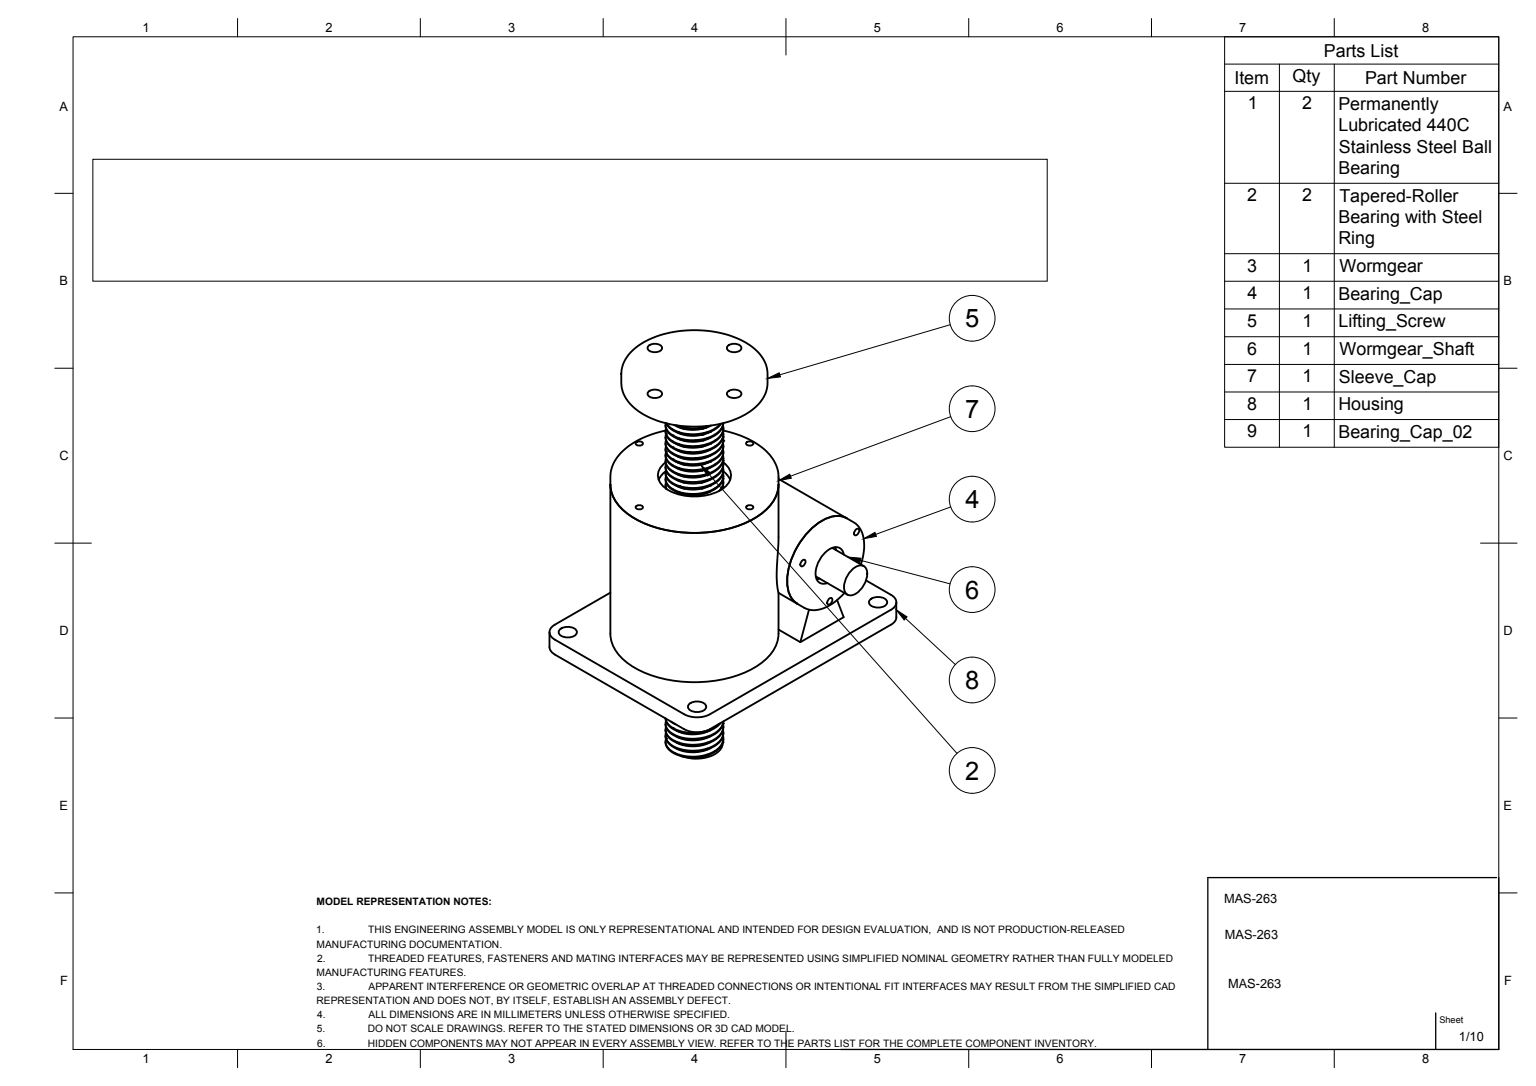
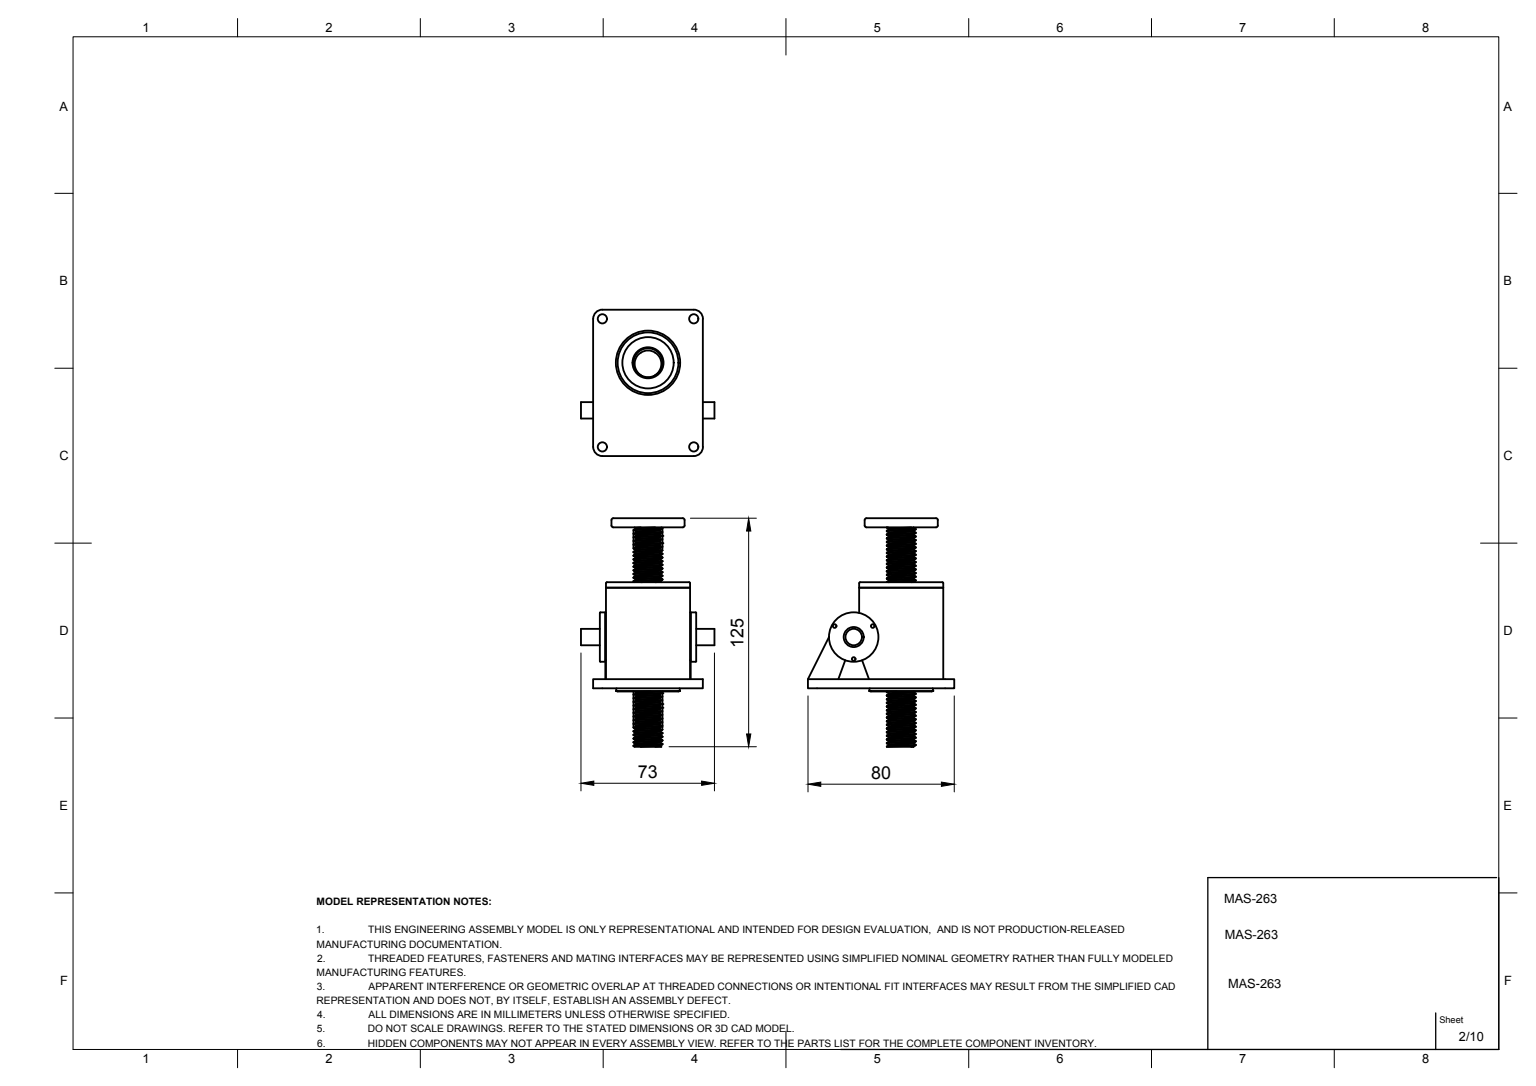
ISO-10303-21;
HEADER;
/* Generated by software containing ST-Developer
 * from STEP Tools, Inc. (www.steptools.com) 
 */

FILE_DESCRIPTION(
/* description */ (''),
/* implementation_level */ '2;1');

FILE_NAME(
/* name */ 'MAS-263',
/* time_stamp */ '2026-10-12T15:47:30-07:00',
/* author */ (''),
/* organization */ (''),
/* preprocessor_version */ 'ST-DEVELOPER v20.2',
/* originating_system */ 'Autodesk Translation Framework v15.15.0.0',
/* authorisation */ '');

FILE_SCHEMA (('AUTOMOTIVE_DESIGN { 1 0 10303 214 3 1 1 }'));
ENDSEC;

DATA;
#10=MECHANICAL_DESIGN_GEOMETRIC_PRESENTATION_REPRESENTATION('',(#82,#83,
#84,#85,#86,#87,#88,#89,#90,#91,#92,#93,#94,#95,#96,#97,#98,#99,#100,#101,
#102,#103,#104,#105,#106,#107,#108,#109,#110,#111,#112,#113,#114,#115,#116),
#88483);
#11=ITEM_DEFINED_TRANSFORMATION($,$,#13993,#14368);
#12=ITEM_DEFINED_TRANSFORMATION($,$,#14115,#14369);
#13=ITEM_DEFINED_TRANSFORMATION($,$,#13128,#14370);
#14=ITEM_DEFINED_TRANSFORMATION($,$,#13713,#14371);
#15=ITEM_DEFINED_TRANSFORMATION($,$,#13735,#14372);
#16=ITEM_DEFINED_TRANSFORMATION($,$,#13828,#14373);
#17=ITEM_DEFINED_TRANSFORMATION($,$,#13851,#14374);
#18=ITEM_DEFINED_TRANSFORMATION($,$,#13876,#14375);
#19=ITEM_DEFINED_TRANSFORMATION($,$,#13971,#14376);
#20=ITEM_DEFINED_TRANSFORMATION($,$,#13993,#14377);
#21=ITEM_DEFINED_TRANSFORMATION($,$,#14115,#14378);
#22=(
REPRESENTATION_RELATIONSHIP($,$,#88527,#88519)
REPRESENTATION_RELATIONSHIP_WITH_TRANSFORMATION(#11)
SHAPE_REPRESENTATION_RELATIONSHIP()
);
#23=(
REPRESENTATION_RELATIONSHIP($,$,#88528,#88519)
REPRESENTATION_RELATIONSHIP_WITH_TRANSFORMATION(#12)
SHAPE_REPRESENTATION_RELATIONSHIP()
);
#24=(
REPRESENTATION_RELATIONSHIP($,$,#88520,#88519)
REPRESENTATION_RELATIONSHIP_WITH_TRANSFORMATION(#13)
SHAPE_REPRESENTATION_RELATIONSHIP()
);
#25=(
REPRESENTATION_RELATIONSHIP($,$,#88521,#88519)
REPRESENTATION_RELATIONSHIP_WITH_TRANSFORMATION(#14)
SHAPE_REPRESENTATION_RELATIONSHIP()
);
#26=(
REPRESENTATION_RELATIONSHIP($,$,#88522,#88519)
REPRESENTATION_RELATIONSHIP_WITH_TRANSFORMATION(#15)
SHAPE_REPRESENTATION_RELATIONSHIP()
);
#27=(
REPRESENTATION_RELATIONSHIP($,$,#88523,#88519)
REPRESENTATION_RELATIONSHIP_WITH_TRANSFORMATION(#16)
SHAPE_REPRESENTATION_RELATIONSHIP()
);
#28=(
REPRESENTATION_RELATIONSHIP($,$,#88524,#88519)
REPRESENTATION_RELATIONSHIP_WITH_TRANSFORMATION(#17)
SHAPE_REPRESENTATION_RELATIONSHIP()
);
#29=(
REPRESENTATION_RELATIONSHIP($,$,#88525,#88519)
REPRESENTATION_RELATIONSHIP_WITH_TRANSFORMATION(#18)
SHAPE_REPRESENTATION_RELATIONSHIP()
);
#30=(
REPRESENTATION_RELATIONSHIP($,$,#88526,#88519)
REPRESENTATION_RELATIONSHIP_WITH_TRANSFORMATION(#19)
SHAPE_REPRESENTATION_RELATIONSHIP()
);
#31=(
REPRESENTATION_RELATIONSHIP($,$,#88527,#88519)
REPRESENTATION_RELATIONSHIP_WITH_TRANSFORMATION(#20)
SHAPE_REPRESENTATION_RELATIONSHIP()
);
#32=(
REPRESENTATION_RELATIONSHIP($,$,#88528,#88519)
REPRESENTATION_RELATIONSHIP_WITH_TRANSFORMATION(#21)
SHAPE_REPRESENTATION_RELATIONSHIP()
);
#33=CONTEXT_DEPENDENT_SHAPE_REPRESENTATION(#22,#88508);
#34=CONTEXT_DEPENDENT_SHAPE_REPRESENTATION(#23,#88509);
#35=CONTEXT_DEPENDENT_SHAPE_REPRESENTATION(#24,#88510);
#36=CONTEXT_DEPENDENT_SHAPE_REPRESENTATION(#25,#88511);
#37=CONTEXT_DEPENDENT_SHAPE_REPRESENTATION(#26,#88512);
#38=CONTEXT_DEPENDENT_SHAPE_REPRESENTATION(#27,#88513);
#39=CONTEXT_DEPENDENT_SHAPE_REPRESENTATION(#28,#88514);
#40=CONTEXT_DEPENDENT_SHAPE_REPRESENTATION(#29,#88515);
#41=CONTEXT_DEPENDENT_SHAPE_REPRESENTATION(#30,#88516);
#42=CONTEXT_DEPENDENT_SHAPE_REPRESENTATION(#31,#88517);
#43=CONTEXT_DEPENDENT_SHAPE_REPRESENTATION(#32,#88518);
#44=NEXT_ASSEMBLY_USAGE_OCCURRENCE(
'Permanently Lubricated 440C Stainless Steel Ball Bearing:1',
'Permanently Lubricated 440C Stainless Steel Ball Bearing:1',
'Permanently Lubricated 440C Stainless Steel Ball Bearing:1',#88530,#88538,
'Permanently Lubricated 440C Stainless Steel Ball Bearing:1');
#45=NEXT_ASSEMBLY_USAGE_OCCURRENCE(
'Tapered-Roller Bearing with Steel Ring:1',
'Tapered-Roller Bearing with Steel Ring:1',
'Tapered-Roller Bearing with Steel Ring:1',#88530,#88539,
'Tapered-Roller Bearing with Steel Ring:1');
#46=NEXT_ASSEMBLY_USAGE_OCCURRENCE('Wormgear:1','Wormgear:1',
'Wormgear:1',#88530,#88531,'Wormgear:1');
#47=NEXT_ASSEMBLY_USAGE_OCCURRENCE('Bearing_Cap:1','Bearing_Cap:1',
'Bearing_Cap:1',#88530,#88532,'Bearing_Cap:1');
#48=NEXT_ASSEMBLY_USAGE_OCCURRENCE('Lifting_Screw:1','Lifting_Screw:1',
'Lifting_Screw:1',#88530,#88533,'Lifting_Screw:1');
#49=NEXT_ASSEMBLY_USAGE_OCCURRENCE('Wormgear_Shaft:1',
'Wormgear_Shaft:1','Wormgear_Shaft:1',#88530,#88534,'Wormgear_Shaft:1');
#50=NEXT_ASSEMBLY_USAGE_OCCURRENCE('Sleeve_Cap:1','Sleeve_Cap:1',
'Sleeve_Cap:1',#88530,#88535,'Sleeve_Cap:1');
#51=NEXT_ASSEMBLY_USAGE_OCCURRENCE('Housing:1','Housing:1','Housing:1',
#88530,#88536,'Housing:1');
#52=NEXT_ASSEMBLY_USAGE_OCCURRENCE('Bearing_Cap_02:1',
'Bearing_Cap_02:1','Bearing_Cap_02:1',#88530,#88537,'Bearing_Cap_02:1');
#53=NEXT_ASSEMBLY_USAGE_OCCURRENCE(
'Permanently Lubricated 440C Stainless Steel Ball Bearing:2',
'Permanently Lubricated 440C Stainless Steel Ball Bearing:2',
'Permanently Lubricated 440C Stainless Steel Ball Bearing:2',#88530,#88538,
'Permanently Lubricated 440C Stainless Steel Ball Bearing:2');
#54=NEXT_ASSEMBLY_USAGE_OCCURRENCE(
'Tapered-Roller Bearing with Steel Ring:2',
'Tapered-Roller Bearing with Steel Ring:2',
'Tapered-Roller Bearing with Steel Ring:2',#88530,#88539,
'Tapered-Roller Bearing with Steel Ring:2');
#55=SPHERICAL_SURFACE('',#14025,2.0625);
#56=SPHERICAL_SURFACE('',#14081,2.0625);
#57=SPHERICAL_SURFACE('',#14083,2.0625);
#58=SPHERICAL_SURFACE('',#14085,2.0625);
#59=SPHERICAL_SURFACE('',#14087,2.0625);
#60=SPHERICAL_SURFACE('',#14089,2.0625);
#61=SPHERICAL_SURFACE('',#14091,2.0625);
#62=SPHERICAL_SURFACE('',#14093,2.0625);
#63=SPHERICAL_SURFACE('',#14095,2.0625);
#64=SHAPE_REPRESENTATION_RELATIONSHIP('SRR','None',#88520,#73);
#65=SHAPE_REPRESENTATION_RELATIONSHIP('SRR','None',#88521,#74);
#66=SHAPE_REPRESENTATION_RELATIONSHIP('SRR','None',#88522,#75);
#67=SHAPE_REPRESENTATION_RELATIONSHIP('SRR','None',#88523,#76);
#68=SHAPE_REPRESENTATION_RELATIONSHIP('SRR','None',#88524,#77);
#69=SHAPE_REPRESENTATION_RELATIONSHIP('SRR','None',#88525,#78);
#70=SHAPE_REPRESENTATION_RELATIONSHIP('SRR','None',#88526,#79);
#71=SHAPE_REPRESENTATION_RELATIONSHIP('SRR','None',#88527,#80);
#72=SHAPE_REPRESENTATION_RELATIONSHIP('SRR','None',#88528,#81);
#73=ADVANCED_BREP_SHAPE_REPRESENTATION('',(#117),#88474);
#74=ADVANCED_BREP_SHAPE_REPRESENTATION('',(#118),#88475);
#75=ADVANCED_BREP_SHAPE_REPRESENTATION('',(#119),#88476);
#76=ADVANCED_BREP_SHAPE_REPRESENTATION('',(#120),#88477);
#77=ADVANCED_BREP_SHAPE_REPRESENTATION('',(#121),#88478);
#78=ADVANCED_BREP_SHAPE_REPRESENTATION('',(#122),#88479);
#79=ADVANCED_BREP_SHAPE_REPRESENTATION('',(#123),#88480);
#80=ADVANCED_BREP_SHAPE_REPRESENTATION('',(#124,#125,#126,#127,#128,#129,
#130,#131,#132,#133,#134,#135,#136,#137),#88481);
#81=ADVANCED_BREP_SHAPE_REPRESENTATION('',(#138,#139,#140,#141,#142,#143,
#144,#145,#146,#147,#148,#149,#150,#151),#88482);
#82=STYLED_ITEM('',(#88574),#117);
#83=STYLED_ITEM('',(#88574),#118);
#84=STYLED_ITEM('',(#88574),#119);
#85=STYLED_ITEM('',(#88574),#120);
#86=STYLED_ITEM('',(#88574),#121);
#87=STYLED_ITEM('',(#88574),#122);
#88=STYLED_ITEM('',(#88574),#123);
#89=STYLED_ITEM('',(#88574),#124);
#90=STYLED_ITEM('',(#88574),#125);
#91=STYLED_ITEM('',(#88574),#126);
#92=STYLED_ITEM('',(#88574),#127);
#93=STYLED_ITEM('',(#88574),#128);
#94=STYLED_ITEM('',(#88574),#129);
#95=STYLED_ITEM('',(#88574),#130);
#96=STYLED_ITEM('',(#88574),#131);
#97=STYLED_ITEM('',(#88574),#132);
#98=STYLED_ITEM('',(#88574),#133);
#99=STYLED_ITEM('',(#88574),#134);
#100=STYLED_ITEM('',(#88574),#135);
#101=STYLED_ITEM('',(#88574),#136);
#102=STYLED_ITEM('',(#88574),#137);
#103=STYLED_ITEM('',(#88574),#138);
#104=STYLED_ITEM('',(#88574),#139);
#105=STYLED_ITEM('',(#88574),#140);
#106=STYLED_ITEM('',(#88574),#141);
#107=STYLED_ITEM('',(#88574),#142);
#108=STYLED_ITEM('',(#88574),#143);
#109=STYLED_ITEM('',(#88574),#144);
#110=STYLED_ITEM('',(#88574),#145);
#111=STYLED_ITEM('',(#88574),#146);
#112=STYLED_ITEM('',(#88574),#147);
#113=STYLED_ITEM('',(#88574),#148);
#114=STYLED_ITEM('',(#88574),#149);
#115=STYLED_ITEM('',(#88574),#150);
#116=STYLED_ITEM('',(#88574),#151);
#117=MANIFOLD_SOLID_BREP('Body1',#12992);
#118=MANIFOLD_SOLID_BREP('Body1',#12993);
#119=MANIFOLD_SOLID_BREP('Body1',#12994);
#120=MANIFOLD_SOLID_BREP('Body1',#12995);
#121=MANIFOLD_SOLID_BREP('Body1',#12996);
#122=MANIFOLD_SOLID_BREP('Body1',#12997);
#123=MANIFOLD_SOLID_BREP('Body1',#12998);
#124=MANIFOLD_SOLID_BREP('Body1',#12999);
#125=MANIFOLD_SOLID_BREP('Body2',#13000);
#126=MANIFOLD_SOLID_BREP('Body3',#13001);
#127=MANIFOLD_SOLID_BREP('Body4',#13002);
#128=MANIFOLD_SOLID_BREP('Body5',#13003);
#129=MANIFOLD_SOLID_BREP('Body6',#13004);
#130=MANIFOLD_SOLID_BREP('Body7',#13005);
#131=MANIFOLD_SOLID_BREP('Body8',#13006);
#132=MANIFOLD_SOLID_BREP('Body9',#13007);
#133=MANIFOLD_SOLID_BREP('Body10',#13008);
#134=MANIFOLD_SOLID_BREP('Body11',#13009);
#135=MANIFOLD_SOLID_BREP('Body12',#13010);
#136=MANIFOLD_SOLID_BREP('Body13',#13011);
#137=MANIFOLD_SOLID_BREP('Body14',#13012);
#138=MANIFOLD_SOLID_BREP('Body1',#13013);
#139=MANIFOLD_SOLID_BREP('Body2',#13014);
#140=MANIFOLD_SOLID_BREP('Body3',#13015);
#141=MANIFOLD_SOLID_BREP('Body4',#13016);
#142=MANIFOLD_SOLID_BREP('Body5',#13017);
#143=MANIFOLD_SOLID_BREP('Body6',#13018);
#144=MANIFOLD_SOLID_BREP('Body7',#13019);
#145=MANIFOLD_SOLID_BREP('Body8',#13020);
#146=MANIFOLD_SOLID_BREP('Body9',#13021);
#147=MANIFOLD_SOLID_BREP('Body10',#13022);
#148=MANIFOLD_SOLID_BREP('Body11',#13023);
#149=MANIFOLD_SOLID_BREP('Body12',#13024);
#150=MANIFOLD_SOLID_BREP('Body13',#13025);
#151=MANIFOLD_SOLID_BREP('Body14',#13026);
#152=TOROIDAL_SURFACE('',#13586,31.2524414898979,12.0232331490224);
#153=TOROIDAL_SURFACE('',#13587,31.2524414898979,12.0232331490224);
#154=TOROIDAL_SURFACE('',#13588,31.2524414898979,12.0232331490224);
#155=TOROIDAL_SURFACE('',#13589,31.2524414898979,12.0232331490224);
#156=TOROIDAL_SURFACE('',#13590,31.2524414898979,12.0232331490224);
#157=TOROIDAL_SURFACE('',#13591,31.2524414898979,12.0232331490224);
#158=TOROIDAL_SURFACE('',#13592,31.2524414898979,12.0232331490224);
#159=TOROIDAL_SURFACE('',#13593,31.2524414898979,12.0232331490224);
#160=TOROIDAL_SURFACE('',#13594,31.2524414898979,12.0232331490224);
#161=TOROIDAL_SURFACE('',#13595,31.2524414898979,12.0232331490224);
#162=TOROIDAL_SURFACE('',#13596,31.2524414898979,12.0232331490224);
#163=TOROIDAL_SURFACE('',#13597,31.2524414898979,12.0232331490224);
#164=TOROIDAL_SURFACE('',#13598,31.2524414898979,12.0232331490224);
#165=TOROIDAL_SURFACE('',#13599,31.2524414898979,12.0232331490224);
#166=TOROIDAL_SURFACE('',#13600,31.2524414898979,12.0232331490224);
#167=TOROIDAL_SURFACE('',#13601,31.2524414898979,12.0232331490224);
#168=TOROIDAL_SURFACE('',#13602,31.2524414898979,12.0232331490224);
#169=TOROIDAL_SURFACE('',#13603,31.2524414898979,12.0232331490224);
#170=TOROIDAL_SURFACE('',#13723,13.2,0.3);
#171=TOROIDAL_SURFACE('',#13814,19.,1.);
#172=TOROIDAL_SURFACE('',#13823,19.,1.);
#173=TOROIDAL_SURFACE('',#13852,22.5,0.5);
#174=TOROIDAL_SURFACE('',#13981,13.2,0.3);
#175=TOROIDAL_SURFACE('',#13994,7.57083333333333,2.0625);
#176=TOROIDAL_SURFACE('',#14007,5.00416666666667,0.260975870478375);
#177=TOROIDAL_SURFACE('',#14010,5.98069079618829,0.260975870478375);
#178=TOROIDAL_SURFACE('',#14017,5.98069079618829,0.260975870478375);
#179=TOROIDAL_SURFACE('',#14020,5.00416666666667,0.260975870478376);
#180=TOROIDAL_SURFACE('',#14030,6.50566666666666,0.0439999999999998);
#181=TOROIDAL_SURFACE('',#14047,6.50566666666666,0.0439999999999998);
#182=TOROIDAL_SURFACE('',#14075,7.57083333333333,2.0625);
#183=TOROIDAL_SURFACE('',#14100,6.32416666666667,0.0824999999999997);
#184=TOROIDAL_SURFACE('',#14105,6.42956528249449,0.0228986158278278);
#185=TOROIDAL_SURFACE('',#14116,19.725,0.275);
#186=TOROIDAL_SURFACE('',#14121,19.725,0.275);
#187=TOROIDAL_SURFACE('',#14141,13.4297712445485,0.500000000000001);
#188=TOROIDAL_SURFACE('',#14288,8.775,0.275);
#189=TOROIDAL_SURFACE('',#14293,8.775,0.275);
#190=ELLIPSE('',#13431,4.95617711892471,2.63133228090511);
#191=ELLIPSE('',#13435,4.75668688712327,2.27225375309584);
#192=ELLIPSE('',#13437,4.75863627530638,2.27415348140964);
#193=ELLIPSE('',#13440,4.95728877126817,2.63371397588203);
#194=ELLIPSE('',#13442,4.75866828260205,2.27425851275333);
#195=ELLIPSE('',#13445,4.75676106745748,2.27242229825786);
#196=ELLIPSE('',#13449,4.95667352087062,2.63240829794641);
#197=ELLIPSE('',#13451,4.7584190628443,2.27363285019894);
#198=ELLIPSE('',#13454,4.95667835669603,2.63239579497757);
#199=ELLIPSE('',#13456,4.75854812753772,2.27394108049538);
#200=ELLIPSE('',#13459,4.75677100793017,2.27242870543475);
#201=ELLIPSE('',#13461,4.75867193464204,2.27425380136302);
#202=ELLIPSE('',#13464,4.95726759568865,2.6336926662635);
#203=ELLIPSE('',#13468,4.95701438814411,2.63313504607068);
#204=ELLIPSE('',#13470,4.75854681981732,2.2739502765965);
#205=ELLIPSE('',#13473,4.95618501228156,2.63134042899261);
#206=ELLIPSE('',#13475,4.7584142614767,2.27361309014758);
#207=ELLIPSE('',#13478,4.75669159480521,2.2722579746974);
#208=ELLIPSE('',#13480,4.75864115660623,2.27415786894356);
#209=ELLIPSE('',#13483,4.95728232466036,2.63370732110983);
#210=ELLIPSE('',#13487,4.75677068526519,2.27243087287144);
#211=ELLIPSE('',#13489,4.7586448406126,2.27416728394003);
#212=ELLIPSE('',#13492,4.95668328813391,2.63241837237374);
#213=ELLIPSE('',#13494,4.75842436294074,2.27363759998898);
#214=ELLIPSE('',#13497,4.95667013101771,2.63238731158809);
#215=ELLIPSE('',#13499,4.75854743391675,2.27394045782711);
#216=ELLIPSE('',#13502,4.75676675579442,2.2724249104892);
#217=ELLIPSE('',#13504,4.75867738441917,2.27425870334034);
#218=ELLIPSE('',#13507,4.95726880833492,2.63369391317148);
#219=ELLIPSE('',#13511,4.75669596930896,2.27226683434943);
#220=ELLIPSE('',#13516,4.95643307274524,2.6318762393004);
#221=ELLIPSE('',#13520,4.75673549365485,2.27235394216187);
#222=ELLIPSE('',#13524,4.75679029012967,2.27247967692196);
#223=ELLIPSE('',#13528,4.7567393782921,2.272363575723);
#224=ELLIPSE('',#13532,4.75651933654551,2.27183321728508);
#225=ELLIPSE('',#13536,4.75664142700045,2.27213579341419);
#226=ELLIPSE('',#13540,4.75678866048944,2.27247015627199);
#227=ELLIPSE('',#13544,4.75677929568429,2.27246401653084);
#228=ELLIPSE('',#13548,4.7566467644084,2.27215101059843);
#229=ELLIPSE('',#13552,4.75649416981517,2.27179513573923);
#230=ELLIPSE('',#13556,4.75673834040189,2.27235649175302);
#231=ELLIPSE('',#13560,4.7567849310581,2.27247488275134);
#232=ELLIPSE('',#13564,4.75674169310957,2.27236560062855);
#233=ELLIPSE('',#13568,4.75650474573201,2.27182012088408);
#234=ELLIPSE('',#13572,4.75664401077444,2.27213811276921);
#235=ELLIPSE('',#13576,4.75677759115208,2.27246023178278);
#236=ELLIPSE('',#13580,4.95724426884637,2.63364727447111);
#237=ELLIPSE('',#13584,4.95686686267409,2.63282116312156);
#238=ELLIPSE('',#13840,8.40043383461932,7.09899410493904);
#239=ELLIPSE('',#13843,8.34870203930529,7.04180185640227);
#240=ELLIPSE('',#13948,67.247501203751,23.);
#241=ELLIPSE('',#13950,67.247501203751,23.);
#242=ELLIPSE('',#14151,15.0801280312954,14.5834816640173);
#243=ELLIPSE('',#14152,17.3517853554452,16.7803246128912);
#244=ELLIPSE('',#14153,17.3517853554452,16.7803246128912);
#245=ELLIPSE('',#14154,15.0801280312954,14.5834816640173);
#246=ELLIPSE('',#14155,15.0801280312954,14.5834816640173);
#247=ELLIPSE('',#14156,17.3517853554452,16.7803246128912);
#248=ELLIPSE('',#14157,17.3517853554886,16.7803246129121);
#249=ELLIPSE('',#14158,15.0801280313552,14.5834816640461);
#250=ELLIPSE('',#14159,17.351785355493,16.7803246129139);
#251=ELLIPSE('',#14160,15.0801280313139,14.5834816640261);
#252=ELLIPSE('',#14161,17.3517853552649,16.7803246128045);
#253=ELLIPSE('',#14162,15.0801280313118,14.583481664025);
#254=ELLIPSE('',#14163,17.3517853554016,16.7803246128701);
#255=ELLIPSE('',#14164,15.0801280313076,14.583481664023);
#256=ELLIPSE('',#14165,17.3517853554702,16.780324612903);
#257=ELLIPSE('',#14166,15.0801280313709,14.5834816640533);
#258=ELLIPSE('',#14167,17.3517853554861,16.7803246129107);
#259=ELLIPSE('',#14168,15.08012803127,14.583481664005);
#260=ELLIPSE('',#14169,17.3517853554707,16.7803246129033);
#261=ELLIPSE('',#14170,15.0801280312716,14.5834816640059);
#262=ELLIPSE('',#14171,17.3517853553197,16.7803246128311);
#263=ELLIPSE('',#14172,15.0801280311918,14.5834816639677);
#264=ELLIPSE('',#14173,17.3517853552856,16.7803246128146);
#265=ELLIPSE('',#14174,15.0801280313508,14.5834816640437);
#266=ELLIPSE('',#14176,18.421055935048,17.8143800174044);
#267=ELLIPSE('',#14177,16.1493986108983,15.6175370685304);
#268=ELLIPSE('',#14178,16.1493986108983,15.6175370685304);
#269=ELLIPSE('',#14179,18.421055935048,17.8143800174044);
#270=ELLIPSE('',#14180,16.1493986108983,15.6175370685304);
#271=ELLIPSE('',#14181,18.421055935048,17.8143800174044);
#272=ELLIPSE('',#14182,18.4210559352732,17.8143800175124);
#273=ELLIPSE('',#14183,16.1493986107542,15.6175370684613);
#274=ELLIPSE('',#14184,18.4210559346699,17.8143800172222);
#275=ELLIPSE('',#14185,16.1493986106406,15.6175370684066);
#276=ELLIPSE('',#14186,18.421055934899,17.8143800173331);
#277=ELLIPSE('',#14187,16.1493986106858,15.6175370684285);
#278=ELLIPSE('',#14188,18.4210559350675,17.8143800174135);
#279=ELLIPSE('',#14189,16.1493986109801,15.6175370685696);
#280=ELLIPSE('',#14190,18.4210559350065,17.8143800173844);
#281=ELLIPSE('',#14191,16.1493986108565,15.6175370685105);
#282=ELLIPSE('',#14192,18.4210559345343,17.8143800171572);
#283=ELLIPSE('',#14193,16.1493986108155,15.6175370684905);
#284=ELLIPSE('',#14194,18.4210559346994,17.8143800172367);
#285=ELLIPSE('',#14195,16.1493986107405,15.6175370684544);
#286=ELLIPSE('',#14196,18.4210559344304,17.814380017107);
#287=ELLIPSE('',#14197,16.1493986109695,15.6175370685645);
#288=ELLIPSE('',#14198,18.4210559346512,17.8143800172135);
#289=ELLIPSE('',#14199,16.1493986107542,15.6175370684612);
#290=CONICAL_SURFACE('',#13250,17.9979895488606,0.785398163397448);
#291=CONICAL_SURFACE('',#13253,17.9979895488606,0.785398163397448);
#292=CONICAL_SURFACE('',#13256,17.9979895488606,0.785398163397448);
#293=CONICAL_SURFACE('',#13259,17.9979895488606,0.785398163397448);
#294=CONICAL_SURFACE('',#13262,17.9979895488606,0.785398163397448);
#295=CONICAL_SURFACE('',#13265,17.9979895488606,0.785398163397448);
#296=CONICAL_SURFACE('',#13268,17.9979895488606,0.785398163397448);
#297=CONICAL_SURFACE('',#13271,17.9979895488606,0.785398163397448);
#298=CONICAL_SURFACE('',#13274,17.9979895488606,0.785398163397448);
#299=CONICAL_SURFACE('',#13277,17.9979895488606,0.785398163397448);
#300=CONICAL_SURFACE('',#13280,17.9979895488606,0.785398163397448);
#301=CONICAL_SURFACE('',#13283,17.9979895488606,0.785398163397448);
#302=CONICAL_SURFACE('',#13286,17.9979895488606,0.785398163397448);
#303=CONICAL_SURFACE('',#13289,17.9979895488606,0.785398163397448);
#304=CONICAL_SURFACE('',#13292,17.9979895488606,0.785398163397448);
#305=CONICAL_SURFACE('',#13295,17.9979895488606,0.785398163397448);
#306=CONICAL_SURFACE('',#13298,17.9979895488606,0.785398163397448);
#307=CONICAL_SURFACE('',#13301,17.9979895488606,0.785398163397448);
#308=CONICAL_SURFACE('',#13304,17.9979895488606,0.785398163397448);
#309=CONICAL_SURFACE('',#13309,17.9979895488606,0.785398163397448);
#310=CONICAL_SURFACE('',#13314,17.9979895488606,0.785398163397448);
#311=CONICAL_SURFACE('',#13319,17.9979895488606,0.785398163397448);
#312=CONICAL_SURFACE('',#13324,17.9979895488606,0.785398163397448);
#313=CONICAL_SURFACE('',#13329,17.9979895488606,0.785398163397448);
#314=CONICAL_SURFACE('',#13334,17.9979895488606,0.785398163397448);
#315=CONICAL_SURFACE('',#13339,17.9979895488606,0.785398163397448);
#316=CONICAL_SURFACE('',#13344,17.9979895488606,0.785398163397448);
#317=CONICAL_SURFACE('',#13349,17.9979895488606,0.785398163397448);
#318=CONICAL_SURFACE('',#13354,17.9979895488606,0.785398163397448);
#319=CONICAL_SURFACE('',#13359,17.9979895488606,0.785398163397448);
#320=CONICAL_SURFACE('',#13364,17.9979895488606,0.785398163397448);
#321=CONICAL_SURFACE('',#13369,17.9979895488606,0.785398163397448);
#322=CONICAL_SURFACE('',#13374,17.9979895488606,0.785398163397448);
#323=CONICAL_SURFACE('',#13379,17.9979895488606,0.785398163397448);
#324=CONICAL_SURFACE('',#13384,17.9979895488606,0.785398163397448);
#325=CONICAL_SURFACE('',#13389,17.9979895488606,0.785398163397448);
#326=CONICAL_SURFACE('',#13998,4.5,0.26179938779915);
#327=CONICAL_SURFACE('',#14005,4.75208333333333,0.261799387799149);
#328=CONICAL_SURFACE('',#14033,8.9,0.523598775598299);
#329=CONICAL_SURFACE('',#14050,8.79,0.523598775598297);
#330=CONICAL_SURFACE('',#14054,9.01847925309041,0.349065850398861);
#331=CONICAL_SURFACE('',#14057,9.16847925309041,0.78539816339744);
#332=CONICAL_SURFACE('',#14059,10.,0.523598775598291);
#333=CONICAL_SURFACE('',#14065,9.82679491924311,0.52359877559829);
#334=CONICAL_SURFACE('',#14067,9.0184792530904,0.78539816339744);
#335=CONICAL_SURFACE('',#14070,8.9,0.349065850398861);
#336=CONICAL_SURFACE('',#14109,6.46166666666667,0.17453292519942);
#337=CONICAL_SURFACE('',#14125,15.4,0.249233017184783);
#338=CONICAL_SURFACE('',#14131,12.7058184384753,1.32156330961012);
#339=CONICAL_SURFACE('',#14136,16.6071946160828,1.32156330961011);
#340=CONICAL_SURFACE('',#14146,13.3064408708579,1.32156330961011);
#341=CONICAL_SURFACE('',#14149,12.4591576910941,0.249233017184783);
#342=CONICAL_SURFACE('',#14150,13.0685506725942,0.249233017184784);
#343=CONICAL_SURFACE('',#14175,17.5762965073726,0.249233017184784);
#344=CONICAL_SURFACE('',#14297,10.6410293263727,1.32156330961011);
#345=CONICAL_SURFACE('',#14301,12.6998790237181,0.249233017184785);
#346=CONICAL_SURFACE('',#14304,14.0317131491268,1.32156330961011);
#347=FACE_BOUND('',#1491,.T.);
#348=FACE_BOUND('',#1720,.T.);
#349=FACE_BOUND('',#1788,.T.);
#350=FACE_BOUND('',#1789,.T.);
#351=FACE_BOUND('',#1790,.T.);
#352=FACE_BOUND('',#1791,.T.);
#353=FACE_BOUND('',#1794,.T.);
#354=FACE_BOUND('',#1795,.T.);
#355=FACE_BOUND('',#1796,.T.);
#356=FACE_BOUND('',#1797,.T.);
#357=FACE_BOUND('',#1869,.T.);
#358=FACE_BOUND('',#1870,.T.);
#359=FACE_BOUND('',#1871,.T.);
#360=FACE_BOUND('',#1872,.T.);
#361=FACE_BOUND('',#1873,.T.);
#362=FACE_BOUND('',#1876,.T.);
#363=FACE_BOUND('',#1877,.T.);
#364=FACE_BOUND('',#1878,.T.);
#365=FACE_BOUND('',#1879,.T.);
#366=FACE_BOUND('',#1889,.T.);
#367=FACE_BOUND('',#1894,.T.);
#368=FACE_BOUND('',#1937,.T.);
#369=FACE_BOUND('',#1938,.T.);
#370=FACE_BOUND('',#1939,.T.);
#371=FACE_BOUND('',#1940,.T.);
#372=FACE_BOUND('',#1941,.T.);
#373=FACE_BOUND('',#1948,.T.);
#374=FACE_BOUND('',#1949,.T.);
#375=FACE_BOUND('',#1950,.T.);
#376=FACE_BOUND('',#1951,.T.);
#377=FACE_BOUND('',#1952,.T.);
#378=FACE_BOUND('',#1974,.T.);
#379=FACE_BOUND('',#1975,.T.);
#380=FACE_BOUND('',#1976,.T.);
#381=FACE_BOUND('',#1977,.T.);
#382=FACE_BOUND('',#1995,.T.);
#383=FACE_BOUND('',#1999,.T.);
#384=FACE_BOUND('',#2001,.T.);
#385=FACE_BOUND('',#2003,.T.);
#386=FACE_BOUND('',#2004,.T.);
#387=FACE_BOUND('',#2005,.T.);
#388=FACE_BOUND('',#2006,.T.);
#389=FACE_BOUND('',#2007,.T.);
#390=FACE_BOUND('',#2010,.T.);
#391=FACE_BOUND('',#2011,.T.);
#392=FACE_BOUND('',#2012,.T.);
#393=FACE_BOUND('',#2013,.T.);
#394=FACE_BOUND('',#2015,.T.);
#395=FACE_BOUND('',#2016,.T.);
#396=FACE_BOUND('',#2017,.T.);
#397=FACE_BOUND('',#2018,.T.);
#398=FACE_BOUND('',#2019,.T.);
#399=FACE_BOUND('',#2026,.T.);
#400=FACE_BOUND('',#2027,.T.);
#401=FACE_BOUND('',#2028,.T.);
#402=FACE_BOUND('',#2029,.T.);
#403=FACE_BOUND('',#2032,.T.);
#404=FACE_BOUND('',#2033,.T.);
#405=FACE_BOUND('',#2034,.T.);
#406=FACE_BOUND('',#2035,.T.);
#407=FACE_BOUND('',#2047,.T.);
#408=FACE_BOUND('',#2049,.T.);
#409=FACE_BOUND('',#2056,.T.);
#410=FACE_BOUND('',#2058,.T.);
#411=FACE_BOUND('',#2064,.T.);
#412=FACE_BOUND('',#2066,.T.);
#413=FACE_BOUND('',#2078,.T.);
#414=FACE_BOUND('',#2080,.T.);
#415=FACE_BOUND('',#2096,.T.);
#416=FACE_BOUND('',#2102,.T.);
#417=FACE_BOUND('',#2104,.T.);
#418=FACE_BOUND('',#2111,.T.);
#419=FACE_BOUND('',#2112,.T.);
#420=FACE_BOUND('',#2113,.T.);
#421=FACE_BOUND('',#2114,.T.);
#422=FACE_BOUND('',#2115,.T.);
#423=FACE_BOUND('',#2116,.T.);
#424=FACE_BOUND('',#2117,.T.);
#425=FACE_BOUND('',#2118,.T.);
#426=FACE_BOUND('',#2119,.T.);
#427=FACE_BOUND('',#2120,.T.);
#428=FACE_BOUND('',#2122,.T.);
#429=FACE_BOUND('',#2123,.T.);
#430=FACE_BOUND('',#2124,.T.);
#431=FACE_BOUND('',#2125,.T.);
#432=FACE_BOUND('',#2126,.T.);
#433=FACE_BOUND('',#2127,.T.);
#434=FACE_BOUND('',#2128,.T.);
#435=FACE_BOUND('',#2129,.T.);
#436=FACE_BOUND('',#2130,.T.);
#437=FACE_BOUND('',#2131,.T.);
#438=FACE_BOUND('',#2185,.T.);
#439=FACE_BOUND('',#2187,.T.);
#440=PLANE('',#13159);
#441=PLANE('',#13196);
#442=PLANE('',#13199);
#443=PLANE('',#13202);
#444=PLANE('',#13205);
#445=PLANE('',#13208);
#446=PLANE('',#13211);
#447=PLANE('',#13214);
#448=PLANE('',#13217);
#449=PLANE('',#13220);
#450=PLANE('',#13223);
#451=PLANE('',#13226);
#452=PLANE('',#13229);
#453=PLANE('',#13232);
#454=PLANE('',#13235);
#455=PLANE('',#13238);
#456=PLANE('',#13241);
#457=PLANE('',#13244);
#458=PLANE('',#13247);
#459=PLANE('',#13394);
#460=PLANE('',#13396);
#461=PLANE('',#13398);
#462=PLANE('',#13400);
#463=PLANE('',#13402);
#464=PLANE('',#13404);
#465=PLANE('',#13406);
#466=PLANE('',#13408);
#467=PLANE('',#13410);
#468=PLANE('',#13412);
#469=PLANE('',#13414);
#470=PLANE('',#13416);
#471=PLANE('',#13418);
#472=PLANE('',#13420);
#473=PLANE('',#13422);
#474=PLANE('',#13424);
#475=PLANE('',#13426);
#476=PLANE('',#13428);
#477=PLANE('',#13430);
#478=PLANE('',#13434);
#479=PLANE('',#13439);
#480=PLANE('',#13444);
#481=PLANE('',#13448);
#482=PLANE('',#13453);
#483=PLANE('',#13458);
#484=PLANE('',#13463);
#485=PLANE('',#13467);
#486=PLANE('',#13472);
#487=PLANE('',#13477);
#488=PLANE('',#13482);
#489=PLANE('',#13486);
#490=PLANE('',#13491);
#491=PLANE('',#13496);
#492=PLANE('',#13501);
#493=PLANE('',#13506);
#494=PLANE('',#13510);
#495=PLANE('',#13514);
#496=PLANE('',#13518);
#497=PLANE('',#13522);
#498=PLANE('',#13526);
#499=PLANE('',#13530);
#500=PLANE('',#13534);
#501=PLANE('',#13538);
#502=PLANE('',#13542);
#503=PLANE('',#13546);
#504=PLANE('',#13550);
#505=PLANE('',#13554);
#506=PLANE('',#13558);
#507=PLANE('',#13562);
#508=PLANE('',#13566);
#509=PLANE('',#13570);
#510=PLANE('',#13574);
#511=PLANE('',#13578);
#512=PLANE('',#13582);
#513=PLANE('',#13680);
#514=PLANE('',#13730);
#515=PLANE('',#13734);
#516=PLANE('',#13822);
#517=PLANE('',#13826);
#518=PLANE('',#13827);
#519=PLANE('',#13839);
#520=PLANE('',#13842);
#521=PLANE('',#13849);
#522=PLANE('',#13850);
#523=PLANE('',#13859);
#524=PLANE('',#13875);
#525=PLANE('',#13880);
#526=PLANE('',#13884);
#527=PLANE('',#13888);
#528=PLANE('',#13892);
#529=PLANE('',#13899);
#530=PLANE('',#13903);
#531=PLANE('',#13907);
#532=PLANE('',#13923);
#533=PLANE('',#13929);
#534=PLANE('',#13934);
#535=PLANE('',#13937);
#536=PLANE('',#13938);
#537=PLANE('',#13940);
#538=PLANE('',#13941);
#539=PLANE('',#13946);
#540=PLANE('',#13947);
#541=PLANE('',#13949);
#542=PLANE('',#13951);
#543=PLANE('',#13954);
#544=PLANE('',#13955);
#545=PLANE('',#13957);
#546=PLANE('',#13959);
#547=PLANE('',#13962);
#548=PLANE('',#13966);
#549=PLANE('',#13969);
#550=PLANE('',#13970);
#551=PLANE('',#13988);
#552=PLANE('',#13992);
#553=PLANE('',#14023);
#554=PLANE('',#14024);
#555=PLANE('',#14039);
#556=PLANE('',#14040);
#557=PLANE('',#14052);
#558=PLANE('',#14053);
#559=PLANE('',#14079);
#560=PLANE('',#14080);
#561=PLANE('',#14114);
#562=PLANE('',#14129);
#563=PLANE('',#14130);
#564=PLANE('',#14206);
#565=PLANE('',#14207);
#566=PLANE('',#14214);
#567=PLANE('',#14215);
#568=PLANE('',#14222);
#569=PLANE('',#14223);
#570=PLANE('',#14230);
#571=PLANE('',#14231);
#572=PLANE('',#14238);
#573=PLANE('',#14239);
#574=PLANE('',#14246);
#575=PLANE('',#14247);
#576=PLANE('',#14254);
#577=PLANE('',#14255);
#578=PLANE('',#14262);
#579=PLANE('',#14263);
#580=PLANE('',#14270);
#581=PLANE('',#14271);
#582=PLANE('',#14278);
#583=PLANE('',#14279);
#584=PLANE('',#14286);
#585=PLANE('',#14287);
#586=PLANE('',#14311);
#587=PLANE('',#14312);
#588=PLANE('',#14316);
#589=PLANE('',#14317);
#590=PLANE('',#14321);
#591=PLANE('',#14322);
#592=PLANE('',#14326);
#593=PLANE('',#14327);
#594=PLANE('',#14331);
#595=PLANE('',#14332);
#596=PLANE('',#14336);
#597=PLANE('',#14337);
#598=PLANE('',#14341);
#599=PLANE('',#14342);
#600=PLANE('',#14346);
#601=PLANE('',#14347);
#602=PLANE('',#14351);
#603=PLANE('',#14352);
#604=PLANE('',#14356);
#605=PLANE('',#14357);
#606=PLANE('',#14361);
#607=PLANE('',#14362);
#608=PLANE('',#14366);
#609=PLANE('',#14367);
#610=B_SPLINE_SURFACE_WITH_KNOTS('',3,3,((#25169,#25170,#25171,#25172,#25173,
#25174,#25175,#25176,#25177,#25178,#25179,#25180,#25181,#25182,#25183,#25184,
#25185,#25186,#25187,#25188,#25189,#25190,#25191,#25192,#25193,#25194,#25195,
#25196,#25197,#25198,#25199,#25200,#25201,#25202,#25203,#25204,#25205,#25206,
#25207,#25208,#25209,#25210,#25211,#25212,#25213,#25214,#25215,#25216,#25217,
#25218,#25219,#25220,#25221,#25222,#25223,#25224,#25225,#25226,#25227,#25228,
#25229,#25230,#25231,#25232,#25233,#25234,#25235,#25236,#25237,#25238,#25239,
#25240,#25241,#25242,#25243,#25244,#25245,#25246,#25247,#25248,#25249,#25250,
#25251,#25252,#25253,#25254,#25255,#25256,#25257,#25258,#25259,#25260,#25261,
#25262,#25263,#25264,#25265,#25266,#25267,#25268,#25269,#25270,#25271,#25272,
#25273,#25274,#25275,#25276,#25277,#25278,#25279,#25280,#25281,#25282,#25283,
#25284,#25285,#25286,#25287,#25288,#25289,#25290,#25291,#25292,#25293,#25294,
#25295,#25296,#25297,#25298,#25299,#25300,#25301,#25302,#25303,#25304,#25305,
#25306,#25307,#25308,#25309,#25310,#25311,#25312,#25313,#25314,#25315,#25316,
#25317,#25318,#25319,#25320,#25321,#25322,#25323,#25324,#25325,#25326,#25327),
(#25328,#25329,#25330,#25331,#25332,#25333,#25334,#25335,#25336,#25337,
#25338,#25339,#25340,#25341,#25342,#25343,#25344,#25345,#25346,#25347,#25348,
#25349,#25350,#25351,#25352,#25353,#25354,#25355,#25356,#25357,#25358,#25359,
#25360,#25361,#25362,#25363,#25364,#25365,#25366,#25367,#25368,#25369,#25370,
#25371,#25372,#25373,#25374,#25375,#25376,#25377,#25378,#25379,#25380,#25381,
#25382,#25383,#25384,#25385,#25386,#25387,#25388,#25389,#25390,#25391,#25392,
#25393,#25394,#25395,#25396,#25397,#25398,#25399,#25400,#25401,#25402,#25403,
#25404,#25405,#25406,#25407,#25408,#25409,#25410,#25411,#25412,#25413,#25414,
#25415,#25416,#25417,#25418,#25419,#25420,#25421,#25422,#25423,#25424,#25425,
#25426,#25427,#25428,#25429,#25430,#25431,#25432,#25433,#25434,#25435,#25436,
#25437,#25438,#25439,#25440,#25441,#25442,#25443,#25444,#25445,#25446,#25447,
#25448,#25449,#25450,#25451,#25452,#25453,#25454,#25455,#25456,#25457,#25458,
#25459,#25460,#25461,#25462,#25463,#25464,#25465,#25466,#25467,#25468,#25469,
#25470,#25471,#25472,#25473,#25474,#25475,#25476,#25477,#25478,#25479,#25480,
#25481,#25482,#25483,#25484,#25485,#25486),(#25487,#25488,#25489,#25490,
#25491,#25492,#25493,#25494,#25495,#25496,#25497,#25498,#25499,#25500,#25501,
#25502,#25503,#25504,#25505,#25506,#25507,#25508,#25509,#25510,#25511,#25512,
#25513,#25514,#25515,#25516,#25517,#25518,#25519,#25520,#25521,#25522,#25523,
#25524,#25525,#25526,#25527,#25528,#25529,#25530,#25531,#25532,#25533,#25534,
#25535,#25536,#25537,#25538,#25539,#25540,#25541,#25542,#25543,#25544,#25545,
#25546,#25547,#25548,#25549,#25550,#25551,#25552,#25553,#25554,#25555,#25556,
#25557,#25558,#25559,#25560,#25561,#25562,#25563,#25564,#25565,#25566,#25567,
#25568,#25569,#25570,#25571,#25572,#25573,#25574,#25575,#25576,#25577,#25578,
#25579,#25580,#25581,#25582,#25583,#25584,#25585,#25586,#25587,#25588,#25589,
#25590,#25591,#25592,#25593,#25594,#25595,#25596,#25597,#25598,#25599,#25600,
#25601,#25602,#25603,#25604,#25605,#25606,#25607,#25608,#25609,#25610,#25611,
#25612,#25613,#25614,#25615,#25616,#25617,#25618,#25619,#25620,#25621,#25622,
#25623,#25624,#25625,#25626,#25627,#25628,#25629,#25630,#25631,#25632,#25633,
#25634,#25635,#25636,#25637,#25638,#25639,#25640,#25641,#25642,#25643,#25644,
#25645),(#25646,#25647,#25648,#25649,#25650,#25651,#25652,#25653,#25654,
#25655,#25656,#25657,#25658,#25659,#25660,#25661,#25662,#25663,#25664,#25665,
#25666,#25667,#25668,#25669,#25670,#25671,#25672,#25673,#25674,#25675,#25676,
#25677,#25678,#25679,#25680,#25681,#25682,#25683,#25684,#25685,#25686,#25687,
#25688,#25689,#25690,#25691,#25692,#25693,#25694,#25695,#25696,#25697,#25698,
#25699,#25700,#25701,#25702,#25703,#25704,#25705,#25706,#25707,#25708,#25709,
#25710,#25711,#25712,#25713,#25714,#25715,#25716,#25717,#25718,#25719,#25720,
#25721,#25722,#25723,#25724,#25725,#25726,#25727,#25728,#25729,#25730,#25731,
#25732,#25733,#25734,#25735,#25736,#25737,#25738,#25739,#25740,#25741,#25742,
#25743,#25744,#25745,#25746,#25747,#25748,#25749,#25750,#25751,#25752,#25753,
#25754,#25755,#25756,#25757,#25758,#25759,#25760,#25761,#25762,#25763,#25764,
#25765,#25766,#25767,#25768,#25769,#25770,#25771,#25772,#25773,#25774,#25775,
#25776,#25777,#25778,#25779,#25780,#25781,#25782,#25783,#25784,#25785,#25786,
#25787,#25788,#25789,#25790,#25791,#25792,#25793,#25794,#25795,#25796,#25797,
#25798,#25799,#25800,#25801,#25802,#25803,#25804)),.UNSPECIFIED.,.F.,.F.,
 .F.,(4,4),(4,1,1,1,1,1,1,1,1,1,1,1,1,1,1,1,1,1,1,1,1,1,1,1,1,1,1,1,1,1,
1,1,1,1,1,1,1,1,1,1,1,1,1,1,1,1,1,1,1,1,1,1,1,1,1,1,1,1,1,1,1,1,1,1,1,1,
1,1,1,1,1,1,1,1,1,1,1,1,1,1,1,1,1,1,1,1,1,1,1,1,1,1,1,1,1,1,1,1,1,1,1,1,
1,1,1,1,1,1,1,1,1,1,1,1,1,1,1,1,1,1,1,1,1,1,1,1,1,1,1,1,1,1,1,1,1,1,1,1,
1,1,1,1,1,1,1,1,1,1,1,1,1,1,1,1,1,1,4),(-8.30696747198589E-5,0.128693006748574),
(11.8548247440635,12.351182148212,12.8474564826858,13.3437308171596,13.8400051516334,
14.3362794861072,14.832553820581,15.3288281550548,15.8251024895286,16.3213768240024,
16.8176511584762,17.31392549295,17.8101998274238,18.3064741618976,18.8027484963714,
19.2990228308452,19.7952971653189,20.2915714997927,20.7878458342665,21.2841201687403,
21.7803945032141,22.2766688376879,22.7729431721617,23.2692175066355,23.7654918411093,
24.2617661755831,24.7580405100569,25.2543148445307,25.7505891790045,26.2468635134783,
26.7431378479521,27.2394121824259,27.7356865168997,28.2319608513735,28.7282351858473,
29.224509520321,29.7207838547948,30.2170581892686,30.7133325237424,31.2096068582162,
31.70588119269,32.2021555271638,32.6984298616376,33.1947041961114,33.6909785305852,
34.187252865059,34.6835271995328,35.1798015340066,35.6760758684804,36.1723502029542,
36.668624537428,37.1648988719018,37.6611732063756,38.1574475408493,38.6537218753231,
39.1499962097969,39.6462705442707,40.1425448787445,40.6388192132183,41.1350935476921,
41.6313678821659,42.1276422166397,42.6239165511135,43.1201908855873,43.6164652200611,
44.1127395545349,44.6090138890087,45.1052882234825,45.6015625579563,46.0978368924301,
46.5941112269039,47.0903855613777,47.5866598958514,48.0829342303252,48.579208564799,
49.0754828992728,49.5717572337466,50.0680315682204,50.5643059026942,51.060580237168,
51.5568545716418,52.0531289061156,52.5494032405894,53.0456775750632,53.541951909537,
54.0382262440108,54.5345005784846,55.0307749129584,55.5270492474322,56.023323581906,
56.5195979163798,57.0158722508535,57.5121465853273,58.0084209198011,58.5046952542749,
59.0009695887487,59.4972439232225,59.9935182576963,60.4897925921701,60.9860669266439,
61.4823412611177,61.9786155955915,62.4748899300653,62.9711642645391,63.4674385990129,
63.9637129334867,64.4599872679605,64.9562616024343,65.452535936908,65.9488102713818,
66.4450846058556,66.9413589403294,67.4376332748032,67.933907609277,68.4301819437508,
68.9264562782246,69.4227306126984,69.9190049471722,70.415279281646,70.9115536161198,
71.4078279505936,71.9041022850674,72.4003766195412,72.896650954015,73.3929252884888,
73.8891996229626,74.3854739574363,74.8817482919101,75.3780226263839,75.8742969608577,
76.3705712953315,76.8668456298053,77.3631199642791,77.8593942987529,78.3556686332267,
78.8519429677005,79.3482173021743,79.8444916366481,80.3407659711219,80.8370403055957,
81.3333146400695,81.8295889745433,82.3258633090171,82.8221376434909,83.3184119779647,
83.8146863124385,84.3109606469122,84.807234981386,85.3035093158598,85.7997836503336,
86.2960579848074,86.7923323192812,87.288606653755,87.7848809882288,88.2811553227026,
88.7774296571764,89.2737039916502),.UNSPECIFIED.);
#611=B_SPLINE_SURFACE_WITH_KNOTS('',3,3,((#26032,#26033,#26034,#26035,#26036,
#26037,#26038,#26039,#26040,#26041,#26042,#26043,#26044,#26045,#26046,#26047,
#26048,#26049,#26050,#26051,#26052,#26053,#26054,#26055,#26056,#26057,#26058,
#26059,#26060,#26061,#26062,#26063,#26064,#26065,#26066,#26067,#26068,#26069,
#26070,#26071,#26072,#26073,#26074,#26075,#26076,#26077,#26078,#26079,#26080,
#26081,#26082,#26083,#26084,#26085,#26086,#26087,#26088,#26089,#26090,#26091,
#26092,#26093,#26094,#26095,#26096,#26097,#26098,#26099,#26100,#26101,#26102,
#26103,#26104,#26105,#26106,#26107,#26108,#26109,#26110,#26111,#26112,#26113,
#26114,#26115,#26116,#26117,#26118,#26119,#26120,#26121,#26122,#26123,#26124,
#26125,#26126,#26127,#26128,#26129,#26130,#26131,#26132,#26133,#26134,#26135,
#26136,#26137,#26138,#26139,#26140,#26141,#26142,#26143,#26144,#26145,#26146,
#26147,#26148,#26149,#26150,#26151,#26152,#26153,#26154,#26155,#26156,#26157,
#26158,#26159,#26160,#26161,#26162,#26163,#26164,#26165,#26166,#26167,#26168,
#26169,#26170,#26171,#26172,#26173,#26174,#26175,#26176,#26177,#26178,#26179,
#26180,#26181,#26182,#26183,#26184,#26185,#26186,#26187,#26188,#26189,#26190),
(#26191,#26192,#26193,#26194,#26195,#26196,#26197,#26198,#26199,#26200,
#26201,#26202,#26203,#26204,#26205,#26206,#26207,#26208,#26209,#26210,#26211,
#26212,#26213,#26214,#26215,#26216,#26217,#26218,#26219,#26220,#26221,#26222,
#26223,#26224,#26225,#26226,#26227,#26228,#26229,#26230,#26231,#26232,#26233,
#26234,#26235,#26236,#26237,#26238,#26239,#26240,#26241,#26242,#26243,#26244,
#26245,#26246,#26247,#26248,#26249,#26250,#26251,#26252,#26253,#26254,#26255,
#26256,#26257,#26258,#26259,#26260,#26261,#26262,#26263,#26264,#26265,#26266,
#26267,#26268,#26269,#26270,#26271,#26272,#26273,#26274,#26275,#26276,#26277,
#26278,#26279,#26280,#26281,#26282,#26283,#26284,#26285,#26286,#26287,#26288,
#26289,#26290,#26291,#26292,#26293,#26294,#26295,#26296,#26297,#26298,#26299,
#26300,#26301,#26302,#26303,#26304,#26305,#26306,#26307,#26308,#26309,#26310,
#26311,#26312,#26313,#26314,#26315,#26316,#26317,#26318,#26319,#26320,#26321,
#26322,#26323,#26324,#26325,#26326,#26327,#26328,#26329,#26330,#26331,#26332,
#26333,#26334,#26335,#26336,#26337,#26338,#26339,#26340,#26341,#26342,#26343,
#26344,#26345,#26346,#26347,#26348,#26349),(#26350,#26351,#26352,#26353,
#26354,#26355,#26356,#26357,#26358,#26359,#26360,#26361,#26362,#26363,#26364,
#26365,#26366,#26367,#26368,#26369,#26370,#26371,#26372,#26373,#26374,#26375,
#26376,#26377,#26378,#26379,#26380,#26381,#26382,#26383,#26384,#26385,#26386,
#26387,#26388,#26389,#26390,#26391,#26392,#26393,#26394,#26395,#26396,#26397,
#26398,#26399,#26400,#26401,#26402,#26403,#26404,#26405,#26406,#26407,#26408,
#26409,#26410,#26411,#26412,#26413,#26414,#26415,#26416,#26417,#26418,#26419,
#26420,#26421,#26422,#26423,#26424,#26425,#26426,#26427,#26428,#26429,#26430,
#26431,#26432,#26433,#26434,#26435,#26436,#26437,#26438,#26439,#26440,#26441,
#26442,#26443,#26444,#26445,#26446,#26447,#26448,#26449,#26450,#26451,#26452,
#26453,#26454,#26455,#26456,#26457,#26458,#26459,#26460,#26461,#26462,#26463,
#26464,#26465,#26466,#26467,#26468,#26469,#26470,#26471,#26472,#26473,#26474,
#26475,#26476,#26477,#26478,#26479,#26480,#26481,#26482,#26483,#26484,#26485,
#26486,#26487,#26488,#26489,#26490,#26491,#26492,#26493,#26494,#26495,#26496,
#26497,#26498,#26499,#26500,#26501,#26502,#26503,#26504,#26505,#26506,#26507,
#26508),(#26509,#26510,#26511,#26512,#26513,#26514,#26515,#26516,#26517,
#26518,#26519,#26520,#26521,#26522,#26523,#26524,#26525,#26526,#26527,#26528,
#26529,#26530,#26531,#26532,#26533,#26534,#26535,#26536,#26537,#26538,#26539,
#26540,#26541,#26542,#26543,#26544,#26545,#26546,#26547,#26548,#26549,#26550,
#26551,#26552,#26553,#26554,#26555,#26556,#26557,#26558,#26559,#26560,#26561,
#26562,#26563,#26564,#26565,#26566,#26567,#26568,#26569,#26570,#26571,#26572,
#26573,#26574,#26575,#26576,#26577,#26578,#26579,#26580,#26581,#26582,#26583,
#26584,#26585,#26586,#26587,#26588,#26589,#26590,#26591,#26592,#26593,#26594,
#26595,#26596,#26597,#26598,#26599,#26600,#26601,#26602,#26603,#26604,#26605,
#26606,#26607,#26608,#26609,#26610,#26611,#26612,#26613,#26614,#26615,#26616,
#26617,#26618,#26619,#26620,#26621,#26622,#26623,#26624,#26625,#26626,#26627,
#26628,#26629,#26630,#26631,#26632,#26633,#26634,#26635,#26636,#26637,#26638,
#26639,#26640,#26641,#26642,#26643,#26644,#26645,#26646,#26647,#26648,#26649,
#26650,#26651,#26652,#26653,#26654,#26655,#26656,#26657,#26658,#26659,#26660,
#26661,#26662,#26663,#26664,#26665,#26666,#26667)),.UNSPECIFIED.,.F.,.F.,
 .F.,(4,4),(4,1,1,1,1,1,1,1,1,1,1,1,1,1,1,1,1,1,1,1,1,1,1,1,1,1,1,1,1,1,
1,1,1,1,1,1,1,1,1,1,1,1,1,1,1,1,1,1,1,1,1,1,1,1,1,1,1,1,1,1,1,1,1,1,1,1,
1,1,1,1,1,1,1,1,1,1,1,1,1,1,1,1,1,1,1,1,1,1,1,1,1,1,1,1,1,1,1,1,1,1,1,1,
1,1,1,1,1,1,1,1,1,1,1,1,1,1,1,1,1,1,1,1,1,1,1,1,1,1,1,1,1,1,1,1,1,1,1,1,
1,1,1,1,1,1,1,1,1,1,1,1,1,1,1,1,1,1,4),(-5.91850316919151E-5,0.128716709650167),
(14.3988535768129,14.8951279112866,15.3914022457604,15.8876765802342,16.383950914708,
16.8802252491818,17.3764995836556,17.8727739181294,18.3690482526032,18.865322587077,
19.3615969215508,19.8578712560246,20.3541455904984,20.8504199249722,21.346694259446,
21.8429685939198,22.3392429283936,22.8355172628674,23.3317915973412,23.828065931815,
24.3243402662887,24.8206146007625,25.3168889352363,25.8131632697101,26.3094376041839,
26.8057119386577,27.3019862731315,27.7982606076053,28.2945349420791,28.7908092765529,
29.2870836110267,29.7833579455005,30.2796322799743,30.7759066144481,31.2721809489219,
31.7684552833957,32.2647296178695,32.7610039523433,33.2572782868171,33.7535526212909,
34.2498269557646,34.7461012902384,35.2423756247122,35.738649959186,36.2349242936598,
36.7311986281336,37.2274729626074,37.7237472970812,38.220021631555,38.7162959660288,
39.2125703005026,39.7088446349764,40.2051189694502,40.701393303924,41.1976676383978,
41.6939419728716,42.1902163073454,42.6864906418191,43.1827649762929,43.6790393107667,
44.1753136452405,44.6715879797143,45.1678623141881,45.6641366486619,46.1604109831357,
46.6566853176095,47.1529596520833,47.6492339865571,48.1455083210309,48.6417826555047,
49.1380569899785,49.6343313244523,50.1306056589261,50.6268799933999,51.1231543278737,
51.6194286623475,52.1157029968213,52.6119773312951,53.1082516657688,53.6045260002426,
54.1008003347164,54.5970746691902,55.093349003664,55.5896233381378,56.0858976726116,
56.5821720070854,57.0784463415592,57.574720676033,58.0709950105068,58.5672693449806,
59.0635436794544,59.5598180139282,60.056092348402,60.5523666828758,61.0486410173496,
61.5449153518233,62.0411896862971,62.5374640207709,63.0337383552447,63.5300126897185,
64.0262870241923,64.5225613586661,65.0188356931399,65.5151100276137,66.0113843620875,
66.5076586965613,67.0039330310351,67.5002073655089,67.9964816999827,68.4927560344565,
68.9890303689303,69.4853047034041,69.9815790378779,70.4778533723517,70.9741277068254,
71.4704020412992,71.966676375773,72.4629507102468,72.9592250447206,73.4554993791944,
73.9517737136682,74.448048048142,74.9443223826158,75.4405967170896,75.9368710515634,
76.4331453860372,76.929419720511,77.4256940549848,77.9219683894586,78.4182427239324,
78.9145170584062,79.41079139288,79.9070657273538,80.4033400618275,80.8996143963013,
81.3958887307751,81.8921630652489,82.3884373997227,82.8847117341965,83.3809860686703,
83.8772604031441,84.3735347376179,84.8698090720917,85.3660834065655,85.8623577410393,
86.3586320755131,86.8549064099869,87.3511807444607,87.8474550789345,88.3437294134083,
88.8400037478821,89.3362780823559,89.8325524168297,90.3288267513034,90.8251010857772,
91.321375420251,91.8177328243995),.UNSPECIFIED.);
#612=B_SPLINE_SURFACE_WITH_KNOTS('',3,3,((#29359,#29360,#29361,#29362),
(#29363,#29364,#29365,#29366),(#29367,#29368,#29369,#29370),(#29371,#29372,
#29373,#29374)),.UNSPECIFIED.,.F.,.F.,.F.,(4,4),(4,4),(-1.00000000738492,
6.33181493099193E-12),(-0.228566601102733,0.828566601102733),
 .UNSPECIFIED.);
#613=B_SPLINE_SURFACE_WITH_KNOTS('',3,3,((#29383,#29384,#29385,#29386),
(#29387,#29388,#29389,#29390),(#29391,#29392,#29393,#29394),(#29395,#29396,
#29397,#29398)),.UNSPECIFIED.,.F.,.F.,.F.,(4,4),(4,4),(-1.00000000738848,
7.85174896767267E-12),(-0.228566601102733,0.828566601102734),
 .UNSPECIFIED.);
#614=B_SPLINE_SURFACE_WITH_KNOTS('',3,3,((#29407,#29408,#29409,#29410),
(#29411,#29412,#29413,#29414),(#29415,#29416,#29417,#29418),(#29419,#29420,
#29421,#29422)),.UNSPECIFIED.,.F.,.F.,.F.,(4,4),(4,4),(-1.00000000739146,
1.55845144401953E-11),(-0.228566601102734,0.828566601102734),
 .UNSPECIFIED.);
#615=B_SPLINE_SURFACE_WITH_KNOTS('',3,3,((#29431,#29432,#29433,#29434),
(#29435,#29436,#29437,#29438),(#29439,#29440,#29441,#29442),(#29443,#29444,
#29445,#29446)),.UNSPECIFIED.,.F.,.F.,.F.,(4,4),(4,4),(-1.00000000737499,
1.10248632487242E-11),(-0.228566601102733,0.828566601102734),
 .UNSPECIFIED.);
#616=B_SPLINE_SURFACE_WITH_KNOTS('',3,3,((#29455,#29456,#29457,#29458),
(#29459,#29460,#29461,#29462),(#29463,#29464,#29465,#29466),(#29467,#29468,
#29469,#29470)),.UNSPECIFIED.,.F.,.F.,.F.,(4,4),(4,4),(-1.00000000737555,
8.62684039186831E-12),(-0.228566601102733,0.828566601102733),
 .UNSPECIFIED.);
#617=B_SPLINE_SURFACE_WITH_KNOTS('',3,3,((#29479,#29480,#29481,#29482),
(#29483,#29484,#29485,#29486),(#29487,#29488,#29489,#29490),(#29491,#29492,
#29493,#29494)),.UNSPECIFIED.,.F.,.F.,.F.,(4,4),(4,4),(-1.00000000738693,
5.72012097454778E-12),(-0.228566601102733,0.828566601102734),
 .UNSPECIFIED.);
#618=B_SPLINE_SURFACE_WITH_KNOTS('',3,3,((#29503,#29504,#29505,#29506),
(#29507,#29508,#29509,#29510),(#29511,#29512,#29513,#29514),(#29515,#29516,
#29517,#29518)),.UNSPECIFIED.,.F.,.F.,.F.,(4,4),(4,4),(-1.00000000738919,
5.62379169111571E-12),(-0.228566601102733,0.828566601102734),
 .UNSPECIFIED.);
#619=B_SPLINE_SURFACE_WITH_KNOTS('',3,3,((#29527,#29528,#29529,#29530),
(#29531,#29532,#29533,#29534),(#29535,#29536,#29537,#29538),(#29539,#29540,
#29541,#29542)),.UNSPECIFIED.,.F.,.F.,.F.,(4,4),(4,4),(-1.00000000739289,
6.50467340161261E-12),(-0.228566601102733,0.828566601102733),
 .UNSPECIFIED.);
#620=B_SPLINE_SURFACE_WITH_KNOTS('',3,3,((#29551,#29552,#29553,#29554),
(#29555,#29556,#29557,#29558),(#29559,#29560,#29561,#29562),(#29563,#29564,
#29565,#29566)),.UNSPECIFIED.,.F.,.F.,.F.,(4,4),(4,4),(-1.00000000739148,
1.40793838710229E-11),(-0.228566601102733,0.828566601102734),
 .UNSPECIFIED.);
#621=B_SPLINE_SURFACE_WITH_KNOTS('',3,3,((#29575,#29576,#29577,#29578),
(#29579,#29580,#29581,#29582),(#29583,#29584,#29585,#29586),(#29587,#29588,
#29589,#29590)),.UNSPECIFIED.,.F.,.F.,.F.,(4,4),(4,4),(-1.00000000738262,
1.82838412051694E-11),(-0.228566601102733,0.828566601102734),
 .UNSPECIFIED.);
#622=B_SPLINE_SURFACE_WITH_KNOTS('',3,3,((#29599,#29600,#29601,#29602),
(#29603,#29604,#29605,#29606),(#29607,#29608,#29609,#29610),(#29611,#29612,
#29613,#29614)),.UNSPECIFIED.,.F.,.F.,.F.,(4,4),(4,4),(-1.00000000737784,
1.02973089179534E-11),(-0.228566601102733,0.828566601102734),
 .UNSPECIFIED.);
#623=B_SPLINE_SURFACE_WITH_KNOTS('',3,3,((#29623,#29624,#29625,#29626),
(#29627,#29628,#29629,#29630),(#29631,#29632,#29633,#29634),(#29635,#29636,
#29637,#29638)),.UNSPECIFIED.,.F.,.F.,.F.,(4,4),(4,4),(-1.00000000738658,
8.03237988227756E-12),(-0.228566601102733,0.828566601102733),
 .UNSPECIFIED.);
#624=B_SPLINE_SURFACE_WITH_KNOTS('',3,3,((#29647,#29648,#29649,#29650),
(#29651,#29652,#29653,#29654),(#29655,#29656,#29657,#29658),(#29659,#29660,
#29661,#29662)),.UNSPECIFIED.,.F.,.F.,.F.,(4,4),(4,4),(-1.00000000738646,
1.53840942326398E-11),(-0.228566601102734,0.828566601102734),
 .UNSPECIFIED.);
#625=B_SPLINE_SURFACE_WITH_KNOTS('',3,3,((#29671,#29672,#29673,#29674),
(#29675,#29676,#29677,#29678),(#29679,#29680,#29681,#29682),(#29683,#29684,
#29685,#29686)),.UNSPECIFIED.,.F.,.F.,.F.,(4,4),(4,4),(-1.00000000737555,
1.43664760969259E-11),(-0.228566601102733,0.828566601102734),
 .UNSPECIFIED.);
#626=B_SPLINE_SURFACE_WITH_KNOTS('',3,3,((#29695,#29696,#29697,#29698),
(#29699,#29700,#29701,#29702),(#29703,#29704,#29705,#29706),(#29707,#29708,
#29709,#29710)),.UNSPECIFIED.,.F.,.F.,.F.,(4,4),(4,4),(-1.00000000738601,
1.73046711715086E-14),(-0.228566601102733,0.828566601102733),
 .UNSPECIFIED.);
#627=B_SPLINE_SURFACE_WITH_KNOTS('',3,3,((#29719,#29720,#29721,#29722),
(#29723,#29724,#29725,#29726),(#29727,#29728,#29729,#29730),(#29731,#29732,
#29733,#29734)),.UNSPECIFIED.,.F.,.F.,.F.,(4,4),(4,4),(-1.00000000738919,
1.07500378715111E-11),(-0.228566601102733,0.828566601102734),
 .UNSPECIFIED.);
#628=B_SPLINE_SURFACE_WITH_KNOTS('',3,3,((#29743,#29744,#29745,#29746),
(#29747,#29748,#29749,#29750),(#29751,#29752,#29753,#29754),(#29755,#29756,
#29757,#29758)),.UNSPECIFIED.,.F.,.F.,.F.,(4,4),(4,4),(-1.00000000739238,
1.18069447204771E-11),(-0.228566601102733,0.828566601102734),
 .UNSPECIFIED.);
#629=B_SPLINE_SURFACE_WITH_KNOTS('',3,3,((#29767,#29768,#29769,#29770),
(#29771,#29772,#29773,#29774),(#29775,#29776,#29777,#29778),(#29779,#29780,
#29781,#29782)),.UNSPECIFIED.,.F.,.F.,.F.,(4,4),(4,4),(-1.00000000739217,
1.4414592214071E-11),(-0.228566601102733,0.828566601102734),
 .UNSPECIFIED.);
#630=B_SPLINE_SURFACE_WITH_KNOTS('',3,3,((#29791,#29792,#29793,#29794),
(#29795,#29796,#29797,#29798),(#29799,#29800,#29801,#29802),(#29803,#29804,
#29805,#29806),(#29807,#29808,#29809,#29810),(#29811,#29812,#29813,#29814),
(#29815,#29816,#29817,#29818)),.UNSPECIFIED.,.F.,.F.,.F.,(4,1,1,1,4),(4,
4),(-5.05014469441185E-14,0.1428571428571,0.28571428571425,0.571428571428551,
1.00000036560903),(-0.228509057368286,0.828509057368286),.UNSPECIFIED.);
#631=B_SPLINE_SURFACE_WITH_KNOTS('',3,3,((#29825,#29826,#29827,#29828),
(#29829,#29830,#29831,#29832),(#29833,#29834,#29835,#29836),(#29837,#29838,
#29839,#29840),(#29841,#29842,#29843,#29844),(#29845,#29846,#29847,#29848)),
 .UNSPECIFIED.,.F.,.F.,.F.,(4,1,1,4),(4,4),(-1.00000000000001,-0.42857142857138,
-0.214285714285645,9.03251141877686E-14),(-0.228509057368286,0.828509057368286),
 .UNSPECIFIED.);
#632=B_SPLINE_SURFACE_WITH_KNOTS('',3,3,((#29851,#29852,#29853,#29854),
(#29855,#29856,#29857,#29858),(#29859,#29860,#29861,#29862),(#29863,#29864,
#29865,#29866)),.UNSPECIFIED.,.F.,.F.,.F.,(4,4),(4,4),(-1.25904053593043E-16,
0.0850880881510745),(-0.100000001340248,0.1),.UNSPECIFIED.);
#633=B_SPLINE_SURFACE_WITH_KNOTS('',3,3,((#29867,#29868,#29869,#29870),
(#29871,#29872,#29873,#29874),(#29875,#29876,#29877,#29878),(#29879,#29880,
#29881,#29882)),.UNSPECIFIED.,.F.,.F.,.F.,(4,4),(4,4),(-1.25904053593043E-16,
0.0850880881510745),(0.5,0.700000001340097),.UNSPECIFIED.);
#634=B_SPLINE_SURFACE_WITH_KNOTS('',3,3,((#29883,#29884,#29885,#29886),
(#29887,#29888,#29889,#29890),(#29891,#29892,#29893,#29894),(#29895,#29896,
#29897,#29898),(#29899,#29900,#29901,#29902),(#29903,#29904,#29905,#29906)),
 .UNSPECIFIED.,.F.,.F.,.F.,(4,1,1,4),(4,4),(-5.14134515353765E-14,0.214285714285675,
0.4285714285714,1.),(-0.228509057368286,0.828509057368286),
 .UNSPECIFIED.);
#635=B_SPLINE_SURFACE_WITH_KNOTS('',3,3,((#29913,#29914,#29915,#29916),
(#29917,#29918,#29919,#29920),(#29921,#29922,#29923,#29924),(#29925,#29926,
#29927,#29928),(#29929,#29930,#29931,#29932),(#29933,#29934,#29935,#29936)),
 .UNSPECIFIED.,.F.,.F.,.F.,(4,1,1,4),(4,4),(-1.00000000000001,-0.428571428571412,
-0.214285714285689,3.45222547669068E-14),(-0.228509057368286,0.828509057368286),
 .UNSPECIFIED.);
#636=B_SPLINE_SURFACE_WITH_KNOTS('',3,3,((#29939,#29940,#29941,#29942),
(#29943,#29944,#29945,#29946),(#29947,#29948,#29949,#29950),(#29951,#29952,
#29953,#29954)),.UNSPECIFIED.,.F.,.F.,.F.,(4,4),(4,4),(-6.55275566865934E-17,
0.0850880881510748),(-0.100000001340248,0.1),.UNSPECIFIED.);
#637=B_SPLINE_SURFACE_WITH_KNOTS('',3,3,((#29955,#29956,#29957,#29958),
(#29959,#29960,#29961,#29962),(#29963,#29964,#29965,#29966),(#29967,#29968,
#29969,#29970)),.UNSPECIFIED.,.F.,.F.,.F.,(4,4),(4,4),(-6.55275566865934E-17,
0.0850880881510748),(0.5,0.700000001340096),.UNSPECIFIED.);
#638=B_SPLINE_SURFACE_WITH_KNOTS('',3,3,((#29971,#29972,#29973,#29974),
(#29975,#29976,#29977,#29978),(#29979,#29980,#29981,#29982),(#29983,#29984,
#29985,#29986),(#29987,#29988,#29989,#29990),(#29991,#29992,#29993,#29994),
(#29995,#29996,#29997,#29998)),.UNSPECIFIED.,.F.,.F.,.F.,(4,1,1,1,4),(4,
4),(-1.49004572061584E-13,0.142857142857015,0.28571428571418,0.571428571428509,
1.),(-0.228509057368286,0.828509057368286),.UNSPECIFIED.);
#639=B_SPLINE_SURFACE_WITH_KNOTS('',3,3,((#30005,#30006,#30007,#30008),
(#30009,#30010,#30011,#30012),(#30013,#30014,#30015,#30016),(#30017,#30018,
#30019,#30020),(#30021,#30022,#30023,#30024),(#30025,#30026,#30027,#30028),
(#30029,#30030,#30031,#30032)),.UNSPECIFIED.,.F.,.F.,.F.,(4,1,1,1,4),(4,
4),(-1.00000000194169,-0.571428572538049,-0.285714286268955,-0.142857143134408,
1.38482423202144E-13),(-0.228509057368286,0.828509057368287),
 .UNSPECIFIED.);
#640=B_SPLINE_SURFACE_WITH_KNOTS('',3,3,((#30035,#30036,#30037,#30038),
(#30039,#30040,#30041,#30042),(#30043,#30044,#30045,#30046),(#30047,#30048,
#30049,#30050)),.UNSPECIFIED.,.F.,.F.,.F.,(4,4),(4,4),(-8.47096787732307E-17,
0.0850880881510746),(-0.100000001340248,0.1),.UNSPECIFIED.);
#641=B_SPLINE_SURFACE_WITH_KNOTS('',3,3,((#30051,#30052,#30053,#30054),
(#30055,#30056,#30057,#30058),(#30059,#30060,#30061,#30062),(#30063,#30064,
#30065,#30066)),.UNSPECIFIED.,.F.,.F.,.F.,(4,4),(4,4),(-8.47096787732307E-17,
0.0850880881510746),(0.5,0.700000001340097),.UNSPECIFIED.);
#642=B_SPLINE_SURFACE_WITH_KNOTS('',3,3,((#30067,#30068,#30069,#30070),
(#30071,#30072,#30073,#30074),(#30075,#30076,#30077,#30078),(#30079,#30080,
#30081,#30082),(#30083,#30084,#30085,#30086),(#30087,#30088,#30089,#30090)),
 .UNSPECIFIED.,.F.,.F.,.F.,(4,1,1,4),(4,4),(-5.51374837743005E-14,0.214285714285672,
0.428571428571398,1.),(-0.228509057368286,0.828509057368286),
 .UNSPECIFIED.);
#643=B_SPLINE_SURFACE_WITH_KNOTS('',3,3,((#30097,#30098,#30099,#30100),
(#30101,#30102,#30103,#30104),(#30105,#30106,#30107,#30108),(#30109,#30110,
#30111,#30112),(#30113,#30114,#30115,#30116),(#30117,#30118,#30119,#30120),
(#30121,#30122,#30123,#30124)),.UNSPECIFIED.,.F.,.F.,.F.,(4,1,1,1,4),(4,
4),(-1.00000000194169,-0.571428572538072,-0.285714286268993,-0.142857143134453,
8.6647533219349E-14),(-0.228509057368286,0.828509057368286),
 .UNSPECIFIED.);
#644=B_SPLINE_SURFACE_WITH_KNOTS('',3,3,((#30127,#30128,#30129,#30130),
(#30131,#30132,#30133,#30134),(#30135,#30136,#30137,#30138),(#30139,#30140,
#30141,#30142)),.UNSPECIFIED.,.F.,.F.,.F.,(4,4),(4,4),(-7.29201002821673E-17,
0.0850880881510746),(-0.100000001340248,0.1),.UNSPECIFIED.);
#645=B_SPLINE_SURFACE_WITH_KNOTS('',3,3,((#30143,#30144,#30145,#30146),
(#30147,#30148,#30149,#30150),(#30151,#30152,#30153,#30154),(#30155,#30156,
#30157,#30158)),.UNSPECIFIED.,.F.,.F.,.F.,(4,4),(4,4),(-7.29201002821673E-17,
0.0850880881510746),(0.5,0.700000001340097),.UNSPECIFIED.);
#646=B_SPLINE_SURFACE_WITH_KNOTS('',3,3,((#30159,#30160,#30161,#30162),
(#30163,#30164,#30165,#30166),(#30167,#30168,#30169,#30170),(#30171,#30172,
#30173,#30174),(#30175,#30176,#30177,#30178),(#30179,#30180,#30181,#30182)),
 .UNSPECIFIED.,.F.,.F.,.F.,(4,1,1,4),(4,4),(-8.88579894424611E-14,0.214285714285645,
0.428571428571379,1.00000036560548),(-0.228509057368286,0.828509057368286),
 .UNSPECIFIED.);
#647=B_SPLINE_SURFACE_WITH_KNOTS('',3,3,((#30189,#30190,#30191,#30192),
(#30193,#30194,#30195,#30196),(#30197,#30198,#30199,#30200),(#30201,#30202,
#30203,#30204),(#30205,#30206,#30207,#30208),(#30209,#30210,#30211,#30212),
(#30213,#30214,#30215,#30216)),.UNSPECIFIED.,.F.,.F.,.F.,(4,1,1,1,4),(4,
4),(-1.00000000194169,-0.571428572538067,-0.285714286268987,-0.142857143134447,
9.29481593602791E-14),(-0.228509057368286,0.828509057368287),
 .UNSPECIFIED.);
#648=B_SPLINE_SURFACE_WITH_KNOTS('',3,3,((#30219,#30220,#30221,#30222),
(#30223,#30224,#30225,#30226),(#30227,#30228,#30229,#30230),(#30231,#30232,
#30233,#30234)),.UNSPECIFIED.,.F.,.F.,.F.,(4,4),(4,4),(-4.15613902556478E-17,
0.0850880881510746),(-0.100000001340247,0.1),.UNSPECIFIED.);
#649=B_SPLINE_SURFACE_WITH_KNOTS('',3,3,((#30235,#30236,#30237,#30238),
(#30239,#30240,#30241,#30242),(#30243,#30244,#30245,#30246),(#30247,#30248,
#30249,#30250)),.UNSPECIFIED.,.F.,.F.,.F.,(4,4),(4,4),(-4.15613902556478E-17,
0.0850880881510746),(0.5,0.700000001340097),.UNSPECIFIED.);
#650=B_SPLINE_SURFACE_WITH_KNOTS('',3,3,((#30251,#30252,#30253,#30254),
(#30255,#30256,#30257,#30258),(#30259,#30260,#30261,#30262),(#30263,#30264,
#30265,#30266),(#30267,#30268,#30269,#30270),(#30271,#30272,#30273,#30274),
(#30275,#30276,#30277,#30278)),.UNSPECIFIED.,.F.,.F.,.F.,(4,1,1,1,4),(4,
4),(-1.61169275568063E-13,0.142857142857005,0.285714285714171,0.571428571428504,
1.00000036560902),(-0.228509057368287,0.828509057368287),.UNSPECIFIED.);
#651=B_SPLINE_SURFACE_WITH_KNOTS('',3,3,((#30285,#30286,#30287,#30288),
(#30289,#30290,#30291,#30292),(#30293,#30294,#30295,#30296),(#30297,#30298,
#30299,#30300),(#30301,#30302,#30303,#30304),(#30305,#30306,#30307,#30308),
(#30309,#30310,#30311,#30312)),.UNSPECIFIED.,.F.,.F.,.F.,(4,1,1,1,4),(4,
4),(-1.00000000194169,-0.571428572538077,-0.285714286269001,-0.142857143134464,
7.42392258779034E-14),(-0.228509057368286,0.828509057368287),
 .UNSPECIFIED.);
#652=B_SPLINE_SURFACE_WITH_KNOTS('',3,3,((#30315,#30316,#30317,#30318),
(#30319,#30320,#30321,#30322),(#30323,#30324,#30325,#30326),(#30327,#30328,
#30329,#30330)),.UNSPECIFIED.,.F.,.F.,.F.,(4,4),(4,4),(-2.07473905953491E-17,
0.0850880881510745),(-0.100000001340248,0.1),.UNSPECIFIED.);
#653=B_SPLINE_SURFACE_WITH_KNOTS('',3,3,((#30331,#30332,#30333,#30334),
(#30335,#30336,#30337,#30338),(#30339,#30340,#30341,#30342),(#30343,#30344,
#30345,#30346)),.UNSPECIFIED.,.F.,.F.,.F.,(4,4),(4,4),(-2.07473905953491E-17,
0.0850880881510745),(0.5,0.700000001340097),.UNSPECIFIED.);
#654=B_SPLINE_SURFACE_WITH_KNOTS('',3,3,((#30347,#30348,#30349,#30350),
(#30351,#30352,#30353,#30354),(#30355,#30356,#30357,#30358),(#30359,#30360,
#30361,#30362),(#30363,#30364,#30365,#30366),(#30367,#30368,#30369,#30370)),
 .UNSPECIFIED.,.F.,.F.,.F.,(4,1,1,4),(4,4),(-5.7507029460608E-14,0.214285714285669,
0.428571428571396,1.),(-0.228509057368286,0.828509057368286),
 .UNSPECIFIED.);
#655=B_SPLINE_SURFACE_WITH_KNOTS('',3,3,((#30377,#30378,#30379,#30380),
(#30381,#30382,#30383,#30384),(#30385,#30386,#30387,#30388),(#30389,#30390,
#30391,#30392),(#30393,#30394,#30395,#30396),(#30397,#30398,#30399,#30400),
(#30401,#30402,#30403,#30404)),.UNSPECIFIED.,.F.,.F.,.F.,(4,1,1,1,4),(4,
4),(-1.00000036560901,-0.571428571428521,-0.285714285714198,-0.142857142857037,
1.24679780388881E-13),(-0.228509057368286,0.828509057368287),
 .UNSPECIFIED.);
#656=B_SPLINE_SURFACE_WITH_KNOTS('',3,3,((#30407,#30408,#30409,#30410),
(#30411,#30412,#30413,#30414),(#30415,#30416,#30417,#30418),(#30419,#30420,
#30421,#30422)),.UNSPECIFIED.,.F.,.F.,.F.,(4,4),(4,4),(-1.07135358020602E-16,
0.0850880881510746),(-0.100000001340247,0.1),.UNSPECIFIED.);
#657=B_SPLINE_SURFACE_WITH_KNOTS('',3,3,((#30423,#30424,#30425,#30426),
(#30427,#30428,#30429,#30430),(#30431,#30432,#30433,#30434),(#30435,#30436,
#30437,#30438)),.UNSPECIFIED.,.F.,.F.,.F.,(4,4),(4,4),(-1.07135358020602E-16,
0.0850880881510746),(0.5,0.700000001340097),.UNSPECIFIED.);
#658=B_SPLINE_SURFACE_WITH_KNOTS('',3,3,((#30439,#30440,#30441,#30442),
(#30443,#30444,#30445,#30446),(#30447,#30448,#30449,#30450),(#30451,#30452,
#30453,#30454),(#30455,#30456,#30457,#30458),(#30459,#30460,#30461,#30462),
(#30463,#30464,#30465,#30466)),.UNSPECIFIED.,.F.,.F.,.F.,(4,1,1,1,4),(4,
4),(-1.32140165738655E-13,0.14285714285703,0.285714285714192,0.571428571428516,
1.),(-0.228509057368287,0.828509057368286),.UNSPECIFIED.);
#659=B_SPLINE_SURFACE_WITH_KNOTS('',3,3,((#30473,#30474,#30475,#30476),
(#30477,#30478,#30479,#30480),(#30481,#30482,#30483,#30484),(#30485,#30486,
#30487,#30488),(#30489,#30490,#30491,#30492),(#30493,#30494,#30495,#30496),
(#30497,#30498,#30499,#30500)),.UNSPECIFIED.,.F.,.F.,.F.,(4,1,1,1,4),(4,
4),(-1.00000000194169,-0.571428572538052,-0.285714286268958,-0.142857143134411,
1.35967626047062E-13),(-0.228509057368286,0.828509057368287),
 .UNSPECIFIED.);
#660=B_SPLINE_SURFACE_WITH_KNOTS('',3,3,((#30503,#30504,#30505,#30506),
(#30507,#30508,#30509,#30510),(#30511,#30512,#30513,#30514),(#30515,#30516,
#30517,#30518)),.UNSPECIFIED.,.F.,.F.,.F.,(4,4),(4,4),(-8.26060906882159E-17,
0.0850880881510746),(-0.100000001340248,0.1),.UNSPECIFIED.);
#661=B_SPLINE_SURFACE_WITH_KNOTS('',3,3,((#30519,#30520,#30521,#30522),
(#30523,#30524,#30525,#30526),(#30527,#30528,#30529,#30530),(#30531,#30532,
#30533,#30534)),.UNSPECIFIED.,.F.,.F.,.F.,(4,4),(4,4),(-8.26060906882159E-17,
0.0850880881510746),(0.5,0.700000001340097),.UNSPECIFIED.);
#662=B_SPLINE_SURFACE_WITH_KNOTS('',3,3,((#30535,#30536,#30537,#30538),
(#30539,#30540,#30541,#30542),(#30543,#30544,#30545,#30546),(#30547,#30548,
#30549,#30550),(#30551,#30552,#30553,#30554),(#30555,#30556,#30557,#30558)),
 .UNSPECIFIED.,.F.,.F.,.F.,(4,1,1,4),(4,4),(-4.84798868997719E-14,0.214285714285676,
0.428571428571401,1.),(-0.228509057368286,0.828509057368286),
 .UNSPECIFIED.);
#663=B_SPLINE_SURFACE_WITH_KNOTS('',3,3,((#30565,#30566,#30567,#30568),
(#30569,#30570,#30571,#30572),(#30573,#30574,#30575,#30576),(#30577,#30578,
#30579,#30580),(#30581,#30582,#30583,#30584),(#30585,#30586,#30587,#30588),
(#30589,#30590,#30591,#30592)),.UNSPECIFIED.,.F.,.F.,.F.,(4,1,1,1,4),(4,
4),(-1.00000000194169,-0.571428572538047,-0.285714286268952,-0.142857143134404,
1.43590337818802E-13),(-0.228509057368286,0.828509057368287),
 .UNSPECIFIED.);
#664=B_SPLINE_SURFACE_WITH_KNOTS('',3,3,((#30595,#30596,#30597,#30598),
(#30599,#30600,#30601,#30602),(#30603,#30604,#30605,#30606),(#30607,#30608,
#30609,#30610)),.UNSPECIFIED.,.F.,.F.,.F.,(4,4),(4,4),(-2.90655708167386E-17,
0.0850880881510745),(-0.100000001340248,0.1),.UNSPECIFIED.);
#665=B_SPLINE_SURFACE_WITH_KNOTS('',3,3,((#30611,#30612,#30613,#30614),
(#30615,#30616,#30617,#30618),(#30619,#30620,#30621,#30622),(#30623,#30624,
#30625,#30626)),.UNSPECIFIED.,.F.,.F.,.F.,(4,4),(4,4),(-2.90655708167386E-17,
0.0850880881510745),(0.5,0.700000001340097),.UNSPECIFIED.);
#666=B_SPLINE_SURFACE_WITH_KNOTS('',3,3,((#30627,#30628,#30629,#30630),
(#30631,#30632,#30633,#30634),(#30635,#30636,#30637,#30638),(#30639,#30640,
#30641,#30642),(#30643,#30644,#30645,#30646),(#30647,#30648,#30649,#30650)),
 .UNSPECIFIED.,.F.,.F.,.F.,(4,1,1,4),(4,4),(-1.28256780196345E-13,0.214285714285614,
0.428571428571356,1.00000036560545),(-0.228509057368286,0.828509057368287),
 .UNSPECIFIED.);
#667=B_SPLINE_SURFACE_WITH_KNOTS('',3,3,((#30657,#30658,#30659,#30660),
(#30661,#30662,#30663,#30664),(#30665,#30666,#30667,#30668),(#30669,#30670,
#30671,#30672),(#30673,#30674,#30675,#30676),(#30677,#30678,#30679,#30680),
(#30681,#30682,#30683,#30684)),.UNSPECIFIED.,.F.,.F.,.F.,(4,1,1,1,4),(4,
4),(-1.00000000194169,-0.571428572538048,-0.285714286268956,-0.142857143134409,
1.3670329409697E-13),(-0.228509057368286,0.828509057368286),
 .UNSPECIFIED.);
#668=B_SPLINE_SURFACE_WITH_KNOTS('',3,3,((#30687,#30688,#30689,#30690),
(#30691,#30692,#30693,#30694),(#30695,#30696,#30697,#30698),(#30699,#30700,
#30701,#30702)),.UNSPECIFIED.,.F.,.F.,.F.,(4,4),(4,4),(-8.38546438727493E-17,
0.0850880881510746),(-0.100000001340248,0.1),.UNSPECIFIED.);
#669=B_SPLINE_SURFACE_WITH_KNOTS('',3,3,((#30703,#30704,#30705,#30706),
(#30707,#30708,#30709,#30710),(#30711,#30712,#30713,#30714),(#30715,#30716,
#30717,#30718)),.UNSPECIFIED.,.F.,.F.,.F.,(4,4),(4,4),(-8.38546438727493E-17,
0.0850880881510746),(0.5,0.700000001340096),.UNSPECIFIED.);
#670=B_SPLINE_SURFACE_WITH_KNOTS('',3,3,((#30719,#30720,#30721,#30722),
(#30723,#30724,#30725,#30726),(#30727,#30728,#30729,#30730),(#30731,#30732,
#30733,#30734),(#30735,#30736,#30737,#30738),(#30739,#30740,#30741,#30742)),
 .UNSPECIFIED.,.F.,.F.,.F.,(4,1,1,4),(4,4),(-8.42716484967992E-14,0.214285714285649,
0.428571428571382,1.),(-0.228509057368286,0.828509057368286),
 .UNSPECIFIED.);
#671=B_SPLINE_SURFACE_WITH_KNOTS('',3,3,((#30749,#30750,#30751,#30752),
(#30753,#30754,#30755,#30756),(#30757,#30758,#30759,#30760),(#30761,#30762,
#30763,#30764),(#30765,#30766,#30767,#30768),(#30769,#30770,#30771,#30772),
(#30773,#30774,#30775,#30776)),.UNSPECIFIED.,.F.,.F.,.F.,(4,1,1,1,4),(4,
4),(-1.00000000000001,-0.571428571428515,-0.285714285714187,-0.142857142857022,
1.42032265556368E-13),(-0.228509057368286,0.828509057368287),
 .UNSPECIFIED.);
#672=B_SPLINE_SURFACE_WITH_KNOTS('',3,3,((#30779,#30780,#30781,#30782),
(#30783,#30784,#30785,#30786),(#30787,#30788,#30789,#30790),(#30791,#30792,
#30793,#30794)),.UNSPECIFIED.,.F.,.F.,.F.,(4,4),(4,4),(-2.97741345382747E-17,
0.0850880881510747),(-0.100000001340248,0.1),.UNSPECIFIED.);
#673=B_SPLINE_SURFACE_WITH_KNOTS('',3,3,((#30795,#30796,#30797,#30798),
(#30799,#30800,#30801,#30802),(#30803,#30804,#30805,#30806),(#30807,#30808,
#30809,#30810)),.UNSPECIFIED.,.F.,.F.,.F.,(4,4),(4,4),(-2.97741345382747E-17,
0.0850880881510747),(0.5,0.700000001340097),.UNSPECIFIED.);
#674=B_SPLINE_SURFACE_WITH_KNOTS('',3,3,((#30811,#30812,#30813,#30814),
(#30815,#30816,#30817,#30818),(#30819,#30820,#30821,#30822),(#30823,#30824,
#30825,#30826),(#30827,#30828,#30829,#30830),(#30831,#30832,#30833,#30834),
(#30835,#30836,#30837,#30838)),.UNSPECIFIED.,.F.,.F.,.F.,(4,1,1,1,4),(4,
4),(-2.83059630199531E-14,0.142857142857119,0.285714285714266,0.57142857142856,
1.),(-0.228509057368285,0.828509057368286),.UNSPECIFIED.);
#675=B_SPLINE_SURFACE_WITH_KNOTS('',3,3,((#30845,#30846,#30847,#30848),
(#30849,#30850,#30851,#30852),(#30853,#30854,#30855,#30856),(#30857,#30858,
#30859,#30860),(#30861,#30862,#30863,#30864),(#30865,#30866,#30867,#30868),
(#30869,#30870,#30871,#30872)),.UNSPECIFIED.,.F.,.F.,.F.,(4,1,1,1,4),(4,
4),(-1.00000000194169,-0.571428572538095,-0.285714286269031,-0.1428571431345,
3.20438120482436E-14),(-0.228509057368286,0.828509057368286),
 .UNSPECIFIED.);
#676=B_SPLINE_SURFACE_WITH_KNOTS('',3,3,((#30875,#30876,#30877,#30878),
(#30879,#30880,#30881,#30882),(#30883,#30884,#30885,#30886),(#30887,#30888,
#30889,#30890)),.UNSPECIFIED.,.F.,.F.,.F.,(4,4),(4,4),(-5.63046512512485E-17,
0.0850880881510746),(-0.100000001340247,0.1),.UNSPECIFIED.);
#677=B_SPLINE_SURFACE_WITH_KNOTS('',3,3,((#30891,#30892,#30893,#30894),
(#30895,#30896,#30897,#30898),(#30899,#30900,#30901,#30902),(#30903,#30904,
#30905,#30906)),.UNSPECIFIED.,.F.,.F.,.F.,(4,4),(4,4),(-5.63046512512485E-17,
0.0850880881510746),(0.5,0.700000001340097),.UNSPECIFIED.);
#678=B_SPLINE_SURFACE_WITH_KNOTS('',3,3,((#30907,#30908,#30909,#30910),
(#30911,#30912,#30913,#30914),(#30915,#30916,#30917,#30918),(#30919,#30920,
#30921,#30922),(#30923,#30924,#30925,#30926),(#30927,#30928,#30929,#30930)),
 .UNSPECIFIED.,.F.,.F.,.F.,(4,1,1,4),(4,4),(-7.28930804605454E-14,0.214285714285657,
0.428571428571387,1.),(-0.228509057368286,0.828509057368286),
 .UNSPECIFIED.);
#679=B_SPLINE_SURFACE_WITH_KNOTS('',3,3,((#30937,#30938,#30939,#30940),
(#30941,#30942,#30943,#30944),(#30945,#30946,#30947,#30948),(#30949,#30950,
#30951,#30952),(#30953,#30954,#30955,#30956),(#30957,#30958,#30959,#30960),
(#30961,#30962,#30963,#30964)),.UNSPECIFIED.,.F.,.F.,.F.,(4,1,1,1,4),(4,
4),(-1.00000000194169,-0.571428572538071,-0.285714286268993,-0.142857143134454,
8.48557335508815E-14),(-0.228509057368286,0.828509057368286),
 .UNSPECIFIED.);
#680=B_SPLINE_SURFACE_WITH_KNOTS('',3,3,((#30967,#30968,#30969,#30970),
(#30971,#30972,#30973,#30974),(#30975,#30976,#30977,#30978),(#30979,#30980,
#30981,#30982)),.UNSPECIFIED.,.F.,.F.,.F.,(4,4),(4,4),(-2.55704448513501E-18,
0.0850880881510746),(-0.100000001340247,0.1),.UNSPECIFIED.);
#681=B_SPLINE_SURFACE_WITH_KNOTS('',3,3,((#30983,#30984,#30985,#30986),
(#30987,#30988,#30989,#30990),(#30991,#30992,#30993,#30994),(#30995,#30996,
#30997,#30998)),.UNSPECIFIED.,.F.,.F.,.F.,(4,4),(4,4),(-2.55704448513501E-18,
0.0850880881510746),(0.5,0.700000001340097),.UNSPECIFIED.);
#682=B_SPLINE_SURFACE_WITH_KNOTS('',3,3,((#30999,#31000,#31001,#31002),
(#31003,#31004,#31005,#31006),(#31007,#31008,#31009,#31010),(#31011,#31012,
#31013,#31014),(#31015,#31016,#31017,#31018),(#31019,#31020,#31021,#31022)),
 .UNSPECIFIED.,.F.,.F.,.F.,(4,1,1,4),(4,4),(-7.99234215486585E-14,0.214285714285652,
0.428571428571384,1.00000036560556),(-0.228509057368286,0.828509057368286),
 .UNSPECIFIED.);
#683=B_SPLINE_SURFACE_WITH_KNOTS('',3,3,((#31029,#31030,#31031,#31032),
(#31033,#31034,#31035,#31036),(#31037,#31038,#31039,#31040),(#31041,#31042,
#31043,#31044),(#31045,#31046,#31047,#31048),(#31049,#31050,#31051,#31052),
(#31053,#31054,#31055,#31056)),.UNSPECIFIED.,.F.,.F.,.F.,(4,1,1,1,4),(4,
4),(-1.00000000194169,-0.571428572538088,-0.28571428626902,-0.142857143134486,
4.79429694563687E-14),(-0.228509057368286,0.828509057368286),
 .UNSPECIFIED.);
#684=B_SPLINE_SURFACE_WITH_KNOTS('',3,3,((#31059,#31060,#31061,#31062),
(#31063,#31064,#31065,#31066),(#31067,#31068,#31069,#31070),(#31071,#31072,
#31073,#31074)),.UNSPECIFIED.,.F.,.F.,.F.,(4,4),(4,4),(-3.9786331981339E-17,
0.0850880881510746),(-0.100000001340247,0.1),.UNSPECIFIED.);
#685=B_SPLINE_SURFACE_WITH_KNOTS('',3,3,((#31075,#31076,#31077,#31078),
(#31079,#31080,#31081,#31082),(#31083,#31084,#31085,#31086),(#31087,#31088,
#31089,#31090)),.UNSPECIFIED.,.F.,.F.,.F.,(4,4),(4,4),(-3.9786331981339E-17,
0.0850880881510746),(0.5,0.700000001340097),.UNSPECIFIED.);
#686=B_SPLINE_SURFACE_WITH_KNOTS('',3,3,((#31091,#31092,#31093,#31094),
(#31095,#31096,#31097,#31098),(#31099,#31100,#31101,#31102),(#31103,#31104,
#31105,#31106),(#31107,#31108,#31109,#31110),(#31111,#31112,#31113,#31114),
(#31115,#31116,#31117,#31118)),.UNSPECIFIED.,.F.,.F.,.F.,(4,1,1,1,4),(4,
4),(-4.11753964257855E-14,0.142857142857108,0.285714285714257,0.571428571428555,
1.00000036560902),(-0.228509057368286,0.828509057368286),.UNSPECIFIED.);
#687=B_SPLINE_SURFACE_WITH_KNOTS('',3,3,((#31125,#31126,#31127,#31128),
(#31129,#31130,#31131,#31132),(#31133,#31134,#31135,#31136),(#31137,#31138,
#31139,#31140),(#31141,#31142,#31143,#31144),(#31145,#31146,#31147,#31148),
(#31149,#31150,#31151,#31152)),.UNSPECIFIED.,.F.,.F.,.F.,(4,1,1,1,4),(4,
4),(-1.00000000000001,-0.571428571428513,-0.285714285714184,-0.14285714285702,
1.44717038445973E-13),(-0.228509057368286,0.828509057368287),
 .UNSPECIFIED.);
#688=B_SPLINE_SURFACE_WITH_KNOTS('',3,3,((#31155,#31156,#31157,#31158),
(#31159,#31160,#31161,#31162),(#31163,#31164,#31165,#31166),(#31167,#31168,
#31169,#31170)),.UNSPECIFIED.,.F.,.F.,.F.,(4,4),(4,4),(-5.86293617278695E-17,
0.0850880881510746),(-0.100000001340248,0.1),.UNSPECIFIED.);
#689=B_SPLINE_SURFACE_WITH_KNOTS('',3,3,((#31171,#31172,#31173,#31174),
(#31175,#31176,#31177,#31178),(#31179,#31180,#31181,#31182),(#31183,#31184,
#31185,#31186)),.UNSPECIFIED.,.F.,.F.,.F.,(4,4),(4,4),(-5.86293617278695E-17,
0.0850880881510746),(0.5,0.700000001340097),.UNSPECIFIED.);
#690=B_SPLINE_SURFACE_WITH_KNOTS('',3,3,((#31187,#31188,#31189,#31190),
(#31191,#31192,#31193,#31194),(#31195,#31196,#31197,#31198),(#31199,#31200,
#31201,#31202),(#31203,#31204,#31205,#31206),(#31207,#31208,#31209,#31210)),
 .UNSPECIFIED.,.F.,.F.,.F.,(4,1,1,4),(4,4),(-9.25699570363353E-14,0.214285714285642,
0.428571428571376,1.),(-0.228509057368286,0.828509057368287),
 .UNSPECIFIED.);
#691=B_SPLINE_SURFACE_WITH_KNOTS('',3,3,((#31217,#31218,#31219,#31220),
(#31221,#31222,#31223,#31224),(#31225,#31226,#31227,#31228),(#31229,#31230,
#31231,#31232),(#31233,#31234,#31235,#31236),(#31237,#31238,#31239,#31240),
(#31241,#31242,#31243,#31244)),.UNSPECIFIED.,.F.,.F.,.F.,(4,1,1,1,4),(4,
4),(-1.00000000194169,-0.571428572538053,-0.285714286268962,-0.142857143134417,
1.28531982146453E-13),(-0.228509057368285,0.828509057368287),
 .UNSPECIFIED.);
#692=B_SPLINE_SURFACE_WITH_KNOTS('',3,3,((#31247,#31248,#31249,#31250),
(#31251,#31252,#31253,#31254),(#31255,#31256,#31257,#31258),(#31259,#31260,
#31261,#31262)),.UNSPECIFIED.,.F.,.F.,.F.,(4,4),(4,4),(-1.09019546950253E-16,
0.0850880881510746),(-0.100000001340248,0.1),.UNSPECIFIED.);
#693=B_SPLINE_SURFACE_WITH_KNOTS('',3,3,((#31263,#31264,#31265,#31266),
(#31267,#31268,#31269,#31270),(#31271,#31272,#31273,#31274),(#31275,#31276,
#31277,#31278)),.UNSPECIFIED.,.F.,.F.,.F.,(4,4),(4,4),(-1.09019546950253E-16,
0.0850880881510746),(0.5,0.700000001340097),.UNSPECIFIED.);
#694=B_SPLINE_SURFACE_WITH_KNOTS('',3,3,((#31279,#31280,#31281,#31282),
(#31283,#31284,#31285,#31286),(#31287,#31288,#31289,#31290),(#31291,#31292,
#31293,#31294),(#31295,#31296,#31297,#31298),(#31299,#31300,#31301,#31302),
(#31303,#31304,#31305,#31306)),.UNSPECIFIED.,.F.,.F.,.F.,(4,1,1,1,4),(4,
4),(-8.76619728054132E-14,0.142857142857068,0.285714285714223,0.571428571428534,
1.),(-0.228509057368286,0.828509057368286),.UNSPECIFIED.);
#695=B_SPLINE_SURFACE_WITH_KNOTS('',3,3,((#31313,#31314,#31315,#31316),
(#31317,#31318,#31319,#31320),(#31321,#31322,#31323,#31324),(#31325,#31326,
#31327,#31328),(#31329,#31330,#31331,#31332),(#31333,#31334,#31335,#31336),
(#31337,#31338,#31339,#31340)),.UNSPECIFIED.,.F.,.F.,.F.,(4,1,1,1,4),(4,
4),(-1.00000000194169,-0.571428572538084,-0.285714286269015,-0.14285714313448,
5.42037452861625E-14),(-0.228509057368285,0.828509057368286),
 .UNSPECIFIED.);
#696=B_SPLINE_SURFACE_WITH_KNOTS('',3,3,((#31343,#31344,#31345,#31346),
(#31347,#31348,#31349,#31350),(#31351,#31352,#31353,#31354),(#31355,#31356,
#31357,#31358)),.UNSPECIFIED.,.F.,.F.,.F.,(4,4),(4,4),(-7.28779245561565E-17,
0.0850880881510746),(-0.100000001340248,0.1),.UNSPECIFIED.);
#697=B_SPLINE_SURFACE_WITH_KNOTS('',3,3,((#31359,#31360,#31361,#31362),
(#31363,#31364,#31365,#31366),(#31367,#31368,#31369,#31370),(#31371,#31372,
#31373,#31374)),.UNSPECIFIED.,.F.,.F.,.F.,(4,4),(4,4),(-7.28779245561565E-17,
0.0850880881510746),(0.5,0.700000001340097),.UNSPECIFIED.);
#698=B_SPLINE_SURFACE_WITH_KNOTS('',3,3,((#31375,#31376,#31377,#31378),
(#31379,#31380,#31381,#31382),(#31383,#31384,#31385,#31386),(#31387,#31388,
#31389,#31390),(#31391,#31392,#31393,#31394),(#31395,#31396,#31397,#31398)),
 .UNSPECIFIED.,.F.,.F.,.F.,(4,1,1,4),(4,4),(-4.97324904964964E-14,0.214285714285675,
0.4285714285714,1.),(-0.228509057368285,0.828509057368286),
 .UNSPECIFIED.);
#699=B_SPLINE_SURFACE_WITH_KNOTS('',3,3,((#31405,#31406,#31407,#31408),
(#31409,#31410,#31411,#31412),(#31413,#31414,#31415,#31416),(#31417,#31418,
#31419,#31420),(#31421,#31422,#31423,#31424),(#31425,#31426,#31427,#31428)),
 .UNSPECIFIED.,.F.,.F.,.F.,(4,1,1,4),(4,4),(-1.0000003656055,-0.428571428571403,
-0.214285714285677,4.91672674796106E-14),(-0.228509057368286,0.828509057368286),
 .UNSPECIFIED.);
#700=B_SPLINE_SURFACE_WITH_KNOTS('',3,3,((#31431,#31432,#31433,#31434),
(#31435,#31436,#31437,#31438),(#31439,#31440,#31441,#31442),(#31443,#31444,
#31445,#31446)),.UNSPECIFIED.,.F.,.F.,.F.,(4,4),(4,4),(-2.90655708167386E-17,
0.0850880881510745),(-0.100000001340247,0.1),.UNSPECIFIED.);
#701=B_SPLINE_SURFACE_WITH_KNOTS('',3,3,((#31447,#31448,#31449,#31450),
(#31451,#31452,#31453,#31454),(#31455,#31456,#31457,#31458),(#31459,#31460,
#31461,#31462)),.UNSPECIFIED.,.F.,.F.,.F.,(4,4),(4,4),(-2.90655708167386E-17,
0.0850880881510745),(0.5,0.700000001340097),.UNSPECIFIED.);
#702=B_SPLINE_SURFACE_WITH_KNOTS('',3,3,((#31463,#31464,#31465,#31466),
(#31467,#31468,#31469,#31470),(#31471,#31472,#31473,#31474),(#31475,#31476,
#31477,#31478)),.UNSPECIFIED.,.F.,.F.,.F.,(4,4),(4,4),(-0.871332876340297,
-0.774999998579001),(-0.3,0.9),.UNSPECIFIED.);
#703=B_SPLINE_SURFACE_WITH_KNOTS('',3,3,((#31494,#31495,#31496,#31497),
(#31498,#31499,#31500,#31501),(#31502,#31503,#31504,#31505),(#31506,#31507,
#31508,#31509)),.UNSPECIFIED.,.F.,.F.,.F.,(4,4),(4,4),(-5.14197626699797E-6,
1.00000003476692),(-0.228566601398621,0.828566601398622),.UNSPECIFIED.);
#704=B_SPLINE_SURFACE_WITH_KNOTS('',3,3,((#31514,#31515,#31516,#31517),
(#31518,#31519,#31520,#31521),(#31522,#31523,#31524,#31525),(#31526,#31527,
#31528,#31529)),.UNSPECIFIED.,.F.,.F.,.F.,(4,4),(4,4),(0.774999998579001,
0.871332876340297),(-0.3,0.9),.UNSPECIFIED.);
#705=B_SPLINE_SURFACE_WITH_KNOTS('',3,3,((#31577,#31578,#31579,#31580),
(#31581,#31582,#31583,#31584),(#31585,#31586,#31587,#31588),(#31589,#31590,
#31591,#31592)),.UNSPECIFIED.,.F.,.F.,.F.,(4,4),(4,4),(0.774999998579001,
0.871332876340298),(-0.3,0.9),.UNSPECIFIED.);
#706=B_SPLINE_SURFACE_WITH_KNOTS('',3,3,((#31612,#31613,#31614,#31615),
(#31616,#31617,#31618,#31619),(#31620,#31621,#31622,#31623),(#31624,#31625,
#31626,#31627)),.UNSPECIFIED.,.F.,.F.,.F.,(4,4),(4,4),(-0.871332876340297,
-0.774999998579),(-0.3,0.9),.UNSPECIFIED.);
#707=B_SPLINE_SURFACE_WITH_KNOTS('',3,3,((#31629,#31630,#31631,#31632),
(#31633,#31634,#31635,#31636),(#31637,#31638,#31639,#31640),(#31641,#31642,
#31643,#31644)),.UNSPECIFIED.,.F.,.F.,.F.,(4,4),(4,4),(-5.14198768541974E-6,
1.00000001443829),(-0.228566601398622,0.828566601398622),.UNSPECIFIED.);
#708=B_SPLINE_SURFACE_WITH_KNOTS('',3,3,((#31645,#31646,#31647,#31648),
(#31649,#31650,#31651,#31652),(#31653,#31654,#31655,#31656),(#31657,#31658,
#31659,#31660)),.UNSPECIFIED.,.F.,.F.,.F.,(4,4),(4,4),(-0.871332876340297,
-0.774999998579),(-0.3,0.9),.UNSPECIFIED.);
#709=B_SPLINE_SURFACE_WITH_KNOTS('',3,3,((#31676,#31677,#31678,#31679),
(#31680,#31681,#31682,#31683),(#31684,#31685,#31686,#31687),(#31688,#31689,
#31690,#31691)),.UNSPECIFIED.,.F.,.F.,.F.,(4,4),(4,4),(0.774999998579,0.871332876340298),
(-0.3,0.9),.UNSPECIFIED.);
#710=B_SPLINE_SURFACE_WITH_KNOTS('',3,3,((#31711,#31712,#31713,#31714),
(#31715,#31716,#31717,#31718),(#31719,#31720,#31721,#31722),(#31723,#31724,
#31725,#31726)),.UNSPECIFIED.,.F.,.F.,.F.,(4,4),(4,4),(-5.14198403323007E-6,
1.00000003476684),(-0.228566601398622,0.828566601398622),.UNSPECIFIED.);
#711=B_SPLINE_SURFACE_WITH_KNOTS('',3,3,((#31817,#31818,#31819,#31820),
(#31821,#31822,#31823,#31824),(#31825,#31826,#31827,#31828),(#31829,#31830,
#31831,#31832)),.UNSPECIFIED.,.F.,.F.,.F.,(4,4),(4,4),(-0.871332876340297,
-0.774999998579),(-0.3,0.9),.UNSPECIFIED.);
#712=B_SPLINE_SURFACE_WITH_KNOTS('',3,3,((#31833,#31834,#31835,#31836),
(#31837,#31838,#31839,#31840),(#31841,#31842,#31843,#31844),(#31845,#31846,
#31847,#31848)),.UNSPECIFIED.,.F.,.F.,.F.,(4,4),(4,4),(-5.14197252954318E-6,
1.00000003476695),(-0.228566601398621,0.828566601398621),.UNSPECIFIED.);
#713=B_SPLINE_SURFACE_WITH_KNOTS('',3,3,((#31853,#31854,#31855,#31856),
(#31857,#31858,#31859,#31860),(#31861,#31862,#31863,#31864),(#31865,#31866,
#31867,#31868)),.UNSPECIFIED.,.F.,.F.,.F.,(4,4),(4,4),(0.774999998579001,
0.871332876340297),(-0.3,0.9),.UNSPECIFIED.);
#714=B_SPLINE_SURFACE_WITH_KNOTS('',3,3,((#31897,#31898,#31899,#31900),
(#31901,#31902,#31903,#31904),(#31905,#31906,#31907,#31908),(#31909,#31910,
#31911,#31912)),.UNSPECIFIED.,.F.,.F.,.F.,(4,4),(4,4),(0.774999998579,0.871332876340298),
(-0.3,0.9),.UNSPECIFIED.);
#715=B_SPLINE_SURFACE_WITH_KNOTS('',3,3,((#31930,#31931,#31932,#31933),
(#31934,#31935,#31936,#31937),(#31938,#31939,#31940,#31941),(#31942,#31943,
#31944,#31945)),.UNSPECIFIED.,.F.,.F.,.F.,(4,4),(4,4),(-0.871332876340297,
-0.774999998579),(-0.3,0.9),.UNSPECIFIED.);
#716=B_SPLINE_SURFACE_WITH_KNOTS('',3,3,((#31946,#31947,#31948,#31949),
(#31950,#31951,#31952,#31953),(#31954,#31955,#31956,#31957),(#31958,#31959,
#31960,#31961)),.UNSPECIFIED.,.F.,.F.,.F.,(4,4),(4,4),(-5.14197203926869E-6,
1.00000003476844),(-0.228566601398621,0.828566601398622),.UNSPECIFIED.);
#717=B_SPLINE_SURFACE_WITH_KNOTS('',3,3,((#31962,#31963,#31964,#31965),
(#31966,#31967,#31968,#31969),(#31970,#31971,#31972,#31973),(#31974,#31975,
#31976,#31977)),.UNSPECIFIED.,.F.,.F.,.F.,(4,4),(4,4),(-0.871332876340297,
-0.774999998579),(-0.3,0.9),.UNSPECIFIED.);
#718=B_SPLINE_SURFACE_WITH_KNOTS('',3,3,((#31991,#31992,#31993,#31994),
(#31995,#31996,#31997,#31998),(#31999,#32000,#32001,#32002),(#32003,#32004,
#32005,#32006)),.UNSPECIFIED.,.F.,.F.,.F.,(4,4),(4,4),(0.774999998579,0.871332876340298),
(-0.3,0.9),.UNSPECIFIED.);
#719=B_SPLINE_SURFACE_WITH_KNOTS('',3,3,((#32024,#32025,#32026,#32027),
(#32028,#32029,#32030,#32031),(#32032,#32033,#32034,#32035),(#32036,#32037,
#32038,#32039)),.UNSPECIFIED.,.F.,.F.,.F.,(4,4),(4,4),(-5.14197986944964E-6,
1.00000003476884),(-0.228566601398622,0.828566601398622),.UNSPECIFIED.);
#720=B_SPLINE_SURFACE_WITH_KNOTS('',3,3,((#32054,#32055,#32056,#32057),
(#32058,#32059,#32060,#32061),(#32062,#32063,#32064,#32065),(#32066,#32067,
#32068,#32069)),.UNSPECIFIED.,.F.,.F.,.F.,(4,4),(4,4),(-0.871332876340297,
-0.774999998579),(-0.3,0.9),.UNSPECIFIED.);
#721=B_SPLINE_SURFACE_WITH_KNOTS('',3,3,((#32070,#32071,#32072,#32073),
(#32074,#32075,#32076,#32077),(#32078,#32079,#32080,#32081),(#32082,#32083,
#32084,#32085)),.UNSPECIFIED.,.F.,.F.,.F.,(4,4),(4,4),(-5.14196888445895E-6,
1.0000000144377),(-0.228566601398621,0.828566601398621),.UNSPECIFIED.);
#722=B_SPLINE_SURFACE_WITH_KNOTS('',3,3,((#32090,#32091,#32092,#32093),
(#32094,#32095,#32096,#32097),(#32098,#32099,#32100,#32101),(#32102,#32103,
#32104,#32105)),.UNSPECIFIED.,.F.,.F.,.F.,(4,4),(4,4),(0.774999998579,0.871332876340297),
(-0.3,0.9),.UNSPECIFIED.);
#723=B_SPLINE_SURFACE_WITH_KNOTS('',3,3,((#32134,#32135,#32136,#32137),
(#32138,#32139,#32140,#32141),(#32142,#32143,#32144,#32145),(#32146,#32147,
#32148,#32149)),.UNSPECIFIED.,.F.,.F.,.F.,(4,4),(4,4),(0.774999998579,0.871332876340298),
(-0.3,0.9),.UNSPECIFIED.);
#724=B_SPLINE_SURFACE_WITH_KNOTS('',3,3,((#32167,#32168,#32169,#32170),
(#32171,#32172,#32173,#32174),(#32175,#32176,#32177,#32178),(#32179,#32180,
#32181,#32182)),.UNSPECIFIED.,.F.,.F.,.F.,(4,4),(4,4),(-0.871332876340297,
-0.774999998579),(-0.3,0.9),.UNSPECIFIED.);
#725=B_SPLINE_SURFACE_WITH_KNOTS('',3,3,((#32183,#32184,#32185,#32186),
(#32187,#32188,#32189,#32190),(#32191,#32192,#32193,#32194),(#32195,#32196,
#32197,#32198)),.UNSPECIFIED.,.F.,.F.,.F.,(4,4),(4,4),(-5.14198304557567E-6,
1.00000001443821),(-0.228566601398622,0.828566601398623),.UNSPECIFIED.);
#726=B_SPLINE_SURFACE_WITH_KNOTS('',3,3,((#32199,#32200,#32201,#32202),
(#32203,#32204,#32205,#32206),(#32207,#32208,#32209,#32210),(#32211,#32212,
#32213,#32214)),.UNSPECIFIED.,.F.,.F.,.F.,(4,4),(4,4),(-0.871332876340297,
-0.774999998579),(-0.3,0.9),.UNSPECIFIED.);
#727=B_SPLINE_SURFACE_WITH_KNOTS('',3,3,((#32228,#32229,#32230,#32231),
(#32232,#32233,#32234,#32235),(#32236,#32237,#32238,#32239),(#32240,#32241,
#32242,#32243)),.UNSPECIFIED.,.F.,.F.,.F.,(4,4),(4,4),(0.774999998579,0.871332876340297),
(-0.3,0.9),.UNSPECIFIED.);
#728=B_SPLINE_SURFACE_WITH_KNOTS('',3,3,((#32261,#32262,#32263,#32264),
(#32265,#32266,#32267,#32268),(#32269,#32270,#32271,#32272),(#32273,#32274,
#32275,#32276)),.UNSPECIFIED.,.F.,.F.,.F.,(4,4),(4,4),(-5.14198393375409E-6,
1.0000000347646),(-0.228566601398622,0.828566601398623),.UNSPECIFIED.);
#729=B_SPLINE_SURFACE_WITH_KNOTS('',3,3,((#32291,#32292,#32293,#32294),
(#32295,#32296,#32297,#32298),(#32299,#32300,#32301,#32302),(#32303,#32304,
#32305,#32306)),.UNSPECIFIED.,.F.,.F.,.F.,(4,4),(4,4),(-0.871332876340297,
-0.774999998579),(-0.3,0.9),.UNSPECIFIED.);
#730=B_SPLINE_SURFACE_WITH_KNOTS('',3,3,((#32307,#32308,#32309,#32310),
(#32311,#32312,#32313,#32314),(#32315,#32316,#32317,#32318),(#32319,#32320,
#32321,#32322)),.UNSPECIFIED.,.F.,.F.,.F.,(4,4),(4,4),(-5.14198745804606E-6,
1.00000001443741),(-0.228566601398622,0.828566601398622),.UNSPECIFIED.);
#731=B_SPLINE_SURFACE_WITH_KNOTS('',3,3,((#32327,#32328,#32329,#32330),
(#32331,#32332,#32333,#32334),(#32335,#32336,#32337,#32338),(#32339,#32340,
#32341,#32342)),.UNSPECIFIED.,.F.,.F.,.F.,(4,4),(4,4),(0.774999998579001,
0.871332876340298),(-0.3,0.900000000000001),.UNSPECIFIED.);
#732=B_SPLINE_SURFACE_WITH_KNOTS('',3,3,((#32371,#32372,#32373,#32374),
(#32375,#32376,#32377,#32378),(#32379,#32380,#32381,#32382),(#32383,#32384,
#32385,#32386)),.UNSPECIFIED.,.F.,.F.,.F.,(4,4),(4,4),(0.774999998579001,
0.871332876340297),(-0.3,0.9),.UNSPECIFIED.);
#733=B_SPLINE_SURFACE_WITH_KNOTS('',3,3,((#32404,#32405,#32406,#32407),
(#32408,#32409,#32410,#32411),(#32412,#32413,#32414,#32415),(#32416,#32417,
#32418,#32419)),.UNSPECIFIED.,.F.,.F.,.F.,(4,4),(4,4),(-0.871332876340297,
-0.774999998579),(-0.3,0.9),.UNSPECIFIED.);
#734=B_SPLINE_SURFACE_WITH_KNOTS('',3,3,((#32420,#32421,#32422,#32423),
(#32424,#32425,#32426,#32427),(#32428,#32429,#32430,#32431),(#32432,#32433,
#32434,#32435)),.UNSPECIFIED.,.F.,.F.,.F.,(4,4),(4,4),(-5.14199177104047E-6,
1.0000000347666),(-0.228566601398622,0.828566601398623),.UNSPECIFIED.);
#735=B_SPLINE_SURFACE_WITH_KNOTS('',3,3,((#32436,#32437,#32438,#32439),
(#32440,#32441,#32442,#32443),(#32444,#32445,#32446,#32447),(#32448,#32449,
#32450,#32451)),.UNSPECIFIED.,.F.,.F.,.F.,(4,4),(4,4),(-0.871332876340297,
-0.774999998579),(-0.3,0.9),.UNSPECIFIED.);
#736=B_SPLINE_SURFACE_WITH_KNOTS('',3,3,((#32465,#32466,#32467,#32468),
(#32469,#32470,#32471,#32472),(#32473,#32474,#32475,#32476),(#32477,#32478,
#32479,#32480)),.UNSPECIFIED.,.F.,.F.,.F.,(4,4),(4,4),(0.774999998579,0.871332876340298),
(-0.3,0.9),.UNSPECIFIED.);
#737=B_SPLINE_SURFACE_WITH_KNOTS('',3,3,((#32498,#32499,#32500,#32501),
(#32502,#32503,#32504,#32505),(#32506,#32507,#32508,#32509),(#32510,#32511,
#32512,#32513)),.UNSPECIFIED.,.F.,.F.,.F.,(4,4),(4,4),(-5.14197888179524E-6,
1.00000003476801),(-0.228566601398622,0.828566601398622),.UNSPECIFIED.);
#738=B_SPLINE_SURFACE_WITH_KNOTS('',3,3,((#32528,#32529,#32530,#32531),
(#32532,#32533,#32534,#32535),(#32536,#32537,#32538,#32539),(#32540,#32541,
#32542,#32543)),.UNSPECIFIED.,.F.,.F.,.F.,(4,4),(4,4),(-0.871332876340297,
-0.774999998579),(-0.3,0.9),.UNSPECIFIED.);
#739=B_SPLINE_SURFACE_WITH_KNOTS('',3,3,((#32544,#32545,#32546,#32547),
(#32548,#32549,#32550,#32551),(#32552,#32553,#32554,#32555),(#32556,#32557,
#32558,#32559)),.UNSPECIFIED.,.F.,.F.,.F.,(4,4),(4,4),(-5.1419737019387E-6,
1.00000001443723),(-0.228566601398621,0.828566601398621),.UNSPECIFIED.);
#740=B_SPLINE_SURFACE_WITH_KNOTS('',3,3,((#32564,#32565,#32566,#32567),
(#32568,#32569,#32570,#32571),(#32572,#32573,#32574,#32575),(#32576,#32577,
#32578,#32579)),.UNSPECIFIED.,.F.,.F.,.F.,(4,4),(4,4),(0.774999998579,0.871332876340297),
(-0.3,0.9),.UNSPECIFIED.);
#741=B_SPLINE_SURFACE_WITH_KNOTS('',3,3,((#32608,#32609,#32610,#32611),
(#32612,#32613,#32614,#32615),(#32616,#32617,#32618,#32619),(#32620,#32621,
#32622,#32623)),.UNSPECIFIED.,.F.,.F.,.F.,(4,4),(4,4),(0.774999998579,0.871332876340297),
(-0.3,0.9),.UNSPECIFIED.);
#742=B_SPLINE_SURFACE_WITH_KNOTS('',3,3,((#32641,#32642,#32643,#32644),
(#32645,#32646,#32647,#32648),(#32649,#32650,#32651,#32652),(#32653,#32654,
#32655,#32656)),.UNSPECIFIED.,.F.,.F.,.F.,(4,4),(4,4),(-0.871332876340297,
-0.774999998579),(-0.3,0.9),.UNSPECIFIED.);
#743=B_SPLINE_SURFACE_WITH_KNOTS('',3,3,((#32657,#32658,#32659,#32660),
(#32661,#32662,#32663,#32664),(#32665,#32666,#32667,#32668),(#32669,#32670,
#32671,#32672)),.UNSPECIFIED.,.F.,.F.,.F.,(4,4),(4,4),(-5.1419868967173E-6,
1.00000003476766),(-0.228566601398622,0.828566601398622),.UNSPECIFIED.);
#744=B_SPLINE_SURFACE_WITH_KNOTS('',3,3,((#32673,#32674,#32675,#32676),
(#32677,#32678,#32679,#32680),(#32681,#32682,#32683,#32684),(#32685,#32686,
#32687,#32688)),.UNSPECIFIED.,.F.,.F.,.F.,(4,4),(4,4),(-0.871332876340297,
-0.774999998579),(-0.3,0.9),.UNSPECIFIED.);
#745=B_SPLINE_SURFACE_WITH_KNOTS('',3,3,((#32702,#32703,#32704,#32705),
(#32706,#32707,#32708,#32709),(#32710,#32711,#32712,#32713),(#32714,#32715,
#32716,#32717)),.UNSPECIFIED.,.F.,.F.,.F.,(4,4),(4,4),(0.774999998579001,
0.871332876340297),(-0.3,0.9),.UNSPECIFIED.);
#746=B_SPLINE_SURFACE_WITH_KNOTS('',3,3,((#32735,#32736,#32737,#32738),
(#32739,#32740,#32741,#32742),(#32743,#32744,#32745,#32746),(#32747,#32748,
#32749,#32750)),.UNSPECIFIED.,.F.,.F.,.F.,(4,4),(4,4),(-5.14197624568169E-6,
1.00000001444045),(-0.228566601398621,0.828566601398622),.UNSPECIFIED.);
#747=B_SPLINE_SURFACE_WITH_KNOTS('',3,3,((#32765,#32766,#32767,#32768),
(#32769,#32770,#32771,#32772),(#32773,#32774,#32775,#32776),(#32777,#32778,
#32779,#32780)),.UNSPECIFIED.,.F.,.F.,.F.,(4,4),(4,4),(-0.871332876340297,
-0.774999998579),(-0.3,0.9),.UNSPECIFIED.);
#748=B_SPLINE_SURFACE_WITH_KNOTS('',3,3,((#32781,#32782,#32783,#32784),
(#32785,#32786,#32787,#32788),(#32789,#32790,#32791,#32792),(#32793,#32794,
#32795,#32796)),.UNSPECIFIED.,.F.,.F.,.F.,(4,4),(4,4),(-5.14197358114643E-6,
1.00000003476771),(-0.228566601398621,0.828566601398622),.UNSPECIFIED.);
#749=B_SPLINE_SURFACE_WITH_KNOTS('',3,3,((#32801,#32802,#32803,#32804),
(#32805,#32806,#32807,#32808),(#32809,#32810,#32811,#32812),(#32813,#32814,
#32815,#32816)),.UNSPECIFIED.,.F.,.F.,.F.,(4,4),(4,4),(0.774999998579,0.871332876340297),
(-0.3,0.9),.UNSPECIFIED.);
#750=B_SPLINE_SURFACE_WITH_KNOTS('',3,3,((#32845,#32846,#32847,#32848),
(#32849,#32850,#32851,#32852),(#32853,#32854,#32855,#32856),(#32857,#32858,
#32859,#32860)),.UNSPECIFIED.,.F.,.F.,.F.,(4,4),(4,4),(0.774999998579,0.871332876340298),
(-0.3,0.9),.UNSPECIFIED.);
#751=B_SPLINE_SURFACE_WITH_KNOTS('',3,3,((#32878,#32879,#32880,#32881),
(#32882,#32883,#32884,#32885),(#32886,#32887,#32888,#32889),(#32890,#32891,
#32892,#32893)),.UNSPECIFIED.,.F.,.F.,.F.,(4,4),(4,4),(-0.871332876340297,
-0.774999998579001),(-0.3,0.9),.UNSPECIFIED.);
#752=B_SPLINE_SURFACE_WITH_KNOTS('',3,3,((#32894,#32895,#32896,#32897),
(#32898,#32899,#32900,#32901),(#32902,#32903,#32904,#32905),(#32906,#32907,
#32908,#32909)),.UNSPECIFIED.,.F.,.F.,.F.,(4,4),(4,4),(-5.14197949286199E-6,
1.00000003476611),(-0.228566601398621,0.828566601398622),.UNSPECIFIED.);
#753=B_SPLINE_SURFACE_WITH_KNOTS('',3,3,((#32910,#32911,#32912,#32913),
(#32914,#32915,#32916,#32917),(#32918,#32919,#32920,#32921),(#32922,#32923,
#32924,#32925)),.UNSPECIFIED.,.F.,.F.,.F.,(4,4),(4,4),(-0.871332876340297,
-0.774999998579),(-0.3,0.9),.UNSPECIFIED.);
#754=B_SPLINE_SURFACE_WITH_KNOTS('',3,3,((#32939,#32940,#32941,#32942),
(#32943,#32944,#32945,#32946),(#32947,#32948,#32949,#32950),(#32951,#32952,
#32953,#32954)),.UNSPECIFIED.,.F.,.F.,.F.,(4,4),(4,4),(0.774999998579,0.871332876340297),
(-0.3,0.9),.UNSPECIFIED.);
#755=B_SPLINE_SURFACE_WITH_KNOTS('',3,3,((#32959,#32960,#32961,#32962),
(#32963,#32964,#32965,#32966),(#32967,#32968,#32969,#32970),(#32971,#32972,
#32973,#32974)),.UNSPECIFIED.,.F.,.F.,.F.,(4,4),(4,4),(-5.14197984813336E-6,
1.00000003476548),(-0.228566601398621,0.828566601398622),.UNSPECIFIED.);
#756=B_SPLINE_SURFACE_WITH_KNOTS('',3,3,((#77101,#77102,#77103,#77104,#77105,
#77106,#77107,#77108,#77109,#77110,#77111,#77112,#77113,#77114,#77115,#77116,
#77117,#77118,#77119,#77120,#77121,#77122,#77123,#77124,#77125,#77126,#77127,
#77128,#77129,#77130,#77131,#77132,#77133,#77134,#77135,#77136,#77137,#77138,
#77139,#77140,#77141,#77142,#77143,#77144,#77145,#77146,#77147,#77148,#77149,
#77150,#77151,#77152,#77153,#77154,#77155,#77156,#77157,#77158,#77159,#77160,
#77161,#77162,#77163,#77164,#77165,#77166,#77167,#77168,#77169,#77170,#77171,
#77172,#77173,#77174,#77175,#77176,#77177,#77178,#77179,#77180,#77181,#77182,
#77183,#77184,#77185,#77186,#77187,#77188,#77189,#77190,#77191,#77192,#77193,
#77194,#77195,#77196,#77197,#77198,#77199,#77200,#77201,#77202,#77203,#77204,
#77205,#77206,#77207,#77208,#77209,#77210,#77211,#77212,#77213,#77214,#77215,
#77216,#77217,#77218,#77219,#77220,#77221,#77222,#77223,#77224,#77225,#77226,
#77227,#77228,#77229,#77230,#77231,#77232,#77233,#77234,#77235,#77236,#77237,
#77238,#77239,#77240,#77241,#77242,#77243,#77244,#77245,#77246,#77247,#77248,
#77249,#77250,#77251,#77252,#77253,#77254,#77255,#77256,#77257,#77258,#77259,
#77260,#77261,#77262,#77263,#77264,#77265,#77266,#77267,#77268,#77269,#77270,
#77271,#77272,#77273,#77274,#77275,#77276,#77277,#77278,#77279,#77280,#77281,
#77282,#77283,#77284,#77285,#77286,#77287,#77288,#77289,#77290,#77291,#77292,
#77293,#77294,#77295,#77296,#77297,#77298,#77299,#77300,#77301,#77302,#77303,
#77304,#77305,#77306,#77307,#77308,#77309,#77310,#77311,#77312,#77313,#77314,
#77315,#77316,#77317,#77318,#77319,#77320,#77321,#77322,#77323,#77324,#77325,
#77326,#77327,#77328,#77329,#77330,#77331,#77332,#77333,#77334,#77335,#77336,
#77337,#77338,#77339,#77340,#77341,#77342,#77343,#77344,#77345,#77346,#77347,
#77348,#77349,#77350,#77351,#77352,#77353,#77354,#77355,#77356,#77357,#77358,
#77359,#77360,#77361,#77362,#77363,#77364,#77365,#77366,#77367,#77368,#77369,
#77370,#77371,#77372,#77373,#77374,#77375,#77376,#77377,#77378,#77379,#77380,
#77381,#77382,#77383,#77384,#77385,#77386,#77387,#77388,#77389,#77390,#77391,
#77392,#77393,#77394,#77395,#77396,#77397,#77398,#77399,#77400,#77401,#77402,
#77403,#77404,#77405,#77406,#77407,#77408,#77409,#77410,#77411,#77412,#77413,
#77414,#77415,#77416,#77417,#77418,#77419,#77420,#77421,#77422,#77423,#77424,
#77425,#77426,#77427,#77428,#77429,#77430,#77431,#77432,#77433,#77434,#77435,
#77436,#77437,#77438,#77439,#77440,#77441,#77442,#77443,#77444,#77445,#77446,
#77447,#77448,#77449,#77450,#77451,#77452,#77453,#77454,#77455,#77456,#77457,
#77458,#77459,#77460,#77461,#77462,#77463,#77464,#77465,#77466,#77467,#77468,
#77469,#77470,#77471,#77472,#77473,#77474,#77475,#77476,#77477,#77478,#77479,
#77480,#77481,#77482,#77483,#77484,#77485,#77486,#77487,#77488,#77489,#77490,
#77491,#77492,#77493,#77494,#77495,#77496,#77497,#77498,#77499,#77500,#77501,
#77502,#77503,#77504,#77505,#77506,#77507,#77508,#77509,#77510,#77511,#77512,
#77513,#77514,#77515,#77516,#77517,#77518,#77519,#77520,#77521,#77522,#77523,
#77524,#77525,#77526,#77527,#77528,#77529,#77530,#77531,#77532,#77533,#77534,
#77535,#77536,#77537,#77538,#77539,#77540,#77541,#77542,#77543,#77544,#77545,
#77546,#77547,#77548,#77549,#77550,#77551,#77552,#77553,#77554,#77555,#77556,
#77557,#77558,#77559,#77560,#77561,#77562,#77563,#77564,#77565,#77566,#77567,
#77568,#77569,#77570,#77571,#77572,#77573,#77574,#77575,#77576,#77577,#77578,
#77579,#77580,#77581,#77582,#77583,#77584,#77585,#77586,#77587,#77588,#77589,
#77590,#77591,#77592,#77593,#77594,#77595,#77596,#77597,#77598,#77599,#77600,
#77601,#77602,#77603,#77604,#77605,#77606,#77607,#77608,#77609,#77610,#77611,
#77612,#77613,#77614,#77615,#77616,#77617,#77618,#77619,#77620,#77621,#77622,
#77623,#77624,#77625,#77626,#77627,#77628,#77629,#77630,#77631,#77632,#77633,
#77634,#77635,#77636,#77637,#77638,#77639,#77640,#77641,#77642,#77643,#77644,
#77645,#77646),(#77647,#77648,#77649,#77650,#77651,#77652,#77653,#77654,
#77655,#77656,#77657,#77658,#77659,#77660,#77661,#77662,#77663,#77664,#77665,
#77666,#77667,#77668,#77669,#77670,#77671,#77672,#77673,#77674,#77675,#77676,
#77677,#77678,#77679,#77680,#77681,#77682,#77683,#77684,#77685,#77686,#77687,
#77688,#77689,#77690,#77691,#77692,#77693,#77694,#77695,#77696,#77697,#77698,
#77699,#77700,#77701,#77702,#77703,#77704,#77705,#77706,#77707,#77708,#77709,
#77710,#77711,#77712,#77713,#77714,#77715,#77716,#77717,#77718,#77719,#77720,
#77721,#77722,#77723,#77724,#77725,#77726,#77727,#77728,#77729,#77730,#77731,
#77732,#77733,#77734,#77735,#77736,#77737,#77738,#77739,#77740,#77741,#77742,
#77743,#77744,#77745,#77746,#77747,#77748,#77749,#77750,#77751,#77752,#77753,
#77754,#77755,#77756,#77757,#77758,#77759,#77760,#77761,#77762,#77763,#77764,
#77765,#77766,#77767,#77768,#77769,#77770,#77771,#77772,#77773,#77774,#77775,
#77776,#77777,#77778,#77779,#77780,#77781,#77782,#77783,#77784,#77785,#77786,
#77787,#77788,#77789,#77790,#77791,#77792,#77793,#77794,#77795,#77796,#77797,
#77798,#77799,#77800,#77801,#77802,#77803,#77804,#77805,#77806,#77807,#77808,
#77809,#77810,#77811,#77812,#77813,#77814,#77815,#77816,#77817,#77818,#77819,
#77820,#77821,#77822,#77823,#77824,#77825,#77826,#77827,#77828,#77829,#77830,
#77831,#77832,#77833,#77834,#77835,#77836,#77837,#77838,#77839,#77840,#77841,
#77842,#77843,#77844,#77845,#77846,#77847,#77848,#77849,#77850,#77851,#77852,
#77853,#77854,#77855,#77856,#77857,#77858,#77859,#77860,#77861,#77862,#77863,
#77864,#77865,#77866,#77867,#77868,#77869,#77870,#77871,#77872,#77873,#77874,
#77875,#77876,#77877,#77878,#77879,#77880,#77881,#77882,#77883,#77884,#77885,
#77886,#77887,#77888,#77889,#77890,#77891,#77892,#77893,#77894,#77895,#77896,
#77897,#77898,#77899,#77900,#77901,#77902,#77903,#77904,#77905,#77906,#77907,
#77908,#77909,#77910,#77911,#77912,#77913,#77914,#77915,#77916,#77917,#77918,
#77919,#77920,#77921,#77922,#77923,#77924,#77925,#77926,#77927,#77928,#77929,
#77930,#77931,#77932,#77933,#77934,#77935,#77936,#77937,#77938,#77939,#77940,
#77941,#77942,#77943,#77944,#77945,#77946,#77947,#77948,#77949,#77950,#77951,
#77952,#77953,#77954,#77955,#77956,#77957,#77958,#77959,#77960,#77961,#77962,
#77963,#77964,#77965,#77966,#77967,#77968,#77969,#77970,#77971,#77972,#77973,
#77974,#77975,#77976,#77977,#77978,#77979,#77980,#77981,#77982,#77983,#77984,
#77985,#77986,#77987,#77988,#77989,#77990,#77991,#77992,#77993,#77994,#77995,
#77996,#77997,#77998,#77999,#78000,#78001,#78002,#78003,#78004,#78005,#78006,
#78007,#78008,#78009,#78010,#78011,#78012,#78013,#78014,#78015,#78016,#78017,
#78018,#78019,#78020,#78021,#78022,#78023,#78024,#78025,#78026,#78027,#78028,
#78029,#78030,#78031,#78032,#78033,#78034,#78035,#78036,#78037,#78038,#78039,
#78040,#78041,#78042,#78043,#78044,#78045,#78046,#78047,#78048,#78049,#78050,
#78051,#78052,#78053,#78054,#78055,#78056,#78057,#78058,#78059,#78060,#78061,
#78062,#78063,#78064,#78065,#78066,#78067,#78068,#78069,#78070,#78071,#78072,
#78073,#78074,#78075,#78076,#78077,#78078,#78079,#78080,#78081,#78082,#78083,
#78084,#78085,#78086,#78087,#78088,#78089,#78090,#78091,#78092,#78093,#78094,
#78095,#78096,#78097,#78098,#78099,#78100,#78101,#78102,#78103,#78104,#78105,
#78106,#78107,#78108,#78109,#78110,#78111,#78112,#78113,#78114,#78115,#78116,
#78117,#78118,#78119,#78120,#78121,#78122,#78123,#78124,#78125,#78126,#78127,
#78128,#78129,#78130,#78131,#78132,#78133,#78134,#78135,#78136,#78137,#78138,
#78139,#78140,#78141,#78142,#78143,#78144,#78145,#78146,#78147,#78148,#78149,
#78150,#78151,#78152,#78153,#78154,#78155,#78156,#78157,#78158,#78159,#78160,
#78161,#78162,#78163,#78164,#78165,#78166,#78167,#78168,#78169,#78170,#78171,
#78172,#78173,#78174,#78175,#78176,#78177,#78178,#78179,#78180,#78181,#78182,
#78183,#78184,#78185,#78186,#78187,#78188,#78189,#78190,#78191,#78192),
(#78193,#78194,#78195,#78196,#78197,#78198,#78199,#78200,#78201,#78202,
#78203,#78204,#78205,#78206,#78207,#78208,#78209,#78210,#78211,#78212,#78213,
#78214,#78215,#78216,#78217,#78218,#78219,#78220,#78221,#78222,#78223,#78224,
#78225,#78226,#78227,#78228,#78229,#78230,#78231,#78232,#78233,#78234,#78235,
#78236,#78237,#78238,#78239,#78240,#78241,#78242,#78243,#78244,#78245,#78246,
#78247,#78248,#78249,#78250,#78251,#78252,#78253,#78254,#78255,#78256,#78257,
#78258,#78259,#78260,#78261,#78262,#78263,#78264,#78265,#78266,#78267,#78268,
#78269,#78270,#78271,#78272,#78273,#78274,#78275,#78276,#78277,#78278,#78279,
#78280,#78281,#78282,#78283,#78284,#78285,#78286,#78287,#78288,#78289,#78290,
#78291,#78292,#78293,#78294,#78295,#78296,#78297,#78298,#78299,#78300,#78301,
#78302,#78303,#78304,#78305,#78306,#78307,#78308,#78309,#78310,#78311,#78312,
#78313,#78314,#78315,#78316,#78317,#78318,#78319,#78320,#78321,#78322,#78323,
#78324,#78325,#78326,#78327,#78328,#78329,#78330,#78331,#78332,#78333,#78334,
#78335,#78336,#78337,#78338,#78339,#78340,#78341,#78342,#78343,#78344,#78345,
#78346,#78347,#78348,#78349,#78350,#78351,#78352,#78353,#78354,#78355,#78356,
#78357,#78358,#78359,#78360,#78361,#78362,#78363,#78364,#78365,#78366,#78367,
#78368,#78369,#78370,#78371,#78372,#78373,#78374,#78375,#78376,#78377,#78378,
#78379,#78380,#78381,#78382,#78383,#78384,#78385,#78386,#78387,#78388,#78389,
#78390,#78391,#78392,#78393,#78394,#78395,#78396,#78397,#78398,#78399,#78400,
#78401,#78402,#78403,#78404,#78405,#78406,#78407,#78408,#78409,#78410,#78411,
#78412,#78413,#78414,#78415,#78416,#78417,#78418,#78419,#78420,#78421,#78422,
#78423,#78424,#78425,#78426,#78427,#78428,#78429,#78430,#78431,#78432,#78433,
#78434,#78435,#78436,#78437,#78438,#78439,#78440,#78441,#78442,#78443,#78444,
#78445,#78446,#78447,#78448,#78449,#78450,#78451,#78452,#78453,#78454,#78455,
#78456,#78457,#78458,#78459,#78460,#78461,#78462,#78463,#78464,#78465,#78466,
#78467,#78468,#78469,#78470,#78471,#78472,#78473,#78474,#78475,#78476,#78477,
#78478,#78479,#78480,#78481,#78482,#78483,#78484,#78485,#78486,#78487,#78488,
#78489,#78490,#78491,#78492,#78493,#78494,#78495,#78496,#78497,#78498,#78499,
#78500,#78501,#78502,#78503,#78504,#78505,#78506,#78507,#78508,#78509,#78510,
#78511,#78512,#78513,#78514,#78515,#78516,#78517,#78518,#78519,#78520,#78521,
#78522,#78523,#78524,#78525,#78526,#78527,#78528,#78529,#78530,#78531,#78532,
#78533,#78534,#78535,#78536,#78537,#78538,#78539,#78540,#78541,#78542,#78543,
#78544,#78545,#78546,#78547,#78548,#78549,#78550,#78551,#78552,#78553,#78554,
#78555,#78556,#78557,#78558,#78559,#78560,#78561,#78562,#78563,#78564,#78565,
#78566,#78567,#78568,#78569,#78570,#78571,#78572,#78573,#78574,#78575,#78576,
#78577,#78578,#78579,#78580,#78581,#78582,#78583,#78584,#78585,#78586,#78587,
#78588,#78589,#78590,#78591,#78592,#78593,#78594,#78595,#78596,#78597,#78598,
#78599,#78600,#78601,#78602,#78603,#78604,#78605,#78606,#78607,#78608,#78609,
#78610,#78611,#78612,#78613,#78614,#78615,#78616,#78617,#78618,#78619,#78620,
#78621,#78622,#78623,#78624,#78625,#78626,#78627,#78628,#78629,#78630,#78631,
#78632,#78633,#78634,#78635,#78636,#78637,#78638,#78639,#78640,#78641,#78642,
#78643,#78644,#78645,#78646,#78647,#78648,#78649,#78650,#78651,#78652,#78653,
#78654,#78655,#78656,#78657,#78658,#78659,#78660,#78661,#78662,#78663,#78664,
#78665,#78666,#78667,#78668,#78669,#78670,#78671,#78672,#78673,#78674,#78675,
#78676,#78677,#78678,#78679,#78680,#78681,#78682,#78683,#78684,#78685,#78686,
#78687,#78688,#78689,#78690,#78691,#78692,#78693,#78694,#78695,#78696,#78697,
#78698,#78699,#78700,#78701,#78702,#78703,#78704,#78705,#78706,#78707,#78708,
#78709,#78710,#78711,#78712,#78713,#78714,#78715,#78716,#78717,#78718,#78719,
#78720,#78721,#78722,#78723,#78724,#78725,#78726,#78727,#78728,#78729,#78730,
#78731,#78732,#78733,#78734,#78735,#78736,#78737,#78738),(#78739,#78740,
#78741,#78742,#78743,#78744,#78745,#78746,#78747,#78748,#78749,#78750,#78751,
#78752,#78753,#78754,#78755,#78756,#78757,#78758,#78759,#78760,#78761,#78762,
#78763,#78764,#78765,#78766,#78767,#78768,#78769,#78770,#78771,#78772,#78773,
#78774,#78775,#78776,#78777,#78778,#78779,#78780,#78781,#78782,#78783,#78784,
#78785,#78786,#78787,#78788,#78789,#78790,#78791,#78792,#78793,#78794,#78795,
#78796,#78797,#78798,#78799,#78800,#78801,#78802,#78803,#78804,#78805,#78806,
#78807,#78808,#78809,#78810,#78811,#78812,#78813,#78814,#78815,#78816,#78817,
#78818,#78819,#78820,#78821,#78822,#78823,#78824,#78825,#78826,#78827,#78828,
#78829,#78830,#78831,#78832,#78833,#78834,#78835,#78836,#78837,#78838,#78839,
#78840,#78841,#78842,#78843,#78844,#78845,#78846,#78847,#78848,#78849,#78850,
#78851,#78852,#78853,#78854,#78855,#78856,#78857,#78858,#78859,#78860,#78861,
#78862,#78863,#78864,#78865,#78866,#78867,#78868,#78869,#78870,#78871,#78872,
#78873,#78874,#78875,#78876,#78877,#78878,#78879,#78880,#78881,#78882,#78883,
#78884,#78885,#78886,#78887,#78888,#78889,#78890,#78891,#78892,#78893,#78894,
#78895,#78896,#78897,#78898,#78899,#78900,#78901,#78902,#78903,#78904,#78905,
#78906,#78907,#78908,#78909,#78910,#78911,#78912,#78913,#78914,#78915,#78916,
#78917,#78918,#78919,#78920,#78921,#78922,#78923,#78924,#78925,#78926,#78927,
#78928,#78929,#78930,#78931,#78932,#78933,#78934,#78935,#78936,#78937,#78938,
#78939,#78940,#78941,#78942,#78943,#78944,#78945,#78946,#78947,#78948,#78949,
#78950,#78951,#78952,#78953,#78954,#78955,#78956,#78957,#78958,#78959,#78960,
#78961,#78962,#78963,#78964,#78965,#78966,#78967,#78968,#78969,#78970,#78971,
#78972,#78973,#78974,#78975,#78976,#78977,#78978,#78979,#78980,#78981,#78982,
#78983,#78984,#78985,#78986,#78987,#78988,#78989,#78990,#78991,#78992,#78993,
#78994,#78995,#78996,#78997,#78998,#78999,#79000,#79001,#79002,#79003,#79004,
#79005,#79006,#79007,#79008,#79009,#79010,#79011,#79012,#79013,#79014,#79015,
#79016,#79017,#79018,#79019,#79020,#79021,#79022,#79023,#79024,#79025,#79026,
#79027,#79028,#79029,#79030,#79031,#79032,#79033,#79034,#79035,#79036,#79037,
#79038,#79039,#79040,#79041,#79042,#79043,#79044,#79045,#79046,#79047,#79048,
#79049,#79050,#79051,#79052,#79053,#79054,#79055,#79056,#79057,#79058,#79059,
#79060,#79061,#79062,#79063,#79064,#79065,#79066,#79067,#79068,#79069,#79070,
#79071,#79072,#79073,#79074,#79075,#79076,#79077,#79078,#79079,#79080,#79081,
#79082,#79083,#79084,#79085,#79086,#79087,#79088,#79089,#79090,#79091,#79092,
#79093,#79094,#79095,#79096,#79097,#79098,#79099,#79100,#79101,#79102,#79103,
#79104,#79105,#79106,#79107,#79108,#79109,#79110,#79111,#79112,#79113,#79114,
#79115,#79116,#79117,#79118,#79119,#79120,#79121,#79122,#79123,#79124,#79125,
#79126,#79127,#79128,#79129,#79130,#79131,#79132,#79133,#79134,#79135,#79136,
#79137,#79138,#79139,#79140,#79141,#79142,#79143,#79144,#79145,#79146,#79147,
#79148,#79149,#79150,#79151,#79152,#79153,#79154,#79155,#79156,#79157,#79158,
#79159,#79160,#79161,#79162,#79163,#79164,#79165,#79166,#79167,#79168,#79169,
#79170,#79171,#79172,#79173,#79174,#79175,#79176,#79177,#79178,#79179,#79180,
#79181,#79182,#79183,#79184,#79185,#79186,#79187,#79188,#79189,#79190,#79191,
#79192,#79193,#79194,#79195,#79196,#79197,#79198,#79199,#79200,#79201,#79202,
#79203,#79204,#79205,#79206,#79207,#79208,#79209,#79210,#79211,#79212,#79213,
#79214,#79215,#79216,#79217,#79218,#79219,#79220,#79221,#79222,#79223,#79224,
#79225,#79226,#79227,#79228,#79229,#79230,#79231,#79232,#79233,#79234,#79235,
#79236,#79237,#79238,#79239,#79240,#79241,#79242,#79243,#79244,#79245,#79246,
#79247,#79248,#79249,#79250,#79251,#79252,#79253,#79254,#79255,#79256,#79257,
#79258,#79259,#79260,#79261,#79262,#79263,#79264,#79265,#79266,#79267,#79268,
#79269,#79270,#79271,#79272,#79273,#79274,#79275,#79276,#79277,#79278,#79279,
#79280,#79281,#79282,#79283,#79284)),.UNSPECIFIED.,.F.,.F.,.F.,(4,4),(4,
1,1,1,1,1,1,1,1,1,1,1,1,1,1,1,1,1,1,1,1,1,1,1,1,1,1,1,1,1,1,1,1,1,1,1,1,
1,1,1,1,1,1,1,1,1,1,1,1,1,1,1,1,1,1,1,1,1,1,1,1,1,1,1,1,1,1,1,1,1,1,1,1,
1,1,1,1,1,1,1,1,1,1,1,1,1,1,1,1,1,1,1,1,1,1,1,1,1,1,1,1,1,1,1,1,1,1,1,1,
1,1,1,1,1,1,1,1,1,1,1,1,1,1,1,1,1,1,1,1,1,1,1,1,1,1,1,1,1,1,1,1,1,1,1,1,
1,1,1,1,1,1,1,1,1,1,1,1,1,1,1,1,1,1,1,1,1,1,1,1,1,1,1,1,1,1,1,1,1,1,1,1,
1,1,1,1,1,1,1,1,1,1,1,1,1,1,1,1,1,1,1,1,1,1,1,1,1,1,1,1,1,1,1,1,1,1,1,1,
1,1,1,1,1,1,1,1,1,1,1,1,1,1,1,1,1,1,1,1,1,1,1,1,1,1,1,1,1,1,1,1,1,1,1,1,
1,1,1,1,1,1,1,1,1,1,1,1,1,1,1,1,1,1,1,1,1,1,1,1,1,1,1,1,1,1,1,1,1,1,1,1,
1,1,1,1,1,1,1,1,1,1,1,1,1,1,1,1,1,1,1,1,1,1,1,1,1,1,1,1,1,1,1,1,1,1,1,1,
1,1,1,1,1,1,1,1,1,1,1,1,1,1,1,1,1,1,1,1,1,1,1,1,1,1,1,1,1,1,1,1,1,1,1,1,
1,1,1,1,1,1,1,1,1,1,1,1,1,1,1,1,1,1,1,1,1,1,1,1,1,1,1,1,1,1,1,1,1,1,1,1,
1,1,1,1,1,1,1,1,1,1,1,1,1,1,1,1,1,1,1,1,1,1,1,1,1,1,1,1,1,1,1,1,1,1,1,1,
1,1,1,1,1,1,1,1,1,1,1,1,1,1,1,1,1,1,1,1,1,1,1,1,1,1,1,1,1,1,1,1,1,1,1,1,
1,1,1,1,1,1,1,1,1,1,1,1,1,1,1,1,1,1,1,1,1,1,1,1,1,1,1,1,1,1,1,1,1,1,1,1,
1,1,1,1,1,1,1,1,1,1,1,1,1,1,1,1,1,1,1,1,1,1,1,1,1,1,1,1,1,1,1,1,1,1,1,1,
1,1,4),(-0.000633646794057276,0.135400040464203),(8.30104353460145,8.79990044528941,
9.29867163595186,9.7974428266143,10.2962140172767,11.2937563986016,12.2912987799265,
13.2888411612514,13.7876123519139,14.2863835425763,14.7851547332388,15.2839259239012,
16.2814683052261,16.7802394958886,17.279010686551,18.2765530678759,19.2740954492008,
20.2716378305257,20.7704090211881,21.2691802118506,21.767951402513,22.2667225931755,
23.2642649745004,23.7630361651628,24.2618073558252,25.2593497371501,26.256892118475,
27.2544344997999,27.7532056904624,28.2519768811248,28.7507480717873,29.2495192624497,
30.2470616437746,30.745832834437,31.2446040250995,32.2421464064244,33.2396887877493,
34.2372311690742,34.7360023597366,35.2347735503991,35.7335447410615,36.232315931724,
37.2298583130489,37.7286295037113,38.2274006943737,39.2249430756986,40.2224854570235,
41.2200278383484,41.7187990290109,42.2175702196733,42.7163414103358,43.2151126009982,
44.2126549823231,44.7114261729855,45.210197363648,46.2077397449729,47.2052821262978,
48.2028245076227,48.7015956982851,49.2003668889476,49.69913807961,50.1979092702725,
51.1954516515974,51.6942228422598,52.1929940329222,53.1905364142471,54.188078795572,
55.1856211768969,55.6843923675594,56.1831635582218,56.6819347488843,57.1807059395467,
58.1782483208716,58.677019511534,59.1757907021965,60.1733330835214,61.1708754648463,
62.1684178461712,62.6671890368336,63.1659602274961,63.6647314181585,64.1635026088209,
65.1610449901458,65.6598161808083,66.1585873714707,67.1561297527956,68.1536721341205,
69.1512145154454,69.6499857061079,70.1487568967703,70.6475280874328,71.1462992780952,
72.1438416594201,72.6426128500825,73.141384040745,74.1389264220699,75.1364688033948,
76.1340111847197,76.6327823753821,77.1315535660446,77.630324756707,78.1290959473694,
79.1266383286943,79.6254095193568,80.1241807100192,81.1217230913441,82.119265472669,
83.1168078539939,83.6155790446564,84.1143502353188,84.6131214259813,85.1118926166437,
86.1094349979686,86.608206188631,87.1069773792935,88.1045197606184,89.1020621419433,
90.0996045232682,90.5983757139306,91.097146904593,91.5959180952555,92.0946892859179,
93.0922316672428,93.5910028579053,94.0897740485677,95.0873164298926,96.0848588112175,
97.0824011925424,97.5811723832049,98.0799435738673,98.5787147645297,99.0774859551922,
100.075028336517,100.57379952718,101.072570717842,102.070113099167,103.067655480492,
104.065197861817,104.563969052479,105.062740243142,105.561511433804,106.060282624466,
107.057825005791,107.556596196454,108.055367387116,109.052909768441,110.050452149766,
111.047994531091,111.546765721753,112.045536912416,112.544308103078,113.043079293741,
114.040621675066,114.539392865728,115.03816405639,116.035706437715,117.03324881904,
118.030791200365,118.529562391028,119.02833358169,119.527104772352,120.025875963015,
121.02341834434,121.522189535002,122.020960725665,123.01850310699,124.016045488315,
125.013587869639,125.512359060302,126.011130250964,126.509901441627,127.008672632289,
128.006215013614,128.504986204277,129.003757394939,130.001299776264,130.998842157589,
131.996384538914,132.495155729576,132.993926920239,133.492698110901,133.991469301563,
134.989011682888,135.487782873551,135.986554064213,136.984096445538,137.981638826863,
138.979181208188,139.47795239885,139.976723589513,140.475494780175,140.974265970838,
141.971808352163,142.470579542825,142.969350733487,143.966893114812,144.964435496137,
145.961977877462,146.460749068125,146.959520258787,147.45829144945,147.957062640112,
148.954605021437,149.453376212099,149.952147402762,150.949689784087,151.947232165412,
152.944774546736,153.443545737399,153.942316928061,154.441088118724,154.939859309386,
155.937401690711,156.436172881374,156.934944072036,157.932486453361,158.930028834686,
159.927571216011,160.426342406673,160.925113597336,161.423884787998,161.92265597866,
162.920198359985,163.418969550648,163.91774074131,164.915283122635,165.91282550396,
166.910367885285,167.409139075947,167.90791026661,168.406681457272,168.905452647935,
169.90299502926,170.401766219922,170.900537410584,171.898079791909,172.895622173234,
173.893164554559,174.391935745222,174.890706935884,175.389478126546,175.888249317209,
176.885791698534,177.384562889196,177.883334079859,178.880876461184,179.878418842509,
180.875961223833,181.374732414496,181.873503605158,182.372274795821,182.871045986483,
183.868588367808,184.367359558471,184.866130749133,185.863673130458,186.861215511783,
187.858757893108,188.35752908377,188.856300274433,189.355071465095,189.853842655757,
190.851385037082,191.350156227745,191.848927418407,192.846469799732,193.844012181057,
194.841554562382,195.340325753044,195.839096943707,196.337868134369,196.836639325032,
197.834181706357,198.332952897019,198.831724087681,199.829266469006,200.826808850331,
201.824351231656,202.821893612981,203.819435994306,204.318207184968,204.816978375631,
205.814520756956,206.313291947618,206.812063138281,207.310834328943,207.809605519605,
208.80714790093,209.804690282255,210.80223266358,211.301003854243,211.799775044905,
212.79731742623,213.296088616892,213.794859807555,214.293630998217,214.79240218888,
215.789944570205,216.78748695153,217.785029332854,218.283800523517,218.782571714179,
219.780114095504,220.278885286167,220.777656476829,221.276427667492,221.775198858154,
222.772741239479,223.770283620804,224.767826002129,225.266597192791,225.765368383454,
226.762910764778,227.261681955441,227.760453146103,228.259224336766,228.757995527428,
229.755537908753,230.753080290078,231.750622671403,232.249393862065,232.748165052728,
233.745707434053,234.244478624715,234.743249815378,235.24202100604,235.740792196703,
236.738334578027,237.735876959352,238.733419340677,239.23219053134,239.730961722002,
240.728504103327,241.227275293989,241.726046484652,242.224817675314,242.723588865977,
243.721131247302,244.718673628627,245.716216009951,246.214987200614,246.713758391276,
247.711300772601,248.210071963264,248.708843153926,249.207614344589,249.706385535251,
250.703927916576,251.701470297901,252.699012679226,253.197783869888,253.696555060551,
254.694097441875,255.192868632538,255.6916398232,256.190411013863,256.689182204525,
257.68672458585,258.684266967175,259.6818093485,260.180580539162,260.679351729825,
261.67689411115,262.175665301812,262.674436492475,263.173207683137,263.6719788738,
264.669521255124,265.667063636449,266.664606017774,267.163377208437,267.662148399099,
268.659690780424,269.158461971086,269.657233161749,270.156004352411,270.654775543074,
271.652317924399,272.649860305724,273.647402687048,274.146173877711,274.644945068373,
275.642487449698,276.141258640361,276.640029831023,277.138801021686,277.637572212348,
278.635114593673,279.632656974998,280.630199356323,281.128970546985,281.627741737648,
282.625284118972,283.124055309635,283.622826500297,284.12159769096,284.620368881622,
285.617911262947,286.615453644272,287.612996025597,288.111767216259,288.610538406922,
289.608080788247,290.106851978909,290.605623169572,291.104394360234,291.603165550897,
292.600707932221,293.598250313546,294.595792694871,295.094563885534,295.593335076196,
296.590877457521,297.089648648183,297.588419838846,298.087191029508,298.585962220171,
299.583504601496,300.581046982821,301.578589364145,302.077360554808,302.57613174547,
303.573674126795,304.072445317458,304.57121650812,305.069987698783,305.568758889445,
306.56630127077,307.563843652095,308.56138603342,309.060157224082,309.558928414745,
310.556470796069,311.055241986732,311.554013177394,312.052784368057,312.551555558719,
313.549097940044,314.546640321369,315.544182702694,316.042953893356,316.541725084019,
317.539267465344,318.038038656006,318.536809846669,319.035581037331,319.534352227994,
320.531894609318,321.529436990643,322.526979371968,323.025750562631,323.524521753293,
324.522064134618,325.02083532528,325.519606515943,326.018377706605,326.517148897268,
327.514691278593,328.512233659918,329.509776041242,330.008547231905,330.507318422567,
331.504860803892,332.003631994555,332.502403185217,333.00117437588,333.499945566542,
334.497487947867,335.495030329192,336.492572710517,336.991343901179,337.490115091842,
338.487657473166,338.986428663829,339.485199854491,339.983971045154,340.482742235816,
341.480284617141,342.477826998466,343.475369379791,343.974140570453,344.472911761116,
345.470454142441,345.969225333103,346.467996523766,346.966767714428,347.465538905091,
348.463081286415,349.46062366774,350.458166049065,350.956937239728,351.45570843039,
352.453250811715,352.952022002377,353.45079319304,353.949564383702,354.448335574365,
355.44587795569,356.443420337015,357.440962718339,357.939733909002,358.438505099664,
359.436047480989,359.934818671652,360.433589862314,360.932361052977,361.431132243639,
362.428674624964,363.426217006289,364.423759387614,364.922530578276,365.421301768939,
366.418844150263,366.917615340926,367.416386531588,367.915157722251,368.413928912913,
369.411471294238,370.409013675563,371.406556056888,371.90532724755,372.404098438213,
373.401640819538,373.9004120102,374.399183200863,374.897954391525,375.396725582188,
376.394267963512,377.391810344837,378.389352726162,378.888123916825,379.386895107487,
380.384437488812,380.883208679474,381.381979870137,381.880751060799,382.379522251462,
383.377064632787,384.374607014112,385.372149395436,385.870920586099,386.369691776761,
386.868462967424,387.367297249874),.UNSPECIFIED.);
#757=B_SPLINE_SURFACE_WITH_KNOTS('',3,3,((#79509,#79510,#79511,#79512,#79513,
#79514,#79515,#79516,#79517,#79518,#79519,#79520,#79521,#79522,#79523,#79524,
#79525,#79526,#79527,#79528,#79529,#79530,#79531,#79532,#79533,#79534,#79535,
#79536,#79537,#79538,#79539,#79540,#79541,#79542,#79543,#79544,#79545,#79546,
#79547,#79548,#79549,#79550,#79551,#79552,#79553,#79554,#79555,#79556,#79557,
#79558,#79559,#79560,#79561,#79562,#79563,#79564,#79565,#79566,#79567,#79568,
#79569,#79570,#79571,#79572,#79573,#79574,#79575,#79576,#79577,#79578,#79579,
#79580,#79581,#79582,#79583,#79584,#79585,#79586,#79587,#79588,#79589,#79590,
#79591,#79592,#79593,#79594,#79595,#79596,#79597,#79598,#79599,#79600,#79601,
#79602,#79603,#79604,#79605,#79606,#79607,#79608,#79609,#79610,#79611,#79612,
#79613,#79614,#79615,#79616,#79617,#79618,#79619,#79620,#79621,#79622,#79623,
#79624,#79625,#79626,#79627,#79628,#79629,#79630,#79631,#79632,#79633,#79634,
#79635,#79636,#79637,#79638,#79639,#79640,#79641,#79642,#79643,#79644,#79645,
#79646,#79647,#79648,#79649,#79650,#79651,#79652,#79653,#79654,#79655,#79656,
#79657,#79658,#79659,#79660,#79661,#79662,#79663,#79664,#79665,#79666,#79667,
#79668,#79669,#79670,#79671,#79672,#79673,#79674,#79675,#79676,#79677,#79678,
#79679,#79680,#79681,#79682,#79683,#79684,#79685,#79686,#79687,#79688,#79689,
#79690,#79691,#79692,#79693,#79694,#79695,#79696,#79697,#79698,#79699,#79700,
#79701,#79702,#79703,#79704,#79705,#79706,#79707,#79708,#79709,#79710,#79711,
#79712,#79713,#79714,#79715,#79716,#79717,#79718,#79719,#79720,#79721,#79722,
#79723,#79724,#79725,#79726,#79727,#79728,#79729,#79730,#79731,#79732,#79733,
#79734,#79735,#79736,#79737,#79738,#79739,#79740,#79741,#79742,#79743,#79744,
#79745,#79746,#79747,#79748,#79749,#79750,#79751,#79752,#79753,#79754,#79755,
#79756,#79757,#79758,#79759,#79760,#79761,#79762,#79763,#79764,#79765,#79766,
#79767,#79768,#79769,#79770,#79771,#79772,#79773,#79774,#79775,#79776,#79777,
#79778,#79779,#79780,#79781,#79782,#79783,#79784,#79785,#79786,#79787,#79788,
#79789,#79790,#79791,#79792,#79793,#79794,#79795,#79796,#79797,#79798,#79799,
#79800,#79801,#79802,#79803,#79804,#79805,#79806,#79807,#79808,#79809,#79810,
#79811,#79812,#79813,#79814,#79815,#79816,#79817,#79818,#79819,#79820,#79821,
#79822,#79823,#79824,#79825,#79826,#79827,#79828,#79829,#79830,#79831,#79832,
#79833,#79834,#79835,#79836,#79837,#79838,#79839,#79840,#79841,#79842,#79843,
#79844,#79845,#79846,#79847,#79848,#79849,#79850,#79851,#79852,#79853,#79854,
#79855,#79856,#79857,#79858,#79859,#79860,#79861,#79862,#79863,#79864,#79865,
#79866,#79867,#79868,#79869,#79870,#79871,#79872,#79873,#79874,#79875,#79876,
#79877,#79878,#79879,#79880,#79881,#79882,#79883,#79884,#79885,#79886,#79887,
#79888,#79889,#79890,#79891,#79892,#79893,#79894,#79895,#79896,#79897,#79898,
#79899,#79900,#79901,#79902,#79903,#79904,#79905,#79906,#79907,#79908,#79909,
#79910,#79911,#79912,#79913,#79914,#79915,#79916,#79917,#79918,#79919,#79920,
#79921,#79922,#79923,#79924,#79925,#79926,#79927,#79928,#79929,#79930,#79931,
#79932,#79933,#79934,#79935,#79936,#79937,#79938,#79939,#79940,#79941,#79942,
#79943,#79944,#79945,#79946,#79947,#79948,#79949,#79950,#79951,#79952,#79953,
#79954,#79955,#79956,#79957,#79958,#79959,#79960,#79961,#79962,#79963,#79964,
#79965,#79966,#79967,#79968,#79969,#79970,#79971,#79972,#79973,#79974,#79975,
#79976,#79977,#79978,#79979,#79980,#79981,#79982,#79983,#79984,#79985,#79986,
#79987,#79988,#79989,#79990,#79991,#79992,#79993,#79994,#79995,#79996,#79997,
#79998,#79999,#80000,#80001,#80002,#80003,#80004,#80005,#80006,#80007,#80008,
#80009,#80010,#80011,#80012,#80013,#80014,#80015,#80016,#80017,#80018,#80019,
#80020,#80021,#80022,#80023,#80024,#80025,#80026,#80027,#80028,#80029,#80030,
#80031,#80032,#80033,#80034,#80035,#80036,#80037,#80038,#80039,#80040,#80041,
#80042,#80043,#80044,#80045,#80046,#80047,#80048,#80049,#80050,#80051,#80052,
#80053,#80054),(#80055,#80056,#80057,#80058,#80059,#80060,#80061,#80062,
#80063,#80064,#80065,#80066,#80067,#80068,#80069,#80070,#80071,#80072,#80073,
#80074,#80075,#80076,#80077,#80078,#80079,#80080,#80081,#80082,#80083,#80084,
#80085,#80086,#80087,#80088,#80089,#80090,#80091,#80092,#80093,#80094,#80095,
#80096,#80097,#80098,#80099,#80100,#80101,#80102,#80103,#80104,#80105,#80106,
#80107,#80108,#80109,#80110,#80111,#80112,#80113,#80114,#80115,#80116,#80117,
#80118,#80119,#80120,#80121,#80122,#80123,#80124,#80125,#80126,#80127,#80128,
#80129,#80130,#80131,#80132,#80133,#80134,#80135,#80136,#80137,#80138,#80139,
#80140,#80141,#80142,#80143,#80144,#80145,#80146,#80147,#80148,#80149,#80150,
#80151,#80152,#80153,#80154,#80155,#80156,#80157,#80158,#80159,#80160,#80161,
#80162,#80163,#80164,#80165,#80166,#80167,#80168,#80169,#80170,#80171,#80172,
#80173,#80174,#80175,#80176,#80177,#80178,#80179,#80180,#80181,#80182,#80183,
#80184,#80185,#80186,#80187,#80188,#80189,#80190,#80191,#80192,#80193,#80194,
#80195,#80196,#80197,#80198,#80199,#80200,#80201,#80202,#80203,#80204,#80205,
#80206,#80207,#80208,#80209,#80210,#80211,#80212,#80213,#80214,#80215,#80216,
#80217,#80218,#80219,#80220,#80221,#80222,#80223,#80224,#80225,#80226,#80227,
#80228,#80229,#80230,#80231,#80232,#80233,#80234,#80235,#80236,#80237,#80238,
#80239,#80240,#80241,#80242,#80243,#80244,#80245,#80246,#80247,#80248,#80249,
#80250,#80251,#80252,#80253,#80254,#80255,#80256,#80257,#80258,#80259,#80260,
#80261,#80262,#80263,#80264,#80265,#80266,#80267,#80268,#80269,#80270,#80271,
#80272,#80273,#80274,#80275,#80276,#80277,#80278,#80279,#80280,#80281,#80282,
#80283,#80284,#80285,#80286,#80287,#80288,#80289,#80290,#80291,#80292,#80293,
#80294,#80295,#80296,#80297,#80298,#80299,#80300,#80301,#80302,#80303,#80304,
#80305,#80306,#80307,#80308,#80309,#80310,#80311,#80312,#80313,#80314,#80315,
#80316,#80317,#80318,#80319,#80320,#80321,#80322,#80323,#80324,#80325,#80326,
#80327,#80328,#80329,#80330,#80331,#80332,#80333,#80334,#80335,#80336,#80337,
#80338,#80339,#80340,#80341,#80342,#80343,#80344,#80345,#80346,#80347,#80348,
#80349,#80350,#80351,#80352,#80353,#80354,#80355,#80356,#80357,#80358,#80359,
#80360,#80361,#80362,#80363,#80364,#80365,#80366,#80367,#80368,#80369,#80370,
#80371,#80372,#80373,#80374,#80375,#80376,#80377,#80378,#80379,#80380,#80381,
#80382,#80383,#80384,#80385,#80386,#80387,#80388,#80389,#80390,#80391,#80392,
#80393,#80394,#80395,#80396,#80397,#80398,#80399,#80400,#80401,#80402,#80403,
#80404,#80405,#80406,#80407,#80408,#80409,#80410,#80411,#80412,#80413,#80414,
#80415,#80416,#80417,#80418,#80419,#80420,#80421,#80422,#80423,#80424,#80425,
#80426,#80427,#80428,#80429,#80430,#80431,#80432,#80433,#80434,#80435,#80436,
#80437,#80438,#80439,#80440,#80441,#80442,#80443,#80444,#80445,#80446,#80447,
#80448,#80449,#80450,#80451,#80452,#80453,#80454,#80455,#80456,#80457,#80458,
#80459,#80460,#80461,#80462,#80463,#80464,#80465,#80466,#80467,#80468,#80469,
#80470,#80471,#80472,#80473,#80474,#80475,#80476,#80477,#80478,#80479,#80480,
#80481,#80482,#80483,#80484,#80485,#80486,#80487,#80488,#80489,#80490,#80491,
#80492,#80493,#80494,#80495,#80496,#80497,#80498,#80499,#80500,#80501,#80502,
#80503,#80504,#80505,#80506,#80507,#80508,#80509,#80510,#80511,#80512,#80513,
#80514,#80515,#80516,#80517,#80518,#80519,#80520,#80521,#80522,#80523,#80524,
#80525,#80526,#80527,#80528,#80529,#80530,#80531,#80532,#80533,#80534,#80535,
#80536,#80537,#80538,#80539,#80540,#80541,#80542,#80543,#80544,#80545,#80546,
#80547,#80548,#80549,#80550,#80551,#80552,#80553,#80554,#80555,#80556,#80557,
#80558,#80559,#80560,#80561,#80562,#80563,#80564,#80565,#80566,#80567,#80568,
#80569,#80570,#80571,#80572,#80573,#80574,#80575,#80576,#80577,#80578,#80579,
#80580,#80581,#80582,#80583,#80584,#80585,#80586,#80587,#80588,#80589,#80590,
#80591,#80592,#80593,#80594,#80595,#80596,#80597,#80598,#80599,#80600),
(#80601,#80602,#80603,#80604,#80605,#80606,#80607,#80608,#80609,#80610,
#80611,#80612,#80613,#80614,#80615,#80616,#80617,#80618,#80619,#80620,#80621,
#80622,#80623,#80624,#80625,#80626,#80627,#80628,#80629,#80630,#80631,#80632,
#80633,#80634,#80635,#80636,#80637,#80638,#80639,#80640,#80641,#80642,#80643,
#80644,#80645,#80646,#80647,#80648,#80649,#80650,#80651,#80652,#80653,#80654,
#80655,#80656,#80657,#80658,#80659,#80660,#80661,#80662,#80663,#80664,#80665,
#80666,#80667,#80668,#80669,#80670,#80671,#80672,#80673,#80674,#80675,#80676,
#80677,#80678,#80679,#80680,#80681,#80682,#80683,#80684,#80685,#80686,#80687,
#80688,#80689,#80690,#80691,#80692,#80693,#80694,#80695,#80696,#80697,#80698,
#80699,#80700,#80701,#80702,#80703,#80704,#80705,#80706,#80707,#80708,#80709,
#80710,#80711,#80712,#80713,#80714,#80715,#80716,#80717,#80718,#80719,#80720,
#80721,#80722,#80723,#80724,#80725,#80726,#80727,#80728,#80729,#80730,#80731,
#80732,#80733,#80734,#80735,#80736,#80737,#80738,#80739,#80740,#80741,#80742,
#80743,#80744,#80745,#80746,#80747,#80748,#80749,#80750,#80751,#80752,#80753,
#80754,#80755,#80756,#80757,#80758,#80759,#80760,#80761,#80762,#80763,#80764,
#80765,#80766,#80767,#80768,#80769,#80770,#80771,#80772,#80773,#80774,#80775,
#80776,#80777,#80778,#80779,#80780,#80781,#80782,#80783,#80784,#80785,#80786,
#80787,#80788,#80789,#80790,#80791,#80792,#80793,#80794,#80795,#80796,#80797,
#80798,#80799,#80800,#80801,#80802,#80803,#80804,#80805,#80806,#80807,#80808,
#80809,#80810,#80811,#80812,#80813,#80814,#80815,#80816,#80817,#80818,#80819,
#80820,#80821,#80822,#80823,#80824,#80825,#80826,#80827,#80828,#80829,#80830,
#80831,#80832,#80833,#80834,#80835,#80836,#80837,#80838,#80839,#80840,#80841,
#80842,#80843,#80844,#80845,#80846,#80847,#80848,#80849,#80850,#80851,#80852,
#80853,#80854,#80855,#80856,#80857,#80858,#80859,#80860,#80861,#80862,#80863,
#80864,#80865,#80866,#80867,#80868,#80869,#80870,#80871,#80872,#80873,#80874,
#80875,#80876,#80877,#80878,#80879,#80880,#80881,#80882,#80883,#80884,#80885,
#80886,#80887,#80888,#80889,#80890,#80891,#80892,#80893,#80894,#80895,#80896,
#80897,#80898,#80899,#80900,#80901,#80902,#80903,#80904,#80905,#80906,#80907,
#80908,#80909,#80910,#80911,#80912,#80913,#80914,#80915,#80916,#80917,#80918,
#80919,#80920,#80921,#80922,#80923,#80924,#80925,#80926,#80927,#80928,#80929,
#80930,#80931,#80932,#80933,#80934,#80935,#80936,#80937,#80938,#80939,#80940,
#80941,#80942,#80943,#80944,#80945,#80946,#80947,#80948,#80949,#80950,#80951,
#80952,#80953,#80954,#80955,#80956,#80957,#80958,#80959,#80960,#80961,#80962,
#80963,#80964,#80965,#80966,#80967,#80968,#80969,#80970,#80971,#80972,#80973,
#80974,#80975,#80976,#80977,#80978,#80979,#80980,#80981,#80982,#80983,#80984,
#80985,#80986,#80987,#80988,#80989,#80990,#80991,#80992,#80993,#80994,#80995,
#80996,#80997,#80998,#80999,#81000,#81001,#81002,#81003,#81004,#81005,#81006,
#81007,#81008,#81009,#81010,#81011,#81012,#81013,#81014,#81015,#81016,#81017,
#81018,#81019,#81020,#81021,#81022,#81023,#81024,#81025,#81026,#81027,#81028,
#81029,#81030,#81031,#81032,#81033,#81034,#81035,#81036,#81037,#81038,#81039,
#81040,#81041,#81042,#81043,#81044,#81045,#81046,#81047,#81048,#81049,#81050,
#81051,#81052,#81053,#81054,#81055,#81056,#81057,#81058,#81059,#81060,#81061,
#81062,#81063,#81064,#81065,#81066,#81067,#81068,#81069,#81070,#81071,#81072,
#81073,#81074,#81075,#81076,#81077,#81078,#81079,#81080,#81081,#81082,#81083,
#81084,#81085,#81086,#81087,#81088,#81089,#81090,#81091,#81092,#81093,#81094,
#81095,#81096,#81097,#81098,#81099,#81100,#81101,#81102,#81103,#81104,#81105,
#81106,#81107,#81108,#81109,#81110,#81111,#81112,#81113,#81114,#81115,#81116,
#81117,#81118,#81119,#81120,#81121,#81122,#81123,#81124,#81125,#81126,#81127,
#81128,#81129,#81130,#81131,#81132,#81133,#81134,#81135,#81136,#81137,#81138,
#81139,#81140,#81141,#81142,#81143,#81144,#81145,#81146),(#81147,#81148,
#81149,#81150,#81151,#81152,#81153,#81154,#81155,#81156,#81157,#81158,#81159,
#81160,#81161,#81162,#81163,#81164,#81165,#81166,#81167,#81168,#81169,#81170,
#81171,#81172,#81173,#81174,#81175,#81176,#81177,#81178,#81179,#81180,#81181,
#81182,#81183,#81184,#81185,#81186,#81187,#81188,#81189,#81190,#81191,#81192,
#81193,#81194,#81195,#81196,#81197,#81198,#81199,#81200,#81201,#81202,#81203,
#81204,#81205,#81206,#81207,#81208,#81209,#81210,#81211,#81212,#81213,#81214,
#81215,#81216,#81217,#81218,#81219,#81220,#81221,#81222,#81223,#81224,#81225,
#81226,#81227,#81228,#81229,#81230,#81231,#81232,#81233,#81234,#81235,#81236,
#81237,#81238,#81239,#81240,#81241,#81242,#81243,#81244,#81245,#81246,#81247,
#81248,#81249,#81250,#81251,#81252,#81253,#81254,#81255,#81256,#81257,#81258,
#81259,#81260,#81261,#81262,#81263,#81264,#81265,#81266,#81267,#81268,#81269,
#81270,#81271,#81272,#81273,#81274,#81275,#81276,#81277,#81278,#81279,#81280,
#81281,#81282,#81283,#81284,#81285,#81286,#81287,#81288,#81289,#81290,#81291,
#81292,#81293,#81294,#81295,#81296,#81297,#81298,#81299,#81300,#81301,#81302,
#81303,#81304,#81305,#81306,#81307,#81308,#81309,#81310,#81311,#81312,#81313,
#81314,#81315,#81316,#81317,#81318,#81319,#81320,#81321,#81322,#81323,#81324,
#81325,#81326,#81327,#81328,#81329,#81330,#81331,#81332,#81333,#81334,#81335,
#81336,#81337,#81338,#81339,#81340,#81341,#81342,#81343,#81344,#81345,#81346,
#81347,#81348,#81349,#81350,#81351,#81352,#81353,#81354,#81355,#81356,#81357,
#81358,#81359,#81360,#81361,#81362,#81363,#81364,#81365,#81366,#81367,#81368,
#81369,#81370,#81371,#81372,#81373,#81374,#81375,#81376,#81377,#81378,#81379,
#81380,#81381,#81382,#81383,#81384,#81385,#81386,#81387,#81388,#81389,#81390,
#81391,#81392,#81393,#81394,#81395,#81396,#81397,#81398,#81399,#81400,#81401,
#81402,#81403,#81404,#81405,#81406,#81407,#81408,#81409,#81410,#81411,#81412,
#81413,#81414,#81415,#81416,#81417,#81418,#81419,#81420,#81421,#81422,#81423,
#81424,#81425,#81426,#81427,#81428,#81429,#81430,#81431,#81432,#81433,#81434,
#81435,#81436,#81437,#81438,#81439,#81440,#81441,#81442,#81443,#81444,#81445,
#81446,#81447,#81448,#81449,#81450,#81451,#81452,#81453,#81454,#81455,#81456,
#81457,#81458,#81459,#81460,#81461,#81462,#81463,#81464,#81465,#81466,#81467,
#81468,#81469,#81470,#81471,#81472,#81473,#81474,#81475,#81476,#81477,#81478,
#81479,#81480,#81481,#81482,#81483,#81484,#81485,#81486,#81487,#81488,#81489,
#81490,#81491,#81492,#81493,#81494,#81495,#81496,#81497,#81498,#81499,#81500,
#81501,#81502,#81503,#81504,#81505,#81506,#81507,#81508,#81509,#81510,#81511,
#81512,#81513,#81514,#81515,#81516,#81517,#81518,#81519,#81520,#81521,#81522,
#81523,#81524,#81525,#81526,#81527,#81528,#81529,#81530,#81531,#81532,#81533,
#81534,#81535,#81536,#81537,#81538,#81539,#81540,#81541,#81542,#81543,#81544,
#81545,#81546,#81547,#81548,#81549,#81550,#81551,#81552,#81553,#81554,#81555,
#81556,#81557,#81558,#81559,#81560,#81561,#81562,#81563,#81564,#81565,#81566,
#81567,#81568,#81569,#81570,#81571,#81572,#81573,#81574,#81575,#81576,#81577,
#81578,#81579,#81580,#81581,#81582,#81583,#81584,#81585,#81586,#81587,#81588,
#81589,#81590,#81591,#81592,#81593,#81594,#81595,#81596,#81597,#81598,#81599,
#81600,#81601,#81602,#81603,#81604,#81605,#81606,#81607,#81608,#81609,#81610,
#81611,#81612,#81613,#81614,#81615,#81616,#81617,#81618,#81619,#81620,#81621,
#81622,#81623,#81624,#81625,#81626,#81627,#81628,#81629,#81630,#81631,#81632,
#81633,#81634,#81635,#81636,#81637,#81638,#81639,#81640,#81641,#81642,#81643,
#81644,#81645,#81646,#81647,#81648,#81649,#81650,#81651,#81652,#81653,#81654,
#81655,#81656,#81657,#81658,#81659,#81660,#81661,#81662,#81663,#81664,#81665,
#81666,#81667,#81668,#81669,#81670,#81671,#81672,#81673,#81674,#81675,#81676,
#81677,#81678,#81679,#81680,#81681,#81682,#81683,#81684,#81685,#81686,#81687,
#81688,#81689,#81690,#81691,#81692)),.UNSPECIFIED.,.F.,.F.,.F.,(4,4),(4,
1,1,1,1,1,1,1,1,1,1,1,1,1,1,1,1,1,1,1,1,1,1,1,1,1,1,1,1,1,1,1,1,1,1,1,1,
1,1,1,1,1,1,1,1,1,1,1,1,1,1,1,1,1,1,1,1,1,1,1,1,1,1,1,1,1,1,1,1,1,1,1,1,
1,1,1,1,1,1,1,1,1,1,1,1,1,1,1,1,1,1,1,1,1,1,1,1,1,1,1,1,1,1,1,1,1,1,1,1,
1,1,1,1,1,1,1,1,1,1,1,1,1,1,1,1,1,1,1,1,1,1,1,1,1,1,1,1,1,1,1,1,1,1,1,1,
1,1,1,1,1,1,1,1,1,1,1,1,1,1,1,1,1,1,1,1,1,1,1,1,1,1,1,1,1,1,1,1,1,1,1,1,
1,1,1,1,1,1,1,1,1,1,1,1,1,1,1,1,1,1,1,1,1,1,1,1,1,1,1,1,1,1,1,1,1,1,1,1,
1,1,1,1,1,1,1,1,1,1,1,1,1,1,1,1,1,1,1,1,1,1,1,1,1,1,1,1,1,1,1,1,1,1,1,1,
1,1,1,1,1,1,1,1,1,1,1,1,1,1,1,1,1,1,1,1,1,1,1,1,1,1,1,1,1,1,1,1,1,1,1,1,
1,1,1,1,1,1,1,1,1,1,1,1,1,1,1,1,1,1,1,1,1,1,1,1,1,1,1,1,1,1,1,1,1,1,1,1,
1,1,1,1,1,1,1,1,1,1,1,1,1,1,1,1,1,1,1,1,1,1,1,1,1,1,1,1,1,1,1,1,1,1,1,1,
1,1,1,1,1,1,1,1,1,1,1,1,1,1,1,1,1,1,1,1,1,1,1,1,1,1,1,1,1,1,1,1,1,1,1,1,
1,1,1,1,1,1,1,1,1,1,1,1,1,1,1,1,1,1,1,1,1,1,1,1,1,1,1,1,1,1,1,1,1,1,1,1,
1,1,1,1,1,1,1,1,1,1,1,1,1,1,1,1,1,1,1,1,1,1,1,1,1,1,1,1,1,1,1,1,1,1,1,1,
1,1,1,1,1,1,1,1,1,1,1,1,1,1,1,1,1,1,1,1,1,1,1,1,1,1,1,1,1,1,1,1,1,1,1,1,
1,1,1,1,1,1,1,1,1,1,1,1,1,1,1,1,1,1,1,1,1,1,1,1,1,1,1,1,1,1,1,1,1,1,1,1,
1,1,4),(-0.000757559510207718,0.132914936587996),(11.614729191302,12.1138040384816,
12.612575229144,13.1113464198064,13.6101176104689,14.6076599917938,15.6052023731187,
16.6027447544436,17.101515945106,17.6002871357685,18.0990583264309,18.5978295170934,
19.5953718984182,20.0941430890807,20.5929142797431,21.590456661068,22.5879990423929,
23.5855414237178,24.0843126143803,24.5830838050427,25.0818549957052,25.5806261863676,
26.5781685676925,27.0769397583549,27.5757109490174,28.5732533303423,29.5707957116672,
30.5683380929921,31.0671092836545,31.565880474317,32.0646516649794,32.5634228556418,
33.5609652369667,34.0597364276292,34.5585076182916,35.5560499996165,36.5535923809414,
37.5511347622663,38.0499059529288,38.5486771435912,39.0474483342537,39.5462195249161,
40.543761906241,41.0425330969034,41.5413042875659,42.5388466688908,43.5363890502157,
44.5339314315406,45.032702622203,45.5314738128654,46.0302450035279,46.5290161941903,
47.5265585755152,48.0253297661777,48.5241009568401,49.521643338165,50.5191857194899,
51.5167281008148,52.0154992914772,52.5142704821397,53.0130416728021,53.5118128634646,
54.5093552447895,55.0081264354519,55.5068976261144,56.5044400074393,57.5019823887642,
58.4995247700891,58.9982959607515,59.4970671514139,59.9958383420764,60.4946095327388,
61.4921519140637,61.9909231047262,62.4896942953886,63.4872366767135,64.4847790580384,
65.4823214393633,65.9810926300257,66.4798638206882,66.9786350113506,67.4774062020131,
68.474948583338,68.9737197740004,69.4724909646629,70.4700333459878,71.4675757273126,
72.4651181086375,72.9638892993,73.4626604899624,73.9614316806249,74.4602028712873,
75.4577452526122,75.9565164432747,76.4552876339371,77.452830015262,78.4503723965869,
79.4479147779118,79.9466859685742,80.4454571592367,80.9442283498991,81.4429995405616,
82.4405419218865,82.9393131125489,83.4380843032114,84.4356266845362,85.4331690658612,
86.430711447186,86.9294826378485,87.4282538285109,87.9270250191734,88.4257962098358,
89.4233385911607,89.9221097818232,90.4208809724856,91.4184233538105,92.4159657351354,
93.4135081164603,93.9122793071227,94.4110504977852,94.9098216884476,95.4085928791101,
96.406135260435,96.9049064510974,97.4036776417599,98.4012200230847,99.3987624044096,
100.396304785735,100.895075976397,101.393847167059,101.892618357722,102.391389548384,
103.388931929709,103.887703120372,104.386474311034,105.384016692359,106.381559073684,
107.379101455009,107.877872645671,108.376643836334,108.875415026996,109.374186217659,
110.371728598983,110.870499789646,111.369270980308,112.366813361633,113.364355742958,
114.361898124283,114.860669314945,115.359440505608,115.85821169627,116.356982886933,
117.354525268258,117.85329645892,118.352067649583,119.349610030907,120.347152412232,
121.344694793557,121.84346598422,122.342237174882,122.841008365545,123.339779556207,
124.337321937532,124.836093128194,125.334864318857,126.332406700182,127.329949081507,
128.327491462832,128.826262653494,129.325033844156,129.823805034819,130.322576225481,
131.320118606806,131.818889797469,132.317660988131,133.315203369456,134.312745750781,
135.310288132106,135.809059322768,136.307830513431,136.806601704093,137.305372894756,
138.30291527608,138.801686466743,139.300457657405,140.29800003873,141.295542420055,
142.29308480138,142.791855992042,143.290627182705,143.789398373367,144.28816956403,
145.285711945355,145.784483136017,146.28325432668,147.280796708004,148.278339089329,
149.275881470654,149.774652661317,150.273423851979,150.772195042642,151.270966233304,
152.268508614629,152.767279805291,153.266050995954,154.263593377279,155.261135758604,
156.258678139929,156.757449330591,157.256220521253,157.754991711916,158.253762902578,
159.251305283903,159.750076474566,160.248847665228,161.246390046553,162.243932427878,
163.241474809203,163.740245999865,164.239017190528,164.73778838119,165.236559571853,
166.234101953177,166.73287314384,167.231644334502,168.229186715827,169.226729097152,
170.224271478477,170.723042669139,171.221813859802,171.720585050464,172.219356241127,
173.216898622452,173.715669813114,174.214441003777,175.211983385101,176.209525766426,
177.207068147751,177.705839338414,178.204610529076,178.703381719739,179.202152910401,
180.199695291726,180.698466482388,181.197237673051,182.194780054376,183.192322435701,
184.189864817025,184.688636007688,185.18740719835,185.686178389013,186.184949579675,
187.182491961,187.681263151663,188.180034342325,189.17757672365,190.175119104975,
191.1726614863,191.671432676962,192.170203867625,192.668975058287,193.16774624895,
194.165288630274,194.664059820937,195.162831011599,196.160373392924,197.157915774249,
198.155458155574,198.654229346236,199.153000536899,199.651771727561,200.150542918224,
201.148085299549,201.646856490211,202.145627680874,203.143170062198,204.140712443523,
205.138254824848,206.135797206173,207.133339587498,207.63211077816,208.130881968823,
209.128424350148,209.62719554081,210.125966731473,210.624737922135,211.123509112798,
212.121051494122,213.118593875447,214.116136256772,214.614907447435,215.113678638097,
216.111221019422,216.609992210084,217.108763400747,217.607534591409,218.106305782072,
219.103848163397,220.101390544722,221.098932926047,221.597704116709,222.096475307371,
223.094017688696,223.592788879359,224.091560070021,224.590331260684,225.089102451346,
226.086644832671,227.084187213996,228.081729595321,228.580500785983,229.079271976646,
230.076814357971,230.575585548633,231.074356739295,231.573127929958,232.07189912062,
233.069441501945,234.06698388327,235.064526264595,235.563297455257,236.06206864592,
237.059611027245,237.558382217907,238.05715340857,238.555924599232,239.054695789895,
240.052238171219,241.049780552544,242.047322933869,242.546094124532,243.044865315194,
244.042407696519,244.541178887181,245.039950077844,245.538721268506,246.037492459169,
247.035034840494,248.032577221819,249.030119603143,249.528890793806,250.027661984468,
251.025204365793,251.523975556456,252.022746747118,252.521517937781,253.020289128443,
254.017831509768,255.015373891093,256.012916272418,256.51168746308,257.010458653743,
258.008001035068,258.50677222573,259.005543416392,259.504314607055,260.003085797717,
261.000628179042,261.998170560367,262.995712941692,263.494484132354,263.993255323017,
264.990797704342,265.489568895004,265.988340085667,266.487111276329,266.985882466992,
267.983424848316,268.980967229641,269.978509610966,270.477280801629,270.976051992291,
271.973594373616,272.472365564278,272.971136754941,273.469907945603,273.968679136266,
274.966221517591,275.963763898916,276.96130628024,277.460077470903,277.958848661565,
278.95639104289,279.455162233553,279.953933424215,280.452704614878,280.95147580554,
281.949018186865,282.94656056819,283.944102949515,284.442874140177,284.94164533084,
285.939187712165,286.437958902827,286.936730093489,287.435501284152,287.934272474814,
288.931814856139,289.929357237464,290.926899618789,291.425670809451,291.924442000114,
292.921984381439,293.420755572101,293.919526762764,294.418297953426,294.917069144089,
295.914611525413,296.912153906738,297.909696288063,298.408467478726,298.907238669388,
299.904781050713,300.403552241375,300.902323432038,301.4010946227,301.899865813363,
302.897408194688,303.894950576013,304.892492957337,305.391264148,305.890035338662,
306.887577719987,307.38634891065,307.885120101312,308.383891291975,308.882662482637,
309.880204863962,310.877747245287,311.875289626612,312.374060817274,312.872832007937,
313.870374389261,314.369145579924,314.867916770586,315.366687961249,315.865459151911,
316.863001533236,317.860543914561,318.858086295886,319.356857486548,319.855628677211,
320.853171058536,321.351942249198,321.850713439861,322.349484630523,322.848255821186,
323.84579820251,324.843340583835,325.84088296516,326.339654155823,326.838425346485,
327.83596772781,328.334738918472,328.833510109135,329.332281299797,329.83105249046,
330.828594871785,331.82613725311,332.823679634434,333.322450825097,333.821222015759,
334.818764397084,335.317535587747,335.816306778409,336.315077969072,336.813849159734,
337.811391541059,338.808933922384,339.806476303709,340.305247494371,340.804018685034,
341.801561066358,342.300332257021,342.799103447683,343.297874638346,343.796645829008,
344.794188210333,345.791730591658,346.789272972983,347.288044163645,347.786815354308,
348.784357735633,349.283128926295,349.781900116958,350.28067130762,350.779442498283,
351.776984879607,352.774527260932,353.772069642257,354.27084083292,354.769612023582,
355.767154404907,356.265925595569,356.764696786232,357.263467976894,357.762239167557,
358.759781548882,359.757323930207,360.754866311531,361.253637502194,361.752408692856,
362.749951074181,363.248722264844,363.747493455506,364.246264646169,364.745035836831,
365.742578218156,366.740120599481,367.737662980806,368.236434171468,368.735205362131,
369.732747743455,370.231518934118,370.73029012478,371.229061315443,371.727832506105,
372.72537488743,373.722917268755,374.72045965008,375.219230840742,375.718002031405,
376.71554441273,377.214315603392,377.713086794055,378.211857984717,378.710629175379,
379.708171556704,380.705713938029,381.703256319354,382.202027510017,382.700798700679,
383.698341082004,384.197112272666,384.695883463329,385.194654653991,385.693425844654,
386.690968225979,387.688510607304,388.686052988628,389.184824179291,389.683595369953,
390.182366560616,390.681747047565),.UNSPECIFIED.);
#758=B_SPLINE_SURFACE_WITH_KNOTS('',3,3,((#85029,#85030,#85031,#85032),
(#85033,#85034,#85035,#85036),(#85037,#85038,#85039,#85040),(#85041,#85042,
#85043,#85044)),.UNSPECIFIED.,.F.,.F.,.F.,(4,4),(4,4),(0.0217391304347818,
0.617536119336012),(0.774386899537597,1.),.UNSPECIFIED.);
#759=B_SPLINE_SURFACE_WITH_KNOTS('',3,3,((#85046,#85047,#85048,#85049,#85050,
#85051,#85052,#85053,#85054,#85055),(#85056,#85057,#85058,#85059,#85060,
#85061,#85062,#85063,#85064,#85065),(#85066,#85067,#85068,#85069,#85070,
#85071,#85072,#85073,#85074,#85075),(#85076,#85077,#85078,#85079,#85080,
#85081,#85082,#85083,#85084,#85085)),.UNSPECIFIED.,.F.,.F.,.F.,(4,4),(4,
1,1,1,1,1,1,4),(0.0216104565420008,1.00130145442866),(-0.000128673892780755,
0.142857142857143,0.285714285714286,0.428571428571429,0.571428571428571,
0.714285714285714,0.857142857142857,1.00130145442866),.UNSPECIFIED.);
#760=B_SPLINE_SURFACE_WITH_KNOTS('',3,3,((#85096,#85097,#85098,#85099,#85100,
#85101,#85102,#85103),(#85104,#85105,#85106,#85107,#85108,#85109,#85110,
#85111),(#85112,#85113,#85114,#85115,#85116,#85117,#85118,#85119),(#85120,
#85121,#85122,#85123,#85124,#85125,#85126,#85127)),.UNSPECIFIED.,.F.,.F.,
 .F.,(4,4),(4,1,1,1,1,4),(0.,1.00001448148635),(0.144829272278474,0.266996519095835,
0.389163765913196,0.633498259547918,0.877832753182639,1.00001448148635),
 .UNSPECIFIED.);
#761=B_SPLINE_SURFACE_WITH_KNOTS('',3,3,((#85395,#85396,#85397,#85398,#85399,
#85400,#85401,#85402,#85403),(#85404,#85405,#85406,#85407,#85408,#85409,
#85410,#85411,#85412),(#85413,#85414,#85415,#85416,#85417,#85418,#85419,
#85420,#85421),(#85422,#85423,#85424,#85425,#85426,#85427,#85428,#85429,
#85430)),.UNSPECIFIED.,.F.,.F.,.F.,(4,4),(4,1,1,1,1,1,4),(-1.22172294938054E-5,
1.),(-1.22172294938054E-5,0.12216720883009,0.24433441766018,0.488668835320359,
0.610836044150449,0.733003252980539,0.855170461810629),.UNSPECIFIED.);
#762=B_SPLINE_SURFACE_WITH_KNOTS('',3,3,((#85465,#85466,#85467,#85468),
(#85469,#85470,#85471,#85472),(#85473,#85474,#85475,#85476),(#85477,#85478,
#85479,#85480)),.UNSPECIFIED.,.F.,.F.,.F.,(4,4),(4,4),(0.512899287463832,
1.),(0.,0.18445259717643),.UNSPECIFIED.);
#763=B_SPLINE_SURFACE_WITH_KNOTS('',3,3,((#85482,#85483,#85484,#85485,#85486,
#85487,#85488,#85489,#85490,#85491),(#85492,#85493,#85494,#85495,#85496,
#85497,#85498,#85499,#85500,#85501),(#85502,#85503,#85504,#85505,#85506,
#85507,#85508,#85509,#85510,#85511),(#85512,#85513,#85514,#85515,#85516,
#85517,#85518,#85519,#85520,#85521)),.UNSPECIFIED.,.F.,.F.,.F.,(4,4),(4,
1,1,1,1,1,1,4),(0.0216104646765061,1.),(-0.000128665758275638,0.142857142857143,
0.285714285714286,0.428571428571429,0.571428571428571,0.714285714285714,
0.857142857142857,1.),.UNSPECIFIED.);
#764=B_SPLINE_SURFACE_WITH_KNOTS('',3,3,((#85543,#85544,#85545,#85546),
(#85547,#85548,#85549,#85550),(#85551,#85552,#85553,#85554),(#85555,#85556,
#85557,#85558)),.UNSPECIFIED.,.F.,.F.,.F.,(4,4),(4,4),(0.382464506767468,
0.978260874456547),(0.,0.225612834551505),.UNSPECIFIED.);
#765=B_SPLINE_SURFACE_WITH_KNOTS('',3,3,((#85560,#85561,#85562,#85563,#85564,
#85565,#85566,#85567,#85568,#85569),(#85570,#85571,#85572,#85573,#85574,
#85575,#85576,#85577,#85578,#85579),(#85580,#85581,#85582,#85583,#85584,
#85585,#85586,#85587,#85588,#85589),(#85590,#85591,#85592,#85593,#85594,
#85595,#85596,#85597,#85598,#85599)),.UNSPECIFIED.,.F.,.F.,.F.,(4,4),(4,
1,1,1,1,1,1,4),(0.,0.97838954356546),(-0.00012866910891396,0.142857142857143,
0.285714285714286,0.428571428571429,0.571428571428571,0.714285714285714,
0.857142857142857,1.00010925279131),.UNSPECIFIED.);
#766=B_SPLINE_SURFACE_WITH_KNOTS('',3,3,((#85613,#85614,#85615,#85616,#85617,
#85618,#85619,#85620,#85621,#85622),(#85623,#85624,#85625,#85626,#85627,
#85628,#85629,#85630,#85631,#85632),(#85633,#85634,#85635,#85636,#85637,
#85638,#85639,#85640,#85641,#85642),(#85643,#85644,#85645,#85646,#85647,
#85648,#85649,#85650,#85651,#85652)),.UNSPECIFIED.,.F.,.F.,.F.,(4,4),(4,
1,1,1,1,1,1,4),(0.,1.),(0.,0.142857142857143,0.285714285714286,0.428571428571429,
0.571428571428571,0.714285714285714,0.857142857142857,1.),.UNSPECIFIED.);
#767=B_SPLINE_SURFACE_WITH_KNOTS('',3,3,((#85654,#85655,#85656,#85657,#85658,
#85659,#85660,#85661,#85662,#85663),(#85664,#85665,#85666,#85667,#85668,
#85669,#85670,#85671,#85672,#85673),(#85674,#85675,#85676,#85677,#85678,
#85679,#85680,#85681,#85682,#85683),(#85684,#85685,#85686,#85687,#85688,
#85689,#85690,#85691,#85692,#85693)),.UNSPECIFIED.,.F.,.F.,.F.,(4,4),(4,
1,1,1,1,1,1,4),(0.0216103522188689,1.),(-0.00012877821591213,0.142857142857143,
0.285714285714286,0.428571428571429,0.571428571428571,0.714285714285714,
0.857142857142857,1.00010930858083),.UNSPECIFIED.);
#768=B_SPLINE_SURFACE_WITH_KNOTS('',3,3,((#85708,#85709,#85710,#85711,#85712,
#85713,#85714,#85715,#85716,#85717),(#85718,#85719,#85720,#85721,#85722,
#85723,#85724,#85725,#85726,#85727),(#85728,#85729,#85730,#85731,#85732,
#85733,#85734,#85735,#85736,#85737),(#85738,#85739,#85740,#85741,#85742,
#85743,#85744,#85745,#85746,#85747)),.UNSPECIFIED.,.F.,.F.,.F.,(4,4),(4,
1,1,1,1,1,1,4),(0.,0.97838966897386),(-0.00012879451731267,0.142857142857143,
0.285714285714286,0.428571428571429,0.571428571428571,0.714285714285714,
0.857142857142857,1.00010890844888),.UNSPECIFIED.);
#769=B_SPLINE_SURFACE_WITH_KNOTS('',3,3,((#85762,#85763,#85764,#85765,#85766,
#85767,#85768,#85769,#85770,#85771),(#85772,#85773,#85774,#85775,#85776,
#85777,#85778,#85779,#85780,#85781),(#85782,#85783,#85784,#85785,#85786,
#85787,#85788,#85789,#85790,#85791),(#85792,#85793,#85794,#85795,#85796,
#85797,#85798,#85799,#85800,#85801)),.UNSPECIFIED.,.F.,.F.,.F.,(4,4),(4,
1,1,1,1,1,1,4),(0.,1.),(0.,0.142857142857143,0.285714285714286,0.428571428571429,
0.571428571428571,0.714285714285714,0.857142857142857,1.),.UNSPECIFIED.);
#770=B_SPLINE_SURFACE_WITH_KNOTS('',3,3,((#85804,#85805,#85806,#85807,#85808,
#85809,#85810,#85811,#85812,#85813),(#85814,#85815,#85816,#85817,#85818,
#85819,#85820,#85821,#85822,#85823),(#85824,#85825,#85826,#85827,#85828,
#85829,#85830,#85831,#85832,#85833),(#85834,#85835,#85836,#85837,#85838,
#85839,#85840,#85841,#85842,#85843)),.UNSPECIFIED.,.F.,.F.,.F.,(4,4),(4,
1,1,1,1,1,1,4),(0.0216102027499123,1.),(-0.000128927684868709,0.142857142857143,
0.285714285714286,0.428571428571429,0.571428571428571,0.714285714285714,
0.857142857142857,1.00010894090728),.UNSPECIFIED.);
#771=B_SPLINE_SURFACE_WITH_KNOTS('',3,3,((#85858,#85859,#85860,#85861,#85862,
#85863,#85864,#85865,#85866,#85867),(#85868,#85869,#85870,#85871,#85872,
#85873,#85874,#85875,#85876,#85877),(#85878,#85879,#85880,#85881,#85882,
#85883,#85884,#85885,#85886,#85887),(#85888,#85889,#85890,#85891,#85892,
#85893,#85894,#85895,#85896,#85897)),.UNSPECIFIED.,.F.,.F.,.F.,(4,4),(4,
1,1,1,1,1,1,4),(-3.49469805785124E-7,0.978389836394998),(-0.000128961938451469,
0.142857142857143,0.285714285714286,0.428571428571429,0.571428571428571,
0.714285714285714,0.857142857142857,1.00010852689685),.UNSPECIFIED.);
#772=B_SPLINE_SURFACE_WITH_KNOTS('',3,3,((#85920,#85921,#85922,#85923,#85924,
#85925,#85926,#85927,#85928,#85929),(#85930,#85931,#85932,#85933,#85934,
#85935,#85936,#85937,#85938,#85939),(#85940,#85941,#85942,#85943,#85944,
#85945,#85946,#85947,#85948,#85949),(#85950,#85951,#85952,#85953,#85954,
#85955,#85956,#85957,#85958,#85959)),.UNSPECIFIED.,.F.,.F.,.F.,(4,4),(4,
1,1,1,1,1,1,4),(0.,1.00000113587033),(0.,0.142857142857143,0.285714285714286,
0.428571428571429,0.571428571428571,0.714285714285714,0.857142857142857,
1.),.UNSPECIFIED.);
#773=B_SPLINE_SURFACE_WITH_KNOTS('',3,3,((#85962,#85963,#85964,#85965,#85966,
#85967,#85968,#85969,#85970,#85971),(#85972,#85973,#85974,#85975,#85976,
#85977,#85978,#85979,#85980,#85981),(#85982,#85983,#85984,#85985,#85986,
#85987,#85988,#85989,#85990,#85991),(#85992,#85993,#85994,#85995,#85996,
#85997,#85998,#85999,#86000,#86001)),.UNSPECIFIED.,.F.,.F.,.F.,(4,4),(4,
1,1,1,1,1,1,4),(0.0216101883594699,1.),(-0.000128942075311584,0.142857142857143,
0.285714285714286,0.428571428571429,0.571428571428571,0.714285714285714,
0.857142857142857,1.00010890887743),.UNSPECIFIED.);
#774=B_SPLINE_SURFACE_WITH_KNOTS('',3,3,((#86028,#86029,#86030,#86031,#86032,
#86033,#86034,#86035,#86036,#86037),(#86038,#86039,#86040,#86041,#86042,
#86043,#86044,#86045,#86046,#86047),(#86048,#86049,#86050,#86051,#86052,
#86053,#86054,#86055,#86056,#86057),(#86058,#86059,#86060,#86061,#86062,
#86063,#86064,#86065,#86066,#86067)),.UNSPECIFIED.,.F.,.F.,.F.,(4,4),(4,
1,1,1,1,1,1,4),(0.,0.978389731943835),(-0.00012885748728817,0.142857142857143,
0.285714285714286,0.428571428571429,0.571428571428571,0.714285714285714,
0.857142857142857,1.00010875621283),.UNSPECIFIED.);
#775=B_SPLINE_SURFACE_WITH_KNOTS('',3,3,((#86082,#86083,#86084,#86085,#86086,
#86087,#86088,#86089,#86090,#86091),(#86092,#86093,#86094,#86095,#86096,
#86097,#86098,#86099,#86100,#86101),(#86102,#86103,#86104,#86105,#86106,
#86107,#86108,#86109,#86110,#86111),(#86112,#86113,#86114,#86115,#86116,
#86117,#86118,#86119,#86120,#86121)),.UNSPECIFIED.,.F.,.F.,.F.,(4,4),(4,
1,1,1,1,1,1,4),(0.,1.),(0.,0.142857142857143,0.285714285714286,0.428571428571429,
0.571428571428571,0.714285714285714,0.857142857142857,1.),.UNSPECIFIED.);
#776=B_SPLINE_SURFACE_WITH_KNOTS('',3,3,((#86124,#86125,#86126,#86127,#86128,
#86129,#86130,#86131,#86132,#86133),(#86134,#86135,#86136,#86137,#86138,
#86139,#86140,#86141,#86142,#86143),(#86144,#86145,#86146,#86147,#86148,
#86149,#86150,#86151,#86152,#86153),(#86154,#86155,#86156,#86157,#86158,
#86159,#86160,#86161,#86162,#86163)),.UNSPECIFIED.,.F.,.F.,.F.,(4,4),(4,
1,1,1,1,1,1,4),(0.0216103414761888,1.),(-0.000128788958592299,0.142857142857143,
0.285714285714286,0.428571428571429,0.571428571428571,0.714285714285714,
0.857142857142857,1.00010927970758),.UNSPECIFIED.);
#777=B_SPLINE_SURFACE_WITH_KNOTS('',3,3,((#86190,#86191,#86192,#86193,#86194,
#86195,#86196,#86197,#86198,#86199),(#86200,#86201,#86202,#86203,#86204,
#86205,#86206,#86207,#86208,#86209),(#86210,#86211,#86212,#86213,#86214,
#86215,#86216,#86217,#86218,#86219),(#86220,#86221,#86222,#86223,#86224,
#86225,#86226,#86227,#86228,#86229)),.UNSPECIFIED.,.F.,.F.,.F.,(4,4),(4,
1,1,1,1,1,1,4),(0.,0.978389590969423),(-0.000128716512876252,0.142857142857143,
0.285714285714286,0.428571428571429,0.571428571428571,0.714285714285714,
0.857142857142857,1.00010911520136),.UNSPECIFIED.);
#778=B_SPLINE_SURFACE_WITH_KNOTS('',3,3,((#86244,#86245,#86246,#86247,#86248,
#86249,#86250,#86251,#86252,#86253),(#86254,#86255,#86256,#86257,#86258,
#86259,#86260,#86261,#86262,#86263),(#86264,#86265,#86266,#86267,#86268,
#86269,#86270,#86271,#86272,#86273),(#86274,#86275,#86276,#86277,#86278,
#86279,#86280,#86281,#86282,#86283)),.UNSPECIFIED.,.F.,.F.,.F.,(4,4),(4,
1,1,1,1,1,1,4),(0.,1.),(0.,0.142857142857143,0.285714285714286,0.428571428571429,
0.571428571428571,0.714285714285714,0.857142857142857,1.),.UNSPECIFIED.);
#779=B_SPLINE_SURFACE_WITH_KNOTS('',3,3,((#86286,#86287,#86288,#86289),
(#86290,#86291,#86292,#86293),(#86294,#86295,#86296,#86297),(#86298,#86299,
#86300,#86301)),.UNSPECIFIED.,.F.,.F.,.F.,(4,4),(4,4),(0.,0.487101414751205),
(0.815547136912673,1.),.UNSPECIFIED.);
#780=B_SPLINE_SURFACE_WITH_KNOTS('',3,3,((#86303,#86304,#86305,#86306,#86307,
#86308,#86309,#86310,#86311,#86312),(#86313,#86314,#86315,#86316,#86317,
#86318,#86319,#86320,#86321,#86322),(#86323,#86324,#86325,#86326,#86327,
#86328,#86329,#86330,#86331,#86332),(#86333,#86334,#86335,#86336,#86337,
#86338,#86339,#86340,#86341,#86342)),.UNSPECIFIED.,.F.,.F.,.F.,(4,4),(4,
1,1,1,1,1,1,4),(-0.00139422224055136,0.978389538674135),(-0.00139422224055136,
0.142857142857143,0.285714285714286,0.428571428571429,0.571428571428571,
0.714285714285714,0.857142857142857,1.00012866910892),.UNSPECIFIED.);
#781=B_SPLINE_SURFACE_WITH_KNOTS('',3,3,((#86343,#86344,#86345,#86346,#86347,
#86348,#86349,#86350,#86351,#86352),(#86353,#86354,#86355,#86356,#86357,
#86358,#86359,#86360,#86361,#86362),(#86363,#86364,#86365,#86366,#86367,
#86368,#86369,#86370,#86371,#86372),(#86373,#86374,#86375,#86376,#86377,
#86378,#86379,#86380,#86381,#86382)),.UNSPECIFIED.,.F.,.F.,.F.,(4,4),(4,
1,1,1,1,1,1,4),(0.0216103522188697,1.),(-0.000128778215911952,0.142857142857143,
0.285714285714286,0.428571428571429,0.571428571428571,0.714285714285714,
0.857142857142857,1.00012877821591),.UNSPECIFIED.);
#782=B_SPLINE_SURFACE_WITH_KNOTS('',3,3,((#86393,#86394,#86395,#86396,#86397,
#86398,#86399,#86400,#86401,#86402),(#86403,#86404,#86405,#86406,#86407,
#86408,#86409,#86410,#86411,#86412),(#86413,#86414,#86415,#86416,#86417,
#86418,#86419,#86420,#86421,#86422),(#86423,#86424,#86425,#86426,#86427,
#86428,#86429,#86430,#86431,#86432)),.UNSPECIFIED.,.F.,.F.,.F.,(4,4),(4,
1,1,1,1,1,1,4),(0.,0.978389664082536),(-0.000128794517316134,0.142857142857143,
0.285714285714286,0.428571428571429,0.571428571428571,0.714285714285714,
0.857142857142857,1.00012879451732),.UNSPECIFIED.);
#783=B_SPLINE_SURFACE_WITH_KNOTS('',3,3,((#86443,#86444,#86445,#86446,#86447,
#86448,#86449,#86450,#86451,#86452),(#86453,#86454,#86455,#86456,#86457,
#86458,#86459,#86460,#86461,#86462),(#86463,#86464,#86465,#86466,#86467,
#86468,#86469,#86470,#86471,#86472),(#86473,#86474,#86475,#86476,#86477,
#86478,#86479,#86480,#86481,#86482)),.UNSPECIFIED.,.F.,.F.,.F.,(4,4),(4,
1,1,1,1,1,1,4),(0.,1.),(0.,0.142857142857143,0.285714285714286,0.428571428571429,
0.571428571428571,0.714285714285714,0.857142857142857,1.),.UNSPECIFIED.);
#784=B_SPLINE_SURFACE_WITH_KNOTS('',3,3,((#86483,#86484,#86485,#86486,#86487,
#86488,#86489,#86490,#86491,#86492),(#86493,#86494,#86495,#86496,#86497,
#86498,#86499,#86500,#86501,#86502),(#86503,#86504,#86505,#86506,#86507,
#86508,#86509,#86510,#86511,#86512),(#86513,#86514,#86515,#86516,#86517,
#86518,#86519,#86520,#86521,#86522)),.UNSPECIFIED.,.F.,.F.,.F.,(4,4),(4,
1,1,1,1,1,1,4),(0.0216102027499124,1.),(-0.000128927684869032,0.142857142857143,
0.285714285714286,0.428571428571429,0.571428571428571,0.714285714285714,
0.857142857142857,1.00012892768487),.UNSPECIFIED.);
#785=B_SPLINE_SURFACE_WITH_KNOTS('',3,3,((#86533,#86534,#86535,#86536,#86537,
#86538,#86539,#86540,#86541,#86542),(#86543,#86544,#86545,#86546,#86547,
#86548,#86549,#86550,#86551,#86552),(#86553,#86554,#86555,#86556,#86557,
#86558,#86559,#86560,#86561,#86562),(#86563,#86564,#86565,#86566,#86567,
#86568,#86569,#86570,#86571,#86572)),.UNSPECIFIED.,.F.,.F.,.F.,(4,4),(4,
1,1,1,1,1,1,4),(-3.49469809180723E-7,0.978389831503672),(-0.000128961938453871,
0.142857142857143,0.285714285714286,0.428571428571429,0.571428571428571,
0.714285714285714,0.857142857142857,1.00012896193845),.UNSPECIFIED.);
#786=B_SPLINE_SURFACE_WITH_KNOTS('',3,3,((#86591,#86592,#86593,#86594,#86595,
#86596,#86597,#86598,#86599,#86600),(#86601,#86602,#86603,#86604,#86605,
#86606,#86607,#86608,#86609,#86610),(#86611,#86612,#86613,#86614,#86615,
#86616,#86617,#86618,#86619,#86620),(#86621,#86622,#86623,#86624,#86625,
#86626,#86627,#86628,#86629,#86630)),.UNSPECIFIED.,.F.,.F.,.F.,(4,4),(4,
1,1,1,1,1,1,4),(0.,1.00000113587032),(0.,0.142857142857143,0.285714285714286,
0.428571428571429,0.571428571428571,0.714285714285714,0.857142857142857,
1.),.UNSPECIFIED.);
#787=B_SPLINE_SURFACE_WITH_KNOTS('',3,3,((#86631,#86632,#86633,#86634,#86635,
#86636,#86637,#86638,#86639,#86640),(#86641,#86642,#86643,#86644,#86645,
#86646,#86647,#86648,#86649,#86650),(#86651,#86652,#86653,#86654,#86655,
#86656,#86657,#86658,#86659,#86660),(#86661,#86662,#86663,#86664,#86665,
#86666,#86667,#86668,#86669,#86670)),.UNSPECIFIED.,.F.,.F.,.F.,(4,4),(4,
1,1,1,1,1,1,4),(0.0216101418372936,1.00000073923771),(-0.000128988597488103,
0.142857142857143,0.285714285714286,0.428571428571429,0.571428571428571,
0.714285714285714,0.857142857142857,1.00012898859749),.UNSPECIFIED.);
#788=B_SPLINE_SURFACE_WITH_KNOTS('',3,3,((#86689,#86690,#86691,#86692,#86693,
#86694,#86695,#86696,#86697,#86698),(#86699,#86700,#86701,#86702,#86703,
#86704,#86705,#86706,#86707,#86708),(#86709,#86710,#86711,#86712,#86713,
#86714,#86715,#86716,#86717,#86718),(#86719,#86720,#86721,#86722,#86723,
#86724,#86725,#86726,#86727,#86728)),.UNSPECIFIED.,.F.,.F.,.F.,(4,4),(4,
1,1,1,1,1,1,4),(0.,0.978389769713518),(-0.000128900148299539,0.142857142857143,
0.285714285714286,0.428571428571429,0.571428571428571,0.714285714285714,
0.857142857142857,1.0001289001483),.UNSPECIFIED.);
#789=B_SPLINE_SURFACE_WITH_KNOTS('',3,3,((#86739,#86740,#86741,#86742,#86743,
#86744,#86745,#86746,#86747,#86748),(#86749,#86750,#86751,#86752,#86753,
#86754,#86755,#86756,#86757,#86758),(#86759,#86760,#86761,#86762,#86763,
#86764,#86765,#86766,#86767,#86768),(#86769,#86770,#86771,#86772,#86773,
#86774,#86775,#86776,#86777,#86778)),.UNSPECIFIED.,.F.,.F.,.F.,(4,4),(4,
1,1,1,1,1,1,4),(-6.04327751791771E-7,1.),(0.,0.142857142857143,0.285714285714286,
0.428571428571429,0.571428571428571,0.714285714285714,0.857142857142857,
1.),.UNSPECIFIED.);
#790=B_SPLINE_SURFACE_WITH_KNOTS('',3,3,((#86779,#86780,#86781,#86782,#86783,
#86784,#86785,#86786,#86787,#86788),(#86789,#86790,#86791,#86792,#86793,
#86794,#86795,#86796,#86797,#86798),(#86799,#86800,#86801,#86802,#86803,
#86804,#86805,#86806,#86807,#86808),(#86809,#86810,#86811,#86812,#86813,
#86814,#86815,#86816,#86817,#86818)),.UNSPECIFIED.,.F.,.F.,.F.,(4,4),(4,
1,1,1,1,1,1,4),(0.0216103068508826,1.),(-0.000128823583898755,0.142857142857143,
0.285714285714286,0.428571428571429,0.571428571428571,0.714285714285714,
0.857142857142857,1.0001288235839),.UNSPECIFIED.);
#791=B_SPLINE_SURFACE_WITH_KNOTS('',3,3,((#86841,#86842,#86843,#86844,#86845,
#86846,#86847,#86848,#86849,#86850),(#86851,#86852,#86853,#86854,#86855,
#86856,#86857,#86858,#86859,#86860),(#86861,#86862,#86863,#86864,#86865,
#86866,#86867,#86868,#86869,#86870),(#86871,#86872,#86873,#86874,#86875,
#86876,#86877,#86878,#86879,#86880)),.UNSPECIFIED.,.F.,.F.,.F.,(4,4),(4,
1,1,1,1,1,1,4),(0.,0.978389618033113),(-0.000128748467894749,0.142857142857143,
0.285714285714286,0.428571428571429,0.571428571428571,0.714285714285714,
0.857142857142857,1.0001287484679),.UNSPECIFIED.);
#792=B_SPLINE_SURFACE_WITH_KNOTS('',3,3,((#86891,#86892,#86893,#86894,#86895,
#86896,#86897,#86898,#86899,#86900),(#86901,#86902,#86903,#86904,#86905,
#86906,#86907,#86908,#86909,#86910),(#86911,#86912,#86913,#86914,#86915,
#86916,#86917,#86918,#86919,#86920),(#86921,#86922,#86923,#86924,#86925,
#86926,#86927,#86928,#86929,#86930)),.UNSPECIFIED.,.F.,.F.,.F.,(4,4),(4,
1,1,1,1,1,1,4),(0.,1.),(0.,0.142857142857143,0.285714285714286,0.428571428571429,
0.571428571428571,0.714285714285714,0.857142857142857,1.),.UNSPECIFIED.);
#793=B_SPLINE_SURFACE_WITH_KNOTS('',3,3,((#86931,#86932,#86933,#86934,#86935,
#86936,#86937,#86938,#86939,#86940),(#86941,#86942,#86943,#86944,#86945,
#86946,#86947,#86948,#86949,#86950),(#86951,#86952,#86953,#86954,#86955,
#86956,#86957,#86958,#86959,#86960),(#86961,#86962,#86963,#86964,#86965,
#86966,#86967,#86968,#86969,#86970)),.UNSPECIFIED.,.F.,.F.,.F.,(4,4),(4,
1,1,1,1,1,1,4),(0.0216104303767174,1.),(-0.000128700058064298,0.142857142857143,
0.285714285714286,0.428571428571429,0.571428571428571,0.714285714285714,
0.857142857142857,1.00012870005806),.UNSPECIFIED.);
#794=B_SPLINE_SURFACE_WITH_KNOTS('',3,3,((#86993,#86994,#86995,#86996,#86997,
#86998,#86999,#87000,#87001,#87002),(#87003,#87004,#87005,#87006,#87007,
#87008,#87009,#87010,#87011,#87012),(#87013,#87014,#87015,#87016,#87017,
#87018,#87019,#87020,#87021,#87022),(#87023,#87024,#87025,#87026,#87027,
#87028,#87029,#87030,#87031,#87032)),.UNSPECIFIED.,.F.,.F.,.F.,(4,4),(4,
1,1,1,1,1,1,4),(0.,0.978370229937023),(0.,0.142857142857143,0.285714285714286,
0.428571428571429,0.571428571428571,0.714285714285714,0.857142857142857,
1.0001093603718),.UNSPECIFIED.);
#795=B_SPLINE_SURFACE_WITH_KNOTS('',3,3,((#87043,#87044,#87045,#87046,#87047,
#87048,#87049,#87050,#87051,#87052),(#87053,#87054,#87055,#87056,#87057,
#87058,#87059,#87060,#87061,#87062),(#87063,#87064,#87065,#87066,#87067,
#87068,#87069,#87070,#87071,#87072),(#87073,#87074,#87075,#87076,#87077,
#87078,#87079,#87080,#87081,#87082)),.UNSPECIFIED.,.F.,.F.,.F.,(4,4),(4,
1,1,1,1,1,1,4),(0.,1.),(0.,0.142857142857143,0.285714285714286,0.428571428571429,
0.571428571428571,0.714285714285714,0.857142857142857,1.),.UNSPECIFIED.);
#796=FACE_OUTER_BOUND('',#1462,.T.);
#797=FACE_OUTER_BOUND('',#1463,.T.);
#798=FACE_OUTER_BOUND('',#1464,.T.);
#799=FACE_OUTER_BOUND('',#1465,.T.);
#800=FACE_OUTER_BOUND('',#1466,.T.);
#801=FACE_OUTER_BOUND('',#1467,.T.);
#802=FACE_OUTER_BOUND('',#1468,.T.);
#803=FACE_OUTER_BOUND('',#1469,.T.);
#804=FACE_OUTER_BOUND('',#1470,.T.);
#805=FACE_OUTER_BOUND('',#1471,.T.);
#806=FACE_OUTER_BOUND('',#1472,.T.);
#807=FACE_OUTER_BOUND('',#1473,.T.);
#808=FACE_OUTER_BOUND('',#1474,.T.);
#809=FACE_OUTER_BOUND('',#1475,.T.);
#810=FACE_OUTER_BOUND('',#1476,.T.);
#811=FACE_OUTER_BOUND('',#1477,.T.);
#812=FACE_OUTER_BOUND('',#1478,.T.);
#813=FACE_OUTER_BOUND('',#1479,.T.);
#814=FACE_OUTER_BOUND('',#1480,.T.);
#815=FACE_OUTER_BOUND('',#1481,.T.);
#816=FACE_OUTER_BOUND('',#1482,.T.);
#817=FACE_OUTER_BOUND('',#1483,.T.);
#818=FACE_OUTER_BOUND('',#1484,.T.);
#819=FACE_OUTER_BOUND('',#1485,.T.);
#820=FACE_OUTER_BOUND('',#1486,.T.);
#821=FACE_OUTER_BOUND('',#1487,.T.);
#822=FACE_OUTER_BOUND('',#1488,.T.);
#823=FACE_OUTER_BOUND('',#1489,.T.);
#824=FACE_OUTER_BOUND('',#1490,.T.);
#825=FACE_OUTER_BOUND('',#1492,.T.);
#826=FACE_OUTER_BOUND('',#1493,.T.);
#827=FACE_OUTER_BOUND('',#1494,.T.);
#828=FACE_OUTER_BOUND('',#1495,.T.);
#829=FACE_OUTER_BOUND('',#1496,.T.);
#830=FACE_OUTER_BOUND('',#1497,.T.);
#831=FACE_OUTER_BOUND('',#1498,.T.);
#832=FACE_OUTER_BOUND('',#1499,.T.);
#833=FACE_OUTER_BOUND('',#1500,.T.);
#834=FACE_OUTER_BOUND('',#1501,.T.);
#835=FACE_OUTER_BOUND('',#1502,.T.);
#836=FACE_OUTER_BOUND('',#1503,.T.);
#837=FACE_OUTER_BOUND('',#1504,.T.);
#838=FACE_OUTER_BOUND('',#1505,.T.);
#839=FACE_OUTER_BOUND('',#1506,.T.);
#840=FACE_OUTER_BOUND('',#1507,.T.);
#841=FACE_OUTER_BOUND('',#1508,.T.);
#842=FACE_OUTER_BOUND('',#1509,.T.);
#843=FACE_OUTER_BOUND('',#1510,.T.);
#844=FACE_OUTER_BOUND('',#1511,.T.);
#845=FACE_OUTER_BOUND('',#1512,.T.);
#846=FACE_OUTER_BOUND('',#1513,.T.);
#847=FACE_OUTER_BOUND('',#1514,.T.);
#848=FACE_OUTER_BOUND('',#1515,.T.);
#849=FACE_OUTER_BOUND('',#1516,.T.);
#850=FACE_OUTER_BOUND('',#1517,.T.);
#851=FACE_OUTER_BOUND('',#1518,.T.);
#852=FACE_OUTER_BOUND('',#1519,.T.);
#853=FACE_OUTER_BOUND('',#1520,.T.);
#854=FACE_OUTER_BOUND('',#1521,.T.);
#855=FACE_OUTER_BOUND('',#1522,.T.);
#856=FACE_OUTER_BOUND('',#1523,.T.);
#857=FACE_OUTER_BOUND('',#1524,.T.);
#858=FACE_OUTER_BOUND('',#1525,.T.);
#859=FACE_OUTER_BOUND('',#1526,.T.);
#860=FACE_OUTER_BOUND('',#1527,.T.);
#861=FACE_OUTER_BOUND('',#1528,.T.);
#862=FACE_OUTER_BOUND('',#1529,.T.);
#863=FACE_OUTER_BOUND('',#1530,.T.);
#864=FACE_OUTER_BOUND('',#1531,.T.);
#865=FACE_OUTER_BOUND('',#1532,.T.);
#866=FACE_OUTER_BOUND('',#1533,.T.);
#867=FACE_OUTER_BOUND('',#1534,.T.);
#868=FACE_OUTER_BOUND('',#1535,.T.);
#869=FACE_OUTER_BOUND('',#1536,.T.);
#870=FACE_OUTER_BOUND('',#1537,.T.);
#871=FACE_OUTER_BOUND('',#1538,.T.);
#872=FACE_OUTER_BOUND('',#1539,.T.);
#873=FACE_OUTER_BOUND('',#1540,.T.);
#874=FACE_OUTER_BOUND('',#1541,.T.);
#875=FACE_OUTER_BOUND('',#1542,.T.);
#876=FACE_OUTER_BOUND('',#1543,.T.);
#877=FACE_OUTER_BOUND('',#1544,.T.);
#878=FACE_OUTER_BOUND('',#1545,.T.);
#879=FACE_OUTER_BOUND('',#1546,.T.);
#880=FACE_OUTER_BOUND('',#1547,.T.);
#881=FACE_OUTER_BOUND('',#1548,.T.);
#882=FACE_OUTER_BOUND('',#1549,.T.);
#883=FACE_OUTER_BOUND('',#1550,.T.);
#884=FACE_OUTER_BOUND('',#1551,.T.);
#885=FACE_OUTER_BOUND('',#1552,.T.);
#886=FACE_OUTER_BOUND('',#1553,.T.);
#887=FACE_OUTER_BOUND('',#1554,.T.);
#888=FACE_OUTER_BOUND('',#1555,.T.);
#889=FACE_OUTER_BOUND('',#1556,.T.);
#890=FACE_OUTER_BOUND('',#1557,.T.);
#891=FACE_OUTER_BOUND('',#1558,.T.);
#892=FACE_OUTER_BOUND('',#1559,.T.);
#893=FACE_OUTER_BOUND('',#1560,.T.);
#894=FACE_OUTER_BOUND('',#1561,.T.);
#895=FACE_OUTER_BOUND('',#1562,.T.);
#896=FACE_OUTER_BOUND('',#1563,.T.);
#897=FACE_OUTER_BOUND('',#1564,.T.);
#898=FACE_OUTER_BOUND('',#1565,.T.);
#899=FACE_OUTER_BOUND('',#1566,.T.);
#900=FACE_OUTER_BOUND('',#1567,.T.);
#901=FACE_OUTER_BOUND('',#1568,.T.);
#902=FACE_OUTER_BOUND('',#1569,.T.);
#903=FACE_OUTER_BOUND('',#1570,.T.);
#904=FACE_OUTER_BOUND('',#1571,.T.);
#905=FACE_OUTER_BOUND('',#1572,.T.);
#906=FACE_OUTER_BOUND('',#1573,.T.);
#907=FACE_OUTER_BOUND('',#1574,.T.);
#908=FACE_OUTER_BOUND('',#1575,.T.);
#909=FACE_OUTER_BOUND('',#1576,.T.);
#910=FACE_OUTER_BOUND('',#1577,.T.);
#911=FACE_OUTER_BOUND('',#1578,.T.);
#912=FACE_OUTER_BOUND('',#1579,.T.);
#913=FACE_OUTER_BOUND('',#1580,.T.);
#914=FACE_OUTER_BOUND('',#1581,.T.);
#915=FACE_OUTER_BOUND('',#1582,.T.);
#916=FACE_OUTER_BOUND('',#1583,.T.);
#917=FACE_OUTER_BOUND('',#1584,.T.);
#918=FACE_OUTER_BOUND('',#1585,.T.);
#919=FACE_OUTER_BOUND('',#1586,.T.);
#920=FACE_OUTER_BOUND('',#1587,.T.);
#921=FACE_OUTER_BOUND('',#1588,.T.);
#922=FACE_OUTER_BOUND('',#1589,.T.);
#923=FACE_OUTER_BOUND('',#1590,.T.);
#924=FACE_OUTER_BOUND('',#1591,.T.);
#925=FACE_OUTER_BOUND('',#1592,.T.);
#926=FACE_OUTER_BOUND('',#1593,.T.);
#927=FACE_OUTER_BOUND('',#1594,.T.);
#928=FACE_OUTER_BOUND('',#1595,.T.);
#929=FACE_OUTER_BOUND('',#1596,.T.);
#930=FACE_OUTER_BOUND('',#1597,.T.);
#931=FACE_OUTER_BOUND('',#1598,.T.);
#932=FACE_OUTER_BOUND('',#1599,.T.);
#933=FACE_OUTER_BOUND('',#1600,.T.);
#934=FACE_OUTER_BOUND('',#1601,.T.);
#935=FACE_OUTER_BOUND('',#1602,.T.);
#936=FACE_OUTER_BOUND('',#1603,.T.);
#937=FACE_OUTER_BOUND('',#1604,.T.);
#938=FACE_OUTER_BOUND('',#1605,.T.);
#939=FACE_OUTER_BOUND('',#1606,.T.);
#940=FACE_OUTER_BOUND('',#1607,.T.);
#941=FACE_OUTER_BOUND('',#1608,.T.);
#942=FACE_OUTER_BOUND('',#1609,.T.);
#943=FACE_OUTER_BOUND('',#1610,.T.);
#944=FACE_OUTER_BOUND('',#1611,.T.);
#945=FACE_OUTER_BOUND('',#1612,.T.);
#946=FACE_OUTER_BOUND('',#1613,.T.);
#947=FACE_OUTER_BOUND('',#1614,.T.);
#948=FACE_OUTER_BOUND('',#1615,.T.);
#949=FACE_OUTER_BOUND('',#1616,.T.);
#950=FACE_OUTER_BOUND('',#1617,.T.);
#951=FACE_OUTER_BOUND('',#1618,.T.);
#952=FACE_OUTER_BOUND('',#1619,.T.);
#953=FACE_OUTER_BOUND('',#1620,.T.);
#954=FACE_OUTER_BOUND('',#1621,.T.);
#955=FACE_OUTER_BOUND('',#1622,.T.);
#956=FACE_OUTER_BOUND('',#1623,.T.);
#957=FACE_OUTER_BOUND('',#1624,.T.);
#958=FACE_OUTER_BOUND('',#1625,.T.);
#959=FACE_OUTER_BOUND('',#1626,.T.);
#960=FACE_OUTER_BOUND('',#1627,.T.);
#961=FACE_OUTER_BOUND('',#1628,.T.);
#962=FACE_OUTER_BOUND('',#1629,.T.);
#963=FACE_OUTER_BOUND('',#1630,.T.);
#964=FACE_OUTER_BOUND('',#1631,.T.);
#965=FACE_OUTER_BOUND('',#1632,.T.);
#966=FACE_OUTER_BOUND('',#1633,.T.);
#967=FACE_OUTER_BOUND('',#1634,.T.);
#968=FACE_OUTER_BOUND('',#1635,.T.);
#969=FACE_OUTER_BOUND('',#1636,.T.);
#970=FACE_OUTER_BOUND('',#1637,.T.);
#971=FACE_OUTER_BOUND('',#1638,.T.);
#972=FACE_OUTER_BOUND('',#1639,.T.);
#973=FACE_OUTER_BOUND('',#1640,.T.);
#974=FACE_OUTER_BOUND('',#1641,.T.);
#975=FACE_OUTER_BOUND('',#1642,.T.);
#976=FACE_OUTER_BOUND('',#1643,.T.);
#977=FACE_OUTER_BOUND('',#1644,.T.);
#978=FACE_OUTER_BOUND('',#1645,.T.);
#979=FACE_OUTER_BOUND('',#1646,.T.);
#980=FACE_OUTER_BOUND('',#1647,.T.);
#981=FACE_OUTER_BOUND('',#1648,.T.);
#982=FACE_OUTER_BOUND('',#1649,.T.);
#983=FACE_OUTER_BOUND('',#1650,.T.);
#984=FACE_OUTER_BOUND('',#1651,.T.);
#985=FACE_OUTER_BOUND('',#1652,.T.);
#986=FACE_OUTER_BOUND('',#1653,.T.);
#987=FACE_OUTER_BOUND('',#1654,.T.);
#988=FACE_OUTER_BOUND('',#1655,.T.);
#989=FACE_OUTER_BOUND('',#1656,.T.);
#990=FACE_OUTER_BOUND('',#1657,.T.);
#991=FACE_OUTER_BOUND('',#1658,.T.);
#992=FACE_OUTER_BOUND('',#1659,.T.);
#993=FACE_OUTER_BOUND('',#1660,.T.);
#994=FACE_OUTER_BOUND('',#1661,.T.);
#995=FACE_OUTER_BOUND('',#1662,.T.);
#996=FACE_OUTER_BOUND('',#1663,.T.);
#997=FACE_OUTER_BOUND('',#1664,.T.);
#998=FACE_OUTER_BOUND('',#1665,.T.);
#999=FACE_OUTER_BOUND('',#1666,.T.);
#1000=FACE_OUTER_BOUND('',#1667,.T.);
#1001=FACE_OUTER_BOUND('',#1668,.T.);
#1002=FACE_OUTER_BOUND('',#1669,.T.);
#1003=FACE_OUTER_BOUND('',#1670,.T.);
#1004=FACE_OUTER_BOUND('',#1671,.T.);
#1005=FACE_OUTER_BOUND('',#1672,.T.);
#1006=FACE_OUTER_BOUND('',#1673,.T.);
#1007=FACE_OUTER_BOUND('',#1674,.T.);
#1008=FACE_OUTER_BOUND('',#1675,.T.);
#1009=FACE_OUTER_BOUND('',#1676,.T.);
#1010=FACE_OUTER_BOUND('',#1677,.T.);
#1011=FACE_OUTER_BOUND('',#1678,.T.);
#1012=FACE_OUTER_BOUND('',#1679,.T.);
#1013=FACE_OUTER_BOUND('',#1680,.T.);
#1014=FACE_OUTER_BOUND('',#1681,.T.);
#1015=FACE_OUTER_BOUND('',#1682,.T.);
#1016=FACE_OUTER_BOUND('',#1683,.T.);
#1017=FACE_OUTER_BOUND('',#1684,.T.);
#1018=FACE_OUTER_BOUND('',#1685,.T.);
#1019=FACE_OUTER_BOUND('',#1686,.T.);
#1020=FACE_OUTER_BOUND('',#1687,.T.);
#1021=FACE_OUTER_BOUND('',#1688,.T.);
#1022=FACE_OUTER_BOUND('',#1689,.T.);
#1023=FACE_OUTER_BOUND('',#1690,.T.);
#1024=FACE_OUTER_BOUND('',#1691,.T.);
#1025=FACE_OUTER_BOUND('',#1692,.T.);
#1026=FACE_OUTER_BOUND('',#1693,.T.);
#1027=FACE_OUTER_BOUND('',#1694,.T.);
#1028=FACE_OUTER_BOUND('',#1695,.T.);
#1029=FACE_OUTER_BOUND('',#1696,.T.);
#1030=FACE_OUTER_BOUND('',#1697,.T.);
#1031=FACE_OUTER_BOUND('',#1698,.T.);
#1032=FACE_OUTER_BOUND('',#1699,.T.);
#1033=FACE_OUTER_BOUND('',#1700,.T.);
#1034=FACE_OUTER_BOUND('',#1701,.T.);
#1035=FACE_OUTER_BOUND('',#1702,.T.);
#1036=FACE_OUTER_BOUND('',#1703,.T.);
#1037=FACE_OUTER_BOUND('',#1704,.T.);
#1038=FACE_OUTER_BOUND('',#1705,.T.);
#1039=FACE_OUTER_BOUND('',#1706,.T.);
#1040=FACE_OUTER_BOUND('',#1707,.T.);
#1041=FACE_OUTER_BOUND('',#1708,.T.);
#1042=FACE_OUTER_BOUND('',#1709,.T.);
#1043=FACE_OUTER_BOUND('',#1710,.T.);
#1044=FACE_OUTER_BOUND('',#1711,.T.);
#1045=FACE_OUTER_BOUND('',#1712,.T.);
#1046=FACE_OUTER_BOUND('',#1713,.T.);
#1047=FACE_OUTER_BOUND('',#1714,.T.);
#1048=FACE_OUTER_BOUND('',#1715,.T.);
#1049=FACE_OUTER_BOUND('',#1716,.T.);
#1050=FACE_OUTER_BOUND('',#1717,.T.);
#1051=FACE_OUTER_BOUND('',#1718,.T.);
#1052=FACE_OUTER_BOUND('',#1719,.T.);
#1053=FACE_OUTER_BOUND('',#1721,.T.);
#1054=FACE_OUTER_BOUND('',#1722,.T.);
#1055=FACE_OUTER_BOUND('',#1723,.T.);
#1056=FACE_OUTER_BOUND('',#1724,.T.);
#1057=FACE_OUTER_BOUND('',#1725,.T.);
#1058=FACE_OUTER_BOUND('',#1726,.T.);
#1059=FACE_OUTER_BOUND('',#1727,.T.);
#1060=FACE_OUTER_BOUND('',#1728,.T.);
#1061=FACE_OUTER_BOUND('',#1729,.T.);
#1062=FACE_OUTER_BOUND('',#1730,.T.);
#1063=FACE_OUTER_BOUND('',#1731,.T.);
#1064=FACE_OUTER_BOUND('',#1732,.T.);
#1065=FACE_OUTER_BOUND('',#1733,.T.);
#1066=FACE_OUTER_BOUND('',#1734,.T.);
#1067=FACE_OUTER_BOUND('',#1735,.T.);
#1068=FACE_OUTER_BOUND('',#1736,.T.);
#1069=FACE_OUTER_BOUND('',#1737,.T.);
#1070=FACE_OUTER_BOUND('',#1738,.T.);
#1071=FACE_OUTER_BOUND('',#1739,.T.);
#1072=FACE_OUTER_BOUND('',#1740,.T.);
#1073=FACE_OUTER_BOUND('',#1741,.T.);
#1074=FACE_OUTER_BOUND('',#1742,.T.);
#1075=FACE_OUTER_BOUND('',#1743,.T.);
#1076=FACE_OUTER_BOUND('',#1744,.T.);
#1077=FACE_OUTER_BOUND('',#1745,.T.);
#1078=FACE_OUTER_BOUND('',#1746,.T.);
#1079=FACE_OUTER_BOUND('',#1747,.T.);
#1080=FACE_OUTER_BOUND('',#1748,.T.);
#1081=FACE_OUTER_BOUND('',#1749,.T.);
#1082=FACE_OUTER_BOUND('',#1750,.T.);
#1083=FACE_OUTER_BOUND('',#1751,.T.);
#1084=FACE_OUTER_BOUND('',#1752,.T.);
#1085=FACE_OUTER_BOUND('',#1753,.T.);
#1086=FACE_OUTER_BOUND('',#1754,.T.);
#1087=FACE_OUTER_BOUND('',#1755,.T.);
#1088=FACE_OUTER_BOUND('',#1756,.T.);
#1089=FACE_OUTER_BOUND('',#1757,.T.);
#1090=FACE_OUTER_BOUND('',#1758,.T.);
#1091=FACE_OUTER_BOUND('',#1759,.T.);
#1092=FACE_OUTER_BOUND('',#1760,.T.);
#1093=FACE_OUTER_BOUND('',#1761,.T.);
#1094=FACE_OUTER_BOUND('',#1762,.T.);
#1095=FACE_OUTER_BOUND('',#1763,.T.);
#1096=FACE_OUTER_BOUND('',#1764,.T.);
#1097=FACE_OUTER_BOUND('',#1765,.T.);
#1098=FACE_OUTER_BOUND('',#1766,.T.);
#1099=FACE_OUTER_BOUND('',#1767,.T.);
#1100=FACE_OUTER_BOUND('',#1768,.T.);
#1101=FACE_OUTER_BOUND('',#1769,.T.);
#1102=FACE_OUTER_BOUND('',#1770,.T.);
#1103=FACE_OUTER_BOUND('',#1771,.T.);
#1104=FACE_OUTER_BOUND('',#1772,.T.);
#1105=FACE_OUTER_BOUND('',#1773,.T.);
#1106=FACE_OUTER_BOUND('',#1774,.T.);
#1107=FACE_OUTER_BOUND('',#1775,.T.);
#1108=FACE_OUTER_BOUND('',#1776,.T.);
#1109=FACE_OUTER_BOUND('',#1777,.T.);
#1110=FACE_OUTER_BOUND('',#1778,.T.);
#1111=FACE_OUTER_BOUND('',#1779,.T.);
#1112=FACE_OUTER_BOUND('',#1780,.T.);
#1113=FACE_OUTER_BOUND('',#1781,.T.);
#1114=FACE_OUTER_BOUND('',#1782,.T.);
#1115=FACE_OUTER_BOUND('',#1783,.T.);
#1116=FACE_OUTER_BOUND('',#1784,.T.);
#1117=FACE_OUTER_BOUND('',#1785,.T.);
#1118=FACE_OUTER_BOUND('',#1786,.T.);
#1119=FACE_OUTER_BOUND('',#1787,.T.);
#1120=FACE_OUTER_BOUND('',#1792,.T.);
#1121=FACE_OUTER_BOUND('',#1793,.T.);
#1122=FACE_OUTER_BOUND('',#1798,.T.);
#1123=FACE_OUTER_BOUND('',#1799,.T.);
#1124=FACE_OUTER_BOUND('',#1800,.T.);
#1125=FACE_OUTER_BOUND('',#1801,.T.);
#1126=FACE_OUTER_BOUND('',#1802,.T.);
#1127=FACE_OUTER_BOUND('',#1803,.T.);
#1128=FACE_OUTER_BOUND('',#1804,.T.);
#1129=FACE_OUTER_BOUND('',#1805,.T.);
#1130=FACE_OUTER_BOUND('',#1806,.T.);
#1131=FACE_OUTER_BOUND('',#1807,.T.);
#1132=FACE_OUTER_BOUND('',#1808,.T.);
#1133=FACE_OUTER_BOUND('',#1809,.T.);
#1134=FACE_OUTER_BOUND('',#1810,.T.);
#1135=FACE_OUTER_BOUND('',#1811,.T.);
#1136=FACE_OUTER_BOUND('',#1812,.T.);
#1137=FACE_OUTER_BOUND('',#1813,.T.);
#1138=FACE_OUTER_BOUND('',#1814,.T.);
#1139=FACE_OUTER_BOUND('',#1815,.T.);
#1140=FACE_OUTER_BOUND('',#1816,.T.);
#1141=FACE_OUTER_BOUND('',#1817,.T.);
#1142=FACE_OUTER_BOUND('',#1818,.T.);
#1143=FACE_OUTER_BOUND('',#1819,.T.);
#1144=FACE_OUTER_BOUND('',#1820,.T.);
#1145=FACE_OUTER_BOUND('',#1821,.T.);
#1146=FACE_OUTER_BOUND('',#1822,.T.);
#1147=FACE_OUTER_BOUND('',#1823,.T.);
#1148=FACE_OUTER_BOUND('',#1824,.T.);
#1149=FACE_OUTER_BOUND('',#1825,.T.);
#1150=FACE_OUTER_BOUND('',#1826,.T.);
#1151=FACE_OUTER_BOUND('',#1827,.T.);
#1152=FACE_OUTER_BOUND('',#1828,.T.);
#1153=FACE_OUTER_BOUND('',#1829,.T.);
#1154=FACE_OUTER_BOUND('',#1830,.T.);
#1155=FACE_OUTER_BOUND('',#1831,.T.);
#1156=FACE_OUTER_BOUND('',#1832,.T.);
#1157=FACE_OUTER_BOUND('',#1833,.T.);
#1158=FACE_OUTER_BOUND('',#1834,.T.);
#1159=FACE_OUTER_BOUND('',#1835,.T.);
#1160=FACE_OUTER_BOUND('',#1836,.T.);
#1161=FACE_OUTER_BOUND('',#1837,.T.);
#1162=FACE_OUTER_BOUND('',#1838,.T.);
#1163=FACE_OUTER_BOUND('',#1839,.T.);
#1164=FACE_OUTER_BOUND('',#1840,.T.);
#1165=FACE_OUTER_BOUND('',#1841,.T.);
#1166=FACE_OUTER_BOUND('',#1842,.T.);
#1167=FACE_OUTER_BOUND('',#1843,.T.);
#1168=FACE_OUTER_BOUND('',#1844,.T.);
#1169=FACE_OUTER_BOUND('',#1845,.T.);
#1170=FACE_OUTER_BOUND('',#1846,.T.);
#1171=FACE_OUTER_BOUND('',#1847,.T.);
#1172=FACE_OUTER_BOUND('',#1848,.T.);
#1173=FACE_OUTER_BOUND('',#1849,.T.);
#1174=FACE_OUTER_BOUND('',#1850,.T.);
#1175=FACE_OUTER_BOUND('',#1851,.T.);
#1176=FACE_OUTER_BOUND('',#1852,.T.);
#1177=FACE_OUTER_BOUND('',#1853,.T.);
#1178=FACE_OUTER_BOUND('',#1854,.T.);
#1179=FACE_OUTER_BOUND('',#1855,.T.);
#1180=FACE_OUTER_BOUND('',#1856,.T.);
#1181=FACE_OUTER_BOUND('',#1857,.T.);
#1182=FACE_OUTER_BOUND('',#1858,.T.);
#1183=FACE_OUTER_BOUND('',#1859,.T.);
#1184=FACE_OUTER_BOUND('',#1860,.T.);
#1185=FACE_OUTER_BOUND('',#1861,.T.);
#1186=FACE_OUTER_BOUND('',#1862,.T.);
#1187=FACE_OUTER_BOUND('',#1863,.T.);
#1188=FACE_OUTER_BOUND('',#1864,.T.);
#1189=FACE_OUTER_BOUND('',#1865,.T.);
#1190=FACE_OUTER_BOUND('',#1866,.T.);
#1191=FACE_OUTER_BOUND('',#1867,.T.);
#1192=FACE_OUTER_BOUND('',#1868,.T.);
#1193=FACE_OUTER_BOUND('',#1874,.T.);
#1194=FACE_OUTER_BOUND('',#1875,.T.);
#1195=FACE_OUTER_BOUND('',#1880,.T.);
#1196=FACE_OUTER_BOUND('',#1881,.T.);
#1197=FACE_OUTER_BOUND('',#1882,.T.);
#1198=FACE_OUTER_BOUND('',#1883,.T.);
#1199=FACE_OUTER_BOUND('',#1884,.T.);
#1200=FACE_OUTER_BOUND('',#1885,.T.);
#1201=FACE_OUTER_BOUND('',#1886,.T.);
#1202=FACE_OUTER_BOUND('',#1887,.T.);
#1203=FACE_OUTER_BOUND('',#1888,.T.);
#1204=FACE_OUTER_BOUND('',#1890,.T.);
#1205=FACE_OUTER_BOUND('',#1891,.T.);
#1206=FACE_OUTER_BOUND('',#1892,.T.);
#1207=FACE_OUTER_BOUND('',#1893,.T.);
#1208=FACE_OUTER_BOUND('',#1895,.T.);
#1209=FACE_OUTER_BOUND('',#1896,.T.);
#1210=FACE_OUTER_BOUND('',#1897,.T.);
#1211=FACE_OUTER_BOUND('',#1898,.T.);
#1212=FACE_OUTER_BOUND('',#1899,.T.);
#1213=FACE_OUTER_BOUND('',#1900,.T.);
#1214=FACE_OUTER_BOUND('',#1901,.T.);
#1215=FACE_OUTER_BOUND('',#1902,.T.);
#1216=FACE_OUTER_BOUND('',#1903,.T.);
#1217=FACE_OUTER_BOUND('',#1904,.T.);
#1218=FACE_OUTER_BOUND('',#1905,.T.);
#1219=FACE_OUTER_BOUND('',#1906,.T.);
#1220=FACE_OUTER_BOUND('',#1907,.T.);
#1221=FACE_OUTER_BOUND('',#1908,.T.);
#1222=FACE_OUTER_BOUND('',#1909,.T.);
#1223=FACE_OUTER_BOUND('',#1910,.T.);
#1224=FACE_OUTER_BOUND('',#1911,.T.);
#1225=FACE_OUTER_BOUND('',#1912,.T.);
#1226=FACE_OUTER_BOUND('',#1913,.T.);
#1227=FACE_OUTER_BOUND('',#1914,.T.);
#1228=FACE_OUTER_BOUND('',#1915,.T.);
#1229=FACE_OUTER_BOUND('',#1916,.T.);
#1230=FACE_OUTER_BOUND('',#1917,.T.);
#1231=FACE_OUTER_BOUND('',#1918,.T.);
#1232=FACE_OUTER_BOUND('',#1919,.T.);
#1233=FACE_OUTER_BOUND('',#1920,.T.);
#1234=FACE_OUTER_BOUND('',#1921,.T.);
#1235=FACE_OUTER_BOUND('',#1922,.T.);
#1236=FACE_OUTER_BOUND('',#1923,.T.);
#1237=FACE_OUTER_BOUND('',#1924,.T.);
#1238=FACE_OUTER_BOUND('',#1925,.T.);
#1239=FACE_OUTER_BOUND('',#1926,.T.);
#1240=FACE_OUTER_BOUND('',#1927,.T.);
#1241=FACE_OUTER_BOUND('',#1928,.T.);
#1242=FACE_OUTER_BOUND('',#1929,.T.);
#1243=FACE_OUTER_BOUND('',#1930,.T.);
#1244=FACE_OUTER_BOUND('',#1931,.T.);
#1245=FACE_OUTER_BOUND('',#1932,.T.);
#1246=FACE_OUTER_BOUND('',#1933,.T.);
#1247=FACE_OUTER_BOUND('',#1934,.T.);
#1248=FACE_OUTER_BOUND('',#1935,.T.);
#1249=FACE_OUTER_BOUND('',#1936,.T.);
#1250=FACE_OUTER_BOUND('',#1942,.T.);
#1251=FACE_OUTER_BOUND('',#1943,.T.);
#1252=FACE_OUTER_BOUND('',#1944,.T.);
#1253=FACE_OUTER_BOUND('',#1945,.T.);
#1254=FACE_OUTER_BOUND('',#1946,.T.);
#1255=FACE_OUTER_BOUND('',#1947,.T.);
#1256=FACE_OUTER_BOUND('',#1953,.T.);
#1257=FACE_OUTER_BOUND('',#1954,.T.);
#1258=FACE_OUTER_BOUND('',#1955,.T.);
#1259=FACE_OUTER_BOUND('',#1956,.T.);
#1260=FACE_OUTER_BOUND('',#1957,.T.);
#1261=FACE_OUTER_BOUND('',#1958,.T.);
#1262=FACE_OUTER_BOUND('',#1959,.T.);
#1263=FACE_OUTER_BOUND('',#1960,.T.);
#1264=FACE_OUTER_BOUND('',#1961,.T.);
#1265=FACE_OUTER_BOUND('',#1962,.T.);
#1266=FACE_OUTER_BOUND('',#1963,.T.);
#1267=FACE_OUTER_BOUND('',#1964,.T.);
#1268=FACE_OUTER_BOUND('',#1965,.T.);
#1269=FACE_OUTER_BOUND('',#1966,.T.);
#1270=FACE_OUTER_BOUND('',#1967,.T.);
#1271=FACE_OUTER_BOUND('',#1968,.T.);
#1272=FACE_OUTER_BOUND('',#1969,.T.);
#1273=FACE_OUTER_BOUND('',#1970,.T.);
#1274=FACE_OUTER_BOUND('',#1971,.T.);
#1275=FACE_OUTER_BOUND('',#1972,.T.);
#1276=FACE_OUTER_BOUND('',#1973,.T.);
#1277=FACE_OUTER_BOUND('',#1978,.T.);
#1278=FACE_OUTER_BOUND('',#1979,.T.);
#1279=FACE_OUTER_BOUND('',#1980,.T.);
#1280=FACE_OUTER_BOUND('',#1981,.T.);
#1281=FACE_OUTER_BOUND('',#1982,.T.);
#1282=FACE_OUTER_BOUND('',#1983,.T.);
#1283=FACE_OUTER_BOUND('',#1984,.T.);
#1284=FACE_OUTER_BOUND('',#1985,.T.);
#1285=FACE_OUTER_BOUND('',#1986,.T.);
#1286=FACE_OUTER_BOUND('',#1987,.T.);
#1287=FACE_OUTER_BOUND('',#1988,.T.);
#1288=FACE_OUTER_BOUND('',#1989,.T.);
#1289=FACE_OUTER_BOUND('',#1990,.T.);
#1290=FACE_OUTER_BOUND('',#1991,.T.);
#1291=FACE_OUTER_BOUND('',#1992,.T.);
#1292=FACE_OUTER_BOUND('',#1993,.T.);
#1293=FACE_OUTER_BOUND('',#1994,.T.);
#1294=FACE_OUTER_BOUND('',#1996,.T.);
#1295=FACE_OUTER_BOUND('',#1997,.T.);
#1296=FACE_OUTER_BOUND('',#1998,.T.);
#1297=FACE_OUTER_BOUND('',#2000,.T.);
#1298=FACE_OUTER_BOUND('',#2002,.T.);
#1299=FACE_OUTER_BOUND('',#2008,.T.);
#1300=FACE_OUTER_BOUND('',#2009,.T.);
#1301=FACE_OUTER_BOUND('',#2014,.T.);
#1302=FACE_OUTER_BOUND('',#2020,.T.);
#1303=FACE_OUTER_BOUND('',#2021,.T.);
#1304=FACE_OUTER_BOUND('',#2022,.T.);
#1305=FACE_OUTER_BOUND('',#2023,.T.);
#1306=FACE_OUTER_BOUND('',#2024,.T.);
#1307=FACE_OUTER_BOUND('',#2025,.T.);
#1308=FACE_OUTER_BOUND('',#2030,.T.);
#1309=FACE_OUTER_BOUND('',#2031,.T.);
#1310=FACE_OUTER_BOUND('',#2036,.T.);
#1311=FACE_OUTER_BOUND('',#2037,.T.);
#1312=FACE_OUTER_BOUND('',#2038,.T.);
#1313=FACE_OUTER_BOUND('',#2039,.T.);
#1314=FACE_OUTER_BOUND('',#2040,.T.);
#1315=FACE_OUTER_BOUND('',#2041,.T.);
#1316=FACE_OUTER_BOUND('',#2042,.T.);
#1317=FACE_OUTER_BOUND('',#2043,.T.);
#1318=FACE_OUTER_BOUND('',#2044,.T.);
#1319=FACE_OUTER_BOUND('',#2045,.T.);
#1320=FACE_OUTER_BOUND('',#2046,.T.);
#1321=FACE_OUTER_BOUND('',#2048,.T.);
#1322=FACE_OUTER_BOUND('',#2050,.T.);
#1323=FACE_OUTER_BOUND('',#2051,.T.);
#1324=FACE_OUTER_BOUND('',#2052,.T.);
#1325=FACE_OUTER_BOUND('',#2053,.T.);
#1326=FACE_OUTER_BOUND('',#2054,.T.);
#1327=FACE_OUTER_BOUND('',#2055,.T.);
#1328=FACE_OUTER_BOUND('',#2057,.T.);
#1329=FACE_OUTER_BOUND('',#2059,.T.);
#1330=FACE_OUTER_BOUND('',#2060,.T.);
#1331=FACE_OUTER_BOUND('',#2061,.T.);
#1332=FACE_OUTER_BOUND('',#2062,.T.);
#1333=FACE_OUTER_BOUND('',#2063,.T.);
#1334=FACE_OUTER_BOUND('',#2065,.T.);
#1335=FACE_OUTER_BOUND('',#2067,.T.);
#1336=FACE_OUTER_BOUND('',#2068,.T.);
#1337=FACE_OUTER_BOUND('',#2069,.T.);
#1338=FACE_OUTER_BOUND('',#2070,.T.);
#1339=FACE_OUTER_BOUND('',#2071,.T.);
#1340=FACE_OUTER_BOUND('',#2072,.T.);
#1341=FACE_OUTER_BOUND('',#2073,.T.);
#1342=FACE_OUTER_BOUND('',#2074,.T.);
#1343=FACE_OUTER_BOUND('',#2075,.T.);
#1344=FACE_OUTER_BOUND('',#2076,.T.);
#1345=FACE_OUTER_BOUND('',#2077,.T.);
#1346=FACE_OUTER_BOUND('',#2079,.T.);
#1347=FACE_OUTER_BOUND('',#2081,.T.);
#1348=FACE_OUTER_BOUND('',#2082,.T.);
#1349=FACE_OUTER_BOUND('',#2083,.T.);
#1350=FACE_OUTER_BOUND('',#2084,.T.);
#1351=FACE_OUTER_BOUND('',#2085,.T.);
#1352=FACE_OUTER_BOUND('',#2086,.T.);
#1353=FACE_OUTER_BOUND('',#2087,.T.);
#1354=FACE_OUTER_BOUND('',#2088,.T.);
#1355=FACE_OUTER_BOUND('',#2089,.T.);
#1356=FACE_OUTER_BOUND('',#2090,.T.);
#1357=FACE_OUTER_BOUND('',#2091,.T.);
#1358=FACE_OUTER_BOUND('',#2092,.T.);
#1359=FACE_OUTER_BOUND('',#2093,.T.);
#1360=FACE_OUTER_BOUND('',#2094,.T.);
#1361=FACE_OUTER_BOUND('',#2095,.T.);
#1362=FACE_OUTER_BOUND('',#2097,.T.);
#1363=FACE_OUTER_BOUND('',#2098,.T.);
#1364=FACE_OUTER_BOUND('',#2099,.T.);
#1365=FACE_OUTER_BOUND('',#2100,.T.);
#1366=FACE_OUTER_BOUND('',#2101,.T.);
#1367=FACE_OUTER_BOUND('',#2103,.T.);
#1368=FACE_OUTER_BOUND('',#2105,.T.);
#1369=FACE_OUTER_BOUND('',#2106,.T.);
#1370=FACE_OUTER_BOUND('',#2107,.T.);
#1371=FACE_OUTER_BOUND('',#2108,.T.);
#1372=FACE_OUTER_BOUND('',#2109,.T.);
#1373=FACE_OUTER_BOUND('',#2110,.T.);
#1374=FACE_OUTER_BOUND('',#2121,.T.);
#1375=FACE_OUTER_BOUND('',#2132,.T.);
#1376=FACE_OUTER_BOUND('',#2133,.T.);
#1377=FACE_OUTER_BOUND('',#2134,.T.);
#1378=FACE_OUTER_BOUND('',#2135,.T.);
#1379=FACE_OUTER_BOUND('',#2136,.T.);
#1380=FACE_OUTER_BOUND('',#2137,.T.);
#1381=FACE_OUTER_BOUND('',#2138,.T.);
#1382=FACE_OUTER_BOUND('',#2139,.T.);
#1383=FACE_OUTER_BOUND('',#2140,.T.);
#1384=FACE_OUTER_BOUND('',#2141,.T.);
#1385=FACE_OUTER_BOUND('',#2142,.T.);
#1386=FACE_OUTER_BOUND('',#2143,.T.);
#1387=FACE_OUTER_BOUND('',#2144,.T.);
#1388=FACE_OUTER_BOUND('',#2145,.T.);
#1389=FACE_OUTER_BOUND('',#2146,.T.);
#1390=FACE_OUTER_BOUND('',#2147,.T.);
#1391=FACE_OUTER_BOUND('',#2148,.T.);
#1392=FACE_OUTER_BOUND('',#2149,.T.);
#1393=FACE_OUTER_BOUND('',#2150,.T.);
#1394=FACE_OUTER_BOUND('',#2151,.T.);
#1395=FACE_OUTER_BOUND('',#2152,.T.);
#1396=FACE_OUTER_BOUND('',#2153,.T.);
#1397=FACE_OUTER_BOUND('',#2154,.T.);
#1398=FACE_OUTER_BOUND('',#2155,.T.);
#1399=FACE_OUTER_BOUND('',#2156,.T.);
#1400=FACE_OUTER_BOUND('',#2157,.T.);
#1401=FACE_OUTER_BOUND('',#2158,.T.);
#1402=FACE_OUTER_BOUND('',#2159,.T.);
#1403=FACE_OUTER_BOUND('',#2160,.T.);
#1404=FACE_OUTER_BOUND('',#2161,.T.);
#1405=FACE_OUTER_BOUND('',#2162,.T.);
#1406=FACE_OUTER_BOUND('',#2163,.T.);
#1407=FACE_OUTER_BOUND('',#2164,.T.);
#1408=FACE_OUTER_BOUND('',#2165,.T.);
#1409=FACE_OUTER_BOUND('',#2166,.T.);
#1410=FACE_OUTER_BOUND('',#2167,.T.);
#1411=FACE_OUTER_BOUND('',#2168,.T.);
#1412=FACE_OUTER_BOUND('',#2169,.T.);
#1413=FACE_OUTER_BOUND('',#2170,.T.);
#1414=FACE_OUTER_BOUND('',#2171,.T.);
#1415=FACE_OUTER_BOUND('',#2172,.T.);
#1416=FACE_OUTER_BOUND('',#2173,.T.);
#1417=FACE_OUTER_BOUND('',#2174,.T.);
#1418=FACE_OUTER_BOUND('',#2175,.T.);
#1419=FACE_OUTER_BOUND('',#2176,.T.);
#1420=FACE_OUTER_BOUND('',#2177,.T.);
#1421=FACE_OUTER_BOUND('',#2178,.T.);
#1422=FACE_OUTER_BOUND('',#2179,.T.);
#1423=FACE_OUTER_BOUND('',#2180,.T.);
#1424=FACE_OUTER_BOUND('',#2181,.T.);
#1425=FACE_OUTER_BOUND('',#2182,.T.);
#1426=FACE_OUTER_BOUND('',#2183,.T.);
#1427=FACE_OUTER_BOUND('',#2184,.T.);
#1428=FACE_OUTER_BOUND('',#2186,.T.);
#1429=FACE_OUTER_BOUND('',#2188,.T.);
#1430=FACE_OUTER_BOUND('',#2189,.T.);
#1431=FACE_OUTER_BOUND('',#2190,.T.);
#1432=FACE_OUTER_BOUND('',#2191,.T.);
#1433=FACE_OUTER_BOUND('',#2192,.T.);
#1434=FACE_OUTER_BOUND('',#2193,.T.);
#1435=FACE_OUTER_BOUND('',#2194,.T.);
#1436=FACE_OUTER_BOUND('',#2195,.T.);
#1437=FACE_OUTER_BOUND('',#2196,.T.);
#1438=FACE_OUTER_BOUND('',#2197,.T.);
#1439=FACE_OUTER_BOUND('',#2198,.T.);
#1440=FACE_OUTER_BOUND('',#2199,.T.);
#1441=FACE_OUTER_BOUND('',#2200,.T.);
#1442=FACE_OUTER_BOUND('',#2201,.T.);
#1443=FACE_OUTER_BOUND('',#2202,.T.);
#1444=FACE_OUTER_BOUND('',#2203,.T.);
#1445=FACE_OUTER_BOUND('',#2204,.T.);
#1446=FACE_OUTER_BOUND('',#2205,.T.);
#1447=FACE_OUTER_BOUND('',#2206,.T.);
#1448=FACE_OUTER_BOUND('',#2207,.T.);
#1449=FACE_OUTER_BOUND('',#2208,.T.);
#1450=FACE_OUTER_BOUND('',#2209,.T.);
#1451=FACE_OUTER_BOUND('',#2210,.T.);
#1452=FACE_OUTER_BOUND('',#2211,.T.);
#1453=FACE_OUTER_BOUND('',#2212,.T.);
#1454=FACE_OUTER_BOUND('',#2213,.T.);
#1455=FACE_OUTER_BOUND('',#2214,.T.);
#1456=FACE_OUTER_BOUND('',#2215,.T.);
#1457=FACE_OUTER_BOUND('',#2216,.T.);
#1458=FACE_OUTER_BOUND('',#2217,.T.);
#1459=FACE_OUTER_BOUND('',#2218,.T.);
#1460=FACE_OUTER_BOUND('',#2219,.T.);
#1461=FACE_OUTER_BOUND('',#2220,.T.);
#1462=EDGE_LOOP('',(#8072,#8073,#8074,#8075));
#1463=EDGE_LOOP('',(#8076,#8077,#8078,#8079,#8080,#8081));
#1464=EDGE_LOOP('',(#8082,#8083,#8084,#8085,#8086,#8087));
#1465=EDGE_LOOP('',(#8088,#8089,#8090,#8091,#8092,#8093));
#1466=EDGE_LOOP('',(#8094,#8095,#8096,#8097,#8098,#8099));
#1467=EDGE_LOOP('',(#8100,#8101,#8102,#8103,#8104,#8105));
#1468=EDGE_LOOP('',(#8106,#8107,#8108,#8109,#8110,#8111));
#1469=EDGE_LOOP('',(#8112,#8113,#8114,#8115,#8116,#8117));
#1470=EDGE_LOOP('',(#8118,#8119,#8120,#8121,#8122,#8123));
#1471=EDGE_LOOP('',(#8124,#8125,#8126,#8127,#8128,#8129));
#1472=EDGE_LOOP('',(#8130,#8131,#8132,#8133,#8134,#8135));
#1473=EDGE_LOOP('',(#8136,#8137,#8138,#8139,#8140,#8141));
#1474=EDGE_LOOP('',(#8142,#8143,#8144,#8145));
#1475=EDGE_LOOP('',(#8146,#8147,#8148,#8149,#8150));
#1476=EDGE_LOOP('',(#8151,#8152,#8153,#8154,#8155,#8156));
#1477=EDGE_LOOP('',(#8157,#8158,#8159,#8160,#8161,#8162));
#1478=EDGE_LOOP('',(#8163,#8164,#8165,#8166,#8167,#8168));
#1479=EDGE_LOOP('',(#8169,#8170,#8171,#8172,#8173,#8174));
#1480=EDGE_LOOP('',(#8175,#8176,#8177,#8178,#8179,#8180));
#1481=EDGE_LOOP('',(#8181,#8182,#8183,#8184,#8185));
#1482=EDGE_LOOP('',(#8186,#8187,#8188,#8189,#8190,#8191));
#1483=EDGE_LOOP('',(#8192,#8193,#8194,#8195,#8196));
#1484=EDGE_LOOP('',(#8197,#8198,#8199,#8200,#8201));
#1485=EDGE_LOOP('',(#8202,#8203,#8204,#8205,#8206));
#1486=EDGE_LOOP('',(#8207,#8208,#8209,#8210,#8211,#8212));
#1487=EDGE_LOOP('',(#8213,#8214,#8215,#8216,#8217,#8218));
#1488=EDGE_LOOP('',(#8219,#8220,#8221,#8222,#8223,#8224,#8225,#8226,#8227,
#8228,#8229,#8230,#8231,#8232,#8233,#8234,#8235,#8236,#8237,#8238,#8239,
#8240,#8241,#8242,#8243,#8244,#8245,#8246,#8247,#8248,#8249,#8250,#8251,
#8252,#8253,#8254,#8255,#8256,#8257,#8258,#8259,#8260,#8261,#8262,#8263,
#8264,#8265,#8266,#8267,#8268,#8269));
#1489=EDGE_LOOP('',(#8270,#8271,#8272,#8273,#8274,#8275,#8276,#8277,#8278,
#8279,#8280,#8281,#8282,#8283,#8284,#8285,#8286,#8287,#8288,#8289,#8290,
#8291,#8292,#8293,#8294,#8295,#8296,#8297,#8298,#8299,#8300,#8301,#8302,
#8303,#8304,#8305,#8306,#8307,#8308,#8309,#8310,#8311,#8312,#8313,#8314,
#8315,#8316,#8317,#8318));
#1490=EDGE_LOOP('',(#8319,#8320,#8321,#8322,#8323,#8324,#8325,#8326,#8327,
#8328,#8329,#8330,#8331,#8332,#8333,#8334,#8335,#8336,#8337,#8338,#8339,
#8340,#8341,#8342,#8343,#8344,#8345,#8346,#8347,#8348,#8349,#8350,#8351,
#8352,#8353,#8354,#8355,#8356,#8357,#8358,#8359,#8360,#8361,#8362,#8363,
#8364,#8365,#8366,#8367,#8368,#8369,#8370,#8371,#8372,#8373,#8374,#8375,
#8376,#8377,#8378,#8379,#8380,#8381,#8382,#8383,#8384,#8385,#8386,#8387,
#8388,#8389,#8390));
#1491=EDGE_LOOP('',(#8391,#8392,#8393,#8394));
#1492=EDGE_LOOP('',(#8395,#8396,#8397,#8398));
#1493=EDGE_LOOP('',(#8399,#8400,#8401,#8402));
#1494=EDGE_LOOP('',(#8403,#8404,#8405,#8406));
#1495=EDGE_LOOP('',(#8407,#8408,#8409,#8410));
#1496=EDGE_LOOP('',(#8411,#8412,#8413,#8414));
#1497=EDGE_LOOP('',(#8415,#8416,#8417,#8418));
#1498=EDGE_LOOP('',(#8419,#8420,#8421,#8422));
#1499=EDGE_LOOP('',(#8423,#8424,#8425,#8426));
#1500=EDGE_LOOP('',(#8427,#8428,#8429,#8430));
#1501=EDGE_LOOP('',(#8431,#8432,#8433,#8434));
#1502=EDGE_LOOP('',(#8435,#8436,#8437,#8438));
#1503=EDGE_LOOP('',(#8439,#8440,#8441,#8442));
#1504=EDGE_LOOP('',(#8443,#8444,#8445,#8446));
#1505=EDGE_LOOP('',(#8447,#8448,#8449,#8450));
#1506=EDGE_LOOP('',(#8451,#8452,#8453,#8454));
#1507=EDGE_LOOP('',(#8455,#8456,#8457,#8458));
#1508=EDGE_LOOP('',(#8459,#8460,#8461,#8462));
#1509=EDGE_LOOP('',(#8463,#8464,#8465,#8466));
#1510=EDGE_LOOP('',(#8467,#8468,#8469,#8470,#8471,#8472,#8473,#8474));
#1511=EDGE_LOOP('',(#8475,#8476,#8477,#8478,#8479,#8480,#8481,#8482));
#1512=EDGE_LOOP('',(#8483,#8484,#8485,#8486,#8487,#8488,#8489,#8490));
#1513=EDGE_LOOP('',(#8491,#8492,#8493,#8494,#8495,#8496,#8497,#8498));
#1514=EDGE_LOOP('',(#8499,#8500,#8501,#8502,#8503,#8504,#8505,#8506));
#1515=EDGE_LOOP('',(#8507,#8508,#8509,#8510,#8511,#8512,#8513,#8514));
#1516=EDGE_LOOP('',(#8515,#8516,#8517,#8518,#8519,#8520,#8521,#8522));
#1517=EDGE_LOOP('',(#8523,#8524,#8525,#8526,#8527,#8528,#8529,#8530));
#1518=EDGE_LOOP('',(#8531,#8532,#8533,#8534,#8535,#8536,#8537,#8538));
#1519=EDGE_LOOP('',(#8539,#8540,#8541,#8542,#8543,#8544,#8545,#8546));
#1520=EDGE_LOOP('',(#8547,#8548,#8549,#8550,#8551,#8552,#8553,#8554));
#1521=EDGE_LOOP('',(#8555,#8556,#8557,#8558,#8559,#8560,#8561,#8562));
#1522=EDGE_LOOP('',(#8563,#8564,#8565,#8566,#8567,#8568,#8569,#8570));
#1523=EDGE_LOOP('',(#8571,#8572,#8573,#8574,#8575,#8576,#8577,#8578));
#1524=EDGE_LOOP('',(#8579,#8580,#8581,#8582,#8583,#8584,#8585,#8586));
#1525=EDGE_LOOP('',(#8587,#8588,#8589,#8590,#8591,#8592,#8593,#8594));
#1526=EDGE_LOOP('',(#8595,#8596,#8597,#8598,#8599,#8600,#8601,#8602));
#1527=EDGE_LOOP('',(#8603,#8604,#8605,#8606,#8607,#8608,#8609,#8610));
#1528=EDGE_LOOP('',(#8611,#8612,#8613,#8614,#8615,#8616,#8617,#8618));
#1529=EDGE_LOOP('',(#8619,#8620,#8621,#8622,#8623,#8624,#8625,#8626));
#1530=EDGE_LOOP('',(#8627,#8628,#8629,#8630,#8631,#8632,#8633,#8634));
#1531=EDGE_LOOP('',(#8635,#8636,#8637,#8638,#8639,#8640,#8641,#8642));
#1532=EDGE_LOOP('',(#8643,#8644,#8645,#8646,#8647,#8648,#8649,#8650));
#1533=EDGE_LOOP('',(#8651,#8652,#8653,#8654,#8655,#8656,#8657,#8658));
#1534=EDGE_LOOP('',(#8659,#8660,#8661,#8662,#8663,#8664,#8665,#8666));
#1535=EDGE_LOOP('',(#8667,#8668,#8669,#8670,#8671,#8672,#8673,#8674));
#1536=EDGE_LOOP('',(#8675,#8676,#8677,#8678,#8679,#8680,#8681,#8682));
#1537=EDGE_LOOP('',(#8683,#8684,#8685,#8686,#8687,#8688,#8689,#8690));
#1538=EDGE_LOOP('',(#8691,#8692,#8693,#8694,#8695,#8696,#8697,#8698));
#1539=EDGE_LOOP('',(#8699,#8700,#8701,#8702,#8703,#8704,#8705,#8706));
#1540=EDGE_LOOP('',(#8707,#8708,#8709,#8710,#8711,#8712,#8713,#8714));
#1541=EDGE_LOOP('',(#8715,#8716,#8717,#8718,#8719,#8720,#8721,#8722));
#1542=EDGE_LOOP('',(#8723,#8724,#8725,#8726,#8727,#8728,#8729,#8730));
#1543=EDGE_LOOP('',(#8731,#8732,#8733,#8734,#8735,#8736,#8737,#8738));
#1544=EDGE_LOOP('',(#8739,#8740,#8741,#8742,#8743,#8744,#8745,#8746));
#1545=EDGE_LOOP('',(#8747,#8748,#8749,#8750,#8751,#8752,#8753,#8754));
#1546=EDGE_LOOP('',(#8755,#8756,#8757,#8758));
#1547=EDGE_LOOP('',(#8759,#8760,#8761,#8762));
#1548=EDGE_LOOP('',(#8763,#8764,#8765,#8766));
#1549=EDGE_LOOP('',(#8767,#8768,#8769,#8770));
#1550=EDGE_LOOP('',(#8771,#8772,#8773,#8774));
#1551=EDGE_LOOP('',(#8775,#8776,#8777,#8778));
#1552=EDGE_LOOP('',(#8779,#8780,#8781,#8782));
#1553=EDGE_LOOP('',(#8783,#8784,#8785,#8786));
#1554=EDGE_LOOP('',(#8787,#8788,#8789,#8790));
#1555=EDGE_LOOP('',(#8791,#8792,#8793,#8794));
#1556=EDGE_LOOP('',(#8795,#8796,#8797,#8798));
#1557=EDGE_LOOP('',(#8799,#8800,#8801,#8802));
#1558=EDGE_LOOP('',(#8803,#8804,#8805,#8806));
#1559=EDGE_LOOP('',(#8807,#8808,#8809,#8810));
#1560=EDGE_LOOP('',(#8811,#8812,#8813,#8814));
#1561=EDGE_LOOP('',(#8815,#8816,#8817,#8818));
#1562=EDGE_LOOP('',(#8819,#8820,#8821,#8822));
#1563=EDGE_LOOP('',(#8823,#8824,#8825,#8826));
#1564=EDGE_LOOP('',(#8827,#8828,#8829,#8830));
#1565=EDGE_LOOP('',(#8831,#8832,#8833,#8834));
#1566=EDGE_LOOP('',(#8835,#8836,#8837,#8838));
#1567=EDGE_LOOP('',(#8839,#8840,#8841,#8842));
#1568=EDGE_LOOP('',(#8843,#8844,#8845,#8846));
#1569=EDGE_LOOP('',(#8847,#8848,#8849,#8850));
#1570=EDGE_LOOP('',(#8851,#8852,#8853,#8854));
#1571=EDGE_LOOP('',(#8855,#8856,#8857,#8858));
#1572=EDGE_LOOP('',(#8859,#8860,#8861,#8862));
#1573=EDGE_LOOP('',(#8863,#8864,#8865,#8866));
#1574=EDGE_LOOP('',(#8867,#8868,#8869,#8870));
#1575=EDGE_LOOP('',(#8871,#8872,#8873,#8874));
#1576=EDGE_LOOP('',(#8875,#8876,#8877,#8878));
#1577=EDGE_LOOP('',(#8879,#8880,#8881,#8882));
#1578=EDGE_LOOP('',(#8883,#8884,#8885,#8886));
#1579=EDGE_LOOP('',(#8887,#8888,#8889,#8890));
#1580=EDGE_LOOP('',(#8891,#8892,#8893,#8894));
#1581=EDGE_LOOP('',(#8895,#8896,#8897,#8898));
#1582=EDGE_LOOP('',(#8899,#8900,#8901,#8902));
#1583=EDGE_LOOP('',(#8903,#8904,#8905,#8906));
#1584=EDGE_LOOP('',(#8907,#8908,#8909,#8910));
#1585=EDGE_LOOP('',(#8911,#8912,#8913,#8914));
#1586=EDGE_LOOP('',(#8915,#8916,#8917,#8918));
#1587=EDGE_LOOP('',(#8919,#8920,#8921,#8922));
#1588=EDGE_LOOP('',(#8923,#8924,#8925,#8926));
#1589=EDGE_LOOP('',(#8927,#8928,#8929,#8930));
#1590=EDGE_LOOP('',(#8931,#8932,#8933,#8934));
#1591=EDGE_LOOP('',(#8935,#8936,#8937,#8938));
#1592=EDGE_LOOP('',(#8939,#8940,#8941,#8942));
#1593=EDGE_LOOP('',(#8943,#8944,#8945,#8946));
#1594=EDGE_LOOP('',(#8947,#8948,#8949,#8950));
#1595=EDGE_LOOP('',(#8951,#8952,#8953,#8954));
#1596=EDGE_LOOP('',(#8955,#8956,#8957,#8958));
#1597=EDGE_LOOP('',(#8959,#8960,#8961,#8962));
#1598=EDGE_LOOP('',(#8963,#8964,#8965,#8966));
#1599=EDGE_LOOP('',(#8967,#8968,#8969,#8970));
#1600=EDGE_LOOP('',(#8971,#8972,#8973,#8974));
#1601=EDGE_LOOP('',(#8975,#8976,#8977,#8978));
#1602=EDGE_LOOP('',(#8979,#8980,#8981,#8982));
#1603=EDGE_LOOP('',(#8983,#8984,#8985,#8986));
#1604=EDGE_LOOP('',(#8987,#8988,#8989,#8990));
#1605=EDGE_LOOP('',(#8991,#8992,#8993,#8994));
#1606=EDGE_LOOP('',(#8995,#8996,#8997,#8998));
#1607=EDGE_LOOP('',(#8999,#9000,#9001,#9002));
#1608=EDGE_LOOP('',(#9003,#9004,#9005,#9006));
#1609=EDGE_LOOP('',(#9007,#9008,#9009,#9010));
#1610=EDGE_LOOP('',(#9011,#9012,#9013,#9014));
#1611=EDGE_LOOP('',(#9015,#9016,#9017,#9018));
#1612=EDGE_LOOP('',(#9019,#9020,#9021,#9022));
#1613=EDGE_LOOP('',(#9023,#9024,#9025,#9026));
#1614=EDGE_LOOP('',(#9027,#9028,#9029,#9030));
#1615=EDGE_LOOP('',(#9031,#9032,#9033,#9034));
#1616=EDGE_LOOP('',(#9035,#9036,#9037,#9038));
#1617=EDGE_LOOP('',(#9039,#9040,#9041,#9042));
#1618=EDGE_LOOP('',(#9043,#9044,#9045,#9046));
#1619=EDGE_LOOP('',(#9047,#9048,#9049,#9050));
#1620=EDGE_LOOP('',(#9051,#9052,#9053,#9054));
#1621=EDGE_LOOP('',(#9055,#9056,#9057,#9058));
#1622=EDGE_LOOP('',(#9059,#9060,#9061,#9062));
#1623=EDGE_LOOP('',(#9063,#9064,#9065,#9066));
#1624=EDGE_LOOP('',(#9067,#9068,#9069,#9070));
#1625=EDGE_LOOP('',(#9071,#9072,#9073,#9074));
#1626=EDGE_LOOP('',(#9075,#9076,#9077,#9078));
#1627=EDGE_LOOP('',(#9079,#9080,#9081,#9082));
#1628=EDGE_LOOP('',(#9083,#9084,#9085,#9086));
#1629=EDGE_LOOP('',(#9087,#9088,#9089,#9090));
#1630=EDGE_LOOP('',(#9091,#9092,#9093,#9094));
#1631=EDGE_LOOP('',(#9095,#9096,#9097,#9098));
#1632=EDGE_LOOP('',(#9099,#9100,#9101,#9102));
#1633=EDGE_LOOP('',(#9103,#9104,#9105,#9106));
#1634=EDGE_LOOP('',(#9107,#9108,#9109,#9110));
#1635=EDGE_LOOP('',(#9111,#9112,#9113,#9114));
#1636=EDGE_LOOP('',(#9115,#9116,#9117,#9118,#9119,#9120,#9121,#9122,#9123,
#9124));
#1637=EDGE_LOOP('',(#9125,#9126,#9127,#9128,#9129,#9130,#9131,#9132,#9133,
#9134));
#1638=EDGE_LOOP('',(#9135,#9136,#9137,#9138));
#1639=EDGE_LOOP('',(#9139,#9140,#9141,#9142));
#1640=EDGE_LOOP('',(#9143,#9144,#9145,#9146,#9147,#9148,#9149,#9150,#9151,
#9152));
#1641=EDGE_LOOP('',(#9153,#9154,#9155,#9156,#9157,#9158,#9159,#9160,#9161,
#9162));
#1642=EDGE_LOOP('',(#9163,#9164,#9165,#9166));
#1643=EDGE_LOOP('',(#9167,#9168,#9169,#9170));
#1644=EDGE_LOOP('',(#9171,#9172,#9173,#9174,#9175,#9176,#9177,#9178,#9179,
#9180));
#1645=EDGE_LOOP('',(#9181,#9182,#9183,#9184,#9185,#9186,#9187,#9188,#9189,
#9190));
#1646=EDGE_LOOP('',(#9191,#9192,#9193,#9194));
#1647=EDGE_LOOP('',(#9195,#9196,#9197,#9198));
#1648=EDGE_LOOP('',(#9199,#9200,#9201,#9202,#9203,#9204,#9205,#9206,#9207,
#9208));
#1649=EDGE_LOOP('',(#9209,#9210,#9211,#9212,#9213,#9214,#9215,#9216,#9217,
#9218));
#1650=EDGE_LOOP('',(#9219,#9220,#9221,#9222));
#1651=EDGE_LOOP('',(#9223,#9224,#9225,#9226));
#1652=EDGE_LOOP('',(#9227,#9228,#9229,#9230,#9231,#9232,#9233,#9234,#9235,
#9236));
#1653=EDGE_LOOP('',(#9237,#9238,#9239,#9240,#9241,#9242,#9243,#9244,#9245,
#9246));
#1654=EDGE_LOOP('',(#9247,#9248,#9249,#9250));
#1655=EDGE_LOOP('',(#9251,#9252,#9253,#9254));
#1656=EDGE_LOOP('',(#9255,#9256,#9257,#9258,#9259,#9260,#9261,#9262,#9263,
#9264));
#1657=EDGE_LOOP('',(#9265,#9266,#9267,#9268,#9269,#9270,#9271,#9272,#9273,
#9274));
#1658=EDGE_LOOP('',(#9275,#9276,#9277,#9278));
#1659=EDGE_LOOP('',(#9279,#9280,#9281,#9282));
#1660=EDGE_LOOP('',(#9283,#9284,#9285,#9286,#9287,#9288,#9289,#9290,#9291,
#9292));
#1661=EDGE_LOOP('',(#9293,#9294,#9295,#9296,#9297,#9298,#9299,#9300,#9301,
#9302));
#1662=EDGE_LOOP('',(#9303,#9304,#9305,#9306));
#1663=EDGE_LOOP('',(#9307,#9308,#9309,#9310));
#1664=EDGE_LOOP('',(#9311,#9312,#9313,#9314,#9315,#9316,#9317,#9318,#9319,
#9320));
#1665=EDGE_LOOP('',(#9321,#9322,#9323,#9324,#9325,#9326,#9327,#9328,#9329,
#9330));
#1666=EDGE_LOOP('',(#9331,#9332,#9333,#9334));
#1667=EDGE_LOOP('',(#9335,#9336,#9337,#9338));
#1668=EDGE_LOOP('',(#9339,#9340,#9341,#9342,#9343,#9344,#9345,#9346,#9347,
#9348));
#1669=EDGE_LOOP('',(#9349,#9350,#9351,#9352,#9353,#9354,#9355,#9356,#9357,
#9358));
#1670=EDGE_LOOP('',(#9359,#9360,#9361,#9362));
#1671=EDGE_LOOP('',(#9363,#9364,#9365,#9366));
#1672=EDGE_LOOP('',(#9367,#9368,#9369,#9370,#9371,#9372,#9373,#9374,#9375,
#9376));
#1673=EDGE_LOOP('',(#9377,#9378,#9379,#9380,#9381,#9382,#9383,#9384,#9385,
#9386));
#1674=EDGE_LOOP('',(#9387,#9388,#9389,#9390));
#1675=EDGE_LOOP('',(#9391,#9392,#9393,#9394));
#1676=EDGE_LOOP('',(#9395,#9396,#9397,#9398,#9399,#9400,#9401,#9402,#9403,
#9404));
#1677=EDGE_LOOP('',(#9405,#9406,#9407,#9408,#9409,#9410,#9411,#9412,#9413,
#9414));
#1678=EDGE_LOOP('',(#9415,#9416,#9417,#9418));
#1679=EDGE_LOOP('',(#9419,#9420,#9421,#9422));
#1680=EDGE_LOOP('',(#9423,#9424,#9425,#9426,#9427,#9428,#9429,#9430,#9431,
#9432));
#1681=EDGE_LOOP('',(#9433,#9434,#9435,#9436,#9437,#9438,#9439,#9440,#9441,
#9442));
#1682=EDGE_LOOP('',(#9443,#9444,#9445,#9446));
#1683=EDGE_LOOP('',(#9447,#9448,#9449,#9450));
#1684=EDGE_LOOP('',(#9451,#9452,#9453,#9454,#9455,#9456,#9457,#9458,#9459,
#9460));
#1685=EDGE_LOOP('',(#9461,#9462,#9463,#9464,#9465,#9466,#9467,#9468,#9469,
#9470));
#1686=EDGE_LOOP('',(#9471,#9472,#9473,#9474));
#1687=EDGE_LOOP('',(#9475,#9476,#9477,#9478));
#1688=EDGE_LOOP('',(#9479,#9480,#9481,#9482,#9483,#9484,#9485,#9486,#9487,
#9488));
#1689=EDGE_LOOP('',(#9489,#9490,#9491,#9492,#9493,#9494,#9495,#9496,#9497,
#9498));
#1690=EDGE_LOOP('',(#9499,#9500,#9501,#9502));
#1691=EDGE_LOOP('',(#9503,#9504,#9505,#9506));
#1692=EDGE_LOOP('',(#9507,#9508,#9509,#9510,#9511,#9512,#9513,#9514,#9515,
#9516));
#1693=EDGE_LOOP('',(#9517,#9518,#9519,#9520,#9521,#9522,#9523,#9524,#9525,
#9526));
#1694=EDGE_LOOP('',(#9527,#9528,#9529,#9530));
#1695=EDGE_LOOP('',(#9531,#9532,#9533,#9534));
#1696=EDGE_LOOP('',(#9535,#9536,#9537,#9538,#9539,#9540,#9541,#9542,#9543,
#9544));
#1697=EDGE_LOOP('',(#9545,#9546,#9547,#9548,#9549,#9550,#9551,#9552,#9553,
#9554));
#1698=EDGE_LOOP('',(#9555,#9556,#9557,#9558));
#1699=EDGE_LOOP('',(#9559,#9560,#9561,#9562));
#1700=EDGE_LOOP('',(#9563,#9564,#9565,#9566,#9567,#9568,#9569,#9570,#9571,
#9572));
#1701=EDGE_LOOP('',(#9573,#9574,#9575,#9576,#9577,#9578,#9579,#9580,#9581,
#9582));
#1702=EDGE_LOOP('',(#9583,#9584,#9585,#9586));
#1703=EDGE_LOOP('',(#9587,#9588,#9589,#9590));
#1704=EDGE_LOOP('',(#9591,#9592,#9593,#9594,#9595,#9596,#9597,#9598,#9599,
#9600));
#1705=EDGE_LOOP('',(#9601,#9602,#9603,#9604,#9605,#9606,#9607,#9608,#9609,
#9610));
#1706=EDGE_LOOP('',(#9611,#9612,#9613,#9614));
#1707=EDGE_LOOP('',(#9615,#9616,#9617,#9618));
#1708=EDGE_LOOP('',(#9619,#9620,#9621,#9622,#9623,#9624));
#1709=EDGE_LOOP('',(#9625,#9626,#9627,#9628));
#1710=EDGE_LOOP('',(#9629,#9630,#9631,#9632,#9633,#9634));
#1711=EDGE_LOOP('',(#9635,#9636,#9637,#9638));
#1712=EDGE_LOOP('',(#9639,#9640,#9641,#9642));
#1713=EDGE_LOOP('',(#9643,#9644,#9645,#9646,#9647,#9648));
#1714=EDGE_LOOP('',(#9649,#9650,#9651,#9652,#9653,#9654));
#1715=EDGE_LOOP('',(#9655,#9656,#9657,#9658));
#1716=EDGE_LOOP('',(#9659,#9660,#9661,#9662,#9663,#9664));
#1717=EDGE_LOOP('',(#9665,#9666,#9667,#9668,#9669,#9670));
#1718=EDGE_LOOP('',(#9671,#9672,#9673,#9674));
#1719=EDGE_LOOP('',(#9675,#9676,#9677,#9678,#9679,#9680,#9681,#9682,#9683,
#9684,#9685,#9686,#9687,#9688,#9689,#9690,#9691,#9692,#9693,#9694,#9695,
#9696,#9697,#9698,#9699,#9700,#9701,#9702,#9703,#9704,#9705,#9706,#9707,
#9708,#9709,#9710,#9711,#9712,#9713,#9714,#9715,#9716,#9717,#9718,#9719,
#9720,#9721,#9722,#9723,#9724,#9725,#9726,#9727,#9728,#9729,#9730,#9731,
#9732,#9733,#9734,#9735,#9736,#9737,#9738,#9739,#9740,#9741,#9742,#9743,
#9744,#9745,#9746));
#1720=EDGE_LOOP('',(#9747,#9748,#9749,#9750,#9751));
#1721=EDGE_LOOP('',(#9752,#9753,#9754,#9755));
#1722=EDGE_LOOP('',(#9756,#9757,#9758,#9759,#9760,#9761));
#1723=EDGE_LOOP('',(#9762,#9763,#9764,#9765));
#1724=EDGE_LOOP('',(#9766,#9767,#9768,#9769,#9770,#9771));
#1725=EDGE_LOOP('',(#9772,#9773,#9774,#9775));
#1726=EDGE_LOOP('',(#9776,#9777,#9778,#9779));
#1727=EDGE_LOOP('',(#9780,#9781,#9782,#9783,#9784,#9785));
#1728=EDGE_LOOP('',(#9786,#9787,#9788,#9789,#9790,#9791));
#1729=EDGE_LOOP('',(#9792,#9793,#9794,#9795));
#1730=EDGE_LOOP('',(#9796,#9797,#9798,#9799,#9800,#9801));
#1731=EDGE_LOOP('',(#9802,#9803,#9804,#9805,#9806,#9807));
#1732=EDGE_LOOP('',(#9808,#9809,#9810,#9811));
#1733=EDGE_LOOP('',(#9812,#9813,#9814,#9815));
#1734=EDGE_LOOP('',(#9816,#9817,#9818,#9819,#9820,#9821));
#1735=EDGE_LOOP('',(#9822,#9823,#9824,#9825));
#1736=EDGE_LOOP('',(#9826,#9827,#9828,#9829,#9830,#9831));
#1737=EDGE_LOOP('',(#9832,#9833,#9834,#9835));
#1738=EDGE_LOOP('',(#9836,#9837,#9838,#9839));
#1739=EDGE_LOOP('',(#9840,#9841,#9842,#9843,#9844,#9845));
#1740=EDGE_LOOP('',(#9846,#9847,#9848,#9849,#9850,#9851));
#1741=EDGE_LOOP('',(#9852,#9853,#9854,#9855));
#1742=EDGE_LOOP('',(#9856,#9857,#9858,#9859,#9860,#9861));
#1743=EDGE_LOOP('',(#9862,#9863,#9864,#9865,#9866,#9867));
#1744=EDGE_LOOP('',(#9868,#9869,#9870,#9871));
#1745=EDGE_LOOP('',(#9872,#9873,#9874,#9875));
#1746=EDGE_LOOP('',(#9876,#9877,#9878,#9879,#9880,#9881));
#1747=EDGE_LOOP('',(#9882,#9883,#9884,#9885));
#1748=EDGE_LOOP('',(#9886,#9887,#9888,#9889,#9890,#9891));
#1749=EDGE_LOOP('',(#9892,#9893,#9894,#9895));
#1750=EDGE_LOOP('',(#9896,#9897,#9898,#9899));
#1751=EDGE_LOOP('',(#9900,#9901,#9902,#9903,#9904,#9905));
#1752=EDGE_LOOP('',(#9906,#9907,#9908,#9909,#9910,#9911));
#1753=EDGE_LOOP('',(#9912,#9913,#9914,#9915));
#1754=EDGE_LOOP('',(#9916,#9917,#9918,#9919,#9920,#9921));
#1755=EDGE_LOOP('',(#9922,#9923,#9924,#9925,#9926,#9927));
#1756=EDGE_LOOP('',(#9928,#9929,#9930,#9931));
#1757=EDGE_LOOP('',(#9932,#9933,#9934,#9935));
#1758=EDGE_LOOP('',(#9936,#9937,#9938,#9939,#9940,#9941));
#1759=EDGE_LOOP('',(#9942,#9943,#9944,#9945));
#1760=EDGE_LOOP('',(#9946,#9947,#9948,#9949,#9950,#9951));
#1761=EDGE_LOOP('',(#9952,#9953,#9954,#9955));
#1762=EDGE_LOOP('',(#9956,#9957,#9958,#9959));
#1763=EDGE_LOOP('',(#9960,#9961,#9962,#9963,#9964,#9965));
#1764=EDGE_LOOP('',(#9966,#9967,#9968,#9969,#9970,#9971));
#1765=EDGE_LOOP('',(#9972,#9973,#9974,#9975));
#1766=EDGE_LOOP('',(#9976,#9977,#9978,#9979,#9980,#9981));
#1767=EDGE_LOOP('',(#9982,#9983,#9984,#9985,#9986,#9987));
#1768=EDGE_LOOP('',(#9988,#9989,#9990,#9991));
#1769=EDGE_LOOP('',(#9992,#9993,#9994,#9995));
#1770=EDGE_LOOP('',(#9996,#9997,#9998,#9999,#10000,#10001));
#1771=EDGE_LOOP('',(#10002,#10003,#10004,#10005));
#1772=EDGE_LOOP('',(#10006,#10007,#10008,#10009,#10010,#10011));
#1773=EDGE_LOOP('',(#10012,#10013,#10014,#10015));
#1774=EDGE_LOOP('',(#10016,#10017,#10018,#10019));
#1775=EDGE_LOOP('',(#10020,#10021,#10022,#10023,#10024,#10025));
#1776=EDGE_LOOP('',(#10026,#10027,#10028,#10029,#10030,#10031));
#1777=EDGE_LOOP('',(#10032,#10033,#10034,#10035));
#1778=EDGE_LOOP('',(#10036,#10037,#10038,#10039,#10040,#10041));
#1779=EDGE_LOOP('',(#10042,#10043,#10044,#10045,#10046,#10047));
#1780=EDGE_LOOP('',(#10048,#10049,#10050,#10051));
#1781=EDGE_LOOP('',(#10052,#10053,#10054,#10055));
#1782=EDGE_LOOP('',(#10056,#10057,#10058,#10059));
#1783=EDGE_LOOP('',(#10060,#10061,#10062,#10063));
#1784=EDGE_LOOP('',(#10064,#10065,#10066,#10067));
#1785=EDGE_LOOP('',(#10068,#10069,#10070,#10071,#10072));
#1786=EDGE_LOOP('',(#10073,#10074,#10075,#10076,#10077));
#1787=EDGE_LOOP('',(#10078));
#1788=EDGE_LOOP('',(#10079));
#1789=EDGE_LOOP('',(#10080));
#1790=EDGE_LOOP('',(#10081));
#1791=EDGE_LOOP('',(#10082));
#1792=EDGE_LOOP('',(#10083,#10084,#10085,#10086));
#1793=EDGE_LOOP('',(#10087));
#1794=EDGE_LOOP('',(#10088));
#1795=EDGE_LOOP('',(#10089));
#1796=EDGE_LOOP('',(#10090));
#1797=EDGE_LOOP('',(#10091));
#1798=EDGE_LOOP('',(#10092,#10093,#10094,#10095));
#1799=EDGE_LOOP('',(#10096,#10097,#10098,#10099,#10100,#10101));
#1800=EDGE_LOOP('',(#10102,#10103,#10104,#10105,#10106,#10107));
#1801=EDGE_LOOP('',(#10108,#10109,#10110,#10111,#10112,#10113));
#1802=EDGE_LOOP('',(#10114,#10115,#10116,#10117,#10118,#10119));
#1803=EDGE_LOOP('',(#10120,#10121,#10122,#10123,#10124,#10125));
#1804=EDGE_LOOP('',(#10126,#10127,#10128,#10129,#10130,#10131));
#1805=EDGE_LOOP('',(#10132,#10133,#10134,#10135,#10136,#10137));
#1806=EDGE_LOOP('',(#10138,#10139,#10140,#10141,#10142,#10143));
#1807=EDGE_LOOP('',(#10144,#10145,#10146,#10147,#10148,#10149));
#1808=EDGE_LOOP('',(#10150,#10151,#10152,#10153,#10154,#10155));
#1809=EDGE_LOOP('',(#10156,#10157,#10158,#10159,#10160,#10161));
#1810=EDGE_LOOP('',(#10162,#10163,#10164,#10165,#10166,#10167));
#1811=EDGE_LOOP('',(#10168,#10169,#10170,#10171,#10172,#10173));
#1812=EDGE_LOOP('',(#10174,#10175,#10176,#10177,#10178,#10179));
#1813=EDGE_LOOP('',(#10180,#10181,#10182,#10183,#10184,#10185));
#1814=EDGE_LOOP('',(#10186,#10187,#10188,#10189,#10190,#10191));
#1815=EDGE_LOOP('',(#10192,#10193,#10194,#10195,#10196,#10197));
#1816=EDGE_LOOP('',(#10198,#10199,#10200,#10201,#10202,#10203));
#1817=EDGE_LOOP('',(#10204,#10205,#10206,#10207,#10208,#10209));
#1818=EDGE_LOOP('',(#10210,#10211,#10212,#10213,#10214,#10215));
#1819=EDGE_LOOP('',(#10216,#10217,#10218,#10219,#10220,#10221));
#1820=EDGE_LOOP('',(#10222,#10223,#10224,#10225,#10226,#10227));
#1821=EDGE_LOOP('',(#10228,#10229,#10230,#10231,#10232,#10233));
#1822=EDGE_LOOP('',(#10234,#10235,#10236,#10237,#10238,#10239));
#1823=EDGE_LOOP('',(#10240,#10241,#10242,#10243,#10244,#10245));
#1824=EDGE_LOOP('',(#10246,#10247,#10248,#10249,#10250,#10251));
#1825=EDGE_LOOP('',(#10252,#10253,#10254,#10255,#10256,#10257));
#1826=EDGE_LOOP('',(#10258,#10259,#10260,#10261,#10262,#10263));
#1827=EDGE_LOOP('',(#10264,#10265,#10266,#10267,#10268,#10269));
#1828=EDGE_LOOP('',(#10270,#10271,#10272,#10273,#10274,#10275));
#1829=EDGE_LOOP('',(#10276,#10277,#10278,#10279,#10280,#10281));
#1830=EDGE_LOOP('',(#10282,#10283,#10284,#10285,#10286,#10287));
#1831=EDGE_LOOP('',(#10288,#10289,#10290,#10291,#10292,#10293));
#1832=EDGE_LOOP('',(#10294,#10295,#10296,#10297,#10298,#10299));
#1833=EDGE_LOOP('',(#10300,#10301,#10302,#10303,#10304,#10305));
#1834=EDGE_LOOP('',(#10306,#10307,#10308,#10309,#10310,#10311));
#1835=EDGE_LOOP('',(#10312,#10313,#10314,#10315,#10316,#10317));
#1836=EDGE_LOOP('',(#10318,#10319,#10320,#10321,#10322,#10323));
#1837=EDGE_LOOP('',(#10324,#10325,#10326,#10327,#10328,#10329));
#1838=EDGE_LOOP('',(#10330,#10331,#10332,#10333,#10334,#10335));
#1839=EDGE_LOOP('',(#10336,#10337,#10338,#10339,#10340,#10341));
#1840=EDGE_LOOP('',(#10342,#10343,#10344,#10345,#10346,#10347));
#1841=EDGE_LOOP('',(#10348,#10349,#10350,#10351,#10352,#10353));
#1842=EDGE_LOOP('',(#10354,#10355,#10356,#10357,#10358,#10359));
#1843=EDGE_LOOP('',(#10360,#10361,#10362,#10363,#10364,#10365));
#1844=EDGE_LOOP('',(#10366,#10367,#10368,#10369,#10370,#10371));
#1845=EDGE_LOOP('',(#10372,#10373,#10374,#10375,#10376,#10377));
#1846=EDGE_LOOP('',(#10378,#10379,#10380,#10381,#10382,#10383));
#1847=EDGE_LOOP('',(#10384,#10385,#10386,#10387,#10388,#10389));
#1848=EDGE_LOOP('',(#10390,#10391,#10392,#10393,#10394,#10395));
#1849=EDGE_LOOP('',(#10396,#10397,#10398,#10399,#10400,#10401));
#1850=EDGE_LOOP('',(#10402,#10403,#10404,#10405,#10406,#10407));
#1851=EDGE_LOOP('',(#10408,#10409,#10410,#10411,#10412,#10413));
#1852=EDGE_LOOP('',(#10414,#10415,#10416,#10417,#10418,#10419));
#1853=EDGE_LOOP('',(#10420,#10421,#10422,#10423,#10424,#10425));
#1854=EDGE_LOOP('',(#10426,#10427,#10428,#10429,#10430,#10431));
#1855=EDGE_LOOP('',(#10432,#10433,#10434,#10435,#10436,#10437));
#1856=EDGE_LOOP('',(#10438,#10439,#10440,#10441,#10442,#10443));
#1857=EDGE_LOOP('',(#10444,#10445,#10446,#10447,#10448,#10449));
#1858=EDGE_LOOP('',(#10450,#10451,#10452,#10453,#10454,#10455,#10456,#10457,
#10458,#10459,#10460,#10461,#10462,#10463,#10464,#10465,#10466,#10467,#10468,
#10469,#10470,#10471,#10472,#10473,#10474,#10475,#10476,#10477,#10478,#10479,
#10480,#10481,#10482,#10483,#10484,#10485,#10486,#10487,#10488,#10489,#10490,
#10491,#10492,#10493,#10494,#10495,#10496,#10497,#10498,#10499,#10500,#10501,
#10502,#10503,#10504,#10505,#10506,#10507,#10508,#10509,#10510,#10511,#10512,
#10513,#10514,#10515,#10516,#10517,#10518,#10519,#10520,#10521,#10522,#10523,
#10524,#10525,#10526,#10527,#10528,#10529,#10530,#10531,#10532,#10533,#10534,
#10535,#10536,#10537,#10538,#10539,#10540,#10541,#10542,#10543,#10544,#10545,
#10546,#10547,#10548,#10549,#10550,#10551,#10552,#10553));
#1859=EDGE_LOOP('',(#10554,#10555,#10556,#10557,#10558,#10559));
#1860=EDGE_LOOP('',(#10560,#10561,#10562,#10563,#10564,#10565,#10566,#10567,
#10568,#10569,#10570,#10571,#10572,#10573,#10574,#10575,#10576,#10577,#10578,
#10579,#10580,#10581,#10582,#10583,#10584,#10585,#10586,#10587,#10588,#10589,
#10590,#10591,#10592,#10593,#10594,#10595,#10596,#10597,#10598,#10599,#10600,
#10601,#10602,#10603,#10604,#10605,#10606,#10607,#10608,#10609,#10610,#10611,
#10612,#10613,#10614,#10615,#10616,#10617,#10618,#10619,#10620,#10621,#10622,
#10623,#10624,#10625,#10626,#10627,#10628,#10629,#10630,#10631,#10632,#10633,
#10634,#10635,#10636,#10637,#10638,#10639,#10640,#10641,#10642,#10643,#10644,
#10645,#10646,#10647,#10648,#10649,#10650,#10651,#10652,#10653,#10654,#10655,
#10656,#10657,#10658,#10659,#10660,#10661,#10662,#10663,#10664,#10665,#10666,
#10667,#10668,#10669,#10670,#10671,#10672,#10673,#10674,#10675,#10676,#10677,
#10678,#10679,#10680,#10681,#10682,#10683,#10684,#10685,#10686,#10687,#10688,
#10689,#10690,#10691,#10692,#10693,#10694,#10695,#10696,#10697,#10698,#10699,
#10700,#10701,#10702,#10703,#10704,#10705,#10706,#10707,#10708,#10709,#10710,
#10711,#10712,#10713,#10714,#10715,#10716,#10717,#10718,#10719,#10720,#10721,
#10722,#10723));
#1861=EDGE_LOOP('',(#10724,#10725,#10726,#10727,#10728,#10729,#10730,#10731,
#10732,#10733,#10734,#10735,#10736,#10737,#10738,#10739,#10740,#10741,#10742,
#10743,#10744,#10745,#10746,#10747,#10748,#10749,#10750,#10751,#10752,#10753,
#10754,#10755,#10756,#10757,#10758,#10759,#10760,#10761,#10762,#10763,#10764,
#10765,#10766,#10767,#10768,#10769,#10770,#10771,#10772,#10773,#10774,#10775,
#10776,#10777,#10778,#10779,#10780,#10781,#10782,#10783,#10784,#10785,#10786,
#10787,#10788,#10789,#10790,#10791,#10792,#10793,#10794,#10795,#10796,#10797,
#10798,#10799,#10800,#10801,#10802,#10803,#10804,#10805,#10806,#10807,#10808,
#10809,#10810,#10811,#10812,#10813,#10814,#10815,#10816,#10817,#10818,#10819,
#10820,#10821,#10822,#10823,#10824,#10825,#10826,#10827,#10828,#10829,#10830,
#10831,#10832,#10833,#10834,#10835,#10836,#10837,#10838,#10839,#10840,#10841,
#10842,#10843,#10844,#10845,#10846,#10847,#10848,#10849,#10850,#10851,#10852,
#10853,#10854,#10855,#10856,#10857,#10858,#10859,#10860,#10861,#10862,#10863,
#10864,#10865,#10866,#10867,#10868,#10869,#10870,#10871,#10872,#10873,#10874,
#10875,#10876,#10877,#10878,#10879,#10880,#10881,#10882,#10883,#10884,#10885,
#10886,#10887,#10888,#10889,#10890,#10891,#10892,#10893,#10894,#10895,#10896,
#10897,#10898,#10899,#10900,#10901,#10902,#10903,#10904,#10905,#10906,#10907));
#1862=EDGE_LOOP('',(#10908,#10909,#10910,#10911));
#1863=EDGE_LOOP('',(#10912,#10913,#10914,#10915));
#1864=EDGE_LOOP('',(#10916,#10917,#10918,#10919));
#1865=EDGE_LOOP('',(#10920,#10921,#10922,#10923));
#1866=EDGE_LOOP('',(#10924,#10925,#10926,#10927,#10928));
#1867=EDGE_LOOP('',(#10929,#10930,#10931,#10932,#10933,#10934));
#1868=EDGE_LOOP('',(#10935));
#1869=EDGE_LOOP('',(#10936,#10937,#10938,#10939));
#1870=EDGE_LOOP('',(#10940));
#1871=EDGE_LOOP('',(#10941));
#1872=EDGE_LOOP('',(#10942));
#1873=EDGE_LOOP('',(#10943));
#1874=EDGE_LOOP('',(#10944,#10945,#10946,#10947,#10948));
#1875=EDGE_LOOP('',(#10949));
#1876=EDGE_LOOP('',(#10950));
#1877=EDGE_LOOP('',(#10951));
#1878=EDGE_LOOP('',(#10952));
#1879=EDGE_LOOP('',(#10953));
#1880=EDGE_LOOP('',(#10954,#10955,#10956,#10957));
#1881=EDGE_LOOP('',(#10958,#10959,#10960,#10961,#10962,#10963));
#1882=EDGE_LOOP('',(#10964,#10965,#10966,#10967,#10968,#10969,#10970,#10971));
#1883=EDGE_LOOP('',(#10972,#10973,#10974,#10975,#10976,#10977,#10978,#10979));
#1884=EDGE_LOOP('',(#10980,#10981,#10982,#10983,#10984,#10985,#10986,#10987));
#1885=EDGE_LOOP('',(#10988,#10989,#10990,#10991,#10992,#10993,#10994,#10995));
#1886=EDGE_LOOP('',(#10996,#10997,#10998,#10999,#11000,#11001,#11002,#11003,
#11004));
#1887=EDGE_LOOP('',(#11005,#11006,#11007));
#1888=EDGE_LOOP('',(#11008,#11009,#11010,#11011,#11012,#11013));
#1889=EDGE_LOOP('',(#11014));
#1890=EDGE_LOOP('',(#11015,#11016,#11017));
#1891=EDGE_LOOP('',(#11018,#11019,#11020,#11021,#11022,#11023));
#1892=EDGE_LOOP('',(#11024,#11025,#11026,#11027));
#1893=EDGE_LOOP('',(#11028,#11029,#11030,#11031,#11032,#11033,#11034));
#1894=EDGE_LOOP('',(#11035));
#1895=EDGE_LOOP('',(#11036,#11037,#11038,#11039));
#1896=EDGE_LOOP('',(#11040,#11041,#11042));
#1897=EDGE_LOOP('',(#11043,#11044,#11045,#11046,#11047,#11048));
#1898=EDGE_LOOP('',(#11049,#11050,#11051,#11052));
#1899=EDGE_LOOP('',(#11053,#11054,#11055,#11056));
#1900=EDGE_LOOP('',(#11057));
#1901=EDGE_LOOP('',(#11058,#11059,#11060));
#1902=EDGE_LOOP('',(#11061,#11062,#11063,#11064,#11065));
#1903=EDGE_LOOP('',(#11066,#11067,#11068,#11069));
#1904=EDGE_LOOP('',(#11070,#11071,#11072,#11073,#11074));
#1905=EDGE_LOOP('',(#11075,#11076,#11077,#11078,#11079));
#1906=EDGE_LOOP('',(#11080,#11081,#11082,#11083));
#1907=EDGE_LOOP('',(#11084,#11085,#11086,#11087,#11088));
#1908=EDGE_LOOP('',(#11089,#11090,#11091,#11092,#11093));
#1909=EDGE_LOOP('',(#11094,#11095,#11096,#11097));
#1910=EDGE_LOOP('',(#11098,#11099,#11100,#11101,#11102));
#1911=EDGE_LOOP('',(#11103,#11104,#11105,#11106,#11107));
#1912=EDGE_LOOP('',(#11108,#11109,#11110,#11111));
#1913=EDGE_LOOP('',(#11112,#11113,#11114,#11115,#11116));
#1914=EDGE_LOOP('',(#11117,#11118,#11119,#11120,#11121));
#1915=EDGE_LOOP('',(#11122,#11123,#11124,#11125));
#1916=EDGE_LOOP('',(#11126,#11127,#11128));
#1917=EDGE_LOOP('',(#11129,#11130,#11131,#11132,#11133));
#1918=EDGE_LOOP('',(#11134,#11135,#11136,#11137));
#1919=EDGE_LOOP('',(#11138,#11139,#11140,#11141));
#1920=EDGE_LOOP('',(#11142,#11143,#11144,#11145));
#1921=EDGE_LOOP('',(#11146,#11147,#11148,#11149));
#1922=EDGE_LOOP('',(#11150,#11151,#11152,#11153));
#1923=EDGE_LOOP('',(#11154,#11155,#11156,#11157));
#1924=EDGE_LOOP('',(#11158,#11159,#11160,#11161));
#1925=EDGE_LOOP('',(#11162,#11163,#11164,#11165));
#1926=EDGE_LOOP('',(#11166,#11167,#11168,#11169));
#1927=EDGE_LOOP('',(#11170,#11171,#11172,#11173));
#1928=EDGE_LOOP('',(#11174,#11175,#11176,#11177));
#1929=EDGE_LOOP('',(#11178,#11179,#11180,#11181));
#1930=EDGE_LOOP('',(#11182,#11183,#11184,#11185));
#1931=EDGE_LOOP('',(#11186,#11187,#11188,#11189,#11190));
#1932=EDGE_LOOP('',(#11191,#11192,#11193,#11194));
#1933=EDGE_LOOP('',(#11195));
#1934=EDGE_LOOP('',(#11196,#11197,#11198,#11199,#11200));
#1935=EDGE_LOOP('',(#11201,#11202,#11203,#11204,#11205));
#1936=EDGE_LOOP('',(#11206));
#1937=EDGE_LOOP('',(#11207));
#1938=EDGE_LOOP('',(#11208));
#1939=EDGE_LOOP('',(#11209));
#1940=EDGE_LOOP('',(#11210));
#1941=EDGE_LOOP('',(#11211));
#1942=EDGE_LOOP('',(#11212,#11213,#11214,#11215));
#1943=EDGE_LOOP('',(#11216,#11217,#11218,#11219));
#1944=EDGE_LOOP('',(#11220,#11221,#11222,#11223));
#1945=EDGE_LOOP('',(#11224,#11225,#11226,#11227));
#1946=EDGE_LOOP('',(#11228,#11229,#11230,#11231));
#1947=EDGE_LOOP('',(#11232));
#1948=EDGE_LOOP('',(#11233));
#1949=EDGE_LOOP('',(#11234));
#1950=EDGE_LOOP('',(#11235));
#1951=EDGE_LOOP('',(#11236));
#1952=EDGE_LOOP('',(#11237));
#1953=EDGE_LOOP('',(#11238,#11239,#11240,#11241));
#1954=EDGE_LOOP('',(#11242));
#1955=EDGE_LOOP('',(#11243,#11244,#11245,#11246));
#1956=EDGE_LOOP('',(#11247));
#1957=EDGE_LOOP('',(#11248,#11249,#11250,#11251));
#1958=EDGE_LOOP('',(#11252));
#1959=EDGE_LOOP('',(#11253,#11254,#11255,#11256));
#1960=EDGE_LOOP('',(#11257));
#1961=EDGE_LOOP('',(#11258,#11259,#11260,#11261));
#1962=EDGE_LOOP('',(#11262,#11263,#11264,#11265));
#1963=EDGE_LOOP('',(#11266));
#1964=EDGE_LOOP('',(#11267,#11268,#11269,#11270));
#1965=EDGE_LOOP('',(#11271));
#1966=EDGE_LOOP('',(#11272,#11273,#11274,#11275));
#1967=EDGE_LOOP('',(#11276));
#1968=EDGE_LOOP('',(#11277,#11278,#11279,#11280));
#1969=EDGE_LOOP('',(#11281,#11282,#11283,#11284));
#1970=EDGE_LOOP('',(#11285,#11286,#11287,#11288));
#1971=EDGE_LOOP('',(#11289,#11290,#11291,#11292));
#1972=EDGE_LOOP('',(#11293,#11294,#11295,#11296));
#1973=EDGE_LOOP('',(#11297,#11298,#11299,#11300,#11301,#11302,#11303,#11304,
#11305,#11306,#11307,#11308,#11309,#11310,#11311,#11312,#11313,#11314,#11315));
#1974=EDGE_LOOP('',(#11316));
#1975=EDGE_LOOP('',(#11317));
#1976=EDGE_LOOP('',(#11318));
#1977=EDGE_LOOP('',(#11319));
#1978=EDGE_LOOP('',(#11320,#11321,#11322,#11323));
#1979=EDGE_LOOP('',(#11324,#11325,#11326,#11327));
#1980=EDGE_LOOP('',(#11328,#11329,#11330,#11331));
#1981=EDGE_LOOP('',(#11332,#11333,#11334,#11335,#11336,#11337));
#1982=EDGE_LOOP('',(#11338,#11339,#11340,#11341));
#1983=EDGE_LOOP('',(#11342,#11343,#11344,#11345));
#1984=EDGE_LOOP('',(#11346,#11347,#11348,#11349));
#1985=EDGE_LOOP('',(#11350,#11351,#11352,#11353));
#1986=EDGE_LOOP('',(#11354,#11355,#11356,#11357));
#1987=EDGE_LOOP('',(#11358,#11359,#11360,#11361,#11362,#11363,#11364,#11365,
#11366,#11367));
#1988=EDGE_LOOP('',(#11368,#11369,#11370,#11371));
#1989=EDGE_LOOP('',(#11372,#11373,#11374,#11375));
#1990=EDGE_LOOP('',(#11376,#11377,#11378,#11379));
#1991=EDGE_LOOP('',(#11380,#11381,#11382,#11383,#11384));
#1992=EDGE_LOOP('',(#11385,#11386,#11387,#11388));
#1993=EDGE_LOOP('',(#11389,#11390,#11391,#11392));
#1994=EDGE_LOOP('',(#11393,#11394,#11395));
#1995=EDGE_LOOP('',(#11396));
#1996=EDGE_LOOP('',(#11397,#11398,#11399,#11400));
#1997=EDGE_LOOP('',(#11401,#11402,#11403,#11404,#11405,#11406,#11407,#11408,
#11409));
#1998=EDGE_LOOP('',(#11410));
#1999=EDGE_LOOP('',(#11411));
#2000=EDGE_LOOP('',(#11412,#11413,#11414,#11415));
#2001=EDGE_LOOP('',(#11416,#11417,#11418));
#2002=EDGE_LOOP('',(#11419));
#2003=EDGE_LOOP('',(#11420));
#2004=EDGE_LOOP('',(#11421));
#2005=EDGE_LOOP('',(#11422));
#2006=EDGE_LOOP('',(#11423));
#2007=EDGE_LOOP('',(#11424));
#2008=EDGE_LOOP('',(#11425,#11426,#11427,#11428,#11429,#11430,#11431,#11432));
#2009=EDGE_LOOP('',(#11433,#11434));
#2010=EDGE_LOOP('',(#11435));
#2011=EDGE_LOOP('',(#11436));
#2012=EDGE_LOOP('',(#11437));
#2013=EDGE_LOOP('',(#11438));
#2014=EDGE_LOOP('',(#11439,#11440,#11441,#11442,#11443,#11444,#11445,#11446));
#2015=EDGE_LOOP('',(#11447));
#2016=EDGE_LOOP('',(#11448));
#2017=EDGE_LOOP('',(#11449));
#2018=EDGE_LOOP('',(#11450));
#2019=EDGE_LOOP('',(#11451));
#2020=EDGE_LOOP('',(#11452,#11453,#11454,#11455));
#2021=EDGE_LOOP('',(#11456,#11457,#11458,#11459));
#2022=EDGE_LOOP('',(#11460,#11461,#11462,#11463));
#2023=EDGE_LOOP('',(#11464,#11465,#11466,#11467,#11468));
#2024=EDGE_LOOP('',(#11469,#11470,#11471,#11472,#11473));
#2025=EDGE_LOOP('',(#11474));
#2026=EDGE_LOOP('',(#11475));
#2027=EDGE_LOOP('',(#11476));
#2028=EDGE_LOOP('',(#11477));
#2029=EDGE_LOOP('',(#11478));
#2030=EDGE_LOOP('',(#11479,#11480,#11481,#11482));
#2031=EDGE_LOOP('',(#11483));
#2032=EDGE_LOOP('',(#11484));
#2033=EDGE_LOOP('',(#11485));
#2034=EDGE_LOOP('',(#11486));
#2035=EDGE_LOOP('',(#11487));
#2036=EDGE_LOOP('',(#11488,#11489,#11490,#11491));
#2037=EDGE_LOOP('',(#11492,#11493,#11494,#11495,#11496,#11497));
#2038=EDGE_LOOP('',(#11498,#11499,#11500,#11501,#11502));
#2039=EDGE_LOOP('',(#11503,#11504,#11505,#11506));
#2040=EDGE_LOOP('',(#11507,#11508,#11509,#11510));
#2041=EDGE_LOOP('',(#11511,#11512,#11513,#11514));
#2042=EDGE_LOOP('',(#11515,#11516,#11517,#11518));
#2043=EDGE_LOOP('',(#11519,#11520,#11521,#11522));
#2044=EDGE_LOOP('',(#11523,#11524,#11525,#11526));
#2045=EDGE_LOOP('',(#11527,#11528,#11529,#11530,#11531));
#2046=EDGE_LOOP('',(#11532));
#2047=EDGE_LOOP('',(#11533));
#2048=EDGE_LOOP('',(#11534));
#2049=EDGE_LOOP('',(#11535));
#2050=EDGE_LOOP('',(#11536,#11537));
#2051=EDGE_LOOP('',(#11538,#11539,#11540,#11541));
#2052=EDGE_LOOP('',(#11542,#11543,#11544,#11545));
#2053=EDGE_LOOP('',(#11546,#11547,#11548,#11549,#11550));
#2054=EDGE_LOOP('',(#11551,#11552,#11553,#11554,#11555));
#2055=EDGE_LOOP('',(#11556));
#2056=EDGE_LOOP('',(#11557));
#2057=EDGE_LOOP('',(#11558));
#2058=EDGE_LOOP('',(#11559));
#2059=EDGE_LOOP('',(#11560,#11561,#11562,#11563));
#2060=EDGE_LOOP('',(#11564,#11565,#11566,#11567));
#2061=EDGE_LOOP('',(#11568,#11569,#11570,#11571));
#2062=EDGE_LOOP('',(#11572,#11573,#11574,#11575));
#2063=EDGE_LOOP('',(#11576));
#2064=EDGE_LOOP('',(#11577));
#2065=EDGE_LOOP('',(#11578));
#2066=EDGE_LOOP('',(#11579));
#2067=EDGE_LOOP('',(#11580,#11581,#11582,#11583));
#2068=EDGE_LOOP('',(#11584,#11585,#11586,#11587));
#2069=EDGE_LOOP('',(#11588,#11589,#11590,#11591,#11592));
#2070=EDGE_LOOP('',(#11593,#11594,#11595,#11596,#11597));
#2071=EDGE_LOOP('',(#11598,#11599,#11600,#11601));
#2072=EDGE_LOOP('',(#11602,#11603,#11604,#11605));
#2073=EDGE_LOOP('',(#11606,#11607,#11608,#11609,#11610));
#2074=EDGE_LOOP('',(#11611,#11612,#11613,#11614,#11615));
#2075=EDGE_LOOP('',(#11616,#11617,#11618,#11619));
#2076=EDGE_LOOP('',(#11620,#11621,#11622,#11623));
#2077=EDGE_LOOP('',(#11624));
#2078=EDGE_LOOP('',(#11625));
#2079=EDGE_LOOP('',(#11626));
#2080=EDGE_LOOP('',(#11627));
#2081=EDGE_LOOP('',(#11628,#11629));
#2082=EDGE_LOOP('',(#11630,#11631));
#2083=EDGE_LOOP('',(#11632,#11633));
#2084=EDGE_LOOP('',(#11634,#11635));
#2085=EDGE_LOOP('',(#11636,#11637));
#2086=EDGE_LOOP('',(#11638,#11639));
#2087=EDGE_LOOP('',(#11640,#11641));
#2088=EDGE_LOOP('',(#11642,#11643));
#2089=EDGE_LOOP('',(#11644,#11645,#11646,#11647));
#2090=EDGE_LOOP('',(#11648,#11649,#11650,#11651));
#2091=EDGE_LOOP('',(#11652,#11653,#11654,#11655));
#2092=EDGE_LOOP('',(#11656,#11657,#11658,#11659,#11660));
#2093=EDGE_LOOP('',(#11661,#11662,#11663,#11664,#11665,#11666));
#2094=EDGE_LOOP('',(#11667,#11668,#11669,#11670,#11671));
#2095=EDGE_LOOP('',(#11672));
#2096=EDGE_LOOP('',(#11673));
#2097=EDGE_LOOP('',(#11674,#11675,#11676,#11677,#11678));
#2098=EDGE_LOOP('',(#11679,#11680,#11681,#11682));
#2099=EDGE_LOOP('',(#11683,#11684,#11685,#11686));
#2100=EDGE_LOOP('',(#11687,#11688,#11689,#11690,#11691));
#2101=EDGE_LOOP('',(#11692));
#2102=EDGE_LOOP('',(#11693));
#2103=EDGE_LOOP('',(#11694));
#2104=EDGE_LOOP('',(#11695));
#2105=EDGE_LOOP('',(#11696,#11697,#11698,#11699,#11700,#11701));
#2106=EDGE_LOOP('',(#11702,#11703,#11704,#11705,#11706,#11707));
#2107=EDGE_LOOP('',(#11708,#11709,#11710,#11711,#11712));
#2108=EDGE_LOOP('',(#11713,#11714,#11715,#11716,#11717));
#2109=EDGE_LOOP('',(#11718,#11719,#11720,#11721,#11722,#11723));
#2110=EDGE_LOOP('',(#11724,#11725,#11726,#11727,#11728,#11729,#11730,#11731,
#11732,#11733,#11734,#11735,#11736,#11737));
#2111=EDGE_LOOP('',(#11738,#11739,#11740,#11741));
#2112=EDGE_LOOP('',(#11742,#11743,#11744,#11745));
#2113=EDGE_LOOP('',(#11746,#11747,#11748,#11749));
#2114=EDGE_LOOP('',(#11750,#11751,#11752,#11753));
#2115=EDGE_LOOP('',(#11754,#11755,#11756,#11757));
#2116=EDGE_LOOP('',(#11758,#11759,#11760,#11761));
#2117=EDGE_LOOP('',(#11762,#11763,#11764,#11765));
#2118=EDGE_LOOP('',(#11766,#11767,#11768,#11769));
#2119=EDGE_LOOP('',(#11770,#11771,#11772,#11773));
#2120=EDGE_LOOP('',(#11774,#11775,#11776,#11777));
#2121=EDGE_LOOP('',(#11778,#11779,#11780,#11781,#11782,#11783,#11784,#11785,
#11786,#11787,#11788,#11789,#11790,#11791));
#2122=EDGE_LOOP('',(#11792,#11793,#11794,#11795));
#2123=EDGE_LOOP('',(#11796,#11797,#11798,#11799));
#2124=EDGE_LOOP('',(#11800,#11801,#11802,#11803));
#2125=EDGE_LOOP('',(#11804,#11805,#11806,#11807));
#2126=EDGE_LOOP('',(#11808,#11809,#11810,#11811));
#2127=EDGE_LOOP('',(#11812,#11813,#11814,#11815));
#2128=EDGE_LOOP('',(#11816,#11817,#11818,#11819));
#2129=EDGE_LOOP('',(#11820,#11821,#11822,#11823));
#2130=EDGE_LOOP('',(#11824,#11825,#11826,#11827));
#2131=EDGE_LOOP('',(#11828,#11829,#11830,#11831));
#2132=EDGE_LOOP('',(#11832,#11833,#11834,#11835));
#2133=EDGE_LOOP('',(#11836,#11837,#11838,#11839));
#2134=EDGE_LOOP('',(#11840,#11841,#11842,#11843));
#2135=EDGE_LOOP('',(#11844,#11845,#11846,#11847));
#2136=EDGE_LOOP('',(#11848,#11849,#11850,#11851));
#2137=EDGE_LOOP('',(#11852,#11853,#11854,#11855));
#2138=EDGE_LOOP('',(#11856,#11857,#11858,#11859));
#2139=EDGE_LOOP('',(#11860,#11861,#11862,#11863));
#2140=EDGE_LOOP('',(#11864,#11865,#11866,#11867));
#2141=EDGE_LOOP('',(#11868,#11869,#11870,#11871));
#2142=EDGE_LOOP('',(#11872,#11873,#11874,#11875));
#2143=EDGE_LOOP('',(#11876,#11877,#11878,#11879));
#2144=EDGE_LOOP('',(#11880,#11881,#11882,#11883));
#2145=EDGE_LOOP('',(#11884,#11885,#11886,#11887));
#2146=EDGE_LOOP('',(#11888,#11889,#11890,#11891));
#2147=EDGE_LOOP('',(#11892,#11893,#11894,#11895));
#2148=EDGE_LOOP('',(#11896,#11897,#11898,#11899));
#2149=EDGE_LOOP('',(#11900,#11901,#11902,#11903));
#2150=EDGE_LOOP('',(#11904,#11905,#11906,#11907));
#2151=EDGE_LOOP('',(#11908,#11909,#11910,#11911));
#2152=EDGE_LOOP('',(#11912,#11913,#11914,#11915));
#2153=EDGE_LOOP('',(#11916,#11917,#11918,#11919));
#2154=EDGE_LOOP('',(#11920,#11921,#11922,#11923));
#2155=EDGE_LOOP('',(#11924,#11925,#11926,#11927));
#2156=EDGE_LOOP('',(#11928,#11929,#11930,#11931));
#2157=EDGE_LOOP('',(#11932,#11933,#11934,#11935));
#2158=EDGE_LOOP('',(#11936,#11937,#11938,#11939));
#2159=EDGE_LOOP('',(#11940,#11941,#11942,#11943));
#2160=EDGE_LOOP('',(#11944,#11945,#11946,#11947));
#2161=EDGE_LOOP('',(#11948,#11949,#11950,#11951));
#2162=EDGE_LOOP('',(#11952,#11953,#11954,#11955));
#2163=EDGE_LOOP('',(#11956,#11957,#11958,#11959));
#2164=EDGE_LOOP('',(#11960,#11961,#11962,#11963));
#2165=EDGE_LOOP('',(#11964,#11965,#11966,#11967));
#2166=EDGE_LOOP('',(#11968,#11969,#11970,#11971));
#2167=EDGE_LOOP('',(#11972,#11973,#11974,#11975));
#2168=EDGE_LOOP('',(#11976,#11977,#11978,#11979));
#2169=EDGE_LOOP('',(#11980,#11981,#11982,#11983));
#2170=EDGE_LOOP('',(#11984,#11985,#11986,#11987,#11988,#11989));
#2171=EDGE_LOOP('',(#11990,#11991,#11992,#11993,#11994,#11995));
#2172=EDGE_LOOP('',(#11996,#11997,#11998,#11999));
#2173=EDGE_LOOP('',(#12000,#12001,#12002,#12003));
#2174=EDGE_LOOP('',(#12004,#12005,#12006,#12007));
#2175=EDGE_LOOP('',(#12008,#12009,#12010,#12011));
#2176=EDGE_LOOP('',(#12012,#12013,#12014,#12015,#12016));
#2177=EDGE_LOOP('',(#12017,#12018,#12019,#12020));
#2178=EDGE_LOOP('',(#12021,#12022,#12023,#12024,#12025));
#2179=EDGE_LOOP('',(#12026,#12027,#12028,#12029,#12030,#12031));
#2180=EDGE_LOOP('',(#12032,#12033,#12034,#12035,#12036));
#2181=EDGE_LOOP('',(#12037,#12038,#12039,#12040));
#2182=EDGE_LOOP('',(#12041,#12042,#12043,#12044,#12045));
#2183=EDGE_LOOP('',(#12046,#12047,#12048,#12049));
#2184=EDGE_LOOP('',(#12050));
#2185=EDGE_LOOP('',(#12051));
#2186=EDGE_LOOP('',(#12052));
#2187=EDGE_LOOP('',(#12053));
#2188=EDGE_LOOP('',(#12054,#12055,#12056,#12057));
#2189=EDGE_LOOP('',(#12058));
#2190=EDGE_LOOP('',(#12059));
#2191=EDGE_LOOP('',(#12060,#12061,#12062,#12063));
#2192=EDGE_LOOP('',(#12064));
#2193=EDGE_LOOP('',(#12065));
#2194=EDGE_LOOP('',(#12066,#12067,#12068,#12069));
#2195=EDGE_LOOP('',(#12070));
#2196=EDGE_LOOP('',(#12071));
#2197=EDGE_LOOP('',(#12072,#12073,#12074,#12075));
#2198=EDGE_LOOP('',(#12076));
#2199=EDGE_LOOP('',(#12077));
#2200=EDGE_LOOP('',(#12078,#12079,#12080,#12081));
#2201=EDGE_LOOP('',(#12082));
#2202=EDGE_LOOP('',(#12083));
#2203=EDGE_LOOP('',(#12084,#12085,#12086,#12087));
#2204=EDGE_LOOP('',(#12088));
#2205=EDGE_LOOP('',(#12089));
#2206=EDGE_LOOP('',(#12090,#12091,#12092,#12093));
#2207=EDGE_LOOP('',(#12094));
#2208=EDGE_LOOP('',(#12095));
#2209=EDGE_LOOP('',(#12096,#12097,#12098,#12099));
#2210=EDGE_LOOP('',(#12100));
#2211=EDGE_LOOP('',(#12101));
#2212=EDGE_LOOP('',(#12102,#12103,#12104,#12105));
#2213=EDGE_LOOP('',(#12106));
#2214=EDGE_LOOP('',(#12107));
#2215=EDGE_LOOP('',(#12108,#12109,#12110,#12111));
#2216=EDGE_LOOP('',(#12112));
#2217=EDGE_LOOP('',(#12113));
#2218=EDGE_LOOP('',(#12114,#12115,#12116,#12117));
#2219=EDGE_LOOP('',(#12118));
#2220=EDGE_LOOP('',(#12119));
#2221=CIRCLE('',#13130,8.12525);
#2222=CIRCLE('',#13142,8.12525);
#2223=CIRCLE('',#13144,7.01125);
#2224=CIRCLE('',#13156,7.01125);
#2225=CIRCLE('',#13160,15.9979895488606);
#2226=CIRCLE('',#13161,15.5);
#2227=CIRCLE('',#13162,15.9979895488606);
#2228=CIRCLE('',#13163,15.5);
#2229=CIRCLE('',#13164,15.9979895488606);
#2230=CIRCLE('',#13165,15.5);
#2231=CIRCLE('',#13166,15.9979895488606);
#2232=CIRCLE('',#13167,15.5);
#2233=CIRCLE('',#13168,15.9979895488606);
#2234=CIRCLE('',#13169,15.5);
#2235=CIRCLE('',#13170,15.9979895488606);
#2236=CIRCLE('',#13171,15.5);
#2237=CIRCLE('',#13172,15.9979895488606);
#2238=CIRCLE('',#13173,15.5);
#2239=CIRCLE('',#13174,15.9979895488606);
#2240=CIRCLE('',#13175,15.5);
#2241=CIRCLE('',#13176,15.9979895488606);
#2242=CIRCLE('',#13177,15.5);
#2243=CIRCLE('',#13178,15.9979895488606);
#2244=CIRCLE('',#13179,15.5);
#2245=CIRCLE('',#13180,15.9979895488606);
#2246=CIRCLE('',#13181,15.5);
#2247=CIRCLE('',#13182,15.9979895488606);
#2248=CIRCLE('',#13183,15.5);
#2249=CIRCLE('',#13184,15.9979895488606);
#2250=CIRCLE('',#13185,15.5);
#2251=CIRCLE('',#13186,15.9979895488606);
#2252=CIRCLE('',#13187,15.5);
#2253=CIRCLE('',#13188,15.9979895488606);
#2254=CIRCLE('',#13189,15.5);
#2255=CIRCLE('',#13190,15.9979895488606);
#2256=CIRCLE('',#13191,15.5);
#2257=CIRCLE('',#13192,15.9979895488606);
#2258=CIRCLE('',#13193,15.5);
#2259=CIRCLE('',#13194,15.9979895488606);
#2260=CIRCLE('',#13195,15.5);
#2261=CIRCLE('',#13197,19.9979895488606);
#2262=CIRCLE('',#13198,20.0030144756463);
#2263=CIRCLE('',#13200,19.9979895488606);
#2264=CIRCLE('',#13201,20.0030144756504);
#2265=CIRCLE('',#13203,19.9979895488606);
#2266=CIRCLE('',#13204,20.0030144756628);
#2267=CIRCLE('',#13206,19.9979895488606);
#2268=CIRCLE('',#13207,20.0030144756547);
#2269=CIRCLE('',#13209,19.9979895488606);
#2270=CIRCLE('',#13210,20.0030144756757);
#2271=CIRCLE('',#13212,19.9979895488606);
#2272=CIRCLE('',#13213,20.003014475647);
#2273=CIRCLE('',#13215,19.9979895488606);
#2274=CIRCLE('',#13216,20.0030144756693);
#2275=CIRCLE('',#13218,19.9979895488606);
#2276=CIRCLE('',#13219,20.0030144756498);
#2277=CIRCLE('',#13221,19.9979895488606);
#2278=CIRCLE('',#13222,20.0030144756644);
#2279=CIRCLE('',#13224,19.9979895488606);
#2280=CIRCLE('',#13225,20.0030144756482);
#2281=CIRCLE('',#13227,19.9979895488606);
#2282=CIRCLE('',#13228,20.0030144756504);
#2283=CIRCLE('',#13230,19.9979895488606);
#2284=CIRCLE('',#13231,20.0030144756643);
#2285=CIRCLE('',#13233,19.9979895488606);
#2286=CIRCLE('',#13234,20.0030144756551);
#2287=CIRCLE('',#13236,19.9979895488606);
#2288=CIRCLE('',#13237,20.003014475638);
#2289=CIRCLE('',#13239,19.9979895488606);
#2290=CIRCLE('',#13240,20.0030144756176);
#2291=CIRCLE('',#13242,19.9979895488606);
#2292=CIRCLE('',#13243,20.0030144756693);
#2293=CIRCLE('',#13245,19.9979895488606);
#2294=CIRCLE('',#13246,20.0030144756499);
#2295=CIRCLE('',#13248,19.9979895488606);
#2296=CIRCLE('',#13249,20.0030144756645);
#2297=CIRCLE('',#13251,153.58770900085);
#2298=CIRCLE('',#13252,153.587709001305);
#2299=CIRCLE('',#13254,153.587709000006);
#2300=CIRCLE('',#13255,153.587709000986);
#2301=CIRCLE('',#13257,153.587709000895);
#2302=CIRCLE('',#13258,153.587709000364);
#2303=CIRCLE('',#13260,153.587709000872);
#2304=CIRCLE('',#13261,153.587709001053);
#2305=CIRCLE('',#13263,153.587709000643);
#2306=CIRCLE('',#13264,153.587709000849);
#2307=CIRCLE('',#13266,153.587709004083);
#2308=CIRCLE('',#13267,153.587709001836);
#2309=CIRCLE('',#13269,153.5877090017);
#2310=CIRCLE('',#13270,153.587709001977);
#2311=CIRCLE('',#13272,153.587709000674);
#2312=CIRCLE('',#13273,153.587709000286);
#2313=CIRCLE('',#13275,153.58770900064);
#2314=CIRCLE('',#13276,153.587709001091);
#2315=CIRCLE('',#13278,153.587709000099);
#2316=CIRCLE('',#13279,153.587709001243);
#2317=CIRCLE('',#13281,153.587709001448);
#2318=CIRCLE('',#13282,153.587709000446);
#2319=CIRCLE('',#13284,153.587709000445);
#2320=CIRCLE('',#13285,153.587709000972);
#2321=CIRCLE('',#13287,153.587709000937);
#2322=CIRCLE('',#13288,153.587709001348);
#2323=CIRCLE('',#13290,153.587709001259);
#2324=CIRCLE('',#13291,153.587709000715);
#2325=CIRCLE('',#13293,153.587709001696);
#2326=CIRCLE('',#13294,153.587709001411);
#2327=CIRCLE('',#13296,153.587709001257);
#2328=CIRCLE('',#13297,153.587709000945);
#2329=CIRCLE('',#13299,153.587709001131);
#2330=CIRCLE('',#13300,153.58770900096);
#2331=CIRCLE('',#13302,153.587709000845);
#2332=CIRCLE('',#13303,153.587709000983);
#2333=CIRCLE('',#13305,153.587709001349);
#2334=CIRCLE('',#13306,15.9979895488606);
#2335=CIRCLE('',#13307,153.587709000931);
#2336=CIRCLE('',#13308,19.9979895488606);
#2337=CIRCLE('',#13310,153.587709001089);
#2338=CIRCLE('',#13311,15.9979895488606);
#2339=CIRCLE('',#13312,153.587709001593);
#2340=CIRCLE('',#13313,19.9979895488606);
#2341=CIRCLE('',#13315,153.587709000602);
#2342=CIRCLE('',#13316,15.9979895488606);
#2343=CIRCLE('',#13317,153.587709000574);
#2344=CIRCLE('',#13318,19.9979895488606);
#2345=CIRCLE('',#13320,153.587709001501);
#2346=CIRCLE('',#13321,15.9979895488606);
#2347=CIRCLE('',#13322,153.587709000733);
#2348=CIRCLE('',#13323,19.9979895488606);
#2349=CIRCLE('',#13325,153.587709001334);
#2350=CIRCLE('',#13326,15.9979895488606);
#2351=CIRCLE('',#13327,153.587709000931);
#2352=CIRCLE('',#13328,19.9979895488606);
#2353=CIRCLE('',#13330,153.587709000819);
#2354=CIRCLE('',#13331,15.9979895488606);
#2355=CIRCLE('',#13332,153.587709001092);
#2356=CIRCLE('',#13333,19.9979895488606);
#2357=CIRCLE('',#13335,153.587709000441);
#2358=CIRCLE('',#13336,15.9979895488606);
#2359=CIRCLE('',#13337,153.587709000835);
#2360=CIRCLE('',#13338,19.9979895488606);
#2361=CIRCLE('',#13340,153.587708999976);
#2362=CIRCLE('',#13341,15.9979895488606);
#2363=CIRCLE('',#13342,153.587709002011);
#2364=CIRCLE('',#13343,19.9979895488606);
#2365=CIRCLE('',#13345,153.587709000862);
#2366=CIRCLE('',#13346,15.9979895488606);
#2367=CIRCLE('',#13347,153.587709000429);
#2368=CIRCLE('',#13348,19.9979895488606);
#2369=CIRCLE('',#13350,153.587709000768);
#2370=CIRCLE('',#13351,15.9979895488606);
#2371=CIRCLE('',#13352,153.587709000924);
#2372=CIRCLE('',#13353,19.9979895488606);
#2373=CIRCLE('',#13355,153.587709001594);
#2374=CIRCLE('',#13356,15.9979895488606);
#2375=CIRCLE('',#13357,153.587709001193);
#2376=CIRCLE('',#13358,19.9979895488606);
#2377=CIRCLE('',#13360,153.587708999931);
#2378=CIRCLE('',#13361,15.9979895488606);
#2379=CIRCLE('',#13362,153.587709001467);
#2380=CIRCLE('',#13363,19.9979895488606);
#2381=CIRCLE('',#13365,153.587709001247);
#2382=CIRCLE('',#13366,15.9979895488606);
#2383=CIRCLE('',#13367,153.587709000706);
#2384=CIRCLE('',#13368,19.9979895488606);
#2385=CIRCLE('',#13370,153.587709001118);
#2386=CIRCLE('',#13371,15.9979895488606);
#2387=CIRCLE('',#13372,153.587709000915);
#2388=CIRCLE('',#13373,19.9979895488606);
#2389=CIRCLE('',#13375,153.587709000848);
#2390=CIRCLE('',#13376,15.9979895488606);
#2391=CIRCLE('',#13377,153.587709000911);
#2392=CIRCLE('',#13378,19.9979895488606);
#2393=CIRCLE('',#13380,153.587709000116);
#2394=CIRCLE('',#13381,15.9979895488606);
#2395=CIRCLE('',#13382,153.587709000787);
#2396=CIRCLE('',#13383,19.9979895488606);
#2397=CIRCLE('',#13385,153.587709000229);
#2398=CIRCLE('',#13386,15.9979895488606);
#2399=CIRCLE('',#13387,153.587709001888);
#2400=CIRCLE('',#13388,19.9979895488606);
#2401=CIRCLE('',#13390,153.587709000873);
#2402=CIRCLE('',#13391,15.9979895488606);
#2403=CIRCLE('',#13392,153.587709000422);
#2404=CIRCLE('',#13393,19.9979895488606);
#2405=CIRCLE('',#13395,20.0030144756182);
#2406=CIRCLE('',#13397,20.0030144756451);
#2407=CIRCLE('',#13399,20.0030144756147);
#2408=CIRCLE('',#13401,20.0030144756611);
#2409=CIRCLE('',#13403,20.0030144756232);
#2410=CIRCLE('',#13405,20.0030144756284);
#2411=CIRCLE('',#13407,20.0030144756652);
#2412=CIRCLE('',#13409,20.0030144756486);
#2413=CIRCLE('',#13411,20.0030144756281);
#2414=CIRCLE('',#13413,20.0030144756182);
#2415=CIRCLE('',#13415,20.0030144756466);
#2416=CIRCLE('',#13417,20.003014475679);
#2417=CIRCLE('',#13419,20.0030144756625);
#2418=CIRCLE('',#13421,20.0030144756237);
#2419=CIRCLE('',#13423,20.003014475629);
#2420=CIRCLE('',#13425,20.0030144756642);
#2421=CIRCLE('',#13427,20.0030144756486);
#2422=CIRCLE('',#13429,20.0030144756277);
#2423=CIRCLE('',#13432,20.0030144756662);
#2424=CIRCLE('',#13433,19.9140934904867);
#2425=CIRCLE('',#13436,20.0030144756255);
#2426=CIRCLE('',#13438,19.9140934904867);
#2427=CIRCLE('',#13441,20.0030144756289);
#2428=CIRCLE('',#13443,19.9140934904867);
#2429=CIRCLE('',#13446,20.0030144756142);
#2430=CIRCLE('',#13447,19.9140934904867);
#2431=CIRCLE('',#13450,20.0030144756439);
#2432=CIRCLE('',#13452,19.9140934904867);
#2433=CIRCLE('',#13455,20.0030144756117);
#2434=CIRCLE('',#13457,19.9140934904867);
#2435=CIRCLE('',#13460,20.0030144756195);
#2436=CIRCLE('',#13462,19.9140934904867);
#2437=CIRCLE('',#13465,20.003014475617);
#2438=CIRCLE('',#13466,19.9140934904867);
#2439=CIRCLE('',#13469,20.0030144756512);
#2440=CIRCLE('',#13471,19.9140934904867);
#2441=CIRCLE('',#13474,20.0030144756233);
#2442=CIRCLE('',#13476,19.9140934904867);
#2443=CIRCLE('',#13479,20.0030144756255);
#2444=CIRCLE('',#13481,19.9140934904867);
#2445=CIRCLE('',#13484,20.0030144756289);
#2446=CIRCLE('',#13485,19.9140934904867);
#2447=CIRCLE('',#13488,20.0030144756141);
#2448=CIRCLE('',#13490,19.9140934904867);
#2449=CIRCLE('',#13493,20.0030144756447);
#2450=CIRCLE('',#13495,19.9140934904867);
#2451=CIRCLE('',#13498,20.003014475657);
#2452=CIRCLE('',#13500,19.9140934904867);
#2453=CIRCLE('',#13503,20.0030144756171);
#2454=CIRCLE('',#13505,19.9140934904867);
#2455=CIRCLE('',#13508,20.0030144756463);
#2456=CIRCLE('',#13509,19.9140934904867);
#2457=CIRCLE('',#13512,20.003014475691);
#2458=CIRCLE('',#13513,19.9140934904867);
#2459=CIRCLE('',#13515,19.9140934904867);
#2460=CIRCLE('',#13517,20.0030144756501);
#2461=CIRCLE('',#13519,19.9140934904867);
#2462=CIRCLE('',#13521,20.0030144756426);
#2463=CIRCLE('',#13523,19.9140934904867);
#2464=CIRCLE('',#13525,20.0030144756575);
#2465=CIRCLE('',#13527,19.9140934904867);
#2466=CIRCLE('',#13529,20.0030144756947);
#2467=CIRCLE('',#13531,19.9140934904867);
#2468=CIRCLE('',#13533,20.0030144756567);
#2469=CIRCLE('',#13535,19.9140934904867);
#2470=CIRCLE('',#13537,20.0030144756689);
#2471=CIRCLE('',#13539,19.9140934904867);
#2472=CIRCLE('',#13541,20.0030144756252);
#2473=CIRCLE('',#13543,19.9140934904867);
#2474=CIRCLE('',#13545,20.0030144756634);
#2475=CIRCLE('',#13547,19.9140934904867);
#2476=CIRCLE('',#13549,20.0030144756389);
#2477=CIRCLE('',#13551,19.9140934904867);
#2478=CIRCLE('',#13553,20.0030144756501);
#2479=CIRCLE('',#13555,19.9140934904867);
#2480=CIRCLE('',#13557,20.003014475641);
#2481=CIRCLE('',#13559,19.9140934904867);
#2482=CIRCLE('',#13561,20.0030144756575);
#2483=CIRCLE('',#13563,19.9140934904867);
#2484=CIRCLE('',#13565,20.0030144756939);
#2485=CIRCLE('',#13567,19.9140934904867);
#2486=CIRCLE('',#13569,20.0030144756567);
#2487=CIRCLE('',#13571,19.9140934904867);
#2488=CIRCLE('',#13573,20.00301447567);
#2489=CIRCLE('',#13575,19.9140934904867);
#2490=CIRCLE('',#13577,20.0030144756496);
#2491=CIRCLE('',#13579,19.9140934904867);
#2492=CIRCLE('',#13581,20.0030144756634);
#2493=CIRCLE('',#13583,19.9140934904867);
#2494=CIRCLE('',#13585,20.0030144756377);
#2495=CIRCLE('',#13604,1187.25159941003);
#2496=CIRCLE('',#13605,1187.25159940698);
#2497=CIRCLE('',#13606,1187.25159941794);
#2498=CIRCLE('',#13607,1187.25159940193);
#2499=CIRCLE('',#13608,1187.25159944622);
#2500=CIRCLE('',#13609,1187.2515994077);
#2501=CIRCLE('',#13610,1187.25159945662);
#2502=CIRCLE('',#13611,1187.2515994434);
#2503=CIRCLE('',#13612,1187.25159941087);
#2504=CIRCLE('',#13613,1187.2515994045);
#2505=CIRCLE('',#13614,1187.25365514628);
#2506=CIRCLE('',#13615,1187.25431298417);
#2507=CIRCLE('',#13616,1187.25159941029);
#2508=CIRCLE('',#13617,1187.2515994038);
#2509=CIRCLE('',#13618,1187.25365511458);
#2510=CIRCLE('',#13619,1187.25431295325);
#2511=CIRCLE('',#13620,1187.25159942133);
#2512=CIRCLE('',#13621,1187.25159939926);
#2513=CIRCLE('',#13622,1187.25365512903);
#2514=CIRCLE('',#13623,1187.2543129837);
#2515=CIRCLE('',#13624,1187.2515994291);
#2516=CIRCLE('',#13625,1187.25159943443);
#2517=CIRCLE('',#13626,1187.25365512723);
#2518=CIRCLE('',#13627,1187.25431299336);
#2519=CIRCLE('',#13628,1187.25159941435);
#2520=CIRCLE('',#13629,1187.25159942688);
#2521=CIRCLE('',#13630,1187.25159941979);
#2522=CIRCLE('',#13631,1187.25159941986);
#2523=CIRCLE('',#13632,1187.25159943305);
#2524=CIRCLE('',#13633,1187.2515994192);
#2525=CIRCLE('',#13634,1187.25365512172);
#2526=CIRCLE('',#13635,1187.25431297033);
#2527=CIRCLE('',#13636,1187.2515994132);
#2528=CIRCLE('',#13637,1187.25159939511);
#2529=CIRCLE('',#13638,1187.25365511663);
#2530=CIRCLE('',#13639,1187.25431293833);
#2531=CIRCLE('',#13640,1187.25159941033);
#2532=CIRCLE('',#13641,1187.25159940711);
#2533=CIRCLE('',#13642,1187.25365511087);
#2534=CIRCLE('',#13643,1187.25431299739);
#2535=CIRCLE('',#13644,1187.25159944517);
#2536=CIRCLE('',#13645,1187.25159940862);
#2537=CIRCLE('',#13646,1187.25159943111);
#2538=CIRCLE('',#13647,1187.25159944031);
#2539=CIRCLE('',#13648,1187.25159941049);
#2540=CIRCLE('',#13649,1187.25159940449);
#2541=CIRCLE('',#13650,1187.25365511182);
#2542=CIRCLE('',#13651,1187.25431298523);
#2543=CIRCLE('',#13652,1187.25159941186);
#2544=CIRCLE('',#13653,1187.2515994023);
#2545=CIRCLE('',#13654,1187.2536551145);
#2546=CIRCLE('',#13655,1187.25431297681);
#2547=CIRCLE('',#13656,1187.25159942333);
#2548=CIRCLE('',#13657,1187.25159939856);
#2549=CIRCLE('',#13658,1187.25365512919);
#2550=CIRCLE('',#13659,1187.25431298215);
#2551=CIRCLE('',#13660,1187.2515994291);
#2552=CIRCLE('',#13661,1187.25159943443);
#2553=CIRCLE('',#13662,1187.25159944835);
#2554=CIRCLE('',#13663,1187.25159943896);
#2555=CIRCLE('',#13664,1187.25159941435);
#2556=CIRCLE('',#13665,1187.25159942352);
#2557=CIRCLE('',#13666,1187.25365510695);
#2558=CIRCLE('',#13667,1187.25431298853);
#2559=CIRCLE('',#13668,1187.25159940573);
#2560=CIRCLE('',#13669,1187.25159941578);
#2561=CIRCLE('',#13670,1187.25365512172);
#2562=CIRCLE('',#13671,1187.25431296975);
#2563=CIRCLE('',#13672,1187.25159941323);
#2564=CIRCLE('',#13673,1187.25159939663);
#2565=CIRCLE('',#13674,1187.25159940667);
#2566=CIRCLE('',#13675,1187.25159943706);
#2567=CIRCLE('',#13677,15.5);
#2568=CIRCLE('',#13679,15.5);
#2569=CIRCLE('',#13681,15.5);
#2570=CIRCLE('',#13682,15.5);
#2571=CIRCLE('',#13683,15.5);
#2572=CIRCLE('',#13684,15.5);
#2573=CIRCLE('',#13685,15.5);
#2574=CIRCLE('',#13686,15.5);
#2575=CIRCLE('',#13687,15.5);
#2576=CIRCLE('',#13688,15.5);
#2577=CIRCLE('',#13689,15.5);
#2578=CIRCLE('',#13690,15.5);
#2579=CIRCLE('',#13691,15.5);
#2580=CIRCLE('',#13692,15.5);
#2581=CIRCLE('',#13693,15.5);
#2582=CIRCLE('',#13694,15.5);
#2583=CIRCLE('',#13695,15.5);
#2584=CIRCLE('',#13696,15.5);
#2585=CIRCLE('',#13715,1.);
#2586=CIRCLE('',#13716,1.);
#2587=CIRCLE('',#13718,1.);
#2588=CIRCLE('',#13719,1.);
#2589=CIRCLE('',#13721,1.);
#2590=CIRCLE('',#13722,1.);
#2591=CIRCLE('',#13724,13.2);
#2592=CIRCLE('',#13725,0.3);
#2593=CIRCLE('',#13726,13.5);
#2594=CIRCLE('',#13727,13.5);
#2595=CIRCLE('',#13729,13.5);
#2596=CIRCLE('',#13731,5.5);
#2597=CIRCLE('',#13733,5.5);
#2598=CIRCLE('',#13737,6.767);
#2599=CIRCLE('',#13798,7.911);
#2600=CIRCLE('',#13799,7.911);
#2601=CIRCLE('',#13801,6.767);
#2602=CIRCLE('',#13803,2.);
#2603=CIRCLE('',#13804,2.);
#2604=CIRCLE('',#13806,2.);
#2605=CIRCLE('',#13807,2.);
#2606=CIRCLE('',#13809,2.);
#2607=CIRCLE('',#13810,2.);
#2608=CIRCLE('',#13812,2.);
#2609=CIRCLE('',#13813,2.);
#2610=CIRCLE('',#13815,20.);
#2611=CIRCLE('',#13816,1.);
#2612=CIRCLE('',#13817,19.);
#2613=CIRCLE('',#13818,20.);
#2614=CIRCLE('',#13820,20.);
#2615=CIRCLE('',#13821,20.);
#2616=CIRCLE('',#13824,19.);
#2617=CIRCLE('',#13825,1.);
#2618=CIRCLE('',#13830,6.);
#2619=CIRCLE('',#13836,6.);
#2620=CIRCLE('',#13838,6.);
#2621=CIRCLE('',#13841,4.5);
#2622=CIRCLE('',#13844,4.5);
#2623=CIRCLE('',#13846,4.5);
#2624=CIRCLE('',#13848,4.5);
#2625=CIRCLE('',#13853,22.5);
#2626=CIRCLE('',#13854,0.5);
#2627=CIRCLE('',#13855,23.);
#2628=CIRCLE('',#13856,23.);
#2629=CIRCLE('',#13858,23.);
#2630=CIRCLE('',#13860,1.);
#2631=CIRCLE('',#13861,1.);
#2632=CIRCLE('',#13862,1.);
#2633=CIRCLE('',#13863,1.);
#2634=CIRCLE('',#13864,10.);
#2635=CIRCLE('',#13866,1.);
#2636=CIRCLE('',#13868,1.);
#2637=CIRCLE('',#13870,1.);
#2638=CIRCLE('',#13872,1.);
#2639=CIRCLE('',#13874,10.);
#2640=CIRCLE('',#13878,1.);
#2641=CIRCLE('',#13879,1.);
#2642=CIRCLE('',#13882,1.);
#2643=CIRCLE('',#13883,1.);
#2644=CIRCLE('',#13886,1.);
#2645=CIRCLE('',#13887,1.);
#2646=CIRCLE('',#13890,1.);
#2647=CIRCLE('',#13891,1.);
#2648=CIRCLE('',#13894,8.5);
#2649=CIRCLE('',#13895,8.5);
#2650=CIRCLE('',#13897,1.);
#2651=CIRCLE('',#13898,1.);
#2652=CIRCLE('',#13901,1.);
#2653=CIRCLE('',#13902,1.);
#2654=CIRCLE('',#13905,1.);
#2655=CIRCLE('',#13906,1.);
#2656=CIRCLE('',#13909,2.5);
#2657=CIRCLE('',#13910,2.5);
#2658=CIRCLE('',#13912,2.5);
#2659=CIRCLE('',#13913,2.5);
#2660=CIRCLE('',#13915,2.5);
#2661=CIRCLE('',#13916,2.5);
#2662=CIRCLE('',#13918,2.5);
#2663=CIRCLE('',#13919,2.5);
#2664=CIRCLE('',#13921,5.);
#2665=CIRCLE('',#13922,5.);
#2666=CIRCLE('',#13924,5.);
#2667=CIRCLE('',#13925,5.);
#2668=CIRCLE('',#13926,23.);
#2669=CIRCLE('',#13927,23.);
#2670=CIRCLE('',#13928,5.);
#2671=CIRCLE('',#13931,5.);
#2672=CIRCLE('',#13933,5.);
#2673=CIRCLE('',#13936,5.);
#2674=CIRCLE('',#13939,13.5);
#2675=CIRCLE('',#13942,13.5);
#2676=CIRCLE('',#13944,13.5);
#2677=CIRCLE('',#13945,13.5);
#2678=CIRCLE('',#13952,13.5);
#2679=CIRCLE('',#13953,13.5);
#2680=CIRCLE('',#13956,13.5);
#2681=CIRCLE('',#13958,10.5);
#2682=CIRCLE('',#13961,10.5);
#2683=CIRCLE('',#13963,20.);
#2684=CIRCLE('',#13965,20.);
#2685=CIRCLE('',#13967,23.);
#2686=CIRCLE('',#13973,1.);
#2687=CIRCLE('',#13974,1.);
#2688=CIRCLE('',#13976,1.);
#2689=CIRCLE('',#13977,1.);
#2690=CIRCLE('',#13979,1.);
#2691=CIRCLE('',#13980,1.);
#2692=CIRCLE('',#13982,13.2);
#2693=CIRCLE('',#13983,0.3);
#2694=CIRCLE('',#13984,13.5);
#2695=CIRCLE('',#13985,13.5);
#2696=CIRCLE('',#13987,13.5);
#2697=CIRCLE('',#13989,5.5);
#2698=CIRCLE('',#13991,5.5);
#2699=CIRCLE('',#13995,6.24166666666667);
#2700=CIRCLE('',#13996,2.0625);
#2701=CIRCLE('',#13997,6.24166666666667);
#2702=CIRCLE('',#13999,4.5);
#2703=CIRCLE('',#14000,4.75208333333333);
#2704=CIRCLE('',#14001,4.75208333333333);
#2705=CIRCLE('',#14002,4.5);
#2706=CIRCLE('',#14004,4.5);
#2707=CIRCLE('',#14006,4.75208333333333);
#2708=CIRCLE('',#14008,0.260975870478375);
#2709=CIRCLE('',#14009,5.00416666666667);
#2710=CIRCLE('',#14011,5.98069079618829);
#2711=CIRCLE('',#14012,0.260975870478375);
#2712=CIRCLE('',#14013,6.24166666666667);
#2713=CIRCLE('',#14016,6.24166666666667);
#2714=CIRCLE('',#14018,0.260975870478375);
#2715=CIRCLE('',#14019,5.98069079618829);
#2716=CIRCLE('',#14021,5.00416666666667);
#2717=CIRCLE('',#14022,0.260975870478376);
#2718=CIRCLE('',#14026,2.0625);
#2719=CIRCLE('',#14028,6.46166666666667);
#2720=CIRCLE('',#14029,6.46166666666667);
#2721=CIRCLE('',#14031,0.0439999999999998);
#2722=CIRCLE('',#14032,6.50566666666666);
#2723=CIRCLE('',#14034,8.9);
#2724=CIRCLE('',#14035,8.79);
#2725=CIRCLE('',#14036,8.9);
#2726=CIRCLE('',#14038,8.9);
#2727=CIRCLE('',#14042,8.9);
#2728=CIRCLE('',#14043,8.9);
#2729=CIRCLE('',#14045,6.46166666666667);
#2730=CIRCLE('',#14046,6.46166666666667);
#2731=CIRCLE('',#14048,6.50566666666666);
#2732=CIRCLE('',#14049,0.0439999999999998);
#2733=CIRCLE('',#14051,8.79);
#2734=CIRCLE('',#14055,8.9);
#2735=CIRCLE('',#14056,9.01847925309041);
#2736=CIRCLE('',#14058,9.16847925309041);
#2737=CIRCLE('',#14060,10.);
#2738=CIRCLE('',#14061,9.82679491924311);
#2739=CIRCLE('',#14062,10.);
#2740=CIRCLE('',#14064,10.);
#2741=CIRCLE('',#14066,9.82679491924311);
#2742=CIRCLE('',#14068,9.0184792530904);
#2743=CIRCLE('',#14069,9.1684792530904);
#2744=CIRCLE('',#14071,8.9);
#2745=CIRCLE('',#14072,8.9);
#2746=CIRCLE('',#14074,8.9);
#2747=CIRCLE('',#14076,2.0625);
#2748=CIRCLE('',#14077,8.9);
#2749=CIRCLE('',#14082,2.0625);
#2750=CIRCLE('',#14084,2.0625);
#2751=CIRCLE('',#14086,2.0625);
#2752=CIRCLE('',#14088,2.0625);
#2753=CIRCLE('',#14090,2.0625);
#2754=CIRCLE('',#14092,2.0625);
#2755=CIRCLE('',#14094,2.0625);
#2756=CIRCLE('',#14096,2.0625);
#2757=CIRCLE('',#14098,6.24166666666667);
#2758=CIRCLE('',#14099,6.24166666666667);
#2759=CIRCLE('',#14101,0.0824999999999997);
#2760=CIRCLE('',#14102,6.40666666666666);
#2761=CIRCLE('',#14104,6.40666666666667);
#2762=CIRCLE('',#14106,0.0228986158278278);
#2763=CIRCLE('',#14107,6.45211601689499);
#2764=CIRCLE('',#14108,6.45211601689499);
#2765=CIRCLE('',#14110,6.46166666666667);
#2766=CIRCLE('',#14111,6.46166666666667);
#2767=CIRCLE('',#14113,6.46166666666667);
#2768=CIRCLE('',#14117,20.);
#2769=CIRCLE('',#14118,20.);
#2770=CIRCLE('',#14119,0.275);
#2771=CIRCLE('',#14120,19.725);
#2772=CIRCLE('',#14122,20.);
#2773=CIRCLE('',#14123,0.275);
#2774=CIRCLE('',#14124,19.725);
#2775=CIRCLE('',#14126,15.4);
#2776=CIRCLE('',#14127,18.1997760045464);
#2777=CIRCLE('',#14132,13.0685506725942);
#2778=CIRCLE('',#14133,13.0685506725942);
#2779=CIRCLE('',#14134,12.7058184384753);
#2780=CIRCLE('',#14135,12.7058184384753);
#2781=CIRCLE('',#14137,17.5762965073726);
#2782=CIRCLE('',#14138,17.5762965073726);
#2783=CIRCLE('',#14139,16.6071946160828);
#2784=CIRCLE('',#14140,16.6071946160828);
#2785=CIRCLE('',#14142,13.3064408708579);
#2786=CIRCLE('',#14143,0.500000000000001);
#2787=CIRCLE('',#14144,13.9143221901933);
#2788=CIRCLE('',#14145,13.9143221901933);
#2789=CIRCLE('',#14147,12.4591576910941);
#2790=CIRCLE('',#14148,12.4591576910941);
#2791=CIRCLE('',#14201,2.74859462638384);
#2792=CIRCLE('',#14202,2.74859462638384);
#2793=CIRCLE('',#14204,2.74859462638384);
#2794=CIRCLE('',#14205,2.74859462638384);
#2795=CIRCLE('',#14209,2.74859462638384);
#2796=CIRCLE('',#14210,2.74859462638384);
#2797=CIRCLE('',#14212,2.74859462638384);
#2798=CIRCLE('',#14213,2.74859462638384);
#2799=CIRCLE('',#14217,2.74859462638385);
#2800=CIRCLE('',#14218,2.74859462638384);
#2801=CIRCLE('',#14220,2.74859462638384);
#2802=CIRCLE('',#14221,2.74859462638385);
#2803=CIRCLE('',#14225,2.74859462638384);
#2804=CIRCLE('',#14226,2.74859462638384);
#2805=CIRCLE('',#14228,2.74859462638384);
#2806=CIRCLE('',#14229,2.74859462638384);
#2807=CIRCLE('',#14233,2.74859462638384);
#2808=CIRCLE('',#14234,2.74859462638384);
#2809=CIRCLE('',#14236,2.74859462638384);
#2810=CIRCLE('',#14237,2.74859462638384);
#2811=CIRCLE('',#14241,2.74859462638384);
#2812=CIRCLE('',#14242,2.74859462638384);
#2813=CIRCLE('',#14244,2.74859462638384);
#2814=CIRCLE('',#14245,2.74859462638384);
#2815=CIRCLE('',#14249,2.74859462638384);
#2816=CIRCLE('',#14250,2.74859462638384);
#2817=CIRCLE('',#14252,2.74859462638384);
#2818=CIRCLE('',#14253,2.74859462638384);
#2819=CIRCLE('',#14257,2.74859462638384);
#2820=CIRCLE('',#14258,2.74859462638384);
#2821=CIRCLE('',#14260,2.74859462638384);
#2822=CIRCLE('',#14261,2.74859462638384);
#2823=CIRCLE('',#14265,2.74859462638384);
#2824=CIRCLE('',#14266,2.74859462638384);
#2825=CIRCLE('',#14268,2.74859462638384);
#2826=CIRCLE('',#14269,2.74859462638384);
#2827=CIRCLE('',#14273,2.74859462638384);
#2828=CIRCLE('',#14274,2.74859462638384);
#2829=CIRCLE('',#14276,2.74859462638384);
#2830=CIRCLE('',#14277,2.74859462638384);
#2831=CIRCLE('',#14281,2.74859462638384);
#2832=CIRCLE('',#14282,2.74859462638384);
#2833=CIRCLE('',#14284,2.74859462638384);
#2834=CIRCLE('',#14285,2.74859462638384);
#2835=CIRCLE('',#14289,8.775);
#2836=CIRCLE('',#14290,0.275);
#2837=CIRCLE('',#14291,8.5);
#2838=CIRCLE('',#14292,8.5);
#2839=CIRCLE('',#14294,8.775);
#2840=CIRCLE('',#14295,0.275);
#2841=CIRCLE('',#14296,8.5);
#2842=CIRCLE('',#14298,11.9728634517814);
#2843=CIRCLE('',#14299,10.6410293263727);
#2844=CIRCLE('',#14300,10.6410293263727);
#2845=CIRCLE('',#14302,12.6998790237181);
#2846=CIRCLE('',#14303,12.6998790237181);
#2847=CIRCLE('',#14305,14.0317131491268);
#2848=CIRCLE('',#14307,14.0317131491268);
#2849=CIRCLE('',#14310,11.9728634517814);
#2850=CIRCLE('',#14314,2.62159462638384);
#2851=CIRCLE('',#14315,2.62159462638384);
#2852=CIRCLE('',#14319,2.62159462638384);
#2853=CIRCLE('',#14320,2.62159462638384);
#2854=CIRCLE('',#14324,2.62159462638384);
#2855=CIRCLE('',#14325,2.62159462638384);
#2856=CIRCLE('',#14329,2.62159462638384);
#2857=CIRCLE('',#14330,2.62159462638384);
#2858=CIRCLE('',#14334,2.62159462638384);
#2859=CIRCLE('',#14335,2.62159462638384);
#2860=CIRCLE('',#14339,2.62159462638384);
#2861=CIRCLE('',#14340,2.62159462638384);
#2862=CIRCLE('',#14344,2.62159462638384);
#2863=CIRCLE('',#14345,2.62159462638384);
#2864=CIRCLE('',#14349,2.62159462638384);
#2865=CIRCLE('',#14350,2.62159462638384);
#2866=CIRCLE('',#14354,2.62159462638384);
#2867=CIRCLE('',#14355,2.62159462638384);
#2868=CIRCLE('',#14359,2.62159462638384);
#2869=CIRCLE('',#14360,2.62159462638384);
#2870=CIRCLE('',#14364,2.62159462638384);
#2871=CIRCLE('',#14365,2.62159462638384);
#2872=B_SPLINE_CURVE_WITH_KNOTS('',3,(#17360,#17361,#17362,#17363,#17364,
#17365,#17366,#17367),.UNSPECIFIED.,.F.,.F.,(4,1,1,1,1,4),(87.0483584551456,
87.288606653755,87.7848809882288,88.2811553227026,88.7774296571764,89.2737039916502),
 .UNSPECIFIED.);
#2873=B_SPLINE_CURVE_WITH_KNOTS('',3,(#17370,#17371,#17372,#17373,#17374,
#17375,#17376,#17377,#17378),.UNSPECIFIED.,.F.,.F.,(4,1,1,1,1,1,4),(87.0483757384693,
87.3511807444607,87.8474550789345,88.3437294134083,88.8400037478821,89.3362780823559,
89.7970772629679),.UNSPECIFIED.);
#2874=B_SPLINE_CURVE_WITH_KNOTS('',3,(#17384,#17385,#17386,#17387,#17388,
#17389,#17390,#17391,#17392,#17393,#17394,#17395,#17396,#17397,#17398,#17399,
#17400,#17401,#17402,#17403,#17404,#17405,#17406,#17407,#17408,#17409,#17410,
#17411,#17412,#17413,#17414,#17415,#17416,#17417,#17418,#17419,#17420,#17421,
#17422,#17423,#17424,#17425,#17426,#17427,#17428,#17429,#17430,#17431,#17432,
#17433,#17434,#17435,#17436,#17437,#17438,#17439,#17440,#17441,#17442,#17443,
#17444,#17445,#17446,#17447,#17448,#17449,#17450,#17451,#17452,#17453,#17454,
#17455,#17456,#17457,#17458,#17459,#17460,#17461,#17462,#17463,#17464,#17465,
#17466,#17467,#17468,#17469,#17470,#17471,#17472,#17473,#17474,#17475,#17476,
#17477,#17478,#17479,#17480,#17481,#17482,#17483,#17484,#17485,#17486,#17487,
#17488,#17489,#17490,#17491,#17492,#17493,#17494,#17495,#17496,#17497,#17498,
#17499,#17500,#17501,#17502,#17503,#17504,#17505,#17506,#17507,#17508,#17509,
#17510,#17511,#17512,#17513,#17514,#17515,#17516,#17517,#17518,#17519,#17520,
#17521,#17522,#17523,#17524,#17525,#17526,#17527,#17528,#17529,#17530,#17531,
#17532,#17533,#17534,#17535,#17536,#17537,#17538,#17539,#17540,#17541,#17542,
#17543,#17544,#17545,#17546,#17547,#17548,#17549,#17550,#17551,#17552,#17553,
#17554,#17555,#17556,#17557,#17558),.UNSPECIFIED.,.F.,.F.,(4,3,3,3,3,3,
3,3,3,3,3,3,3,3,3,3,3,3,3,3,3,3,3,3,3,3,3,3,3,3,3,3,3,3,3,3,3,3,3,3,3,3,
3,3,3,3,3,3,3,3,3,3,3,3,3,3,3,3,4),(80.7651597880717,80.8370403055957,80.914545344832,
80.9920362923502,81.0695186842698,81.1470072216587,81.2244955439902,81.3020000212182,
81.3333146400695,81.4108196470028,81.4883105620921,81.5657929215612,81.6432814267086,
81.7207697169786,81.7982741626174,81.8295889745433,81.9070940470507,81.9845850279213,
82.0620674531671,82.1395560235961,82.2170443787414,82.2945488882385,82.3258633090171,
82.4033682793892,82.4808591578936,82.5583414808702,82.6358299499321,82.7133182044183,
82.790822614948,82.8221376434909,82.8996427153748,82.9771336953985,83.0546161195796,
83.1321046886325,83.2095930422246,83.2870975499181,83.3184119779647,83.3959170883937,
83.4734081078065,83.5508905720845,83.6283791819793,83.7058675767654,83.7833721259062,
83.8146863124385,83.8921909082518,83.9696814101362,84.0471633556579,84.1246514488292,
84.2021393290257,84.2796433700398,84.3109606469122,84.3884668552791,84.4659589764845,
84.5434425428528,84.6209322471122,84.6984217297766,84.7759273502229,84.807234981386,
84.8230016469244),.UNSPECIFIED.);
#2875=B_SPLINE_CURVE_WITH_KNOTS('',3,(#17559,#17560,#17561,#17562,#17563,
#17564,#17565,#17566),.UNSPECIFIED.,.F.,.F.,(4,1,1,1,1,4),(84.8230016659403,
85.3035093158598,85.7997836503336,86.2960579848074,86.7923323192812,87.0483584551456),
 .UNSPECIFIED.);
#2876=B_SPLINE_CURVE_WITH_KNOTS('',3,(#17568,#17569,#17570,#17571,#17572,
#17573,#17574,#17575,#17576),.UNSPECIFIED.,.F.,.F.,(4,1,1,1,1,1,4),(84.8230016469244,
84.8698090720917,85.3660834065655,85.8623577410393,86.3586320755131,86.8549064099869,
87.0483757384693),.UNSPECIFIED.);
#2877=B_SPLINE_CURVE_WITH_KNOTS('',3,(#17577,#17578,#17579,#17580,#17581,
#17582,#17583,#17584,#17585,#17586,#17587,#17588,#17589,#17590,#17591,#17592,
#17593,#17594,#17595,#17596,#17597,#17598,#17599,#17600,#17601,#17602,#17603,
#17604,#17605,#17606,#17607,#17608,#17609,#17610,#17611,#17612,#17613,#17614,
#17615,#17616,#17617,#17618,#17619,#17620,#17621,#17622,#17623,#17624,#17625,
#17626,#17627,#17628,#17629,#17630,#17631,#17632,#17633,#17634,#17635,#17636,
#17637,#17638,#17639,#17640,#17641,#17642,#17643,#17644,#17645,#17646,#17647,
#17648,#17649,#17650,#17651,#17652,#17653,#17654,#17655,#17656,#17657,#17658,
#17659,#17660,#17661,#17662,#17663,#17664,#17665,#17666,#17667,#17668,#17669,
#17670,#17671,#17672,#17673,#17674,#17675,#17676,#17677,#17678,#17679,#17680,
#17681,#17682,#17683,#17684,#17685,#17686,#17687,#17688,#17689,#17690,#17691,
#17692,#17693,#17694,#17695,#17696,#17697,#17698,#17699,#17700,#17701,#17702,
#17703,#17704,#17705,#17706,#17707,#17708,#17709,#17710,#17711,#17712,#17713,
#17714,#17715,#17716,#17717,#17718,#17719,#17720,#17721,#17722,#17723,#17724,
#17725,#17726,#17727,#17728,#17729,#17730,#17731,#17732,#17733,#17734,#17735,
#17736,#17737,#17738,#17739,#17740,#17741,#17742,#17743,#17744,#17745,#17746,
#17747,#17748),.UNSPECIFIED.,.F.,.F.,(4,3,3,3,3,3,3,3,3,3,3,3,3,3,3,3,3,
3,3,3,3,3,3,3,3,3,3,3,3,3,3,3,3,3,3,3,3,3,3,3,3,3,3,3,3,3,3,3,3,3,3,3,3,
3,3,3,3,4),(80.7651593553048,80.8426649664577,80.8996143963013,80.9771194265575,
81.0546103650544,81.1320927479402,81.2095812763449,81.2870695897373,81.3645740581496,
81.3958887307751,81.4733937598586,81.5508846971797,81.6283670788907,81.7058556061292,
81.7833439183629,81.860848385635,81.8921630652489,81.9696680959697,82.0471590349305,
82.1246414182788,82.2021299471396,82.2796182609839,82.3571227298382,82.3884373997227,
82.4659424292746,82.5434333670696,82.6209157492587,82.6984042769776,82.7758925896912,
82.8533970574419,82.8847117341965,82.962216761565,83.0397076971565,83.1171900771288,
83.1946786026281,83.2721669131255,83.3496713786775,83.3809860686703,83.4584911079066,
83.5359820554258,83.6134644473447,83.6909529847341,83.7684413070656,83.8459457842936,
83.8772604031441,83.9547654100771,84.0322563251666,84.1097386846358,84.1872271897834,
84.2647154800541,84.3422199256925,84.3735347376179,84.4507891948756,84.5280287669538,
84.6052689644067,84.6825047195202,84.7597573289946,84.8230016469244),
 .UNSPECIFIED.);
#2878=B_SPLINE_CURVE_WITH_KNOTS('',3,(#17754,#17755,#17756,#17757,#17758,
#17759,#17760,#17761,#17762,#17763,#17764,#17765),.UNSPECIFIED.,.F.,.F.,
(4,1,1,1,1,1,1,1,1,4),(74.4820139112556,74.8817482919101,75.3780226263839,
75.8742969608577,76.3705712953315,76.8668456298053,77.3631199642791,77.8593942987529,
78.3556686332267,78.5398163045171),.UNSPECIFIED.);
#2879=B_SPLINE_CURVE_WITH_KNOTS('',3,(#17766,#17767,#17768,#17769,#17770,
#17771,#17772,#17773,#17774,#17775,#17776,#17777,#17778,#17779,#17780,#17781,
#17782,#17783,#17784,#17785,#17786,#17787,#17788,#17789,#17790,#17791,#17792,
#17793,#17794,#17795,#17796,#17797,#17798,#17799,#17800,#17801,#17802,#17803,
#17804,#17805,#17806,#17807,#17808,#17809,#17810,#17811,#17812,#17813,#17814,
#17815,#17816,#17817,#17818,#17819,#17820,#17821,#17822,#17823,#17824,#17825,
#17826,#17827,#17828,#17829,#17830,#17831,#17832,#17833,#17834,#17835,#17836,
#17837,#17838,#17839,#17840,#17841,#17842,#17843,#17844,#17845,#17846,#17847,
#17848,#17849,#17850,#17851,#17852,#17853,#17854,#17855,#17856,#17857,#17858,
#17859),.UNSPECIFIED.,.F.,.F.,(4,3,3,3,3,3,3,3,3,3,3,3,3,3,3,3,3,3,3,3,
3,3,3,3,3,3,3,3,3,3,3,4),(78.5398163397448,78.6178479967337,78.6954897638523,
78.7737163657764,78.8519429677005,78.9294479967842,79.0069389341053,79.084421315816,
79.1619098430544,79.2393981552877,79.3169026225599,79.3482173021743,79.4257223328949,
79.5032132718561,79.5806956552048,79.6581841840654,79.735672497909,79.8131769667635,
79.8444916366481,79.9219966662,79.9994876039955,80.0769699861842,80.1544585139031,
80.2319468266171,80.3094512943681,80.3407659711219,80.4182703729319,80.495760433696,
80.5732483850591,80.6507311082695,80.7282234409962,80.7651597880717),
 .UNSPECIFIED.);
#2880=B_SPLINE_CURVE_WITH_KNOTS('',3,(#17861,#17862,#17863,#17864,#17865,
#17866,#17867,#17868,#17869,#17870,#17871,#17872,#17873,#17874,#17875,#17876,
#17877,#17878,#17879,#17880,#17881,#17882,#17883,#17884,#17885,#17886,#17887,
#17888,#17889,#17890,#17891,#17892,#17893,#17894,#17895,#17896,#17897,#17898,
#17899,#17900,#17901,#17902,#17903,#17904,#17905,#17906,#17907,#17908,#17909,
#17910,#17911,#17912,#17913,#17914,#17915,#17916,#17917,#17918,#17919,#17920,
#17921,#17922,#17923,#17924,#17925,#17926,#17927,#17928,#17929,#17930,#17931,
#17932,#17933,#17934,#17935,#17936,#17937,#17938,#17939,#17940,#17941,#17942,
#17943,#17944,#17945,#17946,#17947,#17948,#17949,#17950,#17951,#17952,#17953,
#17954),.UNSPECIFIED.,.F.,.F.,(4,3,3,3,3,3,3,3,3,3,3,3,3,3,3,3,3,3,3,3,
3,3,3,3,3,3,3,3,3,3,3,4),(78.5398163397448,78.6170621768428,78.6943109079355,
78.7715563124194,78.8488208011277,78.9145170584062,78.9920220882176,79.0695130262683,
79.1469954087081,79.2244839366697,79.3019722496216,79.3794767176006,79.41079139288,
79.4882964226991,79.5657873607574,79.6432697432046,79.7207582711736,79.7982465841325,
79.8757510521183,79.9070657273538,79.9845707572399,80.0620616953655,80.139544077881,
80.2170326059175,80.2945209189436,80.3720253869959,80.4033400618275,80.4808443139909,
80.5583386268419,80.6358226274582,80.713310678145,80.7651593553048),
 .UNSPECIFIED.);
#2881=B_SPLINE_CURVE_WITH_KNOTS('',3,(#17955,#17956,#17957,#17958,#17959,
#17960,#17961,#17962,#17963,#17964,#17965,#17966,#17967,#17968,#17969,#17970,
#17971,#17972,#17973,#17974,#17975,#17976,#17977,#17978,#17979,#17980,#17981,
#17982,#17983,#17984,#17985,#17986,#17987,#17988,#17989,#17990,#17991,#17992,
#17993,#17994,#17995,#17996,#17997,#17998,#17999,#18000,#18001,#18002,#18003,
#18004,#18005,#18006,#18007,#18008,#18009,#18010,#18011,#18012,#18013,#18014,
#18015,#18016,#18017,#18018,#18019,#18020,#18021,#18022,#18023,#18024,#18025,
#18026,#18027,#18028,#18029,#18030,#18031,#18032,#18033,#18034,#18035,#18036,
#18037,#18038,#18039,#18040,#18041,#18042,#18043,#18044,#18045,#18046,#18047,
#18048,#18049,#18050,#18051,#18052,#18053,#18054,#18055,#18056,#18057,#18058,
#18059,#18060,#18061,#18062,#18063,#18064,#18065,#18066,#18067,#18068,#18069,
#18070,#18071,#18072,#18073,#18074,#18075,#18076,#18077,#18078,#18079,#18080,
#18081,#18082,#18083,#18084,#18085,#18086,#18087,#18088,#18089,#18090,#18091,
#18092,#18093,#18094,#18095,#18096,#18097,#18098,#18099,#18100,#18101,#18102,
#18103,#18104,#18105,#18106,#18107,#18108,#18109,#18110,#18111,#18112,#18113,
#18114,#18115,#18116,#18117,#18118,#18119,#18120,#18121,#18122,#18123,#18124,
#18125,#18126),.UNSPECIFIED.,.F.,.F.,(4,3,3,3,3,3,3,3,3,3,3,3,3,3,3,3,3,
3,3,3,3,3,3,3,3,3,3,3,3,3,3,3,3,3,3,3,3,3,3,3,3,3,3,3,3,3,3,3,3,3,3,3,3,
3,3,3,3,4),(74.4819991062224,74.5594972817628,74.6369837912023,74.7144748782765,
74.7919626281567,74.8694696203011,74.9443223826158,75.0218274124397,75.0993183505029,
75.1768007329554,75.2542892609294,75.3317775738933,75.4092820418842,75.4405967170896,
75.5181017469132,75.5955926849761,75.6730750674282,75.7505635954018,75.8280519083655,
75.9055563763561,75.9368710515634,76.0143760813873,76.0918670194505,76.1693494019029,
76.2468379298769,76.3243262428409,76.4018307108318,76.4331453860372,76.5106504158612,
76.5881413539246,76.6656237363772,76.7431122643514,76.8206005773155,76.8981050453065,
76.929419720511,77.0069247503333,77.0844156883949,77.1618980708456,77.239386598818,
77.3168749117803,77.3943793797696,77.4256940549848,77.5031990848125,77.5806900228796,
77.658172405336,77.7356609333137,77.8131492462817,77.8906537142763,77.9219683894586,
77.9994734192743,78.0769643573295,78.1544467397738,78.2319352677398,78.3094235806959,
78.3869280486788,78.4182427239324,78.4997461276738,78.5398163396564),
 .UNSPECIFIED.);
#2882=B_SPLINE_CURVE_WITH_KNOTS('',3,(#18132,#18133,#18134,#18135,#18136,
#18137,#18138,#18139,#18140,#18141,#18142,#18143,#18144,#18145,#18146,#18147,
#18148,#18149,#18150,#18151,#18152,#18153,#18154,#18155,#18156,#18157,#18158,
#18159,#18160,#18161,#18162,#18163,#18164,#18165,#18166,#18167,#18168,#18169,
#18170,#18171,#18172,#18173,#18174,#18175,#18176,#18177,#18178,#18179,#18180,
#18181,#18182,#18183,#18184,#18185,#18186,#18187,#18188,#18189,#18190,#18191,
#18192,#18193,#18194,#18195,#18196,#18197,#18198,#18199,#18200,#18201,#18202,
#18203,#18204,#18205,#18206,#18207,#18208,#18209,#18210,#18211,#18212,#18213,
#18214,#18215,#18216,#18217,#18218,#18219,#18220,#18221,#18222,#18223,#18224,
#18225,#18226,#18227,#18228,#18229,#18230,#18231,#18232,#18233,#18234,#18235,
#18236,#18237,#18238,#18239,#18240,#18241,#18242,#18243,#18244,#18245,#18246,
#18247,#18248,#18249,#18250,#18251,#18252,#18253,#18254,#18255,#18256,#18257,
#18258,#18259,#18260,#18261,#18262,#18263,#18264,#18265,#18266,#18267,#18268,
#18269,#18270,#18271,#18272,#18273,#18274,#18275,#18276,#18277,#18278,#18279,
#18280,#18281,#18282,#18283,#18284,#18285,#18286,#18287,#18288,#18289,#18290,
#18291,#18292,#18293,#18294,#18295,#18296,#18297,#18298,#18299,#18300,#18301,
#18302,#18303),.UNSPECIFIED.,.F.,.F.,(4,3,3,3,3,3,3,3,3,3,3,3,3,3,3,3,3,
3,3,3,3,3,3,3,3,3,3,3,3,3,3,3,3,3,3,3,3,3,3,3,3,3,3,3,3,3,3,3,3,3,3,3,3,
3,3,3,3,4),(68.198801431243,68.2762891932681,68.3537963258945,68.4301819437508,
68.5076869735746,68.5851779116379,68.6626602940891,68.740148822063,68.8176371350266,
68.8951416030175,68.9264562782246,69.0039613080483,69.0814522461114,69.1589346285636,
69.2364231565373,69.3139114695007,69.3914159374917,69.4227306126984,69.500235642522,
69.5777265805855,69.6552089630386,69.7326974910125,69.8101858039759,69.8876902719668,
69.9190049471722,69.9965099769959,70.0740009150587,70.1514832975117,70.2289718254855,
70.306460138449,70.38396460644,70.415279281646,70.4927843114698,70.5702752495332,
70.6477576319852,70.7252461599591,70.8027344729236,70.8802389409149,70.9115536161198,
70.9890586459435,71.0665495840061,71.1440319664588,71.2215204944324,71.2990088073963,
71.3765132753868,71.4078279505936,71.4853329804172,71.5628239184807,71.6403063009341,
71.7177948289081,71.7952831418719,71.872787609863,71.9041022850674,71.9814641664295,
72.0588148259056,72.1361550941926,72.213498904701,72.2566310325652),
 .UNSPECIFIED.);
#2883=B_SPLINE_CURVE_WITH_KNOTS('',3,(#18304,#18305,#18306,#18307,#18308,
#18309,#18310,#18311,#18312),.UNSPECIFIED.,.F.,.F.,(4,1,1,1,1,1,4),(72.2566310562343,
72.4003766195412,72.896650954015,73.3929252884888,73.8891996229626,74.3854739574363,
74.4820139112556),.UNSPECIFIED.);
#2884=B_SPLINE_CURVE_WITH_KNOTS('',3,(#18314,#18315,#18316,#18317,#18318,
#18319,#18320,#18321,#18322,#18323,#18324,#18325,#18326,#18327,#18328,#18329,
#18330,#18331,#18332,#18333,#18334,#18335,#18336,#18337,#18338,#18339,#18340,
#18341,#18342,#18343,#18344,#18345,#18346,#18347,#18348,#18349,#18350,#18351,
#18352,#18353,#18354,#18355,#18356,#18357,#18358,#18359,#18360,#18361,#18362,
#18363,#18364,#18365,#18366,#18367,#18368,#18369,#18370,#18371,#18372,#18373,
#18374,#18375,#18376,#18377,#18378,#18379,#18380,#18381,#18382,#18383,#18384,
#18385,#18386,#18387,#18388,#18389,#18390,#18391,#18392,#18393,#18394,#18395,
#18396,#18397,#18398,#18399,#18400,#18401,#18402,#18403,#18404,#18405,#18406,
#18407,#18408,#18409,#18410),.UNSPECIFIED.,.F.,.F.,(4,3,3,3,3,3,3,3,3,3,
3,3,3,3,3,3,3,3,3,3,3,3,3,3,3,3,3,3,3,3,3,3,4),(72.2566310326268,72.3358367452908,
72.4150680313353,72.4629507102468,72.5404557400706,72.6179466781338,72.695429060586,
72.7729175885598,72.8504059015235,72.927910369514,72.9592250447206,73.0367300745445,
73.1142210126076,73.1917033950602,73.269191923034,73.3466802359978,73.4241847039887,
73.4554993791944,73.5330044090182,73.6104953470813,73.6879777295337,73.7654662575075,
73.8429545704714,73.9204590384622,73.9517737136682,74.029278743492,74.1067696815552,
74.1842520640075,74.2617405919814,74.3392289049453,74.4167333729361,74.448048048142,
74.4819991062224),.UNSPECIFIED.);
#2885=B_SPLINE_CURVE_WITH_KNOTS('',3,(#18411,#18412,#18413,#18414,#18415,
#18416,#18417,#18418,#18419,#18420,#18421,#18422,#18423,#18424,#18425,#18426,
#18427,#18428,#18429,#18430,#18431,#18432,#18433,#18434,#18435,#18436,#18437,
#18438,#18439,#18440,#18441,#18442,#18443,#18444,#18445,#18446,#18447,#18448,
#18449,#18450,#18451,#18452,#18453,#18454,#18455,#18456,#18457,#18458,#18459,
#18460,#18461,#18462,#18463,#18464,#18465,#18466,#18467,#18468,#18469,#18470,
#18471,#18472,#18473,#18474,#18475,#18476,#18477,#18478,#18479,#18480,#18481,
#18482,#18483,#18484,#18485,#18486,#18487,#18488,#18489,#18490,#18491,#18492,
#18493,#18494,#18495,#18496,#18497,#18498,#18499,#18500,#18501,#18502,#18503,
#18504,#18505,#18506,#18507,#18508,#18509,#18510,#18511,#18512,#18513,#18514,
#18515,#18516,#18517,#18518,#18519,#18520,#18521,#18522,#18523,#18524,#18525,
#18526,#18527,#18528,#18529,#18530,#18531,#18532,#18533,#18534,#18535,#18536,
#18537,#18538,#18539,#18540,#18541,#18542,#18543,#18544,#18545,#18546,#18547,
#18548,#18549,#18550,#18551,#18552,#18553,#18554,#18555,#18556,#18557,#18558,
#18559,#18560,#18561,#18562,#18563,#18564,#18565,#18566,#18567,#18568,#18569,
#18570,#18571,#18572,#18573,#18574,#18575,#18576,#18577,#18578,#18579,#18580,
#18581,#18582),.UNSPECIFIED.,.F.,.F.,(4,3,3,3,3,3,3,3,3,3,3,3,3,3,3,3,3,
3,3,3,3,3,3,3,3,3,3,3,3,3,3,3,3,3,3,3,3,3,3,3,3,3,3,3,3,3,3,3,3,3,3,3,3,
3,3,3,3,4),(68.198812002236,68.2763021152483,68.3537898515224,68.4312957656329,
68.4927560344565,68.5702610642803,68.6477520023434,68.7252343847957,68.8027229127696,
68.8802112257334,68.9577156937242,68.9890303689303,69.0665353987541,69.1440263368171,
69.2215087192695,69.2989972472433,69.3764855602071,69.4539900281979,69.4853047034041,
69.5628097332279,69.640300671291,69.7177830537434,69.7952715817172,69.8727598946811,
69.9502643626719,69.9815790378779,70.0590840677017,70.1365750057647,70.214057388217,
70.2915459161909,70.3690342291547,70.4465386971454,70.4778533723517,70.5553584021755,
70.6328493402385,70.7103317226907,70.7878202506645,70.8653085636282,70.942813031619,
70.9741277068254,71.0516327366491,71.1291236747122,71.2066060571644,71.2840945851382,
71.361582898102,71.4390873660927,71.4704020412992,71.547907071123,71.6253980091863,
71.7028803916382,71.780368919612,71.8578572325758,71.9353617005666,71.966676375773,
72.0445687492081,72.122444909863,72.2003138435325,72.2566310325652),
 .UNSPECIFIED.);
#2886=B_SPLINE_CURVE_WITH_KNOTS('',3,(#18588,#18589,#18590,#18591,#18592,
#18593,#18594,#18595,#18596,#18597,#18598,#18599,#18600,#18601,#18602,#18603,
#18604,#18605,#18606,#18607,#18608,#18609,#18610,#18611,#18612,#18613,#18614,
#18615,#18616,#18617,#18618,#18619,#18620,#18621,#18622,#18623,#18624,#18625,
#18626,#18627,#18628,#18629,#18630,#18631,#18632,#18633,#18634,#18635,#18636,
#18637,#18638,#18639,#18640,#18641,#18642,#18643,#18644,#18645,#18646,#18647,
#18648,#18649,#18650,#18651,#18652,#18653,#18654,#18655,#18656,#18657,#18658,
#18659,#18660,#18661,#18662,#18663,#18664,#18665,#18666,#18667,#18668,#18669,
#18670,#18671,#18672,#18673,#18674,#18675,#18676,#18677,#18678,#18679,#18680,
#18681,#18682,#18683,#18684,#18685,#18686,#18687,#18688,#18689,#18690,#18691,
#18692,#18693,#18694,#18695,#18696,#18697,#18698,#18699,#18700,#18701,#18702,
#18703,#18704,#18705,#18706,#18707,#18708,#18709,#18710,#18711,#18712,#18713,
#18714,#18715,#18716,#18717,#18718,#18719,#18720,#18721,#18722,#18723,#18724,
#18725,#18726,#18727,#18728,#18729,#18730,#18731,#18732,#18733,#18734,#18735,
#18736,#18737,#18738,#18739,#18740,#18741,#18742,#18743,#18744,#18745,#18746,
#18747,#18748,#18749,#18750,#18751,#18752,#18753,#18754,#18755,#18756,#18757,
#18758,#18759,#18760,#18761,#18762),.UNSPECIFIED.,.F.,.F.,(4,3,3,3,3,3,
3,3,3,3,3,3,3,3,3,3,3,3,3,3,3,3,3,3,3,3,3,3,3,3,3,3,3,3,3,3,3,3,3,3,3,3,
3,3,3,3,3,3,3,3,3,3,3,3,3,3,3,3,4),(61.9156047763896,61.9786155955915,62.0561206254154,
62.1336115634786,62.2110939459307,62.2885824739047,62.3660707868687,62.4435752548594,
62.4748899300653,62.552394959889,62.6298858979524,62.7073682804045,62.7848568083784,
62.862345121342,62.9398495893327,62.9711642645391,63.0486692943629,63.126160232426,
63.2036426148776,63.2811311428513,63.3586194558156,63.4361239238064,63.4674385990129,
63.5449436288367,63.6224345668995,63.6999169493516,63.7774054773254,63.8548937902894,
63.9323982582801,63.9637129334867,64.0412179633103,64.1187089013731,64.1961912838254,
64.2736798117994,64.3511681247633,64.4286725927539,64.4599872679605,64.5374922977843,
64.614983235847,64.6924656183003,64.7699541462741,64.8474424592383,64.924946927229,
64.9562616024343,65.0337666322583,65.1112575703216,65.188739952774,65.266228480748,
65.3437167937126,65.4212212617037,65.452535936908,65.5300409667316,65.6075319047948,
65.6850142872465,65.7625028152201,65.8399911281846,65.9174955961746,65.9488102713818,
65.9734457253856),.UNSPECIFIED.);
#2887=B_SPLINE_CURVE_WITH_KNOTS('',3,(#18763,#18764,#18765,#18766,#18767,
#18768,#18769,#18770,#18771,#18772,#18773,#18774,#18775,#18776,#18777,#18778,
#18779,#18780,#18781,#18782,#18783,#18784,#18785,#18786,#18787,#18788,#18789,
#18790,#18791,#18792,#18793,#18794,#18795,#18796,#18797,#18798,#18799,#18800,
#18801,#18802,#18803,#18804,#18805,#18806,#18807,#18808,#18809,#18810,#18811,
#18812,#18813,#18814,#18815,#18816,#18817,#18818,#18819,#18820,#18821,#18822,
#18823,#18824,#18825,#18826,#18827,#18828,#18829,#18830,#18831,#18832,#18833,
#18834,#18835,#18836,#18837,#18838,#18839,#18840,#18841,#18842,#18843,#18844,
#18845,#18846,#18847,#18848,#18849,#18850,#18851,#18852,#18853,#18854,#18855,
#18856),.UNSPECIFIED.,.F.,.F.,(4,3,3,3,3,3,3,3,3,3,3,3,3,3,3,3,3,3,3,3,
3,3,3,3,3,3,3,3,3,3,3,4),(65.9734457254986,66.0507928770444,66.1281258638911,
66.2073655493822,66.2846965630064,66.364890584431,66.4450846058556,66.5225896356792,
66.6000805737422,66.6775629561948,66.7550514841686,66.8325397971324,66.910044265123,
66.9413589403294,67.0188639701531,67.0963549082163,67.173837290669,67.2513258186429,
67.3288141316065,67.4063185995973,67.4376332748032,67.5151383046269,67.5926292426899,
67.6701116251421,67.7476001531158,67.8250884660794,67.9025929340702,67.933907609277,
68.0114130956238,68.0889034409014,68.1663881412969,68.198801431243),
 .UNSPECIFIED.);
#2888=B_SPLINE_CURVE_WITH_KNOTS('',3,(#18858,#18859,#18860,#18861,#18862,
#18863,#18864,#18865,#18866,#18867,#18868,#18869,#18870,#18871,#18872,#18873,
#18874,#18875,#18876,#18877,#18878,#18879,#18880,#18881,#18882,#18883,#18884,
#18885,#18886,#18887,#18888,#18889,#18890,#18891,#18892,#18893,#18894,#18895,
#18896,#18897,#18898,#18899,#18900,#18901,#18902,#18903,#18904,#18905,#18906,
#18907,#18908,#18909,#18910,#18911,#18912,#18913,#18914,#18915,#18916,#18917,
#18918,#18919,#18920,#18921,#18922,#18923,#18924,#18925,#18926,#18927,#18928,
#18929,#18930,#18931,#18932,#18933,#18934,#18935,#18936,#18937,#18938,#18939,
#18940,#18941,#18942,#18943,#18944,#18945,#18946,#18947,#18948,#18949,#18950,
#18951,#18952,#18953,#18954),.UNSPECIFIED.,.F.,.F.,(4,3,3,3,3,3,3,3,3,3,
3,3,3,3,3,3,3,3,3,3,3,3,3,3,3,3,3,3,3,3,3,3,4),(65.9734457253856,66.0113843620875,
66.0888893919113,66.1663803299744,66.2438627124269,66.3213512404007,66.3988395533646,
66.4763440213554,66.5076586965613,66.5851637263852,66.6626546644483,66.7401370469007,
66.8176255748745,66.8951138878385,66.9726183558293,67.0039330310351,67.0814380608589,
67.1589289989221,67.2364113813744,67.3138999093482,67.3913882223121,67.4688926903028,
67.5002073655089,67.5777123953327,67.6552033333958,67.7326857158482,67.810174243822,
67.8876625567858,67.9651670247766,67.9964816999827,68.0739860168883,68.1514785081145,
68.198812002236),.UNSPECIFIED.);
#2889=B_SPLINE_CURVE_WITH_KNOTS('',3,(#18955,#18956,#18957,#18958,#18959,
#18960,#18961,#18962,#18963,#18964,#18965,#18966),.UNSPECIFIED.,.F.,.F.,
(4,1,1,1,1,1,1,1,1,4),(61.915593798429,62.0411896862971,62.5374640207709,
63.0337383552447,63.5300126897185,64.0262870241923,64.5225613586661,65.0188356931399,
65.5151100276137,65.973445690953),.UNSPECIFIED.);
#2890=B_SPLINE_CURVE_WITH_KNOTS('',3,(#18972,#18973,#18974,#18975,#18976,
#18977,#18978,#18979,#18980,#18981,#18982,#18983,#18984,#18985,#18986,#18987,
#18988,#18989,#18990,#18991,#18992,#18993,#18994,#18995,#18996,#18997,#18998,
#18999,#19000,#19001,#19002,#19003,#19004,#19005,#19006,#19007,#19008,#19009,
#19010,#19011,#19012,#19013,#19014,#19015,#19016,#19017,#19018,#19019,#19020,
#19021,#19022,#19023,#19024,#19025,#19026,#19027,#19028,#19029,#19030,#19031,
#19032,#19033,#19034,#19035,#19036,#19037,#19038,#19039,#19040,#19041,#19042,
#19043,#19044,#19045,#19046,#19047,#19048,#19049,#19050,#19051,#19052,#19053,
#19054,#19055,#19056,#19057,#19058,#19059,#19060,#19061,#19062,#19063,#19064,
#19065,#19066,#19067,#19068,#19069,#19070,#19071,#19072,#19073,#19074,#19075,
#19076,#19077,#19078,#19079,#19080,#19081,#19082,#19083,#19084,#19085,#19086,
#19087,#19088,#19089,#19090,#19091,#19092,#19093,#19094,#19095,#19096,#19097,
#19098,#19099,#19100,#19101,#19102,#19103,#19104,#19105,#19106,#19107,#19108,
#19109,#19110,#19111,#19112,#19113,#19114,#19115,#19116,#19117,#19118,#19119,
#19120,#19121,#19122,#19123,#19124,#19125,#19126,#19127,#19128,#19129,#19130,
#19131,#19132,#19133,#19134,#19135,#19136,#19137,#19138,#19139,#19140,#19141,
#19142,#19143),.UNSPECIFIED.,.F.,.F.,(4,3,3,3,3,3,3,3,3,3,3,3,3,3,3,3,3,
3,3,3,3,3,3,3,3,3,3,3,3,3,3,3,3,3,3,3,3,3,3,3,3,3,3,3,3,3,3,3,3,3,3,3,3,
3,3,3,3,4),(55.6324502817996,55.7099375026088,55.7882840224331,55.8657718222351,
55.9445477020706,56.023323581906,56.1008286117298,56.1783195497928,56.2558019322451,
56.3332904602189,56.4107787731827,56.4882832411734,56.5195979163798,56.5971029462036,
56.6745938842667,56.752076266719,56.8295647946928,56.9070531076567,56.9845575756474,
57.0158722508535,57.0933772806773,57.1708682187403,57.2483506011926,57.3258391291664,
57.4033274421302,57.4808319101209,57.5121465853273,57.5896516151511,57.6671425532142,
57.7446249356666,57.8221134636404,57.8996017766043,57.9771062445951,58.0084209198011,
58.0859259496249,58.1634168876881,58.2408992701405,58.3183877981143,58.3958761110781,
58.4733805790688,58.5046952542749,58.5822002840987,58.6596912221618,58.7371736046139,
58.8146621325877,58.8921504455517,58.9696549135425,59.0009695887487,59.0784746185724,
59.1559655566355,59.2334479390883,59.3109364670621,59.3884247800259,59.4659292480167,
59.4972439232225,59.5767649286567,59.6562642201875,59.6902604181339),
 .UNSPECIFIED.);
#2891=B_SPLINE_CURVE_WITH_KNOTS('',3,(#19144,#19145,#19146,#19147,#19148,
#19149,#19150,#19151,#19152,#19153,#19154,#19155,#19156,#19157,#19158,#19159,
#19160,#19161,#19162,#19163,#19164,#19165,#19166,#19167,#19168,#19169,#19170,
#19171,#19172,#19173,#19174,#19175,#19176,#19177,#19178,#19179,#19180,#19181,
#19182,#19183,#19184,#19185,#19186,#19187,#19188,#19189,#19190,#19191,#19192,
#19193,#19194,#19195,#19196,#19197,#19198,#19199,#19200,#19201,#19202,#19203,
#19204,#19205,#19206,#19207,#19208,#19209,#19210,#19211,#19212,#19213,#19214,
#19215,#19216,#19217,#19218,#19219,#19220,#19221,#19222,#19223,#19224,#19225,
#19226,#19227,#19228,#19229,#19230,#19231,#19232,#19233,#19234,#19235,#19236,
#19237),.UNSPECIFIED.,.F.,.F.,(4,3,3,3,3,3,3,3,3,3,3,3,3,3,3,3,3,3,3,3,
3,3,3,3,3,3,3,3,3,3,3,4),(59.690260418206,59.7679892440258,59.8457171883824,
59.9234656380215,59.9935182576963,60.0710232875201,60.1485142255832,60.2259966080357,
60.3034851360095,60.3809734489736,60.4584779169643,60.4897925921701,60.5672976219939,
60.6447885600572,60.7222709425095,60.7997594704833,60.8772477834472,60.954752251438,
60.9860669266439,61.0635719564677,61.1410628945307,61.2185452769831,61.296033804957,
61.3735221179207,61.4510265859116,61.4823412611177,61.5598457164873,61.6373358615963,
61.714824493991,61.7923078312911,61.8698020429645,61.9156047763896),
 .UNSPECIFIED.);
#2892=B_SPLINE_CURVE_WITH_KNOTS('',3,(#19239,#19240,#19241,#19242,#19243,
#19244,#19245,#19246),.UNSPECIFIED.,.F.,.F.,(4,1,1,1,1,4),(59.690260418206,
60.056092348402,60.5523666828758,61.0486410173496,61.5449153518233,61.915593798429),
 .UNSPECIFIED.);
#2893=B_SPLINE_CURVE_WITH_KNOTS('',3,(#19247,#19248,#19249,#19250,#19251,
#19252,#19253,#19254,#19255,#19256,#19257,#19258,#19259,#19260,#19261,#19262,
#19263,#19264,#19265,#19266,#19267,#19268,#19269,#19270,#19271,#19272,#19273,
#19274,#19275,#19276,#19277,#19278,#19279,#19280,#19281,#19282,#19283,#19284,
#19285,#19286,#19287,#19288,#19289,#19290,#19291,#19292,#19293,#19294,#19295,
#19296,#19297,#19298,#19299,#19300,#19301,#19302,#19303,#19304,#19305,#19306,
#19307,#19308,#19309,#19310,#19311,#19312,#19313,#19314,#19315,#19316,#19317,
#19318,#19319,#19320,#19321,#19322,#19323,#19324,#19325,#19326,#19327,#19328,
#19329,#19330,#19331,#19332,#19333,#19334,#19335,#19336,#19337,#19338,#19339,
#19340,#19341,#19342,#19343,#19344,#19345,#19346,#19347,#19348,#19349,#19350,
#19351,#19352,#19353,#19354,#19355,#19356,#19357,#19358,#19359,#19360,#19361,
#19362,#19363,#19364,#19365,#19366,#19367,#19368,#19369,#19370,#19371,#19372,
#19373,#19374,#19375,#19376,#19377,#19378,#19379,#19380,#19381,#19382,#19383,
#19384,#19385,#19386,#19387,#19388,#19389,#19390,#19391,#19392,#19393,#19394,
#19395,#19396,#19397,#19398,#19399,#19400,#19401,#19402,#19403,#19404,#19405,
#19406,#19407,#19408,#19409,#19410,#19411,#19412,#19413,#19414,#19415,#19416,
#19417,#19418),.UNSPECIFIED.,.F.,.F.,(4,3,3,3,3,3,3,3,3,3,3,3,3,3,3,3,3,
3,3,3,3,3,3,3,3,3,3,3,3,3,3,3,3,3,3,3,3,3,3,3,3,3,3,3,3,3,3,3,3,3,3,3,3,
3,3,3,3,4),(55.6324449452842,55.7099415050222,55.7874270322703,55.8649174558887,
55.9424051781908,56.0199114266392,56.0858976726116,56.1634027024354,56.2408936404985,
56.3183760229507,56.3958645509246,56.4733528638884,56.5508573318792,56.5821720070854,
56.6596770369092,56.7371679749723,56.8146503574246,56.8921388853984,56.9696271983623,
57.0471316663531,57.0784463415592,57.155951371383,57.2334423094461,57.3109246918983,
57.3884132198722,57.465901532836,57.5434060008268,57.574720676033,57.6522257058568,
57.7297166439199,57.8071990263723,57.8846875543461,57.96217586731,58.0396803353008,
58.0709950105068,58.1485000403306,58.2259909783937,58.3034733608458,58.3809618888196,
58.4584502017835,58.5359546697743,58.5672693449806,58.6447743748043,58.7222653128674,
58.7997476953199,58.8772362232938,58.9547245362576,59.0322290042483,59.0635436794544,
59.1410487092782,59.2185396473415,59.2960220297936,59.3735105577675,59.4509988707312,
59.528503338722,59.5598180139282,59.6410306749168,59.6902604165018),
 .UNSPECIFIED.);
#2894=B_SPLINE_CURVE_WITH_KNOTS('',3,(#19424,#19425,#19426,#19427,#19428,
#19429,#19430,#19431,#19432,#19433,#19434,#19435),.UNSPECIFIED.,.F.,.F.,
(4,1,1,1,1,1,1,1,1,4),(49.3492407452519,49.5717572337466,50.0680315682204,
50.5643059026942,51.060580237168,51.5568545716418,52.0531289061156,52.5494032405894,
53.0456775750632,53.4070751110264),.UNSPECIFIED.);
#2895=B_SPLINE_CURVE_WITH_KNOTS('',3,(#19436,#19437,#19438,#19439,#19440,
#19441,#19442,#19443,#19444,#19445,#19446,#19447,#19448,#19449,#19450,#19451,
#19452,#19453,#19454,#19455,#19456,#19457,#19458,#19459,#19460,#19461,#19462,
#19463,#19464,#19465,#19466,#19467,#19468,#19469,#19470,#19471,#19472,#19473,
#19474,#19475,#19476,#19477,#19478,#19479,#19480,#19481,#19482,#19483,#19484,
#19485,#19486,#19487,#19488,#19489,#19490,#19491,#19492,#19493,#19494,#19495,
#19496,#19497,#19498,#19499,#19500,#19501,#19502,#19503,#19504,#19505,#19506,
#19507,#19508,#19509,#19510,#19511,#19512,#19513,#19514,#19515,#19516,#19517,
#19518,#19519,#19520,#19521,#19522,#19523,#19524,#19525,#19526,#19527,#19528,
#19529,#19530,#19531,#19532),.UNSPECIFIED.,.F.,.F.,(4,3,3,3,3,3,3,3,3,3,
3,3,3,3,3,3,3,3,3,3,3,3,3,3,3,3,3,3,3,3,3,3,4),(53.40707511313,53.488147551321,
53.541951909537,53.6194569393608,53.6969478774239,53.7744302598764,53.8519187878503,
53.929407100814,54.0069115688048,54.0382262440108,54.1157312738346,54.1932222118976,
54.2707045943503,54.348193122324,54.425681435288,54.5031859032787,54.5345005784846,
54.6120056083084,54.6894965463715,54.7669789288238,54.8444674567977,54.9219557697616,
54.9994602377522,55.0307749129584,55.1082799427822,55.1857708808453,55.2632532632976,
55.3407417912714,55.4182301042351,55.4957345722259,55.5270492474322,55.6045536371399,
55.6324502817996),.UNSPECIFIED.);
#2896=B_SPLINE_CURVE_WITH_KNOTS('',3,(#19534,#19535,#19536,#19537,#19538,
#19539,#19540,#19541,#19542,#19543,#19544,#19545,#19546,#19547,#19548,#19549,
#19550,#19551,#19552,#19553,#19554,#19555,#19556,#19557,#19558,#19559,#19560,
#19561,#19562,#19563,#19564,#19565,#19566,#19567,#19568,#19569,#19570,#19571,
#19572,#19573,#19574,#19575,#19576,#19577,#19578,#19579,#19580,#19581,#19582,
#19583,#19584,#19585,#19586,#19587,#19588,#19589,#19590,#19591,#19592,#19593,
#19594,#19595,#19596,#19597,#19598,#19599,#19600,#19601,#19602,#19603,#19604,
#19605,#19606,#19607,#19608,#19609,#19610,#19611,#19612,#19613,#19614,#19615,
#19616,#19617,#19618,#19619,#19620,#19621,#19622,#19623,#19624,#19625,#19626,
#19627,#19628,#19629,#19630),.UNSPECIFIED.,.F.,.F.,(4,3,3,3,3,3,3,3,3,3,
3,3,3,3,3,3,3,3,3,3,3,3,3,3,3,3,3,3,3,3,3,3,4),(53.4070751110957,53.4864712424076,
53.5658927786533,53.6045260002426,53.6820310300664,53.7595219681295,53.8370043505816,
53.9144928785553,53.9919811915191,54.0694856595099,54.1008003347164,54.1783053645402,
54.2557963026032,54.3332786850558,54.4107672130297,54.4882555259938,54.5657599939845,
54.5970746691902,54.6745796990139,54.7520706370771,54.8295530195294,54.9070415475032,
54.9845298604671,55.0620343284579,55.093349003664,55.1708540334878,55.2483449715509,
55.3258273540031,55.403315881977,55.4808041949409,55.5583086629317,55.5896233381378,
55.6324449452842),.UNSPECIFIED.);
#2897=B_SPLINE_CURVE_WITH_KNOTS('',3,(#19631,#19632,#19633,#19634,#19635,
#19636,#19637,#19638,#19639,#19640,#19641,#19642,#19643,#19644,#19645,#19646,
#19647,#19648,#19649,#19650,#19651,#19652,#19653,#19654,#19655,#19656,#19657,
#19658,#19659,#19660,#19661,#19662,#19663,#19664,#19665,#19666,#19667,#19668,
#19669,#19670,#19671,#19672,#19673,#19674,#19675,#19676,#19677,#19678,#19679,
#19680,#19681,#19682,#19683,#19684,#19685,#19686,#19687,#19688,#19689,#19690,
#19691,#19692,#19693,#19694,#19695,#19696,#19697,#19698,#19699,#19700,#19701,
#19702,#19703,#19704,#19705,#19706,#19707,#19708,#19709,#19710,#19711,#19712,
#19713,#19714,#19715,#19716,#19717,#19718,#19719,#19720,#19721,#19722,#19723,
#19724,#19725,#19726,#19727,#19728,#19729,#19730,#19731,#19732,#19733,#19734,
#19735,#19736,#19737,#19738,#19739,#19740,#19741,#19742,#19743,#19744,#19745,
#19746,#19747,#19748,#19749,#19750,#19751,#19752,#19753,#19754,#19755,#19756,
#19757,#19758,#19759,#19760,#19761,#19762,#19763,#19764,#19765,#19766,#19767,
#19768,#19769,#19770,#19771,#19772,#19773,#19774,#19775,#19776,#19777,#19778,
#19779,#19780,#19781,#19782,#19783,#19784,#19785,#19786,#19787,#19788,#19789,
#19790,#19791,#19792,#19793,#19794,#19795,#19796,#19797,#19798,#19799,#19800,
#19801,#19802),.UNSPECIFIED.,.F.,.F.,(4,3,3,3,3,3,3,3,3,3,3,3,3,3,3,3,3,
3,3,3,3,3,3,3,3,3,3,3,3,3,3,3,3,3,3,3,3,3,3,3,3,3,3,3,3,3,3,3,3,3,3,3,3,
3,3,3,3,4),(49.3492546709687,49.4267442304708,49.5042320490615,49.581737396915,
49.6343313244523,49.7118363542761,49.7893272923391,49.8668096747915,49.9442982027653,
50.0217865157291,50.0992909837199,50.1306056589261,50.2081106887499,50.285601626813,
50.3630840092653,50.4405725372391,50.5180608502029,50.5955653181937,50.6268799933999,
50.7043850232237,50.7818759612868,50.8593583437391,50.9368468717129,51.0143351846768,
51.0918396526675,51.1231543278737,51.2006593576975,51.2781502957606,51.3556326782129,
51.4331212061867,51.5106095191505,51.5881139871414,51.6194286623475,51.6969336921713,
51.7744246302345,51.8519070126868,51.9293955406606,52.0068838536244,52.0843883216152,
52.1157029968213,52.1932080266451,52.2706989647081,52.3481813471605,52.4256698751343,
52.5031581880983,52.580662656089,52.6119773312951,52.6894823611189,52.7669732991819,
52.8444556816342,52.9219442096081,52.9994325225718,53.0769369905626,53.1082516657688,
53.1860463074653,53.2638247514645,53.3415977600619,53.4070751110264),
 .UNSPECIFIED.);
#2898=B_SPLINE_CURVE_WITH_KNOTS('',3,(#19808,#19809,#19810,#19811,#19812,
#19813,#19814,#19815,#19816,#19817,#19818,#19819,#19820,#19821,#19822,#19823,
#19824,#19825,#19826,#19827,#19828,#19829,#19830,#19831,#19832,#19833,#19834,
#19835,#19836,#19837,#19838,#19839,#19840,#19841,#19842,#19843,#19844,#19845,
#19846,#19847,#19848,#19849,#19850,#19851,#19852,#19853,#19854,#19855,#19856,
#19857,#19858,#19859,#19860,#19861,#19862,#19863,#19864,#19865,#19866,#19867,
#19868,#19869,#19870,#19871,#19872,#19873,#19874,#19875,#19876,#19877,#19878,
#19879,#19880,#19881,#19882,#19883,#19884,#19885,#19886,#19887,#19888,#19889,
#19890,#19891,#19892,#19893,#19894,#19895,#19896,#19897,#19898,#19899,#19900,
#19901,#19902,#19903,#19904,#19905,#19906,#19907,#19908,#19909,#19910,#19911,
#19912,#19913,#19914,#19915,#19916,#19917,#19918,#19919,#19920,#19921,#19922,
#19923,#19924,#19925,#19926,#19927,#19928,#19929,#19930,#19931,#19932,#19933,
#19934,#19935,#19936,#19937,#19938,#19939,#19940,#19941,#19942,#19943,#19944,
#19945,#19946,#19947,#19948,#19949,#19950,#19951,#19952,#19953,#19954,#19955,
#19956,#19957,#19958,#19959,#19960,#19961,#19962,#19963,#19964,#19965,#19966,
#19967,#19968,#19969,#19970,#19971,#19972,#19973,#19974,#19975,#19976,#19977,
#19978,#19979,#19980,#19981,#19982),.UNSPECIFIED.,.F.,.F.,(4,3,3,3,3,3,
3,3,3,3,3,3,3,3,3,3,3,3,3,3,3,3,3,3,3,3,3,3,3,3,3,3,3,3,3,3,3,3,3,3,3,3,
3,3,3,3,3,3,3,3,3,3,3,3,3,3,3,3,4),(43.0660500108131,43.1201908855873,43.1976959154111,
43.2751868534745,43.3526692359268,43.4301577639007,43.5076460768648,43.5851505448554,
43.6164652200611,43.6939702498849,43.7714611879481,43.8489435704003,43.9264320983741,
44.0039204113377,44.0814248793284,44.1127395545349,44.1902445843586,44.2677355224217,
44.3452179048738,44.4227064328476,44.5001947458119,44.5776992138026,44.6090138890087,
44.6865189188325,44.7640098568957,44.841492239348,44.9189807673218,44.9964690802853,
45.0739735482761,45.1052882234825,45.1827932533063,45.2602841913696,45.337766573823,
45.4152551017967,45.4927434147604,45.5702478827512,45.6015625579563,45.6790675877801,
45.7565585258428,45.8340409082948,45.9115294362686,45.9890177492321,46.0665222172227,
46.0978368924301,46.175341922254,46.252832860317,46.3303152427694,46.4078037707431,
46.4852920837064,46.5627965516972,46.5941112269039,46.6716162567278,46.7491071947912,
46.8265895772435,46.9040781052176,46.9815664181814,47.0590708861724,47.0903855613777,
47.1238898038468),.UNSPECIFIED.);
#2899=B_SPLINE_CURVE_WITH_KNOTS('',3,(#19983,#19984,#19985,#19986,#19987,
#19988,#19989,#19990),.UNSPECIFIED.,.F.,.F.,(4,1,1,1,1,4),(47.1238898363668,
47.5866598958514,48.0829342303252,48.579208564799,49.0754828992728,49.3492407452519),
 .UNSPECIFIED.);
#2900=B_SPLINE_CURVE_WITH_KNOTS('',3,(#19992,#19993,#19994,#19995,#19996,
#19997,#19998,#19999,#20000,#20001,#20002,#20003,#20004,#20005,#20006,#20007,
#20008,#20009,#20010,#20011,#20012,#20013,#20014,#20015,#20016,#20017,#20018,
#20019,#20020,#20021,#20022,#20023,#20024,#20025,#20026,#20027,#20028,#20029,
#20030,#20031,#20032,#20033,#20034,#20035,#20036,#20037,#20038,#20039,#20040,
#20041,#20042,#20043,#20044,#20045,#20046,#20047,#20048,#20049,#20050,#20051,
#20052,#20053,#20054,#20055,#20056,#20057,#20058,#20059,#20060,#20061,#20062,
#20063,#20064,#20065,#20066,#20067,#20068,#20069,#20070,#20071,#20072,#20073,
#20074,#20075,#20076,#20077,#20078,#20079,#20080,#20081,#20082,#20083,#20084,
#20085,#20086,#20087,#20088),.UNSPECIFIED.,.F.,.F.,(4,3,3,3,3,3,3,3,3,3,
3,3,3,3,3,3,3,3,3,3,3,3,3,3,3,3,3,3,3,3,3,3,4),(47.1238898038468,47.1529596520833,
47.2304646819071,47.3079556199699,47.3854380024221,47.462926530396,47.5404148433597,
47.6179193113505,47.6492339865571,47.7267390163809,47.8042299544441,47.8817123368962,
47.95920086487,48.0366891778341,48.1141936458248,48.1455083210309,48.2230133508547,
48.3005042889178,48.3779866713703,48.4554751993441,48.5329635123081,48.6104679802988,
48.6417826555047,48.7192876853285,48.7967786233916,48.8742610058439,48.9517495338177,
49.0292378467816,49.1067423147723,49.1380569899785,49.2155613837407,49.2930547509972,
49.3492546709687),.UNSPECIFIED.);
#2901=B_SPLINE_CURVE_WITH_KNOTS('',3,(#20089,#20090,#20091,#20092,#20093,
#20094,#20095,#20096,#20097,#20098,#20099,#20100),.UNSPECIFIED.,.F.,.F.,
(4,1,1,1,1,1,1,1,1,4),(43.0660378051096,43.1827649762929,43.6790393107667,
44.1753136452405,44.6715879797143,45.1678623141881,45.6641366486619,46.1604109831357,
46.6566853176095,47.1238897738335),.UNSPECIFIED.);
#2902=B_SPLINE_CURVE_WITH_KNOTS('',3,(#20106,#20107,#20108,#20109,#20110,
#20111,#20112,#20113,#20114,#20115,#20116,#20117),.UNSPECIFIED.,.F.,.F.,
(4,1,1,1,1,1,1,1,1,4),(36.7829030456445,37.1648988719018,37.6611732063756,
38.1574475408493,38.6537218753231,39.1499962097969,39.6462705442707,40.1425448787445,
40.6388192132183,40.8407044662609),.UNSPECIFIED.);
#2903=B_SPLINE_CURVE_WITH_KNOTS('',3,(#20118,#20119,#20120,#20121,#20122,
#20123,#20124,#20125,#20126,#20127,#20128,#20129,#20130,#20131,#20132,#20133,
#20134,#20135,#20136,#20137,#20138,#20139,#20140,#20141,#20142,#20143,#20144,
#20145,#20146,#20147,#20148,#20149,#20150,#20151,#20152,#20153,#20154,#20155,
#20156,#20157,#20158,#20159,#20160,#20161,#20162,#20163,#20164,#20165,#20166,
#20167,#20168,#20169,#20170,#20171,#20172,#20173,#20174,#20175,#20176,#20177,
#20178,#20179,#20180,#20181,#20182,#20183,#20184,#20185,#20186,#20187,#20188,
#20189,#20190,#20191,#20192,#20193,#20194,#20195,#20196,#20197,#20198,#20199,
#20200,#20201,#20202,#20203,#20204,#20205,#20206,#20207,#20208,#20209,#20210,
#20211),.UNSPECIFIED.,.F.,.F.,(4,3,3,3,3,3,3,3,3,3,3,3,3,3,3,3,3,3,3,3,
3,3,3,3,3,3,3,3,3,3,3,4),(40.8407044966673,40.9185261972124,40.9963482049705,
41.0741901903445,41.1350935476921,41.212598577516,41.2900895155792,41.3675718980314,
41.4450604260052,41.5225487389693,41.6000532069602,41.6313678821659,41.7088729119896,
41.7863638500527,41.8638462325043,41.9413347604782,42.0188230734419,42.0963275414328,
42.1276422166397,42.2051472464636,42.2826381845264,42.3601205669791,42.4376090949529,
42.5150974079168,42.5926018759076,42.6239165511135,42.701421064934,42.7789112992601,
42.8564006396014,42.9338846178947,43.0113808235583,43.0660500108131),
 .UNSPECIFIED.);
#2904=B_SPLINE_CURVE_WITH_KNOTS('',3,(#20213,#20214,#20215,#20216,#20217,
#20218,#20219,#20220),.UNSPECIFIED.,.F.,.F.,(4,1,1,1,1,4),(40.8407044966673,
41.1976676383978,41.6939419728716,42.1902163073454,42.6864906418191,43.0660378051096),
 .UNSPECIFIED.);
#2905=B_SPLINE_CURVE_WITH_KNOTS('',3,(#20221,#20222,#20223,#20224,#20225,
#20226,#20227,#20228,#20229,#20230,#20231,#20232,#20233,#20234,#20235,#20236,
#20237,#20238,#20239,#20240,#20241,#20242,#20243,#20244,#20245,#20246,#20247,
#20248,#20249,#20250,#20251,#20252,#20253,#20254,#20255,#20256,#20257,#20258,
#20259,#20260,#20261,#20262,#20263,#20264,#20265,#20266,#20267,#20268,#20269,
#20270,#20271,#20272,#20273,#20274,#20275,#20276,#20277,#20278,#20279,#20280,
#20281,#20282,#20283,#20284,#20285,#20286,#20287,#20288,#20289,#20290,#20291,
#20292,#20293,#20294,#20295,#20296,#20297,#20298,#20299,#20300,#20301,#20302,
#20303,#20304,#20305,#20306,#20307,#20308,#20309,#20310,#20311,#20312,#20313,
#20314,#20315,#20316,#20317,#20318,#20319,#20320,#20321,#20322,#20323,#20324,
#20325,#20326,#20327,#20328,#20329,#20330,#20331,#20332,#20333,#20334,#20335,
#20336,#20337,#20338,#20339,#20340,#20341,#20342,#20343,#20344,#20345,#20346,
#20347,#20348,#20349,#20350,#20351,#20352,#20353,#20354,#20355,#20356,#20357,
#20358,#20359,#20360,#20361,#20362,#20363,#20364,#20365,#20366,#20367,#20368,
#20369,#20370,#20371,#20372,#20373,#20374,#20375,#20376,#20377,#20378,#20379,
#20380,#20381,#20382,#20383,#20384,#20385,#20386,#20387,#20388,#20389,#20390,
#20391,#20392),.UNSPECIFIED.,.F.,.F.,(4,3,3,3,3,3,3,3,3,3,3,3,3,3,3,3,3,
3,3,3,3,3,3,3,3,3,3,3,3,3,3,3,3,3,3,3,3,3,3,3,3,3,3,3,3,3,3,3,3,3,3,3,3,
3,3,3,3,4),(36.7828905111531,36.8603855276508,36.9378701451936,37.0153599781323,
37.0928477456159,37.1703533678302,37.2274729626074,37.3049779924312,37.3824689304943,
37.4599513129466,37.5374398409205,37.6149281538843,37.6924326218751,37.7237472970812,
37.801252326905,37.8787432649681,37.9562256474204,38.0337141753942,38.111202488358,
38.1887069563488,38.220021631555,38.2975266613788,38.3750175994419,38.4524999818942,
38.529988509868,38.6074768228319,38.6849812908227,38.7162959660288,38.7938009958526,
38.8712919339157,38.9487743163681,39.0262628443419,39.1037511573058,39.1812556252966,
39.2125703005026,39.2900753303264,39.3675662683894,39.4450486508418,39.5225371788156,
39.6000254917794,39.6775299597702,39.7088446349764,39.7863496648002,39.8638406028632,
39.9413229853155,40.0188115132893,40.0962998262532,40.173804294244,40.2051189694502,
40.282623999274,40.3601149373372,40.4375973197892,40.5150858477629,40.592574160727,
40.6700786287177,40.701393303924,40.7823288599563,40.8407044942733),
 .UNSPECIFIED.);
#2906=B_SPLINE_CURVE_WITH_KNOTS('',3,(#20398,#20399,#20400,#20401,#20402,
#20403,#20404,#20405,#20406,#20407,#20408,#20409,#20410,#20411,#20412,#20413,
#20414,#20415,#20416,#20417,#20418,#20419,#20420,#20421,#20422,#20423,#20424,
#20425,#20426,#20427,#20428,#20429,#20430,#20431,#20432,#20433,#20434,#20435,
#20436,#20437,#20438,#20439,#20440,#20441,#20442,#20443,#20444,#20445,#20446,
#20447,#20448,#20449,#20450,#20451,#20452,#20453,#20454,#20455,#20456,#20457,
#20458,#20459,#20460,#20461,#20462,#20463,#20464,#20465,#20466,#20467,#20468,
#20469,#20470,#20471,#20472,#20473,#20474,#20475,#20476,#20477,#20478,#20479,
#20480,#20481,#20482,#20483,#20484,#20485,#20486,#20487,#20488,#20489,#20490,
#20491,#20492,#20493,#20494,#20495,#20496,#20497,#20498,#20499,#20500,#20501,
#20502,#20503,#20504,#20505,#20506,#20507,#20508,#20509,#20510,#20511,#20512,
#20513,#20514,#20515,#20516,#20517,#20518,#20519,#20520,#20521,#20522,#20523,
#20524,#20525,#20526,#20527,#20528,#20529,#20530,#20531,#20532,#20533,#20534,
#20535,#20536,#20537,#20538,#20539,#20540,#20541,#20542,#20543,#20544,#20545,
#20546,#20547,#20548,#20549,#20550,#20551,#20552,#20553,#20554,#20555,#20556,
#20557,#20558,#20559,#20560,#20561,#20562,#20563,#20564,#20565,#20566,#20567,
#20568,#20569),.UNSPECIFIED.,.F.,.F.,(4,3,3,3,3,3,3,3,3,3,3,3,3,3,3,3,3,
3,3,3,3,3,3,3,3,3,3,3,3,3,3,3,3,3,3,3,3,3,3,3,3,3,3,3,3,3,3,3,3,3,3,3,3,
3,3,3,3,4),(30.4996866134875,30.5771743679583,30.6546800900358,30.7133325237424,
30.7908375535663,30.8683284916292,30.9458108740808,31.0232994020546,31.1007877150188,
31.1782921830093,31.2096068582162,31.2871118880399,31.364602826103,31.4420852085554,
31.5195737365294,31.5970620494926,31.6745665174833,31.70588119269,31.7833862225136,
31.8608771605768,31.9383595430285,32.0158480710025,32.0933363839657,32.1708408519566,
32.2021555271638,32.2796605569876,32.3571514950511,32.4346338775035,32.5121224054774,
32.589610718441,32.6671151864316,32.6984298616376,32.7759348914614,32.8534258295247,
32.9309082119769,33.0083967399509,33.0858850529152,33.1633895209059,33.1947041961114,
33.2722092259351,33.3497001639985,33.4271825464495,33.5046710744235,33.5821593873876,
33.6596638553783,33.6909785305852,33.7684835604093,33.8459744984727,33.9234568809248,
34.0009454088985,34.078433721862,34.155938189853,34.187252865059,34.2645317736749,
34.341800711369,34.4190593754722,34.4963250242707,34.5575191894877),
 .UNSPECIFIED.);
#2907=B_SPLINE_CURVE_WITH_KNOTS('',3,(#20570,#20571,#20572,#20573,#20574,
#20575,#20576,#20577,#20578),.UNSPECIFIED.,.F.,.F.,(4,1,1,1,1,1,4),(34.5575191995802,
34.6835271995328,35.1798015340066,35.6760758684804,36.1723502029542,36.668624537428,
36.7829030456445),.UNSPECIFIED.);
#2908=B_SPLINE_CURVE_WITH_KNOTS('',3,(#20580,#20581,#20582,#20583,#20584,
#20585,#20586,#20587,#20588,#20589,#20590,#20591,#20592,#20593,#20594,#20595,
#20596,#20597,#20598,#20599,#20600,#20601,#20602,#20603,#20604,#20605,#20606,
#20607,#20608,#20609,#20610,#20611,#20612,#20613,#20614,#20615,#20616,#20617,
#20618,#20619,#20620,#20621,#20622,#20623,#20624,#20625,#20626,#20627,#20628,
#20629,#20630,#20631,#20632,#20633,#20634,#20635,#20636,#20637,#20638,#20639,
#20640,#20641,#20642,#20643,#20644,#20645,#20646,#20647,#20648,#20649,#20650,
#20651,#20652,#20653,#20654,#20655,#20656,#20657,#20658,#20659,#20660,#20661,
#20662,#20663,#20664,#20665,#20666,#20667,#20668,#20669,#20670,#20671,#20672,
#20673,#20674,#20675,#20676),.UNSPECIFIED.,.F.,.F.,(4,3,3,3,3,3,3,3,3,3,
3,3,3,3,3,3,3,3,3,3,3,3,3,3,3,3,3,3,3,3,3,3,4),(34.5575191941331,34.6371161377194,
34.7167383160435,34.7461012902384,34.8236063200621,34.9010972581253,34.9785796405779,
35.0560681685518,35.1335564815155,35.2110609495063,35.2423756247122,35.319880654536,
35.3973715925991,35.4748539750512,35.5523425030251,35.6298308159892,35.7073352839799,
35.738649959186,35.8161549890098,35.8936459270729,35.9711283095253,36.0486168374991,
36.1261051504629,36.2036096184536,36.2349242936598,36.3124293234836,36.3899202615467,
36.4674026439991,36.5448911719729,36.6223794849368,36.6998839529276,36.7311986281336,
36.7828905111531),.UNSPECIFIED.);
#2909=B_SPLINE_CURVE_WITH_KNOTS('',3,(#20677,#20678,#20679,#20680,#20681,
#20682,#20683,#20684,#20685,#20686,#20687,#20688),.UNSPECIFIED.,.F.,.F.,
(4,1,1,1,1,1,1,1,1,4),(30.4997008468882,30.7759066144481,31.2721809489219,
31.7684552833957,32.2647296178695,32.7610039523433,33.2572782868171,33.7535526212909,
34.2498269557646,34.5575191894877),.UNSPECIFIED.);
#2910=B_SPLINE_CURVE_WITH_KNOTS('',3,(#20694,#20695,#20696,#20697,#20698,
#20699,#20700,#20701,#20702,#20703,#20704,#20705,#20706),.UNSPECIFIED.,
 .F.,.F.,(4,1,1,1,1,1,1,1,1,1,4),(24.2164925491897,24.2617661755831,24.7580405100569,
25.2543148445307,25.7505891790045,26.2468635134783,26.7431378479521,27.2394121824259,
27.7356865168997,28.2319608513735,28.2743338823081),.UNSPECIFIED.);
#2911=B_SPLINE_CURVE_WITH_KNOTS('',3,(#20707,#20708,#20709,#20710,#20711,
#20712,#20713,#20714,#20715,#20716,#20717,#20718,#20719,#20720,#20721,#20722,
#20723,#20724,#20725,#20726,#20727,#20728,#20729,#20730,#20731,#20732,#20733,
#20734,#20735,#20736,#20737,#20738,#20739,#20740,#20741,#20742,#20743,#20744,
#20745,#20746,#20747,#20748,#20749,#20750,#20751,#20752,#20753,#20754,#20755,
#20756,#20757,#20758,#20759,#20760,#20761,#20762,#20763,#20764,#20765,#20766,
#20767,#20768,#20769,#20770,#20771,#20772,#20773,#20774,#20775,#20776,#20777,
#20778,#20779,#20780,#20781,#20782,#20783,#20784,#20785,#20786,#20787,#20788,
#20789,#20790,#20791,#20792,#20793,#20794,#20795,#20796,#20797,#20798,#20799,
#20800),.UNSPECIFIED.,.F.,.F.,(4,3,3,3,3,3,3,3,3,3,3,3,3,3,3,3,3,3,3,3,
3,3,3,3,3,3,3,3,3,3,3,4),(28.2743338823081,28.3516005304913,28.4288535310633,
28.5061092838686,28.5833615214816,28.6606328802227,28.7282351858473,28.805740215671,
28.8832311537342,28.9607135361864,29.0382020641603,29.1156903771241,29.1931948451148,
29.224509520321,29.3020145501449,29.379505488208,29.4569878706601,29.5344763986339,
29.6119647115976,29.6894691795883,29.7207838547948,29.7982888846186,29.8757798226816,
29.9532622051341,30.0307507331081,30.1082390460719,30.1857435140626,30.2170581892686,
30.2945642729969,30.3720550819576,30.4495420149547,30.4996866134875),
 .UNSPECIFIED.);
#2912=B_SPLINE_CURVE_WITH_KNOTS('',3,(#20802,#20803,#20804,#20805,#20806,
#20807,#20808,#20809,#20810),.UNSPECIFIED.,.F.,.F.,(4,1,1,1,1,1,4),(28.2743338823081,
28.2945349420791,28.7908092765529,29.2870836110267,29.7833579455005,30.2796322799743,
30.4997008468882),.UNSPECIFIED.);
#2913=B_SPLINE_CURVE_WITH_KNOTS('',3,(#20811,#20812,#20813,#20814,#20815,
#20816,#20817,#20818,#20819,#20820,#20821,#20822,#20823,#20824,#20825,#20826,
#20827,#20828,#20829,#20830,#20831,#20832,#20833,#20834,#20835,#20836,#20837,
#20838,#20839,#20840,#20841,#20842,#20843,#20844,#20845,#20846,#20847,#20848,
#20849,#20850,#20851,#20852,#20853,#20854,#20855,#20856,#20857,#20858,#20859,
#20860,#20861,#20862,#20863,#20864,#20865,#20866,#20867,#20868,#20869,#20870,
#20871,#20872,#20873,#20874,#20875,#20876,#20877,#20878,#20879,#20880,#20881,
#20882,#20883,#20884,#20885,#20886,#20887,#20888,#20889,#20890,#20891,#20892,
#20893,#20894,#20895,#20896,#20897,#20898,#20899,#20900,#20901,#20902,#20903,
#20904,#20905,#20906,#20907,#20908,#20909,#20910,#20911,#20912,#20913,#20914,
#20915,#20916,#20917,#20918,#20919,#20920,#20921,#20922,#20923,#20924,#20925,
#20926,#20927,#20928,#20929,#20930,#20931,#20932,#20933,#20934,#20935,#20936,
#20937,#20938,#20939,#20940,#20941,#20942,#20943,#20944,#20945,#20946,#20947,
#20948,#20949,#20950,#20951,#20952,#20953,#20954,#20955,#20956,#20957,#20958,
#20959,#20960,#20961,#20962,#20963,#20964,#20965,#20966,#20967,#20968,#20969,
#20970,#20971,#20972,#20973,#20974,#20975,#20976,#20977,#20978,#20979,#20980,
#20981,#20982,#20983,#20984,#20985),.UNSPECIFIED.,.F.,.F.,(4,3,3,3,3,3,
3,3,3,3,3,3,3,3,3,3,3,3,3,3,3,3,3,3,3,3,3,3,3,3,3,3,3,3,3,3,3,3,3,3,3,3,
3,3,3,3,3,3,3,3,3,3,3,3,3,3,3,3,4),(24.2164906146016,24.293995059513,24.3243402662887,
24.4018452953929,24.4793362327265,24.5568186144429,24.6343071416759,24.7117954538968,
24.7892999211475,24.8206146007625,24.8981196310086,24.9756105694992,25.0530929523823,
25.1305814807896,25.2080697941879,25.285574262611,25.3168889352363,25.3943939648685,
25.4718849027378,25.5493672849951,25.6268558127727,25.7043441255404,25.7818485933357,
25.8131632697101,25.8906682995953,25.9681592377207,26.0456416202358,26.1231301482722,
26.2006184612982,26.2781229293511,26.3094376041839,26.3869426340027,26.4644335720607,
26.5419159545076,26.6194044824769,26.6968927954367,26.7743972634227,26.8057119386577,
26.8832169684698,26.9607079065205,27.0381902889601,27.1156788169219,27.1931671298729,
27.2706715978511,27.3019862731315,27.3794913029673,27.4569822410422,27.5344646235078,
27.6119531514941,27.6894414644704,27.7669459324735,27.7982606076053,27.8756329726693,
27.952990826376,28.033326590359,28.1106815343842,28.1880375066588,28.2654085791595,
28.2743338823081),.UNSPECIFIED.);
#2914=B_SPLINE_CURVE_WITH_KNOTS('',3,(#20991,#20992,#20993,#20994,#20995,
#20996,#20997,#20998,#20999),.UNSPECIFIED.,.F.,.F.,(4,1,1,1,1,1,4),(15.7079632679489,
15.8876765802342,16.383950914708,16.8802252491818,17.3764995836556,17.8727739181294,
17.9333400728794),.UNSPECIFIED.);
#2915=B_SPLINE_CURVE_WITH_KNOTS('',3,(#21001,#21002,#21003,#21004,#21005,
#21006),.UNSPECIFIED.,.F.,.F.,(4,1,1,4),(14.3988535768129,14.8951279112866,
15.3914022457604,15.7079632679489),.UNSPECIFIED.);
#2916=B_SPLINE_CURVE_WITH_KNOTS('',3,(#21010,#21011,#21012,#21013,#21014,
#21015,#21016,#21017,#21018,#21019,#21020,#21021,#21022,#21023,#21024,#21025,
#21026,#21027,#21028,#21029,#21030,#21031,#21032,#21033,#21034,#21035,#21036,
#21037,#21038,#21039,#21040,#21041,#21042,#21043,#21044,#21045,#21046,#21047,
#21048,#21049,#21050,#21051,#21052,#21053,#21054,#21055,#21056,#21057,#21058,
#21059,#21060,#21061,#21062,#21063,#21064,#21065,#21066,#21067,#21068,#21069,
#21070,#21071,#21072,#21073,#21074,#21075,#21076,#21077,#21078,#21079,#21080,
#21081,#21082,#21083,#21084,#21085),.UNSPECIFIED.,.F.,.F.,(4,3,3,3,3,3,
3,3,3,3,3,3,3,3,3,3,3,3,3,3,3,3,3,3,3,4),(13.8754803054952,13.9527915991825,
14.0300891179163,14.1073893679387,14.1846856665792,14.2620014441097,14.3362794861072,
14.4137829478898,14.4912723246912,14.5687531577414,14.6462401656036,14.7237269782611,
14.801229985091,14.832553820581,14.9100553301433,14.987542692496,15.0650214555568,
15.142506326132,15.2199909664686,15.2974917626711,15.3288281550548,15.4060793552377,
15.4833212986073,15.5605530255635,15.6377935536614,15.7079632679489),
 .UNSPECIFIED.);
#2917=B_SPLINE_CURVE_WITH_KNOTS('',3,(#21086,#21087,#21088,#21089,#21090,
#21091,#21092,#21093,#21094,#21095,#21096,#21097,#21098,#21099,#21100,#21101,
#21102,#21103,#21104,#21105,#21106,#21107,#21108,#21109,#21110,#21111,#21112,
#21113,#21114,#21115,#21116,#21117,#21118,#21119,#21120,#21121,#21122,#21123,
#21124,#21125,#21126,#21127,#21128,#21129,#21130,#21131,#21132,#21133,#21134,
#21135,#21136,#21137,#21138,#21139,#21140,#21141,#21142,#21143,#21144,#21145,
#21146,#21147,#21148,#21149,#21150,#21151,#21152,#21153,#21154,#21155,#21156,
#21157,#21158,#21159,#21160,#21161,#21162,#21163,#21164,#21165,#21166,#21167,
#21168,#21169,#21170,#21171,#21172,#21173,#21174,#21175,#21176,#21177,#21178,
#21179,#21180,#21181,#21182),.UNSPECIFIED.,.F.,.F.,(4,3,3,3,3,3,3,3,3,3,
3,3,3,3,3,3,3,3,3,3,3,3,3,3,3,3,3,3,3,3,3,3,4),(15.7079632680288,15.7896238438224,
15.8251024895286,15.9026051904092,15.9800937703955,16.0575737733851,16.1350599078411,
16.2125458235925,16.2900479042311,16.3213768240024,16.3988830078092,16.4763751134108,
16.5538586731209,16.6313483840178,16.7088378809863,16.7863435270014,16.8176511584762,
16.895155760811,16.9726462668389,17.0501282141283,17.1276163055372,17.2051041819359,
17.2826082161604,17.31392549295,17.3914306039829,17.4689216237793,17.5464040882215,
17.6238926979533,17.7013810923885,17.7788856409009,17.8101998274238,17.8877048528018,
17.9333380487234),.UNSPECIFIED.);
#2918=B_SPLINE_CURVE_WITH_KNOTS('',3,(#21188,#21189,#21190,#21191,#21192,
#21193,#21194,#21195),.UNSPECIFIED.,.F.,.F.,(4,2,2,4),(-0.24984933934325,
-0.173343887030935,-0.120986450366014,-5.83022767437317E-5),
 .UNSPECIFIED.);
#2919=B_SPLINE_CURVE_WITH_KNOTS('',3,(#21198,#21199,#21200,#21201,#21202,
#21203,#21204,#21205,#21206,#21207,#21208,#21209,#21210,#21211,#21212,#21213,
#21214,#21215,#21216,#21217,#21218,#21219,#21220,#21221,#21222,#21223,#21224,
#21225,#21226,#21227,#21228,#21229,#21230,#21231,#21232,#21233,#21234,#21235,
#21236,#21237,#21238,#21239,#21240,#21241,#21242,#21243,#21244,#21245,#21246,
#21247,#21248,#21249,#21250,#21251,#21252,#21253,#21254,#21255,#21256,#21257,
#21258,#21259,#21260,#21261,#21262,#21263,#21264,#21265,#21266,#21267,#21268,
#21269,#21270,#21271,#21272,#21273,#21274,#21275,#21276,#21277,#21278,#21279,
#21280,#21281,#21282,#21283,#21284,#21285),.UNSPECIFIED.,.F.,.F.,(4,3,3,
3,3,3,3,3,3,3,3,3,3,3,3,3,3,3,3,3,3,3,3,3,3,3,3,3,3,4),(-75.398223608073,
-75.318009037967,-75.2378091726219,-75.1576065863558,-75.0774076436808,
-74.9971894012001,-74.937424505543,-74.8570105508218,-74.7766116468169,
-74.69274627788,-74.6123498096441,-74.5319524963766,-74.4515392340459,-74.4411501710692,
-74.3607382418802,-74.2803414302624,-74.1964750318456,-74.1160807873363,
-74.0356857342678,-73.9552747701957,-73.9448758365954,-73.8644565163834,
-73.7840522023662,-73.700189527305,-73.6197876282239,-73.539384899434,-73.4589662739223,
-73.4486015021216,-73.3682988747528,-73.3238177496334),.UNSPECIFIED.);
#2920=B_SPLINE_CURVE_WITH_KNOTS('',3,(#21290,#21291,#21292,#21293,#21294,
#21295,#21296,#21297,#21298,#21299,#21300,#21301,#21302,#21303,#21304,#21305,
#21306,#21307,#21308,#21309,#21310,#21311,#21312,#21313,#21314,#21315,#21316,
#21317,#21318,#21319,#21320,#21321,#21322,#21323,#21324,#21325,#21326,#21327,
#21328,#21329,#21330,#21331,#21332,#21333,#21334,#21335,#21336,#21337,#21338,
#21339,#21340,#21341,#21342,#21343,#21344,#21345,#21346,#21347,#21348,#21349,
#21350,#21351,#21352,#21353,#21354,#21355,#21356,#21357,#21358,#21359,#21360,
#21361,#21362,#21363,#21364,#21365,#21366,#21367,#21368,#21369,#21370,#21371,
#21372,#21373,#21374,#21375,#21376,#21377,#21378,#21379,#21380,#21381,#21382,
#21383,#21384,#21385,#21386,#21387,#21388,#21389,#21390,#21391,#21392,#21393,
#21394,#21395,#21396,#21397,#21398,#21399,#21400,#21401,#21402,#21403,#21404,
#21405,#21406,#21407,#21408,#21409,#21410,#21411,#21412,#21413,#21414,#21415,
#21416,#21417,#21418,#21419,#21420,#21421,#21422,#21423,#21424,#21425,#21426,
#21427,#21428,#21429,#21430,#21431,#21432,#21433,#21434,#21435,#21436,#21437,
#21438,#21439,#21440,#21441,#21442,#21443),.UNSPECIFIED.,.F.,.F.,(4,2,2,
2,2,2,2,2,2,2,2,2,2,2,2,2,2,2,2,2,2,2,2,2,2,2,2,2,2,2,2,2,2,2,2,2,2,2,2,
2,2,2,2,2,2,2,2,2,2,2,2,2,2,2,2,2,2,2,2,2,2,2,2,2,2,2,2,2,2,2,2,2,2,2,2,
2,4),(-4.6604807148913,-4.61334475694576,-4.55984181574834,-4.53242377612221,
-4.5107875949951,-4.42356313296582,-4.35683282385191,-4.29437188688845,
-4.20601588083401,-4.17280892017205,-4.11426280773656,-4.04896992918726,
-3.99267617112123,-3.91273796752958,-3.86163756290624,-3.82680962834829,
-3.77698350095406,-3.70606384614301,-3.64832213371534,-3.53312480790826,
-3.50975322979048,-3.4763685978861,-3.41697863169213,-3.351940989318,-3.29570890247222,
-3.21866506262813,-3.16591823667992,-3.13061402538623,-3.06420103444955,
-3.02019411022275,-2.95843573977559,-2.83467487239128,-2.78861356788968,
-2.7491478137684,-2.668206714305,-2.60791226229094,-2.49096078734472,-2.45512420992431,
-2.42379811483375,-2.40623558811782,-2.34983856552957,-2.27766018523853,
-2.22111731642953,-2.15489946542858,-2.09929972861543,-2.06675245307284,
-1.98003559810137,-1.91589221954151,-1.85163962848125,-1.76974127329886,
-1.73549093138055,-1.67210578483828,-1.57986492237622,-1.52261465929151,
-1.45413293650151,-1.39911962377229,-1.36454975712187,-1.31406964444337,
-1.23315151866149,-1.17747412332377,-1.11354560615875,-1.05123048084556,
-1.01671421042371,-0.966982982709164,-0.883978144907126,-0.826699521657825,
-0.758975125168801,-0.704205029792625,-0.670313095416478,-0.646154031014603,
-0.534877130256036,-0.483215096994178,-0.419123134283916,-0.357410058846901,
-0.328069350014561,-0.290289649212232,-0.24984933934325),.UNSPECIFIED.);
#2921=B_SPLINE_CURVE_WITH_KNOTS('',3,(#21445,#21446,#21447,#21448,#21449,
#21450,#21451,#21452,#21453,#21454,#21455,#21456,#21457,#21458,#21459,#21460),
 .UNSPECIFIED.,.F.,.F.,(4,3,3,3,3,4),(-73.3238177496334,-73.2435365115161,
-73.1632507410983,-73.0829664079746,-73.0026647607017,-72.9680938357794),
 .UNSPECIFIED.);
#2922=B_SPLINE_CURVE_WITH_KNOTS('',3,(#21461,#21462,#21463,#21464,#21465,
#21466,#21467,#21468,#21469,#21470,#21471,#21472,#21473,#21474,#21475,#21476,
#21477),.UNSPECIFIED.,.F.,.F.,(4,2,1,1,1,1,1,1,1,1,1,1,1,4),(-72.9680938331862,
-72.9523271676478,-72.456052833174,-71.9597784987002,-71.4635041642264,
-70.9672298297526,-70.4709554952788,-69.974681160805,-69.4784068263312,
-68.9821324918575,-68.4858581573837,-67.9895838229099,-67.4933094884361,
-67.0406615200402),.UNSPECIFIED.);
#2923=B_SPLINE_CURVE_WITH_KNOTS('',3,(#21483,#21484,#21485,#21486,#21487,
#21488,#21489,#21490,#21491,#21492,#21493,#21494,#21495,#21496,#21497,#21498),
 .UNSPECIFIED.,.F.,.F.,(4,1,1,1,1,1,1,1,1,1,1,1,1,4),(64.4966950710674,
64.5156634815933,65.0119378160671,65.5082121505409,66.0044864850147,66.5007608194885,
66.9970351539623,67.4933094884361,67.9895838229099,68.4858581573837,68.9821324918575,
69.4784068263313,69.9746811608051,70.4241480285323),.UNSPECIFIED.);
#2924=B_SPLINE_CURVE_WITH_KNOTS('',3,(#21499,#21500,#21501,#21502,#21503,
#21504,#21505,#21506,#21507,#21508,#21509,#21510),.UNSPECIFIED.,.F.,.F.,
(4,2,2,2,2,4),(-4.91020706723789,-4.88001929369499,-4.84959643912597,-4.74176696137822,
-4.68911415734267,-4.6604807148913),.UNSPECIFIED.);
#2925=B_SPLINE_CURVE_WITH_KNOTS('',3,(#21512,#21513,#21514,#21515,#21516),
 .UNSPECIFIED.,.F.,.F.,(4,1,4),(-67.0406615200402,-66.9970351539623,-66.6849085260066),
 .UNSPECIFIED.);
#2926=B_SPLINE_CURVE_WITH_KNOTS('',3,(#21517,#21518,#21519,#21520,#21521,
#21522,#21523,#21524,#21525,#21526,#21527,#21528,#21529,#21530,#21531,#21532,
#21533,#21534,#21535,#21536,#21537,#21538,#21539,#21540,#21541,#21542,#21543,
#21544,#21545,#21546,#21547,#21548,#21549,#21550,#21551,#21552,#21553,#21554,
#21555,#21556,#21557,#21558,#21559,#21560,#21561,#21562,#21563,#21564,#21565,
#21566,#21567,#21568,#21569,#21570,#21571,#21572,#21573,#21574,#21575,#21576,
#21577,#21578,#21579,#21580,#21581,#21582,#21583,#21584,#21585,#21586,#21587,
#21588,#21589,#21590,#21591,#21592,#21593,#21594,#21595,#21596,#21597,#21598,
#21599,#21600,#21601,#21602,#21603,#21604,#21605,#21606,#21607,#21608,#21609,
#21610,#21611,#21612,#21613,#21614,#21615,#21616,#21617,#21618,#21619,#21620,
#21621,#21622,#21623,#21624,#21625,#21626,#21627,#21628,#21629,#21630,#21631,
#21632,#21633,#21634,#21635,#21636,#21637,#21638,#21639,#21640,#21641,#21642,
#21643,#21644,#21645,#21646,#21647,#21648,#21649,#21650,#21651,#21652,#21653,
#21654,#21655,#21656,#21657,#21658,#21659,#21660,#21661,#21662,#21663,#21664,
#21665,#21666,#21667,#21668,#21669,#21670,#21671,#21672,#21673,#21674,#21675,
#21676,#21677,#21678,#21679,#21680,#21681,#21682,#21683,#21684,#21685,#21686,
#21687,#21688,#21689,#21690,#21691,#21692,#21693,#21694,#21695,#21696,#21697,
#21698,#21699,#21700,#21701,#21702,#21703,#21704,#21705,#21706,#21707,#21708,
#21709,#21710,#21711,#21712,#21713,#21714,#21715,#21716,#21717,#21718,#21719,
#21720,#21721,#21722,#21723,#21724,#21725,#21726,#21727,#21728,#21729,#21730,
#21731,#21732,#21733,#21734,#21735,#21736,#21737,#21738,#21739,#21740,#21741,
#21742,#21743,#21744,#21745,#21746,#21747,#21748,#21749,#21750,#21751,#21752,
#21753,#21754,#21755,#21756,#21757,#21758,#21759,#21760,#21761,#21762,#21763,
#21764,#21765,#21766,#21767,#21768,#21769),.UNSPECIFIED.,.F.,.F.,(4,3,3,
3,3,3,3,3,3,3,3,3,3,3,3,3,3,3,3,3,3,3,3,3,3,3,3,3,3,3,3,3,3,3,3,3,3,3,3,
3,3,3,3,3,3,3,3,3,3,3,3,3,3,3,3,3,3,3,3,3,3,3,3,3,3,3,3,3,3,3,3,3,3,3,3,
3,3,3,3,3,3,3,3,3,4),(-66.6849085260066,-66.6022141450956,-66.5194935653768,
-66.5007608194885,-66.4203452380402,-66.3399447147115,-66.2560801572873,
-66.175682114948,-66.0952832498526,-66.0148684756778,-66.0044864850147,
-65.9240709033037,-65.8436703797093,-65.7598058224172,-65.6794077798094,
-65.599008914445,-65.5185941400035,-65.5082121505409,-65.4277965688989,
-65.3473960453742,-65.2635314880474,-65.1831334455096,-65.1027345802153,
-65.0223198058429,-65.0119378160671,-64.9315222344323,-64.8511217109148,
-64.7672571535845,-64.6868591110544,-64.6064602457679,-64.5260454714036,
-64.5156634815933,-64.4352478999337,-64.3548473763912,-64.2709828190733,
-64.1905847765176,-64.1101859112055,-64.0297711368156,-64.0193891471195,
-63.9389735654804,-63.8585730419587,-63.7747084846305,-63.6943104420959,
-63.6139115768051,-63.5334968024362,-63.5231148126457,-63.4426992309946,
-63.3622987074607,-63.2784341501385,-63.1980361075916,-63.1176372422883,
-63.0372224679071,-63.0268404781719,-62.9464248965263,-62.8660243729978,
-62.7821598156729,-62.7017617731316,-62.6213629078341,-62.5409481334585,
-62.5305661436981,-62.4501505620507,-62.3697500385205,-62.2858854811964,
-62.2054874386533,-62.125088573354,-62.0446737989765,-62.0342918092243,
-61.953876227577,-61.873475704047,-61.7896111467229,-61.7092131041798,-61.6288142388805,
-61.5483994645032,-61.5380174747505,-61.4576018931038,-61.3772013695742,
-61.2933368122498,-61.2129387697073,-61.1325399044087,-61.0521251300321,
-61.0417431402768,-60.9613264014195,-60.8809260071003,-60.8005299808948,
-60.7574681838464),.UNSPECIFIED.);
#2927=B_SPLINE_CURVE_WITH_KNOTS('',3,(#21775,#21776,#21777,#21778,#21779,
#21780,#21781,#21782,#21783,#21784,#21785,#21786,#21787,#21788,#21789,#21790,
#21791,#21792,#21793,#21794,#21795,#21796,#21797,#21798,#21799,#21800,#21801,
#21802,#21803,#21804,#21805,#21806,#21807,#21808,#21809,#21810,#21811,#21812,
#21813,#21814,#21815,#21816,#21817,#21818,#21819,#21820,#21821,#21822,#21823,
#21824,#21825,#21826,#21827,#21828,#21829,#21830,#21831,#21832,#21833,#21834,
#21835,#21836,#21837,#21838,#21839,#21840,#21841,#21842,#21843,#21844,#21845,
#21846,#21847,#21848,#21849,#21850,#21851,#21852,#21853,#21854,#21855,#21856,
#21857,#21858,#21859,#21860,#21861,#21862,#21863,#21864,#21865,#21866,#21867,
#21868,#21869,#21870,#21871,#21872,#21873,#21874,#21875,#21876,#21877,#21878,
#21879,#21880,#21881,#21882,#21883,#21884,#21885,#21886,#21887,#21888,#21889,
#21890,#21891,#21892,#21893,#21894,#21895,#21896,#21897,#21898,#21899,#21900,
#21901,#21902,#21903,#21904,#21905,#21906,#21907,#21908,#21909,#21910,#21911,
#21912,#21913,#21914,#21915,#21916,#21917,#21918,#21919,#21920,#21921,#21922,
#21923,#21924,#21925,#21926,#21927,#21928,#21929,#21930,#21931,#21932,#21933,
#21934,#21935,#21936,#21937,#21938,#21939,#21940,#21941,#21942,#21943,#21944,
#21945,#21946,#21947,#21948,#21949,#21950,#21951,#21952,#21953,#21954,#21955,
#21956,#21957,#21958,#21959,#21960,#21961,#21962,#21963,#21964,#21965,#21966,
#21967,#21968,#21969,#21970,#21971,#21972,#21973,#21974,#21975,#21976,#21977,
#21978,#21979,#21980,#21981,#21982,#21983,#21984,#21985,#21986,#21987,#21988,
#21989,#21990,#21991,#21992,#21993,#21994,#21995,#21996,#21997,#21998,#21999,
#22000,#22001,#22002,#22003,#22004,#22005,#22006,#22007,#22008,#22009,#22010,
#22011,#22012,#22013,#22014,#22015,#22016,#22017,#22018,#22019,#22020,#22021,
#22022,#22023,#22024,#22025,#22026,#22027),.UNSPECIFIED.,.F.,.F.,(4,3,3,
3,3,3,3,3,3,3,3,3,3,3,3,3,3,3,3,3,3,3,3,3,3,3,3,3,3,3,3,3,3,3,3,3,3,3,3,
3,3,3,3,3,3,3,3,3,3,3,3,3,3,3,3,3,3,3,3,3,3,3,3,3,3,3,3,3,3,3,3,3,3,3,3,
3,3,3,3,3,3,3,3,3,4),(58.2135306995125,58.2939232292864,58.3743217990603,
58.4547200449574,58.5351349677853,58.5603714679078,58.6407870495549,58.7211875730847,
58.8050521304089,58.8854501729518,58.9658490382507,59.0462638126277,59.0566458023816,
59.1370613840286,59.2174619075586,59.3013264648828,59.3817245074256,59.4621233727246,
59.5425381471016,59.5529201368554,59.6333357185025,59.7137362420324,59.7976007993566,
59.8779988418995,59.9583977071986,60.0388124815757,60.0491944713292,60.1296100529762,
60.210010576506,60.2938751338303,60.374273176373,60.4546720416721,60.5350868160491,
60.545468805803,60.6258843874502,60.7062849109802,60.7901494683044,60.8705475108473,
60.9509463761467,61.0313611505239,61.0417431402768,61.1221587219237,61.2025592454535,
61.2864238027778,61.3668218453204,61.4472207106195,61.5276354849965,61.5380174747506,
61.6184330563977,61.6988335799276,61.7826981372518,61.8630961797946,61.9434950450938,
62.023909819471,62.0342918092243,62.1147073908717,62.195107914402,62.278972471726,
62.3593705142691,62.4397693795688,62.5201841539462,62.5305661436981,62.6109817253437,
62.6913822488721,62.7752468061971,62.8556448487385,62.9360437140362,63.0164584884119,
63.0268404781719,63.107256059823,63.187656583357,63.2715211406792,63.351919183226,
63.4323180485291,63.5127328229102,63.5231148126457,63.6035303942844,63.683930917806,
63.7677954751344,63.8481935176689,63.9285923829598,64.0090071573289,64.0193891471195,
64.1039532538953,64.1409627629319),.UNSPECIFIED.);
#2928=B_SPLINE_CURVE_WITH_KNOTS('',3,(#22028,#22029,#22030,#22031),
 .UNSPECIFIED.,.F.,.F.,(4,4),(64.1409627629319,64.4966950710674),
 .UNSPECIFIED.);
#2929=B_SPLINE_CURVE_WITH_KNOTS('',3,(#22033,#22034,#22035,#22036,#22037,
#22038,#22039,#22040,#22041,#22042,#22043,#22044,#22045,#22046,#22047,#22048),
 .UNSPECIFIED.,.F.,.F.,(4,3,3,3,3,4),(-60.7574681838464,-60.6770705117027,
-60.5966545091061,-60.545468805803,-60.4616324956271,-60.401723218827),
 .UNSPECIFIED.);
#2930=B_SPLINE_CURVE_WITH_KNOTS('',3,(#22049,#22050,#22051,#22052,#22053,
#22054,#22055,#22056,#22057,#22058,#22059,#22060,#22061,#22062,#22063,#22064),
 .UNSPECIFIED.,.F.,.F.,(4,1,1,1,1,1,1,1,1,1,1,1,1,4),(-60.401723218827,
-60.0491944713291,-59.5529201368554,-59.0566458023816,-58.5603714679078,
-58.064097133434,-57.5678227989602,-57.0715484644864,-56.5752741300126,
-56.0789997955388,-55.582725461065,-55.0864511265912,-54.5901767921174,
-54.4742514652626),.UNSPECIFIED.);
#2931=B_SPLINE_CURVE_WITH_KNOTS('',3,(#22070,#22071,#22072,#22073,#22074,
#22075,#22076,#22077,#22078,#22079,#22080,#22081,#22082,#22083,#22084,#22085),
 .UNSPECIFIED.,.F.,.F.,(4,1,1,1,1,1,1,1,1,1,1,1,1,4),(51.9303121562591,
52.1088051197484,52.6050794542222,53.101353788696,53.5976281231698,54.0939024576436,
54.5901767921174,55.0864511265912,55.582725461065,56.0789997955388,56.5752741300126,
57.0715484644864,57.5678227989602,57.8577774557523),.UNSPECIFIED.);
#2932=B_SPLINE_CURVE_WITH_KNOTS('',3,(#22086,#22087,#22088,#22089,#22090,
#22091,#22092,#22093,#22094,#22095,#22096,#22097,#22098,#22099,#22100,#22101),
 .UNSPECIFIED.,.F.,.F.,(4,3,3,3,3,4),(57.8577774557523,57.9399575861014,
58.0221642585411,58.064097133434,58.1445144829838,58.2135306995125),
 .UNSPECIFIED.);
#2933=B_SPLINE_CURVE_WITH_KNOTS('',3,(#22103,#22104,#22105,#22106),
 .UNSPECIFIED.,.F.,.F.,(4,4),(-54.4742514652626,-54.118537942137),
 .UNSPECIFIED.);
#2934=B_SPLINE_CURVE_WITH_KNOTS('',3,(#22107,#22108,#22109,#22110,#22111,
#22112,#22113,#22114,#22115,#22116,#22117,#22118,#22119,#22120,#22121,#22122,
#22123,#22124,#22125,#22126,#22127,#22128,#22129,#22130,#22131,#22132,#22133,
#22134,#22135,#22136,#22137,#22138,#22139,#22140,#22141,#22142,#22143,#22144,
#22145,#22146,#22147,#22148,#22149,#22150,#22151,#22152,#22153,#22154,#22155,
#22156,#22157,#22158,#22159,#22160,#22161,#22162,#22163,#22164,#22165,#22166,
#22167,#22168,#22169,#22170,#22171,#22172,#22173,#22174,#22175,#22176,#22177,
#22178,#22179,#22180,#22181,#22182,#22183,#22184,#22185,#22186,#22187,#22188,
#22189,#22190,#22191,#22192,#22193,#22194,#22195,#22196,#22197,#22198,#22199,
#22200,#22201,#22202,#22203,#22204,#22205,#22206,#22207,#22208,#22209,#22210,
#22211,#22212,#22213,#22214,#22215,#22216,#22217,#22218,#22219,#22220,#22221,
#22222,#22223,#22224,#22225,#22226,#22227,#22228,#22229,#22230,#22231,#22232,
#22233,#22234,#22235,#22236,#22237,#22238,#22239,#22240,#22241,#22242,#22243,
#22244,#22245,#22246,#22247,#22248,#22249,#22250,#22251,#22252,#22253,#22254,
#22255,#22256,#22257,#22258,#22259,#22260,#22261,#22262,#22263,#22264,#22265,
#22266,#22267,#22268,#22269,#22270,#22271,#22272,#22273,#22274,#22275,#22276,
#22277,#22278,#22279,#22280,#22281,#22282,#22283,#22284,#22285,#22286,#22287,
#22288,#22289,#22290,#22291,#22292,#22293,#22294,#22295,#22296,#22297,#22298,
#22299,#22300,#22301,#22302,#22303,#22304,#22305,#22306,#22307,#22308,#22309,
#22310,#22311,#22312,#22313,#22314,#22315,#22316,#22317,#22318,#22319,#22320,
#22321,#22322,#22323,#22324,#22325,#22326,#22327,#22328,#22329,#22330,#22331,
#22332,#22333,#22334,#22335,#22336,#22337,#22338,#22339,#22340,#22341,#22342,
#22343,#22344,#22345,#22346,#22347,#22348,#22349,#22350,#22351,#22352,#22353,
#22354,#22355,#22356,#22357,#22358,#22359),.UNSPECIFIED.,.F.,.F.,(4,3,3,
3,3,3,3,3,3,3,3,3,3,3,3,3,3,3,3,3,3,3,3,3,3,3,3,3,3,3,3,3,3,3,3,3,3,3,3,
3,3,3,3,3,3,3,3,3,3,3,3,3,3,3,3,3,3,3,3,3,3,3,3,3,3,3,3,3,3,3,3,3,3,3,3,
3,3,3,3,3,3,3,3,3,4),(-54.1185379116474,-54.0939024576436,-54.0134868759983,
-53.9330863524702,-53.8492217951451,-53.768823752604,-53.6884248873065,
-53.6080101129313,-53.5976281231698,-53.517212541522,-53.4368120179915,
-53.3529474606676,-53.2725494181242,-53.1921505528245,-53.1117357784469,
-53.101353788696,-53.0209382070492,-52.9405376835194,-52.8566731261951,
-52.7762750836525,-52.6958762183537,-52.6154614439767,-52.6050794542222,
-52.5246638725751,-52.4442633490453,-52.3603987917211,-52.2800007491782,
-52.199601883879,-52.1191871095019,-52.1088051197484,-52.0283895381012,
-51.9479890145712,-51.864124457247,-51.7837264147041,-51.7033275494047,
-51.6229127750274,-51.6125307852746,-51.5321152036277,-51.451714680098,
-51.3678501227737,-51.2874520802311,-51.2070532149321,-51.1266384405552,
-51.1162564508009,-51.0358408691537,-50.9554403456238,-50.8715757882996,
-50.7911777457567,-50.7107788804575,-50.6303641060803,-50.6199821163271,
-50.53956653468,-50.45916601115,-50.3753014538258,-50.294903411283,-50.2145045459838,
-50.1340897716066,-50.1237077818533,-50.0432922002063,-49.9628916766764,
-49.8790271193522,-49.7986290768094,-49.7182302115103,-49.6378154371333,
-49.6274334473795,-49.5470178657324,-49.4666173422025,-49.3827527848783,
-49.3023547423355,-49.2219558770364,-49.1415411026592,-49.1311591129057,
-49.0507435312586,-48.9703430077288,-48.8864784504046,-48.8060804078618,
-48.7256815425627,-48.6452667681856,-48.6348847784319,-48.5544697200655,
-48.4740699157614,-48.3936710920797,-48.3132774925887,-48.232871672302,
-48.1911042754973),.UNSPECIFIED.);
#2935=B_SPLINE_CURVE_WITH_KNOTS('',3,(#22365,#22366,#22367,#22368,#22369,
#22370,#22371,#22372,#22373,#22374,#22375,#22376,#22377,#22378,#22379,#22380,
#22381,#22382,#22383,#22384,#22385,#22386,#22387,#22388,#22389,#22390,#22391,
#22392,#22393,#22394,#22395,#22396,#22397,#22398,#22399,#22400,#22401,#22402,
#22403,#22404,#22405,#22406,#22407,#22408,#22409,#22410,#22411,#22412,#22413,
#22414,#22415,#22416,#22417,#22418,#22419,#22420,#22421,#22422,#22423,#22424,
#22425,#22426,#22427,#22428,#22429,#22430,#22431,#22432,#22433,#22434,#22435,
#22436,#22437,#22438,#22439,#22440,#22441,#22442,#22443,#22444,#22445,#22446,
#22447,#22448,#22449,#22450,#22451,#22452,#22453,#22454,#22455,#22456,#22457,
#22458,#22459,#22460,#22461,#22462,#22463,#22464,#22465,#22466,#22467,#22468,
#22469,#22470,#22471,#22472,#22473,#22474,#22475,#22476,#22477,#22478,#22479,
#22480,#22481,#22482,#22483,#22484,#22485,#22486,#22487,#22488,#22489,#22490,
#22491,#22492,#22493,#22494,#22495,#22496,#22497,#22498,#22499,#22500,#22501,
#22502,#22503,#22504,#22505,#22506,#22507,#22508,#22509,#22510,#22511,#22512,
#22513,#22514,#22515,#22516,#22517,#22518,#22519,#22520,#22521,#22522,#22523,
#22524,#22525,#22526,#22527,#22528,#22529,#22530,#22531,#22532,#22533,#22534,
#22535,#22536,#22537,#22538,#22539,#22540,#22541,#22542,#22543,#22544,#22545,
#22546,#22547,#22548,#22549,#22550,#22551,#22552,#22553,#22554,#22555,#22556,
#22557,#22558,#22559,#22560,#22561,#22562,#22563,#22564,#22565,#22566,#22567,
#22568,#22569,#22570,#22571,#22572,#22573,#22574,#22575,#22576,#22577,#22578,
#22579,#22580,#22581,#22582,#22583,#22584,#22585,#22586,#22587,#22588,#22589,
#22590,#22591,#22592,#22593,#22594,#22595,#22596,#22597,#22598,#22599,#22600,
#22601,#22602,#22603,#22604,#22605,#22606,#22607,#22608,#22609,#22610,#22611,
#22612,#22613,#22614,#22615,#22616,#22617),.UNSPECIFIED.,.F.,.F.,(4,3,3,
3,3,3,3,3,3,3,3,3,3,3,3,3,3,3,3,3,3,3,3,3,3,3,3,3,3,3,3,3,3,3,3,3,3,3,3,
3,3,3,3,3,3,3,3,3,3,3,3,3,3,3,3,3,3,3,3,3,3,3,3,3,3,3,3,3,3,3,3,3,3,3,3,
3,3,3,3,3,3,3,3,3,4),(45.647142400955,45.6572387715891,45.7376543532363,
45.8180548767661,45.9019194340903,45.9823174766332,46.0627163419325,46.1431311163099,
46.1535131060629,46.2339286877099,46.3143292112395,46.3981937685638,46.4785918111067,
46.5589906764063,46.6394054507831,46.6497874405367,46.7302030221839,46.8106035457137,
46.8944681030379,46.9748661455806,47.0552650108795,47.135679785257,47.1460617750105,
47.2264773566577,47.3068778801874,47.3907424375117,47.4711404800545,47.5515393453538,
47.6319541197311,47.6423361094843,47.7227516911314,47.8031522146613,47.8870167719855,
47.9674148145283,48.0478136798277,48.1282284542052,48.1386104439581,48.2190260256053,
48.2994265491352,48.3832911064594,48.4636891490023,48.5440880143019,48.6245027886792,
48.6348847784319,48.7153003600789,48.7957008836091,48.8795654409332,48.959963483476,
49.0403623487745,49.1207771231514,49.1311591129057,49.2115746945528,49.2919752180826,
49.3758397754068,49.4562378179496,49.5366366832484,49.6170514576258,49.6274334473795,
49.7078490290264,49.7882495525564,49.8721141098806,49.9525121524234,50.0329110177216,
50.113325792099,50.1237077818533,50.2041233635004,50.2845238870303,50.3683884443545,
50.4487864868975,50.5291853521968,50.6096001265737,50.6199821163271,50.7003976979744,
50.7807982215041,50.8646627788283,50.9450608213712,51.0254596866705,51.1058744610481,
51.1162564508009,51.1964454262238,51.2766186167369,51.3567929105404,51.4369628388392,
51.5171506432341,51.5745921433062),.UNSPECIFIED.);
#2936=B_SPLINE_CURVE_WITH_KNOTS('',3,(#22618,#22619,#22620,#22621,#22622),
 .UNSPECIFIED.,.F.,.F.,(4,1,4),(51.5745921485727,51.6125307852747,51.9303121562591),
 .UNSPECIFIED.);
#2937=B_SPLINE_CURVE_WITH_KNOTS('',3,(#22624,#22625,#22626,#22627,#22628,
#22629,#22630,#22631,#22632,#22633,#22634,#22635,#22636,#22637,#22638,#22639),
 .UNSPECIFIED.,.F.,.F.,(4,3,3,3,3,4),(-48.1911042754973,-48.1386104439581,
-48.0579420042558,-47.9772908992282,-47.8966451486634,-47.8353526044678),
 .UNSPECIFIED.);
#2938=B_SPLINE_CURVE_WITH_KNOTS('',3,(#22640,#22641,#22642,#22643,#22644,
#22645,#22646,#22647,#22648,#22649,#22650,#22651,#22652,#22653,#22654,#22655),
 .UNSPECIFIED.,.F.,.F.,(4,1,1,1,1,1,1,1,1,1,1,1,1,4),(-47.8353525749775,
-47.6423361094843,-47.1460617750105,-46.6497874405367,-46.1535131060629,
-45.6572387715891,-45.1609644371153,-44.6646901026415,-44.1684157681677,
-43.6721414336939,-43.1758670992201,-42.6795927647463,-42.1833184302725,
-41.9079142575377),.UNSPECIFIED.);
#2939=B_SPLINE_CURVE_WITH_KNOTS('',3,(#22661,#22662,#22663,#22664,#22665,
#22666,#22667,#22668,#22669,#22670,#22671,#22672,#22673,#22674,#22675,#22676,
#22677,#22678,#22679,#22680,#22681,#22682,#22683,#22684,#22685,#22686,#22687,
#22688,#22689,#22690,#22691,#22692,#22693,#22694,#22695,#22696,#22697,#22698,
#22699,#22700,#22701,#22702,#22703,#22704,#22705,#22706,#22707,#22708,#22709,
#22710,#22711,#22712,#22713,#22714,#22715,#22716,#22717,#22718,#22719,#22720,
#22721,#22722,#22723,#22724,#22725,#22726,#22727,#22728,#22729,#22730,#22731,
#22732,#22733,#22734,#22735,#22736,#22737,#22738,#22739,#22740,#22741,#22742,
#22743,#22744,#22745,#22746,#22747,#22748,#22749,#22750,#22751,#22752,#22753,
#22754,#22755,#22756,#22757,#22758,#22759,#22760,#22761,#22762,#22763,#22764,
#22765,#22766,#22767,#22768,#22769,#22770,#22771,#22772,#22773,#22774,#22775,
#22776,#22777,#22778,#22779,#22780,#22781,#22782,#22783,#22784,#22785,#22786,
#22787,#22788,#22789,#22790,#22791,#22792,#22793,#22794,#22795,#22796),
 .UNSPECIFIED.,.F.,.F.,(4,2,2,2,2,2,2,2,2,2,2,2,2,2,2,2,2,2,2,2,2,2,2,2,
2,2,2,2,2,2,2,2,2,2,2,2,2,2,2,2,2,2,2,2,2,2,2,2,2,2,2,2,2,2,2,2,2,2,2,2,
2,2,2,2,2,2,2,4),(-4.16125843062839,-4.1108086605335,-4.05416447052261,
-3.98749224892683,-3.93335266536444,-3.90089760007793,-3.81396261840104,
-3.75034504100606,-3.68650609084296,-3.60473171151153,-3.57003366441495,
-3.50441512059131,-3.41364754281864,-3.35686392893218,-3.28964848409738,
-3.23537623700149,-3.20235008820308,-3.17963213204777,-3.05593950076319,
-2.99418126756799,-2.95018762802497,-2.88372166014699,-2.84839584138017,
-2.79557554860951,-2.71865311166099,-2.66243250284885,-2.59742866299811,
-2.53793459965514,-2.50453156308288,-2.48112530574869,-2.36122344306523,
-2.30092403435905,-2.21995596297141,-2.18052956626483,-2.13434766972314,
-2.01080383157267,-1.94908345957558,-1.83812709929393,-1.80245275651468,
-1.74842312898728,-1.67350706895093,-1.6173100370115,-1.55240221556747,
-1.49258544298174,-1.45911175717965,-1.43557908690942,-1.31490300923238,
-1.25386188550675,-1.16989048405493,-1.13360923308017,-1.08140683606103,
-0.96871936538971,-0.909129093310782,-0.831008023402229,-0.791565263964351,
-0.75438182047145,-0.695006080529864,-0.621258347948833,-0.56218228778284,
-0.486096455137806,-0.442681649268167,-0.404944314135633,-0.343370842314088,
-0.277218096883528,-0.225297486579145,-0.119533728146101,-0.0878835127706171,
-0.000106117481471679),.UNSPECIFIED.);
#2940=B_SPLINE_CURVE_WITH_KNOTS('',3,(#22797,#22798,#22799,#22800,#22801,
#22802,#22803,#22804,#22805,#22806,#22807,#22808,#22809,#22810,#22811,#22812),
 .UNSPECIFIED.,.F.,.F.,(4,3,3,3,3,4),(45.2914068413931,45.3715871243321,
45.4517702421806,45.5319511477599,45.6121488851322,45.647142400955),
 .UNSPECIFIED.);
#2941=B_SPLINE_CURVE_WITH_KNOTS('',3,(#22814,#22815,#22816,#22817,#22818),
 .UNSPECIFIED.,.F.,.F.,(4,1,4),(-41.9079142575377,-41.6870440957988,-41.5521673127012),
 .UNSPECIFIED.);
#2942=B_SPLINE_CURVE_WITH_KNOTS('',3,(#22819,#22820,#22821,#22822,#22823,
#22824,#22825,#22826,#22827,#22828,#22829,#22830,#22831,#22832,#22833,#22834,
#22835,#22836,#22837,#22838,#22839,#22840,#22841,#22842,#22843,#22844,#22845,
#22846,#22847,#22848,#22849,#22850,#22851,#22852,#22853,#22854,#22855,#22856,
#22857,#22858,#22859,#22860,#22861,#22862,#22863,#22864,#22865,#22866,#22867,
#22868,#22869,#22870,#22871,#22872,#22873,#22874,#22875,#22876,#22877,#22878,
#22879,#22880,#22881,#22882,#22883,#22884,#22885,#22886,#22887,#22888,#22889,
#22890,#22891,#22892,#22893,#22894,#22895,#22896,#22897,#22898,#22899,#22900,
#22901,#22902,#22903,#22904,#22905,#22906,#22907,#22908,#22909,#22910,#22911,
#22912,#22913,#22914,#22915,#22916,#22917,#22918,#22919,#22920,#22921,#22922,
#22923,#22924,#22925,#22926,#22927,#22928,#22929,#22930,#22931,#22932,#22933,
#22934,#22935,#22936,#22937,#22938,#22939,#22940,#22941,#22942,#22943,#22944,
#22945,#22946,#22947,#22948,#22949,#22950,#22951,#22952,#22953,#22954,#22955,
#22956,#22957,#22958,#22959,#22960,#22961,#22962,#22963,#22964,#22965,#22966,
#22967,#22968,#22969,#22970,#22971,#22972,#22973,#22974,#22975,#22976,#22977,
#22978,#22979,#22980,#22981,#22982,#22983,#22984,#22985,#22986,#22987,#22988,
#22989,#22990,#22991,#22992,#22993,#22994,#22995,#22996,#22997,#22998,#22999,
#23000,#23001,#23002,#23003,#23004,#23005,#23006,#23007,#23008,#23009,#23010,
#23011,#23012,#23013,#23014,#23015,#23016,#23017,#23018,#23019,#23020,#23021,
#23022,#23023,#23024,#23025,#23026,#23027,#23028,#23029,#23030,#23031,#23032,
#23033,#23034,#23035,#23036,#23037,#23038,#23039,#23040,#23041,#23042,#23043,
#23044,#23045,#23046,#23047,#23048,#23049,#23050,#23051,#23052,#23053,#23054,
#23055,#23056,#23057,#23058,#23059,#23060,#23061,#23062,#23063,#23064,#23065,
#23066,#23067,#23068,#23069,#23070,#23071),.UNSPECIFIED.,.F.,.F.,(4,3,3,
3,3,3,3,3,3,3,3,3,3,3,3,3,3,3,3,3,3,3,3,3,3,3,3,3,3,3,3,3,3,3,3,3,3,3,3,
3,3,3,3,3,3,3,3,3,3,3,3,3,3,3,3,3,3,3,3,3,3,3,3,3,3,3,3,3,3,3,3,3,3,3,3,
3,3,3,3,3,3,3,3,3,4),(-41.5521672972882,-41.4719671688436,-41.3917628968607,
-41.3115604309128,-41.2313396225703,-41.190769761325,-41.1103541796779,
-41.0299536561481,-40.9460890988238,-40.865691056281,-40.7852921909818,
-40.7048774166049,-40.6944954268512,-40.6140798452041,-40.533679321674,
-40.4498147643498,-40.369416721807,-40.2890178565077,-40.2086030821303,
-40.1982210923774,-40.1178055107303,-40.0374049872004,-39.9535404298762,
-39.8731423873333,-39.7927435220346,-39.7123287476571,-39.7019467579036,
-39.6215311762567,-39.5411306527269,-39.4572660954026,-39.3768680528599,
-39.2964691875608,-39.2160544131837,-39.2056724234298,-39.1252568417827,
-39.0448563182525,-38.9609917609284,-38.8805937183855,-38.8001948530866,
-38.7197800787096,-38.709398088956,-38.6289825073088,-38.5485819837791,
-38.4647174264549,-38.3843193839121,-38.3039205186132,-38.2235057442359,
-38.2131237544822,-38.1327081728352,-38.0523076493057,-37.9684430919814,
-37.8880450494384,-37.8076461841394,-37.7272314097624,-37.7168494200084,
-37.6364338383614,-37.5560333148318,-37.4721687575075,-37.3917707149647,
-37.311371849666,-37.2309570752894,-37.2205750855346,-37.1401595038874,
-37.0597589803572,-36.9758944230331,-36.8954963804905,-36.815097515191,
-36.7346827408139,-36.7243007510608,-36.6438851694137,-36.5634846458835,
-36.4796200885594,-36.3992220460168,-36.3188231807168,-36.2384084063399,
-36.228026416587,-36.1476108349403,-36.0672103114103,-35.983345754086,-35.9029477115432,
-35.8225488462444,-35.7421340718673,-35.7317520821132,-35.6515438818655,
-35.6247062080056),.UNSPECIFIED.);
#2943=B_SPLINE_CURVE_WITH_KNOTS('',3,(#23076,#23077,#23078,#23079,#23080,
#23081,#23082,#23083,#23084,#23085,#23086,#23087,#23088,#23089,#23090,#23091,
#23092,#23093,#23094,#23095,#23096,#23097,#23098,#23099,#23100,#23101,#23102,
#23103,#23104,#23105,#23106,#23107,#23108,#23109,#23110,#23111,#23112,#23113,
#23114,#23115,#23116,#23117,#23118,#23119,#23120,#23121,#23122,#23123,#23124,
#23125,#23126,#23127,#23128,#23129,#23130,#23131,#23132,#23133,#23134,#23135,
#23136,#23137,#23138,#23139,#23140,#23141,#23142,#23143,#23144,#23145,#23146,
#23147,#23148,#23149,#23150,#23151,#23152,#23153,#23154,#23155,#23156,#23157,
#23158,#23159,#23160,#23161,#23162,#23163,#23164,#23165,#23166,#23167,#23168,
#23169,#23170,#23171,#23172,#23173,#23174,#23175,#23176,#23177,#23178,#23179,
#23180,#23181,#23182,#23183,#23184,#23185,#23186,#23187,#23188,#23189,#23190,
#23191,#23192,#23193,#23194,#23195,#23196,#23197,#23198,#23199,#23200,#23201,
#23202,#23203,#23204,#23205,#23206,#23207,#23208,#23209,#23210,#23211,#23212,
#23213,#23214,#23215,#23216,#23217,#23218,#23219,#23220,#23221,#23222,#23223,
#23224,#23225,#23226,#23227),.UNSPECIFIED.,.F.,.F.,(4,2,2,2,2,2,2,2,2,2,
2,2,2,2,2,2,2,2,2,2,2,2,2,2,2,2,2,2,2,2,2,2,2,2,2,2,2,2,2,2,2,2,2,2,2,2,
2,2,2,2,2,2,2,2,2,2,2,2,2,2,2,2,2,2,2,2,2,2,2,2,2,2,2,2,2,4),(-8.57214567350776,
-8.5266526945173,-8.47967990369863,-8.45352593416885,-8.41269080105662,
-8.32357750766793,-8.26675918760088,-8.17541753599182,-8.11128974902864,
-8.07734762921564,-7.99492171986943,-7.93051510561155,-7.867438884642,-7.78085350584145,
-7.74794241748207,-7.68271771847744,-7.62071885661382,-7.59482270420592,
-7.53820554178689,-7.41727315483455,-7.38527882315083,-7.30251478290774,
-7.23574075296484,-7.17329952166471,-7.08490414212474,-7.05168861272035,
-6.99309313453794,-6.92780991550629,-6.87151711115175,-6.79163488564728,
-6.74049863515228,-6.70565835006123,-6.65581906752867,-6.58489709551557,
-6.52715000382637,-6.41197745733838,-6.38859477706288,-6.35520388857515,
-6.29576392880009,-6.23073825351169,-6.17451102941036,-6.09734748834294,
-6.0446691883285,-6.00938343143802,-5.96661625394913,-5.89148028632875,
-5.8326462101903,-5.75898501190176,-5.69985734716562,-5.66274231957707,
-5.6232229887053,-5.54517646139644,-5.48560457797253,-5.37305407574671,
-5.32076994023303,-5.28450800708924,-5.20050925348284,-5.13946077987214,
-5.01875985988877,-4.99523565647675,-4.96176632701582,-4.90196426199717,
-4.83704884082245,-4.7808499002071,-4.70579620245074,-4.65185471080323,
-4.61620534622512,-4.56149675036933,-4.49267357885504,-4.46599248140042,
-4.41096987361156,-4.38049219746669,-4.29791625040967,-4.2646669972504,
-4.19899215883652,-4.16125843062839),.UNSPECIFIED.);
#2944=B_SPLINE_CURVE_WITH_KNOTS('',3,(#23229,#23230,#23231,#23232,#23233,
#23234,#23235,#23236,#23237,#23238,#23239,#23240,#23241,#23242,#23243,#23244),
 .UNSPECIFIED.,.F.,.F.,(4,3,3,3,3,4),(-35.6247062080056,-35.5445172087638,
-35.4643253594168,-35.3841357287812,-35.3039293308426,-35.2689819950581),
 .UNSPECIFIED.);
#2945=B_SPLINE_CURVE_WITH_KNOTS('',3,(#23245,#23246,#23247,#23248,#23249,
#23250,#23251,#23252,#23253,#23254,#23255,#23256,#23257,#23258,#23259,#23260),
 .UNSPECIFIED.,.F.,.F.,(4,1,1,1,1,1,1,1,1,1,1,1,1,4),(-35.2689819901086,
-35.2354777476394,-34.7392034131656,-34.2429290786918,-33.746654744218,
-33.2503804097442,-32.7541060752704,-32.2578317407966,-31.7615574063229,
-31.2652830718491,-30.7690087373753,-30.2727344029015,-29.7764600684277,
-29.3415541759224),.UNSPECIFIED.);
#2946=B_SPLINE_CURVE_WITH_KNOTS('',3,(#23266,#23267,#23268,#23269,#23270,
#23271,#23272,#23273,#23274,#23275,#23276,#23277,#23278,#23279,#23280,#23281,
#23282,#23283,#23284,#23285,#23286,#23287,#23288,#23289,#23290,#23291,#23292,
#23293,#23294,#23295,#23296,#23297,#23298,#23299,#23300,#23301,#23302,#23303,
#23304,#23305,#23306,#23307,#23308,#23309,#23310,#23311,#23312,#23313,#23314,
#23315,#23316,#23317,#23318,#23319,#23320,#23321,#23322,#23323,#23324,#23325,
#23326,#23327,#23328,#23329,#23330,#23331,#23332,#23333,#23334,#23335,#23336,
#23337,#23338,#23339,#23340,#23341,#23342,#23343,#23344,#23345,#23346,#23347,
#23348,#23349,#23350,#23351,#23352,#23353,#23354,#23355,#23356,#23357,#23358,
#23359,#23360,#23361,#23362,#23363,#23364,#23365,#23366,#23367,#23368,#23369,
#23370,#23371,#23372,#23373,#23374,#23375,#23376,#23377,#23378,#23379,#23380,
#23381,#23382,#23383,#23384,#23385,#23386,#23387,#23388,#23389,#23390,#23391,
#23392,#23393,#23394,#23395,#23396,#23397,#23398,#23399,#23400,#23401,#23402,
#23403,#23404,#23405,#23406,#23407,#23408,#23409,#23410,#23411,#23412,#23413,
#23414,#23415,#23416,#23417,#23418,#23419,#23420,#23421,#23422,#23423,#23424,
#23425,#23426,#23427,#23428,#23429,#23430,#23431,#23432,#23433,#23434,#23435,
#23436,#23437,#23438,#23439,#23440,#23441,#23442,#23443,#23444,#23445,#23446,
#23447,#23448,#23449,#23450,#23451,#23452,#23453,#23454,#23455,#23456,#23457,
#23458,#23459,#23460,#23461,#23462,#23463,#23464,#23465,#23466,#23467,#23468,
#23469,#23470,#23471,#23472,#23473,#23474,#23475,#23476,#23477,#23478,#23479,
#23480,#23481,#23482,#23483,#23484,#23485,#23486,#23487,#23488,#23489,#23490,
#23491,#23492,#23493,#23494,#23495,#23496,#23497,#23498,#23499,#23500,#23501,
#23502,#23503,#23504,#23505,#23506,#23507,#23508,#23509,#23510,#23511,#23512,
#23513,#23514,#23515,#23516,#23517,#23518),.UNSPECIFIED.,.F.,.F.,(4,3,3,
3,3,3,3,3,3,3,3,3,3,3,3,3,3,3,3,3,3,3,3,3,3,3,3,3,3,3,3,3,3,3,3,3,3,3,3,
3,3,3,3,3,3,3,3,3,3,3,3,3,3,3,3,3,3,3,3,3,3,3,3,3,3,3,3,3,3,3,3,3,3,3,3,
3,3,3,3,3,3,3,3,3,4),(26.7975893262247,26.7988140615849,26.8792296432319,
26.9596301667617,27.043494724086,27.1238927666289,27.2042916319276,27.2847064063046,
27.2950883960587,27.3755039777059,27.4559045012358,27.53976905856,27.6201671011028,
27.700565966402,27.7809807407789,27.7913627305325,27.8717783121796,27.9521788357092,
28.0360433930335,28.1164414355764,28.1968403008755,28.2772550752525,28.2876370650063,
28.3680526466533,28.448453170183,28.5323177275073,28.61271577005,28.6931146353489,
28.7735294097261,28.7839113994801,28.8643269811273,28.9447275046572,29.0285920619814,
29.1089901045244,29.1893889698233,29.2698037442009,29.2801857339539,29.360601315601,
29.4410018391309,29.5248663964551,29.6052644389978,29.6856633042968,29.7660780786739,
29.7764600684277,29.8568756500748,29.9372761736052,30.0211407309293,30.1015387734722,
30.1819376387715,30.262352413149,30.2727344029015,30.3531499845486,30.4335505080785,
30.5174150654027,30.5978131079454,30.6782119732445,30.7586267476212,30.7690087373753,
30.8494243190225,30.929824842553,31.013689399877,31.0940874424199,31.1744863077184,
31.2549010820954,31.2652830718491,31.3456986534964,31.4260991770262,31.5099637343504,
31.5903617768931,31.6707606421923,31.7511754165694,31.7615574063229,31.8419729879701,
31.9223735115007,32.0062380688247,32.0866361113677,32.1670349766674,32.2474497510447,
32.2578317407967,32.3380614960746,32.4182755973972,32.4984913520439,32.5787024990809,
32.6589326269847,32.72503622265),.UNSPECIFIED.);
#2947=B_SPLINE_CURVE_WITH_KNOTS('',3,(#23519,#23520,#23521,#23522,#23523,
#23524,#23525,#23526,#23527,#23528,#23529,#23530),.UNSPECIFIED.,.F.,.F.,
(4,2,2,2,2,4),(-8.82186319664549,-8.79141945747857,-8.74049362082466,-8.66687908944385,
-8.61461409729926,-8.57214567350776),.UNSPECIFIED.);
#2948=B_SPLINE_CURVE_WITH_KNOTS('',3,(#23532,#23533,#23534,#23535,#23536),
 .UNSPECIFIED.,.F.,.F.,(4,1,4),(-29.3415541759224,-29.2801857339539,-28.985796682929),
 .UNSPECIFIED.);
#2949=B_SPLINE_CURVE_WITH_KNOTS('',3,(#23537,#23538,#23539,#23540,#23541,
#23542,#23543,#23544,#23545,#23546,#23547,#23548,#23549,#23550,#23551,#23552,
#23553,#23554,#23555,#23556,#23557,#23558,#23559,#23560,#23561,#23562,#23563,
#23564,#23565,#23566,#23567,#23568,#23569,#23570,#23571,#23572,#23573,#23574,
#23575,#23576,#23577,#23578,#23579,#23580,#23581,#23582,#23583,#23584,#23585,
#23586,#23587,#23588,#23589,#23590,#23591,#23592,#23593,#23594,#23595,#23596,
#23597,#23598,#23599,#23600,#23601,#23602,#23603,#23604,#23605,#23606,#23607,
#23608,#23609,#23610,#23611,#23612,#23613,#23614,#23615,#23616,#23617,#23618,
#23619,#23620,#23621,#23622,#23623,#23624,#23625,#23626,#23627,#23628,#23629,
#23630,#23631,#23632,#23633,#23634,#23635,#23636,#23637,#23638,#23639,#23640,
#23641,#23642,#23643,#23644,#23645,#23646,#23647,#23648,#23649,#23650,#23651,
#23652,#23653,#23654,#23655,#23656,#23657,#23658,#23659,#23660,#23661,#23662,
#23663,#23664,#23665,#23666,#23667,#23668,#23669,#23670,#23671,#23672,#23673,
#23674),.UNSPECIFIED.,.F.,.F.,(4,2,2,2,2,2,2,2,2,2,2,2,2,2,2,2,2,2,2,2,
2,2,2,2,2,2,2,2,2,2,2,2,2,2,2,2,2,2,2,2,2,2,2,2,2,2,2,2,2,2,2,2,2,2,2,2,
2,2,2,2,2,2,2,2,2,2,2,2,4),(-8.82172059392306,-8.71505368676722,-8.68624371205641,
-8.65611514691957,-8.54557674370032,-8.49338883640374,-8.40158893096534,
-8.35665083111386,-8.32980663957806,-8.28691118496182,-8.21003328989268,
-8.15075738237388,-8.07570115263926,-8.01696196782507,-7.97995546412746,
-7.94025100202579,-7.86237138033921,-7.80284299793858,-7.73325471975515,
-7.6705356287488,-7.63244458781466,-7.58491672932839,-7.51108418160777,
-7.45258680549647,-7.37981951316885,-7.32053733326194,-7.28338074337444,
-7.2439083516446,-7.16581840375805,-7.10623786727216,-6.99361175932215,
-6.94138128277694,-6.90510911230878,-6.82112971419231,-6.76008840114547,
-6.63941157246137,-6.61588393384177,-6.58241383775098,-6.52780156363633,
-6.46035964173157,-6.40351868950041,-6.31168471996753,-6.24706609050832,
-6.2124428079742,-6.12588788695974,-6.06419368677298,-5.94075834738571,
-5.89452728609497,-5.85512965052663,-5.77413146740684,-5.71382525966102,
-5.59389389757059,-5.57049885079202,-5.53710218161794,-5.47763050823255,
-5.41261884996788,-5.35639726446858,-5.28316424821052,-5.22801481061597,
-5.19202016590582,-5.08111441265303,-5.01923283027586,-4.9515521806941,
-4.86795926594443,-4.85351588792323,-4.81890838662932,-4.7323315443045,
-4.6706319387406,-4.660704216232),.UNSPECIFIED.);
#2950=B_SPLINE_CURVE_WITH_KNOTS('',3,(#23680,#23681,#23682,#23683,#23684,
#23685,#23686,#23687,#23688,#23689,#23690,#23691,#23692,#23693,#23694,#23695,
#23696,#23697,#23698,#23699,#23700,#23701,#23702,#23703,#23704,#23705,#23706,
#23707,#23708,#23709,#23710,#23711,#23712,#23713,#23714,#23715,#23716,#23717,
#23718,#23719,#23720,#23721,#23722,#23723,#23724,#23725,#23726,#23727,#23728,
#23729,#23730,#23731,#23732,#23733,#23734,#23735,#23736,#23737,#23738,#23739,
#23740,#23741,#23742,#23743,#23744,#23745,#23746,#23747,#23748,#23749,#23750,
#23751,#23752,#23753,#23754,#23755,#23756,#23757,#23758,#23759,#23760,#23761,
#23762,#23763,#23764,#23765,#23766,#23767,#23768,#23769,#23770,#23771,#23772,
#23773,#23774,#23775,#23776,#23777,#23778,#23779,#23780,#23781,#23782,#23783,
#23784,#23785,#23786,#23787,#23788,#23789,#23790,#23791,#23792,#23793,#23794,
#23795,#23796,#23797,#23798,#23799,#23800,#23801,#23802,#23803,#23804,#23805,
#23806,#23807,#23808,#23809,#23810,#23811),.UNSPECIFIED.,.F.,.F.,(4,2,2,
2,2,2,2,2,2,2,2,2,2,2,2,2,2,2,2,2,2,2,2,2,2,2,2,2,2,2,2,2,2,2,2,2,2,2,2,
2,2,2,2,2,2,2,2,2,2,2,2,2,2,2,2,2,2,2,2,2,2,2,2,2,2,4),(-4.16138304547812,
-4.10880352144696,-4.04805008561075,-3.96523095703559,-3.92757479253391,
-3.87734452415319,-3.7613557865919,-3.70123826662044,-3.62100074986933,
-3.58082982128405,-3.53586596392477,-3.40982075028046,-3.34742356816844,
-3.23988682517842,-3.20580322670447,-3.15728421195415,-3.07244360287468,
-3.01596606526195,-2.94994473558394,-2.89376227702972,-2.8609918600829,
-2.83875677645363,-2.713177381296,-2.65091225920373,-2.54277365518383,-2.50846622597842,
-2.4591702484774,-2.37584352543414,-2.31943100330132,-2.25366876917332,
-2.1966509079333,-2.16373525390199,-2.07714140578139,-2.01407762942821,
-1.94966166227699,-1.86723904862984,-1.83330977350635,-1.76858209765694,
-1.67797231069848,-1.62119634461225,-1.55401342392953,-1.49980315704946,
-1.4668438961061,-1.44425152277379,-1.32007145222321,-1.25818624235187,
-1.14729443100237,-1.11131094387604,-1.05620309810477,-0.982935406714329,
-0.926724669947922,-0.861764380026687,-0.802118393454944,-0.768681882116029,
-0.745216402820036,-0.624295447520146,-0.563199493245989,-0.479013994167103,
-0.442911235281126,-0.415516240580332,-0.362141659965845,-0.286147608388949,
-0.233496139249837,-0.125746681025646,-0.0941040473628391,-0.000106119371468615),
 .UNSPECIFIED.);
#2951=B_SPLINE_CURVE_WITH_KNOTS('',3,(#23812,#23813,#23814,#23815,#23816,
#23817,#23818,#23819,#23820,#23821,#23822,#23823,#23824,#23825,#23826,#23827),
 .UNSPECIFIED.,.F.,.F.,(4,3,3,3,3,4),(26.4418509198543,26.522072587646,
26.6022987878389,26.6825236672068,26.7627664191034,26.7975893262247),
 .UNSPECIFIED.);
#2952=B_SPLINE_CURVE_WITH_KNOTS('',3,(#23828,#23829,#23830,#23831,#23832,
#23833,#23834,#23835,#23836,#23837,#23838,#23839,#23840,#23841,#23842,#23843,
#23844,#23845,#23846,#23847,#23848,#23849,#23850,#23851,#23852,#23853,#23854,
#23855,#23856,#23857,#23858,#23859,#23860,#23861,#23862,#23863,#23864,#23865,
#23866,#23867,#23868,#23869,#23870,#23871,#23872,#23873,#23874,#23875,#23876,
#23877,#23878,#23879,#23880,#23881,#23882,#23883,#23884,#23885,#23886,#23887,
#23888,#23889,#23890,#23891,#23892,#23893,#23894,#23895,#23896,#23897,#23898,
#23899,#23900,#23901,#23902,#23903,#23904,#23905,#23906,#23907,#23908,#23909,
#23910,#23911,#23912,#23913,#23914,#23915,#23916,#23917,#23918,#23919,#23920,
#23921,#23922,#23923,#23924,#23925,#23926,#23927,#23928,#23929,#23930,#23931,
#23932,#23933,#23934,#23935,#23936,#23937,#23938,#23939,#23940,#23941,#23942,
#23943,#23944,#23945,#23946,#23947,#23948,#23949,#23950,#23951,#23952,#23953,
#23954,#23955,#23956,#23957,#23958,#23959,#23960,#23961,#23962,#23963,#23964,
#23965,#23966,#23967,#23968,#23969,#23970,#23971,#23972,#23973,#23974,#23975),
 .UNSPECIFIED.,.F.,.F.,(4,2,2,2,2,2,2,2,2,2,2,2,2,2,2,2,2,2,2,2,2,2,2,2,
2,2,2,2,2,2,2,2,2,2,2,2,2,2,2,2,2,2,2,2,2,2,2,2,2,2,2,2,2,2,2,2,2,2,2,2,
2,2,2,2,2,2,2,2,2,2,2,2,2,4),(-4.660704216232,-4.54717480836569,-4.52439802262577,
-4.49134032769968,-4.41095770906608,-4.33846805041116,-4.28202925163412,
-4.21615621482939,-4.15950699887394,-4.12665741613199,-4.08257226621711,
-3.98859124966383,-3.931639734452,-3.8637717708191,-3.8088144078729,-3.77453866438938,
-3.72535087666706,-3.64181968159527,-3.58539993883686,-3.51960524249073,
-3.46269887573972,-3.42980362476136,-3.38554825092803,-3.29191886988205,
-3.23498348594814,-3.16718122252458,-3.11225612445079,-3.07810177585851,
-3.02933756822755,-2.94497659794237,-2.88851973318813,-2.82258247217076,
-2.76612709165884,-2.73330995681478,-2.66158730669186,-2.59494606351099,
-2.53791946566919,-2.46976809087832,-2.41473488817004,-2.37996583558301,
-2.32907305363151,-2.24874533318724,-2.1924410454408,-2.12710903943484,
-2.06868969505259,-2.0355088158653,-1.9472743563323,-1.88471530185778,-1.8181228971323,
-1.73537908631784,-1.70329384084289,-1.58051101535088,-1.52975767095848,
-1.44746322211503,-1.3730957337222,-1.34052211829442,-1.25387596864685,
-1.19030967730142,-1.12641693492717,-1.04155617290932,-1.00816851100997,
-0.875070668338063,-0.820273992003613,-0.793332950341518,-0.722356942616175,
-0.67273142763783,-0.637974179999183,-0.587120874394874,-0.506724252010099,
-0.453316858963204,-0.390466277726096,-0.328215731381091,-0.296710621679306,
-0.249923280266006),.UNSPECIFIED.);
#2953=B_SPLINE_CURVE_WITH_KNOTS('',3,(#23980,#23981,#23982,#23983,#23984,
#23985,#23986,#23987,#23988,#23989,#23990,#23991,#23992,#23993,#23994,#23995,
#23996,#23997,#23998,#23999,#24000,#24001,#24002,#24003,#24004,#24005,#24006,
#24007,#24008,#24009,#24010,#24011,#24012,#24013,#24014,#24015,#24016,#24017,
#24018,#24019,#24020,#24021,#24022,#24023,#24024,#24025,#24026,#24027,#24028,
#24029,#24030,#24031,#24032,#24033,#24034,#24035,#24036,#24037,#24038,#24039,
#24040,#24041,#24042,#24043,#24044,#24045,#24046,#24047,#24048,#24049,#24050,
#24051,#24052,#24053,#24054,#24055,#24056,#24057,#24058,#24059,#24060,#24061,
#24062,#24063,#24064,#24065,#24066,#24067,#24068,#24069,#24070,#24071,#24072,
#24073,#24074,#24075,#24076,#24077,#24078,#24079,#24080,#24081,#24082,#24083,
#24084,#24085,#24086,#24087,#24088,#24089,#24090,#24091,#24092,#24093,#24094,
#24095,#24096,#24097,#24098,#24099,#24100,#24101,#24102,#24103,#24104,#24105,
#24106,#24107,#24108,#24109,#24110,#24111,#24112,#24113,#24114,#24115,#24116,
#24117,#24118,#24119,#24120,#24121,#24122,#24123,#24124,#24125,#24126,#24127),
 .UNSPECIFIED.,.F.,.F.,(4,2,2,2,2,2,2,2,2,2,2,2,2,2,2,2,2,2,2,2,2,2,2,2,
2,2,2,2,2,2,2,2,2,2,2,2,2,2,2,2,2,2,2,2,2,2,2,2,2,2,2,2,2,2,2,2,2,2,2,2,
2,2,2,2,2,2,2,2,2,2,2,2,2,4),(-8.57207326543173,-8.52540157720413,-8.48258196231714,
-8.45354508349237,-8.40816043619921,-8.32814767430087,-8.27172870728119,
-8.18823972312311,-8.13903307648575,-8.104751464036,-7.99668303756801,-7.93440105020989,
-7.80876681606068,-7.78654819712475,-7.75378653899148,-7.69977967941424,
-7.63269438177325,-7.57594519780263,-7.48580263904452,-7.42151370133059,
-7.38811004137267,-7.30325416509756,-7.23938405597625,-7.17580111269242,
-7.08904419035894,-7.05652048815099,-7.00189634746641,-6.9353791069696,
-6.8787756658092,-6.79136222217601,-6.72539664972693,-6.69233904816397,
-6.60740205800124,-6.54309020535531,-6.47865734322217,-6.39324180946986,
-6.37786536766714,-6.34521886813112,-6.26251897439032,-6.19636468789063,
-6.13350594686396,-6.04579945998549,-6.01266771602776,-5.95830159661692,
-5.89103040409763,-5.83423267327737,-5.74321587174528,-5.68184083926186,
-5.64992581521011,-5.56715567188756,-5.50022934259423,-5.43789336089576,
-5.34936433787834,-5.31612168526708,-5.26166689922114,-5.19433972773177,
-5.13752754186971,-5.04624537886821,-4.98104132260954,-4.94632315303402,
-4.86456245237656,-4.80073608887504,-4.73710628141658,-4.65010069051738,
-4.61767551275871,-4.55556568905253,-4.49267278742941,-4.46668244678827,
-4.41110587693669,-4.34647792101919,-4.28573190276621,-4.25204675379642,
-4.22813653827197,-4.16138304547812),.UNSPECIFIED.);
#2954=B_SPLINE_CURVE_WITH_KNOTS('',3,(#24129,#24130,#24131,#24132,#24133,
#24134,#24135,#24136),.UNSPECIFIED.,.F.,.F.,(4,2,2,4),(-0.249923280266006,
-0.171457320855668,-0.119217469302637,-0.000106124780310168),
 .UNSPECIFIED.);
#2955=B_SPLINE_CURVE_WITH_KNOTS('',3,(#24137,#24138,#24139,#24140,#24141,
#24142,#24143,#24144,#24145,#24146,#24147,#24148,#24149,#24150,#24151,#24152,
#24153,#24154,#24155,#24156,#24157,#24158,#24159,#24160,#24161,#24162,#24163,
#24164,#24165,#24166,#24167,#24168,#24169,#24170,#24171,#24172,#24173,#24174,
#24175,#24176,#24177,#24178,#24179,#24180,#24181,#24182,#24183,#24184,#24185,
#24186,#24187,#24188,#24189,#24190,#24191,#24192,#24193,#24194,#24195,#24196,
#24197,#24198,#24199,#24200,#24201,#24202,#24203,#24204,#24205,#24206,#24207,
#24208,#24209,#24210,#24211,#24212,#24213,#24214,#24215,#24216,#24217,#24218,
#24219,#24220,#24221,#24222,#24223,#24224,#24225,#24226,#24227,#24228,#24229,
#24230,#24231,#24232,#24233,#24234,#24235,#24236,#24237,#24238,#24239,#24240,
#24241,#24242,#24243,#24244,#24245,#24246,#24247,#24248,#24249,#24250,#24251,
#24252,#24253,#24254,#24255,#24256,#24257,#24258,#24259,#24260,#24261,#24262,
#24263,#24264,#24265,#24266,#24267,#24268,#24269,#24270,#24271,#24272,#24273,
#24274,#24275,#24276,#24277,#24278,#24279,#24280,#24281,#24282,#24283,#24284,
#24285,#24286,#24287,#24288,#24289,#24290,#24291,#24292,#24293,#24294,#24295,
#24296,#24297,#24298,#24299,#24300,#24301,#24302,#24303,#24304,#24305,#24306,
#24307,#24308,#24309,#24310,#24311,#24312,#24313,#24314,#24315,#24316,#24317,
#24318,#24319,#24320,#24321,#24322,#24323,#24324,#24325,#24326,#24327,#24328,
#24329,#24330,#24331,#24332,#24333,#24334,#24335,#24336,#24337,#24338,#24339,
#24340,#24341,#24342,#24343,#24344,#24345,#24346,#24347,#24348,#24349,#24350,
#24351,#24352,#24353,#24354,#24355,#24356,#24357,#24358,#24359,#24360,#24361,
#24362,#24363,#24364,#24365,#24366,#24367,#24368,#24369,#24370,#24371,#24372,
#24373,#24374,#24375,#24376,#24377,#24378,#24379,#24380,#24381,#24382,#24383,
#24384,#24385,#24386,#24387,#24388,#24389),.UNSPECIFIED.,.F.,.F.,(4,3,3,
3,3,3,3,3,3,3,3,3,3,3,3,3,3,3,3,3,3,3,3,3,3,3,3,3,3,3,3,3,3,3,3,3,3,3,3,
3,3,3,3,3,3,3,3,3,3,3,3,3,3,3,3,3,3,3,3,3,3,3,3,3,3,3,3,3,3,3,3,3,3,3,3,
3,3,3,3,3,3,3,3,3,4),(-16.4194260685698,-16.3770530376352,-16.2966374559875,
-16.2162369324569,-16.132372375133,-16.0519743325897,-15.9715754672898,
-15.8911606929121,-15.8807787031614,-15.8003631215144,-15.7199625979849,
-15.6360980406606,-15.555699998118,-15.4753011328189,-15.394886358442,-15.3845043686876,
-15.3040887870402,-15.2236882635099,-15.1398237061858,-15.0594256636427,
-14.9790267983431,-14.8986120239656,-14.8882300342138,-14.8078144525681,
-14.7274139290397,-14.6435493717148,-14.5631513291734,-14.4827524638757,
-14.4023376895001,-14.39195569974,-14.311540118089,-14.2311395945552,-14.147275037233,
-14.0668769946863,-13.9864781293833,-13.9060633550023,-13.8956813652663,
-13.8152657836274,-13.7348652601058,-13.6510007027774,-13.5706026602428,
-13.4902037949517,-13.4097890205825,-13.3994070307925,-13.3189914491325,
-13.2385909255897,-13.154726368272,-13.0743283257164,-12.9939294604045,
-12.913514686015,-12.9031326963187,-12.8227171146844,-12.7423165911674,
-12.6584520338368,-12.5780539913066,-12.4976551260199,-12.417240351655,
-12.4068583618449,-12.3264427802026,-12.2460422566776,-12.162177699351,
-12.0817796568132,-12.0013807915192,-11.9209660171472,-11.9105840273711,
-11.8301684456594,-11.7497679220645,-11.6659033647727,-11.585505322165,
-11.5051064568015,-11.4246916823607,-11.4143096928973,-11.3338941114529,
-11.2534935881266,-11.1696290307009,-11.0892309883605,-11.0088321232625,
-10.9284173490835,-10.9180353584235,-10.8376204161101,-10.7572207940968,
-10.676823409421,-10.5964311048214,-10.5160291436,-10.4919945899008),
 .UNSPECIFIED.);
#2956=B_SPLINE_CURVE_WITH_KNOTS('',3,(#24395,#24396,#24397,#24398,#24399),
 .UNSPECIFIED.,.F.,.F.,(4,1,4),(-4.20879728873375,-3.97019467579036,-3.85305545639561),
 .UNSPECIFIED.);
#2957=B_SPLINE_CURVE_WITH_KNOTS('',3,(#24401,#24402,#24403,#24404,#24405,
#24406,#24407,#24408,#24409,#24410,#24411,#24412,#24413,#24414,#24415,#24416,
#24417,#24418,#24419,#24420,#24421,#24422,#24423,#24424,#24425,#24426,#24427,
#24428,#24429,#24430,#24431,#24432,#24433,#24434,#24435,#24436,#24437,#24438,
#24439,#24440,#24441,#24442,#24443,#24444,#24445,#24446,#24447,#24448,#24449,
#24450,#24451,#24452,#24453,#24454,#24455,#24456,#24457,#24458,#24459,#24460,
#24461,#24462,#24463,#24464,#24465,#24466,#24467,#24468,#24469,#24470,#24471,
#24472,#24473,#24474,#24475,#24476,#24477,#24478,#24479,#24480,#24481,#24482,
#24483,#24484,#24485,#24486,#24487,#24488,#24489,#24490,#24491,#24492,#24493,
#24494,#24495,#24496,#24497,#24498,#24499,#24500,#24501,#24502,#24503,#24504,
#24505,#24506,#24507,#24508,#24509,#24510,#24511,#24512,#24513,#24514,#24515,
#24516,#24517,#24518,#24519,#24520,#24521,#24522,#24523,#24524,#24525,#24526,
#24527,#24528,#24529,#24530,#24531,#24532,#24533,#24534,#24535,#24536,#24537,
#24538,#24539,#24540,#24541,#24542,#24543,#24544,#24545,#24546,#24547,#24548,
#24549,#24550,#24551,#24552,#24553,#24554,#24555,#24556,#24557,#24558,#24559,
#24560),.UNSPECIFIED.,.F.,.F.,(4,3,3,3,3,3,3,3,3,3,3,3,3,3,3,3,3,3,3,3,
3,3,3,3,3,3,3,3,3,3,3,3,3,3,3,3,3,3,3,3,3,3,3,3,3,3,3,3,3,3,3,3,3,4),(-3.85305545421067,
-3.77291964238566,-3.69278153984504,-3.61264712623592,-3.53249330145913,
-3.47392034131656,-3.39350856937354,-3.31311185551211,-3.22924539334477,
-3.14885109862192,-3.06845594440698,-2.98804480902414,-2.97764600684277,
-2.89723194483455,-2.81683297413262,-2.73296764869171,-2.65257121471742,
-2.5721739704636,-2.4917608250185,-2.48137167236897,-2.40093647695799,-2.32051622613262,
-2.23666150407326,-2.15624377821962,-2.07582532646403,-1.99539121234268,
-1.98509733789518,-1.90474324759607,-1.82440447274427,-1.74050910541355,
-1.66017244479229,-1.57983458393119,-1.4994799427304,-1.48882300342138,
-1.40826740291856,-1.32772640753817,-1.24393197289052,-1.16339467572715,
-1.08285756497712,-1.00230674301718,-0.99254866894759,-0.912388322686476,
-0.832243389392974,-0.748251125663179,-0.668105491870725,-0.587956937046544,
-0.507788147193865,-0.496274334473794,-0.415365456522927,-0.334472363569503,
-0.250854272677127,-0.169974037999006,-0.0849870189995029,0.),
 .UNSPECIFIED.);
#2958=B_SPLINE_CURVE_WITH_KNOTS('',3,(#24563,#24564,#24565,#24566,#24567,
#24568,#24569,#24570,#24571,#24572,#24573,#24574,#24575,#24576,#24577,#24578,
#24579,#24580,#24581,#24582,#24583,#24584,#24585,#24586,#24587,#24588,#24589,
#24590,#24591,#24592,#24593,#24594,#24595,#24596,#24597,#24598,#24599,#24600,
#24601,#24602,#24603,#24604,#24605,#24606,#24607,#24608,#24609,#24610,#24611,
#24612,#24613,#24614,#24615,#24616,#24617,#24618,#24619,#24620,#24621,#24622,
#24623,#24624,#24625,#24626,#24627,#24628,#24629,#24630,#24631,#24632,#24633,
#24634,#24635,#24636,#24637,#24638,#24639,#24640,#24641,#24642,#24643,#24644,
#24645,#24646,#24647,#24648,#24649,#24650,#24651,#24652,#24653,#24654,#24655,
#24656,#24657,#24658,#24659,#24660,#24661,#24662,#24663,#24664,#24665,#24666,
#24667,#24668,#24669,#24670,#24671,#24672,#24673,#24674,#24675,#24676,#24677,
#24678,#24679,#24680,#24681,#24682,#24683,#24684,#24685,#24686,#24687,#24688,
#24689,#24690,#24691,#24692,#24693,#24694,#24695,#24696,#24697,#24698,#24699,
#24700),.UNSPECIFIED.,.F.,.F.,(4,2,2,2,2,2,2,2,2,2,2,2,2,2,2,2,2,2,2,2,
2,2,2,2,2,2,2,2,2,2,2,2,2,2,2,2,2,2,2,2,2,2,2,2,2,2,2,2,2,2,2,2,2,2,2,2,
2,2,2,2,2,2,2,2,2,2,2,2,4),(-8.32193337931491,-8.19665781353201,-8.1427529639967,
-8.02220072731463,-7.99255198247967,-7.94385232850661,-7.87303717104052,
-7.82270695671389,-7.69679462639956,-7.67463489572474,-7.6419389575693,
-7.58786118762996,-7.52072419252838,-7.46394288169517,-7.37415689321913,
-7.30823185140564,-7.27385373582285,-7.19183114545146,-7.12772906426362,
-7.06306346937112,-6.97762663172909,-6.94495075490186,-6.88928089675609,
-6.8230946558089,-6.76657808334903,-6.69760602277879,-6.63903708717948,
-6.60207759364124,-6.56362835461421,-6.48500962592191,-6.42528878653741,
-6.35583897708348,-6.2928149402416,-6.25464003254163,-6.20734561495133,
-6.13334845796692,-6.07480848589869,-6.01432373401582,-5.9465127727114,
-5.90709862009578,-5.86436758857633,-5.77267610384581,-5.74681023095454,
-5.69007100024129,-5.56944863910889,-5.53738516985327,-5.45463390315573,
-5.38799611725067,-5.32546887649081,-5.23719453118219,-5.20400494179616,
-5.14958925729567,-5.08228560596609,-5.02547738868342,-4.9343210120028,
-4.87303275504826,-4.84110725070179,-4.7583339931184,-4.69142205281254,
-4.62907103673601,-4.54055340354179,-4.50731238809251,-4.44858947671009,
-4.38334647012783,-4.32706453012634,-4.24752462083681,-4.19620040999603,
-4.16130608063852,-4.16130056038158),.UNSPECIFIED.);
#2959=B_SPLINE_CURVE_WITH_KNOTS('',3,(#24703,#24704,#24705,#24706,#24707,
#24708,#24709,#24710,#24711,#24712,#24713,#24714,#24715,#24716,#24717,#24718,
#24719,#24720,#24721,#24722,#24723,#24724,#24725,#24726,#24727,#24728,#24729,
#24730,#24731,#24732,#24733,#24734,#24735,#24736,#24737,#24738,#24739,#24740,
#24741,#24742,#24743,#24744,#24745,#24746,#24747,#24748,#24749,#24750,#24751,
#24752,#24753,#24754,#24755,#24756,#24757,#24758,#24759,#24760,#24761,#24762,
#24763,#24764,#24765,#24766,#24767,#24768,#24769,#24770,#24771,#24772,#24773,
#24774,#24775,#24776,#24777,#24778,#24779,#24780,#24781,#24782,#24783,#24784,
#24785,#24786,#24787,#24788,#24789,#24790,#24791,#24792,#24793,#24794,#24795,
#24796,#24797,#24798,#24799,#24800,#24801,#24802,#24803,#24804,#24805,#24806,
#24807,#24808,#24809,#24810,#24811,#24812,#24813,#24814,#24815,#24816,#24817,
#24818,#24819,#24820,#24821,#24822,#24823,#24824,#24825,#24826,#24827,#24828,
#24829,#24830,#24831,#24832,#24833,#24834),.UNSPECIFIED.,.F.,.F.,(4,2,2,
2,2,2,2,2,2,2,2,2,2,2,2,2,2,2,2,2,2,2,2,2,2,2,2,2,2,2,2,2,2,2,2,2,2,2,2,
2,2,2,2,2,2,2,2,2,2,2,2,2,2,2,2,2,2,2,2,2,2,2,2,2,2,4),(-4.16130056038158,
-4.14695393791753,-4.06352973478219,-3.99548150715283,-3.93379535980784,
-3.84727841182617,-3.81262648858228,-3.74894939215065,-3.65595505377096,
-3.59905127916525,-3.53137331181627,-3.47652887803669,-3.44260623387991,
-3.41827850791444,-3.30037702990747,-3.23990795474275,-3.15825244353961,
-3.11950337566717,-3.07200793984769,-2.95226383378267,-2.89199586497062,
-2.81115409710204,-2.77160112118748,-2.72564150774563,-2.60165031294345,
-2.5398150447074,-2.44638631193077,-2.41429831063311,-2.35007478735879,
-2.26329695406303,-2.20672615451093,-2.14033861576261,-2.08531481131674,
-2.05272994009653,-1.96611697937537,-1.90191556761914,-1.83736857855361,
-1.75492110859993,-1.72110895505862,-1.70636375952528,-1.62121747498458,
-1.55519381364485,-1.49224145259603,-1.40074251949297,-1.36878041841618,
-1.30285834918699,-1.21855005778575,-1.162097566399,-1.0961716147161,-1.03968999970123,
-1.00686929024496,-0.962893811918559,-0.868682850224344,-0.811720046912751,
-0.743809316271993,-0.688833908848399,-0.654481905197044,-0.605029867622139,
-0.522007255792696,-0.469543740804877,-0.407196423362226,-0.343212260589455,
-0.312139103092669,-0.206243036740045,-0.149073400185228,-0.000110996093532989),
 .UNSPECIFIED.);
#2960=B_SPLINE_CURVE_WITH_KNOTS('',3,(#24835,#24836,#24837,#24838,#24839,
#24840,#24841,#24842,#24843,#24844,#24845,#24846),.UNSPECIFIED.,.F.,.F.,
(4,2,2,2,2,4),(-8.82178672303514,-8.79444566643878,-8.74517120012775,-8.67475029100605,
-8.62305989272208,-8.57207326543173),.UNSPECIFIED.);
#2961=B_SPLINE_CURVE_WITH_KNOTS('',3,(#24848,#24849,#24850,#24851,#24852,
#24853,#24854,#24855,#24856,#24857,#24858,#24859,#24860,#24861,#24862,#24863),
 .UNSPECIFIED.,.F.,.F.,(4,3,3,3,3,4),(-10.4919945899008,-10.4217610239497,
-10.3408897465942,-10.2600358481682,-10.1791909548845,-10.1362407613903),
 .UNSPECIFIED.);
#2962=B_SPLINE_CURVE_WITH_KNOTS('',3,(#24864,#24865,#24866,#24867,#24868,
#24869,#24870,#24871,#24872,#24873,#24874,#24875,#24876,#24877,#24878,#24879),
 .UNSPECIFIED.,.F.,.F.,(4,1,1,1,1,1,1,1,1,1,1,1,1,4),(-10.1362407381615,
-9.92548668947589,-9.4292123550021,-8.9329380205283,-8.43666368605451,-7.94038935158072,
-7.44411501710692,-6.94784068263312,-6.45156634815933,-5.95529201368554,
-5.45901767921174,-4.96274334473795,-4.46646901026415,-4.20879728873375),
 .UNSPECIFIED.);
#2963=B_SPLINE_CURVE_WITH_KNOTS('',3,(#24882,#24883,#24884,#24885,#24886,
#24887,#24888,#24889,#24890,#24891,#24892,#24893,#24894,#24895,#24896,#24897,
#24898,#24899,#24900,#24901,#24902,#24903,#24904,#24905,#24906,#24907,#24908,
#24909,#24910,#24911,#24912,#24913,#24914,#24915,#24916,#24917,#24918,#24919,
#24920,#24921,#24922,#24923,#24924,#24925,#24926,#24927,#24928,#24929,#24930,
#24931,#24932,#24933,#24934,#24935,#24936,#24937,#24938,#24939,#24940,#24941,
#24942,#24943,#24944,#24945,#24946,#24947,#24948,#24949,#24950,#24951,#24952,
#24953,#24954,#24955,#24956,#24957,#24958,#24959,#24960,#24961,#24962,#24963,
#24964,#24965,#24966,#24967,#24968,#24969,#24970,#24971,#24972,#24973,#24974,
#24975,#24976,#24977,#24978,#24979,#24980,#24981,#24982,#24983,#24984,#24985,
#24986,#24987,#24988,#24989,#24990,#24991,#24992,#24993,#24994,#24995,#24996,
#24997,#24998,#24999,#25000,#25001,#25002,#25003,#25004,#25005,#25006,#25007,
#25008,#25009,#25010,#25011,#25012,#25013,#25014,#25015,#25016,#25017,#25018,
#25019,#25020,#25021,#25022,#25023,#25024,#25025,#25026,#25027,#25028,#25029,
#25030,#25031,#25032,#25033,#25034,#25035,#25036,#25037,#25038,#25039,#25040,
#25041,#25042,#25043,#25044,#25045,#25046,#25047,#25048,#25049,#25050,#25051,
#25052,#25053),.UNSPECIFIED.,.F.,.F.,(4,3,3,3,3,3,3,3,3,3,3,3,3,3,3,3,3,
3,3,3,3,3,3,3,3,3,3,3,3,3,3,3,3,3,3,3,3,3,3,3,3,3,3,3,3,3,3,3,3,3,3,3,3,
3,3,3,3,4),(17.9333380487234,18.0108233197382,18.0883135892053,18.1658013598437,
18.2433074384587,18.3064741618976,18.3839791341702,18.4614700138817,18.538952337374,
18.6164408059227,18.6939290593022,18.7714334678537,18.8027484963714,18.8802535677613,
18.9577445479216,19.0352269728638,19.1127155435947,19.1902038993907,19.2677084100512,
19.2990228308452,19.3765278382868,19.454018753699,19.5315011133061,19.6089896183162,
19.6864779082904,19.7639823534002,19.7952971653189,19.8728022043913,19.9502931518055,
20.027775543681,20.1052640811144,20.1827524035413,20.2602568809398,20.2915714997927,
20.369076527175,20.4465674627749,20.5240498427505,20.6015383682459,20.6790266787349,
20.7565311442723,20.7878458342665,20.8653508638495,20.9428418016642,21.0203241838615,
21.097812711572,21.1753010242683,21.2528054919869,21.2841201687403,21.3616251994293,
21.4391161383701,21.51659852171,21.5940870505792,21.6715753644414,21.7490798333289,
21.7803945032141,21.8595346027181,21.9386551930325,21.9911485717322),
 .UNSPECIFIED.);
#2964=B_SPLINE_CURVE_WITH_KNOTS('',3,(#25054,#25055,#25056,#25057,#25058,
#25059,#25060,#25061),.UNSPECIFIED.,.F.,.F.,(4,1,1,1,1,4),(21.9911485751285,
22.2766688376879,22.7729431721617,23.2692175066355,23.7654918411093,24.2164925491897),
 .UNSPECIFIED.);
#2965=B_SPLINE_CURVE_WITH_KNOTS('',3,(#25063,#25064,#25065,#25066,#25067,
#25068,#25069,#25070,#25071,#25072,#25073,#25074,#25075,#25076,#25077,#25078,
#25079,#25080,#25081,#25082,#25083,#25084,#25085,#25086,#25087,#25088,#25089,
#25090,#25091,#25092,#25093,#25094,#25095,#25096,#25097,#25098,#25099,#25100,
#25101,#25102,#25103,#25104,#25105,#25106,#25107,#25108,#25109,#25110,#25111,
#25112,#25113,#25114,#25115,#25116,#25117,#25118,#25119,#25120,#25121,#25122,
#25123,#25124,#25125,#25126,#25127,#25128,#25129,#25130,#25131,#25132,#25133,
#25134,#25135,#25136,#25137,#25138,#25139,#25140,#25141,#25142,#25143,#25144,
#25145,#25146,#25147,#25148,#25149,#25150,#25151,#25152,#25153,#25154,#25155,
#25156),.UNSPECIFIED.,.F.,.F.,(4,3,3,3,3,3,3,3,3,3,3,3,3,3,3,3,3,3,3,3,
3,3,3,3,3,3,3,3,3,3,3,4),(21.9911485751285,22.0685137227498,22.14588444626,
22.2232545020621,22.3006419241412,22.3392429283936,22.416747967466,22.4942389148803,
22.571721306756,22.6492098441894,22.7266981666165,22.804202644015,22.8355172628674,
22.9130222902497,22.9905132258493,23.0679956058247,23.1454841313203,23.2229724418092,
23.3004769073466,23.3317915973412,23.4092966269243,23.486787564739,23.5642699469356,
23.641758474646,23.7192467873425,23.7967512550612,23.828065931815,23.9055702049626,
23.9833003073723,24.0607857874918,24.1386382010467,24.2164906146016),
 .UNSPECIFIED.);
#2966=B_SPLINE_CURVE_WITH_KNOTS('',3,(#25157,#25158,#25159,#25160,#25161,
#25162,#25163,#25164,#25165,#25166,#25167,#25168),.UNSPECIFIED.,.F.,.F.,
(4,1,1,1,1,1,1,1,1,4),(17.9333400728794,18.3690482526032,18.865322587077,
19.3615969215508,19.8578712560246,20.3541455904984,20.8504199249722,21.346694259446,
21.8429685939198,21.9911485487957),.UNSPECIFIED.);
#2967=B_SPLINE_CURVE_WITH_KNOTS('',3,(#25805,#25806,#25807,#25808,#25809,
#25810,#25811,#25812,#25813,#25814,#25815,#25816,#25817,#25818,#25819,#25820,
#25821,#25822,#25823,#25824,#25825,#25826,#25827,#25828,#25829,#25830,#25831,
#25832,#25833,#25834,#25835,#25836,#25837,#25838,#25839,#25840,#25841,#25842,
#25843,#25844,#25845,#25846,#25847,#25848,#25849,#25850,#25851,#25852,#25853,
#25854,#25855,#25856,#25857,#25858,#25859,#25860,#25861,#25862,#25863,#25864,
#25865,#25866,#25867,#25868,#25869,#25870,#25871,#25872,#25873,#25874,#25875,
#25876,#25877,#25878,#25879,#25880,#25881,#25882,#25883,#25884,#25885,#25886,
#25887,#25888,#25889,#25890,#25891,#25892,#25893,#25894,#25895,#25896,#25897,
#25898,#25899,#25900,#25901,#25902,#25903,#25904,#25905,#25906,#25907,#25908,
#25909,#25910,#25911,#25912,#25913),.UNSPECIFIED.,.F.,.F.,(4,3,3,3,3,3,
3,3,3,3,3,3,3,3,3,3,3,3,3,3,3,3,3,3,3,3,3,3,3,3,3,3,3,3,3,3,4),(0.,0.0625573555055976,
0.125878327368043,0.18909072172842,0.251393671417134,0.304922771869898,
0.312525381797511,0.319603549735867,0.381466347527152,0.398722998462767,
0.460761132960107,0.522788946210543,0.584119984043925,0.609251897050035,
0.616406215049582,0.623860834291625,0.684593333574402,0.744931857036463,
0.784341213415679,0.847163709339813,0.909986205263948,0.918319049054216,
0.97788433880908,1.03729699480677,1.09693860144022,1.15658020807367,1.18303706385244,
1.19757756249814,1.20796090274694,1.26646558172373,1.3247313868406,1.36823505430382,
1.37738657121944,1.43493464047012,1.49171401465407,1.51467421871742,1.53973642054055),
 .UNSPECIFIED.);
#2968=B_SPLINE_CURVE_WITH_KNOTS('',3,(#25914,#25915,#25916,#25917,#25918,
#25919,#25920,#25921,#25922,#25923,#25924,#25925,#25926,#25927,#25928,#25929,
#25930,#25931,#25932,#25933,#25934,#25935,#25936,#25937,#25938,#25939,#25940,
#25941,#25942,#25943,#25944,#25945,#25946,#25947,#25948,#25949,#25950,#25951,
#25952,#25953,#25954,#25955,#25956,#25957,#25958,#25959,#25960,#25961,#25962,
#25963,#25964,#25965,#25966,#25967,#25968,#25969,#25970,#25971,#25972,#25973,
#25974,#25975,#25976,#25977,#25978,#25979,#25980,#25981,#25982,#25983,#25984,
#25985,#25986,#25987,#25988,#25989,#25990,#25991,#25992,#25993,#25994,#25995,
#25996,#25997,#25998,#25999,#26000,#26001,#26002,#26003,#26004,#26005,#26006,
#26007,#26008,#26009,#26010,#26011,#26012,#26013,#26014,#26015,#26016,#26017,
#26018,#26019,#26020,#26021,#26022,#26023,#26024,#26025,#26026,#26027,#26028,
#26029,#26030,#26031),.UNSPECIFIED.,.F.,.F.,(4,3,3,3,3,3,3,3,3,3,3,3,3,
3,3,3,3,3,3,3,3,3,3,3,3,3,3,3,3,3,3,3,3,3,3,3,3,3,3,4),(0.,0.0558770828944057,
0.113141002024866,0.170836081600947,0.226512310746881,0.254350425319848,
0.268269482606332,0.277344944194597,0.282188539892815,0.341010793961021,
0.356700869327603,0.414900143477246,0.473727786287952,0.532755410441651,
0.550847767022388,0.561747769745167,0.570285683041986,0.630075869297723,
0.690421239086179,0.726872796438621,0.786792026171573,0.847034073674744,
0.85453090427754,0.863944001987961,0.925525636112025,0.986994127643801,
1.04863233306401,1.11027053848422,1.15749615432221,1.16513297885951,1.22688035244015,
1.28927963589503,1.32015168917181,1.33465273393439,1.34439171958657,1.35395106897205,
1.4172068923124,1.4805171829652,1.50616871736932,1.53495510956274),
 .UNSPECIFIED.);
#2969=B_SPLINE_CURVE_WITH_KNOTS('',3,(#26668,#26669,#26670,#26671,#26672,
#26673,#26674,#26675,#26676,#26677,#26678,#26679,#26680,#26681,#26682,#26683,
#26684,#26685,#26686,#26687,#26688,#26689,#26690,#26691,#26692,#26693,#26694,
#26695,#26696,#26697,#26698,#26699,#26700,#26701,#26702,#26703,#26704,#26705,
#26706,#26707,#26708,#26709,#26710,#26711,#26712,#26713,#26714,#26715,#26716,
#26717,#26718,#26719,#26720,#26721,#26722,#26723,#26724,#26725,#26726,#26727,
#26728,#26729,#26730,#26731,#26732,#26733,#26734,#26735,#26736,#26737,#26738,
#26739,#26740,#26741,#26742,#26743,#26744,#26745,#26746,#26747,#26748,#26749,
#26750,#26751,#26752,#26753,#26754,#26755,#26756,#26757,#26758,#26759,#26760,
#26761,#26762,#26763,#26764,#26765,#26766,#26767,#26768,#26769,#26770,#26771,
#26772,#26773),.UNSPECIFIED.,.F.,.F.,(4,3,3,3,3,3,3,3,3,3,3,3,3,3,3,3,3,
3,3,3,3,3,3,3,3,3,3,3,3,3,3,3,3,3,3,4),(0.,0.0558602583733117,0.113102874179053,
0.170787757446949,0.228459514024139,0.275917418730984,0.284810036819283,
0.343644920942749,0.35670086932759,0.414962508627316,0.47376239878265,0.532768485616126,
0.557903354456782,0.567232860585173,0.62699085349851,0.687333251691766,
0.726872796438614,0.78679202603564,0.847034072316043,0.85453090427055,0.861553469994431,
0.923732737116866,0.985191220366593,1.04773087942538,1.11027053848417,1.15749615445995,
1.16513297888962,1.22688035264506,1.2892796358153,1.32015168909275,1.34459345495989,
1.35352159663707,1.41677518013709,1.48008662244226,1.50616871736924,1.53495770636289),
 .UNSPECIFIED.);
#2970=B_SPLINE_CURVE_WITH_KNOTS('',3,(#26775,#26776,#26777,#26778),
 .UNSPECIFIED.,.F.,.F.,(4,4),(-0.000938309331961322,0.),.UNSPECIFIED.);
#2971=B_SPLINE_CURVE_WITH_KNOTS('',3,(#26779,#26780,#26781,#26782,#26783,
#26784,#26785,#26786,#26787,#26788,#26789,#26790,#26791,#26792,#26793,#26794,
#26795,#26796,#26797,#26798,#26799,#26800,#26801,#26802,#26803,#26804,#26805,
#26806,#26807,#26808,#26809,#26810,#26811,#26812,#26813,#26814,#26815,#26816,
#26817,#26818,#26819,#26820,#26821,#26822,#26823,#26824,#26825,#26826,#26827,
#26828,#26829,#26830,#26831,#26832,#26833,#26834,#26835,#26836,#26837,#26838,
#26839,#26840,#26841,#26842,#26843,#26844,#26845,#26846,#26847,#26848,#26849,
#26850,#26851,#26852,#26853,#26854,#26855,#26856,#26857,#26858,#26859,#26860,
#26861,#26862,#26863,#26864,#26865,#26866,#26867,#26868,#26869,#26870,#26871,
#26872,#26873,#26874,#26875,#26876,#26877,#26878,#26879,#26880,#26881,#26882,
#26883,#26884,#26885,#26886,#26887,#26888,#26889,#26890,#26891,#26892,#26893),
 .UNSPECIFIED.,.F.,.F.,(4,3,3,3,3,3,3,3,3,3,3,3,3,3,3,3,3,3,3,3,3,3,3,3,
3,3,3,3,3,3,3,3,3,3,3,3,3,3,4),(8.32765479367532E-15,0.0625573555448621,
0.125878327380841,0.189090721668103,0.251393670961933,0.304922771867042,
0.312525381935688,0.319603549767331,0.38146634752137,0.398722998462751,
0.460761132980128,0.522788946141237,0.584119984199227,0.609251897024497,
0.616406215120755,0.623860834300335,0.684593333606756,0.744931857050254,
0.784341213415659,0.845068255831707,0.884007249861946,0.901043059750176,
0.912236715472706,0.920839905576931,0.980342222581217,1.03974346201836,
1.09825254793676,1.15658020807362,1.18303706386245,1.1975775625098,1.20796090260796,
1.26646558135057,1.32473138703364,1.36823505438423,1.37738657107583,1.43493464029449,
1.49171401425249,1.51467421871737,1.53973642054051),.UNSPECIFIED.);
#2972=B_SPLINE_CURVE_WITH_KNOTS('',3,(#27208,#27209,#27210,#27211,#27212,
#27213,#27214,#27215),.UNSPECIFIED.,.F.,.F.,(4,2,2,4),(9.38674526974159E-7,
0.197912071307587,0.244750653263811,0.283675624189322),.UNSPECIFIED.);
#2973=B_SPLINE_CURVE_WITH_KNOTS('',3,(#27217,#27218,#27219,#27220,#27221,
#27222,#27223,#27224,#27225,#27226),.UNSPECIFIED.,.F.,.F.,(4,2,2,2,4),(0.,
0.00238154318238252,0.00529193749553023,0.0121953093380869,0.0169288782364552),
 .UNSPECIFIED.);
#2974=B_SPLINE_CURVE_WITH_KNOTS('',3,(#27235,#27236,#27237,#27238,#27239,
#27240,#27241,#27242),.UNSPECIFIED.,.F.,.F.,(4,2,2,4),(9.39134819485715E-7,
0.313007067364836,0.466067686181722,0.641395236280365),.UNSPECIFIED.);
#2975=B_SPLINE_CURVE_WITH_KNOTS('',3,(#27244,#27245,#27246,#27247,#27248,
#27249,#27250,#27251,#27252,#27253),.UNSPECIFIED.,.F.,.F.,(4,2,2,2,4),(0.,
0.00238340067887078,0.00529624616302871,0.0122051825225569,0.0169424867765656),
 .UNSPECIFIED.);
#2976=B_SPLINE_CURVE_WITH_KNOTS('',3,(#27262,#27263,#27264,#27265,#27266,
#27267,#27268,#27269),.UNSPECIFIED.,.F.,.F.,(4,2,2,4),(9.38674282470181E-7,
0.197987316009641,0.244851770135215,0.28379594641037),.UNSPECIFIED.);
#2977=B_SPLINE_CURVE_WITH_KNOTS('',3,(#27271,#27272,#27273,#27274,#27275,
#27276,#27277,#27278),.UNSPECIFIED.,.F.,.F.,(4,2,2,4),(0.,0.0047633736137187,
0.00902722460288498,0.0150831942940084),.UNSPECIFIED.);
#2978=B_SPLINE_CURVE_WITH_KNOTS('',3,(#27287,#27288,#27289,#27290,#27291,
#27292,#27293,#27294),.UNSPECIFIED.,.F.,.F.,(4,2,2,4),(9.39136670358377E-7,
0.313011184875832,0.466084249009382,0.641473613344403),.UNSPECIFIED.);
#2979=B_SPLINE_CURVE_WITH_KNOTS('',3,(#27296,#27297,#27298,#27299,#27300,
#27301,#27302,#27303,#27304,#27305),.UNSPECIFIED.,.F.,.F.,(4,2,2,2,4),(0.,
0.00237357460738177,0.0052734579858211,0.0121529658906331,0.0168705147066673),
 .UNSPECIFIED.);
#2980=B_SPLINE_CURVE_WITH_KNOTS('',3,(#27314,#27315,#27316,#27317,#27318,
#27319,#27320,#27321),.UNSPECIFIED.,.F.,.F.,(4,2,2,4),(9.39136720441153E-7,
0.313011292240562,0.466084402983163,0.641474389410526),.UNSPECIFIED.);
#2981=B_SPLINE_CURVE_WITH_KNOTS('',3,(#27323,#27324,#27325,#27326,#27327,
#27328,#27329,#27330,#27331,#27332),.UNSPECIFIED.,.F.,.F.,(4,2,2,2,4),(0.,
0.0023782900743644,0.00528439250760633,0.0121780205899161,0.0169050485394452),
 .UNSPECIFIED.);
#2982=B_SPLINE_CURVE_WITH_KNOTS('',3,(#27341,#27342,#27343,#27344,#27345,
#27346,#27347,#27348),.UNSPECIFIED.,.F.,.F.,(4,2,2,4),(9.38674284612347E-7,
0.197985480739605,0.244849302967186,0.283793010207111),.UNSPECIFIED.);
#2983=B_SPLINE_CURVE_WITH_KNOTS('',3,(#27350,#27351,#27352,#27353,#27354,
#27355,#27356,#27357,#27358,#27359),.UNSPECIFIED.,.F.,.F.,(4,2,2,2,4),(0.,
0.00238320602712813,0.00529579462832576,0.0122041478366525,0.016941060634997),
 .UNSPECIFIED.);
#2984=B_SPLINE_CURVE_WITH_KNOTS('',3,(#27368,#27369,#27370,#27371,#27372,
#27373,#27374,#27375),.UNSPECIFIED.,.F.,.F.,(4,2,2,4),(9.39134818369318E-7,
0.31300706365764,0.466067681436598,0.641395213194101),.UNSPECIFIED.);
#2985=B_SPLINE_CURVE_WITH_KNOTS('',3,(#27377,#27378,#27379,#27380,#27381,
#27382,#27383,#27384),.UNSPECIFIED.,.F.,.F.,(4,2,2,4),(0.,0.00476388970796606,
0.00902830722597645,0.0150851135700706),.UNSPECIFIED.);
#2986=B_SPLINE_CURVE_WITH_KNOTS('',3,(#27393,#27394,#27395,#27396,#27397,
#27398,#27399,#27400),.UNSPECIFIED.,.F.,.F.,(4,2,2,4),(9.39135631813739E-7,
0.313008884693273,0.466070291990264,0.641408534042971),.UNSPECIFIED.);
#2987=B_SPLINE_CURVE_WITH_KNOTS('',3,(#27402,#27403,#27404,#27405,#27406,
#27407,#27408,#27409,#27410,#27411),.UNSPECIFIED.,.F.,.F.,(4,2,2,2,4),(0.,
0.0023785439095033,0.00528498118810588,0.0121793694890388,0.0169069077752386),
 .UNSPECIFIED.);
#2988=B_SPLINE_CURVE_WITH_KNOTS('',3,(#27420,#27421,#27422,#27423,#27424,
#27425,#27426,#27427),.UNSPECIFIED.,.F.,.F.,(4,2,2,4),(9.39138223560896E-7,
0.313014634420147,0.466099866256976,0.641546846663167),.UNSPECIFIED.);
#2989=B_SPLINE_CURVE_WITH_KNOTS('',3,(#27429,#27430,#27431,#27432,#27433,
#27434,#27435,#27436,#27437,#27438),.UNSPECIFIED.,.F.,.F.,(4,2,2,2,4),(0.,
0.00237319534257096,0.0052725786320786,0.0121509510394241,0.0168677375635532),
 .UNSPECIFIED.);
#2990=B_SPLINE_CURVE_WITH_KNOTS('',3,(#27447,#27448,#27449,#27450,#27451,
#27452,#27453,#27454),.UNSPECIFIED.,.F.,.F.,(4,2,2,4),(9.38674527823462E-7,
0.197912070601848,0.244750652620493,0.283675623600454),.UNSPECIFIED.);
#2991=B_SPLINE_CURVE_WITH_KNOTS('',3,(#27456,#27457,#27458,#27459,#27460,
#27461,#27462,#27463,#27464,#27465),.UNSPECIFIED.,.F.,.F.,(4,2,2,2,4),(0.,
0.00238154317971207,0.00529193748943623,0.012195309323669,0.0169288782166237),
 .UNSPECIFIED.);
#2992=B_SPLINE_CURVE_WITH_KNOTS('',3,(#27474,#27475,#27476,#27477,#27478,
#27479,#27480,#27481),.UNSPECIFIED.,.F.,.F.,(4,2,2,4),(9.3913481761243E-7,
0.31300706664949,0.466067685923882,0.641395236588582),.UNSPECIFIED.);
#2993=B_SPLINE_CURVE_WITH_KNOTS('',3,(#27483,#27484,#27485,#27486,#27487,
#27488,#27489,#27490),.UNSPECIFIED.,.F.,.F.,(4,2,2,4),(0.,0.00476393585611593,
0.00902840402447764,0.0150852851575008),.UNSPECIFIED.);
#2994=B_SPLINE_CURVE_WITH_KNOTS('',3,(#27499,#27500,#27501,#27502,#27503,
#27504,#27505,#27506),.UNSPECIFIED.,.F.,.F.,(4,2,2,4),(9.38674282697379E-7,
0.197987318201236,0.24485177211621,0.283795948207931),.UNSPECIFIED.);
#2995=B_SPLINE_CURVE_WITH_KNOTS('',3,(#27508,#27509,#27510,#27511,#27512,
#27513,#27514,#27515,#27516,#27517),.UNSPECIFIED.,.F.,.F.,(4,2,2,2,4),(0.,
0.0023816918039995,0.00529228222519305,0.0121960992691896,0.0169299670267326),
 .UNSPECIFIED.);
#2996=B_SPLINE_CURVE_WITH_KNOTS('',3,(#27526,#27527,#27528,#27529,#27530,
#27531,#27532,#27533),.UNSPECIFIED.,.F.,.F.,(4,2,2,4),(9.39136669948809E-7,
0.313011185099831,0.466084249090031,0.641473613246853),.UNSPECIFIED.);
#2997=B_SPLINE_CURVE_WITH_KNOTS('',3,(#27535,#27536,#27537,#27538,#27539,
#27540,#27541,#27542,#27543,#27544),.UNSPECIFIED.,.F.,.F.,(4,2,2,2,4),(0.,
0.00237357460648197,0.00527345798380301,0.0121529658846397,0.016870514699817),
 .UNSPECIFIED.);
#2998=B_SPLINE_CURVE_WITH_KNOTS('',3,(#27553,#27554,#27555,#27556,#27557,
#27558,#27559,#27560),.UNSPECIFIED.,.F.,.F.,(4,2,2,4),(9.39136719522134E-7,
0.313011292197314,0.466084402967806,0.641474389430124),.UNSPECIFIED.);
#2999=B_SPLINE_CURVE_WITH_KNOTS('',3,(#27562,#27563,#27564,#27565,#27566,
#27567,#27568,#27569,#27570,#27571),.UNSPECIFIED.,.F.,.F.,(4,2,2,2,4),(0.,
0.00237829007741614,0.00528439251454885,0.0121780206098593,0.0169050485629513),
 .UNSPECIFIED.);
#3000=B_SPLINE_CURVE_WITH_KNOTS('',3,(#27580,#27581,#27582,#27583,#27584,
#27585,#27586,#27587),.UNSPECIFIED.,.F.,.F.,(4,2,2,4),(9.38674290583485E-7,
0.197985478708047,0.244849301132532,0.283793008543649),.UNSPECIFIED.);
#3001=B_SPLINE_CURVE_WITH_KNOTS('',3,(#27589,#27590,#27591,#27592,#27593,
#27594,#27595,#27596,#27597,#27598),.UNSPECIFIED.,.F.,.F.,(4,2,2,2,4),(0.,
0.00238320602681499,0.00529579462760504,0.0122041478355376,0.0169410606327885),
 .UNSPECIFIED.);
#3002=B_SPLINE_CURVE_WITH_KNOTS('',3,(#27607,#27608,#27609,#27610,#27611,
#27612,#27613,#27614),.UNSPECIFIED.,.F.,.F.,(4,2,2,4),(9.39134818485942E-7,
0.313007063639476,0.466067681430211,0.641395213202689),.UNSPECIFIED.);
#3003=B_SPLINE_CURVE_WITH_KNOTS('',3,(#27616,#27617,#27618,#27619,#27620,
#27621,#27622,#27623,#27624,#27625),.UNSPECIFIED.,.F.,.F.,(4,2,2,2,4),(0.,
0.00288584394666921,0.00676564596185734,0.0194599953243108,0.045988200349411),
 .UNSPECIFIED.);
#3004=B_SPLINE_CURVE_WITH_KNOTS('',3,(#27634,#27635,#27636,#27637,#27638,
#27639,#27640,#27641),.UNSPECIFIED.,.F.,.F.,(4,2,2,4),(9.39138223334931E-7,
0.31301463434841,0.466099866231014,0.641546846692122),.UNSPECIFIED.);
#3005=B_SPLINE_CURVE_WITH_KNOTS('',3,(#27643,#27644,#27645,#27646,#27647,
#27648,#27649,#27650,#27651,#27652),.UNSPECIFIED.,.F.,.F.,(4,2,2,2,4),(0.,
0.00288578889265372,0.00676552602658123,0.0194588364051688,0.0459849509963726),
 .UNSPECIFIED.);
#3006=B_SPLINE_CURVE_WITH_KNOTS('',3,(#27661,#27662,#27663,#27664,#27665,
#27666,#27667,#27668),.UNSPECIFIED.,.F.,.F.,(4,2,2,4),(9.38674512203643E-7,
0.197915707554863,0.244755539870822,0.283681439071384),.UNSPECIFIED.);
#3007=B_SPLINE_CURVE_WITH_KNOTS('',3,(#27670,#27671,#27672,#27673,#27674,
#27675,#27676,#27677,#27678,#27679),.UNSPECIFIED.,.F.,.F.,(4,2,2,2,4),(0.,
0.00288581812123732,0.00676558988611721,0.0194594510099433,0.0459866741536432),
 .UNSPECIFIED.);
#3008=B_SPLINE_CURVE_WITH_KNOTS('',3,(#27692,#27693,#27694,#27695,#27696,
#27697,#27698,#27699),.UNSPECIFIED.,.F.,.F.,(4,2,2,4),(9.3913745254888E-7,
0.313012920882138,0.466097404509773,0.641534556152897),.UNSPECIFIED.);
#3009=B_SPLINE_CURVE_WITH_KNOTS('',3,(#27703,#27704,#27705,#27706,#27707,
#27708,#27709,#27710,#27711,#27712),.UNSPECIFIED.,.F.,.F.,(4,2,2,2,4),(0.,
0.00288577255855134,0.00676549015491415,0.0194584932984043,0.0459839884509012),
 .UNSPECIFIED.);
#3010=B_SPLINE_CURVE_WITH_KNOTS('',3,(#27725,#27726,#27727,#27728,#27729,
#27730,#27731,#27732,#27733,#27734),.UNSPECIFIED.,.F.,.F.,(4,2,2,2,4),(9.38676322936076E-7,
0.190216558583583,0.359875507174653,0.441533870949612,0.507581347070439),
 .UNSPECIFIED.);
#3011=B_SPLINE_CURVE_WITH_KNOTS('',3,(#27738,#27739,#27740,#27741,#27742,
#27743,#27744,#27745),.UNSPECIFIED.,.F.,.F.,(4,2,2,4),(0.,0.00476287317060948,
0.0090261747394427,0.0150813329561307),.UNSPECIFIED.);
#3012=B_SPLINE_CURVE_WITH_KNOTS('',3,(#27758,#27759,#27760,#27761,#27762,
#27763,#27764,#27765,#27766,#27767),.UNSPECIFIED.,.F.,.F.,(4,2,2,2,4),(9.38676132424859E-7,
0.190216675552138,0.359875382199115,0.441534255569763,0.507580281805651),
 .UNSPECIFIED.);
#3013=B_SPLINE_CURVE_WITH_KNOTS('',3,(#27771,#27772,#27773,#27774,#27775,
#27776,#27777,#27778,#27779,#27780),.UNSPECIFIED.,.F.,.F.,(4,2,2,2,4),(0.,
0.00288584518508398,0.00676564864347784,0.0194600214082376,0.0459882734084581),
 .UNSPECIFIED.);
#3014=B_SPLINE_CURVE_WITH_KNOTS('',3,(#27793,#27794,#27795,#27796,#27797,
#27798,#27799,#27800),.UNSPECIFIED.,.F.,.F.,(4,2,2,4),(9.38674377615734E-7,
0.19795837352917,0.244812875199329,0.283749664140645),.UNSPECIFIED.);
#3015=B_SPLINE_CURVE_WITH_KNOTS('',3,(#27804,#27805,#27806,#27807,#27808,
#27809,#27810,#27811),.UNSPECIFIED.,.F.,.F.,(4,2,2,4),(0.,0.00476368678937328,
0.00902788155483768,0.0150843589237395),.UNSPECIFIED.);
#3016=B_SPLINE_CURVE_WITH_KNOTS('',3,(#27824,#27825,#27826,#27827,#27828,
#27829,#27830,#27831,#27832,#27833),.UNSPECIFIED.,.F.,.F.,(4,2,2,2,4),(9.38677117360782E-7,
0.190216058945539,0.359865342787696,0.44150491422111,0.507545138629862),
 .UNSPECIFIED.);
#3017=B_SPLINE_CURVE_WITH_KNOTS('',3,(#27837,#27838,#27839,#27840,#27841,
#27842,#27843,#27844,#27845,#27846),.UNSPECIFIED.,.F.,.F.,(4,2,2,2,4),(0.,
0.00288580557302315,0.00676556252532466,0.0194591867332428,0.0459859327527602),
 .UNSPECIFIED.);
#3018=B_SPLINE_CURVE_WITH_KNOTS('',3,(#27859,#27860,#27861,#27862,#27863,
#27864,#27865,#27866,#27867,#27868),.UNSPECIFIED.,.F.,.F.,(4,2,2,2,4),(9.38676644870429E-7,
0.190216354160521,0.359865058426445,0.441505964266297,0.507542572156931),
 .UNSPECIFIED.);
#3019=B_SPLINE_CURVE_WITH_KNOTS('',3,(#27872,#27873,#27874,#27875,#27876,
#27877,#27878,#27879,#27880,#27881),.UNSPECIFIED.,.F.,.F.,(4,2,2,2,4),(0.,
0.00288580454690941,0.00676556028459874,0.0194591651238233,0.0459858721133107),
 .UNSPECIFIED.);
#3020=B_SPLINE_CURVE_WITH_KNOTS('',3,(#27894,#27895,#27896,#27897,#27898,
#27899,#27900,#27901,#27902,#27903),.UNSPECIFIED.,.F.,.F.,(4,2,2,2,4),(9.38676160620083E-7,
0.19021666331625,0.359875396536414,0.441534218705211,0.507580398815235),
 .UNSPECIFIED.);
#3021=B_SPLINE_CURVE_WITH_KNOTS('',3,(#27907,#27908,#27909,#27910,#27911,
#27912,#27913,#27914),.UNSPECIFIED.,.F.,.F.,(4,2,2,4),(0.,0.00476366682174163,
0.00902783959238785,0.0150842843350958),.UNSPECIFIED.);
#3022=B_SPLINE_CURVE_WITH_KNOTS('',3,(#27927,#27928,#27929,#27930,#27931,
#27932,#27933,#27934),.UNSPECIFIED.,.F.,.F.,(4,2,2,4),(9.38674218968633E-7,
0.198006053174433,0.24487695114834,0.283825910095945),.UNSPECIFIED.);
#3023=B_SPLINE_CURVE_WITH_KNOTS('',3,(#27938,#27939,#27940,#27941,#27942,
#27943,#27944,#27945,#27946,#27947),.UNSPECIFIED.,.F.,.F.,(4,2,2,2,4),(0.,
0.00288584520885465,0.00676564869365475,0.0194600220037921,0.0459882752473628),
 .UNSPECIFIED.);
#3024=B_SPLINE_CURVE_WITH_KNOTS('',3,(#27960,#27961,#27962,#27963,#27964,
#27965,#27966,#27967,#27968,#27969),.UNSPECIFIED.,.F.,.F.,(4,2,2,2,4),(9.38676621047222E-7,
0.190216370014355,0.35986504387141,0.4415060225351,0.507542435940933),
 .UNSPECIFIED.);
#3025=B_SPLINE_CURVE_WITH_KNOTS('',3,(#27973,#27974,#27975,#27976,#27977,
#27978,#27979,#27980,#27981,#27982),.UNSPECIFIED.,.F.,.F.,(4,2,2,2,4),(0.,
0.00288582767659631,0.00676561067367699,0.0194596521031919,0.0459872376775252),
 .UNSPECIFIED.);
#3026=B_SPLINE_CURVE_WITH_KNOTS('',3,(#27995,#27996,#27997,#27998,#27999,
#28000,#28001,#28002,#28003,#28004),.UNSPECIFIED.,.F.,.F.,(4,2,2,2,4),(9.38677156228019E-7,
0.190216034794342,0.359865371222063,0.44150484321002,0.507545363962411),
 .UNSPECIFIED.);
#3027=B_SPLINE_CURVE_WITH_KNOTS('',3,(#28008,#28009,#28010,#28011,#28012,
#28013,#28014,#28015,#28016,#28017),.UNSPECIFIED.,.F.,.F.,(4,2,2,2,4),(0.,
0.00288577255842772,0.00676549015463377,0.0194584932973895,0.0459839884562596),
 .UNSPECIFIED.);
#3028=B_SPLINE_CURVE_WITH_KNOTS('',3,(#28030,#28031,#28032,#28033,#28034,
#28035,#28036,#28037,#28038,#28039),.UNSPECIFIED.,.F.,.F.,(4,2,2,2,4),(9.38676323177046E-7,
0.190216558327547,0.359875507149927,0.441533871021912,0.507581347237268),
 .UNSPECIFIED.);
#3029=B_SPLINE_CURVE_WITH_KNOTS('',3,(#28043,#28044,#28045,#28046,#28047,
#28048,#28049,#28050),.UNSPECIFIED.,.F.,.F.,(4,2,2,4),(0.,0.00476287319732046,
0.00902617482142203,0.0150813331688102),.UNSPECIFIED.);
#3030=B_SPLINE_CURVE_WITH_KNOTS('',3,(#28063,#28064,#28065,#28066,#28067,
#28068,#28069,#28070),.UNSPECIFIED.,.F.,.F.,(4,2,2,4),(9.38674206481295E-7,
0.198010313344894,0.244882676520894,0.28383272291311),.UNSPECIFIED.);
#3031=B_SPLINE_CURVE_WITH_KNOTS('',3,(#28074,#28075,#28076,#28077,#28078,
#28079,#28080,#28081,#28082,#28083),.UNSPECIFIED.,.F.,.F.,(4,2,2,2,4),(0.,
0.00288584517738443,0.00676564862539164,0.0194600213508031,0.0459882734381834),
 .UNSPECIFIED.);
#3032=B_SPLINE_CURVE_WITH_KNOTS('',3,(#28096,#28097,#28098,#28099,#28100,
#28101,#28102,#28103,#28104,#28105),.UNSPECIFIED.,.F.,.F.,(4,2,2,2,4),(9.38676310254617E-7,
0.190216568196222,0.359875496482002,0.441533899642992,0.507581258743622),
 .UNSPECIFIED.);
#3033=B_SPLINE_CURVE_WITH_KNOTS('',3,(#28109,#28110,#28111,#28112,#28113,
#28114,#28115,#28116),.UNSPECIFIED.,.F.,.F.,(4,2,2,4),(0.,0.00476368668604745,
0.0090278812393193,0.0150843581077754),.UNSPECIFIED.);
#3034=B_SPLINE_CURVE_WITH_KNOTS('',3,(#28129,#28130,#28131,#28132,#28133,
#28134,#28135,#28136,#28137,#28138),.UNSPECIFIED.,.F.,.F.,(4,2,2,2,4),(9.38677117179183E-7,
0.190216058846508,0.359865342778253,0.44150491424923,0.507545138694429),
 .UNSPECIFIED.);
#3035=B_SPLINE_CURVE_WITH_KNOTS('',3,(#28142,#28143,#28144,#28145,#28146,
#28147,#28148,#28149,#28150,#28151),.UNSPECIFIED.,.F.,.F.,(4,2,2,2,4),(0.,
0.0028858055760958,0.00676556253253746,0.0194591867562179,0.0459859327383561),
 .UNSPECIFIED.);
#3036=B_SPLINE_CURVE_WITH_KNOTS('',3,(#28164,#28165,#28166,#28167,#28168,
#28169,#28170,#28171,#28172,#28173),.UNSPECIFIED.,.F.,.F.,(4,2,2,2,4),(9.38676644713873E-7,
0.190216354185753,0.359865058428838,0.441505964259139,0.507542572138923),
 .UNSPECIFIED.);
#3037=B_SPLINE_CURVE_WITH_KNOTS('',3,(#28177,#28178,#28179,#28180,#28181,
#28182,#28183,#28184,#28185,#28186),.UNSPECIFIED.,.F.,.F.,(4,2,2,2,4),(0.,
0.00288580454917283,0.00676556028991565,0.0194591651405655,0.045985872109436),
 .UNSPECIFIED.);
#3038=B_SPLINE_CURVE_WITH_KNOTS('',3,(#28199,#28200,#28201,#28202,#28203,
#28204,#28205,#28206,#28207,#28208),.UNSPECIFIED.,.F.,.F.,(4,2,2,2,4),(9.38676160335773E-7,
0.190216663193983,0.35987539652473,0.441534218739778,0.507580398893346),
 .UNSPECIFIED.);
#3039=B_SPLINE_CURVE_WITH_KNOTS('',3,(#28212,#28213,#28214,#28215,#28216,
#28217,#28218,#28219),.UNSPECIFIED.,.F.,.F.,(4,2,2,4),(0.,0.00476366691827938,
0.00902783988845374,0.0150842851027805),.UNSPECIFIED.);
#3040=B_SPLINE_CURVE_WITH_KNOTS('',3,(#28232,#28233,#28234,#28235,#28236,
#28237,#28238,#28239),.UNSPECIFIED.,.F.,.F.,(4,2,2,4),(9.39134874106605E-7,
0.313007195011186,0.466067869529335,0.641396175473332),.UNSPECIFIED.);
#3041=B_SPLINE_CURVE_WITH_KNOTS('',3,(#28243,#28244,#28245,#28246,#28247,
#28248,#28249,#28250,#28251,#28252),.UNSPECIFIED.,.F.,.F.,(4,2,2,2,4),(0.,
0.00288584520947008,0.00676564869509268,0.019460022008105,0.0459882752517017),
 .UNSPECIFIED.);
#3042=B_SPLINE_CURVE_WITH_KNOTS('',3,(#28265,#28266,#28267,#28268,#28269,
#28270,#28271,#28272),.UNSPECIFIED.,.F.,.F.,(4,2,2,4),(9.39136080394831E-7,
0.313009874980368,0.466082370050846,0.641464116445783),.UNSPECIFIED.);
#3043=B_SPLINE_CURVE_WITH_KNOTS('',3,(#28276,#28277,#28278,#28279,#28280,
#28281,#28282,#28283),.UNSPECIFIED.,.F.,.F.,(4,2,2,4),(0.,0.0047629124728381,
0.00902625721222522,0.0150814792303183),.UNSPECIFIED.);
#3044=B_SPLINE_CURVE_WITH_KNOTS('',3,(#28400,#28401,#28402,#28403,#28404,
#28405),.UNSPECIFIED.,.F.,.F.,(4,2,4),(-0.00983438259802202,-0.00492102107344964,
0.),.UNSPECIFIED.);
#3045=B_SPLINE_CURVE_WITH_KNOTS('',3,(#28432,#28433,#28434,#28435,#28436,
#28437),.UNSPECIFIED.,.F.,.F.,(4,2,4),(-0.00983535924918913,-0.00492266478240658,
0.),.UNSPECIFIED.);
#3046=B_SPLINE_CURVE_WITH_KNOTS('',3,(#28473,#28474,#28475,#28476,#28477,
#28478),.UNSPECIFIED.,.F.,.F.,(4,2,4),(-0.00983535878889612,-0.00492266422265586,
0.),.UNSPECIFIED.);
#3047=B_SPLINE_CURVE_WITH_KNOTS('',3,(#28514,#28515,#28516,#28517,#28518,
#28519),.UNSPECIFIED.,.F.,.F.,(4,2,4),(-0.0098353587479088,-0.00492266417261958,
0.),.UNSPECIFIED.);
#3048=B_SPLINE_CURVE_WITH_KNOTS('',3,(#28564,#28565,#28566,#28567,#28568,
#28569),.UNSPECIFIED.,.F.,.F.,(4,2,4),(-0.00983437497489847,-0.00492101512779726,
0.),.UNSPECIFIED.);
#3049=B_SPLINE_CURVE_WITH_KNOTS('',3,(#28578,#28579,#28580,#28581,#28582,
#28583),.UNSPECIFIED.,.F.,.F.,(4,2,4),(-0.0098343785393361,-0.00492101790414255,
0.),.UNSPECIFIED.);
#3050=B_SPLINE_CURVE_WITH_KNOTS('',3,(#28588,#28589,#28590,#28591,#28592,
#28593),.UNSPECIFIED.,.F.,.F.,(4,2,4),(-0.00983438488091109,-0.00492102285998894,
0.),.UNSPECIFIED.);
#3051=B_SPLINE_CURVE_WITH_KNOTS('',3,(#28602,#28603,#28604,#28605,#28606,
#28607),.UNSPECIFIED.,.F.,.F.,(4,2,4),(-0.00983535969514932,-0.00492266532538871,
0.),.UNSPECIFIED.);
#3052=B_SPLINE_CURVE_WITH_KNOTS('',3,(#28616,#28617,#28618,#28619,#28620,
#28621),.UNSPECIFIED.,.F.,.F.,(4,2,4),(-0.00983437480440195,-0.00492101499529718,
0.),.UNSPECIFIED.);
#3053=B_SPLINE_CURVE_WITH_KNOTS('',3,(#28630,#28631,#28632,#28633,#28634,
#28635),.UNSPECIFIED.,.F.,.F.,(4,2,4),(-0.00983535897005503,-0.00492266444295711,
0.),.UNSPECIFIED.);
#3054=B_SPLINE_CURVE_WITH_KNOTS('',3,(#28644,#28645,#28646,#28647,#28648,
#28649),.UNSPECIFIED.,.F.,.F.,(4,2,4),(-0.00983438028091156,-0.00492101926303028,
0.),.UNSPECIFIED.);
#3055=B_SPLINE_CURVE_WITH_KNOTS('',3,(#28658,#28659,#28660,#28661,#28662,
#28663),.UNSPECIFIED.,.F.,.F.,(4,2,4),(-0.00983438042371488,-0.00492101937453644,
0.),.UNSPECIFIED.);
#3056=B_SPLINE_CURVE_WITH_KNOTS('',3,(#28672,#28673,#28674,#28675,#28676,
#28677),.UNSPECIFIED.,.F.,.F.,(4,2,4),(-0.00983535898766203,-0.00492266446437622,
0.),.UNSPECIFIED.);
#3057=B_SPLINE_CURVE_WITH_KNOTS('',3,(#28686,#28687,#28688,#28689,#28690,
#28691),.UNSPECIFIED.,.F.,.F.,(4,2,4),(-0.00983437480033418,-0.00492101499217869,
0.),.UNSPECIFIED.);
#3058=B_SPLINE_CURVE_WITH_KNOTS('',3,(#28700,#28701,#28702,#28703,#28704,
#28705),.UNSPECIFIED.,.F.,.F.,(4,2,4),(-0.00983437721979582,-0.00492101687559478,
0.),.UNSPECIFIED.);
#3059=B_SPLINE_CURVE_WITH_KNOTS('',3,(#28714,#28715,#28716,#28717,#28718,
#28719),.UNSPECIFIED.,.F.,.F.,(4,2,4),(-0.00983438488112925,-0.00492102286014865,
0.),.UNSPECIFIED.);
#3060=B_SPLINE_CURVE_WITH_KNOTS('',3,(#28728,#28729,#28730,#28731,#28732,
#28733),.UNSPECIFIED.,.F.,.F.,(4,2,4),(-0.00983535969514463,-0.0049226653253664,
0.),.UNSPECIFIED.);
#3061=B_SPLINE_CURVE_WITH_KNOTS('',3,(#28742,#28743,#28744,#28745,#28746,
#28747),.UNSPECIFIED.,.F.,.F.,(4,2,4),(-0.00983437480384014,-0.00492101499504691,
0.),.UNSPECIFIED.);
#3062=B_SPLINE_CURVE_WITH_KNOTS('',3,(#28756,#28757,#28758,#28759,#28760,
#28761),.UNSPECIFIED.,.F.,.F.,(4,2,4),(-0.00983535896995666,-0.00492266444279139,
0.),.UNSPECIFIED.);
#3063=B_SPLINE_CURVE_WITH_KNOTS('',3,(#28770,#28771,#28772,#28773,#28774,
#28775),.UNSPECIFIED.,.F.,.F.,(4,2,4),(-0.00983438028095572,-0.00492101926308378,
0.),.UNSPECIFIED.);
#3064=B_SPLINE_CURVE_WITH_KNOTS('',3,(#28784,#28785,#28786,#28787,#28788,
#28789),.UNSPECIFIED.,.F.,.F.,(4,2,4),(-0.00983438042362209,-0.00492101937455925,
0.),.UNSPECIFIED.);
#3065=B_SPLINE_CURVE_WITH_KNOTS('',3,(#28798,#28799,#28800,#28801,#28802,
#28803),.UNSPECIFIED.,.F.,.F.,(4,2,4),(-0.00983535898790276,-0.00492266446462651,
0.),.UNSPECIFIED.);
#3066=B_SPLINE_CURVE_WITH_KNOTS('',3,(#28812,#28813,#28814,#28815,#28816,
#28817),.UNSPECIFIED.,.F.,.F.,(4,2,4),(-0.00983437479993856,-0.00492101499183855,
0.),.UNSPECIFIED.);
#3067=B_SPLINE_CURVE_WITH_KNOTS('',3,(#28826,#28827,#28828,#28829,#28830,
#28831),.UNSPECIFIED.,.F.,.F.,(4,2,4),(-0.00983535966014206,-0.00492266528281923,
0.),.UNSPECIFIED.);
#3068=B_SPLINE_CURVE_WITH_KNOTS('',3,(#28838,#28839,#28840,#28841,#28842,
#28843,#28844,#28845,#28846,#28847,#28848,#28849,#28850,#28851),
 .UNSPECIFIED.,.F.,.F.,(4,2,2,2,2,2,4),(-0.82600395443711,-0.625773509086572,
-0.500319880314509,-0.4128988677948,-0.323416359045162,-0.187269988974532,
-3.37805815843223E-6),.UNSPECIFIED.);
#3069=B_SPLINE_CURVE_WITH_KNOTS('',3,(#28852,#28853,#28854,#28855,#28856,
#28857,#28858,#28859,#28860,#28861,#28862,#28863,#28864,#28865),
 .UNSPECIFIED.,.F.,.F.,(4,2,2,2,2,2,4),(-0.826003693746637,-0.62577441198849,
-0.500320233133826,-0.41289872345655,-0.323415723219816,-0.187268878424026,
-3.38098086435097E-6),.UNSPECIFIED.);
#3070=B_SPLINE_CURVE_WITH_KNOTS('',3,(#28867,#28868,#28869,#28870,#28871,
#28872,#28873,#28874,#28875,#28876,#28877,#28878,#28879,#28880),
 .UNSPECIFIED.,.F.,.F.,(4,2,2,2,2,2,4),(-0.826160973205696,-0.625505733497847,
-0.500256557879679,-0.412982835097184,-0.323646851595676,-0.187689432402941,
-2.22228171383796E-6),.UNSPECIFIED.);
#3071=B_SPLINE_CURVE_WITH_KNOTS('',3,(#28881,#28882,#28883,#28884,#28885,
#28886,#28887,#28888,#28889,#28890,#28891,#28892,#28893,#28894),
 .UNSPECIFIED.,.F.,.F.,(4,2,2,2,2,2,4),(-0.826160921263055,-0.625505869063133,
-0.500256603642305,-0.412982806908025,-0.323646750043836,-0.187689250732374,
-2.2228099030522E-6),.UNSPECIFIED.);
#3072=B_SPLINE_CURVE_WITH_KNOTS('',3,(#28896,#28897,#28898,#28899,#28900,
#28901,#28902,#28903,#28904,#28905,#28906,#28907,#28908,#28909),
 .UNSPECIFIED.,.F.,.F.,(4,2,2,2,2,2,4),(-0.826002804744842,-0.625777498404662,
-0.500321440270458,-0.412898231168244,-0.323413550926482,-0.187265084649461,
-3.39095613572205E-6),.UNSPECIFIED.);
#3073=B_SPLINE_CURVE_WITH_KNOTS('',3,(#28910,#28911,#28912,#28913,#28914,
#28915,#28916,#28917,#28918,#28919,#28920,#28921,#28922,#28923),
 .UNSPECIFIED.,.F.,.F.,(4,2,2,2,2,2,4),(-0.826160850959899,-0.625506052002871,
-0.50025666536275,-0.412982768750562,-0.323646612808788,-0.187689005398769,
-2.22350912481821E-6),.UNSPECIFIED.);
#3074=B_SPLINE_CURVE_WITH_KNOTS('',3,(#28925,#28926,#28927,#28928,#28929,
#28930,#28931,#28932,#28933,#28934,#28935,#28936,#28937,#28938),
 .UNSPECIFIED.,.F.,.F.,(4,2,2,2,2,2,4),(-0.826160879595006,-0.625505976987524,
-0.500256640008355,-0.412982784285415,-0.32364666890615,-0.18768910580297,
-2.22321262101263E-6),.UNSPECIFIED.);
#3075=B_SPLINE_CURVE_WITH_KNOTS('',3,(#28939,#28940,#28941,#28942,#28943,
#28944,#28945,#28946,#28947,#28948,#28949,#28950,#28951,#28952),
 .UNSPECIFIED.,.F.,.F.,(4,2,2,2,2,2,4),(-0.826160915626209,-0.625505883254,
-0.500256608389856,-0.412982803848779,-0.323646739244151,-0.187689231547272,
-2.22285427832525E-6),.UNSPECIFIED.);
#3076=B_SPLINE_CURVE_WITH_KNOTS('',3,(#28954,#28955,#28956,#28957,#28958,
#28959,#28960,#28961,#28962,#28963,#28964,#28965,#28966,#28967),
 .UNSPECIFIED.,.F.,.F.,(4,2,2,2,2,2,4),(-0.826003429306002,-0.625775328896998,
-0.500320591576485,-0.412898577035401,-0.32341507769936,-0.187267750996852,
-3.38394675953995E-6),.UNSPECIFIED.);
#3077=B_SPLINE_CURVE_WITH_KNOTS('',3,(#28968,#28969,#28970,#28971,#28972,
#28973,#28974,#28975,#28976,#28977,#28978,#28979,#28980,#28981),
 .UNSPECIFIED.,.F.,.F.,(4,2,2,2,2,2,4),(-0.826161221320018,-0.625505089589237,
-0.500256340926373,-0.412982969745037,-0.323647335030655,-0.187690296613032,
-2.21982746541616E-6),.UNSPECIFIED.);
#3078=B_SPLINE_CURVE_WITH_KNOTS('',3,(#28983,#28984,#28985,#28986,#28987,
#28988,#28989,#28990,#28991,#28992,#28993,#28994,#28995,#28996),
 .UNSPECIFIED.,.F.,.F.,(4,2,2,2,2,2,4),(-0.826003445592927,-0.625775272398046,
-0.500320569485795,-0.412898586055166,-0.323415117474739,-0.187267820464824,
-3.38376405458033E-6),.UNSPECIFIED.);
#3079=B_SPLINE_CURVE_WITH_KNOTS('',3,(#28997,#28998,#28999,#29000,#29001,
#29002,#29003,#29004,#29005,#29006,#29007,#29008,#29009,#29010),
 .UNSPECIFIED.,.F.,.F.,(4,2,2,2,2,2,4),(-0.826161044059661,-0.625505549780422,
-0.500256495972241,-0.412982873540227,-0.323646989578432,-0.187689678966569,
-2.22158898431419E-6),.UNSPECIFIED.);
#3080=B_SPLINE_CURVE_WITH_KNOTS('',3,(#29012,#29013,#29014,#29015,#29016,
#29017,#29018,#29019,#29020,#29021,#29022,#29023,#29024,#29025),
 .UNSPECIFIED.,.F.,.F.,(4,2,2,2,2,2,4),(-0.826160881882724,-0.62550597104126,
-0.500256638003748,-0.412982785530703,-0.323646673376656,-0.187689113795201,
-2.22318986310915E-6),.UNSPECIFIED.);
#3081=B_SPLINE_CURVE_WITH_KNOTS('',3,(#29026,#29027,#29028,#29029,#29030,
#29031,#29032,#29033,#29034,#29035,#29036,#29037,#29038,#29039),
 .UNSPECIFIED.,.F.,.F.,(4,2,2,2,2,2,4),(-0.826160858333095,-0.625506032805967,
-0.50025665888393,-0.412982772750447,-0.323646627202582,-0.187689031129653,
-2.22343578162597E-6),.UNSPECIFIED.);
#3082=B_SPLINE_CURVE_WITH_KNOTS('',3,(#29041,#29042,#29043,#29044,#29045,
#29046,#29047,#29048,#29049,#29050,#29051,#29052,#29053,#29054),
 .UNSPECIFIED.,.F.,.F.,(4,2,2,2,2,2,4),(-0.82600280426376,-0.625777500099417,
-0.500321440937581,-0.412898230912546,-0.323413549762581,-0.187265082618854,
-3.3909615432171E-6),.UNSPECIFIED.);
#3083=B_SPLINE_CURVE_WITH_KNOTS('',3,(#29055,#29056,#29057,#29058,#29059,
#29060,#29061,#29062,#29063,#29064,#29065,#29066,#29067,#29068),
 .UNSPECIFIED.,.F.,.F.,(4,2,2,2,2,2,4),(-0.826160856252331,-0.625506037746287,
-0.500256660510859,-0.412982771619331,-0.323646623338634,-0.187689024343634,
-2.22344480128072E-6),.UNSPECIFIED.);
#3084=B_SPLINE_CURVE_WITH_KNOTS('',3,(#29070,#29071,#29072,#29073,#29074,
#29075,#29076,#29077,#29078,#29079,#29080,#29081,#29082,#29083),
 .UNSPECIFIED.,.F.,.F.,(4,2,2,2,2,2,4),(-0.826003080122764,-0.625776541178574,
-0.500321065714738,-0.412898383680039,-0.323414224480335,-0.187266260903283,
-3.3878648413558E-6),.UNSPECIFIED.);
#3085=B_SPLINE_CURVE_WITH_KNOTS('',3,(#29084,#29085,#29086,#29087,#29088,
#29089,#29090,#29091,#29092,#29093,#29094,#29095,#29096,#29097),
 .UNSPECIFIED.,.F.,.F.,(4,2,2,2,2,2,4),(-0.826161034493358,-0.625505574643043,
-0.500256504354302,-0.412982868350074,-0.323646970925289,-0.187689645618028,
-2.2216840828131E-6),.UNSPECIFIED.);
#3086=B_SPLINE_CURVE_WITH_KNOTS('',3,(#29099,#29100,#29101,#29102,#29103,
#29104,#29105,#29106,#29107,#29108,#29109,#29110,#29111,#29112),
 .UNSPECIFIED.,.F.,.F.,(4,2,2,2,2,2,4),(-0.826003954437199,-0.62577350908337,
-0.500319880312736,-0.412898867793276,-0.32341635904328,-0.187269988970896,
-3.37805815897863E-6),.UNSPECIFIED.);
#3087=B_SPLINE_CURVE_WITH_KNOTS('',3,(#29113,#29114,#29115,#29116,#29117,
#29118,#29119,#29120,#29121,#29122,#29123,#29124,#29125,#29126),
 .UNSPECIFIED.,.F.,.F.,(4,2,2,2,2,2,4),(-0.826161235539218,-0.62550505270487,
-0.500256328505594,-0.412982977460568,-0.323647362721577,-0.187690346125095,
-2.21968621033823E-6),.UNSPECIFIED.);
#3088=B_SPLINE_CURVE_WITH_KNOTS('',3,(#29128,#29129,#29130,#29131,#29132,
#29133,#29134,#29135,#29136,#29137,#29138,#29139,#29140,#29141),
 .UNSPECIFIED.,.F.,.F.,(4,2,2,2,2,2,4),(-0.826160973205453,-0.625505733506315,
-0.500256557884447,-0.412982835101311,-0.323646851600755,-0.187689432412604,
-2.22228171405919E-6),.UNSPECIFIED.);
#3089=B_SPLINE_CURVE_WITH_KNOTS('',3,(#29142,#29143,#29144,#29145,#29146,
#29147,#29148,#29149,#29150,#29151,#29152,#29153,#29154,#29155),
 .UNSPECIFIED.,.F.,.F.,(4,2,2,2,2,2,4),(-0.826160921263198,-0.625505869052163,
-0.500256603636118,-0.412982806902687,-0.32364675003728,-0.187689250719983,
-2.222809903634E-6),.UNSPECIFIED.);
#3090=B_SPLINE_CURVE_WITH_KNOTS('',3,(#29157,#29158,#29159,#29160,#29161,
#29162,#29163,#29164,#29165,#29166,#29167,#29168,#29169,#29170),
 .UNSPECIFIED.,.F.,.F.,(4,2,2,2,2,2,4),(-0.826002804744918,-0.625777498402643,
-0.500321440269319,-0.412898231167257,-0.323413550925271,-0.187265084647106,
-3.39095613619537E-6),.UNSPECIFIED.);
#3091=B_SPLINE_CURVE_WITH_KNOTS('',3,(#29171,#29172,#29173,#29174,#29175,
#29176,#29177,#29178,#29179,#29180,#29181,#29182,#29183,#29184),
 .UNSPECIFIED.,.F.,.F.,(4,2,2,2,2,2,4),(-0.826160850943245,-0.625506051581447,
-0.500256665182958,-0.412982768745325,-0.32364661298202,-0.187689005830614,
-2.22349760923232E-6),.UNSPECIFIED.);
#3092=B_SPLINE_CURVE_WITH_KNOTS('',3,(#29186,#29187,#29188,#29189,#29190,
#29191,#29192,#29193,#29194,#29195,#29196,#29197,#29198,#29199),
 .UNSPECIFIED.,.F.,.F.,(4,2,2,2,2,2,4),(-0.826160879595277,-0.625505977003457,
-0.500256640017278,-0.412982784293015,-0.32364666891538,-0.187689105820326,
-2.22321261846373E-6),.UNSPECIFIED.);
#3093=B_SPLINE_CURVE_WITH_KNOTS('',3,(#29200,#29201,#29202,#29203,#29204,
#29205,#29206,#29207,#29208,#29209,#29210,#29211,#29212,#29213),
 .UNSPECIFIED.,.F.,.F.,(4,2,2,2,2,2,4),(-0.826160915642974,-0.625505883674515,
-0.500256608569079,-0.41298280385346,-0.323646739070228,-0.187689231114119,
-2.2228657925752E-6),.UNSPECIFIED.);
#3094=B_SPLINE_CURVE_WITH_KNOTS('',3,(#29215,#29216,#29217,#29218,#29219,
#29220,#29221,#29222,#29223,#29224,#29225,#29226,#29227,#29228),
 .UNSPECIFIED.,.F.,.F.,(4,2,2,2,2,2,4),(-0.826003429305969,-0.62577532888724,
-0.500320591570943,-0.412898577030623,-0.323415077693532,-0.187267750985861,
-3.38394675763227E-6),.UNSPECIFIED.);
#3095=B_SPLINE_CURVE_WITH_KNOTS('',3,(#29229,#29230,#29231,#29232,#29233,
#29234,#29235,#29236,#29237,#29238,#29239,#29240,#29241,#29242),
 .UNSPECIFIED.,.F.,.F.,(4,2,2,2,2,2,4),(-0.826161221319965,-0.62550508958843,
-0.500256340925903,-0.412982969744594,-0.323647335030077,-0.187690296611956,
-2.21982746525486E-6),.UNSPECIFIED.);
#3096=B_SPLINE_CURVE_WITH_KNOTS('',3,(#29244,#29245,#29246,#29247,#29248,
#29249,#29250,#29251,#29252,#29253,#29254,#29255,#29256,#29257),
 .UNSPECIFIED.,.F.,.F.,(4,2,2,2,2,2,4),(-0.826003445593229,-0.625775272394187,
-0.500320569483619,-0.41289858605328,-0.323415117472456,-0.187267820460476,
-3.38376405419045E-6),.UNSPECIFIED.);
#3097=B_SPLINE_CURVE_WITH_KNOTS('',3,(#29258,#29259,#29260,#29261,#29262,
#29263,#29264,#29265,#29266,#29267,#29268,#29269,#29270,#29271),
 .UNSPECIFIED.,.F.,.F.,(4,2,2,2,2,2,4),(-0.826161044059727,-0.625505549788039,
-0.500256495976546,-0.412982873543913,-0.32364698958292,-0.187689678975083,
-2.22158898273768E-6),.UNSPECIFIED.);
#3098=B_SPLINE_CURVE_WITH_KNOTS('',3,(#29273,#29274,#29275,#29276,#29277,
#29278,#29279,#29280,#29281,#29282,#29283,#29284,#29285,#29286),
 .UNSPECIFIED.,.F.,.F.,(4,2,2,2,2,2,4),(-0.826160881882804,-0.625505971051268,
-0.500256638009421,-0.412982785535515,-0.32364667338246,-0.187689113806309,
-2.2231898652661E-6),.UNSPECIFIED.);
#3099=B_SPLINE_CURVE_WITH_KNOTS('',3,(#29287,#29288,#29289,#29290,#29291,
#29292,#29293,#29294,#29295,#29296,#29297,#29298,#29299,#29300),
 .UNSPECIFIED.,.F.,.F.,(4,2,2,2,2,2,4),(-0.82616085833322,-0.625506032808248,
-0.500256658885217,-0.412982772751494,-0.323646627203788,-0.187689031131961,
-2.22343578221399E-6),.UNSPECIFIED.);
#3100=B_SPLINE_CURVE_WITH_KNOTS('',3,(#29302,#29303,#29304,#29305,#29306,
#29307,#29308,#29309,#29310,#29311,#29312,#29313,#29314,#29315),
 .UNSPECIFIED.,.F.,.F.,(4,2,2,2,2,2,4),(-0.826002804263561,-0.625777500092833,
-0.500321440933868,-0.412898230909481,-0.32341354975897,-0.187265082612001,
-3.39096154339912E-6),.UNSPECIFIED.);
#3101=B_SPLINE_CURVE_WITH_KNOTS('',3,(#29316,#29317,#29318,#29319,#29320,
#29321,#29322,#29323,#29324,#29325,#29326,#29327,#29328,#29329),
 .UNSPECIFIED.,.F.,.F.,(4,2,2,2,2,2,4),(-0.826002824122889,-0.625777431019925,
-0.500321413899708,-0.412898241904804,-0.323413598347589,-0.187265167461547,
-3.39073857045983E-6),.UNSPECIFIED.);
#3102=B_SPLINE_CURVE_WITH_KNOTS('',3,(#29331,#29332,#29333,#29334,#29335,
#29336,#29337,#29338,#29339,#29340,#29341,#29342,#29343,#29344),
 .UNSPECIFIED.,.F.,.F.,(4,2,2,2,2,2,4),(-0.826160968685895,-0.625505745254935,
-0.500256561845671,-0.412982832646704,-0.323646842781018,-0.187689416644658,
-2.22232665636257E-6),.UNSPECIFIED.);
#3103=B_SPLINE_CURVE_WITH_KNOTS('',3,(#29345,#29346,#29347,#29348,#29349,
#29350,#29351,#29352,#29353,#29354,#29355,#29356,#29357,#29358),
 .UNSPECIFIED.,.F.,.F.,(4,2,2,2,2,2,4),(-0.826003230622126,-0.625776018447498,
-0.500320861233349,-0.412898467008696,-0.323414592324213,-0.18726690330586,
-3.38617589407379E-6),.UNSPECIFIED.);
#3104=B_SPLINE_CURVE_WITH_KNOTS('',3,(#29375,#29376,#29377,#29378),
 .UNSPECIFIED.,.F.,.F.,(4,4),(-0.228509057368285,0.828509057368286),
 .UNSPECIFIED.);
#3105=B_SPLINE_CURVE_WITH_KNOTS('',3,(#29379,#29380,#29381,#29382),
 .UNSPECIFIED.,.F.,.F.,(4,4),(-0.228566601102733,0.828566601102733),
 .UNSPECIFIED.);
#3106=B_SPLINE_CURVE_WITH_KNOTS('',3,(#29399,#29400,#29401,#29402),
 .UNSPECIFIED.,.F.,.F.,(4,4),(-0.228509057368286,0.828509057368286),
 .UNSPECIFIED.);
#3107=B_SPLINE_CURVE_WITH_KNOTS('',3,(#29403,#29404,#29405,#29406),
 .UNSPECIFIED.,.F.,.F.,(4,4),(-0.228566601102733,0.828566601102733),
 .UNSPECIFIED.);
#3108=B_SPLINE_CURVE_WITH_KNOTS('',3,(#29423,#29424,#29425,#29426),
 .UNSPECIFIED.,.F.,.F.,(4,4),(-0.228509057368285,0.828509057368286),
 .UNSPECIFIED.);
#3109=B_SPLINE_CURVE_WITH_KNOTS('',3,(#29427,#29428,#29429,#29430),
 .UNSPECIFIED.,.F.,.F.,(4,4),(-0.228566601102733,0.828566601102733),
 .UNSPECIFIED.);
#3110=B_SPLINE_CURVE_WITH_KNOTS('',3,(#29447,#29448,#29449,#29450),
 .UNSPECIFIED.,.F.,.F.,(4,4),(-0.228509057368286,0.828509057368286),
 .UNSPECIFIED.);
#3111=B_SPLINE_CURVE_WITH_KNOTS('',3,(#29451,#29452,#29453,#29454),
 .UNSPECIFIED.,.F.,.F.,(4,4),(-0.228566601102733,0.828566601102733),
 .UNSPECIFIED.);
#3112=B_SPLINE_CURVE_WITH_KNOTS('',3,(#29471,#29472,#29473,#29474),
 .UNSPECIFIED.,.F.,.F.,(4,4),(-0.228509057368286,0.828509057368286),
 .UNSPECIFIED.);
#3113=B_SPLINE_CURVE_WITH_KNOTS('',3,(#29475,#29476,#29477,#29478),
 .UNSPECIFIED.,.F.,.F.,(4,4),(-0.228566601102733,0.828566601102733),
 .UNSPECIFIED.);
#3114=B_SPLINE_CURVE_WITH_KNOTS('',3,(#29495,#29496,#29497,#29498),
 .UNSPECIFIED.,.F.,.F.,(4,4),(-0.228509057368285,0.828509057368286),
 .UNSPECIFIED.);
#3115=B_SPLINE_CURVE_WITH_KNOTS('',3,(#29499,#29500,#29501,#29502),
 .UNSPECIFIED.,.F.,.F.,(4,4),(-0.228566601102733,0.828566601102733),
 .UNSPECIFIED.);
#3116=B_SPLINE_CURVE_WITH_KNOTS('',3,(#29519,#29520,#29521,#29522),
 .UNSPECIFIED.,.F.,.F.,(4,4),(-0.228509057368285,0.828509057368286),
 .UNSPECIFIED.);
#3117=B_SPLINE_CURVE_WITH_KNOTS('',3,(#29523,#29524,#29525,#29526),
 .UNSPECIFIED.,.F.,.F.,(4,4),(-0.228566601102733,0.828566601102733),
 .UNSPECIFIED.);
#3118=B_SPLINE_CURVE_WITH_KNOTS('',3,(#29543,#29544,#29545,#29546),
 .UNSPECIFIED.,.F.,.F.,(4,4),(-0.228509057368286,0.828509057368286),
 .UNSPECIFIED.);
#3119=B_SPLINE_CURVE_WITH_KNOTS('',3,(#29547,#29548,#29549,#29550),
 .UNSPECIFIED.,.F.,.F.,(4,4),(-0.228566601102733,0.828566601102733),
 .UNSPECIFIED.);
#3120=B_SPLINE_CURVE_WITH_KNOTS('',3,(#29567,#29568,#29569,#29570),
 .UNSPECIFIED.,.F.,.F.,(4,4),(-0.228509057368285,0.828509057368286),
 .UNSPECIFIED.);
#3121=B_SPLINE_CURVE_WITH_KNOTS('',3,(#29571,#29572,#29573,#29574),
 .UNSPECIFIED.,.F.,.F.,(4,4),(-0.228566601102733,0.828566601102733),
 .UNSPECIFIED.);
#3122=B_SPLINE_CURVE_WITH_KNOTS('',3,(#29591,#29592,#29593,#29594),
 .UNSPECIFIED.,.F.,.F.,(4,4),(-0.228509057368285,0.828509057368286),
 .UNSPECIFIED.);
#3123=B_SPLINE_CURVE_WITH_KNOTS('',3,(#29595,#29596,#29597,#29598),
 .UNSPECIFIED.,.F.,.F.,(4,4),(-0.228566601102733,0.828566601102733),
 .UNSPECIFIED.);
#3124=B_SPLINE_CURVE_WITH_KNOTS('',3,(#29615,#29616,#29617,#29618),
 .UNSPECIFIED.,.F.,.F.,(4,4),(-0.228509057368286,0.828509057368286),
 .UNSPECIFIED.);
#3125=B_SPLINE_CURVE_WITH_KNOTS('',3,(#29619,#29620,#29621,#29622),
 .UNSPECIFIED.,.F.,.F.,(4,4),(-0.228566601102733,0.828566601102733),
 .UNSPECIFIED.);
#3126=B_SPLINE_CURVE_WITH_KNOTS('',3,(#29639,#29640,#29641,#29642),
 .UNSPECIFIED.,.F.,.F.,(4,4),(-0.228509057368285,0.828509057368286),
 .UNSPECIFIED.);
#3127=B_SPLINE_CURVE_WITH_KNOTS('',3,(#29643,#29644,#29645,#29646),
 .UNSPECIFIED.,.F.,.F.,(4,4),(-0.228566601102733,0.828566601102733),
 .UNSPECIFIED.);
#3128=B_SPLINE_CURVE_WITH_KNOTS('',3,(#29663,#29664,#29665,#29666),
 .UNSPECIFIED.,.F.,.F.,(4,4),(-0.228509057368285,0.828509057368286),
 .UNSPECIFIED.);
#3129=B_SPLINE_CURVE_WITH_KNOTS('',3,(#29667,#29668,#29669,#29670),
 .UNSPECIFIED.,.F.,.F.,(4,4),(-0.228566601102734,0.828566601102734),
 .UNSPECIFIED.);
#3130=B_SPLINE_CURVE_WITH_KNOTS('',3,(#29687,#29688,#29689,#29690),
 .UNSPECIFIED.,.F.,.F.,(4,4),(-0.228509057368285,0.828509057368286),
 .UNSPECIFIED.);
#3131=B_SPLINE_CURVE_WITH_KNOTS('',3,(#29691,#29692,#29693,#29694),
 .UNSPECIFIED.,.F.,.F.,(4,4),(-0.228566601102733,0.828566601102733),
 .UNSPECIFIED.);
#3132=B_SPLINE_CURVE_WITH_KNOTS('',3,(#29711,#29712,#29713,#29714),
 .UNSPECIFIED.,.F.,.F.,(4,4),(-0.228509057368285,0.828509057368286),
 .UNSPECIFIED.);
#3133=B_SPLINE_CURVE_WITH_KNOTS('',3,(#29715,#29716,#29717,#29718),
 .UNSPECIFIED.,.F.,.F.,(4,4),(-0.228566601102733,0.828566601102733),
 .UNSPECIFIED.);
#3134=B_SPLINE_CURVE_WITH_KNOTS('',3,(#29735,#29736,#29737,#29738),
 .UNSPECIFIED.,.F.,.F.,(4,4),(-0.228509057368285,0.828509057368286),
 .UNSPECIFIED.);
#3135=B_SPLINE_CURVE_WITH_KNOTS('',3,(#29739,#29740,#29741,#29742),
 .UNSPECIFIED.,.F.,.F.,(4,4),(-0.228566601102733,0.828566601102733),
 .UNSPECIFIED.);
#3136=B_SPLINE_CURVE_WITH_KNOTS('',3,(#29759,#29760,#29761,#29762),
 .UNSPECIFIED.,.F.,.F.,(4,4),(-0.228509057368285,0.828509057368286),
 .UNSPECIFIED.);
#3137=B_SPLINE_CURVE_WITH_KNOTS('',3,(#29763,#29764,#29765,#29766),
 .UNSPECIFIED.,.F.,.F.,(4,4),(-0.228566601102733,0.828566601102733),
 .UNSPECIFIED.);
#3138=B_SPLINE_CURVE_WITH_KNOTS('',3,(#29783,#29784,#29785,#29786),
 .UNSPECIFIED.,.F.,.F.,(4,4),(-0.228509057368285,0.828509057368286),
 .UNSPECIFIED.);
#3139=B_SPLINE_CURVE_WITH_KNOTS('',3,(#29787,#29788,#29789,#29790),
 .UNSPECIFIED.,.F.,.F.,(4,4),(-0.228566601102733,0.828566601102733),
 .UNSPECIFIED.);
#3140=B_SPLINE_CURVE_WITH_KNOTS('',3,(#29819,#29820,#29821,#29822),
 .UNSPECIFIED.,.F.,.F.,(4,4),(-0.228509057368286,0.828509057368286),
 .UNSPECIFIED.);
#3141=B_SPLINE_CURVE_WITH_KNOTS('',3,(#29907,#29908,#29909,#29910),
 .UNSPECIFIED.,.F.,.F.,(4,4),(-0.228509057368286,0.828509057368286),
 .UNSPECIFIED.);
#3142=B_SPLINE_CURVE_WITH_KNOTS('',3,(#29999,#30000,#30001,#30002),
 .UNSPECIFIED.,.F.,.F.,(4,4),(-0.228509057368285,0.828509057368286),
 .UNSPECIFIED.);
#3143=B_SPLINE_CURVE_WITH_KNOTS('',3,(#30091,#30092,#30093,#30094),
 .UNSPECIFIED.,.F.,.F.,(4,4),(-0.228509057368286,0.828509057368286),
 .UNSPECIFIED.);
#3144=B_SPLINE_CURVE_WITH_KNOTS('',3,(#30183,#30184,#30185,#30186),
 .UNSPECIFIED.,.F.,.F.,(4,4),(-0.228509057368286,0.828509057368286),
 .UNSPECIFIED.);
#3145=B_SPLINE_CURVE_WITH_KNOTS('',3,(#30279,#30280,#30281,#30282),
 .UNSPECIFIED.,.F.,.F.,(4,4),(-0.228509057368287,0.828509057368287),
 .UNSPECIFIED.);
#3146=B_SPLINE_CURVE_WITH_KNOTS('',3,(#30371,#30372,#30373,#30374),
 .UNSPECIFIED.,.F.,.F.,(4,4),(-0.228509057368286,0.828509057368286),
 .UNSPECIFIED.);
#3147=B_SPLINE_CURVE_WITH_KNOTS('',3,(#30467,#30468,#30469,#30470),
 .UNSPECIFIED.,.F.,.F.,(4,4),(-0.228509057368286,0.828509057368286),
 .UNSPECIFIED.);
#3148=B_SPLINE_CURVE_WITH_KNOTS('',3,(#30559,#30560,#30561,#30562),
 .UNSPECIFIED.,.F.,.F.,(4,4),(-0.228509057368286,0.828509057368286),
 .UNSPECIFIED.);
#3149=B_SPLINE_CURVE_WITH_KNOTS('',3,(#30651,#30652,#30653,#30654),
 .UNSPECIFIED.,.F.,.F.,(4,4),(-0.228509057368286,0.828509057368287),
 .UNSPECIFIED.);
#3150=B_SPLINE_CURVE_WITH_KNOTS('',3,(#30743,#30744,#30745,#30746),
 .UNSPECIFIED.,.F.,.F.,(4,4),(-0.228509057368286,0.828509057368286),
 .UNSPECIFIED.);
#3151=B_SPLINE_CURVE_WITH_KNOTS('',3,(#30839,#30840,#30841,#30842),
 .UNSPECIFIED.,.F.,.F.,(4,4),(-0.228509057368285,0.828509057368286),
 .UNSPECIFIED.);
#3152=B_SPLINE_CURVE_WITH_KNOTS('',3,(#30931,#30932,#30933,#30934),
 .UNSPECIFIED.,.F.,.F.,(4,4),(-0.228509057368286,0.828509057368286),
 .UNSPECIFIED.);
#3153=B_SPLINE_CURVE_WITH_KNOTS('',3,(#31023,#31024,#31025,#31026),
 .UNSPECIFIED.,.F.,.F.,(4,4),(-0.228509057368286,0.828509057368286),
 .UNSPECIFIED.);
#3154=B_SPLINE_CURVE_WITH_KNOTS('',3,(#31119,#31120,#31121,#31122),
 .UNSPECIFIED.,.F.,.F.,(4,4),(-0.228509057368286,0.828509057368286),
 .UNSPECIFIED.);
#3155=B_SPLINE_CURVE_WITH_KNOTS('',3,(#31211,#31212,#31213,#31214),
 .UNSPECIFIED.,.F.,.F.,(4,4),(-0.228509057368286,0.828509057368287),
 .UNSPECIFIED.);
#3156=B_SPLINE_CURVE_WITH_KNOTS('',3,(#31307,#31308,#31309,#31310),
 .UNSPECIFIED.,.F.,.F.,(4,4),(-0.228509057368286,0.828509057368286),
 .UNSPECIFIED.);
#3157=B_SPLINE_CURVE_WITH_KNOTS('',3,(#31399,#31400,#31401,#31402),
 .UNSPECIFIED.,.F.,.F.,(4,4),(-0.228509057368285,0.828509057368286),
 .UNSPECIFIED.);
#3158=B_SPLINE_CURVE_WITH_KNOTS('',3,(#31481,#31482,#31483,#31484,#31485,
#31486,#31487,#31488,#31489,#31490,#31491,#31492,#31493),.UNSPECIFIED.,
 .F.,.F.,(4,3,3,3,4),(-0.301665508889116,0.,0.301549467956627,0.603098935913254,
0.904721008425295),.UNSPECIFIED.);
#3159=B_SPLINE_CURVE_WITH_KNOTS('',3,(#31510,#31511,#31512,#31513),
 .UNSPECIFIED.,.F.,.F.,(4,4),(-0.228566601102733,0.828566601102733),
 .UNSPECIFIED.);
#3160=B_SPLINE_CURVE_WITH_KNOTS('',3,(#31531,#31532,#31533,#31534,#31535,
#31536,#31537,#31538,#31539,#31540,#31541,#31542,#31543),.UNSPECIFIED.,
 .F.,.F.,(4,3,3,3,4),(-0.301622072512042,0.,0.301549467956626,0.603098935913254,
0.90476444480237),.UNSPECIFIED.);
#3161=B_SPLINE_CURVE_WITH_KNOTS('',3,(#31548,#31549,#31550,#31551,#31552,
#31553,#31554,#31555,#31556,#31557,#31558,#31559,#31560),.UNSPECIFIED.,
 .F.,.F.,(4,3,3,3,4),(-0.301622072512042,0.,0.301549467956627,0.603098935913254,
0.904764444802371),.UNSPECIFIED.);
#3162=B_SPLINE_CURVE_WITH_KNOTS('',3,(#31563,#31564,#31565,#31566,#31567,
#31568,#31569,#31570,#31571,#31572,#31573,#31574,#31575),.UNSPECIFIED.,
 .F.,.F.,(4,3,3,3,4),(-0.301665508889117,0.,0.301549467956628,0.603098935913255,
0.904721008425297),.UNSPECIFIED.);
#3163=B_SPLINE_CURVE_WITH_KNOTS('',3,(#31594,#31595,#31596,#31597,#31598,
#31599,#31600,#31601,#31602,#31603,#31604,#31605,#31606),.UNSPECIFIED.,
 .F.,.F.,(4,3,3,3,4),(-0.301622072512041,0.,0.301549467956627,0.603098935913255,
0.904764444802372),.UNSPECIFIED.);
#3164=B_SPLINE_CURVE_WITH_KNOTS('',3,(#31608,#31609,#31610,#31611),
 .UNSPECIFIED.,.F.,.F.,(4,4),(-0.228566601102733,0.828566601102733),
 .UNSPECIFIED.);
#3165=B_SPLINE_CURVE_WITH_KNOTS('',3,(#31663,#31664,#31665,#31666,#31667,
#31668,#31669,#31670,#31671,#31672,#31673,#31674,#31675),.UNSPECIFIED.,
 .F.,.F.,(4,3,3,3,4),(-0.301665508889116,0.,0.301549467956627,0.603098935913254,
0.904721008425296),.UNSPECIFIED.);
#3166=B_SPLINE_CURVE_WITH_KNOTS('',3,(#31693,#31694,#31695,#31696,#31697,
#31698,#31699,#31700,#31701,#31702,#31703,#31704,#31705),.UNSPECIFIED.,
 .F.,.F.,(4,3,3,3,4),(-0.301622072512042,0.,0.301549467956626,0.603098935913253,
0.90476444480237),.UNSPECIFIED.);
#3167=B_SPLINE_CURVE_WITH_KNOTS('',3,(#31707,#31708,#31709,#31710),
 .UNSPECIFIED.,.F.,.F.,(4,4),(-0.228566601102733,0.828566601102733),
 .UNSPECIFIED.);
#3168=B_SPLINE_CURVE_WITH_KNOTS('',3,(#31804,#31805,#31806,#31807,#31808,
#31809,#31810,#31811,#31812,#31813,#31814,#31815,#31816),.UNSPECIFIED.,
 .F.,.F.,(4,3,3,3,4),(-0.301665508889116,0.,0.301549467956627,0.603098935913254,
0.904721008425295),.UNSPECIFIED.);
#3169=B_SPLINE_CURVE_WITH_KNOTS('',3,(#31849,#31850,#31851,#31852),
 .UNSPECIFIED.,.F.,.F.,(4,4),(-0.228566601102733,0.828566601102733),
 .UNSPECIFIED.);
#3170=B_SPLINE_CURVE_WITH_KNOTS('',3,(#31869,#31870,#31871,#31872,#31873,
#31874,#31875,#31876,#31877,#31878,#31879,#31880,#31881),.UNSPECIFIED.,
 .F.,.F.,(4,3,3,3,4),(-0.301622072512042,0.,0.301549467956627,0.603098935913254,
0.90476444480237),.UNSPECIFIED.);
#3171=B_SPLINE_CURVE_WITH_KNOTS('',3,(#31884,#31885,#31886,#31887,#31888,
#31889,#31890,#31891,#31892,#31893,#31894,#31895,#31896),.UNSPECIFIED.,
 .F.,.F.,(4,3,3,3,4),(-0.301665508889116,0.,0.301549467956627,0.603098935913254,
0.904721008425296),.UNSPECIFIED.);
#3172=B_SPLINE_CURVE_WITH_KNOTS('',3,(#31913,#31914,#31915,#31916,#31917,
#31918,#31919,#31920,#31921,#31922,#31923,#31924,#31925),.UNSPECIFIED.,
 .F.,.F.,(4,3,3,3,4),(-0.301622072512042,0.,0.301549467956627,0.603098935913254,
0.90476444480237),.UNSPECIFIED.);
#3173=B_SPLINE_CURVE_WITH_KNOTS('',3,(#31926,#31927,#31928,#31929),
 .UNSPECIFIED.,.F.,.F.,(4,4),(-0.228566601102733,0.828566601102733),
 .UNSPECIFIED.);
#3174=B_SPLINE_CURVE_WITH_KNOTS('',3,(#31978,#31979,#31980,#31981,#31982,
#31983,#31984,#31985,#31986,#31987,#31988,#31989,#31990),.UNSPECIFIED.,
 .F.,.F.,(4,3,3,3,4),(-0.301665508889117,0.,0.301549467956627,0.603098935913253,
0.904721008425295),.UNSPECIFIED.);
#3175=B_SPLINE_CURVE_WITH_KNOTS('',3,(#32007,#32008,#32009,#32010,#32011,
#32012,#32013,#32014,#32015,#32016,#32017,#32018,#32019),.UNSPECIFIED.,
 .F.,.F.,(4,3,3,3,4),(-0.301622072512042,0.,0.301549467956627,0.603098935913255,
0.904764444802371),.UNSPECIFIED.);
#3176=B_SPLINE_CURVE_WITH_KNOTS('',3,(#32020,#32021,#32022,#32023),
 .UNSPECIFIED.,.F.,.F.,(4,4),(-0.228566601102733,0.828566601102733),
 .UNSPECIFIED.);
#3177=B_SPLINE_CURVE_WITH_KNOTS('',3,(#32041,#32042,#32043,#32044,#32045,
#32046,#32047,#32048,#32049,#32050,#32051,#32052,#32053),.UNSPECIFIED.,
 .F.,.F.,(4,3,3,3,4),(-0.301665508889116,0.,0.301549467956625,0.603098935913253,
0.904721008425295),.UNSPECIFIED.);
#3178=B_SPLINE_CURVE_WITH_KNOTS('',3,(#32086,#32087,#32088,#32089),
 .UNSPECIFIED.,.F.,.F.,(4,4),(-0.228566601102733,0.828566601102734),
 .UNSPECIFIED.);
#3179=B_SPLINE_CURVE_WITH_KNOTS('',3,(#32106,#32107,#32108,#32109,#32110,
#32111,#32112,#32113,#32114,#32115,#32116,#32117,#32118),.UNSPECIFIED.,
 .F.,.F.,(4,3,3,3,4),(-0.301622072512042,0.,0.301549467956624,0.603098935913253,
0.90476444480237),.UNSPECIFIED.);
#3180=B_SPLINE_CURVE_WITH_KNOTS('',3,(#32121,#32122,#32123,#32124,#32125,
#32126,#32127,#32128,#32129,#32130,#32131,#32132,#32133),.UNSPECIFIED.,
 .F.,.F.,(4,3,3,3,4),(-0.301665508889116,0.,0.301549467956627,0.603098935913255,
0.904721008425296),.UNSPECIFIED.);
#3181=B_SPLINE_CURVE_WITH_KNOTS('',3,(#32150,#32151,#32152,#32153,#32154,
#32155,#32156,#32157,#32158,#32159,#32160,#32161,#32162),.UNSPECIFIED.,
 .F.,.F.,(4,3,3,3,4),(-0.301622072512042,0.,0.301549467956627,0.603098935913254,
0.904764444802371),.UNSPECIFIED.);
#3182=B_SPLINE_CURVE_WITH_KNOTS('',3,(#32163,#32164,#32165,#32166),
 .UNSPECIFIED.,.F.,.F.,(4,4),(-0.228566601102733,0.828566601102733),
 .UNSPECIFIED.);
#3183=B_SPLINE_CURVE_WITH_KNOTS('',3,(#32215,#32216,#32217,#32218,#32219,
#32220,#32221,#32222,#32223,#32224,#32225,#32226,#32227),.UNSPECIFIED.,
 .F.,.F.,(4,3,3,3,4),(-0.301665508889116,0.,0.301549467956627,0.603098935913254,
0.904721008425295),.UNSPECIFIED.);
#3184=B_SPLINE_CURVE_WITH_KNOTS('',3,(#32244,#32245,#32246,#32247,#32248,
#32249,#32250,#32251,#32252,#32253,#32254,#32255,#32256),.UNSPECIFIED.,
 .F.,.F.,(4,3,3,3,4),(-0.301622072512041,0.,0.301549467956627,0.603098935913254,
0.904764444802371),.UNSPECIFIED.);
#3185=B_SPLINE_CURVE_WITH_KNOTS('',3,(#32257,#32258,#32259,#32260),
 .UNSPECIFIED.,.F.,.F.,(4,4),(-0.228566601102733,0.828566601102734),
 .UNSPECIFIED.);
#3186=B_SPLINE_CURVE_WITH_KNOTS('',3,(#32278,#32279,#32280,#32281,#32282,
#32283,#32284,#32285,#32286,#32287,#32288,#32289,#32290),.UNSPECIFIED.,
 .F.,.F.,(4,3,3,3,4),(-0.301665508889116,0.,0.301549467956629,0.603098935913255,
0.904721008425297),.UNSPECIFIED.);
#3187=B_SPLINE_CURVE_WITH_KNOTS('',3,(#32323,#32324,#32325,#32326),
 .UNSPECIFIED.,.F.,.F.,(4,4),(-0.228566601102733,0.828566601102733),
 .UNSPECIFIED.);
#3188=B_SPLINE_CURVE_WITH_KNOTS('',3,(#32343,#32344,#32345,#32346,#32347,
#32348,#32349,#32350,#32351,#32352,#32353,#32354,#32355),.UNSPECIFIED.,
 .F.,.F.,(4,3,3,3,4),(-0.301622072512042,0.,0.301549467956625,0.603098935913252,
0.904764444802369),.UNSPECIFIED.);
#3189=B_SPLINE_CURVE_WITH_KNOTS('',3,(#32358,#32359,#32360,#32361,#32362,
#32363,#32364,#32365,#32366,#32367,#32368,#32369,#32370),.UNSPECIFIED.,
 .F.,.F.,(4,3,3,3,4),(-0.301665508889116,0.,0.301549467956628,0.603098935913255,
0.904721008425296),.UNSPECIFIED.);
#3190=B_SPLINE_CURVE_WITH_KNOTS('',3,(#32387,#32388,#32389,#32390,#32391,
#32392,#32393,#32394,#32395,#32396,#32397,#32398,#32399),.UNSPECIFIED.,
 .F.,.F.,(4,3,3,3,4),(-0.301622072512042,0.,0.301549467956627,0.603098935913253,
0.90476444480237),.UNSPECIFIED.);
#3191=B_SPLINE_CURVE_WITH_KNOTS('',3,(#32400,#32401,#32402,#32403),
 .UNSPECIFIED.,.F.,.F.,(4,4),(-0.228566601102733,0.828566601102734),
 .UNSPECIFIED.);
#3192=B_SPLINE_CURVE_WITH_KNOTS('',3,(#32452,#32453,#32454,#32455,#32456,
#32457,#32458,#32459,#32460,#32461,#32462,#32463,#32464),.UNSPECIFIED.,
 .F.,.F.,(4,3,3,3,4),(-0.301665508889116,0.,0.301549467956626,0.603098935913255,
0.904721008425298),.UNSPECIFIED.);
#3193=B_SPLINE_CURVE_WITH_KNOTS('',3,(#32481,#32482,#32483,#32484,#32485,
#32486,#32487,#32488,#32489,#32490,#32491,#32492,#32493),.UNSPECIFIED.,
 .F.,.F.,(4,3,3,3,4),(-0.301622072512042,0.,0.301549467956627,0.603098935913252,
0.904764444802368),.UNSPECIFIED.);
#3194=B_SPLINE_CURVE_WITH_KNOTS('',3,(#32494,#32495,#32496,#32497),
 .UNSPECIFIED.,.F.,.F.,(4,4),(-0.228566601102733,0.828566601102733),
 .UNSPECIFIED.);
#3195=B_SPLINE_CURVE_WITH_KNOTS('',3,(#32515,#32516,#32517,#32518,#32519,
#32520,#32521,#32522,#32523,#32524,#32525,#32526,#32527),.UNSPECIFIED.,
 .F.,.F.,(4,3,3,3,4),(-0.301665508889117,0.,0.301549467956627,0.603098935913254,
0.904721008425296),.UNSPECIFIED.);
#3196=B_SPLINE_CURVE_WITH_KNOTS('',3,(#32560,#32561,#32562,#32563),
 .UNSPECIFIED.,.F.,.F.,(4,4),(-0.228566601102733,0.828566601102733),
 .UNSPECIFIED.);
#3197=B_SPLINE_CURVE_WITH_KNOTS('',3,(#32580,#32581,#32582,#32583,#32584,
#32585,#32586,#32587,#32588,#32589,#32590,#32591,#32592),.UNSPECIFIED.,
 .F.,.F.,(4,3,3,3,4),(-0.301622072512042,0.,0.301549467956627,0.603098935913254,
0.90476444480237),.UNSPECIFIED.);
#3198=B_SPLINE_CURVE_WITH_KNOTS('',3,(#32595,#32596,#32597,#32598,#32599,
#32600,#32601,#32602,#32603,#32604,#32605,#32606,#32607),.UNSPECIFIED.,
 .F.,.F.,(4,3,3,3,4),(-0.301665508889116,0.,0.301549467956627,0.603098935913254,
0.904721008425295),.UNSPECIFIED.);
#3199=B_SPLINE_CURVE_WITH_KNOTS('',3,(#32624,#32625,#32626,#32627,#32628,
#32629,#32630,#32631,#32632,#32633,#32634,#32635,#32636),.UNSPECIFIED.,
 .F.,.F.,(4,3,3,3,4),(-0.301622072512042,0.,0.301549467956627,0.603098935913254,
0.904764444802371),.UNSPECIFIED.);
#3200=B_SPLINE_CURVE_WITH_KNOTS('',3,(#32637,#32638,#32639,#32640),
 .UNSPECIFIED.,.F.,.F.,(4,4),(-0.228566601102733,0.828566601102733),
 .UNSPECIFIED.);
#3201=B_SPLINE_CURVE_WITH_KNOTS('',3,(#32689,#32690,#32691,#32692,#32693,
#32694,#32695,#32696,#32697,#32698,#32699,#32700,#32701),.UNSPECIFIED.,
 .F.,.F.,(4,3,3,3,4),(-0.301665508889117,0.,0.301549467956628,0.603098935913255,
0.904721008425296),.UNSPECIFIED.);
#3202=B_SPLINE_CURVE_WITH_KNOTS('',3,(#32718,#32719,#32720,#32721,#32722,
#32723,#32724,#32725,#32726,#32727,#32728,#32729,#32730),.UNSPECIFIED.,
 .F.,.F.,(4,3,3,3,4),(-0.301622072512041,0.,0.301549467956627,0.603098935913255,
0.904764444802371),.UNSPECIFIED.);
#3203=B_SPLINE_CURVE_WITH_KNOTS('',3,(#32731,#32732,#32733,#32734),
 .UNSPECIFIED.,.F.,.F.,(4,4),(-0.228566601102733,0.828566601102733),
 .UNSPECIFIED.);
#3204=B_SPLINE_CURVE_WITH_KNOTS('',3,(#32752,#32753,#32754,#32755,#32756,
#32757,#32758,#32759,#32760,#32761,#32762,#32763,#32764),.UNSPECIFIED.,
 .F.,.F.,(4,3,3,3,4),(-0.301665508889117,0.,0.301549467956625,0.603098935913254,
0.904721008425296),.UNSPECIFIED.);
#3205=B_SPLINE_CURVE_WITH_KNOTS('',3,(#32797,#32798,#32799,#32800),
 .UNSPECIFIED.,.F.,.F.,(4,4),(-0.228566601102733,0.828566601102733),
 .UNSPECIFIED.);
#3206=B_SPLINE_CURVE_WITH_KNOTS('',3,(#32817,#32818,#32819,#32820,#32821,
#32822,#32823,#32824,#32825,#32826,#32827,#32828,#32829),.UNSPECIFIED.,
 .F.,.F.,(4,3,3,3,4),(-0.301622072512042,0.,0.301549467956625,0.603098935913253,
0.90476444480237),.UNSPECIFIED.);
#3207=B_SPLINE_CURVE_WITH_KNOTS('',3,(#32832,#32833,#32834,#32835,#32836,
#32837,#32838,#32839,#32840,#32841,#32842,#32843,#32844),.UNSPECIFIED.,
 .F.,.F.,(4,3,3,3,4),(-0.301665508889116,0.,0.301549467956627,0.603098935913254,
0.904721008425295),.UNSPECIFIED.);
#3208=B_SPLINE_CURVE_WITH_KNOTS('',3,(#32861,#32862,#32863,#32864,#32865,
#32866,#32867,#32868,#32869,#32870,#32871,#32872,#32873),.UNSPECIFIED.,
 .F.,.F.,(4,3,3,3,4),(-0.301622072512042,0.,0.301549467956627,0.603098935913254,
0.90476444480237),.UNSPECIFIED.);
#3209=B_SPLINE_CURVE_WITH_KNOTS('',3,(#32874,#32875,#32876,#32877),
 .UNSPECIFIED.,.F.,.F.,(4,4),(-0.228566601102733,0.828566601102733),
 .UNSPECIFIED.);
#3210=B_SPLINE_CURVE_WITH_KNOTS('',3,(#32926,#32927,#32928,#32929,#32930,
#32931,#32932,#32933,#32934,#32935,#32936,#32937,#32938),.UNSPECIFIED.,
 .F.,.F.,(4,3,3,3,4),(-0.301665508889116,0.,0.301549467956627,0.603098935913253,
0.904721008425295),.UNSPECIFIED.);
#3211=B_SPLINE_CURVE_WITH_KNOTS('',3,(#32955,#32956,#32957,#32958),
 .UNSPECIFIED.,.F.,.F.,(4,4),(-0.228566601102733,0.828566601102733),
 .UNSPECIFIED.);
#3212=B_SPLINE_CURVE_WITH_KNOTS('',3,(#33021,#33022,#33023,#33024,#33025,
#33026,#33027,#33028,#33029,#33030,#33031,#33032,#33033,#33034,#33035,#33036,
#33037,#33038,#33039,#33040,#33041,#33042,#33043,#33044,#33045,#33046,#33047,
#33048,#33049,#33050,#33051,#33052,#33053,#33054,#33055,#33056,#33057,#33058,
#33059,#33060,#33061,#33062,#33063,#33064,#33065,#33066,#33067,#33068,#33069,
#33070,#33071,#33072,#33073,#33074,#33075,#33076,#33077,#33078,#33079,#33080,
#33081,#33082,#33083,#33084,#33085,#33086,#33087,#33088,#33089,#33090,#33091,
#33092,#33093,#33094,#33095,#33096,#33097,#33098,#33099,#33100,#33101,#33102,
#33103,#33104,#33105,#33106,#33107,#33108,#33109,#33110,#33111,#33112,#33113,
#33114,#33115,#33116,#33117,#33118,#33119,#33120,#33121,#33122,#33123,#33124,
#33125,#33126,#33127,#33128,#33129,#33130,#33131,#33132,#33133,#33134,#33135,
#33136,#33137,#33138,#33139,#33140,#33141,#33142,#33143,#33144,#33145,#33146,
#33147,#33148,#33149,#33150,#33151,#33152,#33153),.UNSPECIFIED.,.F.,.F.,
(4,3,3,3,3,3,3,3,3,3,3,3,3,3,3,3,3,3,3,3,3,3,3,3,3,3,3,3,3,3,3,3,3,3,3,
3,3,3,3,3,3,3,3,3,4),(10.3763813528868,10.4542262130358,10.5320112120275,
10.6097514308222,10.6874619179396,10.7651722203897,10.8428857355022,10.9206160760242,
10.998376861546,11.0762274093604,11.1541256248539,11.2321411003828,11.2937563986016,
11.3696586020076,11.4454654112385,11.5211937028804,11.5968602679744,11.672481832139,
11.7498339506124,11.8254308832918,11.9010358142025,11.9766638237259,12.0553225627761,
12.1310851816833,12.206905521287,12.2828337446297,12.2912987799265,12.3696393822356,
12.4478854133682,12.5260516605635,12.6041528549847,12.6822036816841,12.7602218764032,
12.8382231786224,12.9162208344635,12.99422808542,13.0722915935675,13.1503841976854,
13.2285627052136,13.2888411612514,13.3690518606113,13.449169842401,13.5292322801668,
13.6092374927533,13.661551274788),.UNSPECIFIED.);
#3213=B_SPLINE_CURVE_WITH_KNOTS('',3,(#33156,#33157,#33158,#33159,#33160,
#33161,#33162,#33163,#33164,#33165,#33166,#33167,#33168,#33169,#33170,#33171,
#33172,#33173,#33174,#33175,#33176,#33177,#33178,#33179,#33180,#33181,#33182,
#33183,#33184,#33185,#33186,#33187,#33188,#33189,#33190,#33191,#33192,#33193,
#33194,#33195,#33196,#33197,#33198,#33199,#33200,#33201,#33202,#33203,#33204,
#33205,#33206,#33207,#33208,#33209,#33210,#33211,#33212,#33213,#33214,#33215,
#33216,#33217,#33218,#33219,#33220,#33221,#33222,#33223,#33224,#33225,#33226,
#33227,#33228,#33229,#33230,#33231,#33232,#33233,#33234,#33235,#33236,#33237),
 .UNSPECIFIED.,.F.,.F.,(4,3,3,3,3,3,3,3,3,3,3,3,3,3,3,3,3,3,3,3,3,3,3,3,
3,3,3,4),(11.6150328478191,11.6997920262197,11.784576819193,11.8693764519753,
11.9541615193291,12.0389064356849,12.1138040384816,12.1908442532085,12.2678596835335,
12.3448646842034,12.4218948675792,12.4989390429297,12.576038969133,12.612575229144,
12.7000747491645,12.7875920845772,12.875043992548,12.9624105838022,13.0495747511006,
13.1113464198064,13.1892669318928,13.2671805000566,13.3451005231923,13.4230676270369,
13.5010616179069,13.5791262428044,13.6101176104689,13.6616030987896),
 .UNSPECIFIED.);
#3214=B_SPLINE_CURVE_WITH_KNOTS('',3,(#33243,#33244,#33245,#33246,#33247,
#33248,#33249,#33250,#33251,#33252,#33253,#33254,#33255,#33256,#33257,#33258,
#33259,#33260,#33261,#33262,#33263,#33264,#33265,#33266,#33267,#33268,#33269,
#33270,#33271,#33272,#33273,#33274,#33275,#33276,#33277,#33278,#33279,#33280,
#33281,#33282,#33283,#33284,#33285,#33286,#33287,#33288,#33289,#33290,#33291,
#33292,#33293,#33294,#33295,#33296,#33297,#33298,#33299,#33300,#33301,#33302,
#33303,#33304,#33305,#33306,#33307,#33308,#33309,#33310,#33311,#33312,#33313,
#33314,#33315,#33316,#33317,#33318,#33319,#33320,#33321,#33322,#33323,#33324,
#33325,#33326,#33327,#33328,#33329,#33330,#33331,#33332,#33333,#33334,#33335,
#33336,#33337,#33338,#33339,#33340,#33341,#33342,#33343,#33344,#33345,#33346,
#33347,#33348,#33349,#33350,#33351,#33352,#33353,#33354,#33355,#33356,#33357,
#33358,#33359,#33360,#33361,#33362,#33363,#33364,#33365,#33366,#33367,#33368,
#33369,#33370,#33371,#33372,#33373,#33374,#33375,#33376,#33377,#33378,#33379,
#33380,#33381,#33382,#33383,#33384,#33385,#33386,#33387,#33388,#33389,#33390,
#33391,#33392,#33393,#33394,#33395,#33396,#33397,#33398,#33399),
 .UNSPECIFIED.,.F.,.F.,(4,3,3,3,3,3,3,3,3,3,3,3,3,3,3,3,3,3,3,3,3,3,3,3,
3,3,3,3,3,3,3,3,3,3,3,3,3,3,3,3,3,3,3,3,3,3,3,3,3,3,3,3,4),(15.7079632679497,
15.7904254740499,15.8728873318523,15.9553488482074,16.0378100299651,16.1202708839753,
16.2027314170874,16.2851916361505,16.3676515480136,16.4501111595253,16.532570477534,
16.615029508888,16.6974882604348,16.7799467390223,16.8624049514979,16.9448629047087,
17.0273206055016,17.1097780607235,17.1922352772208,17.2782479725068,17.3615727710651,
17.444039376657,17.5265051380402,17.6089700826299,17.6914342378382,17.7738976310748,
17.8563602897465,17.9388222412576,18.02128351301,18.1037441324032,18.1862041268344,
18.2686635236985,18.3511223503886,18.4335806342956,18.5160384028087,18.5984956833151,
18.6826297985062,18.7650957968661,18.8475601734724,18.9300230379678,19.0124844999741,
19.0949446690934,19.1774036549095,19.2598615669898,19.3454590619128,19.4279237989587,
19.510385571345,19.5928448175101,19.6753019757488,19.7577644948314,19.8402221662423,
19.9226809574354,19.9446415263734),.UNSPECIFIED.);
#3215=B_SPLINE_CURVE_WITH_KNOTS('',3,(#33400,#33401,#33402,#33403,#33404,
#33405,#33406,#33407,#33408,#33409,#33410,#33411,#33412,#33413,#33414,#33415,
#33416,#33417,#33418,#33419,#33420,#33421,#33422,#33423,#33424,#33425,#33426,
#33427,#33428,#33429,#33430,#33431,#33432,#33433,#33434,#33435,#33436,#33437,
#33438,#33439,#33440,#33441,#33442,#33443,#33444,#33445,#33446,#33447,#33448,
#33449,#33450,#33451,#33452,#33453,#33454,#33455,#33456,#33457,#33458,#33459,
#33460,#33461,#33462,#33463,#33464,#33465,#33466,#33467,#33468,#33469,#33470,
#33471,#33472,#33473,#33474,#33475,#33476,#33477,#33478,#33479,#33480,#33481),
 .UNSPECIFIED.,.F.,.F.,(4,3,3,3,3,3,3,3,3,3,3,3,3,3,3,3,3,3,3,3,3,3,3,3,
3,3,3,4),(13.661551274788,13.741495797514,13.7876123519139,13.8684595437818,
13.9493475468375,14.0336065457722,14.1146338308566,14.1957114478603,14.2768739065073,
14.2863835425763,14.3718154735951,14.4571706791758,14.5423736904682,14.6274672692567,
14.7123617066816,14.7851547332388,14.8616903646453,14.938220499497,15.0147597510167,
15.0913547207395,15.1679808823156,15.2446904324708,15.2839259239012,15.3707393590102,
15.457380599417,15.5438881964551,15.6301266039185,15.7079632679497),
 .UNSPECIFIED.);
#3216=B_SPLINE_CURVE_WITH_KNOTS('',3,(#33483,#33484,#33485,#33486,#33487,
#33488,#33489,#33490,#33491,#33492,#33493,#33494,#33495,#33496,#33497,#33498,
#33499,#33500,#33501,#33502,#33503,#33504,#33505,#33506,#33507,#33508,#33509,
#33510,#33511,#33512,#33513,#33514,#33515,#33516,#33517,#33518,#33519,#33520,
#33521,#33522,#33523,#33524,#33525,#33526,#33527,#33528,#33529,#33530,#33531,
#33532,#33533,#33534,#33535,#33536,#33537,#33538,#33539,#33540,#33541,#33542,
#33543,#33544,#33545,#33546,#33547,#33548,#33549,#33550,#33551,#33552,#33553,
#33554,#33555,#33556,#33557,#33558,#33559,#33560,#33561,#33562,#33563,#33564),
 .UNSPECIFIED.,.F.,.F.,(4,3,3,3,3,3,3,3,3,3,3,3,3,3,3,3,3,3,3,3,3,3,3,3,
3,3,3,4),(13.6616030987896,13.7400509247693,13.8184450987703,13.8967997953241,
13.9751291593552,14.05419551341,14.132535823946,14.2108945399217,14.2892844834101,
14.368878360506,14.4474090346784,14.5275345132361,14.6076599917938,14.6835621951998,
14.7593690044307,14.8350972960725,14.9107638611665,14.9863854253312,15.0637375438047,
15.139334476484,15.2149394073948,15.2905674169182,15.3692261559683,15.4449887748756,
15.5208091144791,15.5967373378218,15.6052023731187,15.7079632679496),
 .UNSPECIFIED.);
#3217=B_SPLINE_CURVE_WITH_KNOTS('',3,(#33565,#33566,#33567,#33568,#33569,
#33570,#33571,#33572,#33573,#33574,#33575,#33576,#33577,#33578,#33579,#33580,
#33581,#33582,#33583,#33584,#33585,#33586,#33587,#33588,#33589,#33590,#33591,
#33592,#33593,#33594,#33595,#33596,#33597,#33598,#33599,#33600,#33601,#33602,
#33603,#33604,#33605,#33606,#33607,#33608,#33609,#33610,#33611,#33612,#33613,
#33614,#33615,#33616,#33617,#33618,#33619,#33620,#33621,#33622,#33623,#33624,
#33625,#33626,#33627,#33628,#33629,#33630,#33631,#33632,#33633,#33634,#33635,
#33636,#33637,#33638,#33639,#33640,#33641,#33642,#33643,#33644,#33645,#33646,
#33647,#33648,#33649,#33650,#33651,#33652,#33653,#33654,#33655,#33656,#33657,
#33658,#33659,#33660,#33661,#33662,#33663,#33664,#33665,#33666,#33667,#33668,
#33669,#33670,#33671,#33672,#33673,#33674,#33675,#33676,#33677,#33678,#33679,
#33680,#33681,#33682,#33683,#33684,#33685,#33686,#33687,#33688,#33689,#33690,
#33691,#33692,#33693,#33694,#33695,#33696,#33697,#33698,#33699,#33700,#33701,
#33702,#33703,#33704,#33705,#33706,#33707,#33708,#33709,#33710,#33711,#33712,
#33713,#33714,#33715,#33716,#33717,#33718,#33719,#33720,#33721,#33722,#33723,
#33724,#33725,#33726,#33727,#33728,#33729,#33730,#33731,#33732,#33733,#33734,
#33735,#33736),.UNSPECIFIED.,.F.,.F.,(4,3,3,3,3,3,3,3,3,3,3,3,3,3,3,3,3,
3,3,3,3,3,3,3,3,3,3,3,3,3,3,3,3,3,3,3,3,3,3,3,3,3,3,3,3,3,3,3,3,3,3,3,3,
3,3,3,3,4),(15.7079632680317,15.7849462163073,15.8618387115719,15.9386569259526,
16.0154169733244,16.0921360340367,16.1688338913552,16.2455250521911,16.3222240170258,
16.3989783335857,16.475762449498,16.5526324844258,16.6027447544436,16.6829440681553,
16.7630727326106,16.8431403640705,16.9231458883287,17.0031134951737,17.0830489458154,
17.101515945106,17.1823631369738,17.2632511400294,17.3475101389642,17.4285374240485,
17.509615041052,17.5907774996986,17.6002871357685,17.6857190667875,17.7710742723682,
17.8562772836606,17.9413708624499,18.026265299875,18.0990583264309,18.1755939578373,
18.252124092689,18.3286633442088,18.4052583139318,18.4818844755075,18.5585940256627,
18.5978295170934,18.6773734409489,18.7568570513369,18.8362926202057,18.9156923820079,
18.9950685426141,19.0744458783739,19.15382588468,19.2332196505527,19.3126382726157,
19.3921281193603,19.4716563839099,19.5512731075891,19.5953718984182,19.6730799420205,
19.7506743995356,19.8282033634491,19.9056683807068,19.9450135134811),
 .UNSPECIFIED.);
#3218=B_SPLINE_CURVE_WITH_KNOTS('',3,(#33742,#33743,#33744,#33745,#33746,
#33747,#33748,#33749,#33750,#33751,#33752,#33753,#33754,#33755,#33756,#33757,
#33758,#33759,#33760,#33761,#33762,#33763,#33764,#33765,#33766,#33767,#33768,
#33769,#33770,#33771,#33772,#33773,#33774,#33775,#33776,#33777,#33778,#33779,
#33780,#33781,#33782,#33783,#33784,#33785,#33786,#33787,#33788,#33789,#33790,
#33791,#33792,#33793,#33794,#33795,#33796,#33797,#33798,#33799,#33800,#33801,
#33802,#33803,#33804,#33805,#33806,#33807,#33808,#33809,#33810,#33811,#33812,
#33813,#33814,#33815,#33816,#33817,#33818,#33819,#33820,#33821,#33822,#33823,
#33824,#33825,#33826,#33827,#33828,#33829,#33830,#33831,#33832,#33833,#33834,
#33835,#33836,#33837,#33838,#33839,#33840,#33841,#33842,#33843,#33844,#33845,
#33846,#33847,#33848,#33849,#33850,#33851,#33852,#33853,#33854,#33855,#33856,
#33857,#33858,#33859,#33860,#33861,#33862,#33863,#33864,#33865,#33866,#33867,
#33868,#33869,#33870,#33871,#33872,#33873,#33874,#33875,#33876,#33877,#33878,
#33879,#33880,#33881,#33882,#33883,#33884,#33885,#33886,#33887,#33888,#33889,
#33890,#33891,#33892,#33893,#33894,#33895,#33896,#33897,#33898,#33899,#33900,
#33901,#33902,#33903,#33904,#33905,#33906,#33907,#33908,#33909,#33910),
 .UNSPECIFIED.,.F.,.F.,(4,3,3,3,3,3,3,3,3,3,3,3,3,3,3,3,3,3,3,3,3,3,3,3,
3,3,3,3,3,3,3,3,3,3,3,3,3,3,3,3,3,3,3,3,3,3,3,3,3,3,3,3,3,3,3,3,4),(21.9911485751293,
22.073370029129,22.155701741496,22.2382025518265,22.2667225931755,22.3462744183194,
22.425766113522,22.5052099311933,22.5846180863565,22.6640027655525,22.7433887585426,
22.8227774964882,22.9021800515031,22.9816075033574,23.0611061827488,23.1406432843994,
23.2202687745103,23.2642649745004,23.3419325004101,23.4195140009868,23.4970233972062,
23.5744643131551,23.6518655530078,23.7292409089966,23.7630361651628,23.8465275840083,
23.9301752008269,24.0140603945263,24.0980591432093,24.1822433689923,24.2618073558252,
24.3393164898074,24.416743766626,24.4941048029902,24.5714151681249,24.6486903944456,
24.7259588996925,24.8032266354315,24.8805076379063,24.9578159481874,25.0352120613664,
25.1126538238102,25.1902150126104,25.2593497371501,25.3354175880398,25.4113904191998,
25.4872850100609,25.5631180600763,25.6389062073172,25.7146753715244,25.7904368441565,
25.8662056235072,25.9419967122486,26.0178685005078,26.0937833120982,26.1698103065359,
26.2271380078629),.UNSPECIFIED.);
#3219=B_SPLINE_CURVE_WITH_KNOTS('',3,(#33911,#33912,#33913,#33914,#33915,
#33916,#33917,#33918,#33919,#33920,#33921,#33922,#33923,#33924,#33925,#33926,
#33927,#33928,#33929,#33930,#33931,#33932,#33933,#33934,#33935,#33936,#33937,
#33938,#33939,#33940,#33941,#33942,#33943,#33944,#33945,#33946,#33947,#33948,
#33949,#33950,#33951,#33952,#33953,#33954,#33955,#33956,#33957,#33958,#33959,
#33960,#33961,#33962,#33963,#33964,#33965,#33966,#33967,#33968,#33969,#33970,
#33971,#33972,#33973,#33974,#33975,#33976,#33977,#33978,#33979,#33980,#33981,
#33982,#33983,#33984,#33985,#33986),.UNSPECIFIED.,.F.,.F.,(4,3,3,3,3,3,
3,3,3,3,3,3,3,3,3,3,3,3,3,3,3,3,3,3,3,4),(19.9446415263734,20.0271031301035,
20.1095640679554,20.1920243673274,20.2744840556157,20.356943160214,20.4394017085145,
20.521859727907,20.6043172457797,20.690994203864,20.7734609894051,20.855926102473,
20.938389652721,21.0208517497802,21.1033125032619,21.1857720227579,21.268230417843,
21.3506877980765,21.4331541837626,21.5156173852708,21.5980778411205,21.680535989675,
21.7630015934287,21.8454614718166,21.9279255830689,21.9911485751293),
 .UNSPECIFIED.);
#3220=B_SPLINE_CURVE_WITH_KNOTS('',3,(#33988,#33989,#33990,#33991,#33992,
#33993,#33994,#33995,#33996,#33997,#33998,#33999,#34000,#34001,#34002,#34003,
#34004,#34005,#34006,#34007,#34008,#34009,#34010,#34011,#34012,#34013,#34014,
#34015,#34016,#34017,#34018,#34019,#34020,#34021,#34022,#34023,#34024,#34025,
#34026,#34027,#34028,#34029,#34030,#34031,#34032,#34033,#34034,#34035,#34036,
#34037,#34038,#34039,#34040,#34041,#34042,#34043,#34044,#34045,#34046,#34047,
#34048,#34049,#34050,#34051,#34052,#34053,#34054,#34055,#34056,#34057,#34058,
#34059,#34060,#34061,#34062,#34063,#34064,#34065,#34066),.UNSPECIFIED.,
 .F.,.F.,(4,3,3,3,3,3,3,3,3,3,3,3,3,3,3,3,3,3,3,3,3,3,3,3,3,3,4),(19.9450135134811,
20.022424916161,20.0941430890807,20.1776176136089,20.2612475490833,20.3451141481709,
20.429093879934,20.5132587154843,20.5929142797431,20.6704251919161,20.7478542711913,
20.8252171322539,20.9025293423276,20.9798064318453,21.0570768215095,21.1343464544012,
21.2116293650211,21.2889395927012,21.3663376273369,21.4437813163736,21.5213444218647,
21.590456661068,21.6752450130628,21.7596553082193,21.843836383805,21.927646354891,
21.9911485750275),.UNSPECIFIED.);
#3221=B_SPLINE_CURVE_WITH_KNOTS('',3,(#34067,#34068,#34069,#34070,#34071,
#34072,#34073,#34074,#34075,#34076,#34077,#34078,#34079,#34080,#34081,#34082,
#34083,#34084,#34085,#34086,#34087,#34088,#34089,#34090,#34091,#34092,#34093,
#34094,#34095,#34096,#34097,#34098,#34099,#34100,#34101,#34102,#34103,#34104,
#34105,#34106,#34107,#34108,#34109,#34110,#34111,#34112,#34113,#34114,#34115,
#34116,#34117,#34118,#34119,#34120,#34121,#34122,#34123,#34124,#34125,#34126,
#34127,#34128,#34129,#34130,#34131,#34132,#34133,#34134,#34135,#34136,#34137,
#34138,#34139,#34140,#34141,#34142,#34143,#34144,#34145,#34146,#34147,#34148,
#34149,#34150,#34151,#34152,#34153,#34154,#34155,#34156,#34157,#34158,#34159,
#34160,#34161,#34162,#34163,#34164,#34165,#34166,#34167,#34168,#34169,#34170,
#34171,#34172,#34173,#34174,#34175,#34176,#34177,#34178,#34179,#34180,#34181,
#34182,#34183,#34184,#34185,#34186,#34187,#34188,#34189,#34190,#34191,#34192,
#34193,#34194,#34195,#34196,#34197,#34198,#34199,#34200,#34201,#34202,#34203,
#34204,#34205,#34206,#34207,#34208,#34209,#34210,#34211,#34212,#34213,#34214,
#34215,#34216,#34217,#34218,#34219,#34220,#34221,#34222,#34223,#34224,#34225,
#34226,#34227,#34228,#34229,#34230,#34231,#34232),.UNSPECIFIED.,.F.,.F.,
(4,3,3,3,3,3,3,3,3,3,3,3,3,3,3,3,3,3,3,3,3,3,3,3,3,3,3,3,3,3,3,3,3,3,3,
3,3,3,3,3,3,3,3,3,3,3,3,3,3,3,3,3,3,3,3,4),(21.9911485751292,22.0677279286661,
22.1443208546211,22.2209417323296,22.2976049553143,22.3743782822554,22.4512108540594,
22.5281806705101,22.5879990423929,22.6665430117807,22.7449944002324,22.8233677018931,
22.9016773555741,22.9799377545146,23.0581663790971,23.1363785062284,23.2145871226706,
23.292805210708,23.3710782257912,23.4493797856809,23.5277645894362,23.5855414237178,
23.6651913214119,23.7447710878953,23.8242916009709,23.9037553722185,23.9831850756206,
24.0625903140226,24.0843126143803,24.165544261595,24.2468245668753,24.3308893764171,
24.4123210884906,24.4977024467667,24.5830838050427,24.668316709238,24.7534716491106,
24.8384765617015,24.9233748283101,25.0080813472925,25.0818549957052,25.1584140398398,
25.2349676874553,25.3115305349992,25.3881491510158,25.4647990040214,25.541532203083,
25.5806261863676,25.6614896806779,25.7409766543074,25.820418302191,25.8998257438916,
25.9817528431312,26.0611329043551,26.1443335226025,26.2275341408499),
 .UNSPECIFIED.);
#3222=B_SPLINE_CURVE_WITH_KNOTS('',3,(#34238,#34239,#34240,#34241,#34242,
#34243,#34244,#34245,#34246,#34247,#34248,#34249,#34250,#34251,#34252,#34253,
#34254,#34255,#34256,#34257,#34258,#34259,#34260,#34261,#34262,#34263,#34264,
#34265,#34266,#34267,#34268,#34269,#34270,#34271,#34272,#34273,#34274,#34275,
#34276,#34277,#34278,#34279,#34280,#34281,#34282,#34283,#34284,#34285,#34286,
#34287,#34288,#34289,#34290,#34291,#34292,#34293,#34294,#34295,#34296,#34297,
#34298,#34299,#34300,#34301,#34302,#34303,#34304,#34305,#34306,#34307,#34308,
#34309,#34310,#34311,#34312,#34313,#34314,#34315,#34316,#34317,#34318,#34319,
#34320,#34321,#34322,#34323,#34324,#34325,#34326,#34327,#34328,#34329,#34330,
#34331,#34332,#34333,#34334,#34335,#34336,#34337,#34338,#34339,#34340,#34341,
#34342,#34343,#34344,#34345,#34346,#34347,#34348,#34349,#34350,#34351,#34352,
#34353,#34354,#34355,#34356,#34357,#34358,#34359,#34360,#34361,#34362,#34363,
#34364,#34365,#34366,#34367,#34368,#34369,#34370,#34371,#34372,#34373,#34374,
#34375,#34376,#34377,#34378,#34379,#34380,#34381,#34382,#34383,#34384,#34385,
#34386,#34387,#34388,#34389,#34390,#34391,#34392,#34393,#34394,#34395,#34396,
#34397,#34398,#34399,#34400,#34401,#34402,#34403,#34404,#34405,#34406),
 .UNSPECIFIED.,.F.,.F.,(4,3,3,3,3,3,3,3,3,3,3,3,3,3,3,3,3,3,3,3,3,3,3,3,
3,3,3,3,3,3,3,3,3,3,3,3,3,3,3,3,3,3,3,3,3,3,3,3,3,3,3,3,3,3,3,3,4),(28.2743338824462,
28.3590289334677,28.44363761919,28.5280966928244,28.6124520888738,28.6966366011039,
28.7507480717873,28.8273070368857,28.9038606041814,28.9804233701809,29.0570419030758,
29.1336916720016,29.2104247859257,29.2495192624497,29.3290711268508,29.4085628622027,
29.4880067208172,29.5674149176193,29.6467996390536,29.7261856749325,29.805574456112,
29.884977054621,29.9644045501444,30.0439032731761,30.1234404184638,30.2030659518213,
30.2470616437746,30.3247291240364,30.4023105791433,30.4798199301175,30.5572608012783,
30.6346619966133,30.7120373086158,30.745832834437,30.8293242800933,30.9129719248353,
30.9968571476967,31.0808559260971,31.1650401820043,31.2446040250995,31.3221131579345,
31.3995404336048,31.4769014688208,31.5542118328085,31.6314870579847,31.7087555620954,
31.7860232967032,31.8633042980531,31.9406126072162,32.0180087192952,32.0954504806473,
32.1730116683798,32.2421464064244,32.3182081524628,32.394186612896,32.4700773700093,
32.5118535701146),.UNSPECIFIED.);
#3223=B_SPLINE_CURVE_WITH_KNOTS('',3,(#34407,#34408,#34409,#34410,#34411,
#34412,#34413,#34414,#34415,#34416,#34417,#34418,#34419,#34420,#34421,#34422,
#34423,#34424,#34425,#34426,#34427,#34428,#34429,#34430,#34431,#34432,#34433,
#34434,#34435,#34436,#34437,#34438,#34439,#34440,#34441,#34442,#34443,#34444,
#34445,#34446,#34447,#34448,#34449,#34450,#34451,#34452,#34453,#34454,#34455,
#34456,#34457,#34458,#34459,#34460,#34461,#34462,#34463,#34464,#34465,#34466,
#34467,#34468,#34469,#34470,#34471,#34472,#34473,#34474,#34475,#34476,#34477,
#34478,#34479,#34480,#34481,#34482,#34483,#34484,#34485,#34486,#34487,#34488,
#34489,#34490,#34491),.UNSPECIFIED.,.F.,.F.,(4,3,3,3,3,3,3,3,3,3,3,3,3,
3,3,3,3,3,3,3,3,3,3,3,3,3,3,3,4),(26.2271380078629,26.256892118475,26.3354367342183,
26.4138887751831,26.49226273455,26.570573050167,26.6488341143124,26.7270634063487,
26.8052762018615,26.8834854867574,26.961704242466,27.039977920359,27.11828014091,
27.1966655962879,27.2544344997999,27.3340835202497,27.4136624120983,27.4931820549764,
27.5726449666423,27.6520738176217,27.7314782172495,27.7532056904624,27.8344377442233,
27.9157184632528,27.9997830677208,28.081215203302,28.1665960422134,28.2519768811248,
28.2743338823089),.UNSPECIFIED.);
#3224=B_SPLINE_CURVE_WITH_KNOTS('',3,(#34493,#34494,#34495,#34496,#34497,
#34498,#34499,#34500,#34501,#34502,#34503,#34504,#34505,#34506,#34507,#34508,
#34509,#34510,#34511,#34512,#34513,#34514,#34515,#34516,#34517,#34518,#34519,
#34520,#34521,#34522,#34523,#34524,#34525,#34526,#34527,#34528,#34529,#34530,
#34531,#34532,#34533,#34534,#34535,#34536,#34537,#34538,#34539,#34540,#34541,
#34542,#34543,#34544,#34545,#34546,#34547,#34548,#34549,#34550,#34551,#34552,
#34553,#34554,#34555,#34556,#34557,#34558,#34559,#34560,#34561,#34562,#34563,
#34564,#34565,#34566,#34567,#34568,#34569,#34570,#34571,#34572,#34573,#34574,
#34575,#34576,#34577),.UNSPECIFIED.,.F.,.F.,(4,3,3,3,3,3,3,3,3,3,3,3,3,
3,3,3,3,3,3,3,3,3,3,3,3,3,3,3,4),(26.2275341408499,26.3069660971924,26.3864696852463,
26.4660131649361,26.5456425040867,26.5781685676925,26.6558360936021,26.7334175941789,
26.8109269903979,26.8883679063466,26.965769146199,27.0431445021878,27.0769397583549,
27.1604311771999,27.2440787940188,27.3279639877182,27.4119627364012,27.4961469621842,
27.5757109490174,27.6518730153432,27.7296806237139,27.8056774912106,27.8816299400362,
27.9575529772358,28.0367482035041,28.1126749107235,28.1886139449045,28.2645985897077,
28.2743338823088),.UNSPECIFIED.);
#3225=B_SPLINE_CURVE_WITH_KNOTS('',3,(#34578,#34579,#34580,#34581,#34582,
#34583,#34584,#34585,#34586,#34587,#34588,#34589,#34590,#34591,#34592,#34593,
#34594,#34595,#34596,#34597,#34598,#34599,#34600,#34601,#34602,#34603,#34604,
#34605,#34606,#34607,#34608,#34609,#34610,#34611,#34612,#34613,#34614,#34615,
#34616,#34617,#34618,#34619,#34620,#34621,#34622,#34623,#34624,#34625,#34626,
#34627,#34628,#34629,#34630,#34631,#34632,#34633,#34634,#34635,#34636,#34637,
#34638,#34639,#34640,#34641,#34642,#34643,#34644,#34645,#34646,#34647,#34648,
#34649,#34650,#34651,#34652,#34653,#34654,#34655,#34656,#34657,#34658,#34659,
#34660,#34661,#34662,#34663,#34664,#34665,#34666,#34667,#34668,#34669,#34670,
#34671,#34672,#34673,#34674,#34675,#34676,#34677,#34678,#34679,#34680,#34681,
#34682,#34683,#34684,#34685,#34686,#34687,#34688,#34689,#34690,#34691,#34692,
#34693,#34694,#34695,#34696,#34697,#34698,#34699,#34700,#34701,#34702,#34703,
#34704,#34705,#34706,#34707,#34708,#34709,#34710,#34711,#34712,#34713,#34714,
#34715,#34716,#34717,#34718,#34719,#34720,#34721,#34722,#34723,#34724,#34725,
#34726,#34727,#34728,#34729,#34730,#34731,#34732,#34733,#34734,#34735,#34736,
#34737,#34738,#34739,#34740),.UNSPECIFIED.,.F.,.F.,(4,3,3,3,3,3,3,3,3,3,
3,3,3,3,3,3,3,3,3,3,3,3,3,3,3,3,3,3,3,3,3,3,3,3,3,3,3,3,3,3,3,3,3,3,3,3,
3,3,3,3,3,3,3,3,4),(28.2743338823871,28.3727453836561,28.4733999042417,
28.5732533303423,28.6493194915406,28.7252909943352,28.8011846159107,28.8770170539935,
28.9528049453892,29.0300537911739,29.1058175916703,29.1815894995911,29.2573845189297,
29.3357373171141,29.4116658576972,29.4912307846822,29.5707957116672,29.6493403274105,
29.7277923683753,29.8061663277422,29.8844766433592,29.9627377075046,30.0409669995409,
30.1191797950537,30.1973890799497,30.2756078356583,30.3538815135514,30.4321837341024,
30.5105691894803,30.5683380929921,30.647987113442,30.7275660052906,30.8070856481688,
30.8865485598348,30.9659774108142,31.0453818104423,31.0671092836545,31.1483413374153,
31.2296220564447,31.3136866609127,31.3951187964939,31.4804996354054,31.565880474317,
31.6511133966384,31.7362683567024,31.8212732922646,31.9061715832064,31.9908781284146,
32.0646516649794,32.1412084177776,32.2177589008488,32.2943456149223,32.3709501090727,
32.4476276168002,32.5105299619478),.UNSPECIFIED.);
#3226=B_SPLINE_CURVE_WITH_KNOTS('',3,(#34746,#34747,#34748,#34749,#34750,
#34751,#34752,#34753,#34754,#34755,#34756,#34757,#34758,#34759,#34760,#34761,
#34762,#34763,#34764,#34765,#34766,#34767,#34768,#34769,#34770,#34771,#34772,
#34773,#34774,#34775,#34776,#34777,#34778,#34779,#34780,#34781,#34782,#34783,
#34784,#34785,#34786,#34787,#34788,#34789,#34790,#34791,#34792,#34793,#34794,
#34795,#34796,#34797,#34798,#34799,#34800,#34801,#34802,#34803,#34804,#34805,
#34806,#34807,#34808,#34809,#34810,#34811,#34812,#34813,#34814,#34815,#34816,
#34817,#34818,#34819,#34820,#34821,#34822,#34823,#34824,#34825,#34826,#34827,
#34828,#34829,#34830,#34831,#34832,#34833,#34834,#34835,#34836,#34837,#34838,
#34839,#34840,#34841,#34842,#34843,#34844,#34845,#34846,#34847,#34848,#34849,
#34850,#34851,#34852,#34853,#34854,#34855,#34856,#34857,#34858,#34859,#34860,
#34861,#34862,#34863,#34864,#34865,#34866,#34867,#34868,#34869,#34870,#34871,
#34872,#34873,#34874,#34875,#34876,#34877,#34878,#34879,#34880,#34881,#34882,
#34883,#34884,#34885,#34886,#34887,#34888,#34889,#34890,#34891,#34892,#34893,
#34894,#34895,#34896,#34897,#34898,#34899,#34900,#34901,#34902,#34903,#34904,
#34905,#34906,#34907,#34908,#34909,#34910,#34911,#34912,#34913,#34914),
 .UNSPECIFIED.,.F.,.F.,(4,3,3,3,3,3,3,3,3,3,3,3,3,3,3,3,3,3,3,3,3,3,3,3,
3,3,3,3,3,3,3,3,3,3,3,3,3,3,3,3,3,3,3,3,3,3,3,3,3,3,3,3,3,3,3,3,4),(34.5575191896132,
34.6328860307859,34.7082479790274,34.7360023597366,34.8172344128309,34.8985151311743,
34.9825797359805,35.0640118708417,35.1493927106204,35.2347735503991,35.3200064738651,
35.4051614350876,35.4901663718067,35.5750646638952,35.6597712102173,35.7335447410615,
35.8101037057496,35.8866572726299,35.9632200382092,36.0398385706779,36.1164883391738,
36.1932214526645,36.232315931724,36.3118677962225,36.3913595316738,36.4708033903896,
36.5502115872951,36.6295963088339,36.7089823448189,36.7883711261052,36.8677737247216,
36.9472012203527,37.0266999434922,37.1062370888878,37.1858626223519,37.2298583130489,
37.3075257932727,37.3851072483418,37.4626165992783,37.5400574704023,37.6174586657012,
37.6948339776677,37.7286295037113,37.8121209493714,37.8957685941178,37.979653816982,
38.0636525953846,38.1478368512936,38.2274006943737,38.3049039354871,38.3823292364177,
38.4596907462697,38.5370025744167,38.6142794004192,38.6915361823884,38.7687949577837,
38.7940869402089),.UNSPECIFIED.);
#3227=B_SPLINE_CURVE_WITH_KNOTS('',3,(#34915,#34916,#34917,#34918,#34919,
#34920,#34921,#34922,#34923,#34924,#34925,#34926,#34927,#34928,#34929,#34930,
#34931,#34932,#34933,#34934,#34935,#34936,#34937,#34938,#34939,#34940,#34941,
#34942,#34943,#34944,#34945,#34946,#34947,#34948,#34949,#34950,#34951,#34952,
#34953,#34954,#34955,#34956,#34957,#34958,#34959,#34960,#34961,#34962,#34963,
#34964,#34965,#34966,#34967,#34968,#34969,#34970,#34971,#34972,#34973,#34974,
#34975,#34976,#34977,#34978,#34979,#34980,#34981,#34982,#34983,#34984,#34985,
#34986,#34987,#34988,#34989,#34990,#34991,#34992,#34993,#34994,#34995,#34996),
 .UNSPECIFIED.,.F.,.F.,(4,3,3,3,3,3,3,3,3,3,3,3,3,3,3,3,3,3,3,3,3,3,3,3,
3,3,3,4),(32.5118535701146,32.5876594146424,32.6634298563173,32.739195017798,
32.8149612557743,32.890743570437,32.9665569730653,33.0424617773558,33.1184172654376,
33.1944901160972,33.2396887877493,33.3182334046871,33.3966854468569,33.4750594074386,
33.5533697242772,33.6316307896502,33.7098600829166,33.7880728796606,33.8662821657869,
33.944500922725,34.0227746018369,34.1010768236021,34.1794622801768,34.2372311690742,
34.3214988374453,34.4056595487601,34.48964296411,34.5575191894885),
 .UNSPECIFIED.);
#3228=B_SPLINE_CURVE_WITH_KNOTS('',3,(#34998,#34999,#35000,#35001,#35002,
#35003,#35004,#35005,#35006,#35007,#35008,#35009,#35010,#35011,#35012,#35013,
#35014,#35015,#35016,#35017,#35018,#35019,#35020,#35021,#35022,#35023,#35024,
#35025,#35026,#35027,#35028,#35029,#35030,#35031,#35032,#35033,#35034,#35035,
#35036,#35037,#35038,#35039,#35040,#35041,#35042,#35043,#35044,#35045,#35046,
#35047,#35048,#35049,#35050,#35051,#35052,#35053,#35054,#35055,#35056,#35057,
#35058,#35059,#35060,#35061,#35062,#35063,#35064,#35065,#35066,#35067,#35068,
#35069,#35070,#35071,#35072,#35073,#35074,#35075,#35076,#35077,#35078,#35079),
 .UNSPECIFIED.,.F.,.F.,(4,3,3,3,3,3,3,3,3,3,3,3,3,3,3,3,3,3,3,3,3,3,3,3,
3,3,3,4),(32.5105299619478,32.5634228556418,32.6429747200431,32.7224664553949,
32.8019103140094,32.8813185108116,32.9607032322457,33.0400892681246,33.1194780493041,
33.198880647813,33.2783081433365,33.3578068663682,33.4373440116561,33.5169695450135,
33.5609652369667,33.6386327172285,33.7162141723355,33.7937235233092,33.87116439447,
33.9485655898052,34.0259409018075,34.0597364276292,34.1431858165314,34.2267901676328,
34.3106306453124,34.3945842540227,34.478722903774,34.5575191894884),
 .UNSPECIFIED.);
#3229=B_SPLINE_CURVE_WITH_KNOTS('',3,(#35080,#35081,#35082,#35083,#35084,
#35085,#35086,#35087,#35088,#35089,#35090,#35091,#35092,#35093,#35094,#35095,
#35096,#35097,#35098,#35099,#35100,#35101,#35102,#35103,#35104,#35105,#35106,
#35107,#35108,#35109,#35110,#35111,#35112,#35113,#35114,#35115,#35116,#35117,
#35118,#35119,#35120,#35121,#35122,#35123,#35124,#35125,#35126,#35127,#35128,
#35129,#35130,#35131,#35132,#35133,#35134,#35135,#35136,#35137,#35138,#35139,
#35140,#35141,#35142,#35143,#35144,#35145,#35146,#35147,#35148,#35149,#35150,
#35151,#35152,#35153,#35154,#35155,#35156,#35157,#35158,#35159,#35160,#35161,
#35162,#35163,#35164,#35165,#35166,#35167,#35168,#35169,#35170,#35171,#35172,
#35173,#35174,#35175,#35176,#35177,#35178,#35179,#35180,#35181,#35182,#35183,
#35184,#35185,#35186,#35187,#35188,#35189,#35190,#35191,#35192,#35193,#35194,
#35195,#35196,#35197,#35198,#35199,#35200,#35201,#35202,#35203,#35204,#35205,
#35206,#35207,#35208,#35209,#35210,#35211,#35212,#35213,#35214,#35215,#35216,
#35217,#35218,#35219,#35220,#35221,#35222,#35223,#35224,#35225,#35226,#35227,
#35228,#35229,#35230,#35231,#35232,#35233,#35234,#35235,#35236,#35237,#35238,
#35239,#35240,#35241,#35242,#35243,#35244,#35245,#35246,#35247,#35248),
 .UNSPECIFIED.,.F.,.F.,(4,3,3,3,3,3,3,3,3,3,3,3,3,3,3,3,3,3,3,3,3,3,3,3,
3,3,3,3,3,3,3,3,3,3,3,3,3,3,3,3,3,3,3,3,3,3,3,3,3,3,3,3,3,3,3,3,4),(34.5575191895771,
34.5585076182916,34.6360167511266,34.7134440267969,34.7908050620128,34.8681154260008,
34.9453906511771,35.0226591552877,35.0999268898953,35.1772078912449,35.2545162004082,
35.3319123124872,35.4093540738392,35.4869152615718,35.5560499996165,35.6321161590785,
35.7080876601177,35.7839812799196,35.859813716212,35.9356016058013,36.0128504526938,
36.0886142513502,36.1643861574193,36.2401811748956,36.318533976407,36.394462515114,
36.4740274480277,36.5535923809414,36.6321369978792,36.7105890400494,36.7889630006304,
36.8672733174692,36.9455343828414,37.0237636761078,37.1019764728517,37.1801857589785,
37.2584045159164,37.3366781950282,37.4149804167936,37.4933658733684,37.5511347622663,
37.6307837825282,37.7103626741949,37.7898823168981,37.8693452283991,37.9487740792201,
38.0281784786989,38.0499059529288,38.1311380060231,38.2124187243663,38.2964833291725,
38.3779154640338,38.4632963038125,38.5486771435912,38.6339107049348,38.7190353182339,
38.7947691242316),.UNSPECIFIED.);
#3230=B_SPLINE_CURVE_WITH_KNOTS('',3,(#35254,#35255,#35256,#35257,#35258,
#35259,#35260,#35261,#35262,#35263,#35264,#35265,#35266,#35267,#35268,#35269,
#35270,#35271,#35272,#35273,#35274,#35275,#35276,#35277,#35278,#35279,#35280,
#35281,#35282,#35283,#35284,#35285,#35286,#35287,#35288,#35289,#35290,#35291,
#35292,#35293,#35294,#35295,#35296,#35297,#35298,#35299,#35300,#35301,#35302,
#35303,#35304,#35305,#35306,#35307,#35308,#35309,#35310,#35311,#35312,#35313,
#35314,#35315,#35316,#35317,#35318,#35319,#35320,#35321,#35322,#35323,#35324,
#35325,#35326,#35327,#35328,#35329,#35330,#35331,#35332,#35333,#35334,#35335,
#35336,#35337,#35338,#35339,#35340,#35341,#35342,#35343,#35344,#35345,#35346,
#35347,#35348,#35349,#35350,#35351,#35352,#35353,#35354,#35355,#35356,#35357,
#35358,#35359,#35360,#35361,#35362,#35363,#35364,#35365,#35366,#35367,#35368,
#35369,#35370,#35371,#35372,#35373,#35374,#35375,#35376,#35377,#35378,#35379,
#35380,#35381,#35382,#35383,#35384,#35385,#35386,#35387,#35388,#35389,#35390,
#35391,#35392,#35393,#35394,#35395,#35396,#35397,#35398,#35399,#35400,#35401,
#35402,#35403,#35404,#35405,#35406,#35407,#35408,#35409,#35410,#35411,#35412,
#35413,#35414,#35415,#35416,#35417,#35418,#35419,#35420,#35421,#35422),
 .UNSPECIFIED.,.F.,.F.,(4,3,3,3,3,3,3,3,3,3,3,3,3,3,3,3,3,3,3,3,3,3,3,3,
3,3,3,3,3,3,3,3,3,3,3,3,3,3,3,3,3,3,3,3,3,3,3,3,3,3,3,3,3,3,3,3,4),(40.8407044967615,
40.9255123901943,41.0106105815536,41.0958516116635,41.1812825465948,41.2200278383484,
41.2996768586144,41.3792557502852,41.4587753929926,41.5382383044977,41.6176671553226,
41.6970715548056,41.7187990290109,41.8000310821006,41.8813118004394,41.9653764052479,
42.0468085401041,42.1321893798887,42.2175702196733,42.3028031431432,42.3879581043698,
42.4729630410927,42.5578613331851,42.642567879511,42.7163414103358,42.7929003750229,
42.8694539419022,42.9460167074805,43.0226352399482,43.0992850084429,43.1760181219326,
43.2151126009982,43.2946644654967,43.3741562009481,43.453600059664,43.5330082565694,
43.6123929781081,43.6917790140932,43.7711677953796,43.8505703939962,43.9299978896276,
44.0094966127673,44.089033758163,44.1686592916273,44.2126549823231,44.290322462547,
44.3679039176165,44.4454132685533,44.5228541396774,44.6002553349763,44.677630646943,
44.7114261729855,44.794877737273,44.8785677116355,44.9623812548976,45.0463706197337,
45.0770119293198),.UNSPECIFIED.);
#3231=B_SPLINE_CURVE_WITH_KNOTS('',3,(#35423,#35424,#35425,#35426,#35427,
#35428,#35429,#35430,#35431,#35432,#35433,#35434,#35435,#35436,#35437,#35438,
#35439,#35440,#35441,#35442,#35443,#35444,#35445,#35446,#35447,#35448,#35449,
#35450,#35451,#35452,#35453,#35454,#35455,#35456,#35457,#35458,#35459,#35460,
#35461,#35462,#35463,#35464,#35465,#35466,#35467,#35468,#35469,#35470,#35471,
#35472,#35473,#35474,#35475,#35476,#35477,#35478,#35479,#35480,#35481,#35482,
#35483,#35484,#35485,#35486,#35487,#35488,#35489,#35490,#35491,#35492,#35493,
#35494,#35495,#35496,#35497,#35498,#35499,#35500,#35501,#35502,#35503,#35504),
 .UNSPECIFIED.,.F.,.F.,(4,3,3,3,3,3,3,3,3,3,3,3,3,3,3,3,3,3,3,3,3,3,3,3,
3,3,3,4),(38.7940869402089,38.8713753251789,38.9486956114322,39.0261052493249,
39.1035646699761,39.181136360427,39.2249430756986,39.3010092351557,39.37698073619,
39.452874355987,39.5287067922744,39.6044946818586,39.6817435287542,39.7575073274052,
39.8332792334691,39.9090742509398,39.9874270524607,40.0633555911627,40.1429205240931,
40.2224854570235,40.3030798010984,40.3835697204861,40.4639643347003,40.5442727002749,
40.6244792960957,40.7046249184425,40.7847034810469,40.8407044966681),
 .UNSPECIFIED.);
#3232=B_SPLINE_CURVE_WITH_KNOTS('',3,(#35506,#35507,#35508,#35509,#35510,
#35511,#35512,#35513,#35514,#35515,#35516,#35517,#35518,#35519,#35520,#35521,
#35522,#35523,#35524,#35525,#35526,#35527,#35528,#35529,#35530,#35531,#35532,
#35533,#35534,#35535,#35536,#35537,#35538,#35539,#35540,#35541,#35542,#35543,
#35544,#35545,#35546,#35547,#35548,#35549,#35550,#35551,#35552,#35553,#35554,
#35555,#35556,#35557,#35558,#35559,#35560,#35561,#35562,#35563,#35564,#35565,
#35566,#35567,#35568,#35569,#35570,#35571,#35572,#35573,#35574,#35575,#35576,
#35577,#35578,#35579,#35580,#35581,#35582,#35583,#35584,#35585,#35586,#35587),
 .UNSPECIFIED.,.F.,.F.,(4,3,3,3,3,3,3,3,3,3,3,3,3,3,3,3,3,3,3,3,3,3,3,3,
3,3,3,4),(38.7947691242316,38.8796796646918,38.9643964891114,39.0474483342537,
39.1240072989418,39.2005608658222,39.2771236314016,39.3537421638703,39.4303919323663,
39.5071250458572,39.5462195249161,39.6257713894145,39.7052631248656,39.7847069835815,
39.8641151804875,39.9434999020257,40.0228859380105,40.1022747192966,40.1816773179129,
40.2611048135436,40.340603536683,40.4201406820783,40.4997662155423,40.543761906241,
40.6281287683698,40.7123180186424,40.7962321950299,40.840704496668),
 .UNSPECIFIED.);
#3233=B_SPLINE_CURVE_WITH_KNOTS('',3,(#35588,#35589,#35590,#35591,#35592,
#35593,#35594,#35595,#35596,#35597,#35598,#35599,#35600,#35601,#35602,#35603,
#35604,#35605,#35606,#35607,#35608,#35609,#35610,#35611,#35612,#35613,#35614,
#35615,#35616,#35617,#35618,#35619,#35620,#35621,#35622,#35623,#35624,#35625,
#35626,#35627,#35628,#35629,#35630,#35631,#35632,#35633,#35634,#35635,#35636,
#35637,#35638,#35639,#35640,#35641,#35642,#35643,#35644,#35645,#35646,#35647,
#35648,#35649,#35650,#35651,#35652,#35653,#35654,#35655,#35656,#35657,#35658,
#35659,#35660,#35661,#35662,#35663,#35664,#35665,#35666,#35667,#35668,#35669,
#35670,#35671,#35672,#35673,#35674,#35675,#35676,#35677,#35678,#35679,#35680,
#35681,#35682,#35683,#35684,#35685,#35686,#35687,#35688,#35689,#35690,#35691,
#35692,#35693,#35694,#35695,#35696,#35697,#35698,#35699,#35700,#35701,#35702,
#35703,#35704,#35705,#35706,#35707,#35708,#35709,#35710,#35711,#35712,#35713,
#35714,#35715,#35716,#35717,#35718,#35719,#35720,#35721,#35722,#35723,#35724,
#35725,#35726,#35727,#35728,#35729,#35730,#35731,#35732,#35733,#35734,#35735,
#35736,#35737,#35738,#35739,#35740,#35741,#35742,#35743,#35744),
 .UNSPECIFIED.,.F.,.F.,(4,3,3,3,3,3,3,3,3,3,3,3,3,3,3,3,3,3,3,3,3,3,3,3,
3,3,3,3,3,3,3,3,3,3,3,3,3,3,3,3,3,3,3,3,3,3,3,3,3,3,3,3,4),(40.840704496668,
40.9231667027682,41.0056285605707,41.0880900769258,41.1705512586836,41.2530121126939,
41.335472645806,41.4179328648691,41.5003927767322,41.582852388244,41.6653117062528,
41.7477707376065,41.8302294891534,41.9126879677409,41.9951461802166,42.0776041334274,
42.1600618342204,42.2425192894422,42.3249765059394,42.4109892012254,42.4943139997837,
42.5767806053756,42.6592463667588,42.7417113113485,42.8241754665568,42.9066388597934,
42.9891015184651,43.0715634699762,43.1540247417286,43.2364853611217,43.3189453555528,
43.4014047524171,43.4838635791072,43.5663218630143,43.6487796315274,43.7312369120337,
43.8153710272248,43.8978370255847,43.980301402191,44.0627642666864,44.1452257286927,
44.227685897812,44.3101448836281,44.3926027957084,44.4782002906313,44.5606650276772,
44.6431268000635,44.7255860462286,44.8080432044673,44.8905057235499,44.9729633949608,
45.0554221861539,45.0773827550916),.UNSPECIFIED.);
#3234=B_SPLINE_CURVE_WITH_KNOTS('',3,(#35750,#35751,#35752,#35753,#35754,
#35755,#35756,#35757,#35758,#35759,#35760,#35761,#35762,#35763,#35764,#35765,
#35766,#35767,#35768,#35769,#35770,#35771,#35772,#35773,#35774,#35775,#35776,
#35777,#35778,#35779,#35780,#35781,#35782,#35783,#35784,#35785,#35786,#35787,
#35788,#35789,#35790,#35791,#35792,#35793,#35794,#35795,#35796,#35797,#35798,
#35799,#35800,#35801,#35802,#35803,#35804,#35805,#35806,#35807,#35808,#35809,
#35810,#35811,#35812,#35813,#35814,#35815,#35816,#35817,#35818,#35819,#35820,
#35821,#35822,#35823,#35824,#35825,#35826,#35827,#35828,#35829,#35830,#35831,
#35832,#35833,#35834,#35835,#35836,#35837,#35838,#35839,#35840,#35841,#35842,
#35843,#35844,#35845,#35846,#35847,#35848,#35849,#35850,#35851,#35852,#35853,
#35854,#35855,#35856,#35857,#35858,#35859,#35860,#35861,#35862,#35863,#35864,
#35865,#35866,#35867,#35868,#35869,#35870,#35871,#35872,#35873,#35874,#35875,
#35876,#35877,#35878,#35879,#35880,#35881,#35882,#35883,#35884,#35885,#35886,
#35887,#35888,#35889,#35890,#35891,#35892,#35893,#35894,#35895,#35896,#35897,
#35898,#35899,#35900,#35901,#35902,#35903,#35904,#35905,#35906,#35907,#35908,
#35909,#35910,#35911,#35912,#35913,#35914,#35915,#35916,#35917,#35918),
 .UNSPECIFIED.,.F.,.F.,(4,3,3,3,3,3,3,3,3,3,3,3,3,3,3,3,3,3,3,3,3,3,3,3,
3,3,3,3,3,3,3,3,3,3,3,3,3,3,3,3,3,3,3,3,3,3,3,3,3,3,3,3,3,3,3,3,4),(47.1238898038477,
47.2052821262978,47.2838267432363,47.362278785407,47.4406527459888,47.5189630628279,
47.5972241282008,47.6754534214679,47.7536662182125,47.83187550434,47.9100942612782,
47.9883679403908,48.0666701621569,48.1450556187325,48.2028245076227,48.2824735278888,
48.3620524195598,48.4415720622669,48.5210349737721,48.6004638245972,48.6798682240802,
48.7015956982851,48.7828277513748,48.8641084697135,48.948173074522,49.0296052093781,
49.1149860491628,49.2003668889476,49.2855998124176,49.3707547736442,49.4557597103671,
49.5406580024596,49.6253645487856,49.69913807961,49.7756970442971,49.8522506111764,
49.9288133767549,50.0054319092225,50.0820816777174,50.158814791207,50.1979092702725,
50.2774611347711,50.3569528702224,50.4363967289383,50.5158049258438,50.5951896473825,
50.6745756833676,50.7539644646541,50.8333670632707,50.9127945589021,50.9922932820418,
51.0718304274376,51.1514559609018,51.1954516515974,51.2731390205547,51.3507270166998,
51.361293208361),.UNSPECIFIED.);
#3235=B_SPLINE_CURVE_WITH_KNOTS('',3,(#35919,#35920,#35921,#35922,#35923,
#35924,#35925,#35926,#35927,#35928,#35929,#35930,#35931,#35932,#35933,#35934,
#35935,#35936,#35937,#35938,#35939,#35940,#35941,#35942,#35943,#35944,#35945,
#35946,#35947,#35948,#35949,#35950,#35951,#35952,#35953,#35954,#35955,#35956,
#35957,#35958,#35959,#35960,#35961,#35962,#35963,#35964,#35965,#35966,#35967,
#35968,#35969,#35970,#35971,#35972,#35973,#35974,#35975,#35976,#35977,#35978,
#35979,#35980,#35981,#35982,#35983,#35984,#35985,#35986,#35987,#35988,#35989,
#35990,#35991,#35992,#35993,#35994,#35995,#35996,#35997,#35998,#35999,#36000,
#36001,#36002,#36003),.UNSPECIFIED.,.F.,.F.,(4,3,3,3,3,3,3,3,3,3,3,3,3,
3,3,3,3,3,3,3,3,3,3,3,3,3,3,3,4),(45.0770119293198,45.1612179706454,45.210197363648,
45.2877064964886,45.3651337721647,45.4424948073866,45.5198051713802,45.5970803965626,
45.6743489006794,45.7516166352935,45.8288976366497,45.9062059458194,45.983602057905,
46.0610438192636,46.1386050070028,46.2077397449729,46.2830265149734,46.3582198260812,
46.4333368553301,46.5083946723668,46.5853315637925,46.6603308845112,46.7353258134164,
46.810331656291,46.8887211931614,46.9638331599026,47.0389929820916,47.1142482591672,
47.1238898037727),.UNSPECIFIED.);
#3236=B_SPLINE_CURVE_WITH_KNOTS('',3,(#36005,#36006,#36007,#36008,#36009,
#36010,#36011,#36012,#36013,#36014,#36015,#36016,#36017,#36018,#36019,#36020,
#36021,#36022,#36023,#36024,#36025,#36026,#36027,#36028,#36029,#36030,#36031,
#36032,#36033,#36034,#36035,#36036,#36037,#36038,#36039,#36040,#36041,#36042,
#36043,#36044,#36045,#36046,#36047,#36048,#36049,#36050,#36051,#36052,#36053,
#36054,#36055,#36056,#36057,#36058,#36059,#36060,#36061,#36062,#36063,#36064,
#36065,#36066,#36067,#36068,#36069,#36070,#36071,#36072,#36073,#36074,#36075,
#36076,#36077,#36078,#36079,#36080),.UNSPECIFIED.,.F.,.F.,(4,3,3,3,3,3,
3,3,3,3,3,3,3,3,3,3,3,3,3,3,3,3,3,3,3,4),(45.0773827550916,45.1598443588218,
45.2423052966737,45.3247655960457,45.4072252843339,45.4896843889323,45.5721429372327,
45.6546009566253,45.737058474498,45.8237354325824,45.9062022181234,45.9886673311914,
46.0711308814393,46.1535929784986,46.2360537319802,46.3185132514762,46.4009716465613,
46.4834290267949,46.565895412481,46.6483586139892,46.7308190698388,46.8132772183935,
46.8957428221471,46.978202700535,47.0606668117873,47.1238898038476),
 .UNSPECIFIED.);
#3237=B_SPLINE_CURVE_WITH_KNOTS('',3,(#36081,#36082,#36083,#36084,#36085,
#36086,#36087,#36088,#36089,#36090,#36091,#36092,#36093,#36094,#36095,#36096,
#36097,#36098,#36099,#36100,#36101,#36102,#36103,#36104,#36105,#36106,#36107,
#36108,#36109,#36110,#36111,#36112,#36113,#36114,#36115,#36116,#36117,#36118,
#36119,#36120,#36121,#36122,#36123,#36124,#36125,#36126,#36127,#36128,#36129,
#36130,#36131,#36132,#36133,#36134,#36135,#36136,#36137,#36138,#36139,#36140,
#36141,#36142,#36143,#36144,#36145,#36146,#36147,#36148,#36149,#36150,#36151,
#36152,#36153,#36154,#36155,#36156,#36157,#36158,#36159,#36160,#36161,#36162,
#36163,#36164,#36165,#36166,#36167,#36168,#36169,#36170,#36171,#36172,#36173,
#36174,#36175,#36176,#36177,#36178,#36179,#36180,#36181,#36182,#36183,#36184,
#36185,#36186,#36187,#36188,#36189,#36190,#36191,#36192,#36193,#36194,#36195,
#36196,#36197,#36198,#36199,#36200,#36201,#36202,#36203,#36204,#36205,#36206,
#36207,#36208,#36209,#36210,#36211,#36212,#36213,#36214,#36215,#36216,#36217,
#36218,#36219,#36220,#36221,#36222,#36223,#36224,#36225,#36226,#36227,#36228,
#36229,#36230,#36231,#36232,#36233,#36234,#36235,#36236,#36237,#36238,#36239,
#36240,#36241,#36242,#36243,#36244,#36245,#36246),.UNSPECIFIED.,.F.,.F.,
(4,3,3,3,3,3,3,3,3,3,3,3,3,3,3,3,3,3,3,3,3,3,3,3,3,3,3,3,3,3,3,3,3,3,3,
3,3,3,3,3,3,3,3,3,3,3,3,3,3,3,3,3,3,3,3,4),(47.1238898038476,47.2119796337542,
47.3005695584914,47.3893824075732,47.4784338092133,47.5265585755152,47.6042260557391,
47.6818075108085,47.7593168617452,47.8367577328693,47.9141589281681,47.9915342401346,
48.0253297661777,48.1088212118376,48.1924688565826,48.2763540794465,48.360352857849,
48.4445371137578,48.5241009568401,48.6016100896807,48.6790373653567,48.7563984005786,
48.8337087645722,48.9109839897546,48.9882524938714,49.0655202284855,49.1428012298417,
49.2201095390114,49.297505651097,49.3749474124556,49.4525086001948,49.521643338165,
49.5977094976221,49.6736809986562,49.7495746184532,49.8254070547404,49.9011949443246,
49.9784437912203,50.0542075898714,50.1299794959355,50.2057745134066,50.2841273149274,
50.3600558536292,50.4396207865596,50.5191857194899,50.5977395480502,50.6761992297749,
50.7545792646299,50.8328816291235,50.9111392843912,50.9893652504517,51.0675725263625,
51.1457915170971,51.2240148888098,51.3022833526319,51.3603137507763),
 .UNSPECIFIED.);
#3238=B_SPLINE_CURVE_WITH_KNOTS('',3,(#36252,#36253,#36254,#36255,#36256,
#36257,#36258,#36259,#36260,#36261,#36262,#36263,#36264,#36265,#36266,#36267,
#36268,#36269,#36270,#36271,#36272,#36273,#36274,#36275,#36276,#36277,#36278,
#36279,#36280,#36281,#36282,#36283,#36284,#36285,#36286,#36287,#36288,#36289,
#36290,#36291,#36292,#36293,#36294,#36295,#36296,#36297,#36298,#36299,#36300,
#36301,#36302,#36303,#36304,#36305,#36306,#36307,#36308,#36309,#36310,#36311,
#36312,#36313,#36314,#36315,#36316,#36317,#36318,#36319,#36320,#36321,#36322,
#36323,#36324,#36325,#36326,#36327,#36328,#36329,#36330,#36331,#36332,#36333,
#36334,#36335,#36336,#36337,#36338,#36339,#36340,#36341,#36342,#36343,#36344,
#36345,#36346,#36347,#36348,#36349,#36350,#36351,#36352,#36353,#36354,#36355,
#36356,#36357,#36358,#36359,#36360,#36361,#36362,#36363,#36364,#36365,#36366,
#36367,#36368,#36369,#36370,#36371,#36372,#36373,#36374,#36375,#36376,#36377,
#36378,#36379,#36380,#36381,#36382,#36383,#36384,#36385,#36386,#36387,#36388,
#36389,#36390,#36391,#36392,#36393,#36394,#36395,#36396,#36397,#36398,#36399,
#36400,#36401,#36402,#36403,#36404,#36405,#36406,#36407,#36408,#36409,#36410,
#36411,#36412,#36413,#36414,#36415,#36416,#36417,#36418,#36419,#36420),
 .UNSPECIFIED.,.F.,.F.,(4,3,3,3,3,3,3,3,3,3,3,3,3,3,3,3,3,3,3,3,3,3,3,3,
3,3,3,3,3,3,3,3,3,3,3,3,3,3,3,3,3,3,3,3,3,3,3,3,3,3,3,3,3,3,3,3,4),(53.4070751111297,
53.4818397072623,53.5565472546284,53.6312148585454,53.7058712697682,53.7805253462596,
53.8551924996201,53.929888159705,54.0046702141495,54.0795014793999,54.154443083463,
54.188078795572,54.2666234125106,54.3450754546814,54.4234494152635,54.5017597321029,
54.5800207974759,54.658250090743,54.7364628874877,54.8146721736151,54.8928909305534,
54.971164609666,55.0494668314322,55.1278522880078,55.1856211768969,55.2652701971631,
55.3448490888341,55.4243687315413,55.5038316430465,55.5832604938716,55.6626648933549,
55.6843923675594,55.7656244206493,55.8469051389876,55.9309697437962,56.0124018786526,
56.0977827184372,56.1831635582218,56.2683964816917,56.3535514429179,56.4385563796407,
56.523454671733,56.6081612180588,56.6819347488843,56.7584937135713,56.8350472804504,
56.9116100460281,56.9882285784958,57.0648783469907,57.1416114604804,57.1807059395467,
57.2602600160998,57.3397553727982,57.4191965518241,57.4986043528576,57.5779943149647,
57.6435975513154),.UNSPECIFIED.);
#3239=B_SPLINE_CURVE_WITH_KNOTS('',3,(#36421,#36422,#36423,#36424,#36425,
#36426,#36427,#36428,#36429,#36430,#36431,#36432,#36433,#36434,#36435,#36436,
#36437,#36438,#36439,#36440,#36441,#36442,#36443,#36444,#36445,#36446,#36447,
#36448,#36449,#36450,#36451,#36452,#36453,#36454,#36455,#36456,#36457,#36458,
#36459,#36460,#36461,#36462,#36463,#36464,#36465,#36466,#36467,#36468,#36469,
#36470,#36471,#36472,#36473,#36474,#36475,#36476,#36477,#36478,#36479,#36480,
#36481,#36482,#36483,#36484,#36485,#36486,#36487,#36488,#36489,#36490,#36491,
#36492,#36493,#36494,#36495,#36496,#36497,#36498,#36499,#36500,#36501,#36502),
 .UNSPECIFIED.,.F.,.F.,(4,3,3,3,3,3,3,3,3,3,3,3,3,3,3,3,3,3,3,3,3,3,3,3,
3,3,3,4),(51.361293208361,51.4387937872539,51.5162285057782,51.5936252425489,
51.6709973963902,51.6942228422598,51.7777142879196,51.8613619326647,51.9452471555287,
52.029245933931,52.1134301898398,52.1929940329222,52.2705031657628,52.3479304414389,
52.4252914766608,52.5026018406546,52.579877065837,52.6571455699538,52.7344133045679,
52.8116943059241,52.8890026150938,52.9663987271794,53.043840488538,53.1214016762773,
53.1905364142471,53.2988057626372,53.4011481782412,53.4070751110273),
 .UNSPECIFIED.);
#3240=B_SPLINE_CURVE_WITH_KNOTS('',3,(#36504,#36505,#36506,#36507,#36508,
#36509,#36510,#36511,#36512,#36513,#36514,#36515,#36516,#36517,#36518,#36519,
#36520,#36521,#36522,#36523,#36524,#36525,#36526,#36527,#36528,#36529,#36530,
#36531,#36532,#36533,#36534,#36535,#36536,#36537,#36538,#36539,#36540,#36541,
#36542,#36543,#36544,#36545,#36546,#36547,#36548,#36549,#36550,#36551,#36552,
#36553,#36554,#36555,#36556,#36557,#36558,#36559,#36560,#36561,#36562,#36563,
#36564,#36565,#36566,#36567,#36568,#36569,#36570,#36571,#36572,#36573,#36574,
#36575,#36576,#36577,#36578,#36579,#36580,#36581,#36582,#36583,#36584,#36585),
 .UNSPECIFIED.,.F.,.F.,(4,3,3,3,3,3,3,3,3,3,3,3,3,3,3,3,3,3,3,3,3,3,3,3,
3,3,3,4),(51.3603137507763,51.4386948092913,51.5167281008148,51.5963771210809,
51.6759560127519,51.7554756554591,51.8349385669643,51.914367417789,51.9937718172721,
52.0154992914772,52.0967313445668,52.1780120629056,52.2620766677142,52.3435088025703,
52.428889642355,52.5142704821397,52.5995034056097,52.6846583668364,52.7696633035593,
52.8545615956517,52.9392681419776,53.0130416728021,53.0874804553072,53.1619075737966,
53.2363594869538,53.3108262427439,53.3853476244306,53.4064882895547),
 .UNSPECIFIED.);
#3241=B_SPLINE_CURVE_WITH_KNOTS('',3,(#36586,#36587,#36588,#36589,#36590,
#36591,#36592,#36593,#36594,#36595,#36596,#36597,#36598,#36599,#36600,#36601,
#36602,#36603,#36604,#36605,#36606,#36607,#36608,#36609,#36610,#36611,#36612,
#36613,#36614,#36615,#36616,#36617,#36618,#36619,#36620,#36621,#36622,#36623,
#36624,#36625,#36626,#36627,#36628,#36629,#36630,#36631,#36632,#36633,#36634,
#36635,#36636,#36637,#36638,#36639,#36640,#36641,#36642,#36643,#36644,#36645,
#36646,#36647,#36648,#36649,#36650,#36651,#36652,#36653,#36654,#36655,#36656,
#36657,#36658,#36659,#36660,#36661,#36662,#36663,#36664,#36665,#36666,#36667,
#36668,#36669,#36670,#36671,#36672,#36673,#36674,#36675,#36676,#36677,#36678,
#36679,#36680,#36681,#36682,#36683,#36684,#36685,#36686,#36687,#36688,#36689,
#36690,#36691,#36692,#36693,#36694,#36695,#36696,#36697,#36698,#36699,#36700,
#36701,#36702,#36703,#36704,#36705,#36706,#36707,#36708,#36709,#36710,#36711,
#36712,#36713,#36714,#36715,#36716,#36717,#36718,#36719,#36720,#36721,#36722,
#36723,#36724,#36725,#36726,#36727,#36728,#36729,#36730,#36731,#36732,#36733,
#36734,#36735,#36736,#36737,#36738,#36739,#36740,#36741,#36742),
 .UNSPECIFIED.,.F.,.F.,(4,3,3,3,3,3,3,3,3,3,3,3,3,3,3,3,3,3,3,3,3,3,3,3,
3,3,3,3,3,3,3,3,3,3,3,3,3,3,3,3,3,3,3,3,3,3,3,3,3,3,3,3,4),(53.4070751110272,
53.4895373171274,53.5719991749299,53.6544606912851,53.7369218730428,53.819382727053,
53.9018432601651,53.9843034792282,54.0667633910913,54.1492230026029,54.2316823206116,
54.3141413519655,54.3966001035122,54.4790585820998,54.5615167945754,54.6439747477863,
54.7264324485793,54.8088899038012,54.8913471202984,54.9773598155844,55.0606846141428,
55.1431512197346,55.2256169811179,55.3080819257075,55.3905460809158,55.4730094741524,
55.5554721328241,55.6379340843352,55.7203953560876,55.8028559754807,55.8853159699119,
55.9677753667761,56.0502341934662,56.1326924773733,56.2151502458864,56.2976075263927,
56.3817416415839,56.4642076399438,56.54667201655,56.6291348810454,56.7115963430517,
56.794056512171,56.8765154979871,56.9589734100674,57.0445709049904,57.1270356420362,
57.2094974144226,57.2919566605877,57.3744138188264,57.456876337909,57.5393340093198,
57.6217928005129,57.6437533694508),.UNSPECIFIED.);
#3242=B_SPLINE_CURVE_WITH_KNOTS('',3,(#36748,#36749,#36750,#36751,#36752,
#36753,#36754,#36755,#36756,#36757,#36758,#36759,#36760,#36761,#36762,#36763,
#36764,#36765,#36766,#36767,#36768,#36769,#36770,#36771,#36772,#36773,#36774,
#36775,#36776,#36777,#36778,#36779,#36780,#36781,#36782,#36783,#36784,#36785,
#36786,#36787,#36788,#36789,#36790,#36791,#36792,#36793,#36794,#36795,#36796,
#36797,#36798,#36799,#36800,#36801,#36802,#36803,#36804,#36805,#36806,#36807,
#36808,#36809,#36810,#36811,#36812,#36813,#36814,#36815,#36816,#36817,#36818,
#36819,#36820,#36821,#36822,#36823,#36824,#36825,#36826,#36827,#36828,#36829,
#36830,#36831,#36832,#36833,#36834,#36835,#36836,#36837,#36838,#36839,#36840,
#36841,#36842,#36843,#36844,#36845,#36846,#36847,#36848,#36849,#36850,#36851,
#36852,#36853,#36854,#36855,#36856,#36857,#36858,#36859,#36860,#36861,#36862,
#36863,#36864,#36865,#36866,#36867,#36868,#36869,#36870,#36871,#36872,#36873,
#36874,#36875,#36876,#36877,#36878,#36879,#36880,#36881,#36882,#36883,#36884,
#36885,#36886,#36887,#36888,#36889,#36890,#36891,#36892,#36893,#36894,#36895,
#36896,#36897,#36898,#36899,#36900,#36901,#36902,#36903,#36904,#36905,#36906,
#36907,#36908,#36909,#36910,#36911,#36912,#36913),.UNSPECIFIED.,.F.,.F.,
(4,3,3,3,3,3,3,3,3,3,3,3,3,3,3,3,3,3,3,3,3,3,3,3,3,3,3,3,3,3,3,3,3,3,3,
3,3,3,3,3,3,3,3,3,3,3,3,3,3,3,3,3,3,3,3,4),(59.6902604183505,59.773786672866,
59.857514913502,59.9415451416528,60.0257275351874,60.1101466313872,60.1733330835214,
60.2493992429785,60.3253707440126,60.4012643638095,60.4770968000968,60.5528846896809,
60.6301335365766,60.7058973352277,60.7816692412918,60.8574642587629,60.9358170602838,
61.0117455989856,61.0913105319159,61.1708754648463,61.2494200817848,61.3278721239556,
61.4062460845375,61.4845564013767,61.5628174667496,61.6410467600166,61.7192595567613,
61.7974688428887,61.8756875998268,61.9539612789394,62.0322635007056,62.1106489572812,
62.1684178461712,62.2480668664373,62.3276457581083,62.4071654008154,62.4866283123206,
62.5660571631454,62.6454615626284,62.6671890368336,62.7484210899233,62.829701808262,
62.9137664130706,62.9951985479267,63.0805793877114,63.1659602274961,63.2511931509661,
63.3363481121926,63.4213530489155,63.5062513410079,63.5909578873339,63.6647314181585,
63.7412915888735,63.8178421365915,63.8944126561589,63.9265539370322),
 .UNSPECIFIED.);
#3243=B_SPLINE_CURVE_WITH_KNOTS('',3,(#36914,#36915,#36916,#36917,#36918,
#36919,#36920,#36921,#36922,#36923,#36924,#36925,#36926,#36927,#36928,#36929,
#36930,#36931,#36932,#36933,#36934,#36935,#36936,#36937,#36938,#36939,#36940,
#36941,#36942,#36943,#36944,#36945,#36946,#36947,#36948,#36949,#36950,#36951,
#36952,#36953,#36954,#36955,#36956,#36957,#36958,#36959,#36960,#36961,#36962,
#36963,#36964,#36965,#36966,#36967,#36968,#36969,#36970,#36971,#36972,#36973,
#36974,#36975,#36976,#36977,#36978,#36979,#36980,#36981,#36982,#36983,#36984,
#36985,#36986,#36987,#36988,#36989,#36990,#36991,#36992,#36993,#36994,#36995),
 .UNSPECIFIED.,.F.,.F.,(4,3,3,3,3,3,3,3,3,3,3,3,3,3,3,3,3,3,3,3,3,3,3,3,
3,3,3,4),(57.6435975513154,57.7229850624315,57.8023844693303,57.8818068498589,
57.9612999462789,58.0408296972273,58.1204509651146,58.1782483208716,58.2559158010956,
58.3334972561652,58.4110066071021,58.4884474782263,58.5658486735253,58.6432239854919,
58.677019511534,58.7605109571932,58.8441586019384,58.9280438248024,59.0120426032054,
59.0962268591141,59.1757907021965,59.2548924531588,59.3338943814981,59.4128084842863,
59.4916257902556,59.5703864116441,59.6490922606897,59.6902604182069),
 .UNSPECIFIED.);
#3244=B_SPLINE_CURVE_WITH_KNOTS('',3,(#36997,#36998,#36999,#37000,#37001,
#37002,#37003,#37004,#37005,#37006,#37007,#37008,#37009,#37010,#37011,#37012,
#37013,#37014,#37015,#37016,#37017,#37018,#37019,#37020,#37021,#37022,#37023,
#37024,#37025,#37026,#37027,#37028,#37029,#37030,#37031,#37032,#37033,#37034,
#37035,#37036,#37037,#37038,#37039,#37040,#37041,#37042,#37043,#37044,#37045,
#37046,#37047,#37048,#37049,#37050,#37051,#37052,#37053,#37054,#37055,#37056,
#37057,#37058,#37059,#37060,#37061,#37062,#37063,#37064,#37065,#37066,#37067,
#37068,#37069,#37070,#37071,#37072),.UNSPECIFIED.,.F.,.F.,(4,3,3,3,3,3,
3,3,3,3,3,3,3,3,3,3,3,3,3,3,3,3,3,3,3,4),(57.6437533694508,57.7262149731809,
57.8086759110328,57.8911362104048,57.973595898693,58.0560550032914,58.1385135515919,
58.2209715709845,58.3034290888572,58.3901060469355,58.4725728324766,58.5550379455445,
58.6375014957924,58.7199635928517,58.8024243463332,58.8848838658292,58.9673422609144,
59.0497996411478,59.1322660268339,59.2147292283421,59.2971896841918,59.3796478327465,
59.4621134365,59.5445733148879,59.6270374261401,59.690260418109),
 .UNSPECIFIED.);
#3245=B_SPLINE_CURVE_WITH_KNOTS('',3,(#37073,#37074,#37075,#37076,#37077,
#37078,#37079,#37080,#37081,#37082,#37083,#37084,#37085,#37086,#37087,#37088,
#37089,#37090,#37091,#37092,#37093,#37094,#37095,#37096,#37097,#37098,#37099,
#37100,#37101,#37102,#37103,#37104,#37105,#37106,#37107,#37108,#37109,#37110,
#37111,#37112,#37113,#37114,#37115,#37116,#37117,#37118,#37119,#37120,#37121,
#37122,#37123,#37124,#37125,#37126,#37127,#37128,#37129,#37130,#37131,#37132,
#37133,#37134,#37135,#37136,#37137,#37138,#37139,#37140,#37141,#37142,#37143,
#37144,#37145,#37146,#37147,#37148,#37149,#37150,#37151,#37152,#37153,#37154,
#37155,#37156,#37157,#37158,#37159,#37160,#37161,#37162,#37163,#37164,#37165,
#37166,#37167,#37168,#37169,#37170,#37171,#37172,#37173,#37174,#37175,#37176,
#37177,#37178,#37179,#37180,#37181,#37182,#37183,#37184,#37185,#37186,#37187,
#37188,#37189,#37190,#37191,#37192,#37193,#37194,#37195,#37196,#37197,#37198,
#37199,#37200,#37201,#37202,#37203,#37204,#37205,#37206,#37207,#37208,#37209,
#37210,#37211,#37212,#37213,#37214,#37215,#37216,#37217,#37218,#37219,#37220,
#37221,#37222,#37223,#37224,#37225,#37226,#37227,#37228,#37229),
 .UNSPECIFIED.,.F.,.F.,(4,3,3,3,3,3,3,3,3,3,3,3,3,3,3,3,3,3,3,3,3,3,3,3,
3,3,3,3,3,3,3,3,3,3,3,3,3,3,3,3,3,3,3,3,3,3,3,3,3,3,3,3,4),(59.6902604182067,
59.7727226243069,59.8551844821094,59.9376459984645,60.0201071802223,60.1025680342325,
60.1850285673446,60.2674887864077,60.3499486982708,60.4324083097826,60.5148676277913,
60.5973266591451,60.679785410692,60.7622438892796,60.8447021017553,60.9271600549663,
61.0096177557593,61.0920752109812,61.1745324274788,61.2605451227648,61.3438699213231,
61.426336526915,61.5088022882982,61.5912672328878,61.6737313880962,61.7561947813327,
61.8386574400044,61.9211193915156,62.0035806632679,62.0860412826611,62.1685012770921,
62.2509606739563,62.3334195006465,62.4158777845535,62.4983355530665,62.5807928335728,
62.6649269487639,62.7473929471238,62.8298573237301,62.9123201882255,62.9947816502318,
63.077241819351,63.1597008051672,63.2421587172475,63.3277562121703,63.4102209492162,
63.4926827216026,63.5751419677676,63.6575991260063,63.7400616450889,63.8225193164998,
63.9049781076929,63.9269386766303),.UNSPECIFIED.);
#3246=B_SPLINE_CURVE_WITH_KNOTS('',3,(#37235,#37236,#37237,#37238,#37239,
#37240,#37241,#37242,#37243,#37244,#37245,#37246,#37247,#37248,#37249,#37250,
#37251,#37252,#37253,#37254,#37255,#37256,#37257,#37258,#37259,#37260,#37261,
#37262,#37263,#37264,#37265,#37266,#37267,#37268,#37269,#37270,#37271,#37272,
#37273,#37274,#37275,#37276,#37277,#37278,#37279,#37280,#37281,#37282,#37283,
#37284,#37285,#37286,#37287,#37288,#37289,#37290,#37291,#37292,#37293,#37294,
#37295,#37296,#37297,#37298,#37299,#37300,#37301,#37302,#37303,#37304,#37305,
#37306,#37307,#37308,#37309,#37310,#37311,#37312,#37313,#37314,#37315,#37316,
#37317,#37318,#37319,#37320,#37321,#37322,#37323,#37324,#37325,#37326,#37327,
#37328,#37329,#37330,#37331,#37332,#37333,#37334,#37335,#37336,#37337,#37338,
#37339,#37340,#37341,#37342,#37343,#37344,#37345,#37346,#37347,#37348,#37349,
#37350,#37351,#37352,#37353,#37354,#37355,#37356,#37357,#37358,#37359,#37360,
#37361,#37362,#37363,#37364,#37365,#37366,#37367,#37368,#37369,#37370,#37371,
#37372,#37373,#37374,#37375,#37376,#37377,#37378,#37379,#37380,#37381,#37382,
#37383,#37384,#37385,#37386,#37387,#37388,#37389,#37390,#37391,#37392,#37393,
#37394,#37395,#37396,#37397,#37398,#37399,#37400),.UNSPECIFIED.,.F.,.F.,
(4,3,3,3,3,3,3,3,3,3,3,3,3,3,3,3,3,3,3,3,3,3,3,3,3,3,3,3,3,3,3,3,3,3,3,
3,3,3,3,3,3,3,3,3,3,3,3,3,3,3,3,3,3,3,3,4),(65.9734457253864,66.0829124996505,
66.1585873714707,66.2360965043113,66.3135237799874,66.3908848152093,66.4681951792031,
66.5454704043854,66.6227389085023,66.7000066431164,66.7772876444726,66.8545959536425,
66.9319920657281,67.0094338270867,67.086995014826,67.1561297527956,67.2321959122527,
67.3081674132868,67.3840610330838,67.459893469371,67.5356813589552,67.6129302058509,
67.688694004502,67.7644659105661,67.8402609280372,67.918613729558,67.9945422682598,
68.0741072011901,68.1536721341205,68.232216751059,68.3106687932298,68.3890427538117,
68.4673530706508,68.5456141360238,68.6238434292908,68.7020562260355,68.7802655121629,
68.8584842691011,68.9367579482137,69.0150601699799,69.0934456265554,69.1512145154454,
69.2308635357115,69.3104424273825,69.3899620700895,69.4694249815946,69.5488538324195,
69.6282582319025,69.6499857061079,69.7312177591976,69.8124984775364,69.8965630823449,
69.9779952172011,70.0633760569857,70.1487568967703,70.2102685302427),
 .UNSPECIFIED.);
#3247=B_SPLINE_CURVE_WITH_KNOTS('',3,(#37401,#37402,#37403,#37404,#37405,
#37406,#37407,#37408,#37409,#37410,#37411,#37412,#37413,#37414,#37415,#37416,
#37417,#37418,#37419,#37420,#37421,#37422,#37423,#37424,#37425,#37426,#37427,
#37428,#37429,#37430,#37431,#37432,#37433,#37434,#37435,#37436,#37437,#37438,
#37439,#37440,#37441,#37442,#37443,#37444,#37445,#37446,#37447,#37448,#37449,
#37450,#37451,#37452,#37453,#37454,#37455,#37456,#37457,#37458,#37459,#37460,
#37461,#37462,#37463,#37464,#37465,#37466,#37467,#37468,#37469,#37470,#37471,
#37472,#37473,#37474,#37475,#37476,#37477,#37478,#37479,#37480,#37481,#37482),
 .UNSPECIFIED.,.F.,.F.,(4,3,3,3,3,3,3,3,3,3,3,3,3,3,3,3,3,3,3,3,3,3,3,3,
3,3,3,4),(63.9265539370322,64.00318398046,64.0833432946404,64.1635026088209,
64.2430544733194,64.3225462087708,64.4019900674868,64.4813982643922,64.560782985931,
64.6401690219161,64.7195578032026,64.7989604018192,64.8783878974505,64.9578866205902,
65.037423765986,65.1170492994503,65.1610449901458,65.2387124703698,65.3162939254393,
65.3938032763762,65.4712441475004,65.5486453427992,65.6260206547658,65.6598161808083,
65.7382235669259,65.8164648295238,65.8949552774012,65.9734457252786),
 .UNSPECIFIED.);
#3248=B_SPLINE_CURVE_WITH_KNOTS('',3,(#37484,#37485,#37486,#37487,#37488,
#37489,#37490,#37491,#37492,#37493,#37494,#37495,#37496,#37497,#37498,#37499,
#37500,#37501,#37502,#37503,#37504,#37505,#37506,#37507,#37508,#37509,#37510,
#37511,#37512,#37513,#37514,#37515,#37516,#37517,#37518,#37519,#37520,#37521,
#37522,#37523,#37524,#37525,#37526,#37527,#37528,#37529,#37530,#37531,#37532,
#37533,#37534,#37535,#37536,#37537,#37538,#37539,#37540,#37541,#37542,#37543,
#37544,#37545,#37546,#37547,#37548,#37549,#37550,#37551,#37552,#37553,#37554,
#37555,#37556,#37557,#37558,#37559),.UNSPECIFIED.,.F.,.F.,(4,3,3,3,3,3,
3,3,3,3,3,3,3,3,3,3,3,3,3,3,3,3,3,3,3,4),(63.9269386766303,64.0094002803605,
64.0918612182123,64.1743215175843,64.2567812058726,64.3392403104709,64.4216988587714,
64.5041568781639,64.5866143960367,64.673291354121,64.7557581396621,64.83822325273,
64.920686802978,65.0031489000373,65.0856096535188,65.1680691730148,65.2505275681,
65.3329849483335,65.4154513340197,65.4979145355279,65.5803749913775,65.6628331399324,
65.745298743686,65.8277586220738,65.9102227333261,65.9734457253863),
 .UNSPECIFIED.);
#3249=B_SPLINE_CURVE_WITH_KNOTS('',3,(#37560,#37561,#37562,#37563,#37564,
#37565,#37566,#37567,#37568,#37569,#37570,#37571,#37572,#37573,#37574,#37575,
#37576,#37577,#37578,#37579,#37580,#37581,#37582,#37583,#37584,#37585,#37586,
#37587,#37588,#37589,#37590,#37591,#37592,#37593,#37594,#37595,#37596,#37597,
#37598,#37599,#37600,#37601,#37602,#37603,#37604,#37605,#37606,#37607,#37608,
#37609,#37610,#37611,#37612,#37613,#37614,#37615,#37616,#37617,#37618,#37619,
#37620,#37621,#37622,#37623,#37624,#37625,#37626,#37627,#37628,#37629,#37630,
#37631,#37632,#37633,#37634,#37635,#37636,#37637,#37638,#37639,#37640,#37641,
#37642,#37643,#37644,#37645,#37646,#37647,#37648,#37649,#37650,#37651,#37652,
#37653,#37654,#37655,#37656,#37657,#37658,#37659,#37660,#37661,#37662,#37663,
#37664,#37665,#37666,#37667,#37668,#37669,#37670,#37671,#37672,#37673,#37674,
#37675,#37676,#37677,#37678,#37679,#37680,#37681,#37682,#37683,#37684,#37685,
#37686,#37687,#37688,#37689,#37690,#37691,#37692,#37693,#37694,#37695,#37696,
#37697,#37698,#37699,#37700,#37701,#37702,#37703,#37704,#37705,#37706,#37707,
#37708,#37709,#37710,#37711,#37712,#37713,#37714,#37715,#37716,#37717,#37718,
#37719,#37720,#37721,#37722,#37723,#37724,#37725,#37726,#37727,#37728),
 .UNSPECIFIED.,.F.,.F.,(4,3,3,3,3,3,3,3,3,3,3,3,3,3,3,3,3,3,3,3,3,3,3,3,
3,3,3,3,3,3,3,3,3,3,3,3,3,3,3,3,3,3,3,3,3,3,3,3,3,3,3,3,3,3,3,3,4),(65.9734457253863,
65.9810926300257,66.0623246831153,66.1436054014539,66.2276700062625,66.3091021411186,
66.3944829809034,66.4798638206882,66.5650967441582,66.6502517053848,66.7352566421077,
66.8201549341999,66.9048614805259,66.9786350113506,67.0551939760377,67.1317475429172,
67.2083103084957,67.2849288409634,67.3615786094582,67.4383117229479,67.4774062020131,
67.5569580665117,67.636449801963,67.7158936606789,67.7953018575844,67.8746865791232,
67.9540726151082,68.0334613963946,68.1128639950112,68.1922914906426,68.2717902137823,
68.3513273591781,68.4309528926424,68.474948583338,68.5526160635619,68.6301975186313,
68.7077068695681,68.7851477406922,68.8625489359912,68.9399242479578,68.9737197740004,
69.0572112196602,69.1408588644053,69.2247440872693,69.3087428656718,69.3929271215806,
69.4724909646629,69.550013477377,69.6274512587079,69.7048066037302,69.7821149488811,
69.859390366979,69.9366469095249,70.0139157169229,70.0911907175262,70.168510631772,
70.2097424676708),.UNSPECIFIED.);
#3250=B_SPLINE_CURVE_WITH_KNOTS('',3,(#37734,#37735,#37736,#37737,#37738,
#37739,#37740,#37741,#37742,#37743,#37744,#37745,#37746,#37747,#37748,#37749,
#37750,#37751,#37752,#37753,#37754,#37755,#37756,#37757,#37758,#37759,#37760,
#37761,#37762,#37763,#37764,#37765,#37766,#37767,#37768,#37769,#37770,#37771,
#37772,#37773,#37774,#37775,#37776,#37777,#37778,#37779,#37780,#37781,#37782,
#37783,#37784,#37785,#37786,#37787,#37788,#37789,#37790,#37791,#37792,#37793,
#37794,#37795,#37796,#37797,#37798,#37799,#37800,#37801,#37802,#37803,#37804,
#37805,#37806,#37807,#37808,#37809,#37810,#37811,#37812,#37813,#37814,#37815,
#37816,#37817,#37818,#37819,#37820,#37821,#37822,#37823,#37824,#37825,#37826,
#37827,#37828,#37829,#37830,#37831,#37832,#37833,#37834,#37835,#37836,#37837,
#37838,#37839,#37840,#37841,#37842,#37843,#37844,#37845,#37846,#37847,#37848,
#37849,#37850,#37851,#37852,#37853,#37854,#37855,#37856,#37857,#37858,#37859,
#37860,#37861,#37862,#37863,#37864,#37865,#37866,#37867,#37868,#37869,#37870,
#37871,#37872,#37873,#37874,#37875,#37876,#37877,#37878,#37879,#37880,#37881,
#37882,#37883,#37884,#37885,#37886,#37887,#37888,#37889,#37890,#37891,#37892,
#37893,#37894,#37895,#37896,#37897,#37898,#37899,#37900,#37901,#37902),
 .UNSPECIFIED.,.F.,.F.,(4,3,3,3,3,3,3,3,3,3,3,3,3,3,3,3,3,3,3,3,3,3,3,3,
3,3,3,3,3,3,3,3,3,3,3,3,3,3,3,3,3,3,3,3,3,3,3,3,3,3,3,3,3,3,3,3,4),(72.2566310327126,
72.3313121276164,72.4091373082329,72.4837084895956,72.5582532064747,72.632791315131,
72.6426128500825,72.726104295742,72.8097519404872,72.8936371633511,72.9776359417537,
73.0618201976625,73.141384040745,73.2188931735855,73.2963204492617,73.3736814844835,
73.4509918484771,73.5282670736598,73.6055355777766,73.6828033123908,73.760084313747,
73.8373926229171,73.9147887350027,73.9922304963612,74.0697916841005,74.1389264220699,
74.214992581527,74.2909640825609,74.3668577023579,74.4426901386452,74.5184780282295,
74.5957268751251,74.6714906737762,74.7472625798402,74.8230575973111,74.9014103988321,
74.977338937534,75.0569038704644,75.1364688033948,75.2150134203333,75.2934654625038,
75.3718394230859,75.4501497399251,75.5284108052985,75.6066400985656,75.6848528953103,
75.7630621814379,75.8412809383761,75.9195546174888,75.997856839255,76.0762422958305,
76.1340111847197,76.2136727228051,76.2932430320982,76.3727592970901,76.4522228690431,
76.4934152645304),.UNSPECIFIED.);
#3251=B_SPLINE_CURVE_WITH_KNOTS('',3,(#37903,#37904,#37905,#37906,#37907,
#37908,#37909,#37910,#37911,#37912,#37913,#37914,#37915,#37916,#37917,#37918,
#37919,#37920,#37921,#37922,#37923,#37924,#37925,#37926,#37927,#37928,#37929,
#37930,#37931,#37932,#37933,#37934,#37935,#37936,#37937,#37938,#37939,#37940,
#37941,#37942,#37943,#37944,#37945,#37946,#37947,#37948,#37949,#37950,#37951,
#37952,#37953,#37954,#37955,#37956,#37957,#37958,#37959,#37960,#37961,#37962,
#37963,#37964,#37965,#37966,#37967,#37968,#37969,#37970,#37971,#37972,#37973,
#37974,#37975,#37976,#37977,#37978,#37979,#37980,#37981,#37982,#37983,#37984,
#37985,#37986,#37987),.UNSPECIFIED.,.F.,.F.,(4,3,3,3,3,3,3,3,3,3,3,3,3,
3,3,3,3,3,3,3,3,3,3,3,3,3,3,3,4),(70.2102685302427,70.2954469856682,70.3834672611094,
70.4683925970241,70.5532024315297,70.6378374491525,70.6475280874328,70.7240870521199,
70.8006406189992,70.8772033845776,70.9538219170453,71.0304716855401,71.1072047990298,
71.1462992780952,71.2258511425937,71.305342878045,71.3847867367609,71.4641949336664,
71.5435796552054,71.6229656911904,71.7023544724769,71.7817570710934,71.8611845667248,
71.9406832898644,72.0202204352601,72.0998459687243,72.1438416594201,72.2468670271058,
72.256631032566),.UNSPECIFIED.);
#3252=B_SPLINE_CURVE_WITH_KNOTS('',3,(#37989,#37990,#37991,#37992,#37993,
#37994,#37995,#37996,#37997,#37998,#37999,#38000,#38001,#38002,#38003,#38004,
#38005,#38006,#38007,#38008,#38009,#38010,#38011,#38012,#38013,#38014,#38015,
#38016,#38017,#38018,#38019,#38020,#38021,#38022,#38023,#38024,#38025,#38026,
#38027,#38028,#38029,#38030,#38031,#38032,#38033,#38034,#38035,#38036,#38037,
#38038,#38039,#38040,#38041,#38042,#38043,#38044,#38045,#38046,#38047,#38048,
#38049,#38050,#38051,#38052,#38053,#38054,#38055,#38056,#38057,#38058,#38059,
#38060,#38061,#38062,#38063,#38064,#38065,#38066,#38067,#38068,#38069,#38070),
 .UNSPECIFIED.,.F.,.F.,(4,3,3,3,3,3,3,3,3,3,3,3,3,3,3,3,3,3,3,3,3,3,3,3,
3,3,3,4),(70.2097424676708,70.2871613343337,70.3646325929258,70.4422117669932,
70.4700333459878,70.5460995054449,70.6220710064789,70.6979646262759,70.7737970625631,
70.8495849521472,70.9268337990429,71.002597597694,71.0783695037581,71.1541645212292,
71.2325173227501,71.3084458614519,71.3880107943822,71.4675757273126,71.5456282131303,
71.6235863221168,71.7027169109229,71.7805192981694,71.8582788079244,71.9360090598409,
72.0161645530222,72.0938914798003,72.1752612561831,72.2566310325659),
 .UNSPECIFIED.);
#3253=B_SPLINE_CURVE_WITH_KNOTS('',3,(#38071,#38072,#38073,#38074,#38075,
#38076,#38077,#38078,#38079,#38080,#38081,#38082,#38083,#38084,#38085,#38086,
#38087,#38088,#38089,#38090,#38091,#38092,#38093,#38094,#38095,#38096,#38097,
#38098,#38099,#38100,#38101,#38102,#38103,#38104,#38105,#38106,#38107,#38108,
#38109,#38110,#38111,#38112,#38113,#38114,#38115,#38116,#38117,#38118,#38119,
#38120,#38121,#38122,#38123,#38124,#38125,#38126,#38127,#38128,#38129,#38130,
#38131,#38132,#38133,#38134,#38135,#38136,#38137,#38138,#38139,#38140,#38141,
#38142,#38143,#38144,#38145,#38146,#38147,#38148,#38149,#38150,#38151,#38152,
#38153,#38154,#38155,#38156,#38157,#38158,#38159,#38160,#38161,#38162,#38163,
#38164,#38165,#38166,#38167,#38168,#38169,#38170,#38171,#38172,#38173,#38174,
#38175,#38176,#38177,#38178,#38179,#38180,#38181,#38182,#38183,#38184,#38185,
#38186,#38187,#38188,#38189,#38190,#38191,#38192,#38193,#38194,#38195,#38196,
#38197,#38198,#38199,#38200,#38201,#38202,#38203,#38204,#38205,#38206,#38207,
#38208,#38209,#38210,#38211,#38212,#38213,#38214,#38215,#38216,#38217,#38218,
#38219,#38220,#38221,#38222,#38223,#38224,#38225,#38226,#38227,#38228,#38229,
#38230,#38231,#38232,#38233,#38234,#38235,#38236),.UNSPECIFIED.,.F.,.F.,
(4,3,3,3,3,3,3,3,3,3,3,3,3,3,3,3,3,3,3,3,3,3,3,3,3,3,3,3,3,3,3,3,3,3,3,
3,3,3,3,3,3,3,3,3,3,3,3,3,3,3,3,3,3,3,3,4),(72.2566310326885,72.360874570663,
72.4651181086375,72.5447671289035,72.6243460205744,72.7038656632815,72.7833285747867,
72.8627574256116,72.9421618250946,72.9638892993,73.0451213523897,73.1264020707285,
73.2104666755369,73.2918988103931,73.3772796501777,73.4626604899624,73.5478934134323,
73.6330483746588,73.7180533113817,73.802951603474,73.8876581497999,73.9614316806249,
74.037990645312,74.1145442121913,74.1911069777697,74.2677255102374,74.3443752787323,
74.421108392222,74.4602028712873,74.5397547357858,74.6192464712371,74.6986903299531,
74.7780985268585,74.8574832483973,74.9368692843824,75.0162580656689,75.0956606642855,
75.1750881599169,75.2545868830565,75.3341240284524,75.4137495619166,75.4577452526122,
75.5354127328361,75.6129941879055,75.6905035388423,75.7679444099664,75.8453456052653,
75.922720917232,75.9565164432747,76.0400078889345,76.1236555336797,76.2075407565437,
76.2915395349461,76.3757237908549,76.4552876339371,76.493677445244),
 .UNSPECIFIED.);
#3254=B_SPLINE_CURVE_WITH_KNOTS('',3,(#38242,#38243,#38244,#38245,#38246,
#38247,#38248,#38249,#38250,#38251,#38252,#38253,#38254,#38255,#38256,#38257,
#38258,#38259,#38260,#38261,#38262,#38263,#38264,#38265,#38266,#38267,#38268,
#38269,#38270,#38271,#38272,#38273,#38274,#38275,#38276,#38277,#38278,#38279,
#38280,#38281,#38282,#38283,#38284,#38285,#38286,#38287,#38288,#38289,#38290,
#38291,#38292,#38293,#38294,#38295,#38296,#38297,#38298,#38299,#38300,#38301,
#38302,#38303,#38304,#38305,#38306,#38307,#38308,#38309,#38310,#38311,#38312,
#38313,#38314,#38315,#38316,#38317,#38318,#38319,#38320,#38321,#38322,#38323,
#38324,#38325,#38326,#38327,#38328,#38329,#38330,#38331,#38332,#38333,#38334,
#38335,#38336,#38337,#38338,#38339,#38340,#38341,#38342,#38343,#38344,#38345,
#38346,#38347,#38348,#38349,#38350,#38351,#38352,#38353,#38354,#38355,#38356,
#38357,#38358,#38359,#38360,#38361,#38362,#38363,#38364,#38365,#38366,#38367,
#38368,#38369,#38370,#38371,#38372,#38373,#38374,#38375,#38376,#38377,#38378,
#38379,#38380,#38381,#38382,#38383,#38384,#38385,#38386,#38387,#38388,#38389,
#38390,#38391,#38392,#38393,#38394,#38395,#38396,#38397,#38398),
 .UNSPECIFIED.,.F.,.F.,(4,3,3,3,3,3,3,3,3,3,3,3,3,3,3,3,3,3,3,3,3,3,3,3,
3,3,3,3,3,3,3,3,3,3,3,3,3,3,3,3,3,3,3,3,3,3,3,3,3,3,3,3,4),(78.5398163397456,
78.6222785458458,78.7047404036483,78.7872019200034,78.8696631017612,78.9521239557714,
79.0345844888835,79.1170447079467,79.1995046198099,79.2819642313217,79.3644235493305,
79.4468825806843,79.5293413322312,79.6117998108189,79.6942580232945,79.7767159765052,
79.8591736772983,79.9416311325201,80.0240883490175,80.1101010443035,80.1934258428618,
80.2758924484537,80.3583582098369,80.4408231544265,80.5232873096349,80.6057507028715,
80.6882133615431,80.7706753130542,80.8531365848066,80.9355972041998,81.0180571986309,
81.1005165954951,81.1829754221853,81.2654337060924,81.3478914746055,81.4303487551118,
81.5144828703029,81.5969488686628,81.679413245269,81.7618761097644,81.8443375717707,
81.92679774089,82.0092567267061,82.0917146387864,82.1773121337093,82.2597768707552,
82.3422386431415,82.4246978893066,82.5071550475453,82.5896175666279,82.6720752380387,
82.7545340292318,82.7764945981692),.UNSPECIFIED.);
#3255=B_SPLINE_CURVE_WITH_KNOTS('',3,(#38399,#38400,#38401,#38402,#38403,
#38404,#38405,#38406,#38407,#38408,#38409,#38410,#38411,#38412,#38413,#38414,
#38415,#38416,#38417,#38418,#38419,#38420,#38421,#38422,#38423,#38424,#38425,
#38426,#38427,#38428,#38429,#38430,#38431,#38432,#38433,#38434,#38435,#38436,
#38437,#38438,#38439,#38440,#38441,#38442,#38443,#38444,#38445,#38446,#38447,
#38448,#38449,#38450,#38451,#38452,#38453,#38454,#38455,#38456,#38457,#38458,
#38459,#38460,#38461,#38462,#38463,#38464,#38465,#38466,#38467,#38468,#38469,
#38470,#38471,#38472,#38473,#38474,#38475,#38476,#38477),.UNSPECIFIED.,
 .F.,.F.,(4,3,3,3,3,3,3,3,3,3,3,3,3,3,3,3,3,3,3,3,3,3,3,3,3,3,4),(76.4934152645304,
76.5728312760312,76.6327823753821,76.7140144284718,76.7952951468106,76.8793597516191,
76.9607918864751,77.0461727262598,77.1315535660446,77.2167864895144,77.3019414507413,
77.3869463874641,77.471844679557,77.5565512258828,77.630324756707,77.7068837213938,
77.7834372882729,77.8600000538509,77.9366185863188,78.0132683548138,78.0900014683037,
78.1290959473694,78.2166417543684,78.304004464484,78.3912175495642,78.4781314906048,
78.5398163397456),.UNSPECIFIED.);
#3256=B_SPLINE_CURVE_WITH_KNOTS('',3,(#38479,#38480,#38481,#38482,#38483,
#38484,#38485,#38486,#38487,#38488,#38489,#38490,#38491,#38492,#38493,#38494,
#38495,#38496,#38497,#38498,#38499,#38500,#38501,#38502,#38503,#38504,#38505,
#38506,#38507,#38508,#38509,#38510,#38511,#38512,#38513,#38514,#38515,#38516,
#38517,#38518,#38519,#38520,#38521,#38522,#38523,#38524,#38525,#38526,#38527,
#38528,#38529,#38530,#38531,#38532,#38533,#38534,#38535,#38536,#38537,#38538,
#38539,#38540,#38541,#38542,#38543,#38544,#38545,#38546,#38547,#38548,#38549,
#38550,#38551,#38552,#38553,#38554,#38555,#38556,#38557,#38558,#38559,#38560),
 .UNSPECIFIED.,.F.,.F.,(4,3,3,3,3,3,3,3,3,3,3,3,3,3,3,3,3,3,3,3,3,3,3,3,
3,3,3,4),(76.493677445244,76.5711440912438,76.6485366193094,76.7258706212713,
76.8031616468261,76.8843701928806,76.9616365371571,77.038909777402,77.1162039515329,
77.1935331065581,77.2709525658535,77.3484245796304,77.4260042417807,77.452830015262,
77.5288961747191,77.6048676757532,77.6807612955502,77.7565937318376,77.8323816214217,
77.9096304683173,77.9853942669685,78.0611661730325,78.1369611905036,78.2153139920244,
78.2912425307263,78.3708074636566,78.4503723965869,78.5398163397455),
 .UNSPECIFIED.);
#3257=B_SPLINE_CURVE_WITH_KNOTS('',3,(#38561,#38562,#38563,#38564,#38565,
#38566,#38567,#38568,#38569,#38570,#38571,#38572,#38573,#38574,#38575,#38576,
#38577,#38578,#38579,#38580,#38581,#38582,#38583,#38584,#38585,#38586,#38587,
#38588,#38589,#38590,#38591,#38592,#38593,#38594,#38595,#38596,#38597,#38598,
#38599,#38600,#38601,#38602,#38603,#38604,#38605,#38606,#38607,#38608,#38609,
#38610,#38611,#38612,#38613,#38614,#38615,#38616,#38617,#38618,#38619,#38620,
#38621,#38622,#38623,#38624,#38625,#38626,#38627,#38628,#38629,#38630,#38631,
#38632,#38633,#38634,#38635,#38636,#38637,#38638,#38639,#38640,#38641,#38642,
#38643,#38644,#38645,#38646,#38647,#38648,#38649,#38650,#38651,#38652,#38653,
#38654,#38655,#38656,#38657,#38658,#38659,#38660,#38661,#38662,#38663,#38664,
#38665,#38666,#38667,#38668,#38669,#38670,#38671,#38672,#38673,#38674,#38675,
#38676,#38677,#38678,#38679,#38680,#38681,#38682,#38683,#38684,#38685,#38686,
#38687,#38688,#38689,#38690,#38691,#38692,#38693,#38694,#38695,#38696,#38697,
#38698,#38699,#38700,#38701,#38702,#38703,#38704,#38705,#38706,#38707,#38708,
#38709,#38710,#38711,#38712,#38713,#38714,#38715,#38716,#38717,#38718,#38719,
#38720,#38721,#38722,#38723,#38724,#38725,#38726,#38727,#38728,#38729),
 .UNSPECIFIED.,.F.,.F.,(4,3,3,3,3,3,3,3,3,3,3,3,3,3,3,3,3,3,3,3,3,3,3,3,
3,3,3,3,3,3,3,3,3,3,3,3,3,3,3,3,3,3,3,3,3,3,3,3,3,3,3,3,3,3,3,3,4),(78.539816339892,
78.617154154896,78.6944012009266,78.7715733540667,78.8486864351297,78.9257566485886,
79.002804254068,79.0798434968287,79.1568886147571,79.2339870215937,79.3111130641337,
79.3883252186171,79.4479147779118,79.5275637981778,79.607142689849,79.6866623325567,
79.766125244062,79.8455540948865,79.9249584943695,79.9466859685742,80.0279180216639,
80.1091987400025,80.1932633448111,80.2746954796673,80.360076319452,80.4454571592367,
80.5306900827067,80.6158450439336,80.7008499806565,80.7857482727492,80.8704548190752,
80.9442283498991,81.0207873145861,81.0973408814656,81.1739036470445,81.2505221795123,
81.3271719480072,81.4039050614971,81.4429995405616,81.52255140506,81.6020431405114,
81.6814869992272,81.7608951961323,81.8402799176709,81.919665953656,81.9990547349426,
82.0784573335592,82.1578848291906,82.2373835523303,82.3169206977262,82.3965462311905,
82.4405419218865,82.5182286726415,82.5958021443857,82.6733101098667,82.7507541166275,
82.7769101946331),.UNSPECIFIED.);
#3258=B_SPLINE_CURVE_WITH_KNOTS('',3,(#38735,#38736,#38737,#38738,#38739,
#38740,#38741,#38742,#38743,#38744,#38745,#38746,#38747,#38748,#38749,#38750,
#38751,#38752,#38753,#38754,#38755,#38756,#38757,#38758,#38759,#38760,#38761,
#38762,#38763,#38764,#38765,#38766,#38767,#38768,#38769,#38770,#38771,#38772,
#38773,#38774,#38775,#38776,#38777,#38778,#38779,#38780,#38781,#38782,#38783,
#38784,#38785,#38786,#38787,#38788,#38789,#38790,#38791,#38792,#38793,#38794,
#38795,#38796,#38797,#38798,#38799,#38800,#38801,#38802,#38803,#38804,#38805,
#38806,#38807,#38808,#38809,#38810,#38811,#38812,#38813,#38814,#38815,#38816,
#38817,#38818,#38819,#38820,#38821,#38822,#38823,#38824,#38825,#38826,#38827,
#38828,#38829,#38830,#38831,#38832,#38833,#38834,#38835,#38836,#38837,#38838,
#38839,#38840,#38841,#38842,#38843,#38844,#38845,#38846,#38847,#38848,#38849,
#38850,#38851,#38852,#38853,#38854,#38855,#38856,#38857,#38858,#38859,#38860,
#38861,#38862,#38863,#38864,#38865,#38866,#38867,#38868,#38869,#38870,#38871,
#38872,#38873,#38874,#38875,#38876,#38877,#38878,#38879,#38880,#38881,#38882,
#38883,#38884,#38885,#38886,#38887,#38888,#38889,#38890,#38891,#38892,#38893,
#38894,#38895,#38896,#38897,#38898,#38899,#38900,#38901,#38902,#38903),
 .UNSPECIFIED.,.F.,.F.,(4,3,3,3,3,3,3,3,3,3,3,3,3,3,3,3,3,3,3,3,3,3,3,3,
3,3,3,3,3,3,3,3,3,3,3,3,3,3,3,3,3,3,3,3,3,3,3,3,3,3,3,3,3,3,3,3,4),(84.8230016469252,
84.9046620215766,84.986419473943,85.0683393510559,85.1118926166437,85.1914444811422,
85.2709362165935,85.3503800753096,85.4297882722149,85.5091729937536,85.5885590297386,
85.6679478110251,85.7473504096418,85.8267779052732,85.9062766284129,85.9858137738086,
86.0654393072728,86.1094349979686,86.1871024781925,86.2646839332619,86.3421932841988,
86.4196341553229,86.4970353506218,86.5744106625885,86.608206188631,86.6916976342907,
86.7753452790357,86.8592305018997,86.9432292803021,87.0274135362109,87.1069773792935,
87.1844865121341,87.2619137878101,87.339274823032,87.4165851870257,87.4938604122081,
87.571128916325,87.648396650939,87.7256776522952,87.802985961465,87.8803820735506,
87.9578238349092,88.0353850226484,88.1045197606184,88.1805883831446,88.2565618233008,
88.3324568615356,88.4082901980865,88.4840784716002,88.559846870807,88.6356073499835,
88.7113749072108,88.7871645446807,88.8630316358468,88.9389416534897,89.014956447619,
89.0589179048957),.UNSPECIFIED.);
#3259=B_SPLINE_CURVE_WITH_KNOTS('',3,(#38904,#38905,#38906,#38907,#38908,
#38909,#38910,#38911,#38912,#38913,#38914,#38915,#38916,#38917,#38918,#38919,
#38920,#38921,#38922,#38923,#38924,#38925,#38926,#38927,#38928,#38929,#38930,
#38931,#38932,#38933,#38934,#38935,#38936,#38937,#38938,#38939,#38940,#38941,
#38942,#38943,#38944,#38945,#38946,#38947,#38948,#38949,#38950,#38951,#38952,
#38953,#38954,#38955,#38956,#38957,#38958,#38959,#38960,#38961,#38962,#38963,
#38964,#38965,#38966,#38967,#38968,#38969,#38970,#38971,#38972,#38973,#38974,
#38975,#38976,#38977,#38978,#38979),.UNSPECIFIED.,.F.,.F.,(4,3,3,3,3,3,
3,3,3,3,3,3,3,3,3,3,3,3,3,3,3,3,3,3,3,4),(82.7764945981692,82.8589562018994,
82.9414171397513,83.0238774391233,83.1063371274115,83.1887962320099,83.2712547803103,
83.3537127997029,83.4361703175757,83.52284727566,83.6053140612011,83.687779174269,
83.770242724517,83.8527048215763,83.935165575058,84.0176250945539,84.1000834896391,
84.1825408698725,84.2650072555586,84.3474704570668,84.4299309129164,84.5123890614711,
84.5948546652248,84.6773145436127,84.759778654865,84.8230016469252),
 .UNSPECIFIED.);
#3260=B_SPLINE_CURVE_WITH_KNOTS('',3,(#38981,#38982,#38983,#38984,#38985,
#38986,#38987,#38988,#38989,#38990,#38991,#38992,#38993,#38994,#38995,#38996,
#38997,#38998,#38999,#39000,#39001,#39002,#39003,#39004,#39005,#39006,#39007,
#39008,#39009,#39010,#39011,#39012,#39013,#39014,#39015,#39016,#39017,#39018,
#39019,#39020,#39021,#39022,#39023,#39024,#39025,#39026,#39027,#39028,#39029,
#39030,#39031,#39032,#39033,#39034,#39035,#39036,#39037,#39038,#39039,#39040,
#39041,#39042,#39043,#39044,#39045,#39046,#39047,#39048,#39049,#39050,#39051,
#39052,#39053,#39054,#39055,#39056,#39057,#39058,#39059),.UNSPECIFIED.,
 .F.,.F.,(4,3,3,3,3,3,3,3,3,3,3,3,3,3,3,3,3,3,3,3,3,3,3,3,3,3,4),(82.7769101946331,
82.858111653591,82.9393131125489,83.0228045582085,83.1064522029543,83.1903374258182,
83.2743362042209,83.3585204601296,83.4380843032114,83.515593436052,83.593020711728,
83.6703817469499,83.7476921109432,83.8249673361251,83.902235840242,83.979503574856,
84.0567845762123,84.1340928853825,84.2114889974682,84.2889307588269,84.3664919465661,
84.4356266845362,84.5212431429555,84.6064436584641,84.6913848685092,84.7759142460088,
84.8230016468185),.UNSPECIFIED.);
#3261=B_SPLINE_CURVE_WITH_KNOTS('',3,(#39060,#39061,#39062,#39063,#39064,
#39065,#39066,#39067,#39068,#39069,#39070,#39071,#39072,#39073,#39074,#39075,
#39076,#39077,#39078,#39079,#39080,#39081,#39082,#39083,#39084,#39085,#39086,
#39087,#39088,#39089,#39090,#39091,#39092,#39093,#39094,#39095,#39096,#39097,
#39098,#39099,#39100,#39101,#39102,#39103,#39104,#39105,#39106,#39107,#39108,
#39109,#39110,#39111,#39112,#39113,#39114,#39115,#39116,#39117,#39118,#39119,
#39120,#39121,#39122,#39123,#39124,#39125,#39126,#39127,#39128,#39129,#39130,
#39131,#39132,#39133,#39134,#39135,#39136,#39137,#39138,#39139,#39140,#39141,
#39142,#39143,#39144,#39145,#39146,#39147,#39148,#39149,#39150,#39151,#39152,
#39153,#39154,#39155,#39156,#39157,#39158,#39159,#39160,#39161,#39162,#39163,
#39164,#39165,#39166,#39167,#39168,#39169,#39170,#39171,#39172,#39173,#39174,
#39175,#39176,#39177,#39178,#39179,#39180,#39181,#39182,#39183,#39184,#39185,
#39186,#39187,#39188,#39189,#39190,#39191,#39192,#39193,#39194,#39195,#39196,
#39197,#39198,#39199,#39200,#39201,#39202,#39203,#39204,#39205,#39206,#39207,
#39208,#39209,#39210,#39211,#39212,#39213,#39214,#39215,#39216,#39217,#39218,
#39219,#39220,#39221,#39222,#39223,#39224,#39225),.UNSPECIFIED.,.F.,.F.,
(4,3,3,3,3,3,3,3,3,3,3,3,3,3,3,3,3,3,3,3,3,3,3,3,3,3,3,3,3,3,3,3,3,3,3,
3,3,3,3,3,3,3,3,3,3,3,3,3,3,3,3,3,3,3,3,4),(84.8230016469251,84.8993440070806,
84.9756935320769,85.0520647933022,85.1284723735079,85.2049850548415,85.2815520053968,
85.3582581219713,85.4331690658612,85.5117136827997,85.5901657249703,85.6685396855523,
85.7468500023917,85.8251110677647,85.9033403610317,85.9815531577765,86.0597624439038,
86.137981200842,86.2162548799545,86.2945571017208,86.3729425582962,86.430711447186,
86.5103604674521,86.5899393591232,86.6694590018299,86.7489219133351,86.8283507641594,
86.9077551636423,86.9294826378485,87.0107146909381,87.0919954092767,87.1760600140853,
87.2574921489416,87.3428729887263,87.4282538285109,87.5134867519808,87.5986417132072,
87.6836466499301,87.7685449420231,87.853251488349,87.9270250191734,88.0035839838605,
88.0801375507398,88.1567003163181,88.2333188487859,88.3099686172805,88.3867017307701,
88.4257962098358,88.5053412725672,88.584829525727,88.6642721208719,88.743680178324,
88.8230722497529,88.9024514737574,88.9818487872157,89.0593915850525),
 .UNSPECIFIED.);
#3262=B_SPLINE_CURVE_WITH_KNOTS('',3,(#39231,#39232,#39233,#39234,#39235,
#39236,#39237,#39238,#39239,#39240,#39241,#39242,#39243,#39244,#39245,#39246,
#39247,#39248,#39249,#39250,#39251,#39252,#39253,#39254,#39255,#39256,#39257,
#39258,#39259,#39260,#39261,#39262,#39263,#39264,#39265,#39266,#39267,#39268,
#39269,#39270,#39271,#39272,#39273,#39274,#39275,#39276,#39277,#39278,#39279,
#39280,#39281,#39282,#39283,#39284,#39285,#39286,#39287,#39288,#39289,#39290,
#39291,#39292,#39293,#39294,#39295,#39296,#39297,#39298,#39299,#39300,#39301,
#39302,#39303,#39304,#39305,#39306,#39307,#39308,#39309,#39310,#39311,#39312,
#39313,#39314,#39315,#39316,#39317,#39318,#39319,#39320,#39321,#39322,#39323,
#39324,#39325,#39326,#39327,#39328,#39329,#39330,#39331,#39332,#39333,#39334,
#39335,#39336,#39337,#39338,#39339,#39340,#39341,#39342,#39343,#39344,#39345,
#39346,#39347,#39348,#39349,#39350,#39351,#39352,#39353,#39354,#39355,#39356,
#39357,#39358,#39359,#39360,#39361,#39362,#39363,#39364,#39365,#39366,#39367,
#39368,#39369,#39370,#39371,#39372,#39373,#39374,#39375,#39376,#39377,#39378,
#39379,#39380,#39381,#39382,#39383,#39384,#39385,#39386,#39387,#39388,#39389,
#39390,#39391,#39392,#39393,#39394,#39395,#39396,#39397,#39398,#39399),
 .UNSPECIFIED.,.F.,.F.,(4,3,3,3,3,3,3,3,3,3,3,3,3,3,3,3,3,3,3,3,3,3,3,3,
3,3,3,3,3,3,3,3,3,3,3,3,3,3,3,3,3,3,3,3,3,3,3,3,3,3,3,3,3,3,3,3,4),(91.1061869541048,
91.1911951043501,91.2761214668079,91.360897646181,91.4455683287238,91.5300560524809,
91.5959180952555,91.6724770599426,91.7490306268218,91.8255933924003,91.9022119248679,
91.9788616933629,92.0555948068526,92.0946892859179,92.1742411504165,92.2537328858677,
92.3331767445836,92.4125849414891,92.4919696630279,92.5713556990129,92.6507444802995,
92.7301470789161,92.8095745745474,92.889073297687,92.9686104430828,93.048235976547,
93.0922316672428,93.1698991474668,93.2474806025362,93.324989953473,93.4024308245972,
93.479832019896,93.5572073318627,93.5910028579053,93.6744943035652,93.7581419483103,
93.8420271711743,93.9260259495767,94.0102102054854,94.0897740485677,94.1672831814083,
94.2447104570843,94.3220714923062,94.3993818562999,94.4766570814823,94.5539255855992,
94.6311933202132,94.7084743215694,94.7857826307392,94.8631787428249,94.9406205041834,
95.0181816919226,95.0873164298926,95.1633810280806,95.2393622405657,95.3152561915304,
95.343736224813),.UNSPECIFIED.);
#3263=B_SPLINE_CURVE_WITH_KNOTS('',3,(#39400,#39401,#39402,#39403,#39404,
#39405,#39406,#39407,#39408,#39409,#39410,#39411,#39412,#39413,#39414,#39415,
#39416,#39417,#39418,#39419,#39420,#39421,#39422,#39423,#39424,#39425,#39426,
#39427,#39428,#39429,#39430,#39431,#39432,#39433,#39434,#39435,#39436,#39437,
#39438,#39439,#39440,#39441,#39442,#39443,#39444,#39445,#39446,#39447,#39448,
#39449,#39450,#39451,#39452,#39453,#39454,#39455,#39456,#39457,#39458,#39459,
#39460,#39461,#39462,#39463,#39464,#39465,#39466,#39467,#39468,#39469,#39470,
#39471,#39472,#39473,#39474,#39475,#39476,#39477,#39478,#39479,#39480,#39481,
#39482,#39483,#39484),.UNSPECIFIED.,.F.,.F.,(4,3,3,3,3,3,3,3,3,3,3,3,3,
3,3,3,3,3,3,3,3,3,3,3,3,3,3,3,4),(89.0589179048957,89.1020621419433,89.1806067588819,
89.2590588010526,89.3374327616345,89.4157430784736,89.4940041438465,89.5722334371135,
89.6504462338582,89.7286555199856,89.8068742769238,89.8851479560364,89.9634501778026,
90.0418356343781,90.0996045232682,90.1792535435342,90.2588324352052,90.3383520779123,
90.4178149894175,90.4972438402421,90.576648239725,90.5983757139306,90.6796077670204,
90.7608884853588,90.8449530901674,90.9263852250236,91.0117660648083,91.097146904593,
91.1061869541048),.UNSPECIFIED.);
#3264=B_SPLINE_CURVE_WITH_KNOTS('',3,(#39486,#39487,#39488,#39489,#39490,
#39491,#39492,#39493,#39494,#39495,#39496,#39497,#39498,#39499,#39500,#39501,
#39502,#39503,#39504,#39505,#39506,#39507,#39508,#39509,#39510,#39511,#39512,
#39513,#39514,#39515,#39516,#39517,#39518,#39519,#39520,#39521,#39522,#39523,
#39524,#39525,#39526,#39527,#39528,#39529,#39530,#39531,#39532,#39533,#39534,
#39535,#39536,#39537,#39538,#39539,#39540,#39541,#39542,#39543,#39544,#39545,
#39546,#39547,#39548,#39549,#39550,#39551,#39552,#39553,#39554,#39555,#39556,
#39557,#39558,#39559,#39560,#39561,#39562,#39563,#39564,#39565,#39566,#39567),
 .UNSPECIFIED.,.F.,.F.,(4,3,3,3,3,3,3,3,3,3,3,3,3,3,3,3,3,3,3,3,3,3,3,3,
3,3,3,4),(89.0593915850525,89.1388183698175,89.2183163145536,89.2978524425878,
89.3774773761306,89.4233385911607,89.5010060713846,89.5785875264542,89.6560968773908,
89.733537748515,89.8109389438138,89.8883142557805,89.9221097818232,90.0056012274829,
90.089248872227,90.1731340950911,90.2571328734935,90.3413171294022,90.4208809724856,
90.4971492482531,90.5733121606026,90.6494144829602,90.7254712026133,90.8014972719894,
90.8776696925182,90.9536943508863,91.0299406524955,91.1061869541047),
 .UNSPECIFIED.);
#3265=B_SPLINE_CURVE_WITH_KNOTS('',3,(#39568,#39569,#39570,#39571,#39572,
#39573,#39574,#39575,#39576,#39577,#39578,#39579,#39580,#39581,#39582,#39583,
#39584,#39585,#39586,#39587,#39588,#39589,#39590,#39591,#39592,#39593,#39594,
#39595,#39596,#39597,#39598,#39599,#39600,#39601,#39602,#39603,#39604,#39605,
#39606,#39607,#39608,#39609,#39610,#39611,#39612,#39613,#39614,#39615,#39616,
#39617,#39618,#39619,#39620,#39621,#39622,#39623,#39624,#39625,#39626,#39627,
#39628,#39629,#39630,#39631,#39632,#39633,#39634,#39635,#39636,#39637,#39638,
#39639,#39640,#39641,#39642,#39643,#39644,#39645,#39646,#39647,#39648,#39649,
#39650,#39651,#39652,#39653,#39654,#39655,#39656,#39657,#39658,#39659,#39660,
#39661,#39662,#39663,#39664,#39665,#39666,#39667,#39668,#39669,#39670,#39671,
#39672,#39673,#39674,#39675,#39676,#39677,#39678,#39679,#39680,#39681,#39682,
#39683,#39684,#39685,#39686,#39687,#39688,#39689,#39690,#39691,#39692,#39693,
#39694,#39695,#39696,#39697,#39698,#39699,#39700,#39701,#39702,#39703,#39704,
#39705,#39706,#39707,#39708,#39709,#39710,#39711,#39712,#39713,#39714,#39715,
#39716,#39717,#39718,#39719,#39720,#39721,#39722,#39723,#39724,#39725,#39726,
#39727,#39728,#39729,#39730,#39731,#39732,#39733),.UNSPECIFIED.,.F.,.F.,
(4,3,3,3,3,3,3,3,3,3,3,3,3,3,3,3,3,3,3,3,3,3,3,3,3,3,3,3,3,3,3,3,3,3,3,
3,3,3,3,3,3,3,3,3,3,3,3,3,3,3,3,3,3,3,3,4),(91.1061869541992,91.202852706791,
91.300745271717,91.3998480253286,91.4184233538105,91.4944895132676,91.5704610143016,
91.6463546340986,91.7221870703858,91.7979749599698,91.8752238068655,91.9509876055167,
92.0267595115807,92.102554529052,92.1809073305728,92.2568358692746,92.336400802205,
92.4159657351354,92.4945103520739,92.5729623942447,92.6513363548266,92.7296466716657,
92.8079077370387,92.8861370303058,92.9643498270504,93.0425591131778,93.1207778701159,
93.1990515492285,93.2773537709948,93.3557392275703,93.4135081164603,93.4931571367264,
93.5727360283973,93.6522556711044,93.7317185826096,93.8111474334344,93.8905518329174,
93.9122793071227,93.9935113602123,94.0747920785511,94.1588566833596,94.2402888182157,
94.3256696580005,94.4110504977852,94.4962834212552,94.5814383824818,94.6664433192047,
94.7513416112971,94.8360481576231,94.9098216884476,94.9863779586668,95.0629277392939,
95.139511303211,95.2161125564466,95.2927809813326,95.3423637038624),
 .UNSPECIFIED.);
#3266=B_SPLINE_CURVE_WITH_KNOTS('',3,(#39739,#39740,#39741,#39742,#39743,
#39744,#39745,#39746,#39747,#39748,#39749,#39750,#39751,#39752,#39753,#39754,
#39755,#39756,#39757,#39758,#39759,#39760,#39761,#39762,#39763,#39764,#39765,
#39766,#39767,#39768,#39769,#39770,#39771,#39772,#39773,#39774,#39775,#39776,
#39777,#39778,#39779,#39780,#39781,#39782,#39783,#39784,#39785,#39786,#39787,
#39788,#39789,#39790,#39791,#39792,#39793,#39794,#39795,#39796,#39797,#39798,
#39799,#39800,#39801,#39802,#39803,#39804,#39805,#39806,#39807,#39808,#39809,
#39810,#39811,#39812,#39813,#39814,#39815,#39816,#39817,#39818,#39819,#39820,
#39821,#39822,#39823,#39824,#39825,#39826,#39827,#39828,#39829,#39830,#39831,
#39832,#39833,#39834,#39835,#39836,#39837,#39838,#39839,#39840,#39841,#39842,
#39843,#39844,#39845,#39846,#39847,#39848,#39849,#39850,#39851,#39852,#39853,
#39854,#39855,#39856,#39857,#39858,#39859,#39860,#39861,#39862,#39863,#39864,
#39865,#39866,#39867,#39868,#39869,#39870,#39871,#39872,#39873,#39874,#39875,
#39876,#39877,#39878,#39879,#39880,#39881,#39882,#39883,#39884,#39885,#39886,
#39887,#39888,#39889,#39890,#39891,#39892,#39893,#39894,#39895,#39896,#39897,
#39898,#39899,#39900,#39901,#39902,#39903,#39904,#39905,#39906,#39907),
 .UNSPECIFIED.,.F.,.F.,(4,3,3,3,3,3,3,3,3,3,3,3,3,3,3,3,3,3,3,3,3,3,3,3,
3,3,3,3,3,3,3,3,3,3,3,3,3,3,3,3,3,3,3,3,3,3,3,3,3,3,3,3,3,3,3,3,4),(97.3893722613792,
97.4647384476076,97.5400988535631,97.5811723832049,97.6624044362947,97.7436851546336,
97.827749759442,97.9091818942983,97.9945627340828,98.0799435738673,98.1651764973373,
98.2503314585637,98.3353363952866,98.4202346873789,98.5049412337048,98.5787147645297,
98.6552737292166,98.7318272960958,98.8083900616736,98.8850085941413,98.9616583626361,
99.0383914761257,99.0774859551922,99.1570378196909,99.2365295551422,99.315973413858,
99.3953816107634,99.4747663323018,99.5541523682869,99.6335411495736,99.7129437481902,
99.7923712438222,99.8718699669619,99.9514071123577,100.031032645822,100.075028336517,
100.152695816741,100.23027727181,100.307786622747,100.385227493871,100.46262868917,
100.540004001137,100.57379952718,100.65729097284,100.740938617584,100.824823840448,
100.908822618851,100.993006874759,101.072570717842,101.150075052448,101.227501237278,
101.304863422243,101.385140997451,101.462416258506,101.539671877,101.616927213878,
101.625973723073),.UNSPECIFIED.);
#3267=B_SPLINE_CURVE_WITH_KNOTS('',3,(#39908,#39909,#39910,#39911,#39912,
#39913,#39914,#39915,#39916,#39917,#39918,#39919,#39920,#39921,#39922,#39923,
#39924,#39925,#39926,#39927,#39928,#39929,#39930,#39931,#39932,#39933,#39934,
#39935,#39936,#39937,#39938,#39939,#39940,#39941,#39942,#39943,#39944,#39945,
#39946,#39947,#39948,#39949,#39950,#39951,#39952,#39953,#39954,#39955,#39956,
#39957,#39958,#39959,#39960,#39961,#39962,#39963,#39964,#39965,#39966,#39967,
#39968,#39969,#39970,#39971,#39972,#39973,#39974,#39975,#39976,#39977,#39978,
#39979,#39980,#39981,#39982,#39983,#39984,#39985,#39986,#39987,#39988,#39989),
 .UNSPECIFIED.,.F.,.F.,(4,3,3,3,3,3,3,3,3,3,3,3,3,3,3,3,3,3,3,3,3,3,3,3,
3,3,3,4),(95.343736224813,95.4195499814771,95.4953254278548,95.5710919447158,
95.6468569104745,95.7226353245225,95.7984421953838,95.8743395178615,95.9502851548077,
96.0263520783713,96.0848588112175,96.163403428156,96.2418554703267,96.3202294309087,
96.3985397477477,96.4768008131207,96.5550301063878,96.6332429031325,96.7114521892599,
96.7896709461978,96.8679446253104,96.9462468470766,97.0246323036522,97.0824011925424,
97.1672384844942,97.2519609493412,97.3364921077939,97.3893722612844),
 .UNSPECIFIED.);
#3268=B_SPLINE_CURVE_WITH_KNOTS('',3,(#39991,#39992,#39993,#39994,#39995,
#39996,#39997,#39998,#39999,#40000,#40001,#40002,#40003,#40004,#40005,#40006,
#40007,#40008,#40009,#40010,#40011,#40012,#40013,#40014,#40015,#40016,#40017,
#40018,#40019,#40020,#40021,#40022,#40023,#40024,#40025,#40026,#40027,#40028,
#40029,#40030,#40031,#40032,#40033,#40034,#40035,#40036,#40037,#40038,#40039,
#40040,#40041,#40042,#40043,#40044,#40045,#40046,#40047,#40048,#40049,#40050,
#40051,#40052,#40053,#40054,#40055,#40056,#40057,#40058,#40059,#40060,#40061,
#40062,#40063,#40064,#40065,#40066,#40067,#40068,#40069,#40070,#40071,#40072),
 .UNSPECIFIED.,.F.,.F.,(4,3,3,3,3,3,3,3,3,3,3,3,3,3,3,3,3,3,3,3,3,3,3,3,
3,3,3,4),(95.3423637038624,95.4085928791101,95.4881447436086,95.56763647906,
95.6470803377759,95.7264885346813,95.80587325622,95.885259292205,95.9646480734914,
96.0440506721081,96.1234781677394,96.2029768908791,96.2825140362749,96.3621395697392,
96.406135260435,96.483802740659,96.5613841957283,96.6388935466651,96.7163344177893,
96.793735613088,96.8711109250547,96.9049064510974,96.9878070421606,97.0708472264203,
97.1541051534459,97.2374707156566,97.3210147106648,97.3893722612843),
 .UNSPECIFIED.);
#3269=B_SPLINE_CURVE_WITH_KNOTS('',3,(#40073,#40074,#40075,#40076,#40077,
#40078,#40079,#40080,#40081,#40082,#40083,#40084,#40085,#40086,#40087,#40088,
#40089,#40090,#40091,#40092,#40093,#40094,#40095,#40096,#40097,#40098,#40099,
#40100,#40101,#40102,#40103,#40104,#40105,#40106,#40107,#40108,#40109,#40110,
#40111,#40112,#40113,#40114,#40115,#40116,#40117,#40118,#40119,#40120,#40121,
#40122,#40123,#40124,#40125,#40126,#40127,#40128,#40129,#40130,#40131,#40132,
#40133,#40134,#40135,#40136,#40137,#40138,#40139,#40140,#40141,#40142,#40143,
#40144,#40145,#40146,#40147,#40148,#40149,#40150,#40151,#40152,#40153,#40154,
#40155,#40156,#40157,#40158,#40159,#40160,#40161,#40162,#40163,#40164,#40165,
#40166,#40167,#40168,#40169,#40170,#40171,#40172,#40173,#40174,#40175,#40176,
#40177,#40178,#40179,#40180,#40181,#40182,#40183,#40184,#40185,#40186,#40187,
#40188,#40189,#40190,#40191,#40192,#40193,#40194,#40195,#40196,#40197,#40198,
#40199,#40200,#40201,#40202,#40203,#40204,#40205,#40206,#40207,#40208,#40209,
#40210,#40211,#40212,#40213,#40214,#40215,#40216,#40217,#40218,#40219,#40220,
#40221,#40222,#40223,#40224,#40225,#40226,#40227,#40228,#40229,#40230,#40231,
#40232,#40233,#40234,#40235,#40236,#40237,#40238,#40239,#40240,#40241),
 .UNSPECIFIED.,.F.,.F.,(4,3,3,3,3,3,3,3,3,3,3,3,3,3,3,3,3,3,3,3,3,3,3,3,
3,3,3,3,3,3,3,3,3,3,3,3,3,3,3,3,3,3,3,3,3,3,3,3,3,3,3,3,3,3,3,3,4),(97.3893722613959,
97.4036776417599,97.4811867746005,97.5586140502765,97.6359750854984,97.713285449492,
97.7905606746746,97.8678291787915,97.9450969134055,98.0223779147616,98.0996862239315,
98.1770823360171,98.2545240973756,98.3320852851148,98.4012200230847,98.4772861825419,
98.5532576835759,98.6291513033729,98.7049837396601,98.7807716292446,98.8580204761402,
98.9337842747913,99.0095561808557,99.085351198327,99.1637039998477,99.2396325385496,
99.3191974714796,99.3987624044096,99.4773070213482,99.5557590635188,99.6341330241006,
99.7124433409397,99.7907044063129,99.86893369958,99.9471464963246,100.025355782452,
100.10357453939,100.181848218503,100.260150440269,100.338535896844,100.396304785735,
100.475953806001,100.555532697672,100.635052340379,100.714515251884,100.793944102709,
100.873348502192,100.895075976397,100.976308029487,101.057588747826,101.141653352634,
101.22308548749,101.308466327275,101.393847167059,101.479083303059,101.564215036154,
101.626603951495),.UNSPECIFIED.);
#3270=B_SPLINE_CURVE_WITH_KNOTS('',3,(#40247,#40248,#40249,#40250,#40251,
#40252,#40253,#40254,#40255,#40256,#40257,#40258,#40259,#40260,#40261,#40262,
#40263,#40264,#40265,#40266,#40267,#40268,#40269,#40270,#40271,#40272,#40273,
#40274,#40275,#40276,#40277,#40278,#40279,#40280,#40281,#40282,#40283,#40284,
#40285,#40286,#40287,#40288,#40289,#40290,#40291,#40292,#40293,#40294,#40295,
#40296,#40297,#40298,#40299,#40300,#40301,#40302,#40303,#40304,#40305,#40306,
#40307,#40308,#40309,#40310,#40311,#40312,#40313,#40314,#40315,#40316,#40317,
#40318,#40319,#40320,#40321,#40322,#40323,#40324,#40325,#40326,#40327,#40328,
#40329,#40330,#40331,#40332,#40333,#40334,#40335,#40336,#40337,#40338,#40339,
#40340,#40341,#40342,#40343,#40344,#40345,#40346,#40347,#40348,#40349,#40350,
#40351,#40352,#40353,#40354,#40355,#40356,#40357,#40358,#40359,#40360,#40361,
#40362,#40363,#40364,#40365,#40366,#40367,#40368,#40369,#40370,#40371,#40372,
#40373,#40374,#40375,#40376,#40377,#40378,#40379,#40380,#40381,#40382,#40383,
#40384,#40385,#40386,#40387,#40388,#40389,#40390,#40391,#40392,#40393,#40394,
#40395,#40396,#40397,#40398,#40399,#40400,#40401,#40402,#40403,#40404,#40405,
#40406,#40407,#40408,#40409,#40410,#40411,#40412,#40413,#40414,#40415),
 .UNSPECIFIED.,.F.,.F.,(4,3,3,3,3,3,3,3,3,3,3,3,3,3,3,3,3,3,3,3,3,3,3,3,
3,3,3,3,3,3,3,3,3,3,3,3,3,3,3,3,3,3,3,3,3,3,3,3,3,3,3,3,3,3,3,3,4),(103.672557568545,
103.756707913208,103.841117967449,103.925654775611,104.01037559108,104.065197861817,
104.144846882083,104.224425773754,104.303945416462,104.383408327967,104.462837178792,
104.542241578275,104.563969052479,104.645201105569,104.726481823907,104.810546428716,
104.891978563572,104.977359403357,105.062740243142,105.147973166612,105.233128127839,
105.318133064562,105.403031356655,105.487737902981,105.561511433804,105.638070398491,
105.71462396537,105.791186730948,105.867805263416,105.94445503191,106.0211881454,
106.060282624466,106.139834488965,106.219326224416,106.298770083132,106.378178280037,
106.457563001576,106.536949037561,106.616337818847,106.695740417464,106.775167913095,
106.854666636235,106.934203781631,107.013829315095,107.057825005791,107.135492486015,
107.213073941084,107.290583292022,107.368024163146,107.445425358445,107.522800670411,
107.556596196454,107.640043784118,107.723726110521,107.807532534318,107.891508514147,
107.908824909855),.UNSPECIFIED.);
#3271=B_SPLINE_CURVE_WITH_KNOTS('',3,(#40416,#40417,#40418,#40419,#40420,
#40421,#40422,#40423,#40424,#40425,#40426,#40427,#40428,#40429,#40430,#40431,
#40432,#40433,#40434,#40435,#40436,#40437,#40438,#40439,#40440,#40441,#40442,
#40443,#40444,#40445,#40446,#40447,#40448,#40449,#40450,#40451,#40452,#40453,
#40454,#40455,#40456,#40457,#40458,#40459,#40460,#40461,#40462,#40463,#40464,
#40465,#40466,#40467,#40468,#40469,#40470,#40471,#40472,#40473,#40474,#40475,
#40476,#40477,#40478,#40479,#40480,#40481,#40482,#40483,#40484,#40485,#40486,
#40487,#40488,#40489,#40490,#40491,#40492,#40493,#40494,#40495,#40496,#40497),
 .UNSPECIFIED.,.F.,.F.,(4,3,3,3,3,3,3,3,3,3,3,3,3,3,3,3,3,3,3,3,3,3,3,3,
3,3,3,4),(101.625973723073,101.703258039259,101.780571841722,101.857974200672,
101.935424169097,102.012990130556,102.070113099167,102.146179258624,102.222150759659,
102.298044379455,102.373876815743,102.449664705327,102.526913552223,102.602677350874,
102.678449256938,102.75424427441,102.83259707593,102.908525614632,102.988090547562,
103.067655480492,103.148594355004,103.229425492566,103.31015705143,103.390797126932,
103.471326024254,103.551787785923,103.632171854257,103.672557568464),
 .UNSPECIFIED.);
#3272=B_SPLINE_CURVE_WITH_KNOTS('',3,(#40499,#40500,#40501,#40502,#40503,
#40504,#40505,#40506,#40507,#40508,#40509,#40510,#40511,#40512,#40513,#40514,
#40515,#40516,#40517,#40518,#40519,#40520,#40521,#40522,#40523,#40524,#40525,
#40526,#40527,#40528,#40529,#40530,#40531,#40532,#40533,#40534,#40535,#40536,
#40537,#40538,#40539,#40540,#40541,#40542,#40543,#40544,#40545,#40546,#40547,
#40548,#40549,#40550,#40551,#40552,#40553,#40554,#40555,#40556,#40557,#40558,
#40559,#40560,#40561,#40562,#40563,#40564,#40565,#40566,#40567,#40568,#40569,
#40570,#40571,#40572,#40573,#40574,#40575,#40576,#40577,#40578,#40579,#40580,
#40581,#40582,#40583),.UNSPECIFIED.,.F.,.F.,(4,3,3,3,3,3,3,3,3,3,3,3,3,
3,3,3,3,3,3,3,3,3,3,3,3,3,3,3,4),(101.626603951495,101.711531805551,101.796344425241,
101.880981628715,101.892618357722,101.969177322409,102.045730889288,102.122293654866,
102.198912187334,102.275561955829,102.352295069318,102.391389548384,102.470941412883,
102.550433148334,102.62987700705,102.709285203955,102.788669925493,102.868055961478,
102.947444742764,103.02684734138,103.106274837012,103.185773560151,103.265310705547,
103.344936239011,103.388931929709,103.474046022759,103.558963574929,103.643580610126,
103.672557568464),.UNSPECIFIED.);
#3273=B_SPLINE_CURVE_WITH_KNOTS('',3,(#40584,#40585,#40586,#40587,#40588,
#40589,#40590,#40591,#40592,#40593,#40594,#40595,#40596,#40597,#40598,#40599,
#40600,#40601,#40602,#40603,#40604,#40605,#40606,#40607,#40608,#40609,#40610,
#40611,#40612,#40613,#40614,#40615,#40616,#40617,#40618,#40619,#40620,#40621,
#40622,#40623,#40624,#40625,#40626,#40627,#40628,#40629,#40630,#40631,#40632,
#40633,#40634,#40635,#40636,#40637,#40638,#40639,#40640,#40641,#40642,#40643,
#40644,#40645,#40646,#40647,#40648,#40649,#40650,#40651,#40652,#40653,#40654,
#40655,#40656,#40657,#40658,#40659,#40660,#40661,#40662,#40663,#40664,#40665,
#40666,#40667,#40668,#40669,#40670,#40671,#40672,#40673,#40674,#40675,#40676,
#40677,#40678,#40679,#40680,#40681,#40682,#40683,#40684,#40685,#40686,#40687,
#40688,#40689,#40690,#40691,#40692,#40693,#40694,#40695,#40696,#40697,#40698,
#40699,#40700,#40701,#40702,#40703,#40704,#40705,#40706,#40707,#40708,#40709,
#40710,#40711,#40712,#40713,#40714,#40715,#40716,#40717,#40718,#40719,#40720,
#40721,#40722,#40723,#40724,#40725,#40726,#40727,#40728,#40729,#40730,#40731,
#40732,#40733,#40734,#40735,#40736,#40737,#40738,#40739,#40740),
 .UNSPECIFIED.,.F.,.F.,(4,3,3,3,3,3,3,3,3,3,3,3,3,3,3,3,3,3,3,3,3,3,3,3,
3,3,3,3,3,3,3,3,3,3,3,3,3,3,3,3,3,3,3,3,3,3,3,3,3,3,3,3,4),(103.672557568464,
103.755019774564,103.837481632367,103.919943148722,104.00240433048,104.08486518449,
104.167325717602,104.249785936665,104.332245848528,104.41470546004,104.497164778049,
104.579623809402,104.662082560949,104.744541039537,104.826999252012,104.909457205223,
104.991914906016,105.074372361238,105.156829577736,105.242842273022,105.32616707158,
105.408633677172,105.491099438555,105.573564383145,105.656028538353,105.73849193159,
105.820954590261,105.903416541772,105.985877813525,106.068338432918,106.150798427349,
106.233257824213,106.315716650903,106.39817493481,106.480632703323,106.56308998383,
106.647224099021,106.729690097381,106.812154473987,106.894617338482,106.977078800489,
107.059538969608,107.141997955424,107.224455867504,107.310053362427,107.392518099473,
107.474979871859,107.557439118025,107.639896276263,107.722358795346,107.804816466757,
107.88727525795,107.909235826887),.UNSPECIFIED.);
#3274=B_SPLINE_CURVE_WITH_KNOTS('',3,(#40746,#40747,#40748,#40749,#40750,
#40751,#40752,#40753,#40754,#40755,#40756,#40757,#40758,#40759,#40760,#40761,
#40762,#40763,#40764,#40765,#40766,#40767,#40768,#40769,#40770,#40771,#40772,
#40773,#40774,#40775,#40776,#40777,#40778,#40779,#40780,#40781,#40782,#40783,
#40784,#40785,#40786,#40787,#40788,#40789,#40790,#40791,#40792,#40793,#40794,
#40795,#40796,#40797,#40798,#40799,#40800,#40801,#40802,#40803,#40804,#40805,
#40806,#40807,#40808,#40809,#40810,#40811,#40812,#40813,#40814,#40815,#40816,
#40817,#40818,#40819,#40820,#40821,#40822,#40823,#40824,#40825,#40826,#40827,
#40828,#40829,#40830,#40831,#40832,#40833,#40834,#40835,#40836,#40837,#40838,
#40839,#40840,#40841,#40842,#40843,#40844,#40845,#40846,#40847,#40848,#40849,
#40850,#40851,#40852,#40853,#40854,#40855,#40856,#40857,#40858,#40859,#40860,
#40861,#40862,#40863,#40864,#40865,#40866,#40867,#40868,#40869,#40870,#40871,
#40872,#40873,#40874,#40875,#40876,#40877,#40878,#40879,#40880,#40881,#40882,
#40883,#40884,#40885,#40886,#40887,#40888,#40889,#40890,#40891,#40892,#40893,
#40894,#40895,#40896,#40897,#40898,#40899,#40900,#40901,#40902,#40903,#40904,
#40905,#40906,#40907,#40908,#40909,#40910,#40911),.UNSPECIFIED.,.F.,.F.,
(4,3,3,3,3,3,3,3,3,3,3,3,3,3,3,3,3,3,3,3,3,3,3,3,3,3,3,3,3,3,3,3,3,3,3,
3,3,3,3,3,3,3,3,3,3,3,3,3,3,3,3,3,3,3,3,4),(109.955742875644,110.050452149766,
110.128996766704,110.207448808875,110.285822769457,110.364133086296,110.442394151669,
110.520623444936,110.598836241681,110.677045527808,110.755264284746,110.833537963859,
110.911840185625,110.9902256422,111.047994531091,111.127643551357,111.207222443028,
111.286742085736,111.366204997241,111.445633848066,111.525038247549,111.546765721753,
111.627997774842,111.709278493181,111.79334309799,111.874775232845,111.960156072631,
112.045536912416,112.130769835886,112.215924797113,112.300929733837,112.385828025929,
112.470534572256,112.544308103078,112.620867067765,112.697420634644,112.773983400223,
112.85060193269,112.927251701185,113.003984814675,113.043079293741,113.12263115824,
113.202122893691,113.281566752407,113.360974949312,113.440359670851,113.519745706836,
113.599134488123,113.67853708674,113.757964582371,113.837463305511,113.917000450907,
113.996625984371,114.040621675066,114.118278370784,114.193145417554),
 .UNSPECIFIED.);
#3275=B_SPLINE_CURVE_WITH_KNOTS('',3,(#40912,#40913,#40914,#40915,#40916,
#40917,#40918,#40919,#40920,#40921,#40922,#40923,#40924,#40925,#40926,#40927,
#40928,#40929,#40930,#40931,#40932,#40933,#40934,#40935,#40936,#40937,#40938,
#40939,#40940,#40941,#40942,#40943,#40944,#40945,#40946,#40947,#40948,#40949,
#40950,#40951,#40952,#40953,#40954,#40955,#40956,#40957,#40958,#40959,#40960,
#40961,#40962,#40963,#40964,#40965,#40966,#40967,#40968,#40969,#40970,#40971,
#40972,#40973,#40974,#40975,#40976,#40977,#40978,#40979,#40980,#40981,#40982,
#40983,#40984,#40985,#40986,#40987,#40988,#40989,#40990,#40991,#40992,#40993),
 .UNSPECIFIED.,.F.,.F.,(4,3,3,3,3,3,3,3,3,3,3,3,3,3,3,3,3,3,3,3,3,3,3,3,
3,3,3,4),(107.908824909855,107.9930213909,108.055367387116,108.132876519957,
108.210303795633,108.287664830855,108.364975194848,108.442250420031,108.519518924148,
108.596786658762,108.674067660118,108.751375969287,108.828772081373,108.906213842731,
108.98377503047,109.052909768441,109.128120422795,109.203237706626,109.278278831806,
109.353260899253,109.428571146293,109.503494903372,109.578414098686,109.653344062158,
109.72894376551,109.803975886335,109.879859380951,109.955742875567),
 .UNSPECIFIED.);
#3276=B_SPLINE_CURVE_WITH_KNOTS('',3,(#40995,#40996,#40997,#40998,#40999,
#41000,#41001,#41002,#41003,#41004,#41005,#41006,#41007,#41008,#41009,#41010,
#41011,#41012,#41013,#41014,#41015,#41016,#41017,#41018,#41019,#41020,#41021,
#41022,#41023,#41024,#41025,#41026,#41027,#41028,#41029,#41030,#41031,#41032,
#41033,#41034,#41035,#41036,#41037,#41038,#41039,#41040,#41041,#41042,#41043,
#41044,#41045,#41046,#41047,#41048,#41049,#41050,#41051,#41052,#41053,#41054,
#41055,#41056,#41057,#41058,#41059,#41060,#41061,#41062,#41063,#41064,#41065,
#41066,#41067,#41068,#41069,#41070),.UNSPECIFIED.,.F.,.F.,(4,3,3,3,3,3,
3,3,3,3,3,3,3,3,3,3,3,3,3,3,3,3,3,3,3,4),(107.909235826887,107.991697430617,
108.074158368469,108.156618667841,108.239078356129,108.321537460728,108.403996009028,
108.486454028421,108.568911546294,108.655588504378,108.738055289919,108.820520402987,
108.902983953235,108.985446050294,109.067906803776,109.150366323272,109.232824718357,
109.315282098591,109.397748484277,109.480211685785,109.562672141635,109.645130290189,
109.727595893943,109.810055772331,109.892519883583,109.955742875643),
 .UNSPECIFIED.);
#3277=B_SPLINE_CURVE_WITH_KNOTS('',3,(#41071,#41072,#41073,#41074,#41075,
#41076,#41077,#41078,#41079,#41080,#41081,#41082,#41083,#41084,#41085,#41086,
#41087,#41088,#41089,#41090,#41091,#41092,#41093,#41094,#41095,#41096,#41097,
#41098,#41099,#41100,#41101,#41102,#41103,#41104,#41105,#41106,#41107,#41108,
#41109,#41110,#41111,#41112,#41113,#41114,#41115,#41116,#41117,#41118,#41119,
#41120,#41121,#41122,#41123,#41124,#41125,#41126,#41127,#41128,#41129,#41130,
#41131,#41132,#41133,#41134,#41135,#41136,#41137,#41138,#41139,#41140,#41141,
#41142,#41143,#41144,#41145,#41146,#41147,#41148,#41149,#41150,#41151,#41152,
#41153,#41154,#41155,#41156,#41157,#41158,#41159,#41160,#41161,#41162,#41163,
#41164,#41165,#41166,#41167,#41168,#41169,#41170,#41171,#41172,#41173,#41174,
#41175,#41176,#41177,#41178,#41179,#41180,#41181,#41182,#41183,#41184,#41185,
#41186,#41187,#41188,#41189,#41190,#41191,#41192,#41193,#41194,#41195,#41196,
#41197,#41198,#41199,#41200,#41201,#41202,#41203,#41204,#41205,#41206,#41207,
#41208,#41209,#41210,#41211,#41212,#41213,#41214,#41215,#41216,#41217,#41218,
#41219,#41220,#41221,#41222,#41223,#41224,#41225,#41226,#41227,#41228,#41229,
#41230,#41231,#41232,#41233,#41234,#41235,#41236),.UNSPECIFIED.,.F.,.F.,
(4,3,3,3,3,3,3,3,3,3,3,3,3,3,3,3,3,3,3,3,3,3,3,3,3,3,3,3,3,3,3,3,3,3,3,
3,3,3,3,3,3,3,3,3,3,3,3,3,3,3,3,3,3,3,3,4),(109.955742875643,110.04305544946,
110.130814483544,110.21877247887,110.306963574977,110.371728598983,110.449396079207,
110.526977534276,110.604486885213,110.681927756337,110.759328951636,110.836704263602,
110.870499789646,110.953991235306,111.037638880051,111.121524102915,111.205522881317,
111.289707137226,111.369270980308,111.446780113149,111.524207388825,111.601568424046,
111.67887878804,111.756154013223,111.833422517339,111.910690251953,111.987971253309,
112.065279562479,112.142675674565,112.220117435923,112.297678623663,112.366813361633,
112.44287952109,112.518851022124,112.594744641921,112.670577078209,112.746364967793,
112.823613814688,112.89937761334,112.975149519404,113.050944536875,113.129297338396,
113.205225877097,113.284790810028,113.364355742958,113.442910397955,113.52137077222,
113.599751366313,113.678053989655,113.756311716738,113.834537567872,113.912744542277,
113.990961418735,114.069182613729,114.14744453706,114.192166287218),
 .UNSPECIFIED.);
#3278=B_SPLINE_CURVE_WITH_KNOTS('',3,(#41242,#41243,#41244,#41245,#41246,
#41247,#41248,#41249,#41250,#41251,#41252,#41253,#41254,#41255,#41256,#41257,
#41258,#41259,#41260,#41261,#41262,#41263,#41264,#41265,#41266,#41267,#41268,
#41269,#41270,#41271,#41272,#41273,#41274,#41275,#41276,#41277,#41278,#41279,
#41280,#41281,#41282,#41283,#41284,#41285,#41286,#41287,#41288,#41289,#41290,
#41291,#41292,#41293,#41294,#41295,#41296,#41297,#41298,#41299,#41300,#41301,
#41302,#41303,#41304,#41305,#41306,#41307,#41308,#41309,#41310,#41311,#41312,
#41313,#41314,#41315,#41316,#41317,#41318,#41319,#41320,#41321,#41322,#41323,
#41324,#41325,#41326,#41327,#41328,#41329,#41330,#41331,#41332,#41333,#41334,
#41335,#41336,#41337,#41338,#41339,#41340,#41341,#41342,#41343,#41344,#41345,
#41346,#41347,#41348,#41349,#41350,#41351,#41352,#41353,#41354,#41355,#41356,
#41357,#41358,#41359,#41360,#41361,#41362,#41363,#41364,#41365,#41366,#41367,
#41368,#41369,#41370,#41371,#41372,#41373,#41374,#41375,#41376,#41377,#41378,
#41379,#41380,#41381,#41382,#41383,#41384,#41385,#41386,#41387,#41388,#41389,
#41390,#41391,#41392,#41393,#41394,#41395,#41396,#41397,#41398,#41399,#41400,
#41401,#41402,#41403,#41404,#41405,#41406,#41407,#41408,#41409,#41410),
 .UNSPECIFIED.,.F.,.F.,(4,3,3,3,3,3,3,3,3,3,3,3,3,3,3,3,3,3,3,3,3,3,3,3,
3,3,3,3,3,3,3,3,3,3,3,3,3,3,3,3,3,3,3,3,3,3,3,3,3,3,3,3,3,3,3,3,4),(116.238928182898,
116.313671447667,116.38835424761,116.462993716109,116.537617697695,116.61223630112,
116.68686494645,116.761519068711,116.836258196363,116.911043816793,116.985943411631,
117.03324881904,117.111793435979,117.190245478149,117.268619438731,117.34692975557,
117.425190820944,117.503420114211,117.581632910955,117.659842197083,117.738060954021,
117.816334633134,117.8946368549,117.973022311475,118.030791200365,118.110440220631,
118.190019112302,118.269538755009,118.349001666515,118.42843051734,118.507834916823,
118.529562391028,118.610794444118,118.692075162456,118.776139767265,118.857571902121,
118.942952741906,119.02833358169,119.11356650516,119.198721466387,119.283726403109,
119.368624695201,119.453331241527,119.527104772352,119.603663737039,119.680217303918,
119.756780069497,119.833398601965,119.91004837046,119.98678148395,120.025875963015,
120.105430902719,120.184926973534,120.26436824715,120.343776124697,120.42316427217,
120.475463669947),.UNSPECIFIED.);
#3279=B_SPLINE_CURVE_WITH_KNOTS('',3,(#41411,#41412,#41413,#41414,#41415,
#41416,#41417,#41418,#41419,#41420,#41421,#41422,#41423,#41424,#41425,#41426,
#41427,#41428,#41429,#41430,#41431,#41432,#41433,#41434,#41435,#41436,#41437,
#41438,#41439,#41440,#41441,#41442,#41443,#41444,#41445,#41446,#41447,#41448,
#41449,#41450,#41451,#41452,#41453,#41454,#41455,#41456,#41457,#41458,#41459,
#41460,#41461,#41462,#41463,#41464,#41465,#41466,#41467,#41468,#41469,#41470,
#41471,#41472,#41473,#41474,#41475,#41476,#41477,#41478,#41479,#41480,#41481,
#41482,#41483,#41484,#41485,#41486,#41487,#41488,#41489),.UNSPECIFIED.,
 .F.,.F.,(4,3,3,3,3,3,3,3,3,3,3,3,3,3,3,3,3,3,3,3,3,3,3,3,3,3,4),(114.193145417554,
114.270657066993,114.348099558365,114.425501938043,114.502878108584,114.539392865728,
114.622884311388,114.706531956133,114.790417178996,114.874415957399,114.958600213307,
115.03816405639,115.115673189231,115.193100464907,115.270461500129,115.347771864122,
115.425047089304,115.502315593421,115.579583328035,115.656864329392,115.734172638561,
115.811568750647,115.889010512005,115.966571699745,116.035706437715,116.142943422663,
116.238928182823),.UNSPECIFIED.);
#3280=B_SPLINE_CURVE_WITH_KNOTS('',3,(#41491,#41492,#41493,#41494,#41495,
#41496,#41497,#41498,#41499,#41500,#41501,#41502,#41503,#41504,#41505,#41506,
#41507,#41508,#41509,#41510,#41511,#41512,#41513,#41514,#41515,#41516,#41517,
#41518,#41519,#41520,#41521,#41522,#41523,#41524,#41525,#41526,#41527,#41528,
#41529,#41530,#41531,#41532,#41533,#41534,#41535,#41536,#41537,#41538,#41539,
#41540,#41541,#41542,#41543,#41544,#41545,#41546,#41547,#41548,#41549,#41550,
#41551,#41552,#41553,#41554,#41555,#41556,#41557,#41558,#41559,#41560,#41561,
#41562,#41563,#41564,#41565,#41566,#41567,#41568,#41569,#41570,#41571,#41572),
 .UNSPECIFIED.,.F.,.F.,(4,3,3,3,3,3,3,3,3,3,3,3,3,3,3,3,3,3,3,3,3,3,3,3,
3,3,3,4),(114.192166287218,114.27049007846,114.348888723008,114.361898124283,
114.441547144549,114.52112603622,114.600645678928,114.680108590433,114.759537441258,
114.838941840741,114.860669314945,114.941901368034,115.023182086373,115.107246691182,
115.188678826038,115.274059665823,115.359440505608,115.444673429078,115.529828390305,
115.614833327029,115.699731619121,115.784438165448,115.85821169627,115.932457125966,
116.008925505731,116.08318163116,116.160756138093,116.238330645025),
 .UNSPECIFIED.);
#3281=B_SPLINE_CURVE_WITH_KNOTS('',3,(#41573,#41574,#41575,#41576,#41577,
#41578,#41579,#41580,#41581,#41582,#41583,#41584,#41585,#41586,#41587,#41588,
#41589,#41590,#41591,#41592,#41593,#41594,#41595,#41596,#41597,#41598,#41599,
#41600,#41601,#41602,#41603,#41604,#41605,#41606,#41607,#41608,#41609,#41610,
#41611,#41612,#41613,#41614,#41615,#41616,#41617,#41618,#41619,#41620,#41621,
#41622,#41623,#41624,#41625,#41626,#41627,#41628,#41629,#41630,#41631,#41632,
#41633,#41634,#41635,#41636,#41637,#41638,#41639,#41640,#41641,#41642,#41643,
#41644,#41645,#41646,#41647,#41648,#41649,#41650,#41651,#41652,#41653,#41654,
#41655,#41656,#41657,#41658,#41659,#41660,#41661,#41662,#41663,#41664,#41665,
#41666,#41667,#41668,#41669,#41670,#41671,#41672,#41673,#41674,#41675,#41676,
#41677,#41678,#41679,#41680,#41681,#41682,#41683,#41684,#41685,#41686,#41687,
#41688,#41689,#41690,#41691,#41692,#41693,#41694,#41695,#41696,#41697,#41698,
#41699,#41700,#41701,#41702,#41703,#41704,#41705,#41706,#41707,#41708,#41709,
#41710,#41711,#41712,#41713,#41714,#41715,#41716,#41717,#41718,#41719,#41720,
#41721,#41722,#41723,#41724,#41725,#41726,#41727,#41728,#41729),
 .UNSPECIFIED.,.F.,.F.,(4,3,3,3,3,3,3,3,3,3,3,3,3,3,3,3,3,3,3,3,3,3,3,3,
3,3,3,3,3,3,3,3,3,3,3,3,3,3,3,3,3,3,3,3,3,3,3,3,3,3,3,3,4),(116.238928182823,
116.321390388923,116.403852246726,116.486313763081,116.568774944839,116.651235798849,
116.733696331961,116.816156551024,116.898616462887,116.981076074399,117.063535392408,
117.145994423762,117.228453175308,117.310911653896,117.393369866372,117.475827819582,
117.558285520376,117.640742975597,117.723200192095,117.809212887381,117.892537685939,
117.975004291531,118.057470052914,118.139934997504,118.222399152712,118.304862545949,
118.38732520462,118.469787156132,118.552248427884,118.634709047277,118.717169041708,
118.799628438572,118.882087265263,118.96454554917,119.047003317683,119.129460598189,
119.21359471338,119.29606071174,119.378525088346,119.460987952842,119.543449414848,
119.625909583967,119.708368569783,119.790826481864,119.876423976787,119.958888713832,
120.041350486219,120.123809732384,120.206266890623,120.288729409705,120.371187081116,
120.453645872309,120.475606441247),.UNSPECIFIED.);
#3282=B_SPLINE_CURVE_WITH_KNOTS('',3,(#41735,#41736,#41737,#41738,#41739,
#41740,#41741,#41742,#41743,#41744,#41745,#41746,#41747,#41748,#41749,#41750,
#41751,#41752,#41753,#41754,#41755,#41756,#41757,#41758,#41759,#41760,#41761,
#41762,#41763,#41764,#41765,#41766,#41767,#41768,#41769,#41770,#41771,#41772,
#41773,#41774,#41775,#41776,#41777,#41778,#41779,#41780,#41781,#41782,#41783,
#41784,#41785,#41786,#41787,#41788,#41789,#41790,#41791,#41792,#41793,#41794,
#41795,#41796,#41797,#41798,#41799,#41800,#41801,#41802,#41803,#41804,#41805,
#41806,#41807,#41808,#41809,#41810,#41811,#41812,#41813,#41814,#41815,#41816,
#41817,#41818,#41819,#41820,#41821,#41822,#41823,#41824,#41825,#41826,#41827,
#41828,#41829,#41830,#41831,#41832,#41833,#41834,#41835,#41836,#41837,#41838,
#41839,#41840,#41841,#41842,#41843,#41844,#41845,#41846,#41847,#41848,#41849,
#41850,#41851,#41852,#41853,#41854,#41855,#41856,#41857,#41858,#41859,#41860,
#41861,#41862,#41863,#41864,#41865,#41866,#41867,#41868,#41869,#41870,#41871,
#41872,#41873,#41874,#41875,#41876,#41877,#41878,#41879,#41880,#41881,#41882,
#41883,#41884,#41885,#41886,#41887,#41888,#41889,#41890,#41891,#41892,#41893,
#41894,#41895,#41896,#41897,#41898,#41899,#41900),.UNSPECIFIED.,.F.,.F.,
(4,3,3,3,3,3,3,3,3,3,3,3,3,3,3,3,3,3,3,3,3,3,3,3,3,3,3,3,3,3,3,3,3,3,3,
3,3,3,3,3,3,3,3,3,3,3,3,3,3,3,3,3,3,3,3,4),(122.522113490113,122.605069596484,
122.68820086178,122.77160718408,122.855150126164,122.938923640885,123.01850310699,
123.094569266447,123.170540767481,123.246434387278,123.322266823565,123.398054713149,
123.475303560045,123.551067358696,123.62683926476,123.702634282231,123.780987083752,
123.856915622454,123.936480555384,124.016045488315,124.094590105254,124.173042147424,
124.251416108006,124.329726424845,124.407987490218,124.486216783485,124.56442958023,
124.642638866358,124.720857623296,124.799131302408,124.877433524174,124.95581898075,
125.013587869639,125.093236889905,125.172815781575,125.252335424282,125.331798335787,
125.411227186612,125.490631586094,125.512359060302,125.593591113392,125.674871831731,
125.75893643654,125.840368571396,125.92574941118,126.011130250964,126.096363174434,
126.18151813566,126.266523072382,126.351421364474,126.4361279108,126.509901441627,
126.586460327823,126.663009501421,126.739575236472,126.758437754617),
 .UNSPECIFIED.);
#3283=B_SPLINE_CURVE_WITH_KNOTS('',3,(#41901,#41902,#41903,#41904,#41905,
#41906,#41907,#41908,#41909,#41910,#41911,#41912,#41913,#41914,#41915,#41916,
#41917,#41918,#41919,#41920,#41921,#41922,#41923,#41924,#41925,#41926,#41927,
#41928,#41929,#41930,#41931,#41932,#41933,#41934,#41935,#41936,#41937,#41938,
#41939,#41940,#41941,#41942,#41943,#41944,#41945,#41946,#41947,#41948,#41949,
#41950,#41951,#41952,#41953,#41954,#41955,#41956,#41957,#41958,#41959,#41960,
#41961,#41962,#41963,#41964,#41965,#41966,#41967,#41968,#41969,#41970,#41971,
#41972,#41973,#41974,#41975,#41976,#41977,#41978,#41979,#41980,#41981,#41982),
 .UNSPECIFIED.,.F.,.F.,(4,3,3,3,3,3,3,3,3,3,3,3,3,3,3,3,3,3,3,3,3,3,3,3,
3,3,3,4),(120.475463669947,120.554850270742,120.634246911642,120.713664668923,
120.793152621789,120.872675522437,120.952293050511,121.02341834434,121.101085824564,
121.178667279634,121.25617663057,121.333617501694,121.411018696993,121.48839400896,
121.522189535002,121.605680980661,121.689328625406,121.77321384827,121.857212626673,
121.941396882581,122.020960725665,122.100426388793,122.17978824849,122.259057631398,
122.338222246484,122.417325067641,122.496364377615,122.522113490003),
 .UNSPECIFIED.);
#3284=B_SPLINE_CURVE_WITH_KNOTS('',3,(#41984,#41985,#41986,#41987,#41988,
#41989,#41990,#41991,#41992,#41993,#41994,#41995,#41996,#41997,#41998,#41999,
#42000,#42001,#42002,#42003,#42004,#42005,#42006,#42007,#42008,#42009,#42010,
#42011,#42012,#42013,#42014,#42015,#42016,#42017,#42018,#42019,#42020,#42021,
#42022,#42023,#42024,#42025,#42026,#42027,#42028,#42029,#42030,#42031,#42032,
#42033,#42034,#42035,#42036,#42037,#42038,#42039,#42040,#42041,#42042,#42043,
#42044,#42045,#42046,#42047,#42048,#42049,#42050,#42051,#42052,#42053,#42054,
#42055,#42056,#42057,#42058,#42059),.UNSPECIFIED.,.F.,.F.,(4,3,3,3,3,3,
3,3,3,3,3,3,3,3,3,3,3,3,3,3,3,3,3,3,3,4),(120.475606441247,120.558068044977,
120.640528982829,120.722989282201,120.805448970489,120.887908075087,120.970366623388,
121.052824642781,121.135282160653,121.221959118733,121.304425904274,121.386891017342,
121.46935456759,121.551816664649,121.634277418131,121.716736937627,121.799195332712,
121.881652712945,121.964119098632,122.04658230014,122.12904275599,122.211500904544,
122.293966508298,122.376426386686,122.458890497938,122.522113489927),
 .UNSPECIFIED.);
#3285=B_SPLINE_CURVE_WITH_KNOTS('',3,(#42060,#42061,#42062,#42063,#42064,
#42065,#42066,#42067,#42068,#42069,#42070,#42071,#42072,#42073,#42074,#42075,
#42076,#42077,#42078,#42079,#42080,#42081,#42082,#42083,#42084,#42085,#42086,
#42087,#42088,#42089,#42090,#42091,#42092,#42093,#42094,#42095,#42096,#42097,
#42098,#42099,#42100,#42101,#42102,#42103,#42104,#42105,#42106,#42107,#42108,
#42109,#42110,#42111,#42112,#42113,#42114,#42115,#42116,#42117,#42118,#42119,
#42120,#42121,#42122,#42123,#42124,#42125,#42126,#42127,#42128,#42129,#42130,
#42131,#42132,#42133,#42134,#42135,#42136,#42137,#42138,#42139,#42140,#42141,
#42142,#42143,#42144,#42145,#42146,#42147,#42148,#42149,#42150,#42151,#42152,
#42153,#42154,#42155,#42156,#42157,#42158,#42159,#42160,#42161,#42162,#42163,
#42164,#42165,#42166,#42167,#42168,#42169,#42170,#42171,#42172,#42173,#42174,
#42175,#42176,#42177,#42178,#42179,#42180,#42181,#42182,#42183,#42184,#42185,
#42186,#42187,#42188,#42189,#42190,#42191,#42192,#42193,#42194,#42195,#42196,
#42197,#42198,#42199,#42200,#42201,#42202,#42203,#42204,#42205,#42206,#42207,
#42208,#42209,#42210,#42211,#42212,#42213,#42214,#42215,#42216),
 .UNSPECIFIED.,.F.,.F.,(4,3,3,3,3,3,3,3,3,3,3,3,3,3,3,3,3,3,3,3,3,3,3,3,
3,3,3,3,3,3,3,3,3,3,3,3,3,3,3,3,3,3,3,3,3,3,3,3,3,3,3,3,4),(122.522113490003,
122.604575696103,122.687037553906,122.769499070261,122.851960252018,122.934421106029,
123.016881639141,123.099341858204,123.181801770067,123.264261381579,123.346720699588,
123.429179730941,123.511638482488,123.594096961076,123.676555173551,123.759013126762,
123.841470827555,123.923928282777,124.006385499274,124.09239819456,124.175722993119,
124.258189598711,124.340655360094,124.423120304683,124.505584459892,124.588047853128,
124.6705105118,124.752972463311,124.835433735064,124.917894354457,125.000354348888,
125.082813745752,125.165272572442,125.247730856349,125.330188624862,125.412645905368,
125.49678002056,125.579246018919,125.661710395526,125.744173260021,125.826634722027,
125.909094891147,125.991553876963,126.074011789043,126.159609283966,126.242074021012,
126.324535793398,126.406995039563,126.489452197802,126.571914716884,126.654372388295,
126.736831179488,126.758791748426),.UNSPECIFIED.);
#3286=B_SPLINE_CURVE_WITH_KNOTS('',3,(#42222,#42223,#42224,#42225,#42226,
#42227,#42228,#42229,#42230,#42231,#42232,#42233,#42234,#42235,#42236,#42237,
#42238,#42239,#42240,#42241,#42242,#42243,#42244,#42245,#42246,#42247,#42248,
#42249,#42250,#42251,#42252,#42253,#42254,#42255,#42256,#42257,#42258,#42259,
#42260,#42261,#42262,#42263,#42264,#42265,#42266,#42267,#42268,#42269,#42270,
#42271,#42272,#42273,#42274,#42275,#42276,#42277,#42278,#42279,#42280,#42281,
#42282,#42283,#42284,#42285,#42286,#42287,#42288,#42289,#42290,#42291,#42292,
#42293,#42294,#42295,#42296,#42297,#42298,#42299,#42300,#42301,#42302,#42303,
#42304,#42305,#42306,#42307,#42308,#42309,#42310,#42311,#42312,#42313,#42314,
#42315,#42316,#42317,#42318,#42319,#42320,#42321,#42322,#42323,#42324,#42325,
#42326,#42327,#42328,#42329,#42330,#42331,#42332,#42333,#42334,#42335,#42336,
#42337,#42338,#42339,#42340,#42341,#42342,#42343,#42344,#42345,#42346,#42347,
#42348,#42349,#42350,#42351,#42352,#42353,#42354,#42355,#42356,#42357,#42358,
#42359,#42360,#42361,#42362,#42363,#42364,#42365,#42366,#42367,#42368,#42369,
#42370,#42371,#42372,#42373,#42374,#42375,#42376,#42377,#42378,#42379,#42380,
#42381,#42382,#42383,#42384,#42385,#42386,#42387),.UNSPECIFIED.,.F.,.F.,
(4,3,3,3,3,3,3,3,3,3,3,3,3,3,3,3,3,3,3,3,3,3,3,3,3,3,3,3,3,3,3,3,3,3,3,
3,3,3,3,3,3,3,3,3,3,3,3,3,3,3,3,3,3,3,3,4),(128.805298797182,128.911988861494,
129.003757394939,129.08126652778,129.158693803456,129.236054838678,129.313365202671,
129.390640427854,129.46790893197,129.545176666585,129.622457667941,129.699765977111,
129.777162089196,129.854603850555,129.932165038294,130.001299776264,130.077365935721,
130.153337436755,130.229231056552,130.30506349284,130.380851382424,130.458100229319,
130.533864027971,130.609635934035,130.685430951506,130.763783753026,130.839712291728,
130.919277224659,130.998842157589,131.077386774527,131.155838816698,131.23421277728,
131.312523094119,131.390784159492,131.469013452759,131.547226249504,131.625435535631,
131.703654292569,131.781927971682,131.860230193448,131.938615650023,131.996384538914,
132.07603355918,132.155612450851,132.235132093558,132.314595005064,132.394023855889,
132.473428255372,132.495155729576,132.576387782666,132.657668501004,132.741733105813,
132.823165240669,132.908546080454,132.993926920239,133.04207837227),
 .UNSPECIFIED.);
#3287=B_SPLINE_CURVE_WITH_KNOTS('',3,(#42388,#42389,#42390,#42391,#42392,
#42393,#42394,#42395,#42396,#42397,#42398,#42399,#42400,#42401,#42402,#42403,
#42404,#42405,#42406,#42407,#42408,#42409,#42410,#42411,#42412,#42413,#42414,
#42415,#42416,#42417,#42418,#42419,#42420,#42421,#42422,#42423,#42424,#42425,
#42426,#42427,#42428,#42429,#42430,#42431,#42432,#42433,#42434,#42435,#42436,
#42437,#42438,#42439,#42440,#42441,#42442,#42443,#42444,#42445,#42446,#42447,
#42448,#42449,#42450,#42451,#42452,#42453,#42454,#42455,#42456,#42457,#42458,
#42459,#42460,#42461,#42462,#42463,#42464,#42465,#42466,#42467,#42468,#42469,
#42470,#42471,#42472),.UNSPECIFIED.,.F.,.F.,(4,3,3,3,3,3,3,3,3,3,3,3,3,
3,3,3,3,3,3,3,3,3,3,3,3,3,3,3,4),(126.758437754617,126.835062761065,126.911722231118,
126.988461459613,127.008672632289,127.088224496788,127.167716232239,127.247160090955,
127.32656828786,127.405953009399,127.485339045384,127.564727826671,127.644130425287,
127.723557920918,127.803056644058,127.882593789454,127.962219322918,128.006215013614,
128.083882493838,128.161463948907,128.238973299844,128.316414170968,128.393815366268,
128.471190678234,128.504986204277,128.582949343818,128.660954630138,128.739069201868,
128.805298797085),.UNSPECIFIED.);
#3288=B_SPLINE_CURVE_WITH_KNOTS('',3,(#42474,#42475,#42476,#42477,#42478,
#42479,#42480,#42481,#42482,#42483,#42484,#42485,#42486,#42487,#42488,#42489,
#42490,#42491,#42492,#42493,#42494,#42495,#42496,#42497,#42498,#42499,#42500,
#42501,#42502,#42503,#42504,#42505,#42506,#42507,#42508,#42509,#42510,#42511,
#42512,#42513,#42514,#42515,#42516,#42517,#42518,#42519,#42520,#42521,#42522,
#42523,#42524,#42525,#42526,#42527,#42528,#42529,#42530,#42531,#42532,#42533,
#42534,#42535,#42536,#42537,#42538,#42539,#42540,#42541,#42542,#42543,#42544,
#42545,#42546,#42547,#42548,#42549),.UNSPECIFIED.,.F.,.F.,(4,3,3,3,3,3,
3,3,3,3,3,3,3,3,3,3,3,3,3,3,3,3,3,3,3,4),(126.758791748426,126.841253352156,
126.923714290008,127.00617458938,127.088634277668,127.171093382267,127.253551930567,
127.33600994996,127.418467467832,127.505144425917,127.587611211458,127.670076324526,
127.752539874774,127.835001971833,127.917462725315,127.999922244811,128.082380639896,
128.164838020129,128.247304405816,128.329767607324,128.412228063174,128.494686211728,
128.577151815482,128.65961169387,128.742075805122,128.805298797182),
 .UNSPECIFIED.);
#3289=B_SPLINE_CURVE_WITH_KNOTS('',3,(#42550,#42551,#42552,#42553,#42554,
#42555,#42556,#42557,#42558,#42559,#42560,#42561,#42562,#42563,#42564,#42565,
#42566,#42567,#42568,#42569,#42570,#42571,#42572,#42573,#42574,#42575,#42576,
#42577,#42578,#42579,#42580,#42581,#42582,#42583,#42584,#42585,#42586,#42587,
#42588,#42589,#42590,#42591,#42592,#42593,#42594,#42595,#42596,#42597,#42598,
#42599,#42600,#42601,#42602,#42603,#42604,#42605,#42606,#42607,#42608,#42609,
#42610,#42611,#42612,#42613,#42614,#42615,#42616,#42617,#42618,#42619,#42620,
#42621,#42622,#42623,#42624,#42625,#42626,#42627,#42628,#42629,#42630,#42631,
#42632,#42633,#42634,#42635,#42636,#42637,#42638,#42639,#42640,#42641,#42642,
#42643,#42644,#42645,#42646,#42647,#42648,#42649,#42650,#42651,#42652,#42653,
#42654,#42655,#42656,#42657,#42658,#42659,#42660,#42661,#42662,#42663,#42664,
#42665,#42666,#42667,#42668,#42669,#42670,#42671,#42672,#42673,#42674,#42675,
#42676,#42677,#42678,#42679,#42680,#42681,#42682,#42683,#42684,#42685,#42686,
#42687,#42688,#42689,#42690,#42691,#42692,#42693,#42694,#42695,#42696,#42697,
#42698,#42699,#42700,#42701,#42702,#42703,#42704,#42705,#42706,#42707,#42708,
#42709,#42710,#42711,#42712,#42713,#42714,#42715,#42716,#42717,#42718),
 .UNSPECIFIED.,.F.,.F.,(4,3,3,3,3,3,3,3,3,3,3,3,3,3,3,3,3,3,3,3,3,3,3,3,
3,3,3,3,3,3,3,3,3,3,3,3,3,3,3,3,3,3,3,3,3,3,3,3,3,3,3,3,3,3,3,3,4),(128.805298797182,
128.826262653494,128.907494706584,128.988775424924,129.072840029732,129.154272164589,
129.239653004372,129.325033844156,129.410266767626,129.495421728852,129.580426665574,
129.665324957666,129.750031503992,129.823805034819,129.900363999506,129.976917566385,
130.053480331964,130.130098864432,130.206748632926,130.283481746416,130.322576225481,
130.40212808998,130.481619825431,130.561063684147,130.640471881052,130.719856602591,
130.799242638576,130.878631419863,130.958034018479,131.037461514111,131.11696023725,
131.196497382646,131.27612291611,131.320118606806,131.39778608703,131.475367542099,
131.552876893036,131.630317764161,131.707718959459,131.785094271426,131.818889797469,
131.902381243129,131.986028887874,132.069914110738,132.15391288914,132.238097145049,
132.317660988131,132.39518425885,132.475986430167,132.553339738529,132.630646450832,
132.70792063914,132.78517635439,132.862442965893,132.939716235435,133.017029806076,
133.041601629382),.UNSPECIFIED.);
#3290=B_SPLINE_CURVE_WITH_KNOTS('',3,(#42724,#42725,#42726,#42727,#42728,
#42729,#42730,#42731,#42732,#42733,#42734,#42735,#42736,#42737,#42738,#42739,
#42740,#42741,#42742,#42743,#42744,#42745,#42746,#42747,#42748,#42749,#42750,
#42751,#42752,#42753,#42754,#42755,#42756,#42757,#42758,#42759,#42760,#42761,
#42762,#42763,#42764,#42765,#42766,#42767,#42768,#42769,#42770,#42771,#42772,
#42773,#42774,#42775,#42776,#42777,#42778,#42779,#42780,#42781,#42782,#42783,
#42784,#42785,#42786,#42787,#42788,#42789,#42790,#42791,#42792,#42793,#42794,
#42795,#42796,#42797,#42798,#42799,#42800,#42801,#42802,#42803,#42804,#42805,
#42806,#42807,#42808,#42809,#42810,#42811,#42812,#42813,#42814,#42815,#42816,
#42817,#42818,#42819,#42820,#42821,#42822,#42823,#42824,#42825,#42826,#42827,
#42828,#42829,#42830,#42831,#42832,#42833,#42834,#42835,#42836,#42837,#42838,
#42839,#42840,#42841,#42842,#42843,#42844,#42845,#42846,#42847,#42848,#42849,
#42850,#42851,#42852,#42853,#42854,#42855,#42856,#42857,#42858,#42859,#42860,
#42861,#42862,#42863,#42864,#42865,#42866,#42867,#42868,#42869,#42870,#42871,
#42872,#42873,#42874,#42875,#42876,#42877,#42878,#42879,#42880,#42881,#42882,
#42883,#42884,#42885,#42886,#42887,#42888,#42889,#42890,#42891,#42892),
 .UNSPECIFIED.,.F.,.F.,(4,3,3,3,3,3,3,3,3,3,3,3,3,3,3,3,3,3,3,3,3,3,3,3,
3,3,3,3,3,3,3,3,3,3,3,3,3,3,3,3,3,3,3,3,3,3,3,3,3,3,3,3,3,3,3,3,4),(135.088484104504,
135.163442230927,135.238336606457,135.313179200081,135.387991964862,135.462795806253,
135.487782873551,135.571274319211,135.654921963956,135.73880718682,135.822805965222,
135.906990221131,135.986554064213,136.064063197054,136.14149047273,136.218851507951,
136.296161871945,136.373437097127,136.450705601244,136.527973335858,136.605254337215,
136.682562646384,136.75995875847,136.837400519828,136.914961707568,136.984096445538,
137.060162604995,137.136134106029,137.212027725826,137.287860162113,137.363648051697,
137.440896898593,137.516660697244,137.592432603309,137.66822762078,137.746580422301,
137.822508961003,137.902073893933,137.981638826863,138.060183443802,138.138635485972,
138.217009446554,138.295319763393,138.373580828766,138.451810122033,138.530022918778,
138.608232204905,138.686450961843,138.764724640956,138.843026862722,138.921412319298,
138.979181208188,139.058844071035,139.138415807856,139.217933488224,139.297398307652,
139.325292139011),.UNSPECIFIED.);
#3291=B_SPLINE_CURVE_WITH_KNOTS('',3,(#42893,#42894,#42895,#42896,#42897,
#42898,#42899,#42900,#42901,#42902,#42903,#42904,#42905,#42906,#42907,#42908,
#42909,#42910,#42911,#42912,#42913,#42914,#42915,#42916,#42917,#42918,#42919,
#42920,#42921,#42922,#42923,#42924,#42925,#42926,#42927,#42928,#42929,#42930,
#42931,#42932,#42933,#42934,#42935,#42936,#42937,#42938,#42939,#42940,#42941,
#42942,#42943,#42944,#42945,#42946,#42947,#42948,#42949,#42950,#42951,#42952,
#42953,#42954,#42955,#42956,#42957,#42958,#42959,#42960,#42961,#42962,#42963,
#42964,#42965,#42966,#42967,#42968,#42969,#42970,#42971,#42972,#42973,#42974),
 .UNSPECIFIED.,.F.,.F.,(4,3,3,3,3,3,3,3,3,3,3,3,3,3,3,3,3,3,3,3,3,3,3,3,
3,3,3,4),(133.04207837227,133.127269451156,133.212372531528,133.297318640989,
133.382151476148,133.466804667066,133.492698110901,133.569257075588,133.645810642467,
133.722373408045,133.798991940513,133.875641709007,133.952374822497,133.991469301563,
134.071021166062,134.150512901513,134.229956760229,134.309364957134,134.388749678673,
134.468135714658,134.547524495944,134.626927094561,134.706354590192,134.785853313332,
134.865390458728,134.945015992192,134.989011682888,135.088484104362),
 .UNSPECIFIED.);
#3292=B_SPLINE_CURVE_WITH_KNOTS('',3,(#42976,#42977,#42978,#42979,#42980,
#42981,#42982,#42983,#42984,#42985,#42986,#42987,#42988,#42989,#42990,#42991,
#42992,#42993,#42994,#42995,#42996,#42997,#42998,#42999,#43000,#43001,#43002,
#43003,#43004,#43005,#43006,#43007,#43008,#43009,#43010,#43011,#43012,#43013,
#43014,#43015,#43016,#43017,#43018,#43019,#43020,#43021,#43022,#43023,#43024,
#43025,#43026,#43027,#43028,#43029,#43030,#43031,#43032,#43033,#43034,#43035,
#43036,#43037,#43038,#43039,#43040,#43041,#43042,#43043,#43044,#43045,#43046,
#43047,#43048,#43049,#43050,#43051,#43052,#43053,#43054,#43055,#43056,#43057),
 .UNSPECIFIED.,.F.,.F.,(4,3,3,3,3,3,3,3,3,3,3,3,3,3,3,3,3,3,3,3,3,3,3,3,
3,3,3,4),(133.041601629382,133.119012760366,133.196474106686,133.274046992174,
133.315203369456,133.391269528913,133.467241029947,133.543134649744,133.618967086032,
133.694754975616,133.772003822511,133.847767621162,133.923539527227,133.999334544698,
134.077687346218,134.15361588492,134.233180817851,134.312745750781,134.39089412348,
134.46894753747,134.546901574216,134.62479799234,134.702650332631,134.7804721082,
134.858290455892,134.936103782312,135.013953840078,135.088484104362),
 .UNSPECIFIED.);
#3293=B_SPLINE_CURVE_WITH_KNOTS('',3,(#43058,#43059,#43060,#43061,#43062,
#43063,#43064,#43065,#43066,#43067,#43068,#43069,#43070,#43071,#43072,#43073,
#43074,#43075,#43076,#43077,#43078,#43079,#43080,#43081,#43082,#43083,#43084,
#43085,#43086,#43087,#43088,#43089,#43090,#43091,#43092,#43093,#43094,#43095,
#43096,#43097,#43098,#43099,#43100,#43101,#43102,#43103,#43104,#43105,#43106,
#43107,#43108,#43109,#43110,#43111,#43112,#43113,#43114,#43115,#43116,#43117,
#43118,#43119,#43120,#43121,#43122,#43123,#43124,#43125,#43126,#43127,#43128,
#43129,#43130,#43131,#43132,#43133,#43134,#43135,#43136,#43137,#43138,#43139,
#43140,#43141,#43142,#43143,#43144,#43145,#43146,#43147,#43148,#43149,#43150,
#43151,#43152,#43153,#43154,#43155,#43156,#43157,#43158,#43159,#43160,#43161,
#43162,#43163,#43164,#43165,#43166,#43167,#43168,#43169,#43170,#43171,#43172,
#43173,#43174,#43175,#43176,#43177,#43178,#43179,#43180,#43181,#43182,#43183,
#43184,#43185,#43186,#43187,#43188,#43189,#43190,#43191,#43192,#43193,#43194,
#43195,#43196,#43197,#43198,#43199,#43200,#43201,#43202,#43203,#43204,#43205,
#43206,#43207,#43208,#43209,#43210,#43211,#43212,#43213,#43214,#43215,#43216,
#43217,#43218,#43219,#43220,#43221,#43222,#43223,#43224,#43225,#43226),
 .UNSPECIFIED.,.F.,.F.,(4,3,3,3,3,3,3,3,3,3,3,3,3,3,3,3,3,3,3,3,3,3,3,3,
3,3,3,3,3,3,3,3,3,3,3,3,3,3,3,3,3,3,3,3,3,3,3,3,3,3,3,3,3,3,3,3,4),(135.088484104437,
135.187057197254,135.286852023069,135.310288132106,135.389937152372,135.469516044044,
135.549035686751,135.628498598256,135.707927449082,135.787331848565,135.809059322768,
135.890291375857,135.971572094196,136.055636699005,136.137068833861,136.222449673646,
136.307830513431,136.393063436902,136.478218398129,136.563223334852,136.648121626945,
136.732828173272,136.806601704093,136.88316066878,136.959714235659,137.036277001237,
137.112895533704,137.189545302199,137.266278415688,137.305372894756,137.384924759255,
137.464416494706,137.543860353422,137.623268550328,137.702653271866,137.782039307852,
137.861428089138,137.940830687755,138.020258183386,138.099756906526,138.179294051922,
138.258919585386,138.30291527608,138.380582756304,138.458164211373,138.53567356231,
138.613114433433,138.690515628732,138.767890940699,138.801686466743,138.885177912403,
138.968825557148,139.052710780013,139.136709558415,139.220893814324,139.300457657405,
139.325474057287),.UNSPECIFIED.);
#3294=B_SPLINE_CURVE_WITH_KNOTS('',3,(#43232,#43233,#43234,#43235,#43236,
#43237,#43238,#43239,#43240,#43241,#43242,#43243,#43244,#43245,#43246,#43247,
#43248,#43249,#43250,#43251,#43252,#43253,#43254,#43255,#43256,#43257,#43258,
#43259,#43260,#43261,#43262,#43263,#43264,#43265,#43266,#43267,#43268,#43269,
#43270,#43271,#43272,#43273,#43274,#43275,#43276,#43277,#43278,#43279,#43280,
#43281,#43282,#43283,#43284,#43285,#43286,#43287,#43288,#43289,#43290,#43291,
#43292,#43293,#43294,#43295,#43296,#43297,#43298,#43299,#43300,#43301,#43302,
#43303,#43304,#43305,#43306,#43307,#43308,#43309,#43310,#43311,#43312,#43313,
#43314,#43315,#43316,#43317,#43318,#43319,#43320,#43321,#43322,#43323,#43324,
#43325,#43326,#43327,#43328,#43329,#43330,#43331,#43332,#43333,#43334,#43335,
#43336,#43337,#43338,#43339,#43340,#43341,#43342,#43343,#43344,#43345,#43346,
#43347,#43348,#43349,#43350,#43351,#43352,#43353,#43354,#43355,#43356,#43357,
#43358,#43359,#43360,#43361,#43362,#43363,#43364,#43365,#43366,#43367,#43368,
#43369,#43370,#43371,#43372,#43373,#43374,#43375,#43376,#43377,#43378,#43379,
#43380,#43381,#43382,#43383,#43384,#43385,#43386,#43387,#43388),
 .UNSPECIFIED.,.F.,.F.,(4,3,3,3,3,3,3,3,3,3,3,3,3,3,3,3,3,3,3,3,3,3,3,3,
3,3,3,3,3,3,3,3,3,3,3,3,3,3,3,3,3,3,3,3,3,3,3,3,3,3,3,3,4),(141.371669411542,
141.454131617642,141.536593475445,141.6190549918,141.701516173558,141.783977027568,
141.86643756068,141.948897779743,142.031357691606,142.113817303118,142.196276621127,
142.27873565248,142.361194404027,142.443652882615,142.52611109509,142.608569048301,
142.691026749094,142.773484204316,142.855941420814,142.9419541161,143.025278914658,
143.10774552025,143.190211281633,143.272676226223,143.355140381431,143.437603774668,
143.520066433339,143.602528384851,143.684989656603,143.767450275996,143.849910270427,
143.932369667291,144.014828493982,144.097286777889,144.179744546402,144.262201826908,
144.346335942099,144.428801940459,144.511266317065,144.593729181561,144.676190643567,
144.758650812686,144.841109798502,144.923567710583,145.009165205505,145.091629942551,
145.174091714938,145.256550961103,145.339008119341,145.421470638424,145.503928309835,
145.586387101028,145.608347669965),.UNSPECIFIED.);
#3295=B_SPLINE_CURVE_WITH_KNOTS('',3,(#43389,#43390,#43391,#43392,#43393,
#43394,#43395,#43396,#43397,#43398,#43399,#43400,#43401,#43402,#43403,#43404,
#43405,#43406,#43407,#43408,#43409,#43410,#43411,#43412,#43413,#43414,#43415,
#43416,#43417,#43418,#43419,#43420,#43421,#43422,#43423,#43424,#43425,#43426,
#43427,#43428,#43429,#43430,#43431,#43432,#43433,#43434,#43435,#43436,#43437,
#43438,#43439,#43440,#43441,#43442,#43443,#43444,#43445,#43446,#43447,#43448,
#43449,#43450,#43451,#43452,#43453,#43454,#43455,#43456,#43457,#43458,#43459,
#43460,#43461,#43462,#43463,#43464,#43465,#43466,#43467),.UNSPECIFIED.,
 .F.,.F.,(4,3,3,3,3,3,3,3,3,3,3,3,3,3,3,3,3,3,3,3,3,3,3,3,3,3,4),(139.325292139011,
139.404712893845,139.47795239885,139.559184451939,139.640465170277,139.724529775086,
139.805961909942,139.891342749727,139.976723589513,140.061956512983,140.14711147421,
140.232116410933,140.317014703026,140.401721249352,140.475494780175,140.552053744862,
140.628607311741,140.70517007732,140.781788609787,140.858438378282,140.935171491771,
140.974265970838,141.062620839722,141.150779269528,141.238767802836,141.326421620508,
141.371669411542),.UNSPECIFIED.);
#3296=B_SPLINE_CURVE_WITH_KNOTS('',3,(#43469,#43470,#43471,#43472,#43473,
#43474,#43475,#43476,#43477,#43478,#43479,#43480,#43481,#43482,#43483,#43484,
#43485,#43486,#43487,#43488,#43489,#43490,#43491,#43492,#43493,#43494,#43495,
#43496,#43497,#43498,#43499,#43500,#43501,#43502,#43503,#43504,#43505,#43506,
#43507,#43508,#43509,#43510,#43511,#43512,#43513,#43514,#43515,#43516,#43517,
#43518,#43519,#43520,#43521,#43522,#43523,#43524,#43525,#43526,#43527,#43528,
#43529,#43530,#43531,#43532,#43533,#43534,#43535,#43536,#43537,#43538,#43539,
#43540,#43541,#43542,#43543,#43544,#43545,#43546,#43547,#43548,#43549,#43550),
 .UNSPECIFIED.,.F.,.F.,(4,3,3,3,3,3,3,3,3,3,3,3,3,3,3,3,3,3,3,3,3,3,3,3,
3,3,3,4),(139.325474057287,139.402955071056,139.480359271889,139.557702259976,
139.634999591525,139.71226678928,139.789533511538,139.866803992031,139.944092267711,
140.021412382873,140.098821829852,140.176281003969,140.253852542081,140.29800003873,
140.374066198187,140.450037699221,140.525931319018,140.601763755305,140.67755164489,
140.754800491785,140.830564290437,140.9063361965,140.982131213972,141.060484015493,
141.136412554194,141.215977487125,141.295542420055,141.371669411541),
 .UNSPECIFIED.);
#3297=B_SPLINE_CURVE_WITH_KNOTS('',3,(#43551,#43552,#43553,#43554,#43555,
#43556,#43557,#43558,#43559,#43560,#43561,#43562,#43563,#43564,#43565,#43566,
#43567,#43568,#43569,#43570,#43571,#43572,#43573,#43574,#43575,#43576,#43577,
#43578,#43579,#43580,#43581,#43582,#43583,#43584,#43585,#43586,#43587,#43588,
#43589,#43590,#43591,#43592,#43593,#43594,#43595,#43596,#43597,#43598,#43599,
#43600,#43601,#43602,#43603,#43604,#43605,#43606,#43607,#43608,#43609,#43610,
#43611,#43612,#43613,#43614,#43615,#43616,#43617,#43618,#43619,#43620,#43621,
#43622,#43623,#43624,#43625,#43626,#43627,#43628,#43629,#43630,#43631,#43632,
#43633,#43634,#43635,#43636,#43637,#43638,#43639,#43640,#43641,#43642,#43643,
#43644,#43645,#43646,#43647,#43648,#43649,#43650,#43651,#43652,#43653,#43654,
#43655,#43656,#43657,#43658,#43659,#43660,#43661,#43662,#43663,#43664,#43665,
#43666,#43667,#43668,#43669,#43670,#43671,#43672,#43673,#43674,#43675,#43676,
#43677,#43678,#43679,#43680,#43681,#43682,#43683,#43684,#43685,#43686,#43687,
#43688,#43689,#43690,#43691,#43692,#43693,#43694,#43695,#43696,#43697,#43698,
#43699,#43700,#43701,#43702,#43703,#43704,#43705,#43706,#43707,#43708,#43709,
#43710,#43711,#43712,#43713,#43714,#43715,#43716,#43717,#43718,#43719),
 .UNSPECIFIED.,.F.,.F.,(4,3,3,3,3,3,3,3,3,3,3,3,3,3,3,3,3,3,3,3,3,3,3,3,
3,3,3,3,3,3,3,3,3,3,3,3,3,3,3,3,3,3,3,3,3,3,3,3,3,3,3,3,3,3,3,3,4),(141.371669411676,
141.449146283997,141.52653116975,141.603839824246,141.681087947451,141.758291013893,
141.835469916872,141.912638791059,141.989811762845,142.06703702738,142.144288126524,
142.221627655501,142.29308480138,142.372733821646,142.452312713318,142.531832356025,
142.61129526753,142.690724118355,142.770128517839,142.791855992042,142.873088045131,
142.95436876347,143.038433368278,143.119865503134,143.20524634292,143.290627182705,
143.375860106175,143.461015067402,143.546020004126,143.630918296218,143.715624842544,
143.789398373367,143.865957338054,143.942510904934,144.019073670512,144.09569220298,
144.172341971474,144.249075084964,144.28816956403,144.367721428528,144.44721316398,
144.526657022696,144.606065219601,144.68544994114,144.764835977125,144.844224758411,
144.923627357028,145.003054852659,145.082553575799,145.162090721195,145.241716254659,
145.285711945355,145.366485127798,145.444057801989,145.521565384887,145.599009972342,
145.608804675126),.UNSPECIFIED.);
#3298=B_SPLINE_CURVE_WITH_KNOTS('',3,(#43725,#43726,#43727,#43728,#43729,
#43730,#43731,#43732,#43733,#43734,#43735,#43736,#43737,#43738,#43739,#43740,
#43741,#43742,#43743,#43744,#43745,#43746,#43747,#43748,#43749,#43750,#43751,
#43752,#43753,#43754,#43755,#43756,#43757,#43758,#43759,#43760,#43761,#43762,
#43763,#43764,#43765,#43766,#43767,#43768,#43769,#43770,#43771,#43772,#43773,
#43774,#43775,#43776,#43777,#43778,#43779,#43780,#43781,#43782,#43783,#43784,
#43785,#43786,#43787,#43788,#43789,#43790,#43791,#43792,#43793,#43794,#43795,
#43796,#43797,#43798,#43799,#43800,#43801,#43802,#43803,#43804,#43805,#43806,
#43807,#43808,#43809,#43810,#43811,#43812,#43813,#43814,#43815,#43816,#43817,
#43818,#43819,#43820,#43821,#43822,#43823,#43824,#43825,#43826,#43827,#43828,
#43829,#43830,#43831,#43832,#43833,#43834,#43835,#43836,#43837,#43838,#43839,
#43840,#43841,#43842,#43843,#43844,#43845,#43846,#43847,#43848,#43849,#43850,
#43851,#43852,#43853,#43854,#43855,#43856,#43857,#43858,#43859,#43860,#43861,
#43862,#43863,#43864,#43865,#43866,#43867,#43868,#43869,#43870,#43871,#43872,
#43873,#43874,#43875,#43876,#43877,#43878,#43879,#43880,#43881,#43882,#43883,
#43884,#43885,#43886,#43887,#43888,#43889,#43890,#43891,#43892,#43893),
 .UNSPECIFIED.,.F.,.F.,(4,3,3,3,3,3,3,3,3,3,3,3,3,3,3,3,3,3,3,3,3,3,3,3,
3,3,3,3,3,3,3,3,3,3,3,3,3,3,3,3,3,3,3,3,3,3,3,3,3,3,3,3,3,3,3,3,4),(147.654854718721,
147.735992160244,147.81721488668,147.898594140889,147.957062640112,148.036614504611,
148.116106240062,148.195550098778,148.274958295683,148.354343017221,148.433729053206,
148.513117834493,148.592520433109,148.671947928741,148.75144665188,148.830983797276,
148.91060933074,148.954605021437,149.032272501661,149.10985395673,149.187363307667,
149.264804178791,149.34220537409,149.419580686057,149.453376212099,149.536867657759,
149.620515302504,149.704400525368,149.78839930377,149.872583559679,149.952147402762,
150.029656535603,150.107083811279,150.184444846501,150.261755210495,150.339030435677,
150.416298939794,150.493566674408,150.570847675764,150.648155984934,150.72555209702,
150.802993858379,150.880555046118,150.949689784087,151.025759187579,151.101733246166,
151.177628741318,151.253462374057,151.333117788431,151.40888467808,151.484644184838,
151.560411306516,151.636201045329,151.712065430347,151.787973334086,151.863978077359,
151.890705689046),.UNSPECIFIED.);
#3299=B_SPLINE_CURVE_WITH_KNOTS('',3,(#43894,#43895,#43896,#43897,#43898,
#43899,#43900,#43901,#43902,#43903,#43904,#43905,#43906,#43907,#43908,#43909,
#43910,#43911,#43912,#43913,#43914,#43915,#43916,#43917,#43918,#43919,#43920,
#43921,#43922,#43923,#43924,#43925,#43926,#43927,#43928,#43929,#43930,#43931,
#43932,#43933,#43934,#43935,#43936,#43937,#43938,#43939,#43940,#43941,#43942,
#43943,#43944,#43945,#43946,#43947,#43948,#43949,#43950,#43951,#43952,#43953,
#43954,#43955,#43956,#43957,#43958,#43959,#43960,#43961,#43962,#43963,#43964,
#43965,#43966,#43967,#43968,#43969),.UNSPECIFIED.,.F.,.F.,(4,3,3,3,3,3,
3,3,3,3,3,3,3,3,3,3,3,3,3,3,3,3,3,3,3,4),(145.608347669965,145.690809273695,
145.773270211547,145.855730510919,145.938190199207,146.020649303806,146.103107852106,
146.185565871499,146.268023389372,146.354700347456,146.437167132997,146.519632246065,
146.602095796313,146.684557893372,146.767018646854,146.84947816635,146.931936561435,
147.014393941668,147.096860327354,147.179323528863,147.261783984712,147.344242133267,
147.426707737021,147.509167615408,147.591631726661,147.654854718721),
 .UNSPECIFIED.);
#3300=B_SPLINE_CURVE_WITH_KNOTS('',3,(#43971,#43972,#43973,#43974,#43975,
#43976,#43977,#43978,#43979,#43980,#43981,#43982,#43983,#43984,#43985,#43986,
#43987,#43988,#43989,#43990,#43991,#43992,#43993,#43994,#43995,#43996,#43997,
#43998,#43999,#44000,#44001,#44002,#44003,#44004,#44005,#44006,#44007,#44008,
#44009,#44010,#44011,#44012,#44013,#44014,#44015,#44016,#44017,#44018,#44019,
#44020,#44021,#44022,#44023,#44024,#44025,#44026,#44027,#44028,#44029,#44030,
#44031,#44032,#44033,#44034,#44035,#44036,#44037,#44038,#44039,#44040,#44041,
#44042,#44043,#44044,#44045,#44046,#44047,#44048,#44049,#44050,#44051,#44052),
 .UNSPECIFIED.,.F.,.F.,(4,3,3,3,3,3,3,3,3,3,3,3,3,3,3,3,3,3,3,3,3,3,3,3,
3,3,3,4),(145.608804675126,145.68620046657,145.763571967009,145.784483136017,
145.867974581677,145.951622226421,146.035507449285,146.119506227687,146.203690483596,
146.28325432668,146.360763459521,146.438190735197,146.515551770419,146.592862134412,
146.670137359595,146.747405863712,146.824673598326,146.901954599682,146.979262908852,
147.056659020938,147.134100782296,147.211661970036,147.280796708004,147.367304586155,
147.453352142583,147.539103971683,147.624397890549,147.654854718612),
 .UNSPECIFIED.);
#3301=B_SPLINE_CURVE_WITH_KNOTS('',3,(#44053,#44054,#44055,#44056,#44057,
#44058,#44059,#44060,#44061,#44062,#44063,#44064,#44065,#44066,#44067,#44068,
#44069,#44070,#44071,#44072,#44073,#44074,#44075,#44076,#44077,#44078,#44079,
#44080,#44081,#44082,#44083,#44084,#44085,#44086,#44087,#44088,#44089,#44090,
#44091,#44092,#44093,#44094,#44095,#44096,#44097,#44098,#44099,#44100,#44101,
#44102,#44103,#44104,#44105,#44106,#44107,#44108,#44109,#44110,#44111,#44112,
#44113,#44114,#44115,#44116,#44117,#44118,#44119,#44120,#44121,#44122,#44123,
#44124,#44125,#44126,#44127,#44128,#44129,#44130,#44131,#44132,#44133,#44134,
#44135,#44136,#44137,#44138,#44139,#44140,#44141,#44142,#44143,#44144,#44145,
#44146,#44147,#44148,#44149,#44150,#44151,#44152,#44153,#44154,#44155,#44156,
#44157,#44158,#44159,#44160,#44161,#44162,#44163,#44164,#44165,#44166,#44167,
#44168,#44169,#44170,#44171,#44172,#44173,#44174,#44175,#44176,#44177,#44178,
#44179,#44180,#44181,#44182,#44183,#44184,#44185,#44186,#44187,#44188,#44189,
#44190,#44191,#44192,#44193,#44194,#44195,#44196,#44197,#44198,#44199,#44200,
#44201,#44202,#44203,#44204,#44205,#44206,#44207,#44208,#44209,#44210,#44211,
#44212,#44213,#44214,#44215,#44216,#44217,#44218,#44219,#44220,#44221),
 .UNSPECIFIED.,.F.,.F.,(4,3,3,3,3,3,3,3,3,3,3,3,3,3,3,3,3,3,3,3,3,3,3,3,
3,3,3,3,3,3,3,3,3,3,3,3,3,3,3,3,3,3,3,3,3,3,3,3,3,3,3,3,3,3,3,3,4),(147.654854718721,
147.732790265047,147.808916093018,147.885058211055,147.961231357942,148.040508290788,
148.116834096366,148.193223597051,148.269728528119,148.278339089329,148.356883706268,
148.435335748438,148.51370970902,148.59202002586,148.670281091232,148.7485103845,
148.826723181244,148.904932467372,148.98315122431,149.061424903423,149.139727125189,
149.218112581765,149.275881470654,149.35553049092,149.435109382591,149.514629025297,
149.594091936802,149.673520787627,149.75292518711,149.774652661317,149.855884714407,
149.937165432746,150.021230037554,150.102662172411,150.188043012195,150.273423851979,
150.358656775449,150.443811736675,150.528816673398,150.61371496549,150.698421511816,
150.772195042642,150.848754007329,150.925307574209,151.001870339787,151.078488872255,
151.155138640751,151.23187175424,151.270966233304,151.350511861412,151.430000531118,
151.5094433945,151.588851572278,151.668242509683,151.747620582116,151.827013456949,
151.891250266881),.UNSPECIFIED.);
#3302=B_SPLINE_CURVE_WITH_KNOTS('',3,(#44227,#44228,#44229,#44230,#44231,
#44232,#44233,#44234,#44235,#44236,#44237,#44238,#44239,#44240,#44241,#44242,
#44243,#44244,#44245,#44246,#44247,#44248,#44249,#44250,#44251,#44252,#44253,
#44254,#44255,#44256,#44257,#44258,#44259,#44260,#44261,#44262,#44263,#44264,
#44265,#44266,#44267,#44268,#44269,#44270,#44271,#44272,#44273,#44274,#44275,
#44276,#44277,#44278,#44279,#44280,#44281,#44282,#44283,#44284,#44285,#44286,
#44287,#44288,#44289,#44290,#44291,#44292,#44293,#44294,#44295,#44296,#44297,
#44298,#44299,#44300,#44301,#44302,#44303,#44304,#44305,#44306,#44307,#44308,
#44309,#44310,#44311,#44312,#44313,#44314,#44315,#44316,#44317,#44318,#44319,
#44320,#44321,#44322,#44323,#44324,#44325,#44326,#44327,#44328,#44329,#44330,
#44331,#44332,#44333,#44334,#44335,#44336,#44337,#44338,#44339,#44340,#44341,
#44342,#44343,#44344,#44345,#44346,#44347,#44348,#44349,#44350,#44351,#44352,
#44353,#44354,#44355,#44356,#44357,#44358,#44359,#44360,#44361,#44362,#44363,
#44364,#44365,#44366,#44367,#44368,#44369,#44370,#44371,#44372,#44373,#44374,
#44375,#44376,#44377,#44378,#44379,#44380,#44381,#44382,#44383,#44384,#44385,
#44386,#44387,#44388,#44389,#44390,#44391,#44392,#44393,#44394,#44395,#44396,
#44397,#44398),.UNSPECIFIED.,.F.,.F.,(4,3,3,3,3,3,3,3,3,3,3,3,3,3,3,3,3,
3,3,3,3,3,3,3,3,3,3,3,3,3,3,3,3,3,3,3,3,3,3,3,3,3,3,3,3,3,3,3,3,3,3,3,3,
3,3,3,3,4),(153.938040025901,153.942316928061,154.027549851531,154.112704812757,
154.197709749479,154.282608041571,154.367314587896,154.441088118724,154.517647083411,
154.594200650291,154.670763415869,154.747381948337,154.824031716832,154.900764830322,
154.939859309386,155.019411173885,155.098902909336,155.178346768052,155.257754964957,
155.337139686496,155.416525722481,155.495914503768,155.575317102384,155.654744598016,
155.734243321155,155.813780466551,155.893406000015,155.937401690711,156.015069170935,
156.092650626004,156.170159976941,156.247600848065,156.325002043364,156.402377355331,
156.436172881374,156.519664327034,156.603311971779,156.687197194643,156.771195973045,
156.855380228954,156.934944072036,157.012453204877,157.089880480553,157.167241515774,
157.244551879768,157.32182710495,157.399095609067,157.476363343681,157.553644345037,
157.630952654207,157.708348766293,157.785790527651,157.863351715391,157.932486453361,
158.008554031517,158.084538123659,158.160435777525,158.175614821639),
 .UNSPECIFIED.);
#3303=B_SPLINE_CURVE_WITH_KNOTS('',3,(#44399,#44400,#44401,#44402,#44403,
#44404,#44405,#44406,#44407,#44408,#44409,#44410,#44411,#44412,#44413,#44414,
#44415,#44416,#44417,#44418,#44419,#44420,#44421,#44422,#44423,#44424,#44425,
#44426,#44427,#44428,#44429,#44430,#44431,#44432,#44433,#44434,#44435,#44436,
#44437,#44438,#44439,#44440,#44441,#44442,#44443,#44444,#44445,#44446,#44447,
#44448,#44449,#44450,#44451,#44452,#44453,#44454,#44455,#44456,#44457,#44458,
#44459,#44460,#44461,#44462,#44463,#44464,#44465,#44466,#44467,#44468,#44469,
#44470,#44471,#44472,#44473,#44474,#44475,#44476,#44477,#44478,#44479,#44480),
 .UNSPECIFIED.,.F.,.F.,(4,3,3,3,3,3,3,3,3,3,3,3,3,3,3,3,3,3,3,3,3,3,3,3,
3,3,3,4),(151.890705689046,151.947232165412,152.025776782351,152.104228824521,
152.182602785103,152.260913101942,152.339174167315,152.417403460582,152.495616257327,
152.573825543454,152.652044300392,152.730317979505,152.808620201271,152.887005657847,
152.944774546736,153.024423567002,153.104002458673,153.18352210138,153.262985012885,
153.342413863709,153.421818263192,153.443545737399,153.524692192321,153.605886223705,
153.688924674217,153.770267683524,153.854153854638,153.938040025753),
 .UNSPECIFIED.);
#3304=B_SPLINE_CURVE_WITH_KNOTS('',3,(#44482,#44483,#44484,#44485,#44486,
#44487,#44488,#44489,#44490,#44491,#44492,#44493,#44494,#44495,#44496,#44497,
#44498,#44499,#44500,#44501,#44502,#44503,#44504,#44505,#44506,#44507,#44508,
#44509,#44510,#44511,#44512,#44513,#44514,#44515,#44516,#44517,#44518,#44519,
#44520,#44521,#44522,#44523,#44524,#44525,#44526,#44527,#44528,#44529,#44530,
#44531,#44532,#44533,#44534,#44535,#44536,#44537,#44538,#44539,#44540,#44541,
#44542,#44543,#44544,#44545,#44546,#44547,#44548,#44549,#44550,#44551,#44552,
#44553,#44554,#44555,#44556,#44557,#44558,#44559,#44560,#44561,#44562,#44563),
 .UNSPECIFIED.,.F.,.F.,(4,3,3,3,3,3,3,3,3,3,3,3,3,3,3,3,3,3,3,3,3,3,3,3,
3,3,3,4),(151.891250266881,151.970672148343,152.050164692382,152.129693712078,
152.20931457057,152.268508614629,152.346176094853,152.423757549922,152.50126690086,
152.578707771984,152.656108967283,152.73348427925,152.767279805291,152.850771250951,
152.934418895696,153.01830411856,153.102302896962,153.186487152871,153.266050995954,
153.342440609636,153.418723562481,153.494945030612,153.571119933994,153.647263158056,
153.723404093323,153.799541433539,153.875718072013,153.938040025901),
 .UNSPECIFIED.);
#3305=B_SPLINE_CURVE_WITH_KNOTS('',3,(#44564,#44565,#44566,#44567,#44568,
#44569,#44570,#44571,#44572,#44573,#44574,#44575,#44576,#44577,#44578,#44579,
#44580,#44581,#44582,#44583,#44584,#44585,#44586,#44587,#44588,#44589,#44590,
#44591,#44592,#44593,#44594,#44595,#44596,#44597,#44598,#44599,#44600,#44601,
#44602,#44603,#44604,#44605,#44606,#44607,#44608,#44609,#44610,#44611,#44612,
#44613,#44614,#44615,#44616,#44617,#44618,#44619,#44620,#44621,#44622,#44623,
#44624,#44625,#44626,#44627,#44628,#44629,#44630,#44631,#44632,#44633,#44634,
#44635,#44636,#44637,#44638,#44639,#44640,#44641,#44642,#44643,#44644,#44645,
#44646,#44647,#44648,#44649,#44650,#44651,#44652,#44653,#44654,#44655,#44656,
#44657,#44658,#44659,#44660,#44661,#44662,#44663,#44664,#44665,#44666,#44667,
#44668,#44669,#44670,#44671,#44672,#44673,#44674,#44675,#44676,#44677,#44678,
#44679,#44680,#44681,#44682,#44683,#44684,#44685,#44686,#44687,#44688,#44689,
#44690,#44691,#44692,#44693,#44694,#44695,#44696,#44697,#44698,#44699,#44700,
#44701,#44702,#44703,#44704,#44705,#44706,#44707,#44708,#44709,#44710,#44711,
#44712,#44713,#44714,#44715,#44716,#44717,#44718,#44719,#44720,#44721,#44722,
#44723,#44724,#44725,#44726,#44727,#44728,#44729),.UNSPECIFIED.,.F.,.F.,
(4,3,3,3,3,3,3,3,3,3,3,3,3,3,3,3,3,3,3,3,3,3,3,3,3,3,3,3,3,3,3,3,3,3,3,
3,3,3,3,3,3,3,3,3,3,3,3,3,3,3,3,3,3,3,3,4),(153.93804002601,154.033124962491,
154.129221750043,154.22638602197,154.263593377279,154.339659536736,154.41563103777,
154.491524657567,154.567357093854,154.643144983438,154.720393830334,154.796157628985,
154.871929535049,154.94772455252,155.026077354041,155.102005892743,155.181570825674,
155.261135758604,155.339680375543,155.418132417713,155.496506378295,155.574816695134,
155.653077760507,155.731307053774,155.809519850519,155.887729136647,155.965947893585,
156.044221572697,156.122523794464,156.200909251039,156.258678139929,156.338327160195,
156.417906051866,156.497425694573,156.576888606078,156.656317456902,156.735721856385,
156.757449330591,156.838681383681,156.91996210202,157.004026706828,157.085458841684,
157.170839681469,157.256220521253,157.341453444723,157.426608405949,157.511613342672,
157.596511634764,157.68121818109,157.754991711916,157.831547530587,157.908096639881,
157.984677176914,158.061275312524,158.137935144021,158.174202348312),
 .UNSPECIFIED.);
#3306=B_SPLINE_CURVE_WITH_KNOTS('',3,(#44735,#44736,#44737,#44738,#44739,
#44740,#44741,#44742,#44743,#44744,#44745,#44746,#44747,#44748,#44749,#44750,
#44751,#44752,#44753,#44754,#44755,#44756,#44757,#44758,#44759,#44760,#44761,
#44762,#44763,#44764,#44765,#44766,#44767,#44768,#44769,#44770,#44771,#44772,
#44773,#44774,#44775,#44776,#44777,#44778,#44779,#44780,#44781,#44782,#44783,
#44784,#44785,#44786,#44787,#44788,#44789,#44790,#44791,#44792,#44793,#44794,
#44795,#44796,#44797,#44798,#44799,#44800,#44801,#44802,#44803,#44804,#44805,
#44806,#44807,#44808,#44809,#44810,#44811,#44812,#44813,#44814,#44815,#44816,
#44817,#44818,#44819,#44820,#44821,#44822,#44823,#44824,#44825,#44826,#44827,
#44828,#44829,#44830,#44831,#44832,#44833,#44834,#44835,#44836,#44837,#44838,
#44839,#44840,#44841,#44842,#44843,#44844,#44845,#44846,#44847,#44848,#44849,
#44850,#44851,#44852,#44853,#44854,#44855,#44856,#44857,#44858,#44859,#44860,
#44861,#44862,#44863,#44864,#44865,#44866,#44867,#44868,#44869,#44870,#44871,
#44872,#44873,#44874,#44875,#44876,#44877,#44878,#44879,#44880,#44881,#44882,
#44883,#44884,#44885,#44886,#44887,#44888,#44889,#44890,#44891,#44892,#44893,
#44894,#44895,#44896,#44897,#44898,#44899,#44900),.UNSPECIFIED.,.F.,.F.,
(4,3,3,3,3,3,3,3,3,3,3,3,3,3,3,3,3,3,3,3,3,3,3,3,3,3,3,3,3,3,3,3,3,3,3,
3,3,3,3,3,3,3,3,3,3,3,3,3,3,3,3,3,3,3,3,4),(160.22122533321,160.296604869896,
160.371977837822,160.426342406673,160.507574459763,160.588855178101,160.67291978291,
160.754351917766,160.839732757551,160.925113597336,161.010346520806,161.095501482032,
161.180506418755,161.265404710847,161.350111257173,161.423884787998,161.500443752685,
161.576997319564,161.653560085142,161.730178617609,161.806828386104,161.883561499593,
161.92265597866,162.002207843159,162.08169957861,162.161143437326,162.240551634232,
162.319936355771,162.399322391757,162.478711173043,162.55811377166,162.637541267291,
162.717039990431,162.796577135827,162.876202669291,162.920198359985,162.997865840209,
163.075447295279,163.152956646216,163.23039751734,163.307798712638,163.385174024605,
163.418969550648,163.502460996308,163.586108641053,163.669993863916,163.753992642319,
163.838176898228,163.91774074131,163.995246197943,164.072673295197,164.150036183801,
164.227344815413,164.304620636586,164.381889295796,164.457861495641),
 .UNSPECIFIED.);
#3307=B_SPLINE_CURVE_WITH_KNOTS('',3,(#44901,#44902,#44903,#44904,#44905,
#44906,#44907,#44908,#44909,#44910,#44911,#44912,#44913,#44914,#44915,#44916,
#44917,#44918,#44919,#44920,#44921,#44922,#44923,#44924,#44925,#44926,#44927,
#44928,#44929,#44930,#44931,#44932,#44933,#44934,#44935,#44936,#44937,#44938,
#44939,#44940,#44941,#44942,#44943,#44944,#44945,#44946,#44947,#44948,#44949,
#44950,#44951,#44952,#44953,#44954,#44955,#44956,#44957,#44958,#44959,#44960,
#44961,#44962,#44963,#44964,#44965,#44966,#44967,#44968,#44969,#44970,#44971,
#44972,#44973,#44974,#44975,#44976,#44977,#44978,#44979,#44980,#44981,#44982),
 .UNSPECIFIED.,.F.,.F.,(4,3,3,3,3,3,3,3,3,3,3,3,3,3,3,3,3,3,3,3,3,3,3,3,
3,3,3,4),(158.175614821639,158.251437002153,158.327217963255,158.402986296286,
158.478750450059,158.554525423503,158.630326222735,158.706216476536,158.782152675983,
158.858214181058,158.930028834686,159.008573451625,159.087025493795,159.165399454377,
159.243709771216,159.321970836589,159.400200129856,159.478412926601,159.556622212728,
159.634840969667,159.713114648779,159.791416870546,159.869802327121,159.927571216011,
160.013020842873,160.098346443543,160.183465540732,160.22122533308),
 .UNSPECIFIED.);
#3308=B_SPLINE_CURVE_WITH_KNOTS('',3,(#44984,#44985,#44986,#44987,#44988,
#44989,#44990,#44991,#44992,#44993,#44994,#44995,#44996,#44997,#44998,#44999,
#45000,#45001,#45002,#45003,#45004,#45005,#45006,#45007,#45008,#45009,#45010,
#45011,#45012,#45013,#45014,#45015,#45016,#45017,#45018,#45019,#45020,#45021,
#45022,#45023,#45024,#45025,#45026,#45027,#45028,#45029,#45030,#45031,#45032,
#45033,#45034,#45035,#45036,#45037,#45038,#45039,#45040,#45041,#45042,#45043,
#45044,#45045,#45046,#45047,#45048,#45049,#45050,#45051,#45052,#45053,#45054,
#45055,#45056,#45057,#45058,#45059,#45060,#45061,#45062,#45063,#45064,#45065),
 .UNSPECIFIED.,.F.,.F.,(4,3,3,3,3,3,3,3,3,3,3,3,3,3,3,3,3,3,3,3,3,3,3,3,
3,3,3,4),(158.174202348312,158.253762902578,158.333314767077,158.412806502528,
158.492250361244,158.571658558149,158.651043279688,158.730429315673,158.80981809696,
158.889220695576,158.968648191208,159.048146914347,159.127684059743,159.207309593207,
159.251305283903,159.328972764127,159.406554219196,159.484063570133,159.561504441257,
159.638905636556,159.716280948523,159.750076474566,159.832460025215,159.914969935679,
159.997681173828,160.080494964793,160.163479563051,160.22122533308),
 .UNSPECIFIED.);
#3309=B_SPLINE_CURVE_WITH_KNOTS('',3,(#45066,#45067,#45068,#45069,#45070,
#45071,#45072,#45073,#45074,#45075,#45076,#45077,#45078,#45079,#45080,#45081,
#45082,#45083,#45084,#45085,#45086,#45087,#45088,#45089,#45090,#45091,#45092,
#45093,#45094,#45095,#45096,#45097,#45098,#45099,#45100,#45101,#45102,#45103,
#45104,#45105,#45106,#45107,#45108,#45109,#45110,#45111,#45112,#45113,#45114,
#45115,#45116,#45117,#45118,#45119,#45120,#45121,#45122,#45123,#45124,#45125,
#45126,#45127,#45128,#45129,#45130,#45131,#45132,#45133,#45134,#45135,#45136,
#45137,#45138,#45139,#45140,#45141,#45142,#45143,#45144,#45145,#45146,#45147,
#45148,#45149,#45150,#45151,#45152,#45153,#45154,#45155,#45156,#45157,#45158,
#45159,#45160,#45161,#45162,#45163,#45164,#45165,#45166,#45167,#45168,#45169,
#45170,#45171,#45172,#45173,#45174,#45175,#45176,#45177,#45178,#45179,#45180,
#45181,#45182,#45183,#45184,#45185,#45186,#45187,#45188,#45189,#45190,#45191,
#45192,#45193,#45194,#45195,#45196,#45197,#45198,#45199,#45200,#45201,#45202,
#45203,#45204,#45205,#45206,#45207,#45208,#45209,#45210,#45211,#45212,#45213,
#45214,#45215,#45216,#45217,#45218,#45219,#45220,#45221,#45222,#45223,#45224,
#45225,#45226,#45227,#45228,#45229,#45230,#45231,#45232,#45233,#45234),
 .UNSPECIFIED.,.F.,.F.,(4,3,3,3,3,3,3,3,3,3,3,3,3,3,3,3,3,3,3,3,3,3,3,3,
3,3,3,3,3,3,3,3,3,3,3,3,3,3,3,3,3,3,3,3,3,3,3,3,3,3,3,3,3,3,3,3,4),(160.221225333172,
160.248847665228,160.326356798069,160.403784073745,160.481145108966,160.55845547296,
160.635730698142,160.712999202259,160.790266936873,160.86754793823,160.944856247399,
161.022252359485,161.099694120844,161.177255308583,161.246390046553,161.32245620601,
161.398427707044,161.474321326841,161.550153763129,161.625941652713,161.703190499609,
161.77895429826,161.854726204324,161.930521221795,162.008874023316,162.084802562018,
162.164367494948,162.243932427878,162.322477044816,162.400929086987,162.479303047569,
162.557613364408,162.635874429781,162.714103723048,162.792316519793,162.87052580592,
162.948744562858,163.02701824197,163.105320463736,163.183705920312,163.241474809203,
163.321123829469,163.40070272114,163.480222363847,163.559685275352,163.639114126177,
163.71851852566,163.740245999865,163.821478052954,163.902758771292,163.986823376101,
164.068255510957,164.153636350743,164.239017190528,164.324255888769,164.409394694648,
164.4584365467),.UNSPECIFIED.);
#3310=B_SPLINE_CURVE_WITH_KNOTS('',3,(#45240,#45241,#45242,#45243,#45244,
#45245,#45246,#45247,#45248,#45249,#45250,#45251,#45252,#45253,#45254,#45255,
#45256,#45257,#45258,#45259,#45260,#45261,#45262,#45263,#45264,#45265,#45266,
#45267,#45268,#45269,#45270,#45271,#45272,#45273,#45274,#45275,#45276,#45277,
#45278,#45279,#45280,#45281,#45282,#45283,#45284,#45285,#45286,#45287,#45288,
#45289,#45290,#45291,#45292,#45293,#45294,#45295,#45296,#45297,#45298,#45299,
#45300,#45301,#45302,#45303,#45304,#45305,#45306,#45307,#45308,#45309,#45310,
#45311,#45312,#45313,#45314,#45315,#45316,#45317,#45318,#45319,#45320,#45321,
#45322,#45323,#45324,#45325,#45326,#45327,#45328,#45329,#45330,#45331,#45332,
#45333,#45334,#45335,#45336,#45337,#45338,#45339,#45340,#45341,#45342,#45343,
#45344,#45345,#45346,#45347,#45348,#45349,#45350,#45351,#45352,#45353,#45354,
#45355,#45356,#45357,#45358,#45359,#45360,#45361,#45362,#45363,#45364,#45365,
#45366,#45367,#45368,#45369,#45370,#45371,#45372,#45373,#45374,#45375,#45376,
#45377,#45378,#45379,#45380,#45381,#45382,#45383,#45384,#45385,#45386,#45387,
#45388,#45389,#45390,#45391,#45392,#45393,#45394,#45395,#45396,#45397,#45398,
#45399,#45400,#45401,#45402,#45403,#45404,#45405),.UNSPECIFIED.,.F.,.F.,
(4,3,3,3,3,3,3,3,3,3,3,3,3,3,3,3,3,3,3,3,3,3,3,3,3,3,3,3,3,3,3,3,3,3,3,
3,3,3,3,3,3,3,3,3,3,3,3,3,3,3,3,3,3,3,3,4),(166.504410640395,166.587946906,
166.671715849388,166.755597078121,166.839656736721,166.910367885285,166.990016905551,
167.069595797223,167.14911543993,167.228578351436,167.308007202261,167.387411601744,
167.409139075947,167.490371129036,167.571651847375,167.655716452183,167.737148587039,
167.822529426825,167.90791026661,167.99314319008,168.078298151307,168.16330308803,
168.248201380123,168.33290792645,168.406681457272,168.483240421959,168.559793988838,
168.636356754416,168.712975286884,168.789625055379,168.866358168868,168.905452647935,
168.985004512434,169.064496247885,169.143940106601,169.223348303507,169.302733025045,
169.38211906103,169.461507842317,169.540910440934,169.620337936565,169.699836659705,
169.779373805101,169.858999338565,169.90299502926,169.980662509484,170.058243964553,
170.13575331549,170.213194186614,170.290595381913,170.367970693879,170.401766219922,
170.486484918568,170.570161549865,170.655401282185,170.740641014505),
 .UNSPECIFIED.);
#3311=B_SPLINE_CURVE_WITH_KNOTS('',3,(#45406,#45407,#45408,#45409,#45410,
#45411,#45412,#45413,#45414,#45415,#45416,#45417,#45418,#45419,#45420,#45421,
#45422,#45423,#45424,#45425,#45426,#45427,#45428,#45429,#45430,#45431,#45432,
#45433,#45434,#45435,#45436,#45437,#45438,#45439,#45440,#45441,#45442,#45443,
#45444,#45445,#45446,#45447,#45448,#45449,#45450,#45451,#45452,#45453,#45454,
#45455,#45456,#45457,#45458,#45459,#45460,#45461,#45462,#45463,#45464,#45465,
#45466,#45467,#45468,#45469,#45470,#45471,#45472,#45473,#45474,#45475,#45476,
#45477,#45478,#45479,#45480,#45481,#45482,#45483,#45484,#45485,#45486,#45487),
 .UNSPECIFIED.,.F.,.F.,(4,3,3,3,3,3,3,3,3,3,3,3,3,3,3,3,3,3,3,3,3,3,3,3,
3,3,3,4),(164.457861495641,164.535142158086,164.612449892308,164.689845345729,
164.767286236049,164.844846929011,164.915283122635,164.991349282092,165.067320783126,
165.143214402924,165.219046839211,165.294834728795,165.372083575691,165.447847374342,
165.523619280406,165.599414297878,165.677767099398,165.7536956381,165.83326057103,
165.91282550396,165.994134477169,166.075331973723,166.15642500465,166.237420520553,
166.318294474902,166.399094121635,166.479805234646,166.50441064026),
 .UNSPECIFIED.);
#3312=B_SPLINE_CURVE_WITH_KNOTS('',3,(#45489,#45490,#45491,#45492,#45493,
#45494,#45495,#45496,#45497,#45498,#45499,#45500,#45501,#45502,#45503,#45504,
#45505,#45506,#45507,#45508,#45509,#45510,#45511,#45512,#45513,#45514,#45515,
#45516,#45517,#45518,#45519,#45520,#45521,#45522,#45523,#45524,#45525,#45526,
#45527,#45528,#45529,#45530,#45531,#45532,#45533,#45534,#45535,#45536,#45537,
#45538,#45539,#45540,#45541,#45542,#45543,#45544,#45545,#45546,#45547,#45548,
#45549,#45550,#45551,#45552,#45553,#45554,#45555,#45556,#45557,#45558,#45559,
#45560,#45561,#45562,#45563,#45564,#45565,#45566,#45567,#45568,#45569,#45570,
#45571,#45572,#45573),.UNSPECIFIED.,.F.,.F.,(4,3,3,3,3,3,3,3,3,3,3,3,3,
3,3,3,3,3,3,3,3,3,3,3,3,3,3,3,4),(164.4584365467,164.543381424743,164.62821289491,
164.712864999446,164.73778838119,164.814347345877,164.890900912755,164.967463678333,
165.0440822108,165.120731979295,165.197465092784,165.236559571853,165.316111436352,
165.395603171803,165.475047030519,165.554455227425,165.633839948965,165.71322598495,
165.792614766236,165.872017364853,165.951444860484,166.030943583623,166.110480729019,
166.190106262483,166.234101953177,166.320020536337,166.405719948851,166.491090206055,
166.50441064026),.UNSPECIFIED.);
#3313=B_SPLINE_CURVE_WITH_KNOTS('',3,(#45574,#45575,#45576,#45577,#45578,
#45579,#45580,#45581,#45582,#45583,#45584,#45585,#45586,#45587,#45588,#45589,
#45590,#45591,#45592,#45593,#45594,#45595,#45596,#45597,#45598,#45599,#45600,
#45601,#45602,#45603,#45604,#45605,#45606,#45607,#45608,#45609,#45610,#45611,
#45612,#45613,#45614,#45615,#45616,#45617,#45618,#45619,#45620,#45621,#45622,
#45623,#45624,#45625,#45626,#45627,#45628,#45629,#45630,#45631,#45632,#45633,
#45634,#45635,#45636,#45637,#45638,#45639,#45640,#45641,#45642,#45643,#45644,
#45645,#45646,#45647,#45648,#45649,#45650,#45651,#45652,#45653,#45654,#45655,
#45656,#45657,#45658,#45659,#45660,#45661,#45662,#45663,#45664,#45665,#45666,
#45667,#45668,#45669,#45670,#45671,#45672,#45673,#45674,#45675,#45676,#45677,
#45678,#45679,#45680,#45681,#45682,#45683,#45684,#45685,#45686,#45687,#45688,
#45689,#45690,#45691,#45692,#45693,#45694,#45695,#45696,#45697,#45698,#45699,
#45700,#45701,#45702,#45703,#45704,#45705,#45706,#45707,#45708,#45709,#45710,
#45711,#45712,#45713,#45714,#45715,#45716,#45717,#45718,#45719,#45720,#45721,
#45722,#45723,#45724,#45725,#45726,#45727,#45728,#45729,#45730),
 .UNSPECIFIED.,.F.,.F.,(4,3,3,3,3,3,3,3,3,3,3,3,3,3,3,3,3,3,3,3,3,3,3,3,
3,3,3,3,3,3,3,3,3,3,3,3,3,3,3,3,3,3,3,3,3,3,3,3,3,3,3,3,4),(166.50441064026,
166.58687284636,166.669334704163,166.751796220518,166.834257402276,166.916718256286,
166.999178789398,167.081639008461,167.164098920324,167.246558531836,167.329017849845,
167.411476881198,167.493935632745,167.576394111333,167.658852323808,167.741310277019,
167.823767977812,167.906225433034,167.988682649532,168.074695344818,168.158020143376,
168.240486748968,168.322952510351,168.405417454941,168.487881610149,168.570345003385,
168.652807662057,168.735269613568,168.817730885321,168.900191504714,168.982651499145,
169.065110896009,169.147569722699,169.230028006606,169.312485775119,169.394943055626,
169.479077170817,169.561543169177,169.644007545783,169.726470410278,169.808931872285,
169.891392041404,169.97385102722,170.0563089393,170.141906434223,170.224371171269,
170.306832943655,170.38929218982,170.471749348059,170.554211867142,170.636669538553,
170.719128329746,170.741088898683),.UNSPECIFIED.);
#3314=B_SPLINE_CURVE_WITH_KNOTS('',3,(#45736,#45737,#45738,#45739,#45740,
#45741,#45742,#45743,#45744,#45745,#45746,#45747,#45748,#45749,#45750,#45751,
#45752,#45753,#45754,#45755,#45756,#45757,#45758,#45759,#45760,#45761,#45762,
#45763,#45764,#45765,#45766,#45767,#45768,#45769,#45770,#45771,#45772,#45773,
#45774,#45775,#45776,#45777,#45778,#45779,#45780,#45781,#45782,#45783,#45784,
#45785,#45786,#45787,#45788,#45789,#45790,#45791,#45792,#45793,#45794,#45795,
#45796,#45797,#45798,#45799,#45800,#45801,#45802,#45803,#45804,#45805,#45806,
#45807,#45808,#45809,#45810,#45811,#45812,#45813,#45814,#45815,#45816,#45817,
#45818,#45819,#45820,#45821,#45822,#45823,#45824,#45825,#45826,#45827,#45828,
#45829,#45830,#45831,#45832,#45833,#45834,#45835,#45836,#45837,#45838,#45839,
#45840,#45841,#45842,#45843,#45844,#45845,#45846,#45847,#45848,#45849,#45850,
#45851,#45852,#45853,#45854,#45855,#45856,#45857,#45858,#45859,#45860,#45861,
#45862,#45863,#45864,#45865,#45866,#45867,#45868,#45869,#45870,#45871,#45872,
#45873,#45874,#45875,#45876,#45877,#45878,#45879,#45880,#45881,#45882,#45883,
#45884,#45885,#45886,#45887,#45888,#45889,#45890,#45891,#45892,#45893,#45894,
#45895,#45896,#45897,#45898,#45899,#45900,#45901),.UNSPECIFIED.,.F.,.F.,
(4,3,3,3,3,3,3,3,3,3,3,3,3,3,3,3,3,3,3,3,3,3,3,3,3,3,3,3,3,3,3,3,3,3,3,
3,3,3,3,3,3,3,3,3,3,3,3,3,3,3,3,3,3,3,3,4),(172.787595947439,172.895622173234,
172.974166790173,173.052618832344,173.130992792926,173.209303109765,173.287564175138,
173.365793468405,173.44400626515,173.522215551277,173.600434308216,173.678707987328,
173.757010209094,173.83539566567,173.893164554559,173.972813574825,174.052392466497,
174.131912109204,174.21137502071,174.290803871535,174.370208271018,174.391935745222,
174.473167798311,174.554448516648,174.638513121457,174.719945256312,174.805326096098,
174.890706935884,174.975939859356,175.061094820585,175.14609975731,175.230998049405,
175.315704595733,175.389478126546,175.466037091231,175.542590658109,175.619153423685,
175.695771956151,175.772421724644,175.849154838132,175.888249317209,175.967801181708,
176.04729291716,176.126736775876,176.206144972782,176.285529694321,176.364915730306,
176.444304511593,176.52370711021,176.603134605842,176.682633328982,176.762170474378,
176.841796007843,176.885791698534,176.963453310415,177.024993203619),
 .UNSPECIFIED.);
#3315=B_SPLINE_CURVE_WITH_KNOTS('',3,(#45902,#45903,#45904,#45905,#45906,
#45907,#45908,#45909,#45910,#45911,#45912,#45913,#45914,#45915,#45916,#45917,
#45918,#45919,#45920,#45921,#45922,#45923,#45924,#45925,#45926,#45927,#45928,
#45929,#45930,#45931,#45932,#45933,#45934,#45935,#45936,#45937,#45938,#45939,
#45940,#45941,#45942,#45943,#45944,#45945,#45946,#45947,#45948,#45949,#45950,
#45951,#45952,#45953,#45954,#45955,#45956,#45957,#45958,#45959,#45960,#45961,
#45962,#45963,#45964,#45965,#45966,#45967,#45968,#45969,#45970,#45971,#45972,
#45973,#45974,#45975,#45976,#45977,#45978,#45979,#45980,#45981,#45982,#45983),
 .UNSPECIFIED.,.F.,.F.,(4,3,3,3,3,3,3,3,3,3,3,3,3,3,3,3,3,3,3,3,3,3,3,3,
3,3,3,4),(170.740641014505,170.824827998365,170.900537410584,170.978046543425,
171.055473819101,171.132834854323,171.210145218316,171.287420443499,171.364688947616,
171.44195668223,171.519237683587,171.596545992756,171.673942104842,171.7513838662,
171.828945053939,171.898079791909,171.973228297357,172.048283482188,172.123262586557,
172.198182736578,172.273064321956,172.347925999265,172.422783121255,172.49765103696,
172.572584895655,172.647552314513,172.72262266121,172.787595947362),
 .UNSPECIFIED.);
#3316=B_SPLINE_CURVE_WITH_KNOTS('',3,(#45985,#45986,#45987,#45988,#45989,
#45990,#45991,#45992,#45993,#45994,#45995,#45996,#45997,#45998,#45999,#46000,
#46001,#46002,#46003,#46004,#46005,#46006,#46007,#46008,#46009,#46010,#46011,
#46012,#46013,#46014,#46015,#46016,#46017,#46018,#46019,#46020,#46021,#46022,
#46023,#46024,#46025,#46026,#46027,#46028,#46029,#46030,#46031,#46032,#46033,
#46034,#46035,#46036,#46037,#46038,#46039,#46040,#46041,#46042,#46043,#46044,
#46045,#46046,#46047,#46048,#46049,#46050,#46051,#46052,#46053,#46054,#46055,
#46056,#46057,#46058,#46059,#46060),.UNSPECIFIED.,.F.,.F.,(4,3,3,3,3,3,
3,3,3,3,3,3,3,3,3,3,3,3,3,3,3,3,3,3,3,4),(170.741088898683,170.823550502413,
170.906011440265,170.988471739637,171.070931427926,171.153390532524,171.235849080824,
171.318307100217,171.40076461809,171.487441576174,171.569908361715,171.652373474783,
171.734837025031,171.81729912209,171.899759875572,171.982219395068,172.064677790153,
172.147135170387,172.229601556073,172.312064757581,172.394525213431,172.476983361985,
172.559448965739,172.641908844127,172.724372955379,172.787595947439),
 .UNSPECIFIED.);
#3317=B_SPLINE_CURVE_WITH_KNOTS('',3,(#46061,#46062,#46063,#46064,#46065,
#46066,#46067,#46068,#46069,#46070,#46071,#46072,#46073,#46074,#46075,#46076,
#46077,#46078,#46079,#46080,#46081,#46082,#46083,#46084,#46085,#46086,#46087,
#46088,#46089,#46090,#46091,#46092,#46093,#46094,#46095,#46096,#46097,#46098,
#46099,#46100,#46101,#46102,#46103,#46104,#46105,#46106,#46107,#46108,#46109,
#46110,#46111,#46112,#46113,#46114,#46115,#46116,#46117,#46118,#46119,#46120,
#46121,#46122,#46123,#46124,#46125,#46126,#46127,#46128,#46129,#46130,#46131,
#46132,#46133,#46134,#46135,#46136,#46137,#46138,#46139,#46140,#46141,#46142,
#46143,#46144,#46145,#46146,#46147,#46148,#46149,#46150,#46151,#46152,#46153,
#46154,#46155,#46156,#46157,#46158,#46159,#46160,#46161,#46162,#46163,#46164,
#46165,#46166,#46167,#46168,#46169,#46170,#46171,#46172,#46173,#46174,#46175,
#46176,#46177,#46178,#46179,#46180,#46181,#46182,#46183,#46184,#46185,#46186,
#46187,#46188,#46189,#46190,#46191,#46192,#46193,#46194,#46195,#46196,#46197,
#46198,#46199,#46200,#46201,#46202,#46203,#46204,#46205,#46206,#46207,#46208,
#46209,#46210,#46211,#46212,#46213,#46214,#46215,#46216,#46217,#46218,#46219,
#46220,#46221,#46222,#46223,#46224,#46225,#46226),.UNSPECIFIED.,.F.,.F.,
(4,3,3,3,3,3,3,3,3,3,3,3,3,3,3,3,3,3,3,3,3,3,3,3,3,3,3,3,3,3,3,3,3,3,3,
3,3,3,3,3,3,3,3,3,3,3,3,3,3,3,3,3,3,3,3,4),(172.787595947439,172.874185025021,
172.961173772969,173.048340074132,173.135733550733,173.216898622452,173.294566102676,
173.372147557746,173.449656908683,173.527097779807,173.604498975107,173.681874287074,
173.715669813114,173.799161258773,173.882808903518,173.966694126382,174.050692904784,
174.134877160692,174.214441003777,174.291950136618,174.369377412294,174.446738447516,
174.524048811509,174.601324036692,174.678592540809,174.755860275423,174.833141276779,
174.910449585949,174.987845698034,175.065287459393,175.142848647132,175.211983385101,
175.288049544558,175.364021045592,175.439914665389,175.515747101676,175.59153499126,
175.668783838156,175.744547636807,175.820319542871,175.896114560342,175.974467361863,
176.050395900565,176.129960833495,176.209525766426,176.288081254305,176.366542327576,
176.448727218835,176.52702763694,176.605283604676,176.683508141454,176.761714245822,
176.839929050713,176.91814867986,176.996404746631,177.024021457654),
 .UNSPECIFIED.);
#3318=B_SPLINE_CURVE_WITH_KNOTS('',3,(#46232,#46233,#46234,#46235,#46236,
#46237,#46238,#46239,#46240,#46241,#46242,#46243,#46244,#46245,#46246,#46247,
#46248,#46249,#46250,#46251,#46252,#46253,#46254,#46255,#46256,#46257,#46258,
#46259,#46260,#46261,#46262,#46263,#46264,#46265,#46266,#46267,#46268,#46269,
#46270,#46271,#46272,#46273,#46274,#46275,#46276,#46277,#46278,#46279,#46280,
#46281,#46282,#46283,#46284,#46285,#46286,#46287,#46288,#46289,#46290,#46291,
#46292,#46293,#46294,#46295,#46296,#46297,#46298,#46299,#46300,#46301,#46302,
#46303,#46304,#46305,#46306,#46307,#46308,#46309,#46310,#46311,#46312,#46313,
#46314,#46315,#46316,#46317,#46318,#46319,#46320,#46321,#46322,#46323,#46324,
#46325,#46326,#46327,#46328,#46329,#46330,#46331,#46332,#46333,#46334,#46335,
#46336,#46337,#46338,#46339,#46340,#46341,#46342,#46343,#46344,#46345,#46346,
#46347,#46348,#46349,#46350,#46351,#46352,#46353,#46354,#46355,#46356,#46357,
#46358,#46359,#46360,#46361,#46362,#46363,#46364,#46365,#46366,#46367,#46368,
#46369,#46370,#46371,#46372,#46373,#46374,#46375,#46376,#46377,#46378,#46379,
#46380,#46381,#46382,#46383,#46384,#46385,#46386,#46387,#46388,#46389,#46390,
#46391,#46392,#46393,#46394,#46395,#46396,#46397,#46398,#46399,#46400),
 .UNSPECIFIED.,.F.,.F.,(4,3,3,3,3,3,3,3,3,3,3,3,3,3,3,3,3,3,3,3,3,3,3,3,
3,3,3,3,3,3,3,3,3,3,3,3,3,3,3,3,3,3,3,3,3,3,3,3,3,3,3,3,3,3,3,3,4),(179.070781254718,
179.145516621503,179.220188243222,179.294813277258,179.369418651496,179.444015720104,
179.518619908358,179.593246653133,179.667957077619,179.7427113662,179.817583406695,
179.878418842509,179.956963459425,180.035415501573,180.113789462133,180.192099778949,
180.2703608443,180.348590137545,180.426802934267,180.505012220373,180.583230977289,
180.66150465638,180.739806878126,180.818192334681,180.875961223833,180.955610244282,
181.035189136134,181.114708779021,181.194171690702,181.273600541701,181.353004941354,
181.374732414496,181.455964467135,181.537245185018,181.621309790053,181.702741924448,
181.788122764803,181.873503605158,181.958736529484,182.043891491562,182.128896429114,
182.213794722016,182.298501269109,182.372274795821,182.44883376006,182.525387326491,
182.601950091619,182.678568623636,182.75521839168,182.83195150472,182.871045986483,
182.95060181219,183.030098619949,183.109540080683,183.188948127209,183.268334831295,
183.307329714257),.UNSPECIFIED.);
#3319=B_SPLINE_CURVE_WITH_KNOTS('',3,(#46401,#46402,#46403,#46404,#46405,
#46406,#46407,#46408,#46409,#46410,#46411,#46412,#46413,#46414,#46415,#46416,
#46417,#46418,#46419,#46420,#46421,#46422,#46423,#46424,#46425,#46426,#46427,
#46428,#46429,#46430,#46431,#46432,#46433,#46434,#46435,#46436,#46437,#46438,
#46439,#46440,#46441,#46442,#46443,#46444,#46445,#46446,#46447,#46448,#46449,
#46450,#46451,#46452,#46453,#46454,#46455,#46456,#46457,#46458,#46459,#46460,
#46461,#46462,#46463,#46464,#46465,#46466,#46467,#46468,#46469,#46470,#46471,
#46472,#46473,#46474,#46475,#46476,#46477,#46478,#46479),.UNSPECIFIED.,
 .F.,.F.,(4,3,3,3,3,3,3,3,3,3,3,3,3,3,3,3,3,3,3,3,3,3,3,3,3,3,4),(177.024993203619,
177.102516334983,177.179966967019,177.257375356394,177.334755995492,177.384562889196,
177.468054334845,177.551701979579,177.635587202431,177.719585980822,177.803770236719,
177.883334079859,177.960843212706,178.038270488389,178.115631523618,178.192941887618,
178.270217112807,178.347485616931,178.424753351552,178.502034352915,178.579342662092,
178.656738774184,178.734180535549,178.811741723295,178.880876461184,178.991529382284,
179.070781254619),.UNSPECIFIED.);
#3320=B_SPLINE_CURVE_WITH_KNOTS('',3,(#46481,#46482,#46483,#46484,#46485,
#46486,#46487,#46488,#46489,#46490,#46491,#46492,#46493,#46494,#46495,#46496,
#46497,#46498,#46499,#46500,#46501,#46502,#46503,#46504,#46505,#46506,#46507,
#46508,#46509,#46510,#46511,#46512,#46513,#46514,#46515,#46516,#46517,#46518,
#46519,#46520,#46521,#46522,#46523,#46524,#46525,#46526,#46527,#46528,#46529,
#46530,#46531,#46532,#46533,#46534,#46535,#46536,#46537,#46538,#46539,#46540,
#46541,#46542,#46543,#46544,#46545,#46546,#46547,#46548,#46549,#46550,#46551,
#46552,#46553,#46554,#46555,#46556,#46557,#46558,#46559,#46560,#46561,#46562),
 .UNSPECIFIED.,.F.,.F.,(4,3,3,3,3,3,3,3,3,3,3,3,3,3,3,3,3,3,3,3,3,3,3,3,
3,3,3,4),(177.024021457654,177.102338427649,177.180732646031,177.207068147751,
177.286717168017,177.366296059689,177.445815702396,177.525278613901,177.604707464726,
177.684111864209,177.705839338414,177.787071391503,177.868352109841,177.95241671465,
178.033848849505,178.119229689291,178.204610529076,178.289843452548,178.374998413777,
178.460003350502,178.544901642596,178.629608188924,178.703381719739,178.777449137334,
178.851524089071,178.925599451328,178.999727625761,179.070177698457),
 .UNSPECIFIED.);
#3321=B_SPLINE_CURVE_WITH_KNOTS('',3,(#46563,#46564,#46565,#46566,#46567,
#46568,#46569,#46570,#46571,#46572,#46573,#46574,#46575,#46576,#46577,#46578,
#46579,#46580,#46581,#46582,#46583,#46584,#46585,#46586,#46587,#46588,#46589,
#46590,#46591,#46592,#46593,#46594,#46595,#46596,#46597,#46598,#46599,#46600,
#46601,#46602,#46603,#46604,#46605,#46606,#46607,#46608,#46609,#46610,#46611,
#46612,#46613,#46614,#46615,#46616,#46617,#46618,#46619,#46620,#46621,#46622,
#46623,#46624,#46625,#46626,#46627,#46628,#46629,#46630,#46631,#46632,#46633,
#46634,#46635,#46636,#46637,#46638,#46639,#46640,#46641,#46642,#46643,#46644,
#46645,#46646,#46647,#46648,#46649,#46650,#46651,#46652,#46653,#46654,#46655,
#46656,#46657,#46658,#46659,#46660,#46661,#46662,#46663,#46664,#46665,#46666,
#46667,#46668,#46669,#46670,#46671,#46672,#46673,#46674,#46675,#46676,#46677,
#46678,#46679,#46680,#46681,#46682,#46683,#46684,#46685,#46686,#46687,#46688,
#46689,#46690,#46691,#46692,#46693,#46694,#46695,#46696,#46697,#46698,#46699,
#46700,#46701,#46702,#46703,#46704,#46705,#46706,#46707,#46708,#46709,#46710,
#46711,#46712,#46713,#46714,#46715,#46716,#46717,#46718,#46719),
 .UNSPECIFIED.,.F.,.F.,(4,3,3,3,3,3,3,3,3,3,3,3,3,3,3,3,3,3,3,3,3,3,3,3,
3,3,3,3,3,3,3,3,3,3,3,3,3,3,3,3,3,3,3,3,3,3,3,3,3,3,3,3,4),(179.070781254619,
179.153243460719,179.235705318522,179.318166834877,179.400628016635,179.483088870645,
179.565549403757,179.64800962282,179.730469534683,179.812929146195,179.895388464203,
179.977847495557,180.060306247104,180.142764725692,180.225222938167,180.307680891378,
180.390138592171,180.472596047393,180.55505326389,180.641065959176,180.724390757735,
180.806857363326,180.88932312471,180.971788069299,181.054252224508,181.136715617744,
181.219178276416,181.301640227927,181.384101499679,181.466562119072,181.549022113504,
181.631481510368,181.713940337058,181.796398620965,181.878856389478,181.961313669984,
182.045447785175,182.127913783535,182.210378160142,182.292841024637,182.375302486643,
182.457762655763,182.540221641579,182.622679553659,182.708277048582,182.790741785628,
182.873203558014,182.955662804179,183.038119962418,183.1205824815,183.203040152911,
183.285498944104,183.307459513042),.UNSPECIFIED.);
#3322=B_SPLINE_CURVE_WITH_KNOTS('',3,(#46725,#46726,#46727,#46728,#46729,
#46730,#46731,#46732,#46733,#46734,#46735,#46736,#46737,#46738,#46739,#46740,
#46741,#46742,#46743,#46744,#46745,#46746,#46747,#46748,#46749,#46750,#46751,
#46752,#46753,#46754,#46755,#46756,#46757,#46758,#46759,#46760,#46761,#46762,
#46763,#46764,#46765,#46766,#46767,#46768,#46769,#46770,#46771,#46772,#46773,
#46774,#46775,#46776,#46777,#46778,#46779,#46780,#46781,#46782,#46783,#46784,
#46785,#46786,#46787,#46788,#46789,#46790,#46791,#46792,#46793,#46794,#46795,
#46796,#46797,#46798,#46799,#46800,#46801,#46802,#46803,#46804,#46805,#46806,
#46807,#46808,#46809,#46810,#46811,#46812,#46813,#46814,#46815,#46816,#46817,
#46818,#46819,#46820,#46821,#46822,#46823,#46824,#46825,#46826,#46827,#46828,
#46829,#46830,#46831,#46832,#46833,#46834,#46835,#46836,#46837,#46838,#46839,
#46840,#46841,#46842,#46843,#46844,#46845,#46846,#46847,#46848,#46849,#46850,
#46851,#46852,#46853,#46854,#46855,#46856,#46857,#46858,#46859,#46860,#46861,
#46862,#46863,#46864,#46865,#46866,#46867,#46868,#46869,#46870,#46871,#46872,
#46873,#46874,#46875,#46876,#46877,#46878,#46879,#46880,#46881,#46882,#46883,
#46884,#46885,#46886,#46887,#46888,#46889,#46890),.UNSPECIFIED.,.F.,.F.,
(4,3,3,3,3,3,3,3,3,3,3,3,3,3,3,3,3,3,3,3,3,3,3,3,3,3,3,3,3,3,3,3,3,3,3,
3,3,3,3,3,3,3,3,3,3,3,3,3,3,3,3,3,3,3,3,4),(185.353966561872,185.436388795968,
185.518962685979,185.605140297099,185.688092821579,185.771168370801,185.854416769343,
185.863673130458,185.939739291683,186.015710794493,186.091604416073,186.16743685415,
186.24322474553,186.320473591312,186.396237391765,186.472009299633,186.547804318909,
186.626157117128,186.702085657623,186.781650584703,186.861215511783,186.939760116234,
187.018212145929,187.096586094066,187.174896398507,187.253157451547,187.331386732632,
187.409599517296,187.487808791459,187.566027536567,187.644301204122,187.722603414474,
187.800988859965,187.858757893108,187.938406980073,188.017985937837,188.097505645893,
188.17696862134,188.256397535211,188.3358019962,188.35752908377,188.438761019251,
188.520041618791,188.604106282702,188.685538298093,188.770919286263,188.856300274433,
188.941533289162,189.026688340278,189.111693363037,189.196591738378,189.281298362221,
189.355071465095,189.431629262761,189.510976499295,189.590323735828),
 .UNSPECIFIED.);
#3323=B_SPLINE_CURVE_WITH_KNOTS('',3,(#46891,#46892,#46893,#46894,#46895,
#46896,#46897,#46898,#46899,#46900,#46901,#46902,#46903,#46904,#46905,#46906,
#46907,#46908,#46909,#46910,#46911,#46912,#46913,#46914,#46915,#46916,#46917,
#46918,#46919,#46920,#46921,#46922,#46923,#46924,#46925,#46926,#46927,#46928,
#46929,#46930,#46931,#46932,#46933,#46934,#46935,#46936,#46937,#46938,#46939,
#46940,#46941,#46942,#46943,#46944,#46945,#46946,#46947,#46948,#46949,#46950,
#46951,#46952,#46953,#46954,#46955,#46956,#46957,#46958,#46959,#46960,#46961,
#46962,#46963,#46964,#46965,#46966,#46967,#46968,#46969),.UNSPECIFIED.,
 .F.,.F.,(4,3,3,3,3,3,3,3,3,3,3,3,3,3,3,3,3,3,3,3,3,3,3,3,3,3,4),(183.307329714257,
183.386715715262,183.466109900837,183.545523345885,183.626289601365,183.705806557614,
183.787197462711,183.868588367808,183.946255851014,184.023837309042,184.101346662911,
184.178787536922,184.256188735078,184.333564049854,184.367359558471,184.450850997495,
184.534498635367,184.618383851108,184.702382622282,184.786566870907,184.866130749133,
184.945985690768,185.025732308557,185.107790871867,185.187323979618,185.270645270708,
185.353966561798),.UNSPECIFIED.);
#3324=B_SPLINE_CURVE_WITH_KNOTS('',3,(#46971,#46972,#46973,#46974,#46975,
#46976,#46977,#46978,#46979,#46980,#46981,#46982,#46983,#46984,#46985,#46986,
#46987,#46988,#46989,#46990,#46991,#46992,#46993,#46994,#46995,#46996,#46997,
#46998,#46999,#47000,#47001,#47002,#47003,#47004,#47005,#47006,#47007,#47008,
#47009,#47010,#47011,#47012,#47013,#47014,#47015,#47016,#47017,#47018,#47019,
#47020,#47021,#47022,#47023,#47024,#47025,#47026,#47027,#47028,#47029,#47030,
#47031,#47032,#47033,#47034,#47035,#47036,#47037,#47038,#47039,#47040,#47041,
#47042,#47043,#47044,#47045,#47046),.UNSPECIFIED.,.F.,.F.,(4,3,3,3,3,3,
3,3,3,3,3,3,3,3,3,3,3,3,3,3,3,3,3,3,3,4),(183.307459513042,183.389921116772,
183.472382054624,183.554842353996,183.637302042285,183.719761146883,183.802219695183,
183.884677714576,183.967135232449,184.053812190533,184.136278976074,184.218744089142,
184.30120763939,184.383669736449,184.466130489931,184.548590009427,184.631048404512,
184.713505784746,184.795972170432,184.87843537194,184.96089582779,185.043353976344,
185.125819580098,185.208279458486,185.290743569738,185.353966561798),
 .UNSPECIFIED.);
#3325=B_SPLINE_CURVE_WITH_KNOTS('',3,(#47047,#47048,#47049,#47050,#47051,
#47052,#47053,#47054,#47055,#47056,#47057,#47058,#47059,#47060,#47061,#47062,
#47063,#47064,#47065,#47066,#47067,#47068,#47069,#47070,#47071,#47072,#47073,
#47074,#47075,#47076,#47077,#47078,#47079,#47080,#47081,#47082,#47083,#47084,
#47085,#47086,#47087,#47088,#47089,#47090,#47091,#47092,#47093,#47094,#47095,
#47096,#47097,#47098,#47099,#47100,#47101,#47102,#47103,#47104,#47105,#47106,
#47107,#47108,#47109,#47110,#47111,#47112,#47113,#47114,#47115,#47116,#47117,
#47118,#47119,#47120,#47121,#47122,#47123,#47124,#47125,#47126,#47127,#47128,
#47129,#47130,#47131,#47132,#47133,#47134,#47135,#47136,#47137,#47138,#47139,
#47140,#47141,#47142,#47143,#47144,#47145,#47146,#47147,#47148,#47149,#47150,
#47151,#47152,#47153,#47154,#47155,#47156,#47157,#47158,#47159,#47160,#47161,
#47162,#47163,#47164,#47165,#47166,#47167,#47168,#47169,#47170,#47171,#47172,
#47173,#47174,#47175,#47176,#47177,#47178,#47179,#47180,#47181,#47182,#47183,
#47184,#47185,#47186,#47187,#47188,#47189,#47190,#47191,#47192,#47193,#47194,
#47195,#47196,#47197,#47198,#47199,#47200,#47201,#47202,#47203),
 .UNSPECIFIED.,.F.,.F.,(4,3,3,3,3,3,3,3,3,3,3,3,3,3,3,3,3,3,3,3,3,3,3,3,
3,3,3,3,3,3,3,3,3,3,3,3,3,3,3,3,3,3,3,3,3,3,3,3,3,3,3,3,4),(185.353966561918,
185.436428768018,185.518890625821,185.601352142176,185.683813323934,185.766274177944,
185.848734711056,185.931194930119,186.013654841982,186.096114453494,186.178573771503,
186.261032802857,186.343491554403,186.425950032991,186.508408245466,186.590866198677,
186.67332389947,186.755781354692,186.838238571189,186.924251266472,187.007576065026,
187.090042670618,187.172508432001,187.254973376591,187.337437531799,187.419900925036,
187.502363583708,187.584825535219,187.667286806971,187.749747426364,187.832207420795,
187.91466681766,187.99712564435,188.079583928257,188.16204169677,188.244498977276,
188.32863309246,188.41109909082,188.493563467426,188.576026331922,188.658487793928,
188.740947963047,188.823406948864,188.905864860944,188.991462355854,189.0739270929,
189.156388865286,189.238848111451,189.32130526969,189.403767788772,189.486225460183,
189.568684251376,189.590644820222),.UNSPECIFIED.);
#3326=B_SPLINE_CURVE_WITH_KNOTS('',3,(#47209,#47210,#47211,#47212,#47213,
#47214,#47215,#47216,#47217,#47218,#47219,#47220,#47221,#47222,#47223,#47224,
#47225,#47226,#47227,#47228,#47229,#47230,#47231,#47232,#47233,#47234,#47235,
#47236,#47237,#47238,#47239,#47240,#47241,#47242,#47243,#47244,#47245,#47246,
#47247,#47248,#47249,#47250,#47251,#47252,#47253,#47254,#47255,#47256,#47257,
#47258,#47259,#47260,#47261,#47262,#47263,#47264,#47265,#47266,#47267,#47268,
#47269,#47270,#47271,#47272,#47273,#47274,#47275,#47276,#47277,#47278,#47279,
#47280,#47281,#47282,#47283,#47284,#47285,#47286,#47287,#47288,#47289,#47290,
#47291,#47292,#47293,#47294,#47295,#47296,#47297,#47298,#47299,#47300,#47301,
#47302,#47303,#47304,#47305,#47306,#47307,#47308,#47309,#47310,#47311,#47312,
#47313,#47314,#47315,#47316,#47317,#47318,#47319,#47320,#47321,#47322,#47323,
#47324,#47325,#47326,#47327,#47328,#47329,#47330,#47331,#47332,#47333,#47334,
#47335,#47336,#47337,#47338,#47339,#47340,#47341,#47342,#47343,#47344,#47345,
#47346,#47347,#47348,#47349,#47350,#47351,#47352,#47353,#47354,#47355,#47356,
#47357,#47358,#47359,#47360,#47361,#47362,#47363,#47364,#47365,#47366,#47367,
#47368,#47369,#47370,#47371,#47372,#47373,#47374),.UNSPECIFIED.,.F.,.F.,
(4,3,3,3,3,3,3,3,3,3,3,3,3,3,3,3,3,3,3,3,3,3,3,3,3,3,3,3,3,3,3,3,3,3,3,
3,3,3,3,3,3,3,3,3,3,3,3,3,3,3,3,3,3,3,3,4),(191.637151868978,191.743039643692,
191.848927418407,191.92643671887,192.003864162199,192.081225364945,192.158535896175,
192.235811288146,192.31307995782,192.390347857223,192.467629022458,192.544937494451,
192.622333766832,192.699775687347,192.777337030803,192.846469799732,192.922537679677,
192.998510902649,193.074406244851,193.15024040308,193.226030013248,193.303277784224,
193.379043294017,193.454816906719,193.53061362553,193.608963264412,193.68489347934,
193.764452830198,193.844012181057,193.922552739501,194.001000738238,194.079370676038,
194.15767699636,194.235934097122,194.31415949021,194.392368429138,194.470573904931,
194.548788904164,194.627058928218,194.705357549035,194.783739523544,194.841554562382,
194.921213750279,195.000802647214,195.080332112034,195.159804529953,195.239242691842,
195.318656084451,195.340325753044,195.421563458961,195.502850079269,195.586911795378,
195.668350324312,195.75372363401,195.839096943707,195.873887289425),
 .UNSPECIFIED.);
#3327=B_SPLINE_CURVE_WITH_KNOTS('',3,(#47375,#47376,#47377,#47378,#47379,
#47380,#47381,#47382,#47383,#47384,#47385,#47386,#47387,#47388,#47389,#47390,
#47391,#47392,#47393,#47394,#47395,#47396,#47397,#47398,#47399,#47400,#47401,
#47402,#47403,#47404,#47405,#47406,#47407,#47408,#47409,#47410,#47411,#47412,
#47413,#47414,#47415,#47416,#47417,#47418,#47419,#47420,#47421,#47422,#47423,
#47424,#47425,#47426,#47427,#47428,#47429,#47430,#47431,#47432,#47433,#47434,
#47435,#47436,#47437,#47438,#47439,#47440,#47441,#47442,#47443,#47444,#47445,
#47446,#47447,#47448,#47449,#47450,#47451,#47452,#47453,#47454,#47455,#47456,
#47457,#47458,#47459),.UNSPECIFIED.,.F.,.F.,(4,3,3,3,3,3,3,3,3,3,3,3,3,
3,3,3,3,3,3,3,3,3,3,3,3,3,3,3,4),(189.590323735828,189.666944177838,189.743596810827,
189.820331710161,189.853842655757,189.933394206177,190.012885625034,190.092329165352,
190.171737042769,190.251121444441,190.330507161835,190.409895625754,190.489297908858,
190.568725091464,190.648223507518,190.727760349111,190.807385586633,190.851385037082,
190.929053808582,191.006636543012,191.084147160091,191.161589274167,191.238991698868,
191.316368216488,191.350156227745,191.427900202662,191.5056845015,191.583569631828,
191.637151868893),.UNSPECIFIED.);
#3328=B_SPLINE_CURVE_WITH_KNOTS('',3,(#47461,#47462,#47463,#47464,#47465,
#47466,#47467,#47468,#47469,#47470,#47471,#47472,#47473,#47474,#47475,#47476,
#47477,#47478,#47479,#47480,#47481,#47482,#47483,#47484,#47485,#47486,#47487,
#47488,#47489,#47490,#47491,#47492,#47493,#47494,#47495,#47496,#47497,#47498,
#47499,#47500,#47501,#47502,#47503,#47504,#47505,#47506,#47507,#47508,#47509,
#47510,#47511,#47512,#47513,#47514,#47515,#47516,#47517,#47518,#47519,#47520,
#47521,#47522,#47523,#47524,#47525,#47526,#47527,#47528,#47529,#47530,#47531,
#47532,#47533,#47534,#47535,#47536),.UNSPECIFIED.,.F.,.F.,(4,3,3,3,3,3,
3,3,3,3,3,3,3,3,3,3,3,3,3,3,3,3,3,3,3,4),(189.590644820222,189.673106423952,
189.755567361804,189.838027661176,189.920487349464,190.002946454063,190.085405002363,
190.167863021756,190.250320539629,190.336997497713,190.419464283254,190.501929396322,
190.58439294657,190.666855043629,190.749315797111,190.831775316607,190.914233711692,
190.996691091925,191.079157477611,191.161620679119,191.244081134969,191.326539283524,
191.409004887277,191.491464765665,191.573928876918,191.637151868978),
 .UNSPECIFIED.);
#3329=B_SPLINE_CURVE_WITH_KNOTS('',3,(#47537,#47538,#47539,#47540,#47541,
#47542,#47543,#47544,#47545,#47546,#47547,#47548,#47549,#47550,#47551,#47552,
#47553,#47554,#47555,#47556,#47557,#47558,#47559,#47560,#47561,#47562,#47563,
#47564,#47565,#47566,#47567,#47568,#47569,#47570,#47571,#47572,#47573,#47574,
#47575,#47576,#47577,#47578,#47579,#47580,#47581,#47582,#47583,#47584,#47585,
#47586,#47587,#47588,#47589,#47590,#47591,#47592,#47593,#47594,#47595,#47596,
#47597,#47598,#47599,#47600,#47601,#47602,#47603,#47604,#47605,#47606,#47607,
#47608,#47609,#47610,#47611,#47612,#47613,#47614,#47615,#47616,#47617,#47618,
#47619,#47620,#47621,#47622,#47623,#47624,#47625,#47626,#47627,#47628,#47629,
#47630,#47631,#47632,#47633,#47634,#47635,#47636,#47637,#47638,#47639,#47640,
#47641,#47642,#47643,#47644,#47645,#47646,#47647,#47648,#47649,#47650,#47651,
#47652,#47653,#47654,#47655,#47656,#47657,#47658,#47659,#47660,#47661,#47662,
#47663,#47664,#47665,#47666,#47667,#47668,#47669,#47670,#47671,#47672,#47673,
#47674,#47675,#47676,#47677,#47678,#47679,#47680,#47681,#47682,#47683,#47684,
#47685,#47686,#47687,#47688,#47689,#47690,#47691,#47692,#47693,#47694,#47695,
#47696,#47697,#47698,#47699,#47700,#47701,#47702,#47703,#47704,#47705),
 .UNSPECIFIED.,.F.,.F.,(4,3,3,3,3,3,3,3,3,3,3,3,3,3,3,3,3,3,3,3,3,3,3,3,
3,3,3,3,3,3,3,3,3,3,3,3,3,3,3,3,3,3,3,3,3,3,3,3,3,3,3,3,3,3,3,3,4),(191.637151868978,
191.671432676962,191.752664612443,191.833945211983,191.918009875893,191.999441891284,
192.084822879455,192.170203867625,192.255436882354,192.340591933471,192.425596956231,
192.510495331572,192.595201955416,192.668975058287,192.745534097889,192.822087740658,
192.898650583046,192.975269193464,193.051919040613,193.128652233458,193.16774624895,
193.24729779937,193.326789218227,193.406232758545,193.485640635962,193.565025037634,
193.644410755028,193.723799218947,193.803201502051,193.882628684658,193.962127100712,
194.041663942304,194.121289179826,194.165288630274,194.242957401773,194.320540136204,
194.398050753283,194.475492867358,194.55289529206,194.630271809679,194.664059820937,
194.747548890742,194.831194081817,194.915076772407,194.999072986065,195.083254667227,
195.162831011599,195.240355214955,195.319493794587,195.396848759866,195.47415661739,
195.551431439975,195.631939542984,195.709204239896,195.786475770957,195.863783539233,
195.873463852012),.UNSPECIFIED.);
#3330=B_SPLINE_CURVE_WITH_KNOTS('',3,(#47711,#47712,#47713,#47714,#47715,
#47716,#47717,#47718,#47719,#47720,#47721,#47722,#47723,#47724,#47725,#47726,
#47727,#47728,#47729,#47730,#47731,#47732,#47733,#47734,#47735,#47736,#47737,
#47738,#47739,#47740,#47741,#47742,#47743,#47744,#47745,#47746,#47747,#47748,
#47749,#47750,#47751,#47752,#47753,#47754,#47755,#47756,#47757,#47758,#47759,
#47760,#47761,#47762,#47763,#47764,#47765,#47766,#47767,#47768,#47769,#47770,
#47771,#47772,#47773,#47774,#47775,#47776,#47777,#47778,#47779,#47780,#47781,
#47782,#47783,#47784,#47785,#47786,#47787,#47788,#47789,#47790,#47791,#47792,
#47793,#47794,#47795,#47796,#47797,#47798,#47799,#47800,#47801,#47802,#47803,
#47804,#47805,#47806,#47807,#47808,#47809,#47810,#47811,#47812,#47813,#47814,
#47815,#47816,#47817,#47818,#47819,#47820,#47821,#47822,#47823,#47824,#47825,
#47826,#47827,#47828,#47829,#47830,#47831,#47832,#47833,#47834,#47835,#47836,
#47837,#47838,#47839,#47840,#47841,#47842,#47843,#47844,#47845,#47846,#47847,
#47848,#47849,#47850,#47851,#47852,#47853,#47854,#47855,#47856,#47857,#47858,
#47859,#47860,#47861,#47862,#47863,#47864,#47865,#47866,#47867,#47868,#47869,
#47870,#47871,#47872,#47873,#47874,#47875,#47876,#47877,#47878,#47879),
 .UNSPECIFIED.,.F.,.F.,(4,3,3,3,3,3,3,3,3,3,3,3,3,3,3,3,3,3,3,3,3,3,3,3,
3,3,3,3,3,3,3,3,3,3,3,3,3,3,3,3,3,3,3,3,3,3,3,3,3,3,3,3,3,3,3,3,4),(197.920337176296,
197.995786692891,198.071166512278,198.146485647516,198.221769556338,198.297038071666,
198.332952897019,198.416105006492,198.499405917416,198.582938677015,198.666583255601,
198.750416364689,198.831724087681,198.908963344172,198.986118992796,199.063206910824,
199.140242925539,199.217242825609,199.294235412097,199.371226878564,199.448231489223,
199.525263513282,199.602384967768,199.679552527019,199.75684291302,199.829266469006,
199.906142422896,199.982923501785,200.059625966089,200.136266013088,200.212859790473,
200.289603422955,200.366165741792,200.442732814096,200.519319204004,200.596191615586,
200.672896533004,200.749852691668,200.826808850331,200.904657929378,200.982422320009,
201.060117311562,201.137758144491,201.215360020605,201.292948237709,201.370531383653,
201.448123190583,201.52573739284,201.603430020003,201.681163571845,201.759005861736,
201.824351231656,201.901201730848,201.977941849885,202.054618325147,202.131235123842,
202.157407101182),.UNSPECIFIED.);
#3331=B_SPLINE_CURVE_WITH_KNOTS('',3,(#47880,#47881,#47882,#47883,#47884,
#47885,#47886,#47887,#47888,#47889,#47890,#47891,#47892,#47893,#47894,#47895,
#47896,#47897,#47898,#47899,#47900,#47901,#47902,#47903,#47904,#47905,#47906,
#47907,#47908,#47909,#47910,#47911,#47912,#47913,#47914,#47915,#47916,#47917,
#47918,#47919,#47920,#47921,#47922,#47923,#47924,#47925,#47926,#47927,#47928,
#47929,#47930,#47931,#47932,#47933,#47934,#47935,#47936,#47937,#47938,#47939,
#47940,#47941,#47942,#47943,#47944,#47945,#47946,#47947,#47948,#47949,#47950,
#47951,#47952,#47953,#47954,#47955,#47956,#47957,#47958,#47959,#47960,#47961),
 .UNSPECIFIED.,.F.,.F.,(4,3,3,3,3,3,3,3,3,3,3,3,3,3,3,3,3,3,3,3,3,3,3,3,
3,3,3,4),(195.873887289425,195.958993449409,196.044014597101,196.128882576401,
196.213641033484,196.298220101784,196.337868134369,196.414558774872,196.491244931537,
196.56794110509,196.644693851934,196.721478386049,196.79834647228,196.836639325032,
196.916055518261,196.995410541899,197.074716947158,197.153987247531,197.233233927819,
197.312482484322,197.391734311925,197.471000747633,197.550293136381,197.629659279841,
197.709065232079,197.788562924981,197.834181706357,197.920337176158),
 .UNSPECIFIED.);
#3332=B_SPLINE_CURVE_WITH_KNOTS('',3,(#47963,#47964,#47965,#47966,#47967,
#47968,#47969,#47970,#47971,#47972,#47973,#47974,#47975,#47976,#47977,#47978,
#47979,#47980,#47981,#47982,#47983,#47984,#47985,#47986,#47987,#47988,#47989,
#47990,#47991,#47992,#47993,#47994,#47995,#47996,#47997,#47998,#47999,#48000,
#48001,#48002,#48003,#48004,#48005,#48006,#48007,#48008,#48009,#48010,#48011,
#48012,#48013,#48014,#48015,#48016,#48017,#48018,#48019,#48020,#48021,#48022,
#48023,#48024,#48025,#48026,#48027,#48028,#48029,#48030,#48031,#48032,#48033,
#48034,#48035,#48036,#48037,#48038,#48039,#48040,#48041,#48042,#48043,#48044),
 .UNSPECIFIED.,.F.,.F.,(4,3,3,3,3,3,3,3,3,3,3,3,3,3,3,3,3,3,3,3,3,3,3,3,
3,3,3,4),(195.873463852012,195.950867781641,196.028319749536,196.105886963599,
196.160373392924,196.236441272869,196.312414495841,196.388309838043,196.464143996272,
196.53993360644,196.617181377416,196.692946887209,196.768720499911,196.844517218722,
196.922866857604,196.998797072532,197.07835642339,197.157915774249,197.23617105997,
197.314330723584,197.39238967049,197.470390009991,197.548345159058,197.626268506195,
197.704184682042,197.78209465691,197.860034597259,197.920337176157),
 .UNSPECIFIED.);
#3333=B_SPLINE_CURVE_WITH_KNOTS('',3,(#48045,#48046,#48047,#48048,#48049,
#48050,#48051,#48052,#48053,#48054,#48055,#48056,#48057,#48058,#48059,#48060,
#48061,#48062,#48063,#48064,#48065,#48066,#48067,#48068,#48069,#48070,#48071,
#48072,#48073,#48074,#48075,#48076,#48077,#48078,#48079,#48080,#48081,#48082,
#48083,#48084,#48085,#48086,#48087,#48088,#48089,#48090,#48091,#48092,#48093,
#48094,#48095,#48096,#48097,#48098,#48099,#48100,#48101,#48102,#48103,#48104,
#48105,#48106,#48107,#48108,#48109,#48110,#48111,#48112,#48113,#48114,#48115,
#48116,#48117,#48118,#48119,#48120,#48121,#48122,#48123,#48124,#48125,#48126,
#48127,#48128,#48129,#48130,#48131,#48132,#48133,#48134,#48135,#48136,#48137,
#48138,#48139,#48140,#48141,#48142,#48143,#48144,#48145,#48146,#48147,#48148,
#48149,#48150,#48151,#48152,#48153,#48154,#48155,#48156,#48157,#48158,#48159,
#48160,#48161,#48162,#48163,#48164,#48165,#48166,#48167,#48168,#48169,#48170,
#48171,#48172,#48173,#48174,#48175,#48176,#48177,#48178,#48179,#48180,#48181,
#48182,#48183,#48184,#48185,#48186,#48187,#48188,#48189,#48190,#48191,#48192,
#48193,#48194,#48195,#48196,#48197,#48198,#48199,#48200,#48201,#48202,#48203,
#48204,#48205,#48206,#48207,#48208,#48209,#48210,#48211,#48212,#48213),
 .UNSPECIFIED.,.F.,.F.,(4,3,3,3,3,3,3,3,3,3,3,3,3,3,3,3,3,3,3,3,3,3,3,3,
3,3,3,3,3,3,3,3,3,3,3,3,3,3,3,3,3,3,3,3,3,3,3,3,3,3,3,3,3,3,3,3,4),(197.920337176245,
198.017095852488,198.114911702306,198.155458155574,198.235117343471,198.314706240407,
198.394235705227,198.473708123146,198.553146285035,198.632559677644,198.654229346236,
198.735467052153,198.816753672461,198.90081538857,198.982253917504,199.067627227201,
199.153000536899,199.238136566563,199.323194478014,199.408104032074,199.49290859628,
199.57752545438,199.651771727561,199.728462368064,199.805148524729,199.881844698282,
199.958597445127,200.035381979242,200.112250065472,200.150542918224,200.229959111453,
200.309314135091,200.38862054035,200.467890840722,200.547137521011,200.626386077513,
200.705637905117,200.784904340824,200.864196729572,200.943562873032,201.02296882527,
201.102466518172,201.148085299549,201.226055183723,201.303935307852,201.381739272854,
201.459467884952,201.537152794248,201.614805015986,201.646856490211,201.730008599684,
201.813309510607,201.896842270206,201.980486848792,202.064319957879,202.145627680874,
202.157254934226),.UNSPECIFIED.);
#3334=B_SPLINE_CURVE_WITH_KNOTS('',3,(#48219,#48220,#48221,#48222,#48223,
#48224,#48225,#48226,#48227,#48228,#48229,#48230,#48231,#48232,#48233,#48234,
#48235,#48236,#48237,#48238,#48239,#48240,#48241,#48242,#48243,#48244,#48245,
#48246,#48247,#48248,#48249,#48250,#48251,#48252,#48253,#48254,#48255,#48256,
#48257,#48258,#48259,#48260,#48261,#48262,#48263,#48264,#48265,#48266,#48267,
#48268,#48269,#48270,#48271,#48272,#48273,#48274,#48275,#48276,#48277,#48278,
#48279,#48280,#48281,#48282,#48283,#48284,#48285,#48286,#48287,#48288,#48289,
#48290,#48291,#48292,#48293,#48294,#48295,#48296,#48297,#48298,#48299,#48300,
#48301,#48302,#48303,#48304,#48305,#48306,#48307,#48308,#48309,#48310,#48311,
#48312,#48313,#48314,#48315,#48316,#48317,#48318,#48319,#48320,#48321,#48322,
#48323,#48324,#48325,#48326,#48327,#48328,#48329,#48330,#48331,#48332,#48333,
#48334,#48335,#48336,#48337,#48338,#48339,#48340,#48341,#48342,#48343,#48344,
#48345,#48346,#48347,#48348,#48349,#48350,#48351,#48352,#48353,#48354,#48355,
#48356,#48357,#48358,#48359,#48360,#48361,#48362,#48363,#48364,#48365,#48366,
#48367,#48368,#48369,#48370,#48371,#48372,#48373,#48374,#48375,#48376,#48377,
#48378,#48379,#48380,#48381,#48382,#48383,#48384,#48385,#48386,#48387),
 .UNSPECIFIED.,.F.,.F.,(4,3,3,3,3,3,3,3,3,3,3,3,3,3,3,3,3,3,3,3,3,3,3,3,
3,3,3,3,3,3,3,3,3,3,3,3,3,3,3,3,3,3,3,3,3,3,3,3,3,3,3,3,3,3,3,3,4),(204.203522483337,
204.279096250864,204.318207184968,204.395864860296,204.473546509871,204.551265588754,
204.629078219832,204.706944446481,204.784921232184,204.816978375631,204.896476211081,
204.975898867201,205.055258947777,205.134569008754,205.213841567289,205.293095130547,
205.372339038655,205.451584627026,205.530843230627,205.610155979876,205.689497401063,
205.768913514027,205.814520756956,205.891386076715,205.968184122965,206.044929482336,
206.121637400688,206.198323397914,206.275012318157,206.313291947618,206.397871525398,
206.48259324056,206.567510644375,206.652513000439,206.737635319519,206.812063138281,
206.893626765733,206.975115123468,207.059044924837,207.140378225501,207.225606277222,
207.310834328943,207.390254575581,207.469693513538,207.549161881788,207.628703563694,
207.708287119169,207.787954456856,207.809605519605,207.888377344815,207.966692049295,
208.044957511354,208.12318676496,208.202335104042,208.280540557168,208.360160339228,
208.439780121288),.UNSPECIFIED.);
#3335=B_SPLINE_CURVE_WITH_KNOTS('',3,(#48388,#48389,#48390,#48391,#48392,
#48393,#48394,#48395,#48396,#48397,#48398,#48399,#48400,#48401,#48402,#48403,
#48404,#48405,#48406,#48407,#48408,#48409,#48410,#48411,#48412,#48413,#48414,
#48415,#48416,#48417,#48418,#48419,#48420,#48421,#48422,#48423,#48424,#48425,
#48426,#48427,#48428,#48429,#48430,#48431,#48432,#48433,#48434,#48435,#48436,
#48437,#48438,#48439,#48440,#48441,#48442,#48443,#48444,#48445,#48446,#48447,
#48448,#48449,#48450,#48451,#48452,#48453,#48454,#48455,#48456,#48457,#48458,
#48459,#48460,#48461,#48462,#48463,#48464,#48465,#48466,#48467,#48468,#48469),
 .UNSPECIFIED.,.F.,.F.,(4,3,3,3,3,3,3,3,3,3,3,3,3,3,3,3,3,3,3,3,3,3,3,3,
3,3,3,4),(202.157407101182,202.233976138733,202.310541728034,202.38710926321,
202.463693308331,202.54030843525,202.617014883942,202.693771249812,202.77064566072,
202.821893612981,202.899194427024,202.976401365088,203.053530343199,203.130597219573,
203.207617806501,203.284615533229,203.361602667683,203.438593474282,203.515602216988,
203.592685532518,203.669806798868,203.747037420885,203.819435994306,203.908020543679,
203.996275196705,204.084282235795,204.1718575171,204.203522483235),
 .UNSPECIFIED.);
#3336=B_SPLINE_CURVE_WITH_KNOTS('',3,(#48471,#48472,#48473,#48474,#48475,
#48476,#48477,#48478,#48479,#48480,#48481,#48482,#48483,#48484,#48485,#48486,
#48487,#48488,#48489,#48490,#48491,#48492,#48493,#48494,#48495,#48496,#48497,
#48498,#48499,#48500,#48501,#48502,#48503,#48504,#48505,#48506,#48507,#48508,
#48509,#48510,#48511,#48512,#48513,#48514,#48515,#48516,#48517,#48518,#48519,
#48520,#48521,#48522,#48523,#48524,#48525,#48526,#48527,#48528,#48529,#48530,
#48531,#48532,#48533,#48534,#48535,#48536,#48537,#48538,#48539,#48540,#48541,
#48542,#48543,#48544,#48545,#48546,#48547,#48548,#48549,#48550,#48551,#48552),
 .UNSPECIFIED.,.F.,.F.,(4,3,3,3,3,3,3,3,3,3,3,3,3,3,3,3,3,3,3,3,3,3,3,3,
3,3,3,4),(202.157254934226,202.234480594198,202.311625038834,202.388704137127,
202.46573370984,202.542729540775,202.619721047223,202.696713579503,202.773721402066,
202.850758785572,202.927886350971,203.005061952553,203.082356969342,203.143170062198,
203.220046016088,203.296827094977,203.373529559281,203.45016960628,203.526763383665,
203.603507016147,203.680069334984,203.756636407288,203.833222797196,203.910095208777,
203.986800126196,204.063756284859,204.140712443523,204.203522483337),
 .UNSPECIFIED.);
#3337=B_SPLINE_CURVE_WITH_KNOTS('',3,(#48553,#48554,#48555,#48556,#48557,
#48558,#48559,#48560,#48561,#48562,#48563,#48564,#48565,#48566,#48567,#48568,
#48569,#48570,#48571,#48572,#48573,#48574,#48575,#48576,#48577,#48578,#48579,
#48580,#48581,#48582,#48583,#48584,#48585,#48586,#48587,#48588,#48589,#48590,
#48591,#48592,#48593,#48594,#48595,#48596,#48597,#48598,#48599,#48600,#48601,
#48602,#48603,#48604,#48605,#48606,#48607,#48608,#48609,#48610,#48611,#48612,
#48613,#48614,#48615,#48616,#48617,#48618,#48619,#48620,#48621,#48622,#48623,
#48624,#48625,#48626,#48627,#48628,#48629,#48630,#48631,#48632,#48633,#48634,
#48635,#48636,#48637,#48638,#48639,#48640,#48641,#48642,#48643,#48644,#48645,
#48646,#48647,#48648,#48649,#48650,#48651,#48652,#48653,#48654,#48655,#48656,
#48657,#48658,#48659,#48660,#48661,#48662,#48663,#48664,#48665,#48666,#48667,
#48668,#48669,#48670,#48671,#48672,#48673,#48674,#48675,#48676,#48677,#48678,
#48679,#48680,#48681,#48682,#48683,#48684,#48685,#48686,#48687,#48688,#48689,
#48690,#48691,#48692,#48693,#48694,#48695,#48696,#48697,#48698,#48699,#48700,
#48701,#48702,#48703,#48704,#48705,#48706,#48707,#48708,#48709,#48710,#48711,
#48712,#48713,#48714,#48715,#48716,#48717,#48718),.UNSPECIFIED.,.F.,.F.,
(4,3,3,3,3,3,3,3,3,3,3,3,3,3,3,3,3,3,3,3,3,3,3,3,3,3,3,3,3,3,3,3,3,3,3,
3,3,3,3,3,3,3,3,3,3,3,3,3,3,3,3,3,3,3,3,4),(204.203522483439,204.280638712373,
204.357672734015,204.434640552169,204.511558120638,204.589895208664,204.66677088276,
204.74364729744,204.820538833263,204.899967831159,204.976969817163,205.057612321005,
205.138254824848,205.215086266976,205.291830223095,205.368502923075,205.445120540013,
205.521699203249,205.598461453615,205.675026695918,205.751603505063,205.828206449279,
205.905104138502,205.981842244115,206.058819725144,206.135797206173,206.213098020216,
206.29030495828,206.367433936391,206.444500812766,206.521521399694,206.598519126422,
206.675506260877,206.752497067476,206.829505810182,206.906589125712,206.983710392062,
207.060941014079,207.133339587498,207.217202174031,207.300936274521,207.384466767405,
207.467870922295,207.55106929973,207.63211077816,207.709768453488,207.787450103063,
207.865169181945,207.942981813023,208.020848039672,208.098824825375,208.130881968823,
208.210370620897,208.289793196534,208.369146266771,208.440541694968),
 .UNSPECIFIED.);
#3338=B_SPLINE_CURVE_WITH_KNOTS('',3,(#48724,#48725,#48726,#48727,#48728,
#48729,#48730,#48731,#48732,#48733,#48734,#48735,#48736,#48737,#48738,#48739,
#48740,#48741,#48742,#48743,#48744,#48745,#48746,#48747,#48748,#48749,#48750,
#48751,#48752,#48753,#48754,#48755,#48756,#48757,#48758,#48759,#48760,#48761,
#48762,#48763,#48764,#48765,#48766,#48767,#48768,#48769,#48770,#48771,#48772,
#48773,#48774,#48775,#48776,#48777,#48778,#48779,#48780,#48781,#48782,#48783,
#48784,#48785,#48786,#48787,#48788,#48789,#48790,#48791,#48792,#48793,#48794,
#48795,#48796,#48797,#48798,#48799,#48800,#48801,#48802,#48803,#48804,#48805,
#48806,#48807,#48808,#48809,#48810,#48811,#48812,#48813,#48814,#48815,#48816,
#48817,#48818,#48819,#48820,#48821,#48822,#48823,#48824,#48825,#48826,#48827,
#48828,#48829,#48830,#48831,#48832,#48833,#48834,#48835,#48836,#48837,#48838,
#48839,#48840,#48841,#48842,#48843,#48844,#48845,#48846,#48847,#48848,#48849,
#48850,#48851,#48852,#48853,#48854,#48855,#48856,#48857,#48858,#48859,#48860,
#48861,#48862,#48863,#48864,#48865,#48866,#48867,#48868,#48869,#48870,#48871,
#48872,#48873,#48874,#48875,#48876,#48877,#48878,#48879,#48880,#48881,#48882,
#48883,#48884,#48885,#48886,#48887,#48888,#48889),.UNSPECIFIED.,.F.,.F.,
(4,3,3,3,3,3,3,3,3,3,3,3,3,3,3,3,3,3,3,3,3,3,3,3,3,3,3,3,3,3,3,3,3,3,3,
3,3,3,3,3,3,3,3,3,3,3,3,3,3,3,3,3,3,3,3,4),(210.486707790649,210.574035997978,
210.661686182205,210.749760506045,210.80223266358,210.886442245555,210.97052570924,
211.054404114442,211.138153424452,211.221688690448,211.301003854243,211.378384829864,
211.455784219723,211.533215809293,211.610734371807,211.688302600197,211.765977187034,
211.799775044905,211.879399937905,211.958952092152,212.038443808265,212.117887340283,
212.19729490458,212.276685021492,212.356066253251,212.43544967092,212.514846345597,
212.594296643381,212.673775344177,212.753327168943,212.79731742623,212.874048083749,
212.950711760688,213.027323139814,213.103897983228,213.180451388659,213.257008861462,
213.296088616892,213.380757685452,213.465572218932,213.550585623803,213.635685128274,
213.720904607872,213.794859807555,213.876416669066,213.957898399095,214.041831548876,
214.123158669838,214.208394834028,214.293630998217,214.373037155101,214.45246100326,
214.531942537781,214.611455786587,214.691042107325,214.723212227427),
 .UNSPECIFIED.);
#3339=B_SPLINE_CURVE_WITH_KNOTS('',3,(#48890,#48891,#48892,#48893,#48894,
#48895,#48896,#48897,#48898,#48899,#48900,#48901,#48902,#48903,#48904,#48905,
#48906,#48907,#48908,#48909,#48910,#48911,#48912,#48913,#48914,#48915,#48916,
#48917,#48918,#48919,#48920,#48921,#48922,#48923,#48924,#48925,#48926,#48927,
#48928,#48929,#48930,#48931,#48932,#48933,#48934,#48935,#48936,#48937,#48938,
#48939,#48940,#48941,#48942,#48943,#48944,#48945,#48946,#48947,#48948,#48949,
#48950,#48951,#48952,#48953,#48954,#48955,#48956,#48957,#48958,#48959,#48960,
#48961,#48962,#48963,#48964,#48965,#48966,#48967,#48968,#48969,#48970,#48971),
 .UNSPECIFIED.,.F.,.F.,(4,3,3,3,3,3,3,3,3,3,3,3,3,3,3,3,3,3,3,3,3,3,3,3,
3,3,3,4),(208.439780121288,208.518059139744,208.596430820126,208.674852659219,
208.753389883147,208.80714790093,208.883220824591,208.959198260761,209.035096990122,
209.110933712966,209.186725067822,209.263970719626,209.339735933323,209.415508486867,
209.491303382834,209.56965010769,209.645576602262,209.725133442259,209.804690282255,
209.883057417126,209.961290668218,210.039444773925,210.117533004171,210.195568587955,
210.273564240263,210.35153553291,210.429506710964,210.486707790517),
 .UNSPECIFIED.);
#3340=B_SPLINE_CURVE_WITH_KNOTS('',3,(#48973,#48974,#48975,#48976,#48977,
#48978,#48979,#48980,#48981,#48982,#48983,#48984,#48985,#48986,#48987,#48988,
#48989,#48990,#48991,#48992,#48993,#48994,#48995,#48996,#48997,#48998,#48999,
#49000,#49001,#49002,#49003,#49004,#49005,#49006,#49007,#49008,#49009,#49010,
#49011,#49012,#49013,#49014,#49015,#49016,#49017,#49018,#49019,#49020,#49021,
#49022,#49023,#49024,#49025,#49026,#49027,#49028,#49029,#49030,#49031,#49032,
#49033,#49034,#49035,#49036,#49037,#49038,#49039,#49040,#49041,#49042,#49043,
#49044,#49045,#49046,#49047,#49048,#49049,#49050,#49051,#49052,#49053,#49054),
 .UNSPECIFIED.,.F.,.F.,(4,3,3,3,3,3,3,3,3,3,3,3,3,3,3,3,3,3,3,3,3,3,3,3,
3,3,3,4),(208.440541694968,208.519817442129,208.599072594872,208.678316958421,
208.757561868633,208.836818660193,208.916129113754,208.995467201196,209.074881457727,
209.128424350148,209.205289669907,209.282087716157,209.358833075529,209.43554099388,
209.512226991107,209.58891591135,209.62719554081,209.711775118591,209.796496833754,
209.881414237569,209.966416593633,210.051538912713,210.125966731473,210.209270925977,
210.292449952588,210.375545570823,210.458524059154,210.486707790517),
 .UNSPECIFIED.);
#3341=B_SPLINE_CURVE_WITH_KNOTS('',3,(#49055,#49056,#49057,#49058,#49059,
#49060,#49061,#49062,#49063,#49064,#49065,#49066,#49067,#49068,#49069,#49070,
#49071,#49072,#49073,#49074,#49075,#49076,#49077,#49078,#49079,#49080,#49081,
#49082,#49083,#49084,#49085,#49086,#49087,#49088,#49089,#49090,#49091,#49092,
#49093,#49094,#49095,#49096,#49097,#49098,#49099,#49100,#49101,#49102,#49103,
#49104,#49105,#49106,#49107,#49108,#49109,#49110,#49111,#49112,#49113,#49114,
#49115,#49116,#49117,#49118,#49119,#49120,#49121,#49122,#49123,#49124,#49125,
#49126,#49127,#49128,#49129,#49130,#49131,#49132,#49133,#49134,#49135,#49136,
#49137,#49138,#49139,#49140,#49141,#49142,#49143,#49144,#49145,#49146,#49147,
#49148,#49149,#49150,#49151,#49152,#49153,#49154,#49155,#49156,#49157,#49158,
#49159,#49160,#49161,#49162,#49163,#49164,#49165,#49166,#49167,#49168,#49169,
#49170,#49171,#49172,#49173,#49174,#49175,#49176,#49177,#49178,#49179,#49180,
#49181,#49182,#49183,#49184,#49185,#49186,#49187,#49188,#49189,#49190,#49191,
#49192,#49193,#49194,#49195,#49196,#49197,#49198,#49199,#49200,#49201,#49202,
#49203,#49204,#49205,#49206,#49207,#49208,#49209,#49210,#49211),
 .UNSPECIFIED.,.F.,.F.,(4,3,3,3,3,3,3,3,3,3,3,3,3,3,3,3,3,3,3,3,3,3,3,3,
3,3,3,3,3,3,3,3,3,3,3,3,3,3,3,3,3,3,3,3,3,3,3,3,3,3,3,3,4),(210.486707790517,
210.569169996617,210.65163185442,210.734093370775,210.816554552533,210.899015406543,
210.981475939655,211.063936158718,211.146396070581,211.228855682093,211.311315000102,
211.393774031456,211.476232783002,211.55869126159,211.641149474066,211.723607427277,
211.806065128069,211.888522583291,211.970979799789,212.056992495075,212.140317293633,
212.222783899225,212.305249660608,212.387714605198,212.470178760406,212.552642153643,
212.635104812314,212.717566763826,212.800028035578,212.882488654971,212.964948649402,
213.047408046266,213.129866872957,213.212325156864,213.294782925377,213.377240205883,
213.461374321074,213.543840319434,213.62630469604,213.708767560536,213.791229022542,
213.873689191661,213.956148177477,214.038606089558,214.12420358448,214.206668321526,
214.289130093913,214.371589340078,214.454046498316,214.536509017399,214.61896668881,
214.701425480003,214.72338604894),.UNSPECIFIED.);
#3342=B_SPLINE_CURVE_WITH_KNOTS('',3,(#49217,#49218,#49219,#49220,#49221,
#49222,#49223,#49224,#49225,#49226,#49227,#49228,#49229,#49230,#49231,#49232,
#49233,#49234,#49235,#49236,#49237,#49238,#49239,#49240,#49241,#49242,#49243,
#49244,#49245,#49246,#49247,#49248,#49249,#49250,#49251,#49252,#49253,#49254,
#49255,#49256,#49257,#49258,#49259,#49260,#49261,#49262,#49263,#49264,#49265,
#49266,#49267,#49268,#49269,#49270,#49271,#49272,#49273,#49274,#49275,#49276,
#49277,#49278,#49279,#49280,#49281,#49282,#49283,#49284,#49285,#49286,#49287,
#49288,#49289,#49290,#49291,#49292,#49293,#49294,#49295,#49296,#49297,#49298,
#49299,#49300,#49301,#49302,#49303,#49304,#49305,#49306,#49307,#49308,#49309,
#49310,#49311,#49312,#49313,#49314,#49315,#49316,#49317,#49318,#49319,#49320,
#49321,#49322,#49323,#49324,#49325,#49326,#49327,#49328,#49329,#49330,#49331,
#49332,#49333,#49334,#49335,#49336,#49337,#49338,#49339,#49340,#49341,#49342,
#49343,#49344,#49345,#49346,#49347,#49348,#49349,#49350,#49351,#49352,#49353,
#49354,#49355,#49356,#49357,#49358,#49359,#49360,#49361,#49362,#49363,#49364,
#49365,#49366,#49367,#49368,#49369,#49370,#49371,#49372,#49373,#49374,#49375,
#49376,#49377,#49378,#49379,#49380,#49381,#49382,#49383,#49384,#49385),
 .UNSPECIFIED.,.F.,.F.,(4,3,3,3,3,3,3,3,3,3,3,3,3,3,3,3,3,3,3,3,3,3,3,3,
3,3,3,3,3,3,3,3,3,3,3,3,3,3,3,3,3,3,3,3,3,3,3,3,3,3,3,3,3,3,3,3,4),(216.769893097696,
216.78748695153,216.865057174543,216.942535317151,217.01993703317,217.097277921584,
217.174573537611,217.251846979369,217.329110216827,217.40637728642,217.483662224083,
217.561020228582,217.638415761792,217.715917430692,217.785029332854,217.869241477041,
217.953327497511,218.037208412379,218.120960191465,218.204497832145,218.283800523517,
218.361180292665,218.438578456566,218.516008802034,218.593526098427,218.671093047367,
218.748766341805,218.782571714179,218.862196901683,218.941749356195,219.021241377614,
219.100685219253,219.180093096772,219.25948353051,219.338865080873,219.418248818292,
219.497645813234,219.577096429974,219.656575449028,219.7361275883,219.780114095504,
219.85684467338,219.933508271297,220.010119572076,220.086694338341,220.163247667286,
220.239805064844,220.278885286167,220.363554278549,220.448368731396,220.533382050469,
220.618481466828,220.703700856217,220.777656476829,220.859217231912,220.940684707488,
221.007081309262),.UNSPECIFIED.);
#3343=B_SPLINE_CURVE_WITH_KNOTS('',3,(#49386,#49387,#49388,#49389,#49390,
#49391,#49392,#49393,#49394,#49395,#49396,#49397,#49398,#49399,#49400,#49401,
#49402,#49403,#49404,#49405,#49406,#49407,#49408,#49409,#49410,#49411,#49412,
#49413,#49414,#49415,#49416,#49417,#49418,#49419,#49420,#49421,#49422,#49423,
#49424,#49425,#49426,#49427,#49428,#49429,#49430,#49431,#49432,#49433,#49434,
#49435,#49436,#49437,#49438,#49439,#49440,#49441,#49442,#49443,#49444,#49445,
#49446,#49447,#49448,#49449,#49450,#49451,#49452,#49453,#49454,#49455,#49456,
#49457,#49458,#49459,#49460,#49461,#49462,#49463,#49464,#49465,#49466,#49467),
 .UNSPECIFIED.,.F.,.F.,(4,3,3,3,3,3,3,3,3,3,3,3,3,3,3,3,3,3,3,3,3,3,3,3,
3,3,3,4),(214.723212227427,214.79240218888,214.870790556853,214.949112810023,
215.027383347989,215.10561653284,215.183826698642,215.262044821928,215.340270874921,
215.418517844138,215.496798725914,215.575172141155,215.65359512691,215.732134673559,
215.789944570205,215.865782243268,215.941524820589,216.017189214147,216.092792248486,
216.16835068143,216.243891735941,216.319425700808,216.394967679098,216.470532780008,
216.546183611105,216.621878216807,216.697695297951,216.769893097579),
 .UNSPECIFIED.);
#3344=B_SPLINE_CURVE_WITH_KNOTS('',3,(#49469,#49470,#49471,#49472,#49473,
#49474,#49475,#49476,#49477,#49478,#49479,#49480,#49481,#49482,#49483,#49484,
#49485,#49486,#49487,#49488,#49489,#49490,#49491,#49492,#49493,#49494,#49495,
#49496,#49497,#49498,#49499,#49500,#49501,#49502,#49503,#49504,#49505,#49506,
#49507,#49508,#49509,#49510,#49511,#49512,#49513,#49514,#49515,#49516,#49517,
#49518,#49519,#49520,#49521,#49522,#49523,#49524,#49525,#49526,#49527,#49528,
#49529,#49530,#49531,#49532,#49533,#49534,#49535,#49536,#49537,#49538,#49539,
#49540,#49541,#49542,#49543,#49544),.UNSPECIFIED.,.F.,.F.,(4,3,3,3,3,3,
3,3,3,3,3,3,3,3,3,3,3,3,3,3,3,3,3,3,3,4),(214.72338604894,214.805847652671,
214.888308590522,214.970768889894,215.053228578183,215.135687682781,215.218146231082,
215.300604250474,215.383061768347,215.469738726431,215.552205511972,215.63467062504,
215.717134175288,215.799596272347,215.882057025829,215.964516545325,216.04697494041,
216.129432320643,216.21189870633,216.294361907838,216.376822363687,216.459280512242,
216.541746115996,216.624205994384,216.706670105636,216.769893097696),
 .UNSPECIFIED.);
#3345=B_SPLINE_CURVE_WITH_KNOTS('',3,(#49545,#49546,#49547,#49548,#49549,
#49550,#49551,#49552,#49553,#49554,#49555,#49556,#49557,#49558,#49559,#49560,
#49561,#49562,#49563,#49564,#49565,#49566,#49567,#49568,#49569,#49570,#49571,
#49572,#49573,#49574,#49575,#49576,#49577,#49578,#49579,#49580,#49581,#49582,
#49583,#49584,#49585,#49586,#49587,#49588,#49589,#49590,#49591,#49592,#49593,
#49594,#49595,#49596,#49597,#49598,#49599,#49600,#49601,#49602,#49603,#49604,
#49605,#49606,#49607,#49608,#49609,#49610,#49611,#49612,#49613,#49614,#49615,
#49616,#49617,#49618,#49619,#49620,#49621,#49622,#49623,#49624,#49625,#49626,
#49627,#49628,#49629,#49630,#49631,#49632,#49633,#49634,#49635,#49636,#49637,
#49638,#49639,#49640,#49641,#49642,#49643,#49644,#49645,#49646,#49647,#49648,
#49649,#49650,#49651,#49652,#49653,#49654,#49655,#49656,#49657,#49658,#49659,
#49660,#49661,#49662,#49663,#49664,#49665,#49666,#49667,#49668,#49669,#49670,
#49671,#49672,#49673,#49674,#49675,#49676,#49677,#49678,#49679,#49680,#49681,
#49682,#49683,#49684,#49685,#49686,#49687,#49688,#49689,#49690,#49691,#49692,
#49693,#49694,#49695,#49696,#49697,#49698,#49699,#49700,#49701,#49702,#49703,
#49704,#49705,#49706,#49707,#49708,#49709,#49710),.UNSPECIFIED.,.F.,.F.,
(4,3,3,3,3,3,3,3,3,3,3,3,3,3,3,3,3,3,3,3,3,3,3,3,3,3,3,3,3,3,3,3,3,3,3,
3,3,3,3,3,3,3,3,3,3,3,3,3,3,3,3,3,3,3,3,4),(216.769893097696,216.857542834203,
216.94535140566,217.033334882977,217.108763400747,217.190320262258,217.271801992287,
217.355735142068,217.43706226303,217.52229842722,217.607534591409,217.686945851679,
217.766375539313,217.8458344145,217.925366303503,218.004939896209,218.0845970871,
218.106305782072,218.184694150045,218.263016403215,218.341286941181,218.419520126032,
218.497730291834,218.57594841512,218.654174468113,218.73242143733,218.810702319106,
218.889075734348,218.967498720102,219.046038266751,219.103848163397,219.179919442805,
219.255895221033,219.331792279812,219.407627320417,219.483416982312,219.560663677613,
219.636427177676,219.712198010845,219.787991180482,219.866341021542,219.942265786842,
220.021828165782,220.101390544722,220.178966041541,220.256448430164,220.333853368607,
220.41119645919,220.488491688953,220.565761219485,220.643019095461,220.720279352326,
220.797585916934,220.874916814307,220.952325353479,221.006028990015),
 .UNSPECIFIED.);
#3346=B_SPLINE_CURVE_WITH_KNOTS('',3,(#49716,#49717,#49718,#49719,#49720,
#49721,#49722,#49723,#49724,#49725,#49726,#49727,#49728,#49729,#49730,#49731,
#49732,#49733,#49734,#49735,#49736,#49737,#49738,#49739,#49740,#49741,#49742,
#49743,#49744,#49745,#49746,#49747,#49748,#49749,#49750,#49751,#49752,#49753,
#49754,#49755,#49756,#49757,#49758,#49759,#49760,#49761,#49762,#49763,#49764,
#49765,#49766,#49767,#49768,#49769,#49770,#49771,#49772,#49773,#49774,#49775,
#49776,#49777,#49778,#49779,#49780,#49781,#49782,#49783,#49784,#49785,#49786,
#49787,#49788,#49789,#49790,#49791,#49792,#49793,#49794,#49795,#49796,#49797,
#49798,#49799,#49800,#49801,#49802,#49803,#49804,#49805,#49806,#49807,#49808,
#49809,#49810,#49811,#49812,#49813,#49814,#49815,#49816,#49817,#49818,#49819,
#49820,#49821,#49822,#49823,#49824,#49825,#49826,#49827,#49828,#49829,#49830,
#49831,#49832,#49833,#49834,#49835,#49836,#49837,#49838,#49839,#49840,#49841,
#49842,#49843,#49844,#49845,#49846,#49847,#49848,#49849,#49850,#49851,#49852,
#49853,#49854,#49855,#49856,#49857,#49858,#49859,#49860,#49861,#49862,#49863,
#49864,#49865,#49866,#49867,#49868,#49869,#49870,#49871,#49872),
 .UNSPECIFIED.,.F.,.F.,(4,3,3,3,3,3,3,3,3,3,3,3,3,3,3,3,3,3,3,3,3,3,3,3,
3,3,3,3,3,3,3,3,3,3,3,3,3,3,3,3,3,3,3,3,3,3,3,3,3,3,3,3,4),(223.053078404876,
223.135540610976,223.218002468779,223.300463985134,223.382925166892,223.465386020902,
223.547846554014,223.630306773077,223.71276668494,223.795226296452,223.877685614461,
223.960144645815,224.042603397362,224.125061875949,224.207520088425,224.289978041636,
224.372435742429,224.45489319765,224.537350414148,224.623363109434,224.706687907992,
224.789154513584,224.871620274967,224.954085219557,225.036549374765,225.119012768002,
225.201475426674,225.283937378185,225.366398649937,225.44885926933,225.531319263761,
225.613778660626,225.696237487316,225.778695771223,225.861153539736,225.943610820242,
226.027744935433,226.110210933793,226.192675310399,226.275138174895,226.357599636901,
226.44005980602,226.522518791836,226.604976703917,226.690574198839,226.773038935885,
226.855500708272,226.937959954437,227.020417112675,227.102879631758,227.185337303169,
227.267796094362,227.289756663299),.UNSPECIFIED.);
#3347=B_SPLINE_CURVE_WITH_KNOTS('',3,(#49873,#49874,#49875,#49876,#49877,
#49878,#49879,#49880,#49881,#49882,#49883,#49884,#49885,#49886,#49887,#49888,
#49889,#49890,#49891,#49892,#49893,#49894,#49895,#49896,#49897,#49898,#49899,
#49900,#49901,#49902,#49903,#49904,#49905,#49906,#49907,#49908,#49909,#49910,
#49911,#49912,#49913,#49914,#49915,#49916,#49917,#49918,#49919,#49920,#49921,
#49922,#49923,#49924,#49925,#49926,#49927,#49928,#49929,#49930,#49931,#49932,
#49933,#49934,#49935,#49936,#49937,#49938,#49939,#49940,#49941,#49942,#49943,
#49944,#49945,#49946,#49947,#49948,#49949,#49950,#49951,#49952,#49953,#49954),
 .UNSPECIFIED.,.F.,.F.,(4,3,3,3,3,3,3,3,3,3,3,3,3,3,3,3,3,3,3,3,3,3,3,3,
3,3,3,4),(221.007081309262,221.08842070214,221.169705935063,221.250929267071,
221.276427667492,221.355838866142,221.435268490865,221.514727301993,221.594259125629,
221.67383265224,221.753489776388,221.775198858154,221.853587237142,221.931909501563,
222.010180051,222.088413247522,222.166623425177,222.244841560538,222.323067625735,
222.40131460727,222.479595501462,222.557968929194,222.636391927495,222.714931486662,
222.772741239479,222.865773615059,222.959426009967,223.053078404876),
 .UNSPECIFIED.);
#3348=B_SPLINE_CURVE_WITH_KNOTS('',3,(#49956,#49957,#49958,#49959,#49960,
#49961,#49962,#49963,#49964,#49965,#49966,#49967,#49968,#49969,#49970,#49971,
#49972,#49973,#49974,#49975,#49976,#49977,#49978,#49979,#49980,#49981,#49982,
#49983,#49984,#49985,#49986,#49987,#49988,#49989,#49990,#49991,#49992,#49993,
#49994,#49995,#49996,#49997,#49998,#49999,#50000,#50001,#50002,#50003,#50004,
#50005,#50006,#50007,#50008,#50009,#50010,#50011,#50012,#50013,#50014,#50015,
#50016,#50017,#50018,#50019,#50020,#50021,#50022,#50023,#50024,#50025,#50026,
#50027,#50028,#50029,#50030,#50031,#50032,#50033,#50034,#50035,#50036,#50037),
 .UNSPECIFIED.,.F.,.F.,(4,3,3,3,3,3,3,3,3,3,3,3,3,3,3,3,3,3,3,3,3,3,3,3,
3,3,3,4),(221.006028990015,221.08355116665,221.098932926047,221.183145070235,
221.267231090704,221.351112005572,221.434863784658,221.518401425339,221.597704116709,
221.675083885857,221.752482049758,221.829912395226,221.907429691619,221.984996640559,
222.062669934996,222.096475307371,222.175596135735,222.254642773363,222.333628560977,
222.412566793728,222.492630745122,222.57152068099,222.650405615386,222.729297551187,
222.81024276461,222.889213089609,222.971145747242,223.053078404876),
 .UNSPECIFIED.);
#3349=B_SPLINE_CURVE_WITH_KNOTS('',3,(#50038,#50039,#50040,#50041,#50042,
#50043,#50044,#50045,#50046,#50047,#50048,#50049,#50050,#50051,#50052,#50053,
#50054,#50055,#50056,#50057,#50058,#50059,#50060,#50061,#50062,#50063,#50064,
#50065,#50066,#50067,#50068,#50069,#50070,#50071,#50072,#50073,#50074,#50075,
#50076,#50077,#50078,#50079,#50080,#50081,#50082,#50083,#50084,#50085,#50086,
#50087,#50088,#50089,#50090,#50091,#50092,#50093,#50094,#50095,#50096,#50097,
#50098,#50099,#50100,#50101,#50102,#50103,#50104,#50105,#50106,#50107,#50108,
#50109,#50110,#50111,#50112,#50113,#50114,#50115,#50116,#50117,#50118,#50119,
#50120,#50121,#50122,#50123,#50124,#50125,#50126,#50127,#50128,#50129,#50130,
#50131,#50132,#50133,#50134,#50135,#50136,#50137,#50138,#50139,#50140,#50141,
#50142,#50143,#50144,#50145,#50146,#50147,#50148,#50149,#50150,#50151,#50152,
#50153,#50154,#50155,#50156,#50157,#50158,#50159,#50160,#50161,#50162,#50163,
#50164,#50165,#50166,#50167,#50168,#50169,#50170,#50171,#50172,#50173,#50174,
#50175,#50176,#50177,#50178,#50179,#50180,#50181,#50182,#50183,#50184,#50185,
#50186,#50187,#50188,#50189,#50190,#50191,#50192,#50193,#50194),
 .UNSPECIFIED.,.F.,.F.,(4,3,3,3,3,3,3,3,3,3,3,3,3,3,3,3,3,3,3,3,3,3,3,3,
3,3,3,3,3,3,3,3,3,3,3,3,3,3,3,3,3,3,3,3,3,3,3,3,3,3,3,3,4),(223.053078404876,
223.135540610976,223.218002468779,223.300463985134,223.382925166892,223.465386020902,
223.547846554014,223.630306773077,223.71276668494,223.795226296452,223.877685614461,
223.960144645814,224.042603397361,224.125061875949,224.207520088424,224.289978041635,
224.372435742428,224.45489319765,224.537350414148,224.623363109434,224.706687907992,
224.789154513584,224.871620274967,224.954085219557,225.036549374765,225.119012768002,
225.201475426673,225.283937378184,225.366398649937,225.44885926933,225.531319263761,
225.613778660625,225.696237487315,225.778695771222,225.861153539735,225.943610820242,
226.027744935433,226.110210933793,226.192675310399,226.275138174894,226.357599636901,
226.44005980602,226.522518791836,226.604976703916,226.690574198839,226.773038935885,
226.855500708271,226.937959954437,227.020417112675,227.102879631758,227.185337303169,
227.267796094362,227.289756663299),.UNSPECIFIED.);
#3350=B_SPLINE_CURVE_WITH_KNOTS('',3,(#50200,#50201,#50202,#50203,#50204,
#50205,#50206,#50207,#50208,#50209,#50210,#50211,#50212,#50213,#50214,#50215,
#50216,#50217,#50218,#50219,#50220,#50221,#50222,#50223,#50224,#50225,#50226,
#50227,#50228,#50229,#50230,#50231,#50232,#50233,#50234,#50235,#50236,#50237,
#50238,#50239,#50240,#50241,#50242,#50243,#50244,#50245,#50246,#50247,#50248,
#50249,#50250,#50251,#50252,#50253,#50254,#50255,#50256,#50257,#50258,#50259,
#50260,#50261,#50262,#50263,#50264,#50265,#50266,#50267,#50268,#50269,#50270,
#50271,#50272,#50273,#50274,#50275,#50276,#50277,#50278,#50279,#50280,#50281,
#50282,#50283,#50284,#50285,#50286,#50287,#50288,#50289,#50290,#50291,#50292,
#50293,#50294,#50295,#50296,#50297,#50298,#50299,#50300,#50301,#50302,#50303,
#50304,#50305,#50306,#50307,#50308,#50309,#50310,#50311,#50312,#50313,#50314,
#50315,#50316,#50317,#50318,#50319,#50320,#50321,#50322,#50323,#50324,#50325,
#50326,#50327,#50328,#50329,#50330,#50331,#50332,#50333,#50334,#50335,#50336,
#50337,#50338,#50339,#50340,#50341,#50342,#50343,#50344,#50345,#50346,#50347,
#50348,#50349,#50350,#50351,#50352,#50353,#50354,#50355,#50356,#50357,#50358,
#50359,#50360,#50361,#50362,#50363,#50364,#50365),.UNSPECIFIED.,.F.,.F.,
(4,3,3,3,3,3,3,3,3,3,3,3,3,3,3,3,3,3,3,3,3,3,3,3,3,3,3,3,3,3,3,3,3,3,3,
3,3,3,3,3,3,3,3,3,3,3,3,3,3,3,3,3,3,3,3,4),(229.336263712055,229.42420714738,
229.512813714511,229.60173220212,229.691037881645,229.755537908753,229.831609186389,
229.907584962836,229.983482019828,230.059317058641,230.135106718738,230.212353415156,
230.288116913416,230.363887744783,230.439680912617,230.518030756982,230.593955520493,
230.673517905285,230.753080290078,230.830650511021,230.908128651541,230.985530365454,
231.062871251749,231.140166865644,231.217440305258,231.294703540565,231.371970608002,
231.449255543505,231.526613545852,231.604009076909,231.681510743676,231.750622671403,
231.834834822864,231.918920850574,232.00280177252,232.086553558554,232.170091205891,
232.249393862065,232.326773628396,232.404171789439,232.481602132012,232.559119425465,
232.636686371439,232.714359662886,232.748165052728,232.827797669572,232.907356129713,
232.990558092998,233.069996494092,233.149402444597,233.228787037255,233.30816134938,
233.387551861245,233.46695070344,233.546387278613,233.572971835991),
 .UNSPECIFIED.);
#3351=B_SPLINE_CURVE_WITH_KNOTS('',3,(#50366,#50367,#50368,#50369,#50370,
#50371,#50372,#50373,#50374,#50375,#50376,#50377,#50378,#50379,#50380,#50381,
#50382,#50383,#50384,#50385,#50386,#50387,#50388,#50389,#50390,#50391,#50392,
#50393,#50394,#50395,#50396,#50397,#50398,#50399,#50400,#50401,#50402,#50403,
#50404,#50405,#50406,#50407,#50408,#50409,#50410,#50411,#50412,#50413,#50414,
#50415,#50416,#50417,#50418,#50419,#50420,#50421,#50422,#50423,#50424,#50425,
#50426,#50427,#50428,#50429,#50430,#50431,#50432,#50433,#50434,#50435,#50436,
#50437,#50438,#50439,#50440,#50441),.UNSPECIFIED.,.F.,.F.,(4,3,3,3,3,3,
3,3,3,3,3,3,3,3,3,3,3,3,3,3,3,3,3,3,3,4),(227.289756663299,227.37221826703,
227.454679204882,227.537139504254,227.619599192542,227.70205829714,227.784516845441,
227.866974864833,227.949432382706,228.03610934079,228.118576126331,228.201041239399,
228.283504789647,228.365966886706,228.448427640188,228.530887159684,228.613345554769,
228.695802935002,228.778269320689,228.860732522197,228.943192978047,229.025651126601,
229.108116730355,229.190576608743,229.273040719995,229.336263712055),
 .UNSPECIFIED.);
#3352=B_SPLINE_CURVE_WITH_KNOTS('',3,(#50443,#50444,#50445,#50446,#50447,
#50448,#50449,#50450,#50451,#50452,#50453,#50454,#50455,#50456,#50457,#50458,
#50459,#50460,#50461,#50462,#50463,#50464,#50465,#50466,#50467,#50468,#50469,
#50470,#50471,#50472,#50473,#50474,#50475,#50476,#50477,#50478,#50479,#50480,
#50481,#50482,#50483,#50484,#50485,#50486,#50487,#50488,#50489,#50490,#50491,
#50492,#50493,#50494,#50495,#50496,#50497,#50498,#50499,#50500,#50501,#50502,
#50503,#50504,#50505,#50506,#50507,#50508,#50509,#50510,#50511,#50512,#50513,
#50514,#50515,#50516,#50517,#50518),.UNSPECIFIED.,.F.,.F.,(4,3,3,3,3,3,
3,3,3,3,3,3,3,3,3,3,3,3,3,3,3,3,3,3,3,4),(227.289756663299,227.37221826703,
227.454679204882,227.537139504254,227.619599192542,227.70205829714,227.784516845441,
227.866974864833,227.949432382706,228.036109340785,228.118576126326,228.201041239394,
228.283504789642,228.365966886701,228.448427640183,228.530887159679,228.613345554764,
228.695802934997,228.778269320684,228.860732522192,228.943192978041,229.025651126596,
229.10811673035,229.190576608738,229.27304071999,229.33626371197),
 .UNSPECIFIED.);
#3353=B_SPLINE_CURVE_WITH_KNOTS('',3,(#50519,#50520,#50521,#50522,#50523,
#50524,#50525,#50526,#50527,#50528,#50529,#50530,#50531,#50532,#50533,#50534,
#50535,#50536,#50537,#50538,#50539,#50540,#50541,#50542,#50543,#50544,#50545,
#50546,#50547,#50548,#50549,#50550,#50551,#50552,#50553,#50554,#50555,#50556,
#50557,#50558,#50559,#50560,#50561,#50562,#50563,#50564,#50565,#50566,#50567,
#50568,#50569,#50570,#50571,#50572,#50573,#50574,#50575,#50576,#50577,#50578,
#50579,#50580,#50581,#50582,#50583,#50584,#50585,#50586,#50587,#50588,#50589,
#50590,#50591,#50592,#50593,#50594,#50595,#50596,#50597,#50598,#50599,#50600,
#50601,#50602,#50603,#50604,#50605,#50606,#50607,#50608,#50609,#50610,#50611,
#50612,#50613,#50614,#50615,#50616,#50617,#50618,#50619,#50620,#50621,#50622,
#50623,#50624,#50625,#50626,#50627,#50628,#50629,#50630,#50631,#50632,#50633,
#50634,#50635,#50636,#50637,#50638,#50639,#50640,#50641,#50642,#50643,#50644,
#50645,#50646,#50647,#50648,#50649,#50650,#50651,#50652,#50653,#50654,#50655,
#50656,#50657,#50658,#50659,#50660,#50661,#50662,#50663,#50664,#50665,#50666,
#50667,#50668,#50669,#50670,#50671,#50672,#50673,#50674,#50675),
 .UNSPECIFIED.,.F.,.F.,(4,3,3,3,3,3,3,3,3,3,3,3,3,3,3,3,3,3,3,3,3,3,3,3,
3,3,3,3,3,3,3,3,3,3,3,3,3,3,3,3,3,3,3,3,3,3,3,3,3,3,3,3,4),(229.336263712055,
229.418725918155,229.501187775958,229.583649292313,229.666110474071,229.748571328081,
229.831031861193,229.913492080256,229.995951992119,230.078411603631,230.16087092164,
230.243329952993,230.32578870454,230.408247183128,230.490705395604,230.573163348814,
230.655621049607,230.738078504829,230.820535721327,230.906548416613,230.989873215171,
231.072339820763,231.154805582146,231.237270526736,231.319734681944,231.402198075181,
231.484660733853,231.567122685364,231.649583957116,231.732044576509,231.81450457094,
231.896963967805,231.979422794495,232.061881078402,232.144338846915,232.226796127421,
232.310930242612,232.393396240972,232.475860617579,232.558323482074,232.64078494408,
232.7232451132,232.805704099016,232.888162011096,232.973759506019,233.056224243065,
233.138686015451,233.221145261616,233.303602419855,233.386064938937,233.468522610348,
233.550981401542,233.572941970479),.UNSPECIFIED.);
#3354=B_SPLINE_CURVE_WITH_KNOTS('',3,(#50681,#50682,#50683,#50684,#50685,
#50686,#50687,#50688,#50689,#50690,#50691,#50692,#50693,#50694,#50695,#50696,
#50697,#50698,#50699,#50700,#50701,#50702,#50703,#50704,#50705,#50706,#50707,
#50708,#50709,#50710,#50711,#50712,#50713,#50714,#50715,#50716,#50717,#50718,
#50719,#50720,#50721,#50722,#50723,#50724,#50725,#50726,#50727,#50728,#50729,
#50730,#50731,#50732,#50733,#50734,#50735,#50736,#50737,#50738,#50739,#50740,
#50741,#50742,#50743,#50744,#50745,#50746,#50747,#50748,#50749,#50750,#50751,
#50752,#50753,#50754,#50755,#50756,#50757,#50758,#50759,#50760,#50761,#50762,
#50763,#50764,#50765,#50766,#50767,#50768,#50769,#50770,#50771,#50772,#50773,
#50774,#50775,#50776,#50777,#50778,#50779,#50780,#50781,#50782,#50783,#50784,
#50785,#50786,#50787,#50788,#50789,#50790,#50791,#50792,#50793,#50794,#50795,
#50796,#50797,#50798,#50799,#50800,#50801,#50802,#50803,#50804,#50805,#50806,
#50807,#50808,#50809,#50810,#50811,#50812,#50813,#50814,#50815,#50816,#50817,
#50818,#50819,#50820,#50821,#50822,#50823,#50824,#50825,#50826,#50827,#50828,
#50829,#50830,#50831,#50832,#50833,#50834,#50835,#50836,#50837,#50838,#50839,
#50840,#50841,#50842,#50843,#50844,#50845,#50846,#50847,#50848,#50849),
 .UNSPECIFIED.,.F.,.F.,(4,3,3,3,3,3,3,3,3,3,3,3,3,3,3,3,3,3,3,3,3,3,3,3,
3,3,3,3,3,3,3,3,3,3,3,3,3,3,3,3,3,3,3,3,3,3,3,3,3,3,3,3,3,3,3,3,4),(235.619449019235,
235.719318537606,235.740792196703,235.819180575711,235.897502840153,235.975773389612,
236.054006586156,236.132216763833,236.210434899216,236.288660964436,236.366907945993,
236.445188840208,236.523562267962,236.601985266286,236.680524825476,236.738334578027,
236.814405855663,236.89038163211,236.966278689102,237.042113727915,237.117903388012,
237.195150084429,237.27091358269,237.346684414057,237.42247758189,237.500827426256,
237.576752189766,237.656314574559,237.735876959352,237.813447180295,237.890925320815,
237.968327034729,238.045667921024,238.122963534918,238.200236974532,238.277500209839,
238.354767277276,238.43205221278,238.509410215127,238.586805746184,238.664307412951,
238.733419340677,238.817631492138,238.901717519848,238.985598441794,239.069350227828,
239.152887875165,239.23219053134,239.309570297671,239.386968458714,239.464398801287,
239.54191609474,239.619483040714,239.697156332161,239.730961722002,239.81058672982,
239.856215740081),.UNSPECIFIED.);
#3355=B_SPLINE_CURVE_WITH_KNOTS('',3,(#50850,#50851,#50852,#50853,#50854,
#50855,#50856,#50857,#50858,#50859,#50860,#50861,#50862,#50863,#50864,#50865,
#50866,#50867,#50868,#50869,#50870,#50871,#50872,#50873,#50874,#50875,#50876,
#50877,#50878,#50879,#50880,#50881,#50882,#50883,#50884,#50885,#50886,#50887,
#50888,#50889,#50890,#50891,#50892,#50893,#50894,#50895,#50896,#50897,#50898,
#50899,#50900,#50901,#50902,#50903,#50904,#50905,#50906,#50907,#50908,#50909,
#50910,#50911,#50912,#50913,#50914,#50915,#50916,#50917,#50918,#50919,#50920,
#50921,#50922,#50923,#50924,#50925,#50926,#50927,#50928,#50929,#50930,#50931),
 .UNSPECIFIED.,.F.,.F.,(4,3,3,3,3,3,3,3,3,3,3,3,3,3,3,3,3,3,3,3,3,3,3,3,
3,3,3,4),(233.572971835991,233.652464355483,233.732024717962,233.745707434053,
233.822438012378,233.899101610745,233.975712911973,234.052287678688,234.128841008082,
234.205398406087,234.244478624715,234.329147616333,234.413962068381,234.498975386618,
234.584074802128,234.66929419066,234.743249815378,234.824806795004,234.906288643971,
234.990221734488,235.071548974518,235.156784990279,235.24202100604,235.318774721805,
235.395557004039,235.472352167508,235.549215192412,235.619449019133),
 .UNSPECIFIED.);
#3356=B_SPLINE_CURVE_WITH_KNOTS('',3,(#50933,#50934,#50935,#50936,#50937,
#50938,#50939,#50940,#50941,#50942,#50943,#50944,#50945,#50946,#50947,#50948,
#50949,#50950,#50951,#50952,#50953,#50954,#50955,#50956,#50957,#50958,#50959,
#50960,#50961,#50962,#50963,#50964,#50965,#50966,#50967,#50968,#50969,#50970,
#50971,#50972,#50973,#50974,#50975,#50976,#50977,#50978,#50979,#50980,#50981,
#50982,#50983,#50984,#50985,#50986,#50987,#50988,#50989,#50990,#50991,#50992,
#50993,#50994,#50995,#50996,#50997,#50998,#50999,#51000,#51001,#51002,#51003,
#51004,#51005,#51006,#51007,#51008),.UNSPECIFIED.,.F.,.F.,(4,3,3,3,3,3,
3,3,3,3,3,3,3,3,3,3,3,3,3,3,3,3,3,3,3,4),(233.572941970479,233.655403574209,
233.737864512061,233.820324811433,233.902784499722,233.98524360432,234.06770215262,
234.150160172013,234.232617689886,234.31929464797,234.401761433511,234.484226546579,
234.566690096827,234.649152193886,234.731612947368,234.814072466864,234.896530861949,
234.978988242183,235.061454627869,235.143917829377,235.226378285227,235.308836433781,
235.391302037535,235.473761915923,235.556226027175,235.619449019235),
 .UNSPECIFIED.);
#3357=B_SPLINE_CURVE_WITH_KNOTS('',3,(#51009,#51010,#51011,#51012,#51013,
#51014,#51015,#51016,#51017,#51018,#51019,#51020,#51021,#51022,#51023,#51024,
#51025,#51026,#51027,#51028,#51029,#51030,#51031,#51032,#51033,#51034,#51035,
#51036,#51037,#51038,#51039,#51040,#51041,#51042,#51043,#51044,#51045,#51046,
#51047,#51048,#51049,#51050,#51051,#51052,#51053,#51054,#51055,#51056,#51057,
#51058,#51059,#51060,#51061,#51062,#51063,#51064,#51065,#51066,#51067,#51068,
#51069,#51070,#51071,#51072,#51073,#51074,#51075,#51076,#51077,#51078,#51079,
#51080,#51081,#51082,#51083,#51084,#51085,#51086,#51087,#51088,#51089,#51090,
#51091,#51092,#51093,#51094,#51095,#51096,#51097,#51098,#51099,#51100,#51101,
#51102,#51103,#51104,#51105,#51106,#51107,#51108,#51109,#51110,#51111,#51112,
#51113,#51114,#51115,#51116,#51117,#51118,#51119,#51120,#51121,#51122,#51123,
#51124,#51125,#51126,#51127,#51128,#51129,#51130,#51131,#51132,#51133,#51134,
#51135,#51136,#51137,#51138,#51139,#51140,#51141,#51142,#51143,#51144,#51145,
#51146,#51147,#51148,#51149,#51150,#51151,#51152,#51153,#51154,#51155,#51156,
#51157,#51158,#51159,#51160,#51161,#51162,#51163,#51164,#51165,#51166,#51167,
#51168,#51169,#51170,#51171,#51172,#51173,#51174,#51175,#51176,#51177),
 .UNSPECIFIED.,.F.,.F.,(4,3,3,3,3,3,3,3,3,3,3,3,3,3,3,3,3,3,3,3,3,3,3,3,
3,3,3,3,3,3,3,3,3,3,3,3,3,3,3,3,3,3,3,3,3,3,3,3,3,3,3,3,3,3,3,3,4),(235.619449019235,
235.697995435465,235.776589771173,235.855293804889,235.934057908597,236.012948288771,
236.06206864592,236.141693833781,236.221246288657,236.300738310445,236.38018215246,
236.459590030358,236.53898046448,236.618362015229,236.697745753035,236.777142748366,
236.856593365491,236.93607238493,237.015624524582,237.059611027245,237.13634160557,
237.213005203937,237.289616505166,237.36619127188,237.442744601275,237.51930199928,
237.558382217907,237.643051209525,237.727865661573,237.81287897981,237.897978395319,
237.983197783851,238.05715340857,238.138710388197,238.220192237163,238.30412532768,
238.385452567711,238.470688583471,238.555924599232,238.63533579771,238.714765422258,
238.794224233208,238.873756056663,238.953329583092,239.032986707056,239.054695789895,
239.133091487211,239.211419106365,239.291963083862,239.370196668063,239.448409834818,
239.526615572052,239.608904410625,239.687159228354,239.765440135615,239.843782795569,
239.855770926344),.UNSPECIFIED.);
#3358=B_SPLINE_CURVE_WITH_KNOTS('',3,(#51183,#51184,#51185,#51186,#51187,
#51188,#51189,#51190,#51191,#51192,#51193,#51194,#51195,#51196,#51197,#51198,
#51199,#51200,#51201,#51202,#51203,#51204,#51205,#51206,#51207,#51208,#51209,
#51210,#51211,#51212,#51213,#51214,#51215,#51216,#51217,#51218,#51219,#51220,
#51221,#51222,#51223,#51224,#51225,#51226,#51227,#51228,#51229,#51230,#51231,
#51232,#51233,#51234,#51235,#51236,#51237,#51238,#51239,#51240,#51241,#51242,
#51243,#51244,#51245,#51246,#51247,#51248,#51249,#51250,#51251,#51252,#51253,
#51254,#51255,#51256,#51257,#51258,#51259,#51260,#51261,#51262,#51263,#51264,
#51265,#51266,#51267,#51268,#51269,#51270,#51271,#51272,#51273,#51274,#51275,
#51276,#51277,#51278,#51279,#51280,#51281,#51282,#51283,#51284,#51285,#51286,
#51287,#51288,#51289,#51290,#51291,#51292,#51293,#51294,#51295,#51296,#51297,
#51298,#51299,#51300,#51301,#51302,#51303,#51304,#51305,#51306,#51307,#51308,
#51309,#51310,#51311,#51312,#51313,#51314,#51315,#51316,#51317,#51318,#51319,
#51320,#51321,#51322,#51323,#51324,#51325,#51326,#51327,#51328,#51329,#51330,
#51331,#51332,#51333,#51334,#51335,#51336,#51337,#51338,#51339,#51340,#51341,
#51342,#51343,#51344,#51345,#51346,#51347,#51348),.UNSPECIFIED.,.F.,.F.,
(4,3,3,3,3,3,3,3,3,3,3,3,3,3,3,3,3,3,3,3,3,3,3,3,3,3,3,3,3,3,3,3,3,3,3,
3,3,3,3,3,3,3,3,3,3,3,3,3,3,3,3,3,3,3,3,4),(241.902634326415,241.98318016364,
242.062446252954,242.143631964134,242.224817675314,242.304228873793,242.383658498341,
242.463117309291,242.542649132746,242.622222659175,242.70187978314,242.723588865977,
242.801977244985,242.880299509428,242.958570058886,243.03680325543,243.115013433108,
243.193231568491,243.27145763371,243.349704615268,243.427985509483,243.506358937238,
243.584781935561,243.663321494752,243.721131247302,243.797202524938,243.873178301385,
243.949075358377,244.024910397189,244.100700057287,244.177946753704,244.253710251965,
244.329481083332,244.405274251165,244.48362409553,244.559548859041,244.639111243834,
244.718673628627,244.79624384957,244.87372199009,244.951123704003,245.028464590298,
245.105760204192,245.183033643806,245.260296879113,245.33756394655,245.414848882054,
245.4922068844,245.569602415457,245.647104082225,245.716216009951,245.800441773244,
245.885279409835,245.969191086817,246.054491703213,246.139792319609),
 .UNSPECIFIED.);
#3359=B_SPLINE_CURVE_WITH_KNOTS('',3,(#51349,#51350,#51351,#51352,#51353,
#51354,#51355,#51356,#51357,#51358,#51359,#51360,#51361,#51362,#51363,#51364,
#51365,#51366,#51367,#51368,#51369,#51370,#51371,#51372,#51373,#51374,#51375,
#51376,#51377,#51378,#51379,#51380,#51381,#51382,#51383,#51384,#51385,#51386,
#51387,#51388,#51389,#51390,#51391,#51392,#51393,#51394,#51395,#51396,#51397,
#51398,#51399,#51400,#51401,#51402,#51403,#51404,#51405,#51406,#51407,#51408,
#51409,#51410,#51411,#51412,#51413,#51414,#51415,#51416,#51417,#51418,#51419,
#51420,#51421,#51422,#51423,#51424,#51425,#51426,#51427),.UNSPECIFIED.,
 .F.,.F.,(4,3,3,3,3,3,3,3,3,3,3,3,3,3,3,3,3,3,3,3,3,3,3,3,3,3,4),(239.856215740081,
239.935732037462,240.015194933753,240.094616659583,240.17401425183,240.25339823729,
240.332779688537,240.412169675154,240.491611274401,240.57107694136,240.650622166768,
240.728504103327,240.805234681652,240.881898280019,240.958509581247,241.035084347962,
241.111637677356,241.188195075361,241.227275293989,241.311944285607,241.396758737655,
241.481772055892,241.566871471401,241.652090859933,241.726046484652,241.815739306581,
241.902634326327),.UNSPECIFIED.);
#3360=B_SPLINE_CURVE_WITH_KNOTS('',3,(#51429,#51430,#51431,#51432,#51433,
#51434,#51435,#51436,#51437,#51438,#51439,#51440,#51441,#51442,#51443,#51444,
#51445,#51446,#51447,#51448,#51449,#51450,#51451,#51452,#51453,#51454,#51455,
#51456,#51457,#51458,#51459,#51460,#51461,#51462,#51463,#51464,#51465,#51466,
#51467,#51468,#51469,#51470,#51471,#51472,#51473,#51474,#51475,#51476,#51477,
#51478,#51479,#51480,#51481,#51482,#51483,#51484,#51485,#51486,#51487,#51488,
#51489,#51490,#51491,#51492,#51493,#51494,#51495,#51496,#51497,#51498,#51499,
#51500,#51501,#51502,#51503,#51504,#51505,#51506,#51507,#51508,#51509,#51510),
 .UNSPECIFIED.,.F.,.F.,(4,3,3,3,3,3,3,3,3,3,3,3,3,3,3,3,3,3,3,3,3,3,3,3,
3,3,3,4),(239.855770926344,239.934207194177,240.012754847305,240.052238171219,
240.128309448855,240.204285225302,240.280182282294,240.356017321107,240.431806981204,
240.509053677621,240.584817175882,240.660588007249,240.736381175082,240.814731019448,
240.890655782958,240.970218167751,241.049780552544,241.126660567282,241.203448426267,
241.280160407913,241.357969647713,241.434577319922,241.511162590235,241.587740052588,
241.666463621019,241.743095422845,241.822864874578,241.902634326311),
 .UNSPECIFIED.);
#3361=B_SPLINE_CURVE_WITH_KNOTS('',3,(#51511,#51512,#51513,#51514,#51515,
#51516,#51517,#51518,#51519,#51520,#51521,#51522,#51523,#51524,#51525,#51526,
#51527,#51528,#51529,#51530,#51531,#51532,#51533,#51534,#51535,#51536,#51537,
#51538,#51539,#51540,#51541,#51542,#51543,#51544,#51545,#51546,#51547,#51548,
#51549,#51550,#51551,#51552,#51553,#51554,#51555,#51556,#51557,#51558,#51559,
#51560,#51561,#51562,#51563,#51564,#51565,#51566,#51567,#51568,#51569,#51570,
#51571,#51572,#51573,#51574,#51575,#51576,#51577,#51578,#51579,#51580,#51581,
#51582,#51583,#51584,#51585,#51586,#51587,#51588,#51589,#51590,#51591,#51592,
#51593,#51594,#51595,#51596,#51597,#51598,#51599,#51600,#51601,#51602,#51603,
#51604,#51605,#51606,#51607,#51608,#51609,#51610,#51611,#51612,#51613,#51614,
#51615,#51616,#51617,#51618,#51619,#51620,#51621,#51622,#51623,#51624,#51625,
#51626,#51627,#51628,#51629,#51630,#51631,#51632,#51633,#51634,#51635,#51636,
#51637,#51638,#51639,#51640,#51641,#51642,#51643,#51644,#51645,#51646,#51647,
#51648,#51649,#51650,#51651,#51652,#51653,#51654,#51655,#51656,#51657,#51658,
#51659,#51660,#51661,#51662,#51663,#51664,#51665,#51666,#51667,#51668,#51669,
#51670,#51671,#51672,#51673,#51674,#51675,#51676,#51677,#51678,#51679),
 .UNSPECIFIED.,.F.,.F.,(4,3,3,3,3,3,3,3,3,3,3,3,3,3,3,3,3,3,3,3,3,3,3,3,
3,3,3,3,3,3,3,3,3,3,3,3,3,3,3,3,3,3,3,3,3,3,3,3,3,3,3,3,3,3,3,3,4),(241.902634326414,
242.015184170787,242.047322933869,242.131535085329,242.215621113039,242.299502034985,
242.383253821019,242.466791468355,242.546094124532,242.623473890863,242.700872051906,
242.778302394478,242.855819687931,242.933386633905,243.011059925353,243.044865315194,
243.124490503055,243.204042957931,243.283534979719,243.362978821734,243.442386699632,
243.521777133754,243.601158684503,243.680542422309,243.759939417639,243.839390034765,
243.918869054203,243.998421193856,244.042407696519,244.119138274844,244.195801873211,
244.272413174439,244.348987941154,244.425541270549,244.502098668554,244.541178887181,
244.625847878799,244.710662330847,244.795675649084,244.880775064593,244.965994453125,
245.039950077844,245.12150705747,245.202988906437,245.286921996954,245.368249236984,
245.453485252745,245.538721268506,245.618132466985,245.697562091533,245.777020902483,
245.856552725938,245.936126252367,246.015783376331,246.037492459169,246.115887536402,
246.139534544986),.UNSPECIFIED.);
#3362=B_SPLINE_CURVE_WITH_KNOTS('',3,(#51685,#51686,#51687,#51688,#51689,
#51690,#51691,#51692,#51693,#51694,#51695,#51696,#51697,#51698,#51699,#51700,
#51701,#51702,#51703,#51704,#51705,#51706,#51707,#51708,#51709,#51710,#51711,
#51712,#51713,#51714,#51715,#51716,#51717,#51718,#51719,#51720,#51721,#51722,
#51723,#51724,#51725,#51726,#51727,#51728,#51729,#51730,#51731,#51732,#51733,
#51734,#51735,#51736,#51737,#51738,#51739,#51740,#51741,#51742,#51743,#51744,
#51745,#51746,#51747,#51748,#51749,#51750,#51751,#51752,#51753,#51754,#51755,
#51756,#51757,#51758,#51759,#51760,#51761,#51762,#51763,#51764,#51765,#51766,
#51767,#51768,#51769,#51770,#51771,#51772,#51773,#51774,#51775,#51776,#51777,
#51778,#51779,#51780,#51781,#51782,#51783,#51784,#51785,#51786,#51787,#51788,
#51789,#51790,#51791,#51792,#51793,#51794,#51795,#51796,#51797,#51798,#51799,
#51800,#51801,#51802,#51803,#51804,#51805,#51806,#51807,#51808,#51809,#51810,
#51811,#51812,#51813,#51814,#51815,#51816,#51817,#51818,#51819,#51820,#51821,
#51822,#51823,#51824,#51825,#51826,#51827,#51828,#51829,#51830,#51831,#51832,
#51833,#51834,#51835,#51836,#51837,#51838,#51839,#51840,#51841,#51842,#51843,
#51844,#51845,#51846,#51847,#51848,#51849,#51850,#51851,#51852,#51853),
 .UNSPECIFIED.,.F.,.F.,(4,3,3,3,3,3,3,3,3,3,3,3,3,3,3,3,3,3,3,3,3,3,3,3,
3,3,3,3,3,3,3,3,3,3,3,3,3,3,3,3,3,3,3,3,3,3,3,3,3,3,3,3,3,3,3,3,4),(248.185819633594,
248.210071963264,248.294740954883,248.379555406932,248.46456872517,248.54966814068,
248.634887529213,248.708843153926,248.790400133552,248.871881982518,248.955815073036,
249.037142313065,249.122378328827,249.207614344589,249.287025543068,249.366455167616,
249.445913978566,249.525445802022,249.605019328451,249.684676452415,249.706385535251,
249.784773914259,249.863096178701,249.94136672816,250.019599924704,250.097810102381,
250.176028237764,250.254254302983,250.332501284541,250.410782178755,250.48915560651,
250.567578604833,250.646118164024,250.703927916576,250.779999194212,250.855974970659,
250.931872027651,251.007707066464,251.083496726561,251.160743422979,251.23650692124,
251.312277752606,251.38807092044,251.466420764805,251.542345528316,251.621907913108,
251.701470297901,251.779057283285,251.859412540702,251.936804083104,252.014139407901,
252.091432606192,252.168697742376,252.245959341539,252.323219410462,252.40050714282,
252.421899342621),.UNSPECIFIED.);
#3363=B_SPLINE_CURVE_WITH_KNOTS('',3,(#51854,#51855,#51856,#51857,#51858,
#51859,#51860,#51861,#51862,#51863,#51864,#51865,#51866,#51867,#51868,#51869,
#51870,#51871,#51872,#51873,#51874,#51875,#51876,#51877,#51878,#51879,#51880,
#51881,#51882,#51883,#51884,#51885,#51886,#51887,#51888,#51889,#51890,#51891,
#51892,#51893,#51894,#51895,#51896,#51897,#51898,#51899,#51900,#51901,#51902,
#51903,#51904,#51905,#51906,#51907,#51908,#51909,#51910,#51911,#51912,#51913,
#51914,#51915,#51916,#51917,#51918,#51919,#51920,#51921,#51922,#51923,#51924,
#51925,#51926,#51927,#51928,#51929,#51930,#51931,#51932,#51933,#51934,#51935,
#51936,#51937,#51938),.UNSPECIFIED.,.F.,.F.,(4,3,3,3,3,3,3,3,3,3,3,3,3,
3,3,3,3,3,3,3,3,3,3,3,3,3,3,3,4),(246.139792319609,246.214987200614,246.292366966945,
246.369765127988,246.447195470561,246.524712764014,246.602279709988,246.679953001435,
246.713758391276,246.793383579137,246.872936034014,246.952428055801,247.031871897816,
247.111279775714,247.190670209836,247.270051760585,247.349435498391,247.428832493721,
247.508283110847,247.587762130286,247.667314269938,247.711300772601,247.788353016447,
247.865335961784,247.945456879711,248.022341303414,248.099202416832,248.176058884343,
248.185819633493),.UNSPECIFIED.);
#3364=B_SPLINE_CURVE_WITH_KNOTS('',3,(#51940,#51941,#51942,#51943,#51944,
#51945,#51946,#51947,#51948,#51949,#51950,#51951,#51952,#51953,#51954,#51955,
#51956,#51957,#51958,#51959,#51960,#51961,#51962,#51963,#51964,#51965,#51966,
#51967,#51968,#51969,#51970,#51971,#51972,#51973,#51974,#51975,#51976,#51977,
#51978,#51979,#51980,#51981,#51982,#51983,#51984,#51985,#51986,#51987,#51988,
#51989,#51990,#51991,#51992,#51993,#51994,#51995,#51996,#51997,#51998,#51999,
#52000,#52001,#52002,#52003,#52004,#52005,#52006,#52007,#52008,#52009,#52010,
#52011,#52012,#52013,#52014,#52015,#52016,#52017,#52018),.UNSPECIFIED.,
 .F.,.F.,(4,3,3,3,3,3,3,3,3,3,3,3,3,3,3,3,3,3,3,3,3,3,3,3,3,3,4),(246.139534544986,
246.217839679845,246.296097439495,246.374322176552,246.452528218451,246.53074737945,
246.608978389857,246.687234238348,246.765527925682,246.84391506779,246.922355332936,
247.000905501758,247.035034840494,247.11110611813,247.187081894577,247.262978951569,
247.338813990382,247.414603650479,247.491850346897,247.567613845157,247.643384676524,
247.719177844357,247.797527688723,247.873452452233,247.953014837026,248.032577221819,
248.185819633594),.UNSPECIFIED.);
#3365=B_SPLINE_CURVE_WITH_KNOTS('',3,(#52019,#52020,#52021,#52022,#52023,
#52024,#52025,#52026,#52027,#52028,#52029,#52030,#52031,#52032,#52033,#52034,
#52035,#52036,#52037,#52038,#52039,#52040,#52041,#52042,#52043,#52044,#52045,
#52046,#52047,#52048,#52049,#52050,#52051,#52052,#52053,#52054,#52055,#52056,
#52057,#52058,#52059,#52060,#52061,#52062,#52063,#52064,#52065,#52066,#52067,
#52068,#52069,#52070,#52071,#52072,#52073,#52074,#52075,#52076,#52077,#52078,
#52079,#52080,#52081,#52082,#52083,#52084,#52085,#52086,#52087,#52088,#52089,
#52090,#52091,#52092,#52093,#52094,#52095,#52096,#52097,#52098,#52099,#52100,
#52101,#52102,#52103,#52104,#52105,#52106,#52107,#52108,#52109,#52110,#52111,
#52112,#52113,#52114,#52115,#52116,#52117,#52118,#52119,#52120,#52121,#52122,
#52123,#52124,#52125,#52126,#52127,#52128,#52129,#52130,#52131,#52132,#52133,
#52134,#52135,#52136,#52137,#52138,#52139,#52140,#52141,#52142,#52143,#52144,
#52145,#52146,#52147,#52148,#52149,#52150,#52151,#52152,#52153,#52154,#52155,
#52156,#52157,#52158,#52159,#52160,#52161,#52162,#52163,#52164,#52165,#52166,
#52167,#52168,#52169,#52170,#52171,#52172,#52173,#52174,#52175,#52176,#52177,
#52178,#52179,#52180,#52181,#52182,#52183,#52184),.UNSPECIFIED.,.F.,.F.,
(4,3,3,3,3,3,3,3,3,3,3,3,3,3,3,3,3,3,3,3,3,3,3,3,3,3,3,3,3,3,3,3,3,3,3,
3,3,3,3,3,3,3,3,3,3,3,3,3,3,3,3,3,3,3,3,4),(248.185819633673,248.261727296346,
248.337557347104,248.413326582018,248.490425709659,248.566130909788,248.641829363112,
248.717536151477,248.795682014394,248.87148595455,248.950802778847,249.030119603143,
249.114331754604,249.198417782314,249.28229870426,249.366050490294,249.449588137631,
249.528890793806,249.606270560137,249.68366872118,249.761099063753,249.838616357206,
249.91618330318,249.993856594627,250.027661984468,250.107287172329,250.186839627206,
250.266331648994,250.345775491009,250.425183368907,250.50457380303,250.583955353779,
250.663339091584,250.742736086915,250.82218670404,250.901665723479,250.981217863132,
251.025204365793,251.101934944118,251.178598542485,251.255209843713,251.331784610428,
251.408337939822,251.484895337827,251.523975556456,251.608644548074,251.693459000123,
251.778472318361,251.863571733871,251.948791122404,252.022746747118,252.104313318822,
252.185777478726,252.267178306333,252.348500730148,252.422903338315),
 .UNSPECIFIED.);
#3366=B_SPLINE_CURVE_WITH_KNOTS('',3,(#52190,#52191,#52192,#52193,#52194,
#52195,#52196,#52197,#52198,#52199,#52200,#52201,#52202,#52203,#52204,#52205,
#52206,#52207,#52208,#52209,#52210,#52211,#52212,#52213,#52214,#52215,#52216,
#52217,#52218,#52219,#52220,#52221,#52222,#52223,#52224,#52225,#52226,#52227,
#52228,#52229,#52230,#52231,#52232,#52233,#52234,#52235,#52236,#52237,#52238,
#52239,#52240,#52241,#52242,#52243,#52244,#52245,#52246,#52247,#52248,#52249,
#52250,#52251,#52252,#52253,#52254,#52255,#52256,#52257,#52258,#52259,#52260,
#52261,#52262,#52263,#52264,#52265,#52266,#52267,#52268,#52269,#52270,#52271,
#52272,#52273,#52274,#52275,#52276,#52277,#52278,#52279,#52280,#52281,#52282,
#52283,#52284,#52285,#52286,#52287,#52288,#52289,#52290,#52291,#52292,#52293,
#52294,#52295,#52296,#52297,#52298,#52299,#52300,#52301,#52302,#52303,#52304,
#52305,#52306,#52307,#52308,#52309,#52310,#52311,#52312,#52313,#52314,#52315,
#52316,#52317,#52318,#52319,#52320,#52321,#52322,#52323,#52324,#52325,#52326,
#52327,#52328,#52329,#52330,#52331,#52332,#52333,#52334,#52335,#52336,#52337,
#52338,#52339,#52340,#52341,#52342,#52343,#52344,#52345,#52346),
 .UNSPECIFIED.,.F.,.F.,(4,3,3,3,3,3,3,3,3,3,3,3,3,3,3,3,3,3,3,3,3,3,3,3,
3,3,3,3,3,3,3,3,3,3,3,3,3,3,3,3,3,3,3,3,3,3,3,3,3,3,3,3,4),(254.469004947998,
254.551467154099,254.633929011901,254.716390528256,254.798851710014,254.881312564024,
254.963773097136,255.046233316199,255.128693228062,255.211152839574,255.293612157583,
255.376071188936,255.458529940483,255.540988419071,255.623446631547,255.705904584757,
255.788362285551,255.870819740773,255.95327695727,256.03928965233,256.12261445067,
256.205081056261,256.287546817645,256.370011762234,256.452475917442,256.534939310679,
256.617401969351,256.699863920862,256.782325192614,256.864785812007,256.947245806438,
257.029705203302,257.112164029992,257.194622313899,257.277080082412,257.359537362919,
257.443671477686,257.526137476046,257.608601852652,257.691064717147,257.773526179154,
257.855986348273,257.938445334089,258.020903246169,258.106500740298,258.188965477343,
258.271427249729,258.353886495894,258.436343654133,258.518806173215,258.601263844626,
258.683722635818,258.705683199198),.UNSPECIFIED.);
#3367=B_SPLINE_CURVE_WITH_KNOTS('',3,(#52347,#52348,#52349,#52350,#52351,
#52352,#52353,#52354,#52355,#52356,#52357,#52358,#52359,#52360,#52361,#52362,
#52363,#52364,#52365,#52366,#52367,#52368,#52369,#52370,#52371,#52372,#52373,
#52374,#52375,#52376,#52377,#52378,#52379,#52380,#52381,#52382,#52383,#52384,
#52385,#52386,#52387,#52388,#52389,#52390,#52391,#52392,#52393,#52394,#52395,
#52396,#52397,#52398,#52399,#52400,#52401,#52402,#52403,#52404,#52405,#52406,
#52407,#52408,#52409,#52410,#52411,#52412,#52413,#52414,#52415,#52416,#52417,
#52418,#52419,#52420,#52421,#52422,#52423,#52424,#52425,#52426,#52427,#52428),
 .UNSPECIFIED.,.F.,.F.,(4,3,3,3,3,3,3,3,3,3,3,3,3,3,3,3,3,3,3,3,3,3,3,3,
3,3,3,4),(252.421899342621,252.49926775373,252.576677654447,252.654187664594,
252.699012679226,252.783224830687,252.867310858397,252.951191780343,253.034943566377,
253.118481213714,253.197783869888,253.275163636219,253.352561797262,253.429992139835,
253.507509433288,253.585076379262,253.662749670709,253.696555060551,253.775214607533,
253.853797534827,253.932306748353,254.010773496424,254.089210548492,254.167630654032,
254.246065414596,254.324505545484,254.402994321971,254.468741656967),
 .UNSPECIFIED.);
#3368=B_SPLINE_CURVE_WITH_KNOTS('',3,(#52430,#52431,#52432,#52433,#52434,
#52435,#52436,#52437,#52438,#52439,#52440,#52441,#52442,#52443,#52444,#52445,
#52446,#52447,#52448,#52449,#52450,#52451,#52452,#52453,#52454,#52455,#52456,
#52457,#52458,#52459,#52460,#52461,#52462,#52463,#52464,#52465,#52466,#52467,
#52468,#52469,#52470,#52471,#52472,#52473,#52474,#52475,#52476,#52477,#52478,
#52479,#52480,#52481,#52482,#52483,#52484,#52485,#52486,#52487,#52488,#52489,
#52490,#52491,#52492,#52493,#52494,#52495,#52496,#52497,#52498,#52499,#52500,
#52501,#52502,#52503,#52504,#52505,#52506,#52507,#52508,#52509,#52510,#52511,
#52512,#52513,#52514),.UNSPECIFIED.,.F.,.F.,(4,3,3,3,3,3,3,3,3,3,3,3,3,
3,3,3,3,3,3,3,3,3,3,3,3,3,3,3,4),(252.422903338315,252.504122891163,252.521517937781,
252.60092913626,252.680358760809,252.759817571759,252.839349395215,252.918922921644,
252.998580045609,253.020289128443,253.098677507451,253.176999771893,253.255270321351,
253.333503517895,253.411713695572,253.489931830955,253.568157896175,253.646404877732,
253.724685771947,253.803059199701,253.881482198025,253.960021757215,254.017831509768,
254.099160682654,254.18032212957,254.261253618944,254.342049835182,254.422661110171,
254.469004940773),.UNSPECIFIED.);
#3369=B_SPLINE_CURVE_WITH_KNOTS('',3,(#52515,#52516,#52517,#52518,#52519,
#52520,#52521,#52522,#52523,#52524,#52525,#52526,#52527,#52528,#52529,#52530,
#52531,#52532,#52533,#52534,#52535,#52536,#52537,#52538,#52539,#52540,#52541,
#52542,#52543,#52544,#52545,#52546,#52547,#52548,#52549,#52550,#52551,#52552,
#52553,#52554,#52555,#52556,#52557,#52558,#52559,#52560,#52561,#52562,#52563,
#52564,#52565,#52566,#52567,#52568,#52569,#52570,#52571,#52572,#52573,#52574,
#52575,#52576,#52577,#52578,#52579,#52580,#52581,#52582,#52583,#52584,#52585,
#52586,#52587,#52588,#52589,#52590,#52591,#52592,#52593,#52594,#52595,#52596,
#52597,#52598,#52599,#52600,#52601,#52602,#52603,#52604,#52605,#52606,#52607,
#52608,#52609,#52610,#52611,#52612,#52613,#52614,#52615,#52616,#52617,#52618,
#52619,#52620,#52621,#52622,#52623,#52624,#52625,#52626,#52627,#52628,#52629,
#52630,#52631,#52632,#52633,#52634,#52635,#52636,#52637,#52638,#52639,#52640,
#52641,#52642,#52643,#52644,#52645,#52646,#52647,#52648,#52649,#52650,#52651,
#52652,#52653,#52654,#52655,#52656,#52657,#52658,#52659,#52660,#52661,#52662,
#52663,#52664,#52665,#52666,#52667,#52668,#52669,#52670,#52671),
 .UNSPECIFIED.,.F.,.F.,(4,3,3,3,3,3,3,3,3,3,3,3,3,3,3,3,3,3,3,3,3,3,3,3,
3,3,3,3,3,3,3,3,3,3,3,3,3,3,3,3,3,3,3,3,3,3,3,3,3,3,3,3,4),(254.469004940774,
254.551467146874,254.633929004677,254.716390521032,254.79885170279,254.8813125568,
254.963773089912,255.046233308975,255.128693220838,255.21115283235,255.293612150359,
255.376071181713,255.45852993326,255.540988411847,255.623446624323,255.705904577533,
255.788362278326,255.870819733548,255.953276950046,256.039289645332,256.12261444389,
256.205081049482,256.287546810865,256.370011755455,256.452475910663,256.5349393039,
256.617401962571,256.699863914082,256.782325185835,256.864785805228,256.947245799659,
257.029705196523,257.112164023213,257.194622307121,257.277080075634,257.35953735614,
257.443671471331,257.526137469691,257.608601846297,257.691064710793,257.773526172799,
257.855986341918,257.938445327734,258.020903239815,258.106500734737,258.188965471783,
258.27142724417,258.353886490335,258.436343648574,258.518806167656,258.601263839067,
258.68372263026,258.705683199198),.UNSPECIFIED.);
#3370=B_SPLINE_CURVE_WITH_KNOTS('',3,(#52677,#52678,#52679,#52680,#52681,
#52682,#52683,#52684,#52685,#52686,#52687,#52688,#52689,#52690,#52691,#52692,
#52693,#52694,#52695,#52696,#52697,#52698,#52699,#52700,#52701,#52702,#52703,
#52704,#52705,#52706,#52707,#52708,#52709,#52710,#52711,#52712,#52713,#52714,
#52715,#52716,#52717,#52718,#52719,#52720,#52721,#52722,#52723,#52724,#52725,
#52726,#52727,#52728,#52729,#52730,#52731,#52732,#52733,#52734,#52735,#52736,
#52737,#52738,#52739,#52740,#52741,#52742,#52743,#52744,#52745,#52746,#52747,
#52748,#52749,#52750,#52751,#52752,#52753,#52754,#52755,#52756,#52757,#52758,
#52759,#52760,#52761,#52762,#52763,#52764,#52765,#52766,#52767,#52768,#52769,
#52770,#52771,#52772,#52773,#52774,#52775,#52776,#52777,#52778,#52779,#52780,
#52781,#52782,#52783,#52784,#52785,#52786,#52787,#52788,#52789,#52790,#52791,
#52792,#52793,#52794,#52795,#52796,#52797,#52798,#52799,#52800,#52801,#52802,
#52803,#52804,#52805,#52806,#52807,#52808,#52809,#52810,#52811,#52812,#52813,
#52814,#52815,#52816,#52817,#52818,#52819,#52820,#52821,#52822,#52823,#52824,
#52825,#52826,#52827,#52828,#52829,#52830,#52831,#52832,#52833,#52834,#52835,
#52836,#52837,#52838,#52839,#52840,#52841,#52842,#52843,#52844,#52845),
 .UNSPECIFIED.,.F.,.F.,(4,3,3,3,3,3,3,3,3,3,3,3,3,3,3,3,3,3,3,3,3,3,3,3,
3,3,3,3,3,3,3,3,3,3,3,3,3,3,3,3,3,3,3,3,3,3,3,3,3,3,3,3,3,3,3,3,4),(260.752196538802,
260.830967913365,260.909662513798,260.988294308136,261.066877218579,261.145427802033,
261.223961216436,261.302490027466,261.381026795821,261.459615390821,261.538230451882,
261.616925325411,261.67689411115,261.753624689475,261.830288287842,261.906899589071,
261.983474355786,262.06002768518,262.136585083185,262.175665301812,262.26033429343,
262.345148745477,262.430162063714,262.515261479224,262.600480867756,262.674436492475,
262.755993472102,262.837475321068,262.921408411586,263.002735651616,263.087971667376,
263.173207683137,263.252618881615,263.332048506163,263.411507317113,263.491039140568,
263.570612666997,263.650269790961,263.6719788738,263.750367252808,263.82868951725,
263.906960066709,263.985193263253,264.06340344093,264.141621576313,264.219847641533,
264.29809462309,264.376375517305,264.454748945059,264.533171943383,264.611711502573,
264.669521255124,264.74957128564,264.825540665302,264.901440764819,264.977274285402,
264.989721377187),.UNSPECIFIED.);
#3371=B_SPLINE_CURVE_WITH_KNOTS('',3,(#52846,#52847,#52848,#52849,#52850,
#52851,#52852,#52853,#52854,#52855,#52856,#52857,#52858,#52859,#52860,#52861,
#52862,#52863,#52864,#52865,#52866,#52867,#52868,#52869,#52870,#52871,#52872,
#52873,#52874,#52875,#52876,#52877,#52878,#52879,#52880,#52881,#52882,#52883,
#52884,#52885,#52886,#52887,#52888,#52889,#52890,#52891,#52892,#52893,#52894,
#52895,#52896,#52897,#52898,#52899,#52900,#52901,#52902,#52903,#52904,#52905,
#52906,#52907,#52908,#52909,#52910,#52911,#52912,#52913,#52914,#52915,#52916,
#52917,#52918,#52919,#52920,#52921),.UNSPECIFIED.,.F.,.F.,(4,3,3,3,3,3,
3,3,3,3,3,3,3,3,3,3,3,3,3,3,3,3,3,3,3,4),(258.705683199198,258.788144802928,
258.87060574078,258.953066040152,259.03552572844,259.117984833038,259.200443381339,
259.282901400731,259.365358918604,259.452035876688,259.534502662229,259.616967775297,
259.699431325545,259.781893422604,259.864354176086,259.946813695582,260.029272090667,
260.111729470901,260.194195856587,260.276659058095,260.359119513945,260.4415776625,
260.524043266253,260.606503144641,260.688967255893,260.752190247953),
 .UNSPECIFIED.);
#3372=B_SPLINE_CURVE_WITH_KNOTS('',3,(#52923,#52924,#52925,#52926,#52927,
#52928,#52929,#52930,#52931,#52932,#52933,#52934,#52935,#52936,#52937,#52938,
#52939,#52940,#52941,#52942,#52943,#52944,#52945,#52946,#52947,#52948,#52949,
#52950,#52951,#52952,#52953,#52954,#52955,#52956,#52957,#52958,#52959,#52960,
#52961,#52962,#52963,#52964,#52965,#52966,#52967,#52968,#52969,#52970,#52971,
#52972,#52973,#52974,#52975,#52976,#52977,#52978,#52979,#52980,#52981,#52982,
#52983,#52984,#52985,#52986,#52987,#52988,#52989,#52990,#52991,#52992,#52993,
#52994,#52995,#52996,#52997,#52998),.UNSPECIFIED.,.F.,.F.,(4,3,3,3,3,3,
3,3,3,3,3,3,3,3,3,3,3,3,3,3,3,3,3,3,3,4),(258.705683199198,258.788144802928,
258.87060574078,258.953066040152,259.03552572844,259.117984833038,259.200443381339,
259.282901400731,259.365358918604,259.452035876688,259.534502662229,259.616967775297,
259.699431325545,259.781893422605,259.864354176086,259.946813695582,260.029272090667,
260.111729470901,260.194195856587,260.276659058095,260.359119513945,260.441577662499,
260.524043266253,260.606503144641,260.688967255893,260.752190247953),
 .UNSPECIFIED.);
#3373=B_SPLINE_CURVE_WITH_KNOTS('',3,(#52999,#53000,#53001,#53002,#53003,
#53004,#53005,#53006,#53007,#53008,#53009,#53010,#53011,#53012,#53013,#53014,
#53015,#53016,#53017,#53018,#53019,#53020,#53021,#53022,#53023,#53024,#53025,
#53026,#53027,#53028,#53029,#53030,#53031,#53032,#53033,#53034,#53035,#53036,
#53037,#53038,#53039,#53040,#53041,#53042,#53043,#53044,#53045,#53046,#53047,
#53048,#53049,#53050,#53051,#53052,#53053,#53054,#53055,#53056,#53057,#53058,
#53059,#53060,#53061,#53062,#53063,#53064,#53065,#53066,#53067,#53068,#53069,
#53070,#53071,#53072,#53073,#53074,#53075,#53076,#53077,#53078,#53079,#53080,
#53081,#53082,#53083,#53084,#53085,#53086,#53087,#53088,#53089,#53090,#53091,
#53092,#53093,#53094,#53095,#53096,#53097,#53098,#53099,#53100,#53101,#53102,
#53103,#53104,#53105,#53106,#53107,#53108,#53109,#53110,#53111,#53112,#53113,
#53114,#53115,#53116,#53117,#53118,#53119,#53120,#53121,#53122,#53123,#53124,
#53125,#53126,#53127,#53128,#53129,#53130,#53131,#53132,#53133,#53134,#53135,
#53136,#53137,#53138,#53139,#53140,#53141,#53142,#53143,#53144,#53145,#53146,
#53147,#53148,#53149,#53150,#53151,#53152,#53153,#53154,#53155,#53156,#53157,
#53158,#53159,#53160,#53161,#53162,#53163,#53164),.UNSPECIFIED.,.F.,.F.,
(4,3,3,3,3,3,3,3,3,3,3,3,3,3,3,3,3,3,3,3,3,3,3,3,3,3,3,3,3,3,3,3,3,3,3,
3,3,3,3,3,3,3,3,3,3,3,3,3,3,3,3,3,3,3,3,4),(260.752190247953,260.861381773017,
260.975984016104,261.000628179042,261.076699456678,261.152675233125,261.228572290117,
261.30440732893,261.380196989027,261.457443685445,261.533207183705,261.608978015072,
261.684771182906,261.763121027271,261.839045790782,261.918608175574,261.998170560367,
262.07574078131,262.15321892183,262.230620635743,262.307961522038,262.385257135933,
262.462530575547,262.539793810854,262.61706087829,262.694345813794,262.771703816141,
262.849099347198,262.926601013965,262.995712941692,263.079925093153,263.164011120863,
263.247892042809,263.331643828844,263.41518147618,263.494484132354,263.571863898685,
263.649262059728,263.726692402301,263.804209695754,263.881776641728,263.959449933175,
263.993255323017,264.072880574431,264.152433079837,264.231925139183,264.31136900583,
264.390776895467,264.470167265223,264.549548734105,264.628932372527,264.708329250924,
264.787779482255,264.867258113544,264.946809269139,264.989216780594),
 .UNSPECIFIED.);
#3374=B_SPLINE_CURVE_WITH_KNOTS('',3,(#53170,#53171,#53172,#53173,#53174,
#53175,#53176,#53177,#53178,#53179,#53180,#53181,#53182,#53183,#53184,#53185,
#53186,#53187,#53188,#53189,#53190,#53191,#53192,#53193,#53194,#53195,#53196,
#53197,#53198,#53199,#53200,#53201,#53202,#53203,#53204,#53205,#53206,#53207,
#53208,#53209,#53210,#53211,#53212,#53213,#53214,#53215,#53216,#53217,#53218,
#53219,#53220,#53221,#53222,#53223,#53224,#53225,#53226,#53227,#53228,#53229,
#53230,#53231,#53232,#53233,#53234,#53235,#53236,#53237,#53238,#53239,#53240,
#53241,#53242,#53243,#53244,#53245,#53246,#53247,#53248,#53249,#53250,#53251,
#53252,#53253,#53254,#53255,#53256,#53257,#53258,#53259,#53260,#53261,#53262,
#53263,#53264,#53265,#53266,#53267,#53268,#53269,#53270,#53271,#53272,#53273,
#53274,#53275,#53276,#53277,#53278,#53279,#53280,#53281,#53282,#53283,#53284,
#53285,#53286,#53287,#53288,#53289,#53290,#53291,#53292,#53293,#53294,#53295,
#53296,#53297,#53298,#53299,#53300,#53301,#53302,#53303,#53304,#53305,#53306,
#53307,#53308,#53309,#53310,#53311,#53312,#53313,#53314,#53315,#53316,#53317,
#53318,#53319,#53320,#53321,#53322,#53323,#53324,#53325,#53326,#53327,#53328,
#53329,#53330,#53331,#53332,#53333,#53334,#53335,#53336,#53337,#53338),
 .UNSPECIFIED.,.F.,.F.,(4,3,3,3,3,3,3,3,3,3,3,3,3,3,3,3,3,3,3,3,3,3,3,3,
3,3,3,3,3,3,3,3,3,3,3,3,3,3,3,3,3,3,3,3,3,3,3,3,3,3,3,3,3,3,3,3,4),(267.035375555133,
267.111715052275,267.163377208437,267.240756974768,267.318155135812,267.395585478384,
267.473102771837,267.550669717811,267.628343009258,267.662148399099,267.74177358696,
267.821326041836,267.900818063625,267.98026190564,268.059669783537,268.139060217659,
268.218441768408,268.297825506214,268.377222501545,268.45667311867,268.536152138109,
268.615704277761,268.659690780424,268.73642135875,268.813084957116,268.889696258344,
268.966271025059,269.042824354454,269.119381752459,269.158461971086,269.243130962704,
269.327945414752,269.412958732989,269.498058148498,269.58327753703,269.657233161749,
269.738790141376,269.820271990342,269.904205080859,269.985532320889,270.07076833665,
270.156004352411,270.23541555089,270.314845175438,270.394303986388,270.473835809843,
270.553409336272,270.633066460236,270.654775543074,270.733157031107,270.811476038419,
270.889745625621,270.967978821928,271.046197558055,271.124405445832,271.202637380801,
271.271644794101),.UNSPECIFIED.);
#3375=B_SPLINE_CURVE_WITH_KNOTS('',3,(#53339,#53340,#53341,#53342,#53343,
#53344,#53345,#53346,#53347,#53348,#53349,#53350,#53351,#53352,#53353,#53354,
#53355,#53356,#53357,#53358,#53359,#53360,#53361,#53362,#53363,#53364,#53365,
#53366,#53367,#53368,#53369,#53370,#53371,#53372,#53373,#53374,#53375,#53376,
#53377,#53378,#53379,#53380,#53381,#53382,#53383,#53384,#53385,#53386,#53387,
#53388,#53389,#53390,#53391,#53392,#53393,#53394,#53395,#53396,#53397,#53398,
#53399,#53400,#53401,#53402,#53403,#53404,#53405,#53406,#53407,#53408,#53409,
#53410,#53411,#53412,#53413,#53414,#53415,#53416,#53417,#53418,#53419,#53420),
 .UNSPECIFIED.,.F.,.F.,(4,3,3,3,3,3,3,3,3,3,3,3,3,3,3,3,3,3,3,3,3,3,3,3,
3,3,3,4),(264.989721377187,265.065503395217,265.141271860983,265.217035617893,
265.292809664754,265.368609007136,265.444496684426,265.520429859431,265.596486860221,
265.667063636449,265.744633857392,265.822111997912,265.899513711826,265.976854598122,
266.054150212016,266.13142365163,266.208686886937,266.285953954373,266.363238889877,
266.440596892224,266.517992423281,266.595494090048,266.664606017774,266.757298402093,
266.84637076419,266.93517428811,267.023523487286,267.035375555049),
 .UNSPECIFIED.);
#3376=B_SPLINE_CURVE_WITH_KNOTS('',3,(#53422,#53423,#53424,#53425,#53426,
#53427,#53428,#53429,#53430,#53431,#53432,#53433,#53434,#53435,#53436,#53437,
#53438,#53439,#53440,#53441,#53442,#53443,#53444,#53445,#53446,#53447,#53448,
#53449,#53450,#53451,#53452,#53453,#53454,#53455,#53456,#53457,#53458,#53459,
#53460,#53461,#53462,#53463,#53464,#53465,#53466,#53467,#53468,#53469,#53470,
#53471,#53472,#53473,#53474,#53475,#53476,#53477,#53478,#53479,#53480,#53481,
#53482,#53483,#53484,#53485,#53486,#53487,#53488,#53489,#53490,#53491,#53492,
#53493,#53494,#53495,#53496,#53497,#53498,#53499,#53500,#53501,#53502,#53503,
#53504,#53505,#53506),.UNSPECIFIED.,.F.,.F.,(4,3,3,3,3,3,3,3,3,3,3,3,3,
3,3,3,3,3,3,3,3,3,3,3,3,3,3,3,4),(264.989216780594,264.990797704342,265.067528282667,
265.144191881034,265.220803182262,265.297377948977,265.373931278371,265.450488676376,
265.489568895004,265.574237886622,265.65905233867,265.744065656907,265.829165072416,
265.914384460948,265.988340085667,266.069897065294,266.15137891426,266.235312004777,
266.316639244808,266.401875260568,266.487111276329,266.566522474807,266.645952099355,
266.725410910304,266.804942733759,266.884516260188,266.964173384152,266.985882466992,
267.035375555133),.UNSPECIFIED.);
#3377=B_SPLINE_CURVE_WITH_KNOTS('',3,(#53507,#53508,#53509,#53510,#53511,
#53512,#53513,#53514,#53515,#53516,#53517,#53518,#53519,#53520,#53521,#53522,
#53523,#53524,#53525,#53526,#53527,#53528,#53529,#53530,#53531,#53532,#53533,
#53534,#53535,#53536,#53537,#53538,#53539,#53540,#53541,#53542,#53543,#53544,
#53545,#53546,#53547,#53548,#53549,#53550,#53551,#53552,#53553,#53554,#53555,
#53556,#53557,#53558,#53559,#53560,#53561,#53562,#53563,#53564,#53565,#53566,
#53567,#53568,#53569,#53570,#53571,#53572,#53573,#53574,#53575,#53576,#53577,
#53578,#53579,#53580,#53581,#53582,#53583,#53584,#53585,#53586,#53587,#53588,
#53589,#53590,#53591,#53592,#53593,#53594,#53595,#53596,#53597,#53598,#53599,
#53600,#53601,#53602,#53603,#53604,#53605,#53606,#53607,#53608,#53609,#53610,
#53611,#53612,#53613,#53614,#53615,#53616,#53617,#53618,#53619,#53620,#53621,
#53622,#53623,#53624,#53625,#53626,#53627,#53628,#53629,#53630,#53631,#53632,
#53633,#53634,#53635,#53636,#53637,#53638,#53639,#53640,#53641,#53642,#53643,
#53644,#53645,#53646,#53647,#53648,#53649,#53650,#53651,#53652,#53653,#53654,
#53655,#53656,#53657,#53658,#53659,#53660,#53661,#53662,#53663,#53664,#53665,
#53666,#53667,#53668,#53669,#53670,#53671,#53672,#53673,#53674,#53675),
 .UNSPECIFIED.,.F.,.F.,(4,3,3,3,3,3,3,3,3,3,3,3,3,3,3,3,3,3,3,3,3,3,3,3,
3,3,3,3,3,3,3,3,3,3,3,3,3,3,3,3,3,3,3,3,3,3,3,3,3,3,3,3,3,3,3,3,4),(267.035375555213,
267.113312000005,267.191183295891,267.269004458145,267.346790466105,267.426369763881,
267.504146913764,267.581936059632,267.659750746375,267.74066927186,267.818616933769,
267.896620423716,267.974726358261,267.983424848316,268.059496125952,268.135471902399,
268.211368959391,268.287203998204,268.362993658301,268.440240354718,268.516003852979,
268.591774684346,268.66756785218,268.745917696545,268.821842460055,268.901404844848,
268.980967229641,269.058537450584,269.136015591105,269.213417305018,269.290758191313,
269.368053805207,269.445327244821,269.522590480128,269.599857547566,269.677142483069,
269.754500485416,269.831896016473,269.90939768324,269.978509610966,270.062721762427,
270.146807790137,270.230688712083,270.314440498118,270.397978145454,270.477280801629,
270.55466056796,270.632058729003,270.709489071576,270.787006365029,270.864573311003,
270.94224660245,270.976051992291,271.055670219224,271.135224360004,271.214711332198,
271.272349559382),.UNSPECIFIED.);
#3378=B_SPLINE_CURVE_WITH_KNOTS('',3,(#53681,#53682,#53683,#53684,#53685,
#53686,#53687,#53688,#53689,#53690,#53691,#53692,#53693,#53694,#53695,#53696,
#53697,#53698,#53699,#53700,#53701,#53702,#53703,#53704,#53705,#53706,#53707,
#53708,#53709,#53710,#53711,#53712,#53713,#53714,#53715,#53716,#53717,#53718,
#53719,#53720,#53721,#53722,#53723,#53724,#53725,#53726,#53727,#53728,#53729,
#53730,#53731,#53732,#53733,#53734,#53735,#53736,#53737,#53738,#53739,#53740,
#53741,#53742,#53743,#53744,#53745,#53746,#53747,#53748,#53749,#53750,#53751,
#53752,#53753,#53754,#53755,#53756,#53757,#53758,#53759,#53760,#53761,#53762,
#53763,#53764,#53765,#53766,#53767,#53768,#53769,#53770,#53771,#53772,#53773,
#53774,#53775,#53776,#53777,#53778,#53779,#53780,#53781,#53782,#53783,#53784,
#53785,#53786,#53787,#53788,#53789,#53790,#53791,#53792,#53793,#53794,#53795,
#53796,#53797,#53798,#53799,#53800,#53801,#53802,#53803,#53804,#53805,#53806,
#53807,#53808,#53809,#53810,#53811,#53812,#53813,#53814,#53815,#53816,#53817,
#53818,#53819,#53820,#53821,#53822,#53823,#53824,#53825,#53826,#53827,#53828,
#53829,#53830,#53831,#53832,#53833,#53834,#53835,#53836,#53837,#53838,#53839,
#53840,#53841,#53842,#53843,#53844,#53845,#53846),.UNSPECIFIED.,.F.,.F.,
(4,3,3,3,3,3,3,3,3,3,3,3,3,3,3,3,3,3,3,3,3,3,3,3,3,3,3,3,3,3,3,3,3,3,3,
3,3,3,3,3,3,3,3,3,3,3,3,3,3,3,3,3,3,3,3,4),(273.318560862442,273.405000238929,
273.491718545237,273.578829877679,273.647402687048,273.731614838509,273.815700866218,
273.899581788165,273.983333574198,274.066871221535,274.146173877711,274.223553644042,
274.300951805085,274.378382147658,274.45589944111,274.533466387085,274.611139678532,
274.644945068373,274.724570256234,274.804122711111,274.883614732899,274.963058574914,
275.042466452812,275.121856886934,275.201238437683,275.280622175489,275.360019170819,
275.439469787945,275.518948807384,275.598500947036,275.642487449698,275.719218028023,
275.79588162639,275.872492927618,275.949067694333,276.025621023727,276.102178421732,
276.141258640361,276.225927631979,276.310742084028,276.395755402266,276.480854817776,
276.566074206309,276.640029831023,276.721586810649,276.803068659615,276.887001750133,
276.968328990162,277.053565005924,277.138801021686,277.218206203887,277.297628934143,
277.37710710278,277.456616972324,277.536195134398,277.55504144039),
 .UNSPECIFIED.);
#3379=B_SPLINE_CURVE_WITH_KNOTS('',3,(#53847,#53848,#53849,#53850,#53851,
#53852,#53853,#53854,#53855,#53856,#53857,#53858,#53859,#53860,#53861,#53862,
#53863,#53864,#53865,#53866,#53867,#53868,#53869,#53870,#53871,#53872,#53873,
#53874,#53875,#53876,#53877,#53878,#53879,#53880,#53881,#53882,#53883,#53884,
#53885,#53886,#53887,#53888,#53889,#53890,#53891,#53892,#53893,#53894,#53895,
#53896,#53897,#53898,#53899,#53900,#53901,#53902,#53903,#53904,#53905,#53906,
#53907,#53908,#53909,#53910,#53911,#53912,#53913,#53914,#53915,#53916,#53917,
#53918,#53919,#53920,#53921,#53922,#53923,#53924,#53925,#53926,#53927,#53928),
 .UNSPECIFIED.,.F.,.F.,(4,3,3,3,3,3,3,3,3,3,3,3,3,3,3,3,3,3,3,3,3,3,3,3,
3,3,3,4),(271.271644794101,271.34992100394,271.428289355457,271.506705887669,
271.585241659055,271.652317924399,271.728389202035,271.804364978482,271.880262035474,
271.956097074287,272.031886734384,272.109133430802,272.184896929063,272.260667760429,
272.336460928263,272.414810772628,272.490735536139,272.570297920931,272.649860305724,
272.72846319729,272.806929470045,272.885314382992,272.963630897435,273.041891931622,
273.120107163257,273.198295155157,273.276474989067,273.318560862312),
 .UNSPECIFIED.);
#3380=B_SPLINE_CURVE_WITH_KNOTS('',3,(#53930,#53931,#53932,#53933,#53934,
#53935,#53936,#53937,#53938,#53939,#53940,#53941,#53942,#53943,#53944,#53945,
#53946,#53947,#53948,#53949,#53950,#53951,#53952,#53953,#53954,#53955,#53956,
#53957,#53958,#53959,#53960,#53961,#53962,#53963,#53964,#53965,#53966,#53967,
#53968,#53969,#53970,#53971,#53972,#53973,#53974,#53975,#53976,#53977,#53978,
#53979,#53980,#53981,#53982,#53983,#53984,#53985,#53986,#53987,#53988,#53989,
#53990,#53991,#53992,#53993,#53994,#53995,#53996,#53997,#53998,#53999,#54000,
#54001,#54002,#54003,#54004,#54005,#54006,#54007,#54008,#54009,#54010,#54011),
 .UNSPECIFIED.,.F.,.F.,(4,3,3,3,3,3,3,3,3,3,3,3,3,3,3,3,3,3,3,3,3,3,3,3,
3,3,3,4),(271.272349559382,271.351766100178,271.431160912595,271.510543800256,
271.589925834822,271.669318086045,271.748762684496,271.828232893785,271.907780304428,
271.973594373616,272.050324951941,272.126988550308,272.203599851536,272.280174618251,
272.356727947646,272.433285345651,272.472365564278,272.557034555896,272.641849007944,
272.726862326181,272.811961741691,272.897181130223,272.971136754941,273.057992781784,
273.14141558143,273.224751553311,273.307968176738,273.318560862312),
 .UNSPECIFIED.);
#3381=B_SPLINE_CURVE_WITH_KNOTS('',3,(#54012,#54013,#54014,#54015,#54016,
#54017,#54018,#54019,#54020,#54021,#54022,#54023,#54024,#54025,#54026,#54027,
#54028,#54029,#54030,#54031,#54032,#54033,#54034,#54035,#54036,#54037,#54038,
#54039,#54040,#54041,#54042,#54043,#54044,#54045,#54046,#54047,#54048,#54049,
#54050,#54051,#54052,#54053,#54054,#54055,#54056,#54057,#54058,#54059,#54060,
#54061,#54062,#54063,#54064,#54065,#54066,#54067,#54068,#54069,#54070,#54071,
#54072,#54073,#54074,#54075,#54076,#54077,#54078,#54079,#54080,#54081,#54082,
#54083,#54084,#54085,#54086,#54087,#54088,#54089,#54090,#54091,#54092,#54093,
#54094,#54095,#54096,#54097,#54098,#54099,#54100,#54101,#54102,#54103,#54104,
#54105,#54106,#54107,#54108,#54109,#54110,#54111,#54112,#54113,#54114,#54115,
#54116,#54117,#54118,#54119,#54120,#54121,#54122,#54123,#54124,#54125,#54126,
#54127,#54128,#54129,#54130,#54131,#54132,#54133,#54134,#54135,#54136,#54137,
#54138,#54139,#54140,#54141,#54142,#54143,#54144,#54145,#54146,#54147,#54148,
#54149,#54150,#54151,#54152,#54153,#54154,#54155,#54156,#54157,#54158,#54159,
#54160,#54161,#54162,#54163,#54164,#54165,#54166,#54167,#54168),
 .UNSPECIFIED.,.F.,.F.,(4,3,3,3,3,3,3,3,3,3,3,3,3,3,3,3,3,3,3,3,3,3,3,3,
3,3,3,3,3,3,3,3,3,3,3,3,3,3,3,3,3,3,3,3,3,3,3,3,3,3,3,3,4),(273.318560862312,
273.401023068412,273.483484926215,273.56594644257,273.648407624328,273.730868478338,
273.81332901145,273.895789230513,273.978249142376,274.060708753888,274.143168071897,
274.22562710325,274.308085854797,274.390544333385,274.473002545861,274.555460499071,
274.637918199864,274.720375655086,274.802832871584,274.88884556687,274.972170365428,
275.05463697102,275.137102732403,275.219567676993,275.302031832201,275.384495225438,
275.46695788411,275.549419835621,275.631881107373,275.714341726766,275.796801721197,
275.879261118062,275.961719944752,276.044178228659,276.126635997172,276.209093277678,
276.293227392869,276.375693391229,276.458157767836,276.540620632331,276.623082094337,
276.705542263457,276.788001249273,276.870459161353,276.956056656276,277.038521393322,
277.120983165708,277.203442411873,277.285899570112,277.368362089195,277.450819760606,
277.533278551799,277.555239120736),.UNSPECIFIED.);
#3382=B_SPLINE_CURVE_WITH_KNOTS('',3,(#54174,#54175,#54176,#54177,#54178,
#54179,#54180,#54181,#54182,#54183,#54184,#54185,#54186,#54187,#54188,#54189,
#54190,#54191,#54192,#54193,#54194,#54195,#54196,#54197,#54198,#54199,#54200,
#54201,#54202,#54203,#54204,#54205,#54206,#54207,#54208,#54209,#54210,#54211,
#54212,#54213,#54214,#54215,#54216,#54217,#54218,#54219,#54220,#54221,#54222,
#54223,#54224,#54225,#54226,#54227,#54228,#54229,#54230,#54231,#54232,#54233,
#54234,#54235,#54236,#54237,#54238,#54239,#54240,#54241,#54242,#54243,#54244,
#54245,#54246,#54247,#54248,#54249,#54250,#54251,#54252,#54253,#54254,#54255,
#54256,#54257,#54258,#54259,#54260,#54261,#54262,#54263,#54264,#54265,#54266,
#54267,#54268,#54269,#54270,#54271,#54272,#54273,#54274,#54275,#54276,#54277,
#54278,#54279,#54280,#54281,#54282,#54283,#54284,#54285,#54286,#54287,#54288,
#54289,#54290,#54291,#54292,#54293,#54294,#54295,#54296,#54297,#54298,#54299,
#54300,#54301,#54302,#54303,#54304,#54305,#54306,#54307,#54308,#54309,#54310,
#54311,#54312,#54313,#54314,#54315,#54316,#54317,#54318,#54319,#54320,#54321,
#54322,#54323,#54324,#54325,#54326,#54327,#54328,#54329,#54330,#54331,#54332,
#54333,#54334,#54335,#54336,#54337,#54338,#54339,#54340,#54341,#54342),
 .UNSPECIFIED.,.F.,.F.,(4,3,3,3,3,3,3,3,3,3,3,3,3,3,3,3,3,3,3,3,3,3,3,3,
3,3,3,3,3,3,3,3,3,3,3,3,3,3,3,3,3,3,3,3,3,3,3,3,3,3,3,3,3,3,3,3,4),(279.601746169492,
279.632656974998,279.710227195941,279.787705336461,279.865107050374,279.942447936669,
280.019743550563,280.097016990177,280.174280225484,280.251547292921,280.328832228425,
280.406190230771,280.483585761829,280.561087428595,280.630199356323,280.714411507784,
280.798497535494,280.882378457441,280.966130243475,281.049667890812,281.128970546985,
281.206350313315,281.283748474359,281.361178816931,281.438696110384,281.516263056358,
281.593936347805,281.627741737648,281.707366925509,281.786919380386,281.866411402174,
281.945855244189,282.025263122087,282.104653556209,282.184035106958,282.263418844764,
282.342815840095,282.422266457221,282.501745476659,282.581297616312,282.625284118972,
282.702014697297,282.778678295663,282.855289596891,282.931864363606,283.008417693,
283.084975091004,283.124055309635,283.208724301254,283.293538753303,283.378552071541,
283.463651487051,283.548870875584,283.622826500297,283.704389857304,283.785861431739,
283.838928063841),.UNSPECIFIED.);
#3383=B_SPLINE_CURVE_WITH_KNOTS('',3,(#54343,#54344,#54345,#54346,#54347,
#54348,#54349,#54350,#54351,#54352,#54353,#54354,#54355,#54356,#54357,#54358,
#54359,#54360,#54361,#54362,#54363,#54364,#54365,#54366,#54367,#54368,#54369,
#54370,#54371,#54372,#54373,#54374,#54375,#54376,#54377,#54378,#54379,#54380,
#54381,#54382,#54383,#54384,#54385,#54386,#54387,#54388,#54389,#54390,#54391,
#54392,#54393,#54394,#54395,#54396,#54397,#54398,#54399,#54400,#54401,#54402,
#54403,#54404,#54405,#54406,#54407,#54408,#54409,#54410,#54411,#54412,#54413,
#54414,#54415,#54416,#54417,#54418,#54419,#54420,#54421,#54422,#54423,#54424),
 .UNSPECIFIED.,.F.,.F.,(4,3,3,3,3,3,3,3,3,3,3,3,3,3,3,3,3,3,3,3,3,3,3,3,
3,3,3,4),(277.55504144039,277.637572212348,277.715960591356,277.794282855798,
277.872553405257,277.950786601801,278.028996779478,278.107214914861,278.185440980081,
278.263687961638,278.341968855853,278.420342283607,278.498765281931,278.577304841121,
278.635114593673,278.710793424333,278.786377441824,278.861883641082,278.937328924206,
279.01273012275,279.08811438325,279.163492108499,279.23887846607,279.314288630994,
279.389783238998,279.465322399708,279.540978914284,279.601746169399),
 .UNSPECIFIED.);
#3384=B_SPLINE_CURVE_WITH_KNOTS('',3,(#54426,#54427,#54428,#54429,#54430,
#54431,#54432,#54433,#54434,#54435,#54436,#54437,#54438,#54439,#54440,#54441,
#54442,#54443,#54444,#54445,#54446,#54447,#54448,#54449,#54450,#54451,#54452,
#54453,#54454,#54455,#54456,#54457,#54458,#54459,#54460,#54461,#54462,#54463,
#54464,#54465,#54466,#54467,#54468,#54469,#54470,#54471,#54472,#54473,#54474,
#54475,#54476,#54477,#54478,#54479,#54480,#54481,#54482,#54483,#54484,#54485,
#54486,#54487,#54488,#54489,#54490,#54491,#54492,#54493,#54494,#54495,#54496,
#54497,#54498,#54499,#54500,#54501),.UNSPECIFIED.,.F.,.F.,(4,3,3,3,3,3,
3,3,3,3,3,3,3,3,3,3,3,3,3,3,3,3,3,3,3,4),(277.555239120736,277.637700724466,
277.720161662318,277.80262196169,277.885081649979,277.967540754577,278.049999302877,
278.13245732227,278.214914840143,278.301591798227,278.384058583768,278.466523696836,
278.548987247084,278.631449344143,278.713910097625,278.796369617121,278.878828012206,
278.96128539244,279.043751778126,279.126214979634,279.208675435484,279.291133584038,
279.373599187792,279.45605906618,279.538523177432,279.601746169492),
 .UNSPECIFIED.);
#3385=B_SPLINE_CURVE_WITH_KNOTS('',3,(#54502,#54503,#54504,#54505,#54506,
#54507,#54508,#54509,#54510,#54511,#54512,#54513,#54514,#54515,#54516,#54517,
#54518,#54519,#54520,#54521,#54522,#54523,#54524,#54525,#54526,#54527,#54528,
#54529,#54530,#54531,#54532,#54533,#54534,#54535,#54536,#54537,#54538,#54539,
#54540,#54541,#54542,#54543,#54544,#54545,#54546,#54547,#54548,#54549,#54550,
#54551,#54552,#54553,#54554,#54555,#54556,#54557,#54558,#54559,#54560,#54561,
#54562,#54563,#54564,#54565,#54566,#54567,#54568,#54569,#54570,#54571,#54572,
#54573,#54574,#54575,#54576,#54577,#54578,#54579,#54580,#54581,#54582,#54583,
#54584,#54585,#54586,#54587,#54588,#54589,#54590,#54591,#54592,#54593,#54594,
#54595,#54596,#54597,#54598,#54599,#54600,#54601,#54602,#54603,#54604,#54605,
#54606,#54607,#54608,#54609,#54610,#54611,#54612,#54613,#54614,#54615,#54616,
#54617,#54618,#54619,#54620,#54621,#54622,#54623,#54624,#54625,#54626,#54627,
#54628,#54629,#54630,#54631,#54632,#54633,#54634,#54635,#54636,#54637,#54638,
#54639,#54640,#54641,#54642,#54643,#54644,#54645,#54646,#54647,#54648,#54649,
#54650,#54651,#54652,#54653,#54654,#54655,#54656,#54657,#54658,#54659,#54660,
#54661,#54662,#54663,#54664,#54665,#54666,#54667),.UNSPECIFIED.,.F.,.F.,
(4,3,3,3,3,3,3,3,3,3,3,3,3,3,3,3,3,3,3,3,3,3,3,3,3,3,3,3,3,3,3,3,3,3,3,
3,3,3,3,3,3,3,3,3,3,3,3,3,3,3,3,3,3,3,3,4),(279.601746169492,279.689792983173,
279.777223068222,279.865578246219,279.953933424215,280.035490403841,280.116972252807,
280.200905343325,280.282232583354,280.367468599116,280.452704614878,280.532115813357,
280.611545437905,280.691004248855,280.77053607231,280.850109598739,280.929766722704,
280.95147580554,281.029864184548,281.10818644899,281.186456998449,281.264690194993,
281.34290037267,281.421118508053,281.499344573272,281.57759155483,281.655872449044,
281.734245876799,281.812668875122,281.891208434313,281.949018186865,282.025089464501,
282.101065240948,282.17696229794,282.252797336753,282.32858699685,282.405833693268,
282.481597191528,282.557368022895,282.633161190729,282.711511035094,282.787435798605,
282.866998183397,282.94656056819,283.024136849311,283.101619874536,283.179025302498,
283.256368736008,283.333663725309,283.410932806938,283.488190025617,283.565449416688,
283.642752625717,283.720080084015,283.797479430723,283.837852220474),
 .UNSPECIFIED.);
#3386=B_SPLINE_CURVE_WITH_KNOTS('',3,(#54673,#54674,#54675,#54676,#54677,
#54678,#54679,#54680,#54681,#54682,#54683,#54684,#54685,#54686,#54687,#54688,
#54689,#54690,#54691,#54692,#54693,#54694,#54695,#54696,#54697,#54698,#54699,
#54700,#54701,#54702,#54703,#54704,#54705,#54706,#54707,#54708,#54709,#54710,
#54711,#54712,#54713,#54714,#54715,#54716,#54717,#54718,#54719,#54720,#54721,
#54722,#54723,#54724,#54725,#54726,#54727,#54728,#54729,#54730,#54731,#54732,
#54733,#54734,#54735,#54736,#54737,#54738,#54739,#54740,#54741,#54742,#54743,
#54744,#54745,#54746,#54747,#54748,#54749,#54750,#54751,#54752,#54753,#54754,
#54755,#54756,#54757,#54758,#54759,#54760,#54761,#54762,#54763,#54764,#54765,
#54766,#54767,#54768,#54769,#54770,#54771,#54772,#54773,#54774,#54775,#54776,
#54777,#54778,#54779,#54780,#54781,#54782,#54783,#54784,#54785,#54786,#54787,
#54788,#54789,#54790,#54791,#54792,#54793,#54794,#54795,#54796,#54797,#54798,
#54799,#54800,#54801,#54802,#54803,#54804,#54805,#54806,#54807,#54808,#54809,
#54810,#54811,#54812,#54813,#54814,#54815,#54816,#54817,#54818,#54819,#54820,
#54821,#54822,#54823,#54824,#54825,#54826,#54827,#54828,#54829),
 .UNSPECIFIED.,.F.,.F.,(4,3,3,3,3,3,3,3,3,3,3,3,3,3,3,3,3,3,3,3,3,3,3,3,
3,3,3,3,3,3,3,3,3,3,3,3,3,3,3,3,3,3,3,3,3,3,3,3,3,3,3,3,4),(285.884931476671,
285.967393682771,286.049855540574,286.132317056929,286.214778238687,286.297239092697,
286.379699625809,286.462159844872,286.544619756735,286.627079368247,286.709538686256,
286.79199771761,286.874456469157,286.956914947744,287.03937316022,287.121831113431,
287.204288814224,287.286746269445,287.369203485943,287.455216181229,287.538540979787,
287.621007585379,287.703473346762,287.785938291352,287.86840244656,287.950865839797,
288.033328498468,288.115790449979,288.198251721732,288.280712341125,288.363172335556,
288.44563173242,288.52809055911,288.610548843017,288.69300661153,288.775463892037,
288.859598007228,288.942064005588,289.024528382194,289.106991246689,289.189452708696,
289.271912877815,289.354371863631,289.436829775711,289.522427270634,289.60489200768,
289.687353780067,289.769813026232,289.85227018447,289.934732703553,290.017190374964,
290.099649166157,290.121609735095),.UNSPECIFIED.);
#3387=B_SPLINE_CURVE_WITH_KNOTS('',3,(#54830,#54831,#54832,#54833,#54834,
#54835,#54836,#54837,#54838,#54839,#54840,#54841,#54842,#54843,#54844,#54845,
#54846,#54847,#54848,#54849,#54850,#54851,#54852,#54853,#54854,#54855,#54856,
#54857,#54858,#54859,#54860,#54861,#54862,#54863,#54864,#54865,#54866,#54867,
#54868,#54869,#54870,#54871,#54872,#54873,#54874,#54875,#54876,#54877,#54878,
#54879,#54880,#54881,#54882,#54883,#54884,#54885,#54886,#54887,#54888,#54889,
#54890,#54891,#54892,#54893,#54894,#54895,#54896,#54897,#54898,#54899,#54900,
#54901,#54902,#54903,#54904,#54905,#54906,#54907,#54908,#54909,#54910,#54911),
 .UNSPECIFIED.,.F.,.F.,(4,3,3,3,3,3,3,3,3,3,3,3,3,3,3,3,3,3,3,3,3,3,3,3,
3,3,3,4),(283.838928063841,283.920276857637,284.001570576253,284.082800319923,
284.12159769096,284.201008889439,284.280438513987,284.359897324937,284.439429148393,
284.519002674822,284.598659798787,284.620368881622,284.69875726063,284.777079525072,
284.85535007453,284.933583271075,285.011793448752,285.090011584135,285.168237649354,
285.246484630912,285.324765525126,285.403138952881,285.481561951204,285.560101510394,
285.617911262947,285.712522593592,285.805716091708,285.884931476671),
 .UNSPECIFIED.);
#3388=B_SPLINE_CURVE_WITH_KNOTS('',3,(#54913,#54914,#54915,#54916,#54917,
#54918,#54919,#54920,#54921,#54922,#54923,#54924,#54925,#54926,#54927,#54928,
#54929,#54930,#54931,#54932,#54933,#54934,#54935,#54936,#54937,#54938,#54939,
#54940,#54941,#54942,#54943,#54944,#54945,#54946,#54947,#54948,#54949,#54950,
#54951,#54952,#54953,#54954,#54955,#54956,#54957,#54958,#54959,#54960,#54961,
#54962,#54963,#54964,#54965,#54966,#54967,#54968,#54969,#54970,#54971,#54972,
#54973,#54974,#54975,#54976,#54977,#54978,#54979,#54980,#54981,#54982,#54983,
#54984,#54985,#54986,#54987,#54988,#54989,#54990,#54991,#54992,#54993,#54994),
 .UNSPECIFIED.,.F.,.F.,(4,3,3,3,3,3,3,3,3,3,3,3,3,3,3,3,3,3,3,3,3,3,3,3,
3,3,3,4),(283.837852220474,283.915368600167,283.944102949515,284.028315100976,
284.112401128686,284.196282050633,284.280033836667,284.363571484004,284.442874140177,
284.520253906507,284.597652067551,284.675082410124,284.752599703576,284.83016664955,
284.907839940997,284.94164533084,285.020635129152,285.099550436348,285.178404835331,
285.257211863794,285.335988443429,285.414748496302,285.493504247453,285.572267917277,
285.651085075272,285.729927923759,285.808855343169,285.884931476671),
 .UNSPECIFIED.);
#3389=B_SPLINE_CURVE_WITH_KNOTS('',3,(#54995,#54996,#54997,#54998,#54999,
#55000,#55001,#55002,#55003,#55004,#55005,#55006,#55007,#55008,#55009,#55010,
#55011,#55012,#55013,#55014,#55015,#55016,#55017,#55018,#55019,#55020,#55021,
#55022,#55023,#55024,#55025,#55026,#55027,#55028,#55029,#55030,#55031,#55032,
#55033,#55034,#55035,#55036,#55037,#55038,#55039,#55040,#55041,#55042,#55043,
#55044,#55045,#55046,#55047,#55048,#55049,#55050,#55051,#55052,#55053,#55054,
#55055,#55056,#55057,#55058,#55059,#55060,#55061,#55062,#55063,#55064,#55065,
#55066,#55067,#55068,#55069,#55070,#55071,#55072,#55073,#55074,#55075,#55076,
#55077,#55078,#55079,#55080,#55081,#55082,#55083,#55084,#55085,#55086,#55087,
#55088,#55089,#55090,#55091,#55092,#55093,#55094,#55095,#55096,#55097,#55098,
#55099,#55100,#55101,#55102,#55103,#55104,#55105,#55106,#55107,#55108,#55109,
#55110,#55111,#55112,#55113,#55114,#55115,#55116,#55117,#55118,#55119,#55120,
#55121,#55122,#55123,#55124,#55125,#55126,#55127,#55128,#55129,#55130,#55131,
#55132,#55133,#55134,#55135,#55136,#55137,#55138,#55139,#55140,#55141,#55142,
#55143,#55144,#55145,#55146,#55147,#55148,#55149,#55150,#55151),
 .UNSPECIFIED.,.F.,.F.,(4,3,3,3,3,3,3,3,3,3,3,3,3,3,3,3,3,3,3,3,3,3,3,3,
3,3,3,3,3,3,3,3,3,3,3,3,3,3,3,3,3,3,3,3,3,3,3,3,3,3,3,3,4),(285.884931476671,
285.967393682771,286.049855540574,286.132317056929,286.214778238687,286.297239092697,
286.379699625809,286.462159844872,286.544619756735,286.627079368247,286.709538686256,
286.791997717609,286.874456469156,286.956914947744,287.039373160219,287.12183111343,
287.204288814223,287.286746269445,287.369203485942,287.455216181228,287.538540979787,
287.621007585379,287.703473346762,287.785938291352,287.86840244656,287.950865839796,
288.033328498468,288.115790449979,288.198251721732,288.280712341125,288.363172335556,
288.44563173242,288.52809055911,288.610548843017,288.69300661153,288.775463892036,
288.859598007228,288.942064005588,289.024528382194,289.106991246689,289.189452708696,
289.271912877815,289.354371863631,289.436829775711,289.522427270634,289.60489200768,
289.687353780067,289.769813026232,289.85227018447,289.934732703553,290.017190374964,
290.099649166157,290.121609735095),.UNSPECIFIED.);
#3390=B_SPLINE_CURVE_WITH_KNOTS('',3,(#55157,#55158,#55159,#55160,#55161,
#55162,#55163,#55164,#55165,#55166,#55167,#55168,#55169,#55170,#55171,#55172,
#55173,#55174,#55175,#55176,#55177,#55178,#55179,#55180,#55181,#55182,#55183,
#55184,#55185,#55186,#55187,#55188,#55189,#55190,#55191,#55192,#55193,#55194,
#55195,#55196,#55197,#55198,#55199,#55200,#55201,#55202,#55203,#55204,#55205,
#55206,#55207,#55208,#55209,#55210,#55211,#55212,#55213,#55214,#55215,#55216,
#55217,#55218,#55219,#55220,#55221,#55222,#55223,#55224,#55225,#55226,#55227,
#55228,#55229,#55230,#55231,#55232,#55233,#55234,#55235,#55236,#55237,#55238,
#55239,#55240,#55241,#55242,#55243,#55244,#55245,#55246,#55247,#55248,#55249,
#55250,#55251,#55252,#55253,#55254,#55255,#55256,#55257,#55258,#55259,#55260,
#55261,#55262,#55263,#55264,#55265,#55266,#55267,#55268,#55269,#55270,#55271,
#55272,#55273,#55274,#55275,#55276,#55277,#55278,#55279,#55280,#55281,#55282,
#55283,#55284,#55285,#55286,#55287,#55288,#55289,#55290,#55291,#55292,#55293,
#55294,#55295,#55296,#55297,#55298,#55299,#55300,#55301,#55302,#55303,#55304,
#55305,#55306,#55307,#55308,#55309,#55310,#55311,#55312,#55313,#55314,#55315,
#55316,#55317,#55318,#55319,#55320,#55321,#55322),.UNSPECIFIED.,.F.,.F.,
(4,3,3,3,3,3,3,3,3,3,3,3,3,3,3,3,3,3,3,3,3,3,3,3,3,3,3,3,3,3,3,3,3,3,3,
3,3,3,3,3,3,3,3,3,3,3,3,3,3,3,3,3,3,3,3,4),(292.168116783851,292.255250415141,
292.342972619817,292.430969857911,292.51933491208,292.600707932221,292.676779209857,
292.752754986304,292.828652043296,292.904487082109,292.980276742206,293.057523438624,
293.133286936884,293.209057768251,293.284850936085,293.36320078045,293.439125543961,
293.518687928753,293.598250313546,293.675820534489,293.753298675009,293.830700388923,
293.908041275218,293.985336889112,294.062610328726,294.139873564033,294.21714063147,
294.294425566974,294.371783569321,294.449179100378,294.526680767145,294.595792694871,
294.680004846332,294.764090874042,294.847971795988,294.931723582022,295.015261229359,
295.094563885534,295.171943651865,295.249341812908,295.326772155481,295.404289448934,
295.481856394908,295.559529686355,295.593335076196,295.672968306783,295.752527270792,
295.834063474569,295.9135027365,295.992909167164,296.072293859906,296.15542462018,
296.234813253758,296.314210466724,296.393641864363,296.404816901002),
 .UNSPECIFIED.);
#3391=B_SPLINE_CURVE_WITH_KNOTS('',3,(#55323,#55324,#55325,#55326,#55327,
#55328,#55329,#55330,#55331,#55332,#55333,#55334,#55335,#55336,#55337,#55338,
#55339,#55340,#55341,#55342,#55343,#55344,#55345,#55346,#55347,#55348,#55349,
#55350,#55351,#55352,#55353,#55354,#55355,#55356,#55357,#55358,#55359,#55360,
#55361,#55362,#55363,#55364,#55365,#55366,#55367,#55368,#55369,#55370,#55371,
#55372,#55373,#55374,#55375,#55376,#55377,#55378,#55379,#55380,#55381,#55382,
#55383,#55384,#55385,#55386,#55387,#55388,#55389,#55390,#55391,#55392,#55393,
#55394,#55395,#55396,#55397,#55398),.UNSPECIFIED.,.F.,.F.,(4,3,3,3,3,3,
3,3,3,3,3,3,3,3,3,3,3,3,3,3,3,3,3,3,3,4),(290.121609735095,290.204071338826,
290.286532276678,290.36899257605,290.451452264338,290.533911368936,290.616369917237,
290.698827936629,290.781285454502,290.867962412586,290.950429198127,291.032894311195,
291.115357861443,291.197819958503,291.280280711984,291.36274023148,291.445198626565,
291.527656006799,291.610122392485,291.692585593993,291.775046049843,291.857504198398,
291.939969802151,292.022429680539,292.104893791791,292.168116783851),
 .UNSPECIFIED.);
#3392=B_SPLINE_CURVE_WITH_KNOTS('',3,(#55400,#55401,#55402,#55403,#55404,
#55405,#55406,#55407,#55408,#55409,#55410,#55411,#55412,#55413,#55414,#55415,
#55416,#55417,#55418,#55419,#55420,#55421,#55422,#55423,#55424,#55425,#55426,
#55427,#55428,#55429,#55430,#55431,#55432,#55433,#55434,#55435,#55436,#55437,
#55438,#55439,#55440,#55441,#55442,#55443,#55444,#55445,#55446,#55447,#55448,
#55449,#55450,#55451,#55452,#55453,#55454,#55455,#55456,#55457,#55458,#55459,
#55460,#55461,#55462,#55463,#55464,#55465,#55466,#55467,#55468,#55469,#55470,
#55471,#55472,#55473,#55474,#55475),.UNSPECIFIED.,.F.,.F.,(4,3,3,3,3,3,
3,3,3,3,3,3,3,3,3,3,3,3,3,3,3,3,3,3,3,4),(290.121609735095,290.204071338826,
290.286532276677,290.368992576049,290.451452264338,290.533911368936,290.616369917236,
290.698827936629,290.781285454502,290.867962412577,290.950429198118,291.032894311186,
291.115357861434,291.197819958493,291.280280711975,291.362740231471,291.445198626556,
291.52765600679,291.610122392476,291.692585593984,291.775046049833,291.857504198388,
291.939969802142,292.02242968053,292.104893791782,292.16811678371),
 .UNSPECIFIED.);
#3393=B_SPLINE_CURVE_WITH_KNOTS('',3,(#55476,#55477,#55478,#55479,#55480,
#55481,#55482,#55483,#55484,#55485,#55486,#55487,#55488,#55489,#55490,#55491,
#55492,#55493,#55494,#55495,#55496,#55497,#55498,#55499,#55500,#55501,#55502,
#55503,#55504,#55505,#55506,#55507,#55508,#55509,#55510,#55511,#55512,#55513,
#55514,#55515,#55516,#55517,#55518,#55519,#55520,#55521,#55522,#55523,#55524,
#55525,#55526,#55527,#55528,#55529,#55530,#55531,#55532,#55533,#55534,#55535,
#55536,#55537,#55538,#55539,#55540,#55541,#55542,#55543,#55544,#55545,#55546,
#55547,#55548,#55549,#55550,#55551,#55552,#55553,#55554,#55555,#55556,#55557,
#55558,#55559,#55560,#55561,#55562,#55563,#55564,#55565,#55566,#55567,#55568,
#55569,#55570,#55571,#55572,#55573,#55574,#55575,#55576,#55577,#55578,#55579,
#55580,#55581,#55582,#55583,#55584,#55585,#55586,#55587,#55588,#55589,#55590,
#55591,#55592,#55593,#55594,#55595,#55596,#55597,#55598,#55599,#55600,#55601,
#55602,#55603,#55604,#55605,#55606,#55607,#55608,#55609,#55610,#55611,#55612,
#55613,#55614,#55615,#55616,#55617,#55618,#55619,#55620,#55621,#55622,#55623,
#55624,#55625,#55626,#55627,#55628,#55629,#55630,#55631,#55632),
 .UNSPECIFIED.,.F.,.F.,(4,3,3,3,3,3,3,3,3,3,3,3,3,3,3,3,3,3,3,3,3,3,3,3,
3,3,3,3,3,3,3,3,3,3,3,3,3,3,3,3,3,3,3,3,3,3,3,3,3,3,3,3,4),(292.168116783851,
292.250578989951,292.333040847754,292.415502364109,292.497963545867,292.580424399877,
292.662884932989,292.745345152052,292.827805063915,292.910264675427,292.992723993436,
293.07518302479,293.157641776337,293.240100254924,293.3225584674,293.405016420611,
293.487474121404,293.569931576626,293.652388793123,293.738401488409,293.821726286967,
293.904192892559,293.986658653942,294.069123598532,294.151587753741,294.234051146977,
294.316513805649,294.39897575716,294.481437028912,294.563897648306,294.646357642737,
294.728817039601,294.811275866291,294.893734150198,294.976191918711,295.058649199218,
295.142783314409,295.225249312769,295.307713689375,295.39017655387,295.472638015877,
295.555098184996,295.637557170812,295.720015082892,295.805612577815,295.888077314861,
295.970539087247,296.052998333412,296.135455491651,296.217918010734,296.300375682145,
296.382834473338,296.404795042275),.UNSPECIFIED.);
#3394=B_SPLINE_CURVE_WITH_KNOTS('',3,(#55638,#55639,#55640,#55641,#55642,
#55643,#55644,#55645,#55646,#55647,#55648,#55649,#55650,#55651,#55652,#55653,
#55654,#55655,#55656,#55657,#55658,#55659,#55660,#55661,#55662,#55663,#55664,
#55665,#55666,#55667,#55668,#55669,#55670,#55671,#55672,#55673,#55674,#55675,
#55676,#55677,#55678,#55679,#55680,#55681,#55682,#55683,#55684,#55685,#55686,
#55687,#55688,#55689,#55690,#55691,#55692,#55693,#55694,#55695,#55696,#55697,
#55698,#55699,#55700,#55701,#55702,#55703,#55704,#55705,#55706,#55707,#55708,
#55709,#55710,#55711,#55712,#55713,#55714,#55715,#55716,#55717,#55718,#55719,
#55720,#55721,#55722,#55723,#55724,#55725,#55726,#55727,#55728,#55729,#55730,
#55731,#55732,#55733,#55734,#55735,#55736,#55737,#55738,#55739,#55740,#55741,
#55742,#55743,#55744,#55745,#55746,#55747,#55748,#55749,#55750,#55751,#55752,
#55753,#55754,#55755,#55756,#55757,#55758,#55759,#55760,#55761,#55762,#55763,
#55764,#55765,#55766,#55767,#55768,#55769,#55770,#55771,#55772,#55773,#55774,
#55775,#55776,#55777,#55778,#55779,#55780,#55781,#55782,#55783,#55784,#55785,
#55786,#55787,#55788,#55789,#55790,#55791,#55792,#55793,#55794,#55795,#55796,
#55797,#55798,#55799,#55800,#55801,#55802,#55803,#55804,#55805,#55806),
 .UNSPECIFIED.,.F.,.F.,(4,3,3,3,3,3,3,3,3,3,3,3,3,3,3,3,3,3,3,3,3,3,3,3,
3,3,3,3,3,3,3,3,3,3,3,3,3,3,3,3,3,3,3,3,3,3,3,3,3,3,3,3,3,3,3,3,4),(298.451302091031,
298.549288570198,298.585962220171,298.664350599179,298.742672863622,298.82094341308,
298.899176609624,298.977386787301,299.055604922684,299.133830987904,299.212077969461,
299.290358863676,299.368732291431,299.447155289754,299.525694848945,299.583504601496,
299.659575879132,299.735551655579,299.811448712571,299.887283751384,299.963073411481,
300.040320107898,300.116083606159,300.191854437526,300.267647605359,300.345997449725,
300.421922213235,300.501484598028,300.581046982821,300.658617203764,300.736095344284,
300.813497058198,300.890837944493,300.968133558387,301.045406998001,301.122670233308,
301.199937300745,301.277222236249,301.354580238595,301.431975769652,301.509477436419,
301.578589364145,301.662801515606,301.746887543315,301.830768465262,301.914520251295,
301.998057898632,302.077360554808,302.154740321139,302.232138482182,302.309568824755,
302.387086118208,302.464653064182,302.54232635563,302.57613174547,302.655761215605,
302.688034846856),.UNSPECIFIED.);
#3395=B_SPLINE_CURVE_WITH_KNOTS('',3,(#55807,#55808,#55809,#55810,#55811,
#55812,#55813,#55814,#55815,#55816,#55817,#55818,#55819,#55820,#55821,#55822,
#55823,#55824,#55825,#55826,#55827,#55828,#55829,#55830,#55831,#55832,#55833,
#55834,#55835,#55836,#55837,#55838,#55839,#55840,#55841,#55842,#55843,#55844,
#55845,#55846,#55847,#55848,#55849,#55850,#55851,#55852,#55853,#55854,#55855,
#55856,#55857,#55858,#55859,#55860,#55861,#55862,#55863,#55864,#55865,#55866,
#55867,#55868,#55869,#55870,#55871,#55872,#55873,#55874,#55875,#55876,#55877,
#55878,#55879,#55880,#55881,#55882,#55883,#55884,#55885,#55886,#55887,#55888),
 .UNSPECIFIED.,.F.,.F.,(4,3,3,3,3,3,3,3,3,3,3,3,3,3,3,3,3,3,3,3,3,3,3,3,
3,3,3,4),(296.404816901002,296.484303298207,296.563859804948,296.590877457521,
296.667608035846,296.744271634213,296.820882935442,296.897457702157,296.974011031551,
297.050568429556,297.089648648183,297.174317639801,297.259132091849,297.344145410086,
297.429244825595,297.514464214127,297.588419838846,297.669976818473,297.751458667439,
297.835391757956,297.916718997986,298.001955013747,298.087191029508,298.163747110249,
298.240328867758,298.316923015151,298.393579483727,298.451302090923),
 .UNSPECIFIED.);
#3396=B_SPLINE_CURVE_WITH_KNOTS('',3,(#55890,#55891,#55892,#55893,#55894,
#55895,#55896,#55897,#55898,#55899,#55900,#55901,#55902,#55903,#55904,#55905,
#55906,#55907,#55908,#55909,#55910,#55911,#55912,#55913,#55914,#55915,#55916,
#55917,#55918,#55919,#55920,#55921,#55922,#55923,#55924,#55925,#55926,#55927,
#55928,#55929,#55930,#55931,#55932,#55933,#55934,#55935,#55936,#55937,#55938,
#55939,#55940,#55941,#55942,#55943,#55944,#55945,#55946,#55947,#55948,#55949,
#55950,#55951,#55952,#55953,#55954,#55955,#55956,#55957,#55958,#55959,#55960,
#55961,#55962,#55963,#55964,#55965),.UNSPECIFIED.,.F.,.F.,(4,3,3,3,3,3,
3,3,3,3,3,3,3,3,3,3,3,3,3,3,3,3,3,3,3,4),(296.404795042275,296.487256646006,
296.569717583857,296.652177883229,296.734637571518,296.817096676116,296.899555224416,
296.982013243809,297.064470761682,297.151147719766,297.233614505307,297.316079618375,
297.398543168623,297.481005265682,297.563466019164,297.64592553866,297.728383933745,
297.810841313978,297.893307699665,297.975770901173,298.058231357022,298.140689505577,
298.223155109331,298.305614987719,298.388079098971,298.451302091031),
 .UNSPECIFIED.);
#3397=B_SPLINE_CURVE_WITH_KNOTS('',3,(#55966,#55967,#55968,#55969,#55970,
#55971,#55972,#55973,#55974,#55975,#55976,#55977,#55978,#55979,#55980,#55981,
#55982,#55983,#55984,#55985,#55986,#55987,#55988,#55989,#55990,#55991,#55992,
#55993,#55994,#55995,#55996,#55997,#55998,#55999,#56000,#56001,#56002,#56003,
#56004,#56005,#56006,#56007,#56008,#56009,#56010,#56011,#56012,#56013,#56014,
#56015,#56016,#56017,#56018,#56019,#56020,#56021,#56022,#56023,#56024,#56025,
#56026,#56027,#56028,#56029,#56030,#56031,#56032,#56033,#56034,#56035,#56036,
#56037,#56038,#56039,#56040,#56041,#56042,#56043,#56044,#56045,#56046,#56047,
#56048,#56049,#56050,#56051,#56052,#56053,#56054,#56055,#56056,#56057,#56058,
#56059,#56060,#56061,#56062,#56063,#56064,#56065,#56066,#56067,#56068,#56069,
#56070,#56071,#56072,#56073,#56074,#56075,#56076,#56077,#56078,#56079,#56080,
#56081,#56082,#56083,#56084,#56085,#56086,#56087,#56088,#56089,#56090,#56091,
#56092,#56093,#56094,#56095,#56096,#56097,#56098,#56099,#56100,#56101,#56102,
#56103,#56104,#56105,#56106,#56107,#56108,#56109,#56110,#56111,#56112,#56113,
#56114,#56115,#56116,#56117,#56118,#56119,#56120,#56121,#56122,#56123,#56124,
#56125,#56126,#56127,#56128,#56129,#56130,#56131),.UNSPECIFIED.,.F.,.F.,
(4,3,3,3,3,3,3,3,3,3,3,3,3,3,3,3,3,3,3,3,3,3,3,3,3,3,3,3,3,3,3,3,3,3,3,
3,3,3,3,3,3,3,3,3,3,3,3,3,3,3,3,3,3,3,3,4),(298.451328562689,298.529563567541,
298.607838564957,298.686215847642,298.764647222749,298.843204822482,298.907238669388,
298.986863857249,299.066416312125,299.145908333914,299.225352175928,299.304760053826,
299.384150487948,299.463532038697,299.542915776503,299.622312771833,299.701763388958,
299.781242408397,299.860794548049,299.904781050713,299.981511629038,300.058175227405,
300.134786528633,300.211361295348,300.287914624742,300.364472022747,300.403552241375,
300.488221232992,300.57303568504,300.658049003277,300.743148418786,300.828367807318,
300.902323432038,300.983880411665,301.065362260631,301.149295351148,301.230622591178,
301.315858606939,301.4010946227,301.480505821178,301.559935445727,301.639394256677,
301.718926080132,301.79849960656,301.878156730524,301.899865813363,301.978262059829,
302.056590094759,302.135466386161,302.213700289115,302.291913310575,302.370118438689,
302.44948893551,302.527739594342,302.607670010156,302.687600425971),
 .UNSPECIFIED.);
#3398=B_SPLINE_CURVE_WITH_KNOTS('',3,(#56137,#56138,#56139,#56140,#56141,
#56142,#56143,#56144,#56145,#56146,#56147,#56148,#56149,#56150,#56151,#56152,
#56153,#56154,#56155,#56156,#56157,#56158,#56159,#56160,#56161,#56162,#56163,
#56164,#56165,#56166,#56167,#56168,#56169,#56170,#56171,#56172,#56173,#56174,
#56175,#56176,#56177,#56178,#56179,#56180,#56181,#56182,#56183,#56184,#56185,
#56186,#56187,#56188,#56189,#56190,#56191,#56192,#56193,#56194,#56195,#56196,
#56197,#56198,#56199,#56200,#56201,#56202,#56203,#56204,#56205,#56206,#56207,
#56208,#56209,#56210,#56211,#56212,#56213,#56214,#56215,#56216,#56217,#56218,
#56219,#56220,#56221,#56222,#56223,#56224,#56225,#56226,#56227,#56228,#56229,
#56230,#56231,#56232,#56233,#56234,#56235,#56236,#56237,#56238,#56239,#56240,
#56241,#56242,#56243,#56244,#56245,#56246,#56247,#56248,#56249,#56250,#56251,
#56252,#56253,#56254,#56255,#56256,#56257,#56258,#56259,#56260,#56261,#56262,
#56263,#56264,#56265,#56266,#56267,#56268,#56269,#56270,#56271,#56272,#56273,
#56274,#56275,#56276,#56277,#56278,#56279,#56280,#56281,#56282,#56283,#56284,
#56285,#56286,#56287,#56288,#56289,#56290,#56291,#56292,#56293,#56294,#56295,
#56296,#56297,#56298,#56299,#56300,#56301,#56302,#56303,#56304,#56305),
 .UNSPECIFIED.,.F.,.F.,(4,3,3,3,3,3,3,3,3,3,3,3,3,3,3,3,3,3,3,3,3,3,3,3,
3,3,3,3,3,3,3,3,3,3,3,3,3,3,3,3,3,3,3,3,3,3,3,3,3,3,3,3,3,3,3,3,4),(304.73448739821,
304.813891893521,304.893222832093,304.972510106595,305.051759714261,305.069987698783,
305.149398897262,305.22882852181,305.30828733276,305.387819156215,305.467392682644,
305.547049806609,305.568758889445,305.647147268453,305.725469532895,305.803740082354,
305.881973278898,305.960183456575,306.038401591958,306.116627657178,306.194874638735,
306.27315553295,306.351528960704,306.429951959028,306.508491518218,306.56630127077,
306.642372548406,306.718348324853,306.794245381845,306.870080420658,306.945870080755,
307.023116777173,307.098880275434,307.1746511068,307.250444274634,307.328794118999,
307.40471888251,307.484281267302,307.563843652095,307.641413873038,307.718892013558,
307.796293727472,307.873634613767,307.950930227661,308.028203667275,308.105466902582,
308.182733970019,308.260018905523,308.337376907869,308.414772438926,308.492274105693,
308.56138603342,308.645614213841,308.729653534376,308.813572069845,308.897291973851,
308.97167806506),.UNSPECIFIED.);
#3399=B_SPLINE_CURVE_WITH_KNOTS('',3,(#56306,#56307,#56308,#56309,#56310,
#56311,#56312,#56313,#56314,#56315,#56316,#56317,#56318,#56319,#56320,#56321,
#56322,#56323,#56324,#56325,#56326,#56327,#56328,#56329,#56330,#56331,#56332,
#56333,#56334,#56335,#56336,#56337,#56338,#56339,#56340,#56341,#56342,#56343,
#56344,#56345,#56346,#56347,#56348,#56349,#56350,#56351,#56352,#56353,#56354,
#56355,#56356,#56357,#56358,#56359,#56360,#56361,#56362,#56363,#56364,#56365,
#56366,#56367,#56368,#56369,#56370,#56371,#56372,#56373,#56374,#56375,#56376,
#56377,#56378,#56379,#56380,#56381,#56382,#56383,#56384),.UNSPECIFIED.,
 .F.,.F.,(4,3,3,3,3,3,3,3,3,3,3,3,3,3,3,3,3,3,3,3,3,3,3,3,3,3,4),(302.688034846856,
302.767561307616,302.847032310861,302.926460093556,303.007361847711,303.086747157603,
303.166128284763,303.245516298769,303.327555755776,303.407018106382,303.490346116589,
303.573674126795,303.65040470512,303.727068303487,303.803679604715,303.88025437143,
303.956807700825,304.03336509883,304.072445317458,304.157114309076,304.241928761125,
304.326942079363,304.412041494873,304.497260883406,304.57121650812,304.661692225701,
304.734487398087),.UNSPECIFIED.);
#3400=B_SPLINE_CURVE_WITH_KNOTS('',3,(#56386,#56387,#56388,#56389,#56390,
#56391,#56392,#56393,#56394,#56395,#56396,#56397,#56398,#56399,#56400,#56401,
#56402,#56403,#56404,#56405,#56406,#56407,#56408,#56409,#56410,#56411,#56412,
#56413,#56414,#56415,#56416,#56417,#56418,#56419,#56420,#56421,#56422,#56423,
#56424,#56425,#56426,#56427,#56428,#56429,#56430,#56431,#56432,#56433,#56434,
#56435,#56436,#56437,#56438,#56439,#56440,#56441,#56442,#56443,#56444,#56445,
#56446,#56447,#56448,#56449,#56450,#56451,#56452,#56453,#56454,#56455,#56456,
#56457,#56458,#56459,#56460,#56461,#56462,#56463,#56464,#56465,#56466,#56467),
 .UNSPECIFIED.,.F.,.F.,(4,3,3,3,3,3,3,3,3,3,3,3,3,3,3,3,3,3,3,3,3,3,3,3,
3,3,3,4),(302.687600425971,302.766026959837,302.844568635012,302.897408194688,
302.973479472324,303.049455248771,303.125352305763,303.201187344575,303.276977004672,
303.35422370109,303.429987199351,303.505758030717,303.581551198551,303.659901042916,
303.735825806427,303.81538819122,303.894950576013,303.971854137115,304.048665300184,
304.125400326618,304.202067988151,304.278698060654,304.355305138939,304.431903801529,
304.508536833966,304.585185693517,304.661908603409,304.73448739821),
 .UNSPECIFIED.);
#3401=B_SPLINE_CURVE_WITH_KNOTS('',3,(#56468,#56469,#56470,#56471,#56472,
#56473,#56474,#56475,#56476,#56477,#56478,#56479,#56480,#56481,#56482,#56483,
#56484,#56485,#56486,#56487,#56488,#56489,#56490,#56491,#56492,#56493,#56494,
#56495,#56496,#56497,#56498,#56499,#56500,#56501,#56502,#56503,#56504,#56505,
#56506,#56507,#56508,#56509,#56510,#56511,#56512,#56513,#56514,#56515,#56516,
#56517,#56518,#56519,#56520,#56521,#56522,#56523,#56524,#56525,#56526,#56527,
#56528,#56529,#56530,#56531,#56532,#56533,#56534,#56535,#56536,#56537,#56538,
#56539,#56540,#56541,#56542,#56543,#56544,#56545,#56546,#56547,#56548,#56549,
#56550,#56551,#56552,#56553,#56554,#56555,#56556,#56557,#56558,#56559,#56560,
#56561,#56562,#56563,#56564,#56565,#56566,#56567,#56568,#56569,#56570,#56571,
#56572,#56573,#56574,#56575,#56576,#56577,#56578,#56579,#56580,#56581,#56582,
#56583,#56584,#56585,#56586,#56587,#56588,#56589,#56590,#56591,#56592,#56593,
#56594,#56595,#56596,#56597,#56598,#56599,#56600,#56601,#56602,#56603,#56604,
#56605,#56606,#56607,#56608,#56609,#56610,#56611,#56612,#56613,#56614,#56615,
#56616,#56617,#56618,#56619,#56620,#56621,#56622,#56623,#56624,#56625,#56626,
#56627,#56628,#56629,#56630,#56631,#56632,#56633,#56634,#56635,#56636),
 .UNSPECIFIED.,.F.,.F.,(4,3,3,3,3,3,3,3,3,3,3,3,3,3,3,3,3,3,3,3,3,3,3,3,
3,3,3,3,3,3,3,3,3,3,3,3,3,3,3,3,3,3,3,3,3,3,3,3,3,3,3,3,3,3,3,3,4),(304.734487398285,
304.843285397621,304.892492957337,304.976705108798,305.060791136507,305.144672058453,
305.228423844487,305.311961491823,305.391264148,305.468643914331,305.546042075374,
305.623472417947,305.7009897114,305.778556657374,305.856229948821,305.890035338662,
305.969660526523,306.0492129814,306.128705003188,306.208148845203,306.287556723101,
306.366947157223,306.446328707972,306.525712445778,306.605109441108,306.684560058234,
306.764039077673,306.843591217325,306.887577719987,306.964308298312,307.040971896679,
307.117583197907,307.194157964622,307.270711294016,307.347268692021,307.38634891065,
307.471017902268,307.555832354317,307.640845672555,307.725945088065,307.811164476598,
307.885120101312,307.966677080938,308.048158929904,308.132092020422,308.213419260451,
308.298655276213,308.383891291975,308.463302490454,308.542732115002,308.622190925952,
308.701722749408,308.781296275836,308.860953399801,308.882662482637,308.961062075537,
308.971371590973),.UNSPECIFIED.);
#3402=B_SPLINE_CURVE_WITH_KNOTS('',3,(#56642,#56643,#56644,#56645,#56646,
#56647,#56648,#56649,#56650,#56651,#56652,#56653,#56654,#56655,#56656,#56657,
#56658,#56659,#56660,#56661,#56662,#56663,#56664,#56665,#56666,#56667,#56668,
#56669,#56670,#56671,#56672,#56673,#56674,#56675,#56676,#56677,#56678,#56679,
#56680,#56681,#56682,#56683,#56684,#56685,#56686,#56687,#56688,#56689,#56690,
#56691,#56692,#56693,#56694,#56695,#56696,#56697,#56698,#56699,#56700,#56701,
#56702,#56703,#56704,#56705,#56706,#56707,#56708,#56709,#56710,#56711,#56712,
#56713,#56714,#56715,#56716,#56717,#56718,#56719,#56720,#56721,#56722,#56723,
#56724,#56725,#56726,#56727,#56728,#56729,#56730,#56731,#56732,#56733,#56734,
#56735,#56736,#56737,#56738,#56739,#56740,#56741,#56742,#56743,#56744,#56745,
#56746,#56747,#56748,#56749,#56750,#56751,#56752,#56753,#56754,#56755,#56756,
#56757,#56758,#56759,#56760,#56761,#56762,#56763,#56764,#56765,#56766,#56767,
#56768,#56769,#56770,#56771,#56772,#56773,#56774,#56775,#56776,#56777,#56778,
#56779,#56780,#56781,#56782,#56783,#56784,#56785,#56786,#56787,#56788,#56789,
#56790,#56791,#56792,#56793,#56794,#56795,#56796,#56797,#56798),
 .UNSPECIFIED.,.F.,.F.,(4,3,3,3,3,3,3,3,3,3,3,3,3,3,3,3,3,3,3,3,3,3,3,3,
3,3,3,3,3,3,3,3,3,3,3,3,3,3,3,3,3,3,3,3,3,3,3,3,3,3,3,3,4),(311.01767270539,
311.10013491149,311.182596769293,311.265058285648,311.347519467406,311.429980321416,
311.512440854528,311.594901073591,311.677360985454,311.759820596966,311.842279914975,
311.924738946328,312.007197697875,312.089656176463,312.172114388939,312.254572342149,
312.337030042942,312.419487498164,312.501944714662,312.587957409948,312.671282208506,
312.753748814098,312.836214575481,312.918679520071,313.001143675279,313.083607068516,
313.166069727187,313.248531678698,313.330992950451,313.413453569844,313.495913564275,
313.578372961139,313.660831787829,313.743290071736,313.825747840249,313.908205120756,
313.992339235947,314.074805234307,314.157269610913,314.239732475408,314.322193937415,
314.404654106534,314.48711309235,314.56957100443,314.655168499353,314.737633236399,
314.820095008786,314.902554254951,314.985011413189,315.067473932272,315.149931603683,
315.232390394876,315.254350963814),.UNSPECIFIED.);
#3403=B_SPLINE_CURVE_WITH_KNOTS('',3,(#56799,#56800,#56801,#56802,#56803,
#56804,#56805,#56806,#56807,#56808,#56809,#56810,#56811,#56812,#56813,#56814,
#56815,#56816,#56817,#56818,#56819,#56820,#56821,#56822,#56823,#56824,#56825,
#56826,#56827,#56828,#56829,#56830,#56831,#56832,#56833,#56834,#56835,#56836,
#56837,#56838,#56839,#56840,#56841,#56842,#56843,#56844,#56845,#56846,#56847,
#56848,#56849,#56850,#56851,#56852,#56853,#56854,#56855,#56856,#56857,#56858,
#56859,#56860,#56861,#56862,#56863,#56864,#56865,#56866,#56867,#56868,#56869,
#56870,#56871,#56872,#56873,#56874,#56875,#56876,#56877,#56878,#56879,#56880,
#56881,#56882,#56883),.UNSPECIFIED.,.F.,.F.,(4,3,3,3,3,3,3,3,3,3,3,3,3,
3,3,3,3,3,3,3,3,3,3,3,3,3,3,3,4),(308.97167806506,309.055126155017,309.060157224082,
309.137536990412,309.214935151455,309.292365494027,309.36988278748,309.447449733453,
309.5251230249,309.558928414745,309.638553602606,309.718106057483,309.797598079271,
309.877041921286,309.956449799184,310.035840233306,310.115221784055,310.194605521861,
310.274002517192,310.353453134318,310.432932153757,310.51248429341,310.556470796069,
310.63372559496,310.710909566525,310.788029325159,310.865110869191,310.942176575884,
311.017385294333),.UNSPECIFIED.);
#3404=B_SPLINE_CURVE_WITH_KNOTS('',3,(#56885,#56886,#56887,#56888,#56889,
#56890,#56891,#56892,#56893,#56894,#56895,#56896,#56897,#56898,#56899,#56900,
#56901,#56902,#56903,#56904,#56905,#56906,#56907,#56908,#56909,#56910,#56911,
#56912,#56913,#56914,#56915,#56916,#56917,#56918,#56919,#56920,#56921,#56922,
#56923,#56924,#56925,#56926,#56927,#56928,#56929,#56930,#56931,#56932,#56933,
#56934,#56935,#56936,#56937,#56938,#56939,#56940,#56941,#56942,#56943,#56944,
#56945,#56946,#56947,#56948,#56949,#56950,#56951,#56952,#56953,#56954,#56955,
#56956,#56957,#56958,#56959,#56960,#56961,#56962,#56963),.UNSPECIFIED.,
 .F.,.F.,(4,3,3,3,3,3,3,3,3,3,3,3,3,3,3,3,3,3,3,3,3,3,3,3,3,3,4),(308.971371590973,
309.04968622051,309.127951028894,309.206180373963,309.284388586774,309.362607024147,
309.440835101417,309.51908580595,309.597372135917,309.675751415483,309.754181815283,
309.832725838633,309.880204863962,309.956276141598,310.032251918045,310.108148975037,
310.18398401385,310.259773673947,310.337020370365,310.412783868626,310.488554699992,
310.564347867826,310.642697712191,310.718622475702,310.798184860494,310.877747245287,
311.01767270539),.UNSPECIFIED.);
#3405=B_SPLINE_CURVE_WITH_KNOTS('',3,(#56964,#56965,#56966,#56967,#56968,
#56969,#56970,#56971,#56972,#56973,#56974,#56975,#56976,#56977,#56978,#56979,
#56980,#56981,#56982,#56983,#56984,#56985,#56986,#56987,#56988,#56989,#56990,
#56991,#56992,#56993,#56994,#56995,#56996,#56997,#56998,#56999,#57000,#57001,
#57002,#57003,#57004,#57005,#57006,#57007,#57008,#57009,#57010,#57011,#57012,
#57013,#57014,#57015,#57016,#57017,#57018,#57019,#57020,#57021,#57022,#57023,
#57024,#57025,#57026,#57027,#57028,#57029,#57030,#57031,#57032,#57033,#57034,
#57035,#57036,#57037,#57038,#57039,#57040,#57041,#57042,#57043,#57044,#57045,
#57046,#57047,#57048,#57049,#57050,#57051,#57052,#57053,#57054,#57055,#57056,
#57057,#57058,#57059,#57060,#57061,#57062,#57063,#57064,#57065,#57066,#57067,
#57068,#57069,#57070,#57071,#57072,#57073,#57074,#57075,#57076,#57077,#57078,
#57079,#57080,#57081,#57082,#57083,#57084,#57085,#57086,#57087,#57088,#57089,
#57090,#57091,#57092,#57093,#57094,#57095,#57096,#57097,#57098,#57099,#57100,
#57101,#57102,#57103,#57104,#57105,#57106,#57107,#57108,#57109,#57110,#57111,
#57112,#57113,#57114,#57115,#57116,#57117,#57118,#57119,#57120,#57121,#57122,
#57123,#57124,#57125,#57126,#57127,#57128,#57129,#57130,#57131,#57132),
 .UNSPECIFIED.,.F.,.F.,(4,3,3,3,3,3,3,3,3,3,3,3,3,3,3,3,3,3,3,3,3,3,3,3,
3,3,3,3,3,3,3,3,3,3,3,3,3,3,3,3,3,3,3,3,3,3,3,3,3,3,3,3,3,3,3,3,4),(311.017672705475,
311.093653448508,311.169554239541,311.245391850987,311.32412907294,311.399896824238,
311.475655932485,311.551421451453,311.627208438666,311.703067230971,311.778968690416,
311.854962775979,311.875289626612,311.959501778073,312.043587805783,312.12746872773,
312.211220513764,312.294758161101,312.374060817274,312.451440583604,312.528838744648,
312.606269087221,312.683786380673,312.761353326647,312.839026618094,312.872832007937,
312.952457195798,313.032009650675,313.111501672463,313.190945514478,313.270353392376,
313.349743826498,313.429125377247,313.508509115053,313.587906110384,313.667356727509,
313.746835746948,313.826387886601,313.870374389261,313.947104967586,314.023768565952,
314.10037986718,314.176954633894,314.253507963288,314.330065361293,314.369145579924,
314.453814571542,314.538629023591,314.623642341829,314.70874175734,314.793961145872,
314.867916770586,314.949484703759,315.030950764819,315.112353629913,315.193678956862,
315.254776117011),.UNSPECIFIED.);
#3406=B_SPLINE_CURVE_WITH_KNOTS('',3,(#57138,#57139,#57140,#57141,#57142,
#57143,#57144,#57145,#57146,#57147,#57148,#57149,#57150,#57151,#57152,#57153,
#57154,#57155,#57156,#57157,#57158,#57159,#57160,#57161,#57162,#57163,#57164,
#57165,#57166,#57167,#57168,#57169,#57170,#57171,#57172,#57173,#57174,#57175,
#57176,#57177,#57178,#57179,#57180,#57181,#57182,#57183,#57184,#57185,#57186,
#57187,#57188,#57189,#57190,#57191,#57192,#57193,#57194,#57195,#57196,#57197,
#57198,#57199,#57200,#57201,#57202,#57203,#57204,#57205,#57206,#57207,#57208,
#57209,#57210,#57211,#57212,#57213,#57214,#57215,#57216,#57217,#57218,#57219,
#57220,#57221,#57222,#57223,#57224,#57225,#57226,#57227,#57228,#57229,#57230,
#57231,#57232,#57233,#57234,#57235,#57236,#57237,#57238,#57239,#57240,#57241,
#57242,#57243,#57244,#57245,#57246,#57247,#57248,#57249,#57250,#57251,#57252,
#57253,#57254,#57255,#57256,#57257,#57258,#57259,#57260,#57261,#57262,#57263,
#57264,#57265,#57266,#57267,#57268,#57269,#57270,#57271,#57272,#57273,#57274,
#57275,#57276,#57277,#57278,#57279,#57280,#57281,#57282,#57283,#57284,#57285,
#57286,#57287,#57288,#57289,#57290,#57291,#57292,#57293,#57294,#57295,#57296,
#57297,#57298,#57299,#57300,#57301,#57302,#57303,#57304,#57305,#57306),
 .UNSPECIFIED.,.F.,.F.,(4,3,3,3,3,3,3,3,3,3,3,3,3,3,3,3,3,3,3,3,3,3,3,3,
3,3,3,3,3,3,3,3,3,3,3,3,3,3,3,3,3,3,3,3,3,3,3,3,3,3,3,3,3,3,3,3,4),(317.300858012569,
317.405449909472,317.511692304035,317.539267465344,317.61599804367,317.692661642036,
317.769272943265,317.84584770998,317.922401039375,317.99895843738,318.038038656006,
318.122707647623,318.207522099672,318.292535417908,318.377634833418,318.462854221949,
318.536809846669,318.618366826296,318.699848675262,318.78378176578,318.86510900581,
318.95034502157,319.035581037331,319.114992235809,319.194421860357,319.273880671307,
319.353412494762,319.432986021191,319.512643145155,319.534352227994,319.612740607002,
319.691062871444,319.769333420903,319.847566617447,319.925776795124,320.003994930507,
320.082220995727,320.160467977284,320.238748871499,320.317122299253,320.395545297577,
320.474084856767,320.531894609318,320.607965886954,320.683941663401,320.759838720393,
320.835673759206,320.911463419303,320.98871011572,321.064473613981,321.140244445348,
321.216037613181,321.294387457547,321.370312221057,321.44987460585,321.529436990643,
321.537211865788),.UNSPECIFIED.);
#3407=B_SPLINE_CURVE_WITH_KNOTS('',3,(#57307,#57308,#57309,#57310,#57311,
#57312,#57313,#57314,#57315,#57316,#57317,#57318,#57319,#57320,#57321,#57322,
#57323,#57324,#57325,#57326,#57327,#57328,#57329,#57330,#57331,#57332,#57333,
#57334,#57335,#57336,#57337,#57338,#57339,#57340,#57341,#57342,#57343,#57344,
#57345,#57346,#57347,#57348,#57349,#57350,#57351,#57352,#57353,#57354,#57355,
#57356,#57357,#57358,#57359,#57360,#57361,#57362,#57363,#57364,#57365,#57366,
#57367,#57368,#57369,#57370,#57371,#57372,#57373,#57374,#57375,#57376,#57377,
#57378,#57379,#57380,#57381,#57382),.UNSPECIFIED.,.F.,.F.,(4,3,3,3,3,3,
3,3,3,3,3,3,3,3,3,3,3,3,3,3,3,3,3,3,3,4),(315.254350963814,315.336812567544,
315.419273505396,315.501733804768,315.584193493056,315.666652597654,315.749111145955,
315.831569165347,315.91402668322,316.000703641305,316.083170426846,316.165635539914,
316.248099090161,316.330561187221,316.413021940702,316.495481460198,316.577939855283,
316.660397235517,316.742863621203,316.825326822711,316.907787278561,316.990245427116,
317.072711030869,317.155170909257,317.237635020509,317.300858012569),
 .UNSPECIFIED.);
#3408=B_SPLINE_CURVE_WITH_KNOTS('',3,(#57384,#57385,#57386,#57387,#57388,
#57389,#57390,#57391,#57392,#57393,#57394,#57395,#57396,#57397,#57398,#57399,
#57400,#57401,#57402,#57403,#57404,#57405,#57406,#57407,#57408,#57409,#57410,
#57411,#57412,#57413,#57414,#57415,#57416,#57417,#57418,#57419,#57420,#57421,
#57422,#57423,#57424,#57425,#57426,#57427,#57428,#57429,#57430,#57431,#57432,
#57433,#57434,#57435,#57436,#57437,#57438,#57439,#57440,#57441,#57442,#57443,
#57444,#57445,#57446,#57447,#57448,#57449,#57450,#57451,#57452,#57453,#57454,
#57455,#57456,#57457,#57458,#57459,#57460,#57461,#57462,#57463,#57464,#57465,
#57466,#57467,#57468),.UNSPECIFIED.,.F.,.F.,(4,3,3,3,3,3,3,3,3,3,3,3,3,
3,3,3,3,3,3,3,3,3,3,3,3,3,3,3,4),(315.254776117011,315.336001919561,315.366687961249,
315.446099159728,315.525528784276,315.604987595228,315.684519418683,315.764092945111,
315.843750069076,315.865459151911,315.943847530919,316.022169795362,316.10044034482,
316.178673541364,316.256883719042,316.335101854425,316.413327919644,316.491574901202,
316.569855795417,316.648229223171,316.726652221494,316.805191780685,316.863001533236,
316.944912825012,317.026643855742,317.108125228796,317.189456846659,317.270585182372,
317.300858012569),.UNSPECIFIED.);
#3409=B_SPLINE_CURVE_WITH_KNOTS('',3,(#57469,#57470,#57471,#57472,#57473,
#57474,#57475,#57476,#57477,#57478,#57479,#57480,#57481,#57482,#57483,#57484,
#57485,#57486,#57487,#57488,#57489,#57490,#57491,#57492,#57493,#57494,#57495,
#57496,#57497,#57498,#57499,#57500,#57501,#57502,#57503,#57504,#57505,#57506,
#57507,#57508,#57509,#57510,#57511,#57512,#57513,#57514,#57515,#57516,#57517,
#57518,#57519,#57520,#57521,#57522,#57523,#57524,#57525,#57526,#57527,#57528,
#57529,#57530,#57531,#57532,#57533,#57534,#57535,#57536,#57537,#57538,#57539,
#57540,#57541,#57542,#57543,#57544,#57545,#57546,#57547,#57548,#57549,#57550,
#57551,#57552,#57553,#57554,#57555,#57556,#57557,#57558,#57559,#57560,#57561,
#57562,#57563,#57564,#57565,#57566,#57567,#57568,#57569,#57570,#57571,#57572,
#57573,#57574,#57575,#57576,#57577,#57578,#57579,#57580,#57581,#57582,#57583,
#57584,#57585,#57586,#57587,#57588,#57589,#57590,#57591,#57592,#57593,#57594,
#57595,#57596,#57597,#57598,#57599,#57600,#57601,#57602,#57603,#57604,#57605,
#57606,#57607,#57608,#57609,#57610,#57611,#57612,#57613,#57614,#57615,#57616,
#57617,#57618,#57619,#57620,#57621,#57622,#57623,#57624,#57625),
 .UNSPECIFIED.,.F.,.F.,(4,3,3,3,3,3,3,3,3,3,3,3,3,3,3,3,3,3,3,3,3,3,3,3,
3,3,3,3,3,3,3,3,3,3,3,3,3,3,3,3,3,3,3,3,3,3,3,3,3,3,3,3,4),(317.300858012569,
317.383320218669,317.465782076472,317.548243592827,317.630704774585,317.713165628595,
317.795626161707,317.87808638077,317.960546292633,318.043005904145,318.125465222154,
318.207924253507,318.290383005054,318.372841483642,318.455299696117,318.537757649328,
318.620215350121,318.702672805343,318.785130021841,318.871142717127,318.954467515685,
319.036934121277,319.11939988266,319.20186482725,319.284328982458,319.366792375695,
319.449255034366,319.531716985877,319.61417825763,319.696638877023,319.779098871454,
319.861558268318,319.944017095009,320.026475378916,320.108933147429,320.191390427935,
320.275524543126,320.357990541486,320.440454918092,320.522917782588,320.605379244594,
320.687839413713,320.770298399529,320.85275631161,320.938353806533,321.020818543579,
321.103280315965,321.18573956213,321.268196720369,321.350659239451,321.433116910862,
321.515575702055,321.537536270993),.UNSPECIFIED.);
#3410=B_SPLINE_CURVE_WITH_KNOTS('',3,(#57631,#57632,#57633,#57634,#57635,
#57636,#57637,#57638,#57639,#57640,#57641,#57642,#57643,#57644,#57645,#57646,
#57647,#57648,#57649,#57650,#57651,#57652,#57653,#57654,#57655,#57656,#57657,
#57658,#57659,#57660,#57661,#57662,#57663,#57664,#57665,#57666,#57667,#57668,
#57669,#57670,#57671,#57672,#57673,#57674,#57675,#57676,#57677,#57678,#57679,
#57680,#57681,#57682,#57683,#57684,#57685,#57686,#57687,#57688,#57689,#57690,
#57691,#57692,#57693,#57694,#57695,#57696,#57697,#57698,#57699,#57700,#57701,
#57702,#57703,#57704,#57705,#57706,#57707,#57708,#57709,#57710,#57711,#57712,
#57713,#57714,#57715,#57716,#57717,#57718,#57719,#57720,#57721,#57722,#57723,
#57724,#57725,#57726,#57727,#57728,#57729,#57730,#57731,#57732,#57733,#57734,
#57735,#57736,#57737,#57738,#57739,#57740,#57741,#57742,#57743,#57744,#57745,
#57746,#57747,#57748,#57749,#57750,#57751,#57752,#57753,#57754,#57755,#57756,
#57757,#57758,#57759,#57760,#57761,#57762,#57763,#57764,#57765,#57766,#57767,
#57768,#57769,#57770,#57771,#57772,#57773,#57774,#57775,#57776,#57777,#57778,
#57779,#57780,#57781,#57782,#57783,#57784,#57785,#57786,#57787,#57788,#57789,
#57790,#57791,#57792,#57793,#57794,#57795,#57796),.UNSPECIFIED.,.F.,.F.,
(4,3,3,3,3,3,3,3,3,3,3,3,3,3,3,3,3,3,3,3,3,3,3,3,3,3,3,3,3,3,3,3,3,3,3,
3,3,3,3,3,3,3,3,3,3,3,3,3,3,3,3,3,3,3,3,4),(323.584043319834,323.662939677337,
323.741758955307,323.820514918581,323.899221285436,323.977894112601,324.056548709419,
324.135197457686,324.213852733542,324.292559073698,324.371290225758,324.450103140527,
324.522064134618,324.598794712943,324.67545831131,324.752069612538,324.828644379253,
324.905197708647,324.981755106653,325.02083532528,325.105504316898,325.190318768946,
325.275332087183,325.360431502692,325.445650891224,325.519606515943,325.601163495569,
325.682645344536,325.766578435053,325.847905675083,325.933141690844,326.018377706605,
326.097788905084,326.177218529632,326.256677340582,326.336209164037,326.415782690466,
326.49543981443,326.517148897268,326.595537276276,326.673859540719,326.752130090177,
326.830363286721,326.908573464398,326.986791599782,327.065017665001,327.143264646559,
327.221545540774,327.299918968528,327.378341966852,327.456881526042,327.514691278593,
327.591422594397,327.667397616857,327.744507079332,327.821616541808),
 .UNSPECIFIED.);
#3411=B_SPLINE_CURVE_WITH_KNOTS('',3,(#57797,#57798,#57799,#57800,#57801,
#57802,#57803,#57804,#57805,#57806,#57807,#57808,#57809,#57810,#57811,#57812,
#57813,#57814,#57815,#57816,#57817,#57818,#57819,#57820,#57821,#57822,#57823,
#57824,#57825,#57826,#57827,#57828,#57829,#57830,#57831,#57832,#57833,#57834,
#57835,#57836,#57837,#57838,#57839,#57840,#57841,#57842,#57843,#57844,#57845,
#57846,#57847,#57848,#57849,#57850,#57851,#57852,#57853,#57854,#57855,#57856,
#57857,#57858,#57859,#57860,#57861,#57862,#57863,#57864,#57865,#57866,#57867,
#57868,#57869,#57870,#57871,#57872,#57873,#57874,#57875,#57876,#57877,#57878),
 .UNSPECIFIED.,.F.,.F.,(4,3,3,3,3,3,3,3,3,3,3,3,3,3,3,3,3,3,3,3,3,3,3,3,
3,3,3,4),(321.537211865788,321.614772155658,321.692241935962,321.769636854507,
321.846972505409,321.924264440088,322.001536224865,322.078799211522,322.156067436099,
322.233354934908,322.31071612535,322.388116108845,322.465620272822,322.526979371968,
322.611191523429,322.695277551139,322.779158473085,322.862910259119,322.946447906456,
323.025750562631,323.103130328962,323.180528490006,323.257958832578,323.335476126032,
323.413043072006,323.490716363454,323.524521753293,323.584043319749),
 .UNSPECIFIED.);
#3412=B_SPLINE_CURVE_WITH_KNOTS('',3,(#57880,#57881,#57882,#57883,#57884,
#57885,#57886,#57887,#57888,#57889,#57890,#57891,#57892,#57893,#57894,#57895,
#57896,#57897,#57898,#57899,#57900,#57901,#57902,#57903,#57904,#57905,#57906,
#57907,#57908,#57909,#57910,#57911,#57912,#57913,#57914,#57915,#57916,#57917,
#57918,#57919,#57920,#57921,#57922,#57923,#57924,#57925,#57926,#57927,#57928,
#57929,#57930,#57931,#57932,#57933,#57934,#57935,#57936,#57937,#57938,#57939,
#57940,#57941,#57942,#57943,#57944,#57945,#57946,#57947,#57948,#57949,#57950,
#57951,#57952,#57953,#57954,#57955),.UNSPECIFIED.,.F.,.F.,(4,3,3,3,3,3,
3,3,3,3,3,3,3,3,3,3,3,3,3,3,3,3,3,3,3,4),(321.537536270993,321.619997874724,
321.702458812576,321.784919111948,321.867378800236,321.949837904834,322.032296453135,
322.114754472527,322.1972119904,322.283888948484,322.366355734025,322.448820847093,
322.531284397341,322.613746494401,322.696207247882,322.778666767378,322.861125162463,
322.943582542697,323.026048928383,323.108512129891,323.190972585741,323.273430734296,
323.355896338049,323.438356216437,323.520820327689,323.584043319749),
 .UNSPECIFIED.);
#3413=B_SPLINE_CURVE_WITH_KNOTS('',3,(#57956,#57957,#57958,#57959,#57960,
#57961,#57962,#57963,#57964,#57965,#57966,#57967,#57968,#57969,#57970,#57971,
#57972,#57973,#57974,#57975,#57976,#57977,#57978,#57979,#57980,#57981,#57982,
#57983,#57984,#57985,#57986,#57987,#57988,#57989,#57990,#57991,#57992,#57993,
#57994,#57995,#57996,#57997,#57998,#57999,#58000,#58001,#58002,#58003,#58004,
#58005,#58006,#58007,#58008,#58009,#58010,#58011,#58012,#58013,#58014,#58015,
#58016,#58017,#58018,#58019,#58020,#58021,#58022,#58023,#58024,#58025,#58026,
#58027,#58028,#58029,#58030,#58031,#58032,#58033,#58034,#58035,#58036,#58037,
#58038,#58039,#58040,#58041,#58042,#58043,#58044,#58045,#58046,#58047,#58048,
#58049,#58050,#58051,#58052,#58053,#58054,#58055,#58056,#58057,#58058,#58059,
#58060,#58061,#58062,#58063,#58064,#58065,#58066,#58067,#58068,#58069,#58070,
#58071,#58072,#58073,#58074,#58075,#58076,#58077,#58078,#58079,#58080,#58081,
#58082,#58083,#58084,#58085,#58086,#58087,#58088,#58089,#58090,#58091,#58092,
#58093,#58094,#58095,#58096,#58097,#58098,#58099,#58100,#58101,#58102,#58103,
#58104,#58105,#58106,#58107,#58108,#58109,#58110,#58111,#58112,#58113,#58114,
#58115,#58116,#58117,#58118,#58119,#58120,#58121),.UNSPECIFIED.,.F.,.F.,
(4,3,3,3,3,3,3,3,3,3,3,3,3,3,3,3,3,3,3,3,3,3,3,3,3,3,3,3,3,3,3,3,3,3,3,
3,3,3,3,3,3,3,3,3,3,3,3,3,3,3,3,3,3,3,3,4),(323.584043319749,323.690372261978,
323.800918922704,323.84579820251,323.921869480146,323.997845256593,324.073742313585,
324.149577352398,324.225367012495,324.302613708912,324.378377207173,324.45414803854,
324.529941206373,324.608291050739,324.684215814249,324.763778199042,324.843340583835,
324.920910804778,324.998388945298,325.075790659212,325.153131545507,325.230427159401,
325.307700599015,325.384963834322,325.462230901759,325.539515837263,325.61687383961,
325.694269370667,325.771771037434,325.84088296516,325.925095116621,326.009181144331,
326.093062066277,326.176813852311,326.260351499648,326.339654155823,326.417033922154,
326.494432083197,326.57186242577,326.649379719223,326.726946665197,326.804619956644,
326.838425346485,326.918051138193,326.997604073827,327.077096453802,327.15654053185,
327.239601489672,327.318990669289,327.398371309586,327.477754480676,327.5571512529,
327.63659935889,327.716076312641,327.795620307696,327.821028194423),
 .UNSPECIFIED.);
#3414=B_SPLINE_CURVE_WITH_KNOTS('',3,(#58127,#58128,#58129,#58130,#58131,
#58132,#58133,#58134,#58135,#58136,#58137,#58138,#58139,#58140,#58141,#58142,
#58143,#58144,#58145,#58146,#58147,#58148,#58149,#58150,#58151,#58152,#58153,
#58154,#58155,#58156,#58157,#58158,#58159,#58160,#58161,#58162,#58163,#58164,
#58165,#58166,#58167,#58168,#58169,#58170,#58171,#58172,#58173,#58174,#58175,
#58176,#58177,#58178,#58179,#58180,#58181,#58182,#58183,#58184,#58185,#58186,
#58187,#58188,#58189,#58190,#58191,#58192,#58193,#58194,#58195,#58196,#58197,
#58198,#58199,#58200,#58201,#58202,#58203,#58204,#58205,#58206,#58207,#58208,
#58209,#58210,#58211,#58212,#58213,#58214,#58215,#58216,#58217,#58218,#58219,
#58220,#58221,#58222,#58223,#58224,#58225,#58226,#58227,#58228,#58229,#58230,
#58231,#58232,#58233,#58234,#58235,#58236,#58237,#58238,#58239,#58240,#58241,
#58242,#58243,#58244,#58245,#58246,#58247,#58248,#58249,#58250,#58251,#58252,
#58253,#58254,#58255,#58256,#58257,#58258,#58259,#58260,#58261,#58262,#58263,
#58264,#58265,#58266,#58267,#58268,#58269,#58270,#58271,#58272,#58273,#58274,
#58275,#58276,#58277,#58278,#58279,#58280,#58281,#58282,#58283,#58284,#58285,
#58286,#58287,#58288,#58289,#58290,#58291,#58292,#58293,#58294,#58295),
 .UNSPECIFIED.,.F.,.F.,(4,3,3,3,3,3,3,3,3,3,3,3,3,3,3,3,3,3,3,3,3,3,3,3,
3,3,3,3,3,3,3,3,3,3,3,3,3,3,3,3,3,3,3,3,3,3,3,3,3,3,3,3,3,3,3,3,4),(329.867228626928,
329.943617592086,330.008547231905,330.085926998236,330.163325159279,330.240755501852,
330.318272795305,330.395839741279,330.473513032726,330.507318422567,330.586943610428,
330.666496065305,330.745988087093,330.825431929108,330.904839807006,330.984230241128,
331.063611791877,331.142995529683,331.222392525014,331.301843142139,331.381322161578,
331.46087430123,331.504860803892,331.581591382217,331.658254980583,331.734866281812,
331.811441048527,331.887994377921,331.964551775926,332.003631994555,332.088300986173,
332.173115438222,332.25812875646,332.34322817197,332.428447560503,332.502403185217,
332.583960164843,332.665442013809,332.749375104327,332.830702344356,332.915938360118,
333.00117437588,333.080585574359,333.160015198907,333.239474009857,333.319005833312,
333.398579359741,333.478236483706,333.499945566542,333.57832772668,333.656647218315,
333.734917102583,333.813150409088,333.891367812278,333.969574304964,334.047801090439,
334.103512245329),.UNSPECIFIED.);
#3415=B_SPLINE_CURVE_WITH_KNOTS('',3,(#58296,#58297,#58298,#58299,#58300,
#58301,#58302,#58303,#58304,#58305,#58306,#58307,#58308,#58309,#58310,#58311,
#58312,#58313,#58314,#58315,#58316,#58317,#58318,#58319,#58320,#58321,#58322,
#58323,#58324,#58325,#58326,#58327,#58328,#58329,#58330,#58331,#58332,#58333,
#58334,#58335,#58336,#58337,#58338,#58339,#58340,#58341,#58342,#58343,#58344,
#58345,#58346,#58347,#58348,#58349,#58350,#58351,#58352,#58353,#58354,#58355,
#58356,#58357,#58358,#58359,#58360,#58361,#58362,#58363,#58364,#58365,#58366,
#58367,#58368,#58369,#58370,#58371,#58372,#58373,#58374),.UNSPECIFIED.,
 .F.,.F.,(4,3,3,3,3,3,3,3,3,3,3,3,3,3,3,3,3,3,3,3,3,3,3,3,3,3,4),(327.821616541808,
327.897404677541,327.974258300338,328.050021802456,328.125793182404,328.201587443917,
328.279248997918,328.355175127646,328.433704393782,328.512233659918,328.589803880861,
328.667282021381,328.744683735295,328.82202462159,328.899320235484,328.976593675098,
329.053856910405,329.131123977842,329.208408913346,329.285766915693,329.36316244675,
329.440664113517,329.509776041242,329.599849599845,329.689690847903,329.778994110244,
329.867228626851),.UNSPECIFIED.);
#3416=B_SPLINE_CURVE_WITH_KNOTS('',3,(#58376,#58377,#58378,#58379,#58380,
#58381,#58382,#58383,#58384,#58385,#58386,#58387,#58388,#58389,#58390,#58391,
#58392,#58393,#58394,#58395,#58396,#58397,#58398,#58399,#58400,#58401,#58402,
#58403,#58404,#58405,#58406,#58407,#58408,#58409,#58410,#58411,#58412,#58413,
#58414,#58415,#58416,#58417,#58418,#58419,#58420,#58421,#58422,#58423,#58424,
#58425,#58426,#58427,#58428,#58429,#58430,#58431,#58432,#58433,#58434,#58435,
#58436,#58437,#58438,#58439,#58440,#58441,#58442,#58443,#58444,#58445,#58446,
#58447,#58448,#58449,#58450,#58451,#58452,#58453,#58454,#58455,#58456,#58457,
#58458,#58459,#58460),.UNSPECIFIED.,.F.,.F.,(4,3,3,3,3,3,3,3,3,3,3,3,3,
3,3,3,3,3,3,3,3,3,3,3,3,3,3,3,4),(327.821028194423,327.83596772781,327.912698306135,
327.989361904502,328.06597320573,328.142547972445,328.21910130184,328.295658699845,
328.334738918472,328.419407910089,328.504222362138,328.589235680374,328.674335095884,
328.759554484416,328.833510109135,328.915067088762,328.996548937728,329.080482028246,
329.161809268276,329.247045284036,329.332281299797,329.411692498275,329.491122122823,
329.570580933772,329.650112757227,329.729686283655,329.80934340762,329.83105249046,
329.867228626928),.UNSPECIFIED.);
#3417=B_SPLINE_CURVE_WITH_KNOTS('',3,(#58461,#58462,#58463,#58464,#58465,
#58466,#58467,#58468,#58469,#58470,#58471,#58472,#58473,#58474,#58475,#58476,
#58477,#58478,#58479,#58480,#58481,#58482,#58483,#58484,#58485,#58486,#58487,
#58488,#58489,#58490,#58491,#58492,#58493,#58494,#58495,#58496,#58497,#58498,
#58499,#58500,#58501,#58502,#58503,#58504,#58505,#58506,#58507,#58508,#58509,
#58510,#58511,#58512,#58513,#58514,#58515,#58516,#58517,#58518,#58519,#58520,
#58521,#58522,#58523,#58524,#58525,#58526,#58527,#58528,#58529,#58530,#58531,
#58532,#58533,#58534,#58535,#58536,#58537,#58538,#58539,#58540,#58541,#58542,
#58543,#58544,#58545,#58546,#58547,#58548,#58549,#58550,#58551,#58552,#58553,
#58554,#58555,#58556,#58557,#58558,#58559,#58560,#58561,#58562,#58563,#58564,
#58565,#58566,#58567,#58568,#58569,#58570,#58571,#58572,#58573,#58574,#58575,
#58576,#58577,#58578,#58579,#58580,#58581,#58582,#58583,#58584,#58585,#58586,
#58587,#58588,#58589,#58590,#58591,#58592,#58593,#58594,#58595,#58596,#58597,
#58598,#58599,#58600,#58601,#58602,#58603,#58604,#58605,#58606,#58607,#58608,
#58609,#58610,#58611,#58612,#58613,#58614,#58615,#58616,#58617,#58618,#58619,
#58620,#58621,#58622,#58623,#58624,#58625,#58626,#58627,#58628,#58629),
 .UNSPECIFIED.,.F.,.F.,(4,3,3,3,3,3,3,3,3,3,3,3,3,3,3,3,3,3,3,3,3,3,3,3,
3,3,3,3,3,3,3,3,3,3,3,3,3,3,3,3,3,3,3,3,3,3,3,3,3,3,3,3,3,3,3,3,4),(329.867228627004,
329.94526820949,330.023241864104,330.101164479558,330.179050907982,330.260243903457,
330.338119015045,330.4160050831,330.493915536161,330.571863814,330.649904125189,
330.727998408715,330.806198926277,330.828594871785,330.904666149421,330.980641925868,
331.05653898286,331.132374021673,331.20816368177,331.285410378187,331.361173876448,
331.436944707815,331.512737875648,331.591087720014,331.667012483524,331.746574868317,
331.82613725311,331.903707474053,331.981185614573,332.058587328486,332.135928214781,
332.213223828676,332.29049726829,332.367760503597,332.445027571034,332.522312506538,
332.599670508884,332.677066039942,332.754567706709,332.823679634434,332.907891785895,
332.991977813603,333.07585873555,333.159610521584,333.24314816892,333.322450825097,
333.399830591428,333.477228752471,333.554659095044,333.632176388497,333.709743334471,
333.787416625919,333.821222015759,333.900842101732,333.9803980806,334.059886867007,
334.104199260309),.UNSPECIFIED.);
#3418=B_SPLINE_CURVE_WITH_KNOTS('',3,(#58635,#58636,#58637,#58638,#58639,
#58640,#58641,#58642,#58643,#58644,#58645,#58646,#58647,#58648,#58649,#58650,
#58651,#58652,#58653,#58654,#58655,#58656,#58657,#58658,#58659,#58660,#58661,
#58662,#58663,#58664,#58665,#58666,#58667,#58668,#58669,#58670,#58671,#58672,
#58673,#58674,#58675,#58676,#58677,#58678,#58679,#58680,#58681,#58682,#58683,
#58684,#58685,#58686,#58687,#58688,#58689,#58690,#58691,#58692,#58693,#58694,
#58695,#58696,#58697,#58698,#58699,#58700,#58701,#58702,#58703,#58704,#58705,
#58706,#58707,#58708,#58709,#58710,#58711,#58712,#58713,#58714,#58715,#58716,
#58717,#58718,#58719,#58720,#58721,#58722,#58723,#58724,#58725,#58726,#58727,
#58728,#58729,#58730,#58731,#58732,#58733,#58734,#58735,#58736,#58737,#58738,
#58739,#58740,#58741,#58742,#58743,#58744,#58745,#58746,#58747,#58748,#58749,
#58750,#58751,#58752,#58753,#58754,#58755,#58756,#58757,#58758,#58759,#58760,
#58761,#58762,#58763,#58764,#58765,#58766,#58767,#58768,#58769,#58770,#58771,
#58772,#58773,#58774,#58775,#58776,#58777,#58778,#58779,#58780,#58781,#58782,
#58783,#58784,#58785,#58786,#58787,#58788,#58789,#58790,#58791,#58792,#58793,
#58794,#58795,#58796,#58797),.UNSPECIFIED.,.F.,.F.,(4,3,3,3,3,3,3,3,3,3,
3,3,3,3,3,3,3,3,3,3,3,3,3,3,3,3,3,3,3,3,3,3,3,3,3,3,3,3,3,3,3,3,3,3,3,3,
3,3,3,3,3,3,3,3,4),(336.150413934233,336.236030499722,336.321889399997,
336.408114041914,336.492572710517,336.576784861978,336.660870889689,336.744751811636,
336.82850359767,336.912041245007,336.991343901179,337.068723667509,337.146121828553,
337.223552171125,337.301069464577,337.378636410551,337.456309701998,337.490115091842,
337.569740279703,337.64929273458,337.728784756368,337.808228598383,337.887636476281,
337.967026910403,338.046408461153,338.125792198958,338.205189194289,338.284639811415,
338.364118830854,338.443670970506,338.487657473166,338.564388051491,338.641051649857,
338.717662951085,338.7942377178,338.870791047194,338.947348445198,338.986428663829,
339.071097655448,339.155912107497,339.240925425735,339.326024841245,339.411244229778,
339.485199854491,339.566756834117,339.648238683083,339.7321717736,339.81349901363,
339.898735029392,339.983971045154,340.063375337463,340.144249967054,340.223725417313,
340.30529963657,340.386873855827),.UNSPECIFIED.);
#3419=B_SPLINE_CURVE_WITH_KNOTS('',3,(#58798,#58799,#58800,#58801,#58802,
#58803,#58804,#58805,#58806,#58807,#58808,#58809,#58810,#58811,#58812,#58813,
#58814,#58815,#58816,#58817,#58818,#58819,#58820,#58821,#58822,#58823,#58824,
#58825,#58826,#58827,#58828,#58829,#58830,#58831,#58832,#58833,#58834,#58835,
#58836,#58837,#58838,#58839,#58840,#58841,#58842,#58843,#58844,#58845,#58846,
#58847,#58848,#58849,#58850,#58851,#58852,#58853,#58854,#58855,#58856,#58857,
#58858,#58859,#58860,#58861,#58862,#58863,#58864,#58865,#58866,#58867,#58868,
#58869,#58870,#58871,#58872,#58873,#58874,#58875,#58876,#58877,#58878,#58879),
 .UNSPECIFIED.,.F.,.F.,(4,3,3,3,3,3,3,3,3,3,3,3,3,3,3,3,3,3,3,3,3,3,3,3,
3,3,3,4),(334.103512245329,334.181782034169,334.260708512593,334.339116405703,
334.418302176785,334.497487947867,334.573559225503,334.64953500195,334.725432058942,
334.801267097755,334.877056757853,334.95430345427,335.030066952531,335.105837783897,
335.181630951731,335.259980796096,335.335905559607,335.415467944399,335.495030329192,
335.576953279807,335.65566819483,335.734299732993,335.812860488271,335.891363009308,
335.96981408632,336.048235026965,336.126640203039,336.150413934108),
 .UNSPECIFIED.);
#3420=B_SPLINE_CURVE_WITH_KNOTS('',3,(#58881,#58882,#58883,#58884,#58885,
#58886,#58887,#58888,#58889,#58890,#58891,#58892,#58893,#58894,#58895,#58896,
#58897,#58898,#58899,#58900,#58901,#58902,#58903,#58904,#58905,#58906,#58907,
#58908,#58909,#58910,#58911,#58912,#58913,#58914,#58915,#58916,#58917,#58918,
#58919,#58920,#58921,#58922,#58923,#58924,#58925,#58926,#58927,#58928,#58929,
#58930,#58931,#58932,#58933,#58934,#58935,#58936,#58937,#58938,#58939,#58940,
#58941,#58942,#58943,#58944,#58945,#58946,#58947,#58948,#58949,#58950,#58951,
#58952,#58953,#58954,#58955,#58956,#58957,#58958,#58959),.UNSPECIFIED.,
 .F.,.F.,(4,3,3,3,3,3,3,3,3,3,3,3,3,3,3,3,3,3,3,3,3,3,3,3,3,3,4),(334.104199260309,
334.183621542074,334.263019438394,334.342403552811,334.421784958005,334.501174723552,
334.580616024033,334.660081231601,334.739626247106,334.818764397084,334.895494975409,
334.972158573775,335.048769875004,335.125344641718,335.201897971113,335.278455369118,
335.317535587747,335.402204579365,335.487019031413,335.572032349651,335.657131765161,
335.742351153693,335.816306778409,335.900123568842,335.98385277894,336.067438212658,
336.150413934108),.UNSPECIFIED.);
#3421=B_SPLINE_CURVE_WITH_KNOTS('',3,(#58960,#58961,#58962,#58963,#58964,
#58965,#58966,#58967,#58968,#58969,#58970,#58971,#58972,#58973,#58974,#58975,
#58976,#58977,#58978,#58979,#58980,#58981,#58982,#58983,#58984,#58985,#58986,
#58987,#58988,#58989,#58990,#58991,#58992,#58993,#58994,#58995,#58996,#58997,
#58998,#58999,#59000,#59001,#59002,#59003,#59004,#59005,#59006,#59007,#59008,
#59009,#59010,#59011,#59012,#59013,#59014,#59015,#59016,#59017,#59018,#59019,
#59020,#59021,#59022,#59023,#59024,#59025,#59026,#59027,#59028,#59029,#59030,
#59031,#59032,#59033,#59034,#59035,#59036,#59037,#59038,#59039,#59040,#59041,
#59042,#59043,#59044,#59045,#59046,#59047,#59048,#59049,#59050,#59051,#59052,
#59053,#59054,#59055,#59056,#59057,#59058,#59059,#59060,#59061,#59062,#59063,
#59064,#59065,#59066,#59067,#59068,#59069,#59070,#59071,#59072,#59073,#59074,
#59075,#59076,#59077,#59078,#59079,#59080,#59081,#59082,#59083,#59084,#59085,
#59086,#59087,#59088,#59089,#59090,#59091,#59092,#59093,#59094,#59095,#59096,
#59097,#59098,#59099,#59100,#59101,#59102,#59103,#59104,#59105,#59106,#59107,
#59108,#59109,#59110,#59111,#59112,#59113,#59114,#59115,#59116),
 .UNSPECIFIED.,.F.,.F.,(4,3,3,3,3,3,3,3,3,3,3,3,3,3,3,3,3,3,3,3,3,3,3,3,
3,3,3,3,3,3,3,3,3,3,3,3,3,3,3,3,3,3,3,3,3,3,3,3,3,3,3,3,4),(336.150413934108,
336.232876140208,336.315337998011,336.397799514366,336.480260696124,336.562721550134,
336.645182083246,336.727642302309,336.810102214172,336.892561825684,336.975021143693,
337.057480175047,337.139938926594,337.222397405181,337.304855617657,337.387313570867,
337.46977127166,337.552228726882,337.63468594338,337.720698638666,337.804023437224,
337.886490042816,337.968955804199,338.051420748789,338.133884903997,338.216348297234,
338.298810955905,338.381272907416,338.463734179169,338.546194798562,338.628654792993,
338.711114189857,338.793573016547,338.876031300454,338.958489068967,339.040946349474,
339.125080464665,339.207546463025,339.290010839631,339.372473704127,339.454935166133,
339.537395335252,339.619854321068,339.702312233149,339.787909728071,339.870374465117,
339.952836237504,340.035295483669,340.117752641908,340.20021516099,340.282672832401,
340.365131623594,340.387092192532),.UNSPECIFIED.);
#3422=B_SPLINE_CURVE_WITH_KNOTS('',3,(#59122,#59123,#59124,#59125,#59126,
#59127,#59128,#59129,#59130,#59131,#59132,#59133,#59134,#59135,#59136,#59137,
#59138,#59139,#59140,#59141,#59142,#59143,#59144,#59145,#59146,#59147,#59148,
#59149,#59150,#59151,#59152,#59153,#59154,#59155,#59156,#59157,#59158,#59159,
#59160,#59161,#59162,#59163,#59164,#59165,#59166,#59167,#59168,#59169,#59170,
#59171,#59172,#59173,#59174,#59175,#59176,#59177,#59178,#59179,#59180,#59181,
#59182,#59183,#59184,#59185,#59186,#59187,#59188,#59189,#59190,#59191,#59192,
#59193,#59194,#59195,#59196,#59197,#59198,#59199,#59200,#59201,#59202,#59203,
#59204,#59205,#59206,#59207,#59208,#59209,#59210,#59211,#59212,#59213,#59214,
#59215,#59216,#59217,#59218,#59219,#59220,#59221,#59222,#59223,#59224,#59225,
#59226,#59227,#59228,#59229,#59230,#59231,#59232,#59233,#59234,#59235,#59236,
#59237,#59238,#59239,#59240,#59241,#59242,#59243,#59244,#59245,#59246,#59247,
#59248,#59249,#59250,#59251,#59252,#59253,#59254,#59255,#59256,#59257,#59258,
#59259,#59260,#59261,#59262,#59263,#59264,#59265,#59266,#59267,#59268,#59269,
#59270,#59271,#59272,#59273,#59274,#59275,#59276,#59277,#59278,#59279,#59280,
#59281,#59282,#59283,#59284,#59285,#59286,#59287,#59288,#59289,#59290),
 .UNSPECIFIED.,.F.,.F.,(4,3,3,3,3,3,3,3,3,3,3,3,3,3,3,3,3,3,3,3,3,3,3,3,
3,3,3,3,3,3,3,3,3,3,3,3,3,3,3,3,3,3,3,3,3,3,3,3,3,3,3,3,3,3,3,3,4),(342.433599241288,
342.477826998466,342.555397219409,342.632875359929,342.710277073842,342.787617960137,
342.864913574031,342.942187013645,343.019450248952,343.096717316389,343.174002251893,
343.251360254239,343.328755785296,343.406257452063,343.475369379791,343.559581531252,
343.643667558962,343.727548480909,343.811300266943,343.89483791428,343.974140570453,
344.051520336784,344.128918497827,344.2063488404,344.283866133853,344.361433079827,
344.439106371274,344.472911761116,344.552536948977,344.632089403854,344.711581425642,
344.791025267657,344.870433145555,344.949823579677,345.029205130426,345.108588868232,
345.187985863562,345.267436480688,345.346915500127,345.426467639779,345.470454142441,
345.547184720766,345.623848319133,345.700459620361,345.777034387076,345.85358771647,
345.930145114475,345.969225333103,346.053894324721,346.138708776769,346.223722095006,
346.308821510515,346.394040899047,346.467996523766,346.549562547653,346.631038481119,
346.670772567163),.UNSPECIFIED.);
#3423=B_SPLINE_CURVE_WITH_KNOTS('',3,(#59291,#59292,#59293,#59294,#59295,
#59296,#59297,#59298,#59299,#59300,#59301,#59302,#59303,#59304,#59305,#59306,
#59307,#59308,#59309,#59310,#59311,#59312,#59313,#59314,#59315,#59316,#59317,
#59318,#59319,#59320,#59321,#59322,#59323,#59324,#59325,#59326,#59327,#59328,
#59329,#59330,#59331,#59332,#59333,#59334,#59335,#59336,#59337,#59338,#59339,
#59340,#59341,#59342,#59343,#59344,#59345,#59346,#59347,#59348,#59349,#59350,
#59351,#59352,#59353,#59354,#59355,#59356,#59357,#59358,#59359,#59360,#59361,
#59362,#59363,#59364,#59365,#59366,#59367,#59368,#59369,#59370,#59371,#59372,
#59373,#59374,#59375),.UNSPECIFIED.,.F.,.F.,(4,3,3,3,3,3,3,3,3,3,3,3,3,
3,3,3,3,3,3,3,3,3,3,3,3,3,3,3,4),(340.386873855827,340.466533053165,340.482742235816,
340.561130614824,340.639452879266,340.717723428725,340.795956625269,340.874166802946,
340.952384938329,341.030611003548,341.108857985106,341.187138879321,341.265512307075,
341.343935305399,341.422474864589,341.480284617141,341.555819702447,341.631260231986,
341.706623272285,341.781925791665,341.857184684089,341.93242693873,342.007663131993,
342.082908485691,342.15817823038,342.233530905522,342.308928811165,342.384438784184,
342.433599241167),.UNSPECIFIED.);
#3424=B_SPLINE_CURVE_WITH_KNOTS('',3,(#59377,#59378,#59379,#59380,#59381,
#59382,#59383,#59384,#59385,#59386,#59387,#59388,#59389,#59390,#59391,#59392,
#59393,#59394,#59395,#59396,#59397,#59398,#59399,#59400,#59401,#59402,#59403,
#59404,#59405,#59406,#59407,#59408,#59409,#59410,#59411,#59412,#59413,#59414,
#59415,#59416,#59417,#59418,#59419,#59420,#59421,#59422,#59423,#59424,#59425,
#59426,#59427,#59428,#59429,#59430,#59431,#59432,#59433,#59434,#59435,#59436,
#59437,#59438,#59439,#59440,#59441,#59442,#59443,#59444,#59445,#59446,#59447,
#59448,#59449,#59450,#59451,#59452),.UNSPECIFIED.,.F.,.F.,(4,3,3,3,3,3,
3,3,3,3,3,3,3,3,3,3,3,3,3,3,3,3,3,3,3,4),(340.387092192532,340.469553796262,
340.552014734114,340.634475033486,340.716934721774,340.799393826373,340.881852374673,
340.964310394066,341.046767911938,341.133444870023,341.215911655564,341.298376768632,
341.38084031888,341.463302415939,341.54576316942,341.628222688916,341.710681084001,
341.793138464235,341.875604849921,341.958068051429,342.040528507279,342.122986655834,
342.205452259587,342.287912137975,342.370376249227,342.433599241287),
 .UNSPECIFIED.);
#3425=B_SPLINE_CURVE_WITH_KNOTS('',3,(#59453,#59454,#59455,#59456,#59457,
#59458,#59459,#59460,#59461,#59462,#59463,#59464,#59465,#59466,#59467,#59468,
#59469,#59470,#59471,#59472,#59473,#59474,#59475,#59476,#59477,#59478,#59479,
#59480,#59481,#59482,#59483,#59484,#59485,#59486,#59487,#59488,#59489,#59490,
#59491,#59492,#59493,#59494,#59495,#59496,#59497,#59498,#59499,#59500,#59501,
#59502,#59503,#59504,#59505,#59506,#59507,#59508,#59509,#59510,#59511,#59512,
#59513,#59514,#59515,#59516,#59517,#59518,#59519,#59520,#59521,#59522,#59523,
#59524,#59525,#59526,#59527,#59528,#59529,#59530,#59531,#59532,#59533,#59534,
#59535,#59536,#59537,#59538,#59539,#59540,#59541,#59542,#59543,#59544,#59545,
#59546,#59547,#59548,#59549,#59550,#59551,#59552,#59553,#59554,#59555,#59556,
#59557,#59558,#59559,#59560,#59561,#59562,#59563,#59564,#59565,#59566,#59567,
#59568,#59569,#59570,#59571,#59572,#59573,#59574,#59575,#59576,#59577,#59578,
#59579,#59580,#59581,#59582,#59583,#59584,#59585,#59586,#59587,#59588,#59589,
#59590,#59591,#59592,#59593,#59594,#59595,#59596,#59597,#59598,#59599,#59600,
#59601,#59602,#59603,#59604,#59605,#59606,#59607,#59608,#59609,#59610,#59611,
#59612,#59613,#59614,#59615,#59616,#59617,#59618,#59619,#59620,#59621),
 .UNSPECIFIED.,.F.,.F.,(4,3,3,3,3,3,3,3,3,3,3,3,3,3,3,3,3,3,3,3,3,3,3,3,
3,3,3,3,3,3,3,3,3,3,3,3,3,3,3,3,3,3,3,3,3,3,3,3,3,3,3,3,3,3,3,3,4),(342.433599241287,
342.524975292886,342.612060527846,342.699260153072,342.786567572675,342.799103447683,
342.880660427309,342.962142276275,343.046075366793,343.127402606822,343.212638622584,
343.297874638346,343.377285836825,343.456715461373,343.536174272323,343.615706095778,
343.695279622207,343.774936746172,343.796645829008,343.875034208016,343.953356472458,
344.031627021917,344.109860218461,344.188070396138,344.266288531521,344.34451459674,
344.422761578298,344.501042472512,344.579415900267,344.65783889859,344.73637845778,
344.794188210333,344.870259487969,344.946235264416,345.022132321408,345.097967360221,
345.173757020318,345.251003716736,345.326767214997,345.402538046363,345.478331214197,
345.556681058562,345.632605822073,345.712168206865,345.791730591658,345.869307666084,
345.946791336978,346.024197263591,346.104882624974,346.182175985526,346.259443837389,
346.336700224768,346.413959182672,346.491259938658,346.568585405038,346.645976866206,
346.669680154653),.UNSPECIFIED.);
#3426=B_SPLINE_CURVE_WITH_KNOTS('',3,(#59627,#59628,#59629,#59630,#59631,
#59632,#59633,#59634,#59635,#59636,#59637,#59638,#59639,#59640,#59641,#59642,
#59643,#59644,#59645,#59646,#59647,#59648,#59649,#59650,#59651,#59652,#59653,
#59654,#59655,#59656,#59657,#59658,#59659,#59660,#59661,#59662,#59663,#59664,
#59665,#59666,#59667,#59668,#59669,#59670,#59671,#59672,#59673,#59674,#59675,
#59676,#59677,#59678,#59679,#59680,#59681,#59682,#59683,#59684,#59685,#59686,
#59687,#59688,#59689,#59690,#59691,#59692,#59693,#59694,#59695,#59696,#59697,
#59698,#59699,#59700,#59701,#59702,#59703,#59704,#59705,#59706,#59707,#59708,
#59709,#59710,#59711,#59712,#59713,#59714,#59715,#59716,#59717,#59718,#59719,
#59720,#59721,#59722,#59723,#59724,#59725,#59726,#59727,#59728,#59729,#59730,
#59731,#59732,#59733,#59734,#59735,#59736,#59737,#59738,#59739,#59740,#59741,
#59742,#59743,#59744,#59745,#59746,#59747,#59748,#59749,#59750,#59751,#59752,
#59753,#59754,#59755,#59756,#59757,#59758,#59759,#59760,#59761,#59762,#59763,
#59764,#59765,#59766,#59767,#59768,#59769,#59770,#59771,#59772,#59773,#59774,
#59775,#59776,#59777,#59778,#59779,#59780,#59781,#59782,#59783),
 .UNSPECIFIED.,.F.,.F.,(4,3,3,3,3,3,3,3,3,3,3,3,3,3,3,3,3,3,3,3,3,3,3,3,
3,3,3,3,3,3,3,3,3,3,3,3,3,3,3,3,3,3,3,3,3,3,3,3,3,3,3,3,4),(348.716784548467,
348.799246754567,348.88170861237,348.964170128725,349.046631310483,349.129092164493,
349.211552697605,349.294012916668,349.376472828531,349.458932440043,349.541391758052,
349.623850789406,349.706309540952,349.78876801954,349.871226232016,349.953684185226,
350.036141886019,350.118599341241,350.201056557739,350.287069253025,350.370394051583,
350.452860657175,350.535326418558,350.617791363148,350.700255518356,350.782718911593,
350.865181570264,350.947643521776,351.030104793528,351.112565412921,351.195025407352,
351.277484804216,351.359943630907,351.442401914814,351.524859683327,351.607316963833,
351.691451079024,351.773917077384,351.85638145399,351.938844318486,352.021305780492,
352.103765949611,352.186224935427,352.268682847508,352.354280342431,352.436745079477,
352.519206851863,352.601666098028,352.684123256267,352.766585775349,352.84904344676,
352.931502237953,352.953462806892),.UNSPECIFIED.);
#3427=B_SPLINE_CURVE_WITH_KNOTS('',3,(#59784,#59785,#59786,#59787,#59788,
#59789,#59790,#59791,#59792,#59793,#59794,#59795,#59796,#59797,#59798,#59799,
#59800,#59801,#59802,#59803,#59804,#59805,#59806,#59807,#59808,#59809,#59810,
#59811,#59812,#59813,#59814,#59815,#59816,#59817,#59818,#59819,#59820,#59821,
#59822,#59823,#59824,#59825,#59826,#59827,#59828,#59829,#59830,#59831,#59832,
#59833,#59834,#59835,#59836,#59837,#59838,#59839,#59840,#59841,#59842,#59843,
#59844,#59845,#59846,#59847,#59848,#59849,#59850,#59851,#59852,#59853,#59854,
#59855,#59856,#59857,#59858,#59859,#59860,#59861,#59862,#59863,#59864,#59865),
 .UNSPECIFIED.,.F.,.F.,(4,3,3,3,3,3,3,3,3,3,3,3,3,3,3,3,3,3,3,3,3,3,3,3,
3,3,3,4),(346.670772567163,346.752130912072,346.833433265937,346.914669680485,
346.966767714428,347.046178912906,347.125608537454,347.205067348404,347.284599171859,
347.364172698288,347.443829822252,347.465538905091,347.543927284099,347.622249548542,
347.700520098,347.778753294544,347.856963472221,347.935181607604,348.013407672824,
348.091654654381,348.169935548596,348.248308976351,348.326731974674,348.405271533864,
348.463081286415,348.559444813209,348.654143106288,348.716784548467),
 .UNSPECIFIED.);
#3428=B_SPLINE_CURVE_WITH_KNOTS('',3,(#59867,#59868,#59869,#59870,#59871,
#59872,#59873,#59874,#59875,#59876,#59877,#59878,#59879,#59880,#59881,#59882,
#59883,#59884,#59885,#59886,#59887,#59888,#59889,#59890,#59891,#59892,#59893,
#59894,#59895,#59896,#59897,#59898,#59899,#59900,#59901,#59902,#59903,#59904,
#59905,#59906,#59907,#59908,#59909,#59910,#59911,#59912,#59913,#59914,#59915,
#59916,#59917,#59918,#59919,#59920,#59921,#59922,#59923,#59924,#59925,#59926,
#59927,#59928,#59929,#59930,#59931,#59932,#59933,#59934,#59935,#59936,#59937,
#59938,#59939,#59940,#59941,#59942,#59943,#59944,#59945,#59946,#59947,#59948),
 .UNSPECIFIED.,.F.,.F.,(4,3,3,3,3,3,3,3,3,3,3,3,3,3,3,3,3,3,3,3,3,3,3,3,
3,3,3,4),(346.669680154653,346.747191203291,346.789272972983,346.873485124444,
346.957571152154,347.041452074101,347.125203860135,347.208741507471,347.288044163645,
347.365423929975,347.442822091019,347.520252433591,347.597769727044,347.675336673018,
347.753009964465,347.786815354308,347.865689846335,347.944489604546,348.023228416047,
348.10192002307,348.180581543913,348.259227091072,348.337869072739,348.416519892818,
348.495224142986,348.573955300432,348.652768292807,348.716784548467),
 .UNSPECIFIED.);
#3429=B_SPLINE_CURVE_WITH_KNOTS('',3,(#59949,#59950,#59951,#59952,#59953,
#59954,#59955,#59956,#59957,#59958,#59959,#59960,#59961,#59962,#59963,#59964,
#59965,#59966,#59967,#59968,#59969,#59970,#59971,#59972,#59973,#59974,#59975,
#59976,#59977,#59978,#59979,#59980,#59981,#59982,#59983,#59984,#59985,#59986,
#59987,#59988,#59989,#59990,#59991,#59992,#59993,#59994,#59995,#59996,#59997,
#59998,#59999,#60000,#60001,#60002,#60003,#60004,#60005,#60006,#60007,#60008,
#60009,#60010,#60011,#60012,#60013,#60014,#60015,#60016,#60017,#60018,#60019,
#60020,#60021,#60022,#60023,#60024,#60025,#60026,#60027,#60028,#60029,#60030,
#60031,#60032,#60033,#60034,#60035,#60036,#60037,#60038,#60039,#60040,#60041,
#60042,#60043,#60044,#60045,#60046,#60047,#60048,#60049,#60050,#60051,#60052,
#60053,#60054,#60055,#60056,#60057,#60058,#60059,#60060,#60061,#60062,#60063,
#60064,#60065,#60066,#60067,#60068,#60069,#60070,#60071,#60072,#60073,#60074,
#60075,#60076,#60077,#60078,#60079,#60080,#60081,#60082,#60083,#60084,#60085,
#60086,#60087,#60088,#60089,#60090,#60091,#60092,#60093,#60094,#60095,#60096,
#60097,#60098,#60099,#60100,#60101,#60102,#60103,#60104,#60105),
 .UNSPECIFIED.,.F.,.F.,(4,3,3,3,3,3,3,3,3,3,3,3,3,3,3,3,3,3,3,3,3,3,3,3,
3,3,3,3,3,3,3,3,3,3,3,3,3,3,3,3,3,3,3,3,3,3,3,3,3,3,3,3,4),(348.716784548467,
348.799246754567,348.88170861237,348.964170128725,349.046631310483,349.129092164493,
349.211552697605,349.294012916668,349.376472828531,349.458932440043,349.541391758052,
349.623850789406,349.706309540952,349.78876801954,349.871226232015,349.953684185226,
350.036141886019,350.118599341241,350.201056557739,350.287069253025,350.370394051583,
350.452860657175,350.535326418558,350.617791363148,350.700255518356,350.782718911593,
350.865181570265,350.947643521776,351.030104793528,351.112565412921,351.195025407353,
351.277484804217,351.359943630907,351.442401914814,351.524859683327,351.607316963833,
351.691451079025,351.773917077384,351.856381453991,351.938844318486,352.021305780492,
352.103765949612,352.186224935428,352.268682847508,352.354280342431,352.436745079477,
352.519206851863,352.601666098028,352.684123256267,352.76658577535,352.849043446761,
352.931502237954,352.953462806892),.UNSPECIFIED.);
#3430=B_SPLINE_CURVE_WITH_KNOTS('',3,(#60111,#60112,#60113,#60114,#60115,
#60116,#60117,#60118,#60119,#60120,#60121,#60122,#60123,#60124,#60125,#60126,
#60127,#60128,#60129,#60130,#60131,#60132,#60133,#60134,#60135,#60136,#60137,
#60138,#60139,#60140,#60141,#60142,#60143,#60144,#60145,#60146,#60147,#60148,
#60149,#60150,#60151,#60152,#60153,#60154,#60155,#60156,#60157,#60158,#60159,
#60160,#60161,#60162,#60163,#60164,#60165,#60166,#60167,#60168,#60169,#60170,
#60171,#60172,#60173,#60174,#60175,#60176,#60177,#60178,#60179,#60180,#60181,
#60182,#60183,#60184,#60185,#60186,#60187,#60188,#60189,#60190,#60191,#60192,
#60193,#60194,#60195,#60196,#60197,#60198,#60199,#60200,#60201,#60202,#60203,
#60204,#60205,#60206,#60207,#60208,#60209,#60210,#60211,#60212,#60213,#60214,
#60215,#60216,#60217,#60218,#60219,#60220,#60221,#60222,#60223,#60224,#60225,
#60226,#60227,#60228,#60229,#60230,#60231,#60232,#60233,#60234,#60235,#60236,
#60237,#60238,#60239,#60240,#60241,#60242,#60243,#60244,#60245,#60246,#60247,
#60248,#60249,#60250,#60251,#60252,#60253,#60254,#60255,#60256,#60257,#60258,
#60259,#60260,#60261,#60262,#60263,#60264,#60265,#60266,#60267,#60268,#60269,
#60270,#60271,#60272,#60273),.UNSPECIFIED.,.F.,.F.,(4,3,3,3,3,3,3,3,3,3,
3,3,3,3,3,3,3,3,3,3,3,3,3,3,3,3,3,3,3,3,3,3,3,3,3,3,3,3,3,3,3,3,3,3,3,3,
3,3,3,3,3,3,3,3,4),(354.999969855647,355.086348997711,355.176231237206,
355.26338554274,355.354631749215,355.44587795569,355.521949233326,355.597925009773,
355.673822066765,355.749657105578,355.825446765675,355.902693462092,355.978456960353,
356.05422779172,356.130020959553,356.208370803918,356.284295567429,356.363857952222,
356.443420337015,356.520990557958,356.598468698478,356.675870412391,356.753211298687,
356.830506912581,356.907780352195,356.985043587502,357.062310654939,357.139595590443,
357.216953592789,357.294349123846,357.371850790613,357.440962718339,357.5251748698,
357.609260897509,357.693141819456,357.77689360549,357.860431252827,357.939733909002,
358.017113675332,358.094511836376,358.171942178949,358.249459472402,358.327026418376,
358.404699709823,358.438505099664,358.518138949726,358.597698423346,358.677569110537,
358.75700926755,358.836416212645,358.915801039783,358.996016760055,359.075403334798,
359.156033627834,359.236663920869),.UNSPECIFIED.);
#3431=B_SPLINE_CURVE_WITH_KNOTS('',3,(#60274,#60275,#60276,#60277,#60278,
#60279,#60280,#60281,#60282,#60283,#60284,#60285,#60286,#60287,#60288,#60289,
#60290,#60291,#60292,#60293,#60294,#60295,#60296,#60297,#60298,#60299,#60300,
#60301,#60302,#60303,#60304,#60305,#60306,#60307,#60308,#60309,#60310,#60311,
#60312,#60313,#60314,#60315,#60316,#60317,#60318,#60319,#60320,#60321,#60322,
#60323,#60324,#60325,#60326,#60327,#60328,#60329,#60330,#60331,#60332,#60333,
#60334,#60335,#60336,#60337,#60338,#60339,#60340,#60341,#60342,#60343,#60344,
#60345,#60346,#60347,#60348,#60349),.UNSPECIFIED.,.F.,.F.,(4,3,3,3,3,3,
3,3,3,3,3,3,3,3,3,3,3,3,3,3,3,3,3,3,3,4),(352.953462806892,353.035924410622,
353.118385348474,353.200845647846,353.283305336134,353.365764440732,353.448222989033,
353.530681008425,353.613138526298,353.699815484382,353.782282269923,353.864747382991,
353.947210933239,354.029673030299,354.11213378378,354.194593303276,354.277051698362,
354.359509078595,354.441975464281,354.524438665789,354.606899121639,354.689357270194,
354.771822873948,354.854282752335,354.936746863588,354.999969855647),
 .UNSPECIFIED.);
#3432=B_SPLINE_CURVE_WITH_KNOTS('',3,(#60351,#60352,#60353,#60354,#60355,
#60356,#60357,#60358,#60359,#60360,#60361,#60362,#60363,#60364,#60365,#60366,
#60367,#60368,#60369,#60370,#60371,#60372,#60373,#60374,#60375,#60376,#60377,
#60378,#60379,#60380,#60381,#60382,#60383,#60384,#60385,#60386,#60387,#60388,
#60389,#60390,#60391,#60392,#60393,#60394,#60395,#60396,#60397,#60398,#60399,
#60400,#60401,#60402,#60403,#60404,#60405,#60406,#60407,#60408,#60409,#60410,
#60411,#60412,#60413,#60414,#60415,#60416,#60417,#60418,#60419,#60420,#60421,
#60422,#60423,#60424,#60425,#60426),.UNSPECIFIED.,.F.,.F.,(4,3,3,3,3,3,
3,3,3,3,3,3,3,3,3,3,3,3,3,3,3,3,3,3,3,4),(352.953462806892,353.035924410622,
353.118385348474,353.200845647846,353.283305336134,353.365764440732,353.448222989033,
353.530681008425,353.613138526298,353.699815484375,353.782282269916,353.864747382984,
353.947210933232,354.029673030292,354.112133783773,354.194593303269,354.277051698355,
354.359509078588,354.441975464274,354.524438665782,354.606899121632,354.689357270187,
354.77182287394,354.854282752328,354.93674686358,354.999969855537),
 .UNSPECIFIED.);
#3433=B_SPLINE_CURVE_WITH_KNOTS('',3,(#60427,#60428,#60429,#60430,#60431,
#60432,#60433,#60434,#60435,#60436,#60437,#60438,#60439,#60440,#60441,#60442,
#60443,#60444,#60445,#60446,#60447,#60448,#60449,#60450,#60451,#60452,#60453,
#60454,#60455,#60456,#60457,#60458,#60459,#60460,#60461,#60462,#60463,#60464,
#60465,#60466,#60467,#60468,#60469,#60470,#60471,#60472,#60473,#60474,#60475,
#60476,#60477,#60478,#60479,#60480,#60481,#60482,#60483,#60484,#60485,#60486,
#60487,#60488,#60489,#60490,#60491,#60492,#60493,#60494,#60495,#60496,#60497,
#60498,#60499,#60500,#60501,#60502,#60503,#60504,#60505,#60506,#60507,#60508,
#60509,#60510,#60511,#60512,#60513,#60514,#60515,#60516,#60517,#60518,#60519,
#60520,#60521,#60522,#60523,#60524,#60525,#60526,#60527,#60528,#60529,#60530,
#60531,#60532,#60533,#60534,#60535,#60536,#60537,#60538,#60539,#60540,#60541,
#60542,#60543,#60544,#60545,#60546,#60547,#60548,#60549,#60550,#60551,#60552,
#60553,#60554,#60555,#60556,#60557,#60558,#60559,#60560,#60561,#60562,#60563,
#60564,#60565,#60566,#60567,#60568,#60569,#60570,#60571,#60572,#60573,#60574,
#60575,#60576,#60577,#60578,#60579,#60580,#60581,#60582,#60583),
 .UNSPECIFIED.,.F.,.F.,(4,3,3,3,3,3,3,3,3,3,3,3,3,3,3,3,3,3,3,3,3,3,3,3,
3,3,3,3,3,3,3,3,3,3,3,3,3,3,3,3,3,3,3,3,3,3,3,3,3,3,3,3,4),(354.999969855647,
355.082432061747,355.16489391955,355.247355435905,355.329816617663,355.412277471673,
355.494738004785,355.577198223848,355.659658135711,355.742117747223,355.824577065232,
355.907036096586,355.989494848132,356.07195332672,356.154411539196,356.236869492407,
356.3193271932,356.401784648421,356.484241864919,356.570254560205,356.653579358763,
356.736045964355,356.818511725738,356.900976670328,356.983440825536,357.065904218773,
357.148366877444,357.230828828955,357.313290100708,357.395750720101,357.478210714532,
357.560670111396,357.643128938086,357.725587221993,357.808044990506,357.890502271013,
357.974636386204,358.057102384564,358.13956676117,358.222029625665,358.304491087672,
358.386951256791,358.469410242607,358.551868154687,358.63746564961,358.719930386656,
358.802392159042,358.884851405207,358.967308563446,359.049771082529,359.13222875394,
359.214687545133,359.236648114071),.UNSPECIFIED.);
#3434=B_SPLINE_CURVE_WITH_KNOTS('',3,(#60589,#60590,#60591,#60592,#60593,
#60594,#60595,#60596,#60597,#60598,#60599,#60600,#60601,#60602,#60603,#60604,
#60605,#60606,#60607,#60608,#60609,#60610,#60611,#60612,#60613,#60614,#60615,
#60616,#60617,#60618,#60619,#60620,#60621,#60622,#60623,#60624,#60625,#60626,
#60627,#60628,#60629,#60630,#60631,#60632,#60633,#60634,#60635,#60636,#60637,
#60638,#60639,#60640,#60641,#60642,#60643,#60644,#60645,#60646,#60647,#60648,
#60649,#60650,#60651,#60652,#60653,#60654,#60655,#60656,#60657,#60658,#60659,
#60660,#60661,#60662,#60663,#60664,#60665,#60666,#60667,#60668,#60669,#60670,
#60671,#60672,#60673,#60674,#60675,#60676,#60677,#60678,#60679,#60680,#60681,
#60682,#60683,#60684,#60685,#60686,#60687,#60688,#60689,#60690,#60691,#60692,
#60693,#60694,#60695,#60696,#60697,#60698,#60699,#60700,#60701,#60702,#60703,
#60704,#60705,#60706,#60707,#60708,#60709,#60710,#60711,#60712,#60713,#60714,
#60715,#60716,#60717,#60718,#60719,#60720,#60721,#60722,#60723,#60724,#60725,
#60726,#60727,#60728,#60729,#60730,#60731,#60732,#60733,#60734,#60735,#60736,
#60737,#60738,#60739,#60740,#60741,#60742,#60743,#60744,#60745,#60746,#60747,
#60748,#60749,#60750,#60751,#60752,#60753,#60754,#60755,#60756,#60757),
 .UNSPECIFIED.,.F.,.F.,(4,3,3,3,3,3,3,3,3,3,3,3,3,3,3,3,3,3,3,3,3,3,3,3,
3,3,3,3,3,3,3,3,3,3,3,3,3,3,3,3,3,3,3,3,3,3,3,3,3,3,3,3,3,3,3,3,4),(361.283155162826,
361.37946164755,361.431132243639,361.509520622646,361.587842887088,361.666113436546,
361.744346633089,361.822556810765,361.900774946147,361.979001011366,362.057247992923,
362.135528887137,362.213902314891,362.292325313213,362.370864872403,362.428674624964,
362.504745902605,362.580721679058,362.656618736055,362.732453774873,362.808243434975,
362.885490131389,362.961253629656,363.037024461027,363.112817628866,363.191167473222,
363.267092236737,363.346654621513,363.426217006289,363.503787227225,363.581265367739,
363.658667081645,363.736007967934,363.813303581822,363.890577021429,363.96784025673,
364.045107324161,364.122392259659,364.199750261999,364.277145793051,364.354647459812,
364.423759387614,364.507971539074,364.592057566781,364.675938488726,364.759690274757,
364.843227922091,364.922530578276,364.999910344642,365.077308505722,365.154738848331,
365.232256141821,365.309823087832,365.387496379317,365.421301768939,365.50093607667,
365.519850897371),.UNSPECIFIED.);
#3435=B_SPLINE_CURVE_WITH_KNOTS('',3,(#60758,#60759,#60760,#60761,#60762,
#60763,#60764,#60765,#60766,#60767,#60768,#60769,#60770,#60771,#60772,#60773,
#60774,#60775,#60776,#60777,#60778,#60779,#60780,#60781,#60782,#60783,#60784,
#60785,#60786,#60787,#60788,#60789,#60790,#60791,#60792,#60793,#60794,#60795,
#60796,#60797,#60798,#60799,#60800,#60801,#60802,#60803,#60804,#60805,#60806,
#60807,#60808,#60809,#60810,#60811,#60812,#60813,#60814,#60815,#60816,#60817,
#60818,#60819,#60820,#60821,#60822,#60823,#60824,#60825,#60826,#60827,#60828,
#60829,#60830,#60831,#60832,#60833,#60834,#60835,#60836,#60837,#60838,#60839),
 .UNSPECIFIED.,.F.,.F.,(4,3,3,3,3,3,3,3,3,3,3,3,3,3,3,3,3,3,3,3,3,3,3,3,
3,3,3,4),(359.236663920869,359.316144482474,359.395697507158,359.436047480989,
359.512778059315,359.589441657683,359.666052958912,359.742627725628,359.819181055023,
359.895738453029,359.934818671652,360.019487663267,360.104302115312,360.189315433545,
360.274414849052,360.359634237581,360.433589862314,360.515146841945,360.596628690916,
360.680561781431,360.761889021465,360.847125037221,360.932361052977,361.008735782809,
361.085133475983,361.161543131563,361.238009836076,361.283155162716),
 .UNSPECIFIED.);
#3436=B_SPLINE_CURVE_WITH_KNOTS('',3,(#60841,#60842,#60843,#60844,#60845,
#60846,#60847,#60848,#60849,#60850,#60851,#60852,#60853,#60854,#60855,#60856,
#60857,#60858,#60859,#60860,#60861,#60862,#60863,#60864,#60865,#60866,#60867,
#60868,#60869,#60870,#60871,#60872,#60873,#60874,#60875,#60876,#60877,#60878,
#60879,#60880,#60881,#60882,#60883,#60884,#60885,#60886,#60887,#60888,#60889,
#60890,#60891,#60892,#60893,#60894,#60895,#60896,#60897,#60898,#60899,#60900,
#60901,#60902,#60903,#60904,#60905,#60906,#60907,#60908,#60909,#60910,#60911,
#60912,#60913,#60914,#60915,#60916),.UNSPECIFIED.,.F.,.F.,(4,3,3,3,3,3,
3,3,3,3,3,3,3,3,3,3,3,3,3,3,3,3,3,3,3,4),(359.236648114071,359.319109717801,
359.401570655653,359.484030955025,359.566490643313,359.648949747912,359.731408296212,
359.813866315605,359.896323833477,359.983000791562,360.065467577103,360.147932690171,
360.230396240419,360.312858337478,360.395319090959,360.477778610456,360.560237005541,
360.642694385774,360.72516077146,360.807623972968,360.890084428818,360.972542577373,
361.055008181126,361.137468059514,361.219932170767,361.283155162826),
 .UNSPECIFIED.);
#3437=B_SPLINE_CURVE_WITH_KNOTS('',3,(#60917,#60918,#60919,#60920,#60921,
#60922,#60923,#60924,#60925,#60926,#60927,#60928,#60929,#60930,#60931,#60932,
#60933,#60934,#60935,#60936,#60937,#60938,#60939,#60940,#60941,#60942,#60943,
#60944,#60945,#60946,#60947,#60948,#60949,#60950,#60951,#60952,#60953,#60954,
#60955,#60956,#60957,#60958,#60959,#60960,#60961,#60962,#60963,#60964,#60965,
#60966,#60967,#60968,#60969,#60970,#60971,#60972,#60973,#60974,#60975,#60976,
#60977,#60978,#60979,#60980,#60981,#60982,#60983,#60984,#60985,#60986,#60987,
#60988,#60989,#60990,#60991,#60992,#60993,#60994,#60995,#60996,#60997,#60998,
#60999,#61000,#61001,#61002,#61003,#61004,#61005,#61006,#61007,#61008,#61009,
#61010,#61011,#61012,#61013,#61014,#61015,#61016,#61017,#61018,#61019,#61020,
#61021,#61022,#61023,#61024,#61025,#61026,#61027,#61028,#61029,#61030,#61031,
#61032,#61033,#61034,#61035,#61036,#61037,#61038,#61039,#61040,#61041,#61042,
#61043,#61044,#61045,#61046,#61047,#61048,#61049,#61050,#61051,#61052,#61053,
#61054,#61055,#61056,#61057,#61058,#61059,#61060,#61061,#61062,#61063,#61064,
#61065,#61066,#61067,#61068,#61069,#61070,#61071,#61072,#61073,#61074,#61075,
#61076,#61077,#61078,#61079,#61080,#61081,#61082),.UNSPECIFIED.,.F.,.F.,
(4,3,3,3,3,3,3,3,3,3,3,3,3,3,3,3,3,3,3,3,3,3,3,3,3,3,3,3,3,3,3,3,3,3,3,
3,3,3,3,3,3,3,3,3,3,3,3,3,3,3,3,3,3,3,3,4),(361.283242682583,361.361188581313,
361.439167184356,361.517477561481,361.595600258852,361.674004475854,361.752408692856,
361.832033880717,361.911586335594,361.991078357382,362.070522199397,362.149930077295,
362.229320511417,362.308702062166,362.388085799972,362.467482795302,362.546933412428,
362.626412431866,362.705964571519,362.749951074181,362.826681652507,362.903345250875,
362.979956552104,363.05653131882,363.133084648215,363.209642046221,363.248722264844,
363.333391256458,363.418205708503,363.503219026736,363.588318442243,363.673537830771,
363.747493455506,363.829050435137,363.910532284107,363.994465374623,364.075792614657,
364.161028630413,364.246264646169,364.325675844644,364.405105469188,364.484564280135,
364.564096103586,364.643669630011,364.723326753972,364.745035836831,364.823432638934,
364.901761096159,364.98002915517,365.058263041594,365.136475758451,365.214680293984,
365.292914335254,365.371161677635,365.449472774848,365.519433547733),
 .UNSPECIFIED.);
#3438=B_SPLINE_CURVE_WITH_KNOTS('',3,(#61088,#61089,#61090,#61091,#61092,
#61093,#61094,#61095,#61096,#61097,#61098,#61099,#61100,#61101,#61102,#61103,
#61104,#61105,#61106,#61107,#61108,#61109,#61110,#61111,#61112,#61113,#61114,
#61115,#61116,#61117,#61118,#61119,#61120,#61121,#61122,#61123,#61124,#61125,
#61126,#61127,#61128,#61129,#61130,#61131,#61132,#61133,#61134,#61135,#61136,
#61137,#61138,#61139,#61140,#61141,#61142,#61143,#61144,#61145,#61146,#61147,
#61148,#61149,#61150,#61151,#61152,#61153,#61154,#61155,#61156,#61157,#61158,
#61159,#61160,#61161,#61162,#61163,#61164,#61165,#61166,#61167,#61168,#61169,
#61170,#61171,#61172,#61173,#61174,#61175,#61176,#61177,#61178,#61179,#61180,
#61181,#61182,#61183,#61184,#61185,#61186,#61187,#61188,#61189,#61190,#61191,
#61192,#61193,#61194,#61195,#61196,#61197,#61198,#61199,#61200,#61201,#61202,
#61203,#61204,#61205,#61206,#61207,#61208,#61209,#61210,#61211,#61212,#61213,
#61214,#61215,#61216,#61217,#61218,#61219,#61220,#61221,#61222,#61223,#61224,
#61225,#61226,#61227,#61228,#61229,#61230,#61231,#61232,#61233,#61234,#61235,
#61236,#61237,#61238,#61239,#61240,#61241,#61242,#61243,#61244,#61245,#61246,
#61247,#61248,#61249,#61250,#61251,#61252,#61253,#61254,#61255,#61256),
 .UNSPECIFIED.,.F.,.F.,(4,3,3,3,3,3,3,3,3,3,3,3,3,3,3,3,3,3,3,3,3,3,3,3,
3,3,3,3,3,3,3,3,3,3,3,3,3,3,3,3,3,3,3,3,3,3,3,3,3,3,3,3,3,3,3,3,4),(367.566340470006,
367.645827499919,367.725237982588,367.804602928402,367.883927771408,367.915157722251,
367.994568920876,368.073998545579,368.153457356692,368.232989180319,368.312562706926,
368.392219831076,368.413928912913,368.492317290727,368.570639553964,368.648910102208,
368.72714329753,368.805353473978,368.883571608129,368.961797672114,369.040044652437,
369.118325545418,369.196698971949,369.275121969053,369.353661527042,369.411471294238,
369.487542573751,369.563518352073,369.639415410935,369.715250451613,369.791040113569,
369.868286808818,369.944050308916,370.019821142111,370.095614311762,370.173964152712,
370.249888918004,370.329451296783,370.409013675563,370.48658389756,370.56406203915,
370.641463754147,370.718804641539,370.796100256541,370.873373697278,370.950636933715,
371.02790400229,371.105188938938,371.182546942431,371.259942474638,371.337444142551,
371.406556056888,371.490786628699,371.574831076646,371.658755274643,371.742487247285,
371.80355994147),.UNSPECIFIED.);
#3439=B_SPLINE_CURVE_WITH_KNOTS('',3,(#61257,#61258,#61259,#61260,#61261,
#61262,#61263,#61264,#61265,#61266,#61267,#61268,#61269,#61270,#61271,#61272,
#61273,#61274,#61275,#61276,#61277,#61278,#61279,#61280,#61281,#61282,#61283,
#61284,#61285,#61286,#61287,#61288,#61289,#61290,#61291,#61292,#61293,#61294,
#61295,#61296,#61297,#61298,#61299,#61300,#61301,#61302,#61303,#61304,#61305,
#61306,#61307,#61308,#61309,#61310,#61311,#61312,#61313,#61314,#61315,#61316,
#61317,#61318,#61319,#61320,#61321,#61322,#61323,#61324,#61325,#61326,#61327,
#61328,#61329,#61330,#61331,#61332,#61333,#61334,#61335,#61336,#61337,#61338),
 .UNSPECIFIED.,.F.,.F.,(4,3,3,3,3,3,3,3,3,3,3,3,3,3,3,3,3,3,3,3,3,3,3,3,
3,3,3,4),(365.519850897371,365.599387868167,365.678867323637,365.758301507332,
365.840869337698,365.920256194552,365.999637242409,366.079023550997,366.158426192054,
366.237883672978,366.317372379599,366.396930317931,366.418844150263,366.495574729022,
366.572238327818,366.648849629473,366.725424396608,366.80197772642,366.878535124835,
366.917615340926,367.002284331427,367.087098782331,367.172112099402,367.257211513743,
367.342430901122,367.416386531588,367.507707819992,367.566340469871),
 .UNSPECIFIED.);
#3440=B_SPLINE_CURVE_WITH_KNOTS('',3,(#61340,#61341,#61342,#61343,#61344,
#61345,#61346,#61347,#61348,#61349,#61350,#61351,#61352,#61353,#61354,#61355,
#61356,#61357,#61358,#61359,#61360,#61361,#61362,#61363,#61364,#61365,#61366,
#61367,#61368,#61369,#61370,#61371,#61372,#61373,#61374,#61375,#61376,#61377,
#61378,#61379,#61380,#61381,#61382,#61383,#61384,#61385,#61386,#61387,#61388,
#61389,#61390,#61391,#61392,#61393,#61394,#61395,#61396,#61397,#61398,#61399,
#61400,#61401,#61402,#61403,#61404,#61405,#61406,#61407,#61408,#61409,#61410,
#61411,#61412,#61413,#61414,#61415,#61416,#61417,#61418,#61419,#61420,#61421),
 .UNSPECIFIED.,.F.,.F.,(4,3,3,3,3,3,3,3,3,3,3,3,3,3,3,3,3,3,3,3,3,3,3,3,
3,3,3,4),(365.519433547733,365.597850690332,365.676386814573,365.742578218156,
365.818649495797,365.894625272249,365.970522329247,366.046357368065,366.122147028167,
366.199393724581,366.275157222847,366.350928054219,366.426721222057,366.505071066413,
366.580995829929,366.660558214705,366.740120599481,366.817062464566,366.893911625604,
366.970684315063,367.047388774677,367.124055194297,367.200698142882,367.277332172827,
367.353997548231,367.430678376817,367.507426594913,367.566340470006),
 .UNSPECIFIED.);
#3441=B_SPLINE_CURVE_WITH_KNOTS('',3,(#61422,#61423,#61424,#61425,#61426,
#61427,#61428,#61429,#61430,#61431,#61432,#61433,#61434,#61435,#61436,#61437,
#61438,#61439,#61440,#61441,#61442,#61443,#61444,#61445,#61446,#61447,#61448,
#61449,#61450,#61451,#61452,#61453,#61454,#61455,#61456,#61457,#61458,#61459,
#61460,#61461,#61462,#61463,#61464,#61465,#61466,#61467,#61468,#61469,#61470,
#61471,#61472,#61473,#61474,#61475,#61476,#61477,#61478,#61479,#61480,#61481,
#61482,#61483,#61484,#61485,#61486,#61487,#61488,#61489,#61490,#61491,#61492,
#61493,#61494,#61495,#61496,#61497,#61498,#61499,#61500,#61501,#61502,#61503,
#61504,#61505,#61506,#61507,#61508,#61509,#61510,#61511,#61512,#61513,#61514,
#61515,#61516,#61517,#61518,#61519,#61520,#61521,#61522,#61523,#61524,#61525,
#61526,#61527,#61528,#61529,#61530,#61531,#61532,#61533,#61534,#61535,#61536,
#61537,#61538,#61539,#61540,#61541,#61542,#61543,#61544,#61545,#61546,#61547,
#61548,#61549,#61550,#61551,#61552,#61553,#61554,#61555,#61556,#61557,#61558,
#61559,#61560,#61561,#61562,#61563,#61564,#61565,#61566,#61567,#61568,#61569,
#61570,#61571,#61572,#61573,#61574,#61575,#61576,#61577,#61578,#61579,#61580,
#61581,#61582,#61583,#61584,#61585,#61586,#61587),.UNSPECIFIED.,.F.,.F.,
(4,3,3,3,3,3,3,3,3,3,3,3,3,3,3,3,3,3,3,3,3,3,3,3,3,3,3,3,3,3,3,3,3,3,3,
3,3,3,3,3,3,3,3,3,3,3,3,3,3,3,3,3,3,3,3,4),(367.566340470089,367.671959825277,
367.737662980806,367.821875132266,367.905961159974,367.989842081919,368.073593867951,
368.157131515285,368.236434171468,368.313813937834,368.391212098914,368.468642441523,
368.546159735013,368.623726681024,368.70139997251,368.735205362131,368.814830549885,
368.894383004655,368.973875026336,369.053318868243,369.132726746034,369.21211718005,
369.291498730693,369.370882468393,369.45027946362,369.529730080644,369.609209099982,
369.688761239537,369.732747743455,369.809478322214,369.88614192101,369.962753222665,
370.0393279898,370.115881319612,370.192438718027,370.231518934118,370.316187924619,
370.401002375523,370.486015692594,370.571115106935,370.656334494314,370.73029012478,
370.811847105145,370.893328954842,370.977262044992,371.058589285723,371.143825300583,
371.229061315443,371.308472514068,371.387902138771,371.467360949883,371.546892773511,
371.626466300118,371.706123424268,371.727832506105,371.803205170848),
 .UNSPECIFIED.);
#3442=B_SPLINE_CURVE_WITH_KNOTS('',3,(#61593,#61594,#61595,#61596,#61597,
#61598,#61599,#61600,#61601,#61602,#61603,#61604,#61605,#61606,#61607,#61608,
#61609,#61610,#61611,#61612,#61613,#61614,#61615,#61616,#61617,#61618,#61619,
#61620,#61621,#61622,#61623,#61624,#61625,#61626,#61627,#61628,#61629,#61630,
#61631,#61632,#61633,#61634,#61635,#61636,#61637,#61638,#61639,#61640,#61641,
#61642,#61643,#61644,#61645,#61646,#61647,#61648,#61649,#61650,#61651,#61652,
#61653,#61654,#61655,#61656,#61657,#61658,#61659,#61660,#61661,#61662,#61663,
#61664,#61665,#61666,#61667,#61668,#61669,#61670,#61671,#61672,#61673,#61674,
#61675,#61676,#61677,#61678,#61679,#61680,#61681,#61682,#61683,#61684,#61685,
#61686,#61687,#61688,#61689,#61690,#61691,#61692,#61693,#61694,#61695,#61696,
#61697,#61698,#61699,#61700,#61701,#61702,#61703,#61704,#61705,#61706,#61707,
#61708,#61709,#61710,#61711,#61712,#61713,#61714,#61715,#61716,#61717,#61718,
#61719,#61720,#61721,#61722,#61723,#61724,#61725,#61726,#61727,#61728,#61729,
#61730,#61731,#61732,#61733,#61734,#61735,#61736,#61737,#61738,#61739,#61740,
#61741,#61742,#61743,#61744,#61745,#61746,#61747,#61748,#61749),
 .UNSPECIFIED.,.F.,.F.,(4,3,3,3,3,3,3,3,3,3,3,3,3,3,3,3,3,3,3,3,3,3,3,3,
3,3,3,3,3,3,3,3,3,3,3,3,3,3,3,3,3,3,3,3,3,3,3,3,3,3,3,3,4),(373.849525777185,
373.931987983285,374.014449841088,374.096911357443,374.179372539201,374.261833393211,
374.344293926323,374.426754145386,374.509214057249,374.591673668761,374.67413298677,
374.756592018124,374.839050769671,374.921509248258,375.003967460734,375.086425413945,
375.168883114738,375.25134056996,375.333797786457,375.419810481743,375.503135280301,
375.585601885893,375.668067647276,375.750532591866,375.832996747075,375.915460140311,
375.997922798983,376.080384750494,376.162846022246,376.24530664164,376.327766636071,
376.410226032935,376.492684859625,376.575143143532,376.657600912045,376.740058192551,
376.824192307743,376.906658306102,376.989122682709,377.071585547204,377.15404700921,
377.23650717833,377.318966164146,377.401424076226,377.487021571149,377.569486308195,
377.651948080581,377.734407326746,377.816864484985,377.899327004068,377.981784675479,
378.064243466672,378.08620403561),.UNSPECIFIED.);
#3443=B_SPLINE_CURVE_WITH_KNOTS('',3,(#61750,#61751,#61752,#61753,#61754,
#61755,#61756,#61757,#61758,#61759,#61760,#61761,#61762,#61763,#61764,#61765,
#61766,#61767,#61768,#61769,#61770,#61771,#61772,#61773,#61774,#61775,#61776,
#61777,#61778,#61779,#61780,#61781,#61782,#61783,#61784,#61785,#61786,#61787,
#61788,#61789,#61790,#61791,#61792,#61793,#61794,#61795,#61796,#61797,#61798,
#61799,#61800,#61801,#61802,#61803,#61804,#61805,#61806,#61807,#61808,#61809,
#61810,#61811,#61812,#61813,#61814,#61815,#61816,#61817,#61818,#61819,#61820,
#61821,#61822,#61823,#61824,#61825,#61826,#61827,#61828,#61829,#61830,#61831,
#61832,#61833,#61834),.UNSPECIFIED.,.F.,.F.,(4,3,3,3,3,3,3,3,3,3,3,3,3,
3,3,3,3,3,3,3,3,3,3,3,3,3,3,3,4),(371.80355994147,371.887023856295,371.90532724755,
371.982707058008,372.060105263626,372.137535651175,372.215052990023,372.292619981656,
372.370293318913,372.404098438213,372.48372358287,372.563275994317,372.642767972546,
372.722211770968,372.801619605335,372.881009996262,372.960391504087,373.039775199325,
373.119172152529,373.19862272848,373.278101707279,373.357653807471,373.401640819538,
373.479117409525,373.556521439858,373.633857436576,373.711153486426,373.788427537233,
373.849284737275),.UNSPECIFIED.);
#3444=B_SPLINE_CURVE_WITH_KNOTS('',3,(#61836,#61837,#61838,#61839,#61840,
#61841,#61842,#61843,#61844,#61845,#61846,#61847,#61848,#61849,#61850,#61851,
#61852,#61853,#61854,#61855,#61856,#61857,#61858,#61859,#61860,#61861,#61862,
#61863,#61864,#61865,#61866,#61867,#61868,#61869,#61870,#61871,#61872,#61873,
#61874,#61875,#61876,#61877,#61878,#61879,#61880,#61881,#61882,#61883,#61884,
#61885,#61886,#61887,#61888,#61889,#61890,#61891,#61892,#61893,#61894,#61895,
#61896,#61897,#61898,#61899,#61900,#61901,#61902,#61903,#61904,#61905,#61906,
#61907,#61908,#61909,#61910,#61911,#61912,#61913,#61914),.UNSPECIFIED.,
 .F.,.F.,(4,3,3,3,3,3,3,3,3,3,3,3,3,3,3,3,3,3,3,3,3,3,3,3,3,3,4),(371.803205170848,
371.881529712004,371.959801984707,372.038036352297,372.116247149726,372.194465238155,
372.272690756781,372.35093669188,372.429216039255,372.507587794488,372.586008667588,
372.664546969386,372.72537488743,372.801446166943,372.877421945265,372.953319004127,
373.029154044804,373.10494370676,373.18219040201,373.257953902108,373.333724735302,
373.409517904954,373.487867745904,373.563792511196,373.643354889975,373.722917268755,
373.849525777185),.UNSPECIFIED.);
#3445=B_SPLINE_CURVE_WITH_KNOTS('',3,(#61915,#61916,#61917,#61918,#61919,
#61920,#61921,#61922,#61923,#61924,#61925,#61926,#61927,#61928,#61929,#61930,
#61931,#61932,#61933,#61934,#61935,#61936,#61937,#61938,#61939,#61940,#61941,
#61942,#61943,#61944,#61945,#61946,#61947,#61948,#61949,#61950,#61951,#61952,
#61953,#61954,#61955,#61956,#61957,#61958,#61959,#61960,#61961,#61962,#61963,
#61964,#61965,#61966,#61967,#61968,#61969,#61970,#61971,#61972,#61973,#61974,
#61975,#61976,#61977,#61978,#61979,#61980,#61981,#61982,#61983,#61984,#61985,
#61986,#61987,#61988,#61989,#61990,#61991,#61992,#61993,#61994,#61995,#61996,
#61997,#61998,#61999,#62000,#62001,#62002,#62003,#62004,#62005,#62006,#62007,
#62008,#62009,#62010,#62011,#62012,#62013,#62014,#62015,#62016,#62017,#62018,
#62019,#62020,#62021,#62022,#62023,#62024,#62025,#62026,#62027,#62028,#62029,
#62030,#62031,#62032,#62033,#62034,#62035,#62036,#62037,#62038,#62039,#62040,
#62041,#62042,#62043,#62044,#62045,#62046,#62047,#62048,#62049,#62050,#62051,
#62052,#62053,#62054,#62055,#62056,#62057,#62058,#62059,#62060,#62061,#62062,
#62063,#62064,#62065,#62066,#62067,#62068,#62069,#62070,#62071,#62072,#62073,
#62074,#62075,#62076,#62077,#62078,#62079,#62080,#62081,#62082,#62083),
 .UNSPECIFIED.,.F.,.F.,(4,3,3,3,3,3,3,3,3,3,3,3,3,3,3,3,3,3,3,3,3,3,3,3,
3,3,3,3,3,3,3,3,3,3,3,3,3,3,3,3,3,3,3,3,3,3,3,3,3,3,3,3,3,3,3,3,4),(373.849525777274,
373.925592910461,374.001577904088,374.077497497404,374.153368363852,374.229213553232,
374.30504741323,374.380884962493,374.456741221151,374.53266819445,374.608635285085,
374.684698717904,374.72045965008,374.80467177142,374.888757769278,374.972638662245,
375.056390419951,375.139928040355,375.219230840742,375.2966106512,375.374008856819,
375.451439244367,375.528956583214,375.606523574847,375.684196912104,375.718002031405,
375.797627176062,375.877179587509,375.956671565738,376.036115364159,376.115523198525,
376.194913589453,376.274295097278,376.353678792515,376.433075745719,376.512526321669,
376.592005300468,376.67155740066,376.71554441273,376.792275076439,376.868938759282,
376.945550144022,377.022124992601,377.098678402943,377.175235880253,377.214315603392,
377.298984567271,377.383798992803,377.468812286926,377.553911679802,377.63913104854,
377.713086794055,377.794655681762,377.876123286358,377.957527832752,378.038855906015,
378.08664702176),.UNSPECIFIED.);
#3446=B_SPLINE_CURVE_WITH_KNOTS('',3,(#62089,#62090,#62091,#62092,#62093,
#62094,#62095,#62096,#62097,#62098,#62099,#62100,#62101,#62102,#62103,#62104,
#62105,#62106,#62107,#62108,#62109,#62110,#62111,#62112,#62113,#62114,#62115,
#62116,#62117,#62118,#62119,#62120,#62121,#62122,#62123,#62124,#62125,#62126,
#62127,#62128,#62129,#62130,#62131,#62132,#62133,#62134,#62135,#62136,#62137,
#62138,#62139,#62140,#62141,#62142,#62143,#62144,#62145,#62146,#62147,#62148,
#62149,#62150,#62151,#62152,#62153,#62154,#62155,#62156,#62157,#62158,#62159,
#62160,#62161,#62162,#62163,#62164,#62165,#62166,#62167,#62168,#62169,#62170,
#62171,#62172,#62173,#62174,#62175,#62176,#62177,#62178,#62179,#62180,#62181,
#62182,#62183,#62184,#62185,#62186,#62187,#62188,#62189,#62190,#62191,#62192,
#62193,#62194,#62195,#62196,#62197,#62198,#62199,#62200,#62201,#62202,#62203,
#62204,#62205,#62206,#62207,#62208,#62209,#62210,#62211,#62212,#62213,#62214,
#62215,#62216,#62217,#62218,#62219,#62220,#62221,#62222,#62223,#62224,#62225,
#62226,#62227,#62228,#62229,#62230,#62231,#62232,#62233,#62234,#62235,#62236,
#62237,#62238,#62239,#62240,#62241,#62242,#62243,#62244,#62245),
 .UNSPECIFIED.,.F.,.F.,(4,3,3,3,3,3,3,3,3,3,3,3,3,3,3,3,3,3,3,3,3,3,3,3,
3,3,3,3,3,3,3,3,3,3,3,3,3,3,3,3,3,3,3,3,3,3,3,3,3,3,3,3,4),(380.132711084458,
380.215173290558,380.297635148361,380.380096664716,380.462557846474,380.545018700484,
380.627479233596,380.709939452659,380.792399364522,380.874858976034,380.957318294042,
381.039777325396,381.122236076943,381.204694555531,381.287152768006,381.369610721217,
381.45206842201,381.534525877232,381.61698309373,381.702995789013,381.786320587568,
381.86878719316,381.951252954543,382.033717899133,382.116182054341,382.198645447578,
382.28110810625,382.363570057761,382.446031329513,382.528491948906,382.610951943337,
382.693411340202,382.775870166892,382.858328450799,382.940786219312,383.023243499818,
383.107377615004,383.189843613364,383.27230798997,383.354770854466,383.437232316472,
383.519692485591,383.602151471407,383.684609383488,383.7702068784,383.852671615446,
383.935133387833,384.017592633998,384.100049792237,384.182512311319,384.26496998273,
384.347428773923,384.36938934279),.UNSPECIFIED.);
#3447=B_SPLINE_CURVE_WITH_KNOTS('',3,(#62246,#62247,#62248,#62249,#62250,
#62251,#62252,#62253,#62254,#62255,#62256,#62257,#62258,#62259,#62260,#62261,
#62262,#62263,#62264,#62265,#62266,#62267,#62268,#62269,#62270,#62271,#62272,
#62273,#62274,#62275,#62276,#62277,#62278,#62279,#62280,#62281,#62282,#62283,
#62284,#62285,#62286,#62287,#62288,#62289,#62290,#62291,#62292,#62293,#62294,
#62295,#62296,#62297,#62298,#62299,#62300,#62301,#62302,#62303,#62304,#62305,
#62306,#62307,#62308,#62309,#62310,#62311,#62312,#62313,#62314,#62315,#62316,
#62317,#62318,#62319,#62320,#62321),.UNSPECIFIED.,.F.,.F.,(4,3,3,3,3,3,
3,3,3,3,3,3,3,3,3,3,3,3,3,3,3,3,3,3,3,4),(378.08620403561,378.16866563934,
378.251126577192,378.333586876564,378.416046564852,378.49850566945,378.580964217751,
378.663422237143,378.745879755016,378.8325567131,378.915023498642,378.99748861171,
379.079952161957,379.162414259017,379.244875012498,379.327334531994,379.409792927079,
379.492250307313,379.574716692999,379.657179894507,379.739640350357,379.822098498912,
379.904564102665,379.987023981053,380.069488092306,380.132711084365),
 .UNSPECIFIED.);
#3448=B_SPLINE_CURVE_WITH_KNOTS('',3,(#62323,#62324,#62325,#62326,#62327,
#62328,#62329,#62330,#62331,#62332,#62333,#62334,#62335,#62336,#62337,#62338,
#62339,#62340,#62341,#62342,#62343,#62344,#62345,#62346,#62347,#62348,#62349,
#62350,#62351,#62352,#62353,#62354,#62355,#62356,#62357,#62358,#62359,#62360,
#62361,#62362,#62363,#62364,#62365,#62366,#62367,#62368,#62369,#62370,#62371,
#62372,#62373,#62374,#62375,#62376,#62377,#62378,#62379,#62380,#62381,#62382,
#62383,#62384,#62385,#62386,#62387,#62388,#62389,#62390,#62391,#62392,#62393,
#62394,#62395,#62396,#62397,#62398,#62399,#62400,#62401,#62402,#62403,#62404,
#62405,#62406,#62407),.UNSPECIFIED.,.F.,.F.,(4,3,3,3,3,3,3,3,3,3,3,3,3,
3,3,3,3,3,3,3,3,3,3,3,3,3,3,3,4),(378.08664702176,378.167878927395,378.211857984717,
378.291270024972,378.370700502916,378.450160177032,378.529692873023,378.609267277008,
378.688925280535,378.710629175379,378.789016903715,378.867338511619,378.945608399641,
379.023840930815,379.102050440153,379.180267905599,379.258493300237,379.336739611424,
379.415019836334,379.493392600461,379.571814937547,379.650353845682,379.708171556704,
379.790707299786,379.876208245931,379.958270423662,380.040165762441,380.121839947867,
380.132711084365),.UNSPECIFIED.);
#3449=B_SPLINE_CURVE_WITH_KNOTS('',3,(#62408,#62409,#62410,#62411,#62412,
#62413,#62414,#62415,#62416,#62417,#62418,#62419,#62420,#62421,#62422,#62423,
#62424,#62425,#62426,#62427,#62428,#62429,#62430,#62431,#62432,#62433,#62434,
#62435,#62436,#62437,#62438,#62439,#62440,#62441,#62442,#62443,#62444,#62445,
#62446,#62447,#62448,#62449,#62450,#62451,#62452,#62453,#62454,#62455,#62456,
#62457,#62458,#62459,#62460,#62461,#62462,#62463,#62464,#62465,#62466,#62467,
#62468,#62469,#62470,#62471,#62472,#62473,#62474,#62475,#62476,#62477,#62478,
#62479,#62480,#62481,#62482,#62483,#62484,#62485,#62486,#62487,#62488,#62489,
#62490,#62491,#62492,#62493,#62494,#62495,#62496,#62497,#62498,#62499,#62500,
#62501,#62502,#62503,#62504,#62505,#62506,#62507,#62508,#62509,#62510,#62511,
#62512,#62513,#62514,#62515,#62516,#62517,#62518,#62519,#62520,#62521,#62522,
#62523,#62524,#62525,#62526,#62527,#62528,#62529,#62530,#62531,#62532,#62533,
#62534,#62535,#62536,#62537,#62538,#62539,#62540,#62541,#62542,#62543,#62544,
#62545,#62546,#62547,#62548,#62549,#62550,#62551,#62552,#62553,#62554,#62555,
#62556,#62557,#62558,#62559,#62560,#62561,#62562,#62563,#62564),
 .UNSPECIFIED.,.F.,.F.,(4,3,3,3,3,3,3,3,3,3,3,3,3,3,3,3,3,3,3,3,3,3,3,3,
3,3,3,3,3,3,3,3,3,3,3,3,3,3,3,3,3,3,3,3,3,3,3,3,3,3,3,3,4),(380.132711084365,
380.215173290465,380.297635148268,380.380096664623,380.46255784638,380.545018700391,
380.627479233503,380.709939452566,380.792399364429,380.874858975941,380.95731829395,
381.039777325303,381.12223607685,381.204694555438,381.287152767914,381.369610721124,
381.452068421917,381.534525877139,381.616983093637,381.702995788923,381.786320587481,
381.868787193073,381.951252954456,382.033717899046,382.116182054254,382.198645447491,
382.281108106162,382.363570057674,382.446031329426,382.528491948819,382.61095194325,
382.693411340114,382.775870166804,382.858328450711,382.940786219224,383.023243499731,
383.107377614922,383.189843613282,383.272307989888,383.354770854383,383.43723231639,
383.519692485509,383.602151471325,383.684609383405,383.770206878328,383.852671615374,
383.935133387761,384.017592633926,384.100049792164,384.182512311247,384.264969982658,
384.347428773851,384.369389342789),.UNSPECIFIED.);
#3450=B_SPLINE_CURVE_WITH_KNOTS('',3,(#62568,#62569,#62570,#62571,#62572,
#62573,#62574,#62575),.UNSPECIFIED.,.F.,.F.,(4,2,2,4),(-4.09262915008374,
-3.25801350823578,-2.42309659634092,-2.07498647268394),.UNSPECIFIED.);
#3451=B_SPLINE_CURVE_WITH_KNOTS('',3,(#62579,#62580,#62581,#62582,#62583,
#62584,#62585,#62586,#62587,#62588,#62589,#62590,#62591,#62592,#62593,#62594,
#62595,#62596,#62597,#62598,#62599,#62600,#62601,#62602,#62603,#62604,#62605,
#62606,#62607,#62608,#62609,#62610,#62611,#62612,#62613,#62614,#62615,#62616,
#62617,#62618,#62619,#62620,#62621,#62622,#62623,#62624,#62625,#62626,#62627,
#62628,#62629,#62630,#62631,#62632,#62633,#62634,#62635,#62636,#62637,#62638,
#62639,#62640,#62641,#62642,#62643,#62644,#62645,#62646,#62647,#62648,#62649,
#62650,#62651,#62652,#62653,#62654,#62655,#62656,#62657,#62658,#62659,#62660,
#62661,#62662,#62663,#62664,#62665,#62666,#62667,#62668,#62669,#62670,#62671,
#62672,#62673,#62674,#62675,#62676,#62677,#62678,#62679,#62680,#62681,#62682,
#62683,#62684,#62685,#62686,#62687,#62688,#62689,#62690,#62691,#62692,#62693,
#62694,#62695,#62696,#62697,#62698,#62699,#62700,#62701,#62702,#62703,#62704,
#62705,#62706,#62707,#62708,#62709,#62710,#62711,#62712,#62713,#62714,#62715,
#62716,#62717,#62718,#62719,#62720,#62721,#62722,#62723,#62724,#62725,#62726,
#62727,#62728,#62729,#62730,#62731,#62732,#62733,#62734,#62735,#62736,#62737,
#62738,#62739,#62740,#62741,#62742,#62743,#62744,#62745,#62746,#62747,#62748,
#62749,#62750,#62751,#62752,#62753,#62754,#62755,#62756,#62757,#62758,#62759,
#62760,#62761,#62762,#62763,#62764,#62765,#62766,#62767,#62768,#62769,#62770,
#62771,#62772,#62773,#62774,#62775,#62776,#62777,#62778,#62779,#62780,#62781,
#62782,#62783,#62784,#62785,#62786,#62787,#62788,#62789,#62790,#62791,#62792,
#62793,#62794,#62795,#62796,#62797,#62798,#62799,#62800,#62801,#62802,#62803,
#62804,#62805,#62806,#62807,#62808,#62809,#62810,#62811,#62812,#62813,#62814,
#62815,#62816,#62817,#62818,#62819,#62820,#62821,#62822,#62823,#62824,#62825,
#62826,#62827,#62828,#62829,#62830,#62831,#62832,#62833,#62834,#62835,#62836,
#62837,#62838,#62839,#62840,#62841,#62842,#62843,#62844,#62845,#62846,#62847,
#62848,#62849,#62850,#62851,#62852,#62853,#62854,#62855,#62856,#62857,#62858,
#62859,#62860,#62861,#62862,#62863,#62864,#62865,#62866,#62867,#62868,#62869,
#62870,#62871,#62872,#62873,#62874,#62875,#62876,#62877,#62878,#62879,#62880,
#62881,#62882,#62883,#62884,#62885,#62886,#62887,#62888,#62889,#62890,#62891,
#62892,#62893,#62894,#62895,#62896,#62897,#62898,#62899,#62900,#62901,#62902,
#62903,#62904),.UNSPECIFIED.,.F.,.F.,(4,2,2,2,2,2,2,2,2,2,2,2,2,2,2,2,2,
2,2,2,2,2,2,2,2,2,2,2,2,2,2,2,2,2,2,2,2,2,2,2,2,2,2,2,2,2,2,2,2,2,2,2,2,
2,2,2,2,2,2,2,2,2,2,2,2,2,2,2,2,2,2,2,2,2,2,2,2,2,2,2,2,2,2,2,2,2,2,2,2,
2,2,2,2,2,2,2,2,2,2,2,2,2,2,2,2,2,2,2,2,2,2,2,2,2,2,2,2,2,2,2,2,2,2,2,2,
2,2,2,2,2,2,2,2,2,2,2,2,2,2,2,2,2,2,2,2,2,2,2,2,2,2,2,2,2,2,2,2,2,2,2,2,
2,4),(6.78680112922089E-5,0.00847455153472558,0.0205550808575541,0.0663470498539596,
0.113846171319888,0.148670368122606,0.162566725200985,0.176093744247133,
0.189517913141263,0.213396993878021,0.29182571289124,0.347515192132862,
0.375621647217002,0.376496789457627,0.376951840483764,0.377870037035494,
0.384922167581578,0.390912715358734,0.397240236351121,0.407290320413488,
0.462396926330204,0.510017537064033,0.530535865261965,0.543040465556326,
0.546604952112527,0.555812596781168,0.564937586640173,0.576899983176677,
0.595573980052425,0.692061246855429,0.764269280602125,0.772954681898515,
0.777327023684247,0.781408333482716,0.785360366438397,0.790575569363848,
0.804894630243167,0.907175577104357,0.996874648878195,1.05009922531605,
1.08495496264516,1.09695613786015,1.10426927752641,1.112186582686,1.12237897970457,
1.13942126892903,1.22471258407554,1.39856915012792,1.50642685078538,1.5426628802634,
1.54775465536353,1.55036026515212,1.55223446846513,1.55421913556645,1.55701010269284,
1.56442222085663,1.68156464426591,1.81040381737534,1.89782059794948,1.93530202771538,
1.94103643567307,1.94399614716539,1.94615941818338,1.94848220726541,1.95180292613558,
1.96094044356202,2.09645512034237,2.13809561274441,2.26936941226598,2.3256715145711,
2.34666926858975,2.3581252927114,2.36075262736178,2.36224606980681,2.36340087055794,
2.36470610779319,2.36714048051926,2.37546562613443,2.50755217540942,2.64920788246672,
2.72224383874213,2.75461875348397,2.7596640780648,2.76227587996437,2.76418792931182,
2.76624379134744,2.76979623942517,2.77969659684181,2.93425550300827,3.14938562823162,
3.16183313195867,3.16430258693048,3.16588452758889,3.16713921036186,3.1685452320664,
3.17088822391385,3.17949234546324,3.23792128164173,3.3847077591732,3.56961379748167,
3.5815420185984,3.58551685517584,3.58802917498927,3.59032009613806,3.59323422924214,
3.59917516221538,3.64707718078749,3.7273875888966,3.78903279180768,3.96680607018146,
3.98042837848918,3.9845680285147,3.98704628921796,3.9890336004651,3.99171066303711,
3.99675809051981,4.02607262921474,4.09545900454798,4.21940280188449,4.40371403835115,
4.42558154069455,4.43390964137369,4.43990048824899,4.44627492355155,4.45477968368953,
4.47377905635575,4.5511144003357,4.63185019722768,4.69211415017163,4.73720400888895,
4.74367540848441,4.74776175135428,4.75103482008021,4.75474172513869,4.76102742964408,
4.7859044486062,4.83384701287002,4.95040076617469,4.98732100802768,4.99186239933497,
5.04240155525838,5.05696691264538,5.06572878518261,5.07283354907773,5.08257688475351,
5.10192112115817,5.20462221176254,5.34868422153004,5.44352082377912,5.44549523237544,
5.44850610235358,5.44952028440821,5.45187024349439,5.456611140767,5.49702337793335,
5.50194083458181,5.50445131553751,5.50630142880113,5.50830504943557,5.51102849058975,
5.51725072199404,5.62175200668662,5.8680590994294),.UNSPECIFIED.);
#3452=B_SPLINE_CURVE_WITH_KNOTS('',3,(#62906,#62907,#62908,#62909,#62910,
#62911,#62912,#62913,#62914,#62915,#62916,#62917,#62918,#62919,#62920,#62921,
#62922,#62923,#62924,#62925,#62926,#62927,#62928,#62929,#62930,#62931,#62932,
#62933,#62934,#62935,#62936,#62937,#62938,#62939,#62940,#62941,#62942,#62943,
#62944,#62945,#62946,#62947,#62948,#62949,#62950,#62951,#62952,#62953,#62954,
#62955,#62956,#62957,#62958,#62959,#62960,#62961,#62962,#62963,#62964,#62965,
#62966,#62967,#62968,#62969,#62970,#62971,#62972,#62973,#62974,#62975,#62976,
#62977,#62978,#62979,#62980,#62981,#62982,#62983,#62984,#62985,#62986,#62987,
#62988,#62989,#62990,#62991,#62992,#62993,#62994,#62995,#62996,#62997,#62998,
#62999,#63000,#63001,#63002,#63003,#63004,#63005,#63006,#63007,#63008,#63009,
#63010,#63011,#63012,#63013,#63014,#63015,#63016,#63017,#63018,#63019,#63020,
#63021,#63022,#63023,#63024,#63025,#63026,#63027,#63028,#63029,#63030,#63031,
#63032,#63033,#63034,#63035,#63036,#63037,#63038,#63039,#63040,#63041,#63042,
#63043,#63044,#63045,#63046,#63047,#63048,#63049,#63050,#63051,#63052,#63053,
#63054,#63055,#63056,#63057,#63058,#63059,#63060,#63061,#63062,#63063,#63064,
#63065,#63066,#63067,#63068,#63069,#63070,#63071,#63072,#63073,#63074,#63075,
#63076,#63077,#63078,#63079,#63080,#63081,#63082,#63083,#63084,#63085,#63086,
#63087,#63088,#63089,#63090,#63091,#63092,#63093,#63094,#63095,#63096,#63097,
#63098,#63099,#63100,#63101,#63102,#63103,#63104,#63105,#63106,#63107,#63108,
#63109,#63110,#63111,#63112,#63113,#63114,#63115,#63116,#63117,#63118,#63119,
#63120,#63121,#63122,#63123,#63124,#63125,#63126,#63127,#63128,#63129,#63130,
#63131,#63132,#63133,#63134,#63135,#63136,#63137,#63138,#63139,#63140,#63141,
#63142,#63143,#63144,#63145,#63146,#63147,#63148,#63149,#63150,#63151,#63152,
#63153,#63154,#63155,#63156,#63157,#63158,#63159,#63160,#63161,#63162,#63163,
#63164,#63165,#63166,#63167,#63168,#63169,#63170,#63171,#63172,#63173,#63174,
#63175,#63176,#63177,#63178,#63179,#63180,#63181,#63182,#63183,#63184,#63185,
#63186,#63187,#63188,#63189,#63190,#63191,#63192,#63193,#63194,#63195,#63196,
#63197,#63198,#63199,#63200,#63201,#63202,#63203,#63204,#63205,#63206,#63207,
#63208,#63209,#63210,#63211,#63212,#63213,#63214,#63215,#63216,#63217,#63218,
#63219,#63220,#63221,#63222,#63223,#63224,#63225,#63226,#63227,#63228,#63229,
#63230,#63231,#63232,#63233,#63234,#63235,#63236,#63237,#63238,#63239,#63240,
#63241,#63242,#63243,#63244,#63245,#63246,#63247,#63248,#63249,#63250,#63251,
#63252,#63253,#63254,#63255,#63256,#63257,#63258,#63259,#63260,#63261,#63262,
#63263,#63264,#63265,#63266,#63267,#63268,#63269,#63270,#63271,#63272,#63273,
#63274,#63275,#63276,#63277,#63278,#63279,#63280,#63281,#63282,#63283,#63284,
#63285,#63286,#63287,#63288,#63289,#63290,#63291,#63292,#63293,#63294,#63295,
#63296,#63297,#63298,#63299,#63300,#63301,#63302,#63303,#63304,#63305,#63306,
#63307,#63308,#63309,#63310,#63311,#63312,#63313,#63314,#63315,#63316,#63317,
#63318,#63319,#63320,#63321,#63322,#63323,#63324,#63325,#63326,#63327,#63328,
#63329,#63330,#63331,#63332,#63333,#63334,#63335,#63336,#63337,#63338,#63339,
#63340,#63341,#63342,#63343,#63344,#63345,#63346,#63347,#63348,#63349,#63350,
#63351,#63352,#63353,#63354,#63355,#63356,#63357,#63358,#63359,#63360,#63361,
#63362,#63363,#63364,#63365,#63366,#63367,#63368,#63369,#63370,#63371,#63372,
#63373,#63374,#63375,#63376,#63377,#63378,#63379,#63380,#63381,#63382,#63383,
#63384,#63385,#63386,#63387,#63388,#63389,#63390,#63391,#63392,#63393,#63394,
#63395,#63396,#63397,#63398,#63399,#63400,#63401,#63402,#63403,#63404,#63405,
#63406,#63407,#63408,#63409,#63410,#63411,#63412,#63413,#63414,#63415,#63416,
#63417,#63418,#63419,#63420,#63421,#63422,#63423,#63424,#63425,#63426,#63427,
#63428,#63429,#63430,#63431,#63432,#63433,#63434,#63435,#63436,#63437,#63438,
#63439,#63440,#63441,#63442,#63443,#63444,#63445,#63446,#63447,#63448,#63449,
#63450,#63451,#63452,#63453,#63454,#63455,#63456,#63457),.UNSPECIFIED.,
 .F.,.F.,(4,2,2,2,2,2,2,2,2,2,2,2,2,2,2,2,2,2,2,2,2,2,2,2,2,2,2,2,2,2,2,
2,2,2,2,2,2,2,2,2,2,2,2,2,2,2,2,2,2,2,2,2,2,2,2,2,2,2,2,2,2,2,2,2,2,2,2,
2,2,2,2,2,2,2,2,2,2,2,2,2,2,2,2,2,2,2,2,2,2,2,2,2,2,2,2,2,2,2,2,2,2,2,2,
2,2,2,2,2,2,2,2,2,2,2,2,2,2,2,2,2,2,2,2,2,2,2,2,2,2,2,2,2,2,2,2,2,2,2,2,
2,2,2,2,2,2,2,2,2,2,2,2,2,2,2,2,2,2,2,2,2,2,2,2,2,2,2,2,2,2,2,2,2,2,2,2,
2,2,2,2,2,2,2,2,2,2,2,2,2,2,2,2,2,2,2,2,2,2,2,2,2,2,2,2,2,2,2,2,2,2,2,2,
2,2,2,2,2,2,2,2,2,2,2,2,2,2,2,2,2,2,2,2,2,2,2,2,2,2,2,2,2,2,2,2,2,2,2,2,
2,2,2,2,2,2,2,2,2,2,2,2,2,2,2,2,2,2,2,2,2,2,2,2,2,2,2,2,4),(0.00217771040208461,
0.0344816819576811,0.0484248271821416,0.0521712334234981,0.054811747531862,
0.0570944089203552,0.0594373547913961,0.062544548743391,0.0686216800216088,
0.103258803958561,0.116907225233592,0.386084646671751,0.407909550866978,
0.457150234070088,0.465711897345782,0.468514138207261,0.47031576693353,
0.472007196551051,0.474223837438873,0.477960414344228,0.500830479885667,
0.681373441914476,0.815521569378699,0.828147376720993,0.833788339008274,
0.837994401687425,0.841923286043086,0.848159861271726,0.854648156497679,
0.897991386954332,1.12014373129146,1.18237094795391,1.21016646677564,1.21464780424494,
1.21698723143654,1.21889087598737,1.22107727941822,1.22475672803362,1.23777966553735,
1.45437614170428,1.56092714026596,1.5885998748474,1.59935851109546,1.60469175229055,
1.60791278089858,1.61083687916309,1.61306691977316,1.615211148419,1.61818774248469,
1.62586810510941,1.72968406360318,1.8339137751426,1.84266881618924,1.87228075308603,
1.89472725344519,1.93367218232155,2.02940238011174,2.03323906857863,2.03491799477074,
2.03615229030273,2.03729050400955,2.03884038059485,2.0419356778204,2.06849902971469,
2.09264680115989,2.31947060272463,2.42592954404666,2.43354518016428,2.43666977374331,
2.43885351574569,2.44105512787418,2.44418555249449,2.45168029689903,2.56118703754135,
2.66286822169186,2.7073263880798,2.72254801315923,2.73998680039428,2.76106406127572,
2.8203574121549,2.82887850102236,2.83119497554349,2.83260877014012,2.8338857307499,
2.83551679414262,2.83884574870767,2.85904109596741,2.88682229798246,3.13282532712108,
3.23994190673852,3.24745286699174,3.25072070844132,3.25311660317803,3.25532210699968,
3.2583038710766,3.26558894973281,3.34042161917931,3.51656237394093,3.57739905987274,
3.60135200555828,3.63962409658751,3.6482655401533,3.65158437706126,3.65387301841201,
3.65611746533737,3.6588271326222,3.66561534248813,3.75059866651629,3.95019840490346,
4.08041416705069,4.0963917911434,4.1044757663243,4.11097749770821,4.11839621232373,
4.13085808084267,4.1775585690903,4.3292999960238,4.3803234026103,4.40547518838493,
4.41134209931604,4.41494402302441,4.41826245167875,4.42252857327128,4.42956852957163,
4.47233402474545,4.54340354635141,4.66150517648929,4.69189133376844,4.71479055677426,
4.72522133159218,4.73314822784188,4.74070060961517,4.75358406833934,4.79153713909647,
4.79387910800581,4.98073628656215,5.14057599251761,5.1415189278427,5.14807159666922,
5.16580787813688,5.16964324588156,5.17211829667321,5.17409712255343,5.17633220688715,
5.18010075917596,5.1944883575077,5.21801665042047,5.25056117768055,5.3121620721385,
5.50059500578965,5.57708633853893,5.58462729228998,5.58772044694801,5.59001084194445,
5.59250140730812,5.59590274983509,5.60374025755479,5.7197191232384,5.79933296225877,
5.87625286545862,5.99101534263647,5.99808106232236,6.00076779615096,6.00236511186596,
6.00387883070559,6.00599134367051,6.01023205924348,6.04411593020551,6.10228467925028,
6.24117697845001,6.34861725605406,6.36040364983722,6.36582787027085,6.37001281424483,
6.3745223491776,6.38166461220902,6.40344210444489,6.51947951209477,6.68416009053745,
6.68586366266339,6.70321996695705,6.74050031957775,6.74575396926641,6.74822322789528,
6.75014570448274,6.75223165541733,6.75555746921463,6.76638560277799,6.86791543534931,
6.9951640469647,7.12914754410345,7.13791749372051,7.14106620868783,7.14325668214021,
7.14528734221631,7.14805115338836,7.15335657347158,7.18639780753178,7.25898684382238,
7.42581419880193,7.53935989058403,7.56157534066716,7.56488673431875,7.56645000717925,
7.5676696971833,7.56899533666508,7.57114102184462,7.57856619954617,7.62596111303262,
7.70394218199319,7.7930142514309,7.95332457056652,7.96352395954735,7.96716003998187,
7.96925808625169,7.97120548146128,7.97385964332833,7.97896673839258,8.011131479465,
8.08277570423716,8.22116902770788,8.30546898708675,8.32885312813485,8.35788569015602,
8.36110491311141,8.36273585841622,8.36393481624283,8.36522996800554,8.36698279753809,
8.37095055516975,8.37628067679727,8.38947539675022,8.4362531619017,8.54619746064972,
8.76150045551478,8.77600834094723,8.78041803540703,8.78305745712411,8.7851737575176,
8.78802220488971,8.79338458500766,8.82393963711053,8.88098643322891,8.93335079496824,
8.96994528516527,9.06248712128003,9.07383123986138,9.17013383081191,9.17889014990768,
9.18233428559776,9.18441690452885,9.18663748648562,9.1888235379032,9.19170371650266,
9.19629762452744,9.20524962464218,9.22775296138128,9.30050572976896,9.3920157285172,
9.51340847384729,9.51472087286398,9.61175353227208,9.62575939980498,9.6341897590963,
9.64074631120598,9.64788641071334,9.65518949421774,9.66586118411138,9.74608359669902,
9.92246480992931,9.9376052360266,9.94274542543644,9.94585731953322,9.94902614956777,
9.95230193033657,9.95729471947809),.UNSPECIFIED.);
#3453=B_SPLINE_CURVE_WITH_KNOTS('',3,(#63459,#63460,#63461,#63462,#63463,
#63464,#63465,#63466,#63467,#63468,#63469,#63470,#63471,#63472,#63473,#63474,
#63475,#63476,#63477,#63478,#63479,#63480,#63481,#63482,#63483,#63484,#63485,
#63486,#63487,#63488,#63489,#63490,#63491,#63492,#63493,#63494,#63495,#63496,
#63497,#63498,#63499,#63500,#63501,#63502,#63503,#63504,#63505,#63506,#63507,
#63508,#63509,#63510,#63511,#63512,#63513,#63514,#63515,#63516,#63517,#63518,
#63519,#63520,#63521,#63522,#63523,#63524,#63525,#63526,#63527,#63528,#63529,
#63530,#63531,#63532,#63533,#63534,#63535,#63536,#63537,#63538,#63539,#63540,
#63541,#63542,#63543,#63544,#63545,#63546,#63547,#63548,#63549,#63550,#63551,
#63552,#63553,#63554,#63555,#63556,#63557,#63558,#63559,#63560,#63561,#63562,
#63563,#63564,#63565,#63566,#63567,#63568,#63569,#63570,#63571,#63572,#63573,
#63574,#63575,#63576,#63577,#63578,#63579,#63580,#63581,#63582,#63583,#63584,
#63585,#63586,#63587,#63588,#63589,#63590,#63591,#63592,#63593,#63594,#63595,
#63596,#63597,#63598,#63599,#63600,#63601,#63602,#63603,#63604,#63605,#63606,
#63607,#63608,#63609,#63610,#63611,#63612,#63613,#63614,#63615,#63616,#63617,
#63618,#63619,#63620,#63621,#63622,#63623,#63624,#63625,#63626,#63627,#63628,
#63629,#63630,#63631,#63632,#63633,#63634,#63635,#63636,#63637,#63638,#63639,
#63640,#63641,#63642,#63643,#63644,#63645,#63646,#63647,#63648,#63649,#63650,
#63651,#63652,#63653,#63654,#63655,#63656,#63657,#63658,#63659,#63660,#63661,
#63662,#63663,#63664,#63665,#63666,#63667,#63668,#63669,#63670,#63671,#63672,
#63673,#63674,#63675,#63676,#63677,#63678,#63679,#63680,#63681,#63682,#63683,
#63684,#63685,#63686,#63687,#63688,#63689,#63690,#63691,#63692,#63693,#63694,
#63695,#63696,#63697,#63698,#63699,#63700,#63701,#63702,#63703,#63704,#63705,
#63706,#63707,#63708,#63709,#63710,#63711,#63712,#63713,#63714,#63715,#63716,
#63717,#63718,#63719,#63720,#63721,#63722,#63723,#63724,#63725,#63726,#63727,
#63728,#63729,#63730,#63731,#63732,#63733,#63734,#63735,#63736,#63737,#63738,
#63739,#63740,#63741,#63742,#63743,#63744,#63745,#63746,#63747,#63748,#63749,
#63750,#63751,#63752,#63753,#63754,#63755,#63756,#63757,#63758,#63759,#63760,
#63761,#63762,#63763,#63764,#63765,#63766,#63767,#63768,#63769,#63770,#63771,
#63772,#63773,#63774,#63775,#63776,#63777,#63778,#63779,#63780,#63781,#63782,
#63783,#63784,#63785,#63786,#63787,#63788,#63789,#63790,#63791,#63792,#63793,
#63794,#63795,#63796,#63797,#63798,#63799,#63800,#63801,#63802,#63803,#63804,
#63805,#63806,#63807,#63808,#63809,#63810,#63811,#63812,#63813,#63814,#63815,
#63816,#63817,#63818,#63819,#63820,#63821,#63822,#63823,#63824,#63825,#63826,
#63827,#63828,#63829,#63830,#63831,#63832,#63833,#63834,#63835,#63836,#63837,
#63838,#63839,#63840,#63841,#63842,#63843,#63844,#63845,#63846,#63847,#63848,
#63849,#63850,#63851,#63852,#63853,#63854,#63855,#63856,#63857,#63858,#63859,
#63860,#63861,#63862,#63863,#63864,#63865,#63866,#63867,#63868,#63869,#63870,
#63871,#63872,#63873,#63874,#63875,#63876,#63877,#63878,#63879,#63880,#63881,
#63882,#63883,#63884,#63885,#63886,#63887,#63888,#63889,#63890,#63891,#63892,
#63893,#63894,#63895,#63896,#63897,#63898,#63899,#63900,#63901,#63902,#63903,
#63904,#63905,#63906,#63907,#63908,#63909,#63910,#63911,#63912,#63913,#63914,
#63915,#63916,#63917,#63918,#63919,#63920,#63921,#63922,#63923,#63924,#63925,
#63926,#63927,#63928,#63929,#63930,#63931,#63932,#63933,#63934,#63935,#63936,
#63937,#63938,#63939,#63940,#63941,#63942,#63943,#63944,#63945,#63946,#63947,
#63948,#63949,#63950,#63951,#63952,#63953,#63954,#63955,#63956,#63957,#63958,
#63959,#63960,#63961,#63962,#63963,#63964,#63965,#63966,#63967,#63968,#63969,
#63970,#63971,#63972),.UNSPECIFIED.,.F.,.F.,(4,2,2,2,2,2,2,2,2,2,2,2,2,
2,2,2,2,2,2,2,2,2,2,2,2,2,2,2,2,2,2,2,2,2,2,2,2,2,2,2,2,2,2,2,2,2,2,2,2,
2,2,2,2,2,2,2,2,2,2,2,2,2,2,2,2,2,2,2,2,2,2,2,2,2,2,2,2,2,2,2,2,2,2,2,2,
2,2,2,2,2,2,2,2,2,2,2,2,2,2,2,2,2,2,2,2,2,2,2,2,2,2,2,2,2,2,2,2,2,2,2,2,
2,2,2,2,2,2,2,2,2,2,2,2,2,2,2,2,2,2,2,2,2,2,2,2,2,2,2,2,2,2,2,2,2,2,2,2,
2,2,2,2,2,2,2,2,2,2,2,2,2,2,2,2,2,2,2,2,2,2,2,2,2,2,2,2,2,2,2,2,2,2,2,2,
2,2,2,2,2,2,2,2,2,2,2,2,2,2,2,2,2,2,2,2,2,2,2,2,2,2,2,2,2,2,2,2,2,2,2,2,
2,2,2,2,2,2,2,2,2,2,2,2,2,2,2,2,2,2,2,2,2,2,2,2,2,2,2,4),(0.00194477749240243,
0.00764117539682748,0.0205707215302883,0.123608016854099,0.232944908166683,
0.265444928942391,0.281957396127948,0.292272408635366,0.300069430396495,
0.308046128403578,0.315505729710164,0.325853021136944,0.353454688474741,
0.541987999039527,0.621661119734957,0.728341535143952,0.742092648891072,
0.744835619976621,0.746860767290477,0.748894394276984,0.750735103243517,
0.753177757034121,0.759297787650504,0.831007528441508,0.851939223796619,
0.869181819275023,0.922901943195041,1.03420307423587,1.11828356832654,1.15530219407324,
1.16110353069289,1.16411193066949,1.16631666673478,1.16868959273105,1.17209157643427,
1.18151197263578,1.33377915080775,1.41842981375281,1.5149151251787,1.55304456490883,
1.57172928729574,1.57515545893047,1.5768067271746,1.57849656556038,1.58008141127905,
1.58226990092565,1.58785372786726,1.68163760330582,1.82588791502246,1.89349259303035,
1.91717511494179,1.92838639431105,1.93489361230526,1.93943348808351,1.94390715913749,
1.94810767246972,1.95362384260449,1.9629532196991,2.01398853016757,2.02556237432937,
2.06239408044429,2.23802298288018,2.30852645512544,2.3157962683899,2.32121804646986,
2.3236094543644,2.32555893996895,2.32734571792745,2.32974970071864,2.33438685291171,
2.37169937210081,2.40978232197433,2.58896074070278,2.70781146615728,2.71469415054384,
2.71776799644888,2.72005309421383,2.72217893568093,2.72508733456416,2.73236692013362,
2.81542680738107,2.91208084175454,3.0392551871556,3.0946765201984,3.12381660852781,
3.13823497961957,3.14093596085108,3.14239071993551,3.14347994519846,3.14467494224146,
3.14683148707961,3.15355837715516,3.25593450946252,3.41944245987133,3.53393033868513,
3.54072153506419,3.54370342815266,3.54590010771965,3.54792950030269,3.55068415398807,
3.55746836619038,3.62889732834507,3.67399253262379,3.83362278464016,3.93301423190129,
3.93701495718578,3.93876636721242,3.94006125600189,3.94126090451689,3.94289428821171,
3.94694048060471,3.99017503945279,4.02026895794056,4.23234444654913,4.31368247927847,
4.3496085414292,4.35520430257812,4.35810196410263,4.36042627977323,4.36309963079874,
4.36766153565265,4.38349953150361,4.62886446591434,4.68798965132942,4.74371375886848,
4.75464123434014,4.75827980530834,4.7606370859362,4.76286367765137,4.76580225184959,
4.77080695806768,4.80347717727004,4.97939432843297,5.17631734566855,5.19948718183741,
5.20816726018814,5.21437887107058,5.2209609488926,5.22970003460272,5.24906602706153,
5.32733625708333,5.43065239659928,5.50915587406734,5.51706479988117,5.52104503069185,
5.52432825713613,5.52815365880615,5.53491641409147,5.56595248577434,5.676392452838,
5.80764159979335,5.82337816962009,5.83332134401914,5.84118907653832,5.8500535684336,
5.86515964221325,5.93057430909038,6.0170236802654,6.25232781759534,6.27282002157152,
6.2768516955123,6.27938736594753,6.28137295028718,6.28357247016948,6.28718091091564,
6.29989265467418,6.38083926219928,6.45801153462545,6.55759742784279,6.68319870529378,
6.69161029373078,6.69485237062276,6.69718190054875,6.69964879411393,6.70290421453076,
6.70994297239214,6.81553705884479,7.07247088653083,7.10312667819184,7.10746126189772,
7.10959330060459,7.11126669793772,7.11312407005727,7.11617886775548,7.12700464979704,
7.20259581491576,7.34328814727695,7.45663625451868,7.46828675097555,7.47377026069598,
7.47797972088986,7.48243490149179,7.48932438116171,7.50927471122013,7.60945208219588,
7.82878573450636,7.85031757557046,7.85432505269809,7.85680705859884,7.8587262610401,
7.86082750032375,7.86421895002785,7.87562726601466,8.03755863910899,8.23373758958363,
8.24578599762793,8.24977652481494,8.25200514974098,8.25422659455003,8.25695279280755,
8.26214721046688,8.26866910468058,8.28276375668469,8.32721379867204,8.41122430655572,
8.65811673957347,8.67174300598273,8.67429467748854,8.67585647188362,8.67707645528398,
8.6784038752094,8.68055584964091,8.68803449686276,8.73597358231969,8.81373966745279,
8.83739789020678,8.91156040404885,8.96491354203416,9.06665038216933,9.07404689353395,
9.0771606914931,9.07935959767508,9.08137894130742,9.08355814058727,9.08896382863302,
9.12963507267496,9.2330125263038,9.44533464322258,9.46822265725664,9.4715681397533,
9.47320008685845,9.47447791253375,9.47589284141639,9.47821158627288,9.48632909854615,
9.53881870096469,9.82662546545269,9.83952194870502,9.88318763120856,9.88898021637239,
9.89196131341892,9.89416749632007,9.89640363694041,9.89873794263655,9.90180675688963,
9.90667201140883,9.95997803070509),.UNSPECIFIED.);
#3454=B_SPLINE_CURVE_WITH_KNOTS('',3,(#63974,#63975,#63976,#63977,#63978,
#63979,#63980,#63981,#63982,#63983,#63984,#63985,#63986),.UNSPECIFIED.,
 .F.,.F.,(4,1,1,1,1,1,1,1,1,1,4),(32.539575242042,32.9188985837215,33.4176697743839,
33.9164409650463,34.4152121557088,34.9139833463713,35.9115257276962,36.4102969183586,
36.909068109021,37.906610490346,38.822750516815),.UNSPECIFIED.);
#3455=B_SPLINE_CURVE_WITH_KNOTS('',3,(#63988,#63989,#63990,#63991,#63992,
#63993,#63994,#63995,#63996,#63997,#63998,#63999,#64000,#64001,#64002,#64003,
#64004,#64005,#64006,#64007,#64008,#64009,#64010,#64011,#64012,#64013,#64014,
#64015,#64016,#64017,#64018,#64019,#64020,#64021,#64022,#64023,#64024,#64025,
#64026,#64027,#64028,#64029,#64030,#64031,#64032,#64033,#64034,#64035,#64036,
#64037,#64038,#64039,#64040,#64041,#64042,#64043,#64044,#64045,#64046,#64047,
#64048,#64049,#64050,#64051,#64052,#64053,#64054,#64055,#64056,#64057,#64058,
#64059,#64060,#64061,#64062,#64063,#64064,#64065,#64066,#64067,#64068,#64069,
#64070,#64071,#64072,#64073,#64074,#64075,#64076,#64077,#64078,#64079,#64080,
#64081,#64082,#64083,#64084,#64085,#64086,#64087,#64088,#64089,#64090,#64091,
#64092,#64093,#64094,#64095,#64096,#64097,#64098,#64099,#64100,#64101,#64102,
#64103,#64104,#64105,#64106,#64107,#64108,#64109,#64110,#64111,#64112,#64113,
#64114,#64115,#64116,#64117,#64118,#64119,#64120,#64121,#64122,#64123,#64124,
#64125,#64126,#64127,#64128,#64129,#64130,#64131,#64132,#64133,#64134,#64135,
#64136,#64137,#64138,#64139,#64140,#64141,#64142,#64143,#64144,#64145,#64146,
#64147,#64148,#64149,#64150,#64151,#64152,#64153,#64154,#64155,#64156,#64157,
#64158,#64159,#64160,#64161,#64162,#64163,#64164,#64165,#64166,#64167,#64168,
#64169,#64170,#64171,#64172,#64173,#64174,#64175,#64176,#64177,#64178,#64179,
#64180,#64181,#64182,#64183,#64184,#64185,#64186,#64187,#64188,#64189,#64190,
#64191,#64192,#64193,#64194,#64195,#64196,#64197,#64198,#64199,#64200,#64201,
#64202,#64203,#64204,#64205,#64206,#64207,#64208,#64209,#64210,#64211,#64212,
#64213,#64214,#64215,#64216,#64217,#64218,#64219,#64220,#64221,#64222,#64223,
#64224,#64225,#64226,#64227,#64228,#64229,#64230,#64231,#64232,#64233,#64234,
#64235,#64236,#64237,#64238,#64239,#64240,#64241,#64242,#64243,#64244,#64245,
#64246,#64247,#64248,#64249,#64250,#64251,#64252,#64253,#64254,#64255,#64256,
#64257,#64258,#64259,#64260,#64261,#64262,#64263,#64264,#64265,#64266,#64267,
#64268,#64269,#64270,#64271,#64272,#64273,#64274,#64275,#64276,#64277,#64278,
#64279,#64280,#64281,#64282,#64283,#64284,#64285,#64286,#64287,#64288,#64289,
#64290,#64291,#64292,#64293,#64294,#64295,#64296,#64297,#64298,#64299,#64300,
#64301,#64302,#64303,#64304,#64305,#64306,#64307,#64308,#64309,#64310,#64311,
#64312,#64313,#64314,#64315,#64316,#64317,#64318,#64319,#64320,#64321,#64322,
#64323,#64324,#64325,#64326,#64327,#64328,#64329,#64330,#64331,#64332,#64333,
#64334,#64335,#64336,#64337,#64338,#64339,#64340,#64341,#64342,#64343,#64344,
#64345,#64346,#64347,#64348,#64349,#64350,#64351,#64352,#64353,#64354,#64355,
#64356,#64357,#64358,#64359,#64360,#64361,#64362,#64363,#64364,#64365,#64366,
#64367,#64368,#64369,#64370,#64371,#64372,#64373,#64374,#64375,#64376,#64377,
#64378,#64379,#64380,#64381,#64382,#64383,#64384,#64385,#64386,#64387,#64388,
#64389,#64390,#64391,#64392,#64393,#64394,#64395,#64396,#64397,#64398,#64399,
#64400,#64401,#64402,#64403,#64404,#64405,#64406,#64407,#64408,#64409,#64410,
#64411,#64412,#64413,#64414,#64415,#64416,#64417,#64418,#64419,#64420,#64421,
#64422,#64423,#64424,#64425,#64426,#64427,#64428,#64429,#64430,#64431,#64432,
#64433,#64434,#64435,#64436,#64437,#64438,#64439,#64440,#64441,#64442,#64443,
#64444,#64445,#64446,#64447,#64448,#64449,#64450,#64451,#64452,#64453,#64454,
#64455,#64456,#64457,#64458,#64459,#64460,#64461,#64462,#64463,#64464,#64465,
#64466,#64467,#64468,#64469,#64470,#64471,#64472,#64473,#64474,#64475,#64476,
#64477,#64478,#64479,#64480,#64481,#64482,#64483,#64484,#64485,#64486,#64487,
#64488,#64489,#64490,#64491),.UNSPECIFIED.,.F.,.F.,(4,2,2,2,2,2,2,2,2,2,
2,2,2,2,2,2,2,2,2,2,2,2,2,2,2,2,2,2,2,2,2,2,2,2,2,2,2,2,2,2,2,2,2,2,2,2,
2,2,2,2,2,2,2,2,2,2,2,2,2,2,2,2,2,2,2,2,2,2,2,2,2,2,2,2,2,2,2,2,2,2,2,2,
2,2,2,2,2,2,2,2,2,2,2,2,2,2,2,2,2,2,2,2,2,2,2,2,2,2,2,2,2,2,2,2,2,2,2,2,
2,2,2,2,2,2,2,2,2,2,2,2,2,2,2,2,2,2,2,2,2,2,2,2,2,2,2,2,2,2,2,2,2,2,2,2,
2,2,2,2,2,2,2,2,2,2,2,2,2,2,2,2,2,2,2,2,2,2,2,2,2,2,2,2,2,2,2,2,2,2,2,2,
2,2,2,2,2,2,2,2,2,2,2,2,2,2,2,2,2,2,2,2,2,2,2,2,2,2,2,2,2,2,2,2,2,2,2,2,
2,2,2,2,2,2,2,2,2,2,2,2,2,2,2,2,2,2,2,2,2,2,2,2,2,4),(0.00201683040818403,
0.0555090148573186,0.0643938470318102,0.0667453893304715,0.0682885389994091,
0.0695126145659887,0.070759772446445,0.0720105510768564,0.0742187584978422,
0.0806712736091462,0.098794631135621,0.134664308353278,0.142909789112026,
0.394731574652877,0.451284979485798,0.480709374429789,0.486016146248271,
0.488852437752199,0.490967264442421,0.493614556785553,0.498060684350159,
0.512883024717616,0.779875996828031,0.878330599117946,0.886319569557424,
0.889535252192457,0.891581385738048,0.893782943749686,0.896789819988317,
0.903472637202945,0.994963931826603,1.08905422398927,1.2832828642102,1.31159029699064,
1.33187073976458,1.34075733881825,1.34736166025531,1.35352731229434,1.3637100421381,
1.39001257046794,1.61336825420023,1.64291287588334,1.64906101581913,1.65271773699212,
1.65602173627205,1.66010344654139,1.66811529807963,1.71930801783313,1.89347072082819,
1.92715086190482,1.95196284104676,1.96272899140048,1.97070719317361,1.97816100793995,
1.98848872299682,2.01591409124277,2.19555058260022,2.33061170284428,2.38058199148277,
2.40359001430013,2.40795733817389,2.41029062824737,2.41222107510303,2.41444830860626,
2.41821780726698,2.43159755842704,2.6734797861835,2.72781288053626,2.78766541481223,
2.81862361574562,2.82415558972066,2.82710640817316,2.82930412274633,2.83205201612524,
2.83665959634171,2.85195944840177,3.15105901313849,3.22562393469632,3.23633944006411,
3.23937993674284,3.2412339244301,3.24290769940844,3.24504494745871,3.24926351741359,
3.27441559198193,3.39285516533644,3.50415751185819,3.5810710723635,3.5975005465717,
3.6037698390979,3.60809285788579,3.61233824194844,3.61747761277771,3.63032259145596,
3.74535114362532,3.86402332411331,3.94880868234255,3.98055389663936,3.98518596978532,
3.98755732974932,3.98944646226141,3.99160521351217,3.99525501486511,4.00761509360781,
4.25311342240517,4.37142486387778,4.37836576164698,4.38145030812162,4.38373728632486,
4.38586053541421,4.3887586777808,4.39597977223854,4.47636307782149,4.64807404244438,
4.7915587504652,4.80250532020607,4.80498934433441,4.80639685901708,4.80748310361709,
4.80889436904514,4.81137271214354,4.8213790109683,4.97947149127639,5.05456119801861,
5.13258915746767,5.19255647557782,5.20301280056308,5.20668638922413,5.20879201342372,
5.21073767829631,5.21337617800424,5.21840839749931,5.24878815241691,5.31308318889736,
5.54076617068461,5.59683791743833,5.60098733944557,5.60263019297209,5.60383237417449,
5.60512574009732,5.60686692010724,5.61076952903634,5.70397167968519,5.77331660971036,
5.88460702817492,6.00934467255547,6.01767298000313,6.02083150543805,6.02308388823859,
6.02521647779603,6.02818938558461,6.03414708982201,6.08108271519217,6.15569128116155,
6.40333844189808,6.41769384945028,6.42190373724689,6.42438861014184,6.42656043992883,
6.42928373697768,6.4345962824552,6.47124126655081,6.57462033686866,6.74235668165456,
6.76362008225968,6.76839560237107,6.85407790019257,6.86714532992767,6.87539033085158,
6.88190869720229,6.88922692980271,6.90154829280269,6.95108510563445,7.04610699437988,
7.12947400693111,7.17423365011768,7.18142201371457,7.18531675587625,7.18826904971285,
7.19204670399925,7.19859096401319,7.22646619120977,7.28364788273798,7.44978565979028,
7.48239220537823,7.49435655521553,7.50173512027721,7.50976393041603,7.52082899722055,
7.54777232072478,7.76501222432846,7.91875159402629,7.91967829935442,7.93738056034355,
7.9412138328333,7.94368849481866,7.94566763856805,7.94790375404052,7.95167566216491,
7.96609493843499,8.12221678171655,8.20374990127786,8.34685604695653,8.3557030985563,
8.35901544273294,8.36136383030206,8.36377296774502,8.36687930296074,8.37028064746644,
8.3758428028379,8.38690112722841,8.41479250530208,8.51843367022146,8.75591379706171,
8.76884797332762,8.77219593555343,8.77413892185669,8.77563581126679,8.77757684437954,
8.78100716816862,8.7962572939637,9.00252260403534,9.12081850775346,9.12784056816598,
9.13494143749434,9.13966288628808,9.1433806041868,9.14818162921303,9.15663711802306,
9.19024694880289,9.42842525606427,9.47502219108499,9.4869489251703,9.51409036420894,
9.51840586847915,9.5209521972705,9.52288756188118,9.52494180505167,9.52812250013544,
9.53773588083188,9.625606287343,9.87038780447967,9.88320377903118,9.90795121349442,
9.91264828770526,9.91553688666106,9.91773482085342,9.91983692491677,9.92224212492766,
9.92562447892427,9.93716499782376,9.96015150473948),.UNSPECIFIED.);
#3456=B_SPLINE_CURVE_WITH_KNOTS('',3,(#64493,#64494,#64495,#64496,#64497,
#64498,#64499,#64500,#64501,#64502,#64503,#64504,#64505,#64506,#64507,#64508,
#64509,#64510,#64511,#64512,#64513,#64514,#64515,#64516,#64517,#64518,#64519,
#64520,#64521,#64522,#64523,#64524,#64525,#64526,#64527,#64528,#64529,#64530,
#64531,#64532,#64533,#64534,#64535,#64536,#64537,#64538,#64539,#64540,#64541,
#64542,#64543,#64544,#64545,#64546,#64547,#64548,#64549,#64550,#64551,#64552,
#64553,#64554,#64555,#64556,#64557,#64558,#64559,#64560,#64561,#64562,#64563,
#64564,#64565,#64566,#64567,#64568,#64569,#64570,#64571,#64572,#64573,#64574,
#64575,#64576,#64577,#64578,#64579,#64580,#64581,#64582,#64583,#64584,#64585,
#64586,#64587,#64588,#64589,#64590,#64591,#64592,#64593,#64594,#64595,#64596,
#64597,#64598,#64599,#64600,#64601,#64602,#64603,#64604,#64605,#64606,#64607,
#64608,#64609,#64610,#64611,#64612,#64613,#64614,#64615,#64616,#64617,#64618,
#64619,#64620,#64621,#64622,#64623,#64624,#64625,#64626,#64627,#64628,#64629,
#64630,#64631,#64632,#64633,#64634,#64635,#64636,#64637,#64638,#64639,#64640,
#64641,#64642,#64643,#64644,#64645,#64646,#64647,#64648,#64649,#64650,#64651,
#64652,#64653,#64654,#64655,#64656,#64657,#64658,#64659,#64660,#64661,#64662,
#64663,#64664,#64665,#64666,#64667,#64668,#64669,#64670,#64671,#64672,#64673,
#64674,#64675,#64676,#64677,#64678,#64679,#64680,#64681,#64682,#64683,#64684,
#64685,#64686,#64687,#64688,#64689,#64690,#64691,#64692,#64693,#64694,#64695,
#64696,#64697,#64698,#64699,#64700,#64701,#64702,#64703,#64704,#64705,#64706,
#64707,#64708,#64709,#64710,#64711,#64712,#64713,#64714,#64715,#64716,#64717,
#64718,#64719,#64720,#64721,#64722,#64723,#64724,#64725,#64726,#64727,#64728,
#64729,#64730,#64731,#64732,#64733,#64734,#64735,#64736,#64737,#64738,#64739,
#64740,#64741,#64742,#64743,#64744,#64745,#64746,#64747,#64748,#64749,#64750,
#64751,#64752,#64753,#64754,#64755,#64756,#64757,#64758,#64759,#64760,#64761,
#64762,#64763,#64764,#64765,#64766,#64767,#64768,#64769,#64770,#64771,#64772,
#64773,#64774,#64775,#64776,#64777,#64778,#64779,#64780,#64781,#64782,#64783,
#64784,#64785,#64786,#64787,#64788,#64789,#64790,#64791,#64792,#64793,#64794,
#64795,#64796,#64797,#64798,#64799,#64800,#64801,#64802,#64803,#64804,#64805,
#64806,#64807,#64808,#64809,#64810,#64811,#64812,#64813,#64814,#64815,#64816,
#64817,#64818,#64819,#64820,#64821,#64822,#64823,#64824,#64825,#64826,#64827,
#64828,#64829,#64830,#64831,#64832,#64833,#64834,#64835,#64836,#64837,#64838,
#64839,#64840,#64841,#64842,#64843,#64844,#64845,#64846,#64847,#64848,#64849,
#64850,#64851,#64852,#64853,#64854,#64855,#64856,#64857,#64858,#64859,#64860,
#64861,#64862,#64863,#64864,#64865,#64866,#64867,#64868,#64869,#64870,#64871,
#64872,#64873,#64874,#64875,#64876,#64877,#64878,#64879,#64880,#64881,#64882,
#64883,#64884,#64885,#64886,#64887,#64888,#64889,#64890,#64891,#64892,#64893,
#64894,#64895,#64896,#64897,#64898,#64899,#64900,#64901,#64902,#64903,#64904,
#64905,#64906,#64907,#64908,#64909,#64910,#64911,#64912,#64913,#64914,#64915,
#64916,#64917,#64918,#64919,#64920,#64921,#64922,#64923,#64924,#64925,#64926,
#64927,#64928,#64929,#64930,#64931,#64932,#64933,#64934,#64935,#64936,#64937,
#64938,#64939,#64940,#64941,#64942,#64943,#64944,#64945,#64946,#64947,#64948,
#64949,#64950,#64951,#64952,#64953,#64954,#64955,#64956,#64957,#64958,#64959,
#64960,#64961,#64962,#64963,#64964,#64965,#64966,#64967,#64968,#64969,#64970,
#64971,#64972,#64973,#64974,#64975,#64976,#64977,#64978,#64979,#64980,#64981,
#64982,#64983,#64984,#64985,#64986,#64987,#64988,#64989,#64990,#64991,#64992,
#64993,#64994),.UNSPECIFIED.,.F.,.F.,(4,2,2,2,2,2,2,2,2,2,2,2,2,2,2,2,2,
2,2,2,2,2,2,2,2,2,2,2,2,2,2,2,2,2,2,2,2,2,2,2,2,2,2,2,2,2,2,2,2,2,2,2,2,
2,2,2,2,2,2,2,2,2,2,2,2,2,2,2,2,2,2,2,2,2,2,2,2,2,2,2,2,2,2,2,2,2,2,2,2,
2,2,2,2,2,2,2,2,2,2,2,2,2,2,2,2,2,2,2,2,2,2,2,2,2,2,2,2,2,2,2,2,2,2,2,2,
2,2,2,2,2,2,2,2,2,2,2,2,2,2,2,2,2,2,2,2,2,2,2,2,2,2,2,2,2,2,2,2,2,2,2,2,
2,2,2,2,2,2,2,2,2,2,2,2,2,2,2,2,2,2,2,2,2,2,2,2,2,2,2,2,2,2,2,2,2,2,2,2,
2,2,2,2,2,2,2,2,2,2,2,2,2,2,2,2,2,2,2,2,2,2,2,2,2,2,2,2,2,2,2,2,2,2,2,2,
2,2,2,2,2,2,2,2,2,2,2,2,2,2,2,2,2,4),(0.00344090123650659,0.248215503652584,
0.325199316815864,0.361756705116737,0.379269440842161,0.382118691064504,
0.383605137854968,0.38481377710383,0.386200966519763,0.388571418706616,
0.397442785636797,0.53607390243376,0.660481583835621,0.774585618337096,
0.781830897072744,0.784892950856695,0.786922671225327,0.789113196444733,
0.792191701583214,0.799398275956577,0.890933199784602,0.962713797610933,
1.08220084343428,1.12716778187331,1.15950233024339,1.17611275782848,1.17894148503769,
1.18046789724749,1.18172478878023,1.18320777696307,1.18576514284896,1.19543545733353,
1.34968071181659,1.47255901722294,1.58683241729188,1.59244459257325,1.59582663168457,
1.59889364258051,1.60125195872541,1.60349103572916,1.60660048371062,1.6146305586267,
1.73099633663034,1.7921319566467,1.92598091506575,1.94965701599503,1.98765921406415,
1.99626351833744,1.99957722682606,2.00186528267131,2.00411147767362,2.00682608241167,
2.01364170415744,2.11691726059793,2.30772809841377,2.42912201463569,2.44470599321589,
2.45271241401749,2.45858616428045,2.46493753933213,2.47607619853322,2.5092210522027,
2.72540262717015,2.75347288492772,2.75953351936804,2.76317397202912,2.7664829986683,
2.77074510062788,2.77930860342132,2.85421491420867,2.98687678325841,3.05304462653619,
3.0681897549913,3.07707243341869,3.08493915069915,3.09486067908611,3.11064095711837,
3.1829083529179,3.43157172362452,3.48899017795257,3.51422330475956,3.51870572428563,
3.52109772642029,3.52287957618972,3.52510937108676,3.52885207873761,3.54130944968555,
3.73341763923747,3.84311546757308,3.90046394085057,3.92961409240206,3.93505546382703,
3.93798773546222,3.94018463669266,3.94294859765071,3.94762423044451,3.9634999859706,
4.24050283438229,4.34401242363817,4.34895863345328,4.35120928704915,4.35289950277004,
4.35448485343561,4.35667427896422,4.36226176518648,4.45678576035414,4.68005287595498,
4.70620435911724,4.71367229637033,4.71825595926134,4.72242146295673,4.7277887302769,
4.73853822592383,4.79792011029415,4.83680791943469,4.98338675358833,5.08928844506195,
5.09551091009682,5.09798604509323,5.09979140605412,5.10172864236923,5.10432999587132,
5.11013712266719,5.19288222117589,5.47270706664273,5.48735481936215,5.49166634742306,
5.49421411274008,5.49623859067265,5.49893981512383,5.50394930888009,5.53068127345038,
5.58260261832545,5.68831214052396,5.73061181366884,5.77684627313265,5.90580081121727,
5.9142130918677,5.91656519499312,5.91795711937655,5.91916538165629,5.92064723478159,
5.92353564752487,5.94316738170192,5.99072486899088,6.14933720109695,6.30487763657126,
6.31481721883493,6.31841494341739,6.320505527776,6.32245530823129,6.32512706874381,
6.33031736613628,6.36460342060074,6.45686138962944,6.5899170899621,6.70391939155122,
6.71134210036557,6.713641859677,6.71491086325772,6.71618159829422,6.71774575907195,
6.7207482121431,6.73933710428698,6.77918257480237,6.91479411669491,6.96344753718218,
7.11863684766936,7.12849935881802,7.13226850477425,7.13451616237806,7.13688756648348,
7.14000214788525,7.14667897027029,7.23706714479836,7.46432325042959,7.52561510674412,
7.53185821822271,7.53473550631765,7.53695245153251,7.53928607395297,7.54289747741423,
7.5471545839431,7.55520552041704,7.63410275899928,7.74479915888493,7.82389347000999,
7.84037715145234,7.95974472042592,7.97596878187591,7.98421109030493,7.99031195965339,
7.99697035698284,8.00615796422281,8.02810792439933,8.11097558117127,8.25133855539605,
8.28637548125199,8.29306698854525,8.29680127572277,8.29980075351515,8.30364414088957,
8.31048635971695,8.34275191622394,8.45355743324095,8.58318057775002,8.59889928398054,
8.60883841008606,8.61670748886037,8.62557831417302,8.64070727773233,8.70177915035901,
8.80940399575536,8.99715819998764,9.00770724202651,9.01133663400182,9.0139279428649,
9.02200672701579,9.0476622371378,9.05199984223864,9.05459993342341,9.0566008075898,
9.05844308231652,9.06148746617733,9.06955114981409,9.08094266348919,9.1117494300351,
9.16303364180909,9.39543957448968,9.46062652199351,9.46727645935126,9.47053311193938,
9.472866472814,9.47533133717993,9.47857387786533,9.48554531974914,9.58323440962424,
9.81656444638671,9.82633501963593,9.83311518614364,9.83476220081181,9.83767327265969,
9.87819248226354,9.88282569193085,9.88499285628806,9.88667566852092,9.88823944841706,
9.89003249905365,9.89256436907517,9.89687948353486,9.96138941159552),
 .UNSPECIFIED.);
#3457=B_SPLINE_CURVE_WITH_KNOTS('',3,(#64996,#64997,#64998,#64999,#65000,
#65001,#65002,#65003,#65004,#65005,#65006,#65007,#65008,#65009,#65010,#65011,
#65012,#65013,#65014,#65015,#65016,#65017,#65018,#65019,#65020,#65021,#65022,
#65023,#65024,#65025,#65026,#65027,#65028,#65029,#65030,#65031,#65032,#65033,
#65034,#65035,#65036,#65037,#65038,#65039,#65040,#65041,#65042,#65043,#65044,
#65045,#65046,#65047,#65048,#65049,#65050,#65051,#65052,#65053,#65054,#65055,
#65056,#65057,#65058,#65059,#65060,#65061,#65062,#65063,#65064,#65065,#65066,
#65067,#65068,#65069,#65070,#65071,#65072,#65073,#65074,#65075,#65076,#65077,
#65078,#65079,#65080,#65081,#65082,#65083,#65084,#65085,#65086,#65087,#65088,
#65089,#65090,#65091,#65092,#65093,#65094,#65095,#65096,#65097,#65098,#65099,
#65100,#65101,#65102,#65103,#65104,#65105,#65106,#65107,#65108,#65109,#65110,
#65111,#65112,#65113,#65114,#65115,#65116,#65117,#65118,#65119,#65120,#65121,
#65122,#65123,#65124,#65125,#65126,#65127,#65128,#65129,#65130,#65131,#65132,
#65133,#65134,#65135,#65136,#65137,#65138,#65139,#65140,#65141,#65142,#65143,
#65144,#65145,#65146,#65147,#65148,#65149,#65150,#65151,#65152,#65153,#65154,
#65155,#65156,#65157,#65158,#65159,#65160,#65161,#65162,#65163,#65164,#65165,
#65166,#65167,#65168,#65169,#65170,#65171,#65172,#65173,#65174,#65175,#65176,
#65177,#65178,#65179,#65180,#65181,#65182,#65183,#65184,#65185,#65186,#65187,
#65188,#65189,#65190,#65191,#65192,#65193,#65194,#65195,#65196,#65197,#65198,
#65199,#65200,#65201,#65202,#65203,#65204,#65205,#65206,#65207,#65208,#65209,
#65210,#65211,#65212,#65213,#65214,#65215,#65216,#65217,#65218,#65219,#65220,
#65221,#65222,#65223,#65224,#65225,#65226,#65227,#65228,#65229,#65230,#65231,
#65232,#65233,#65234,#65235,#65236,#65237,#65238,#65239,#65240,#65241,#65242,
#65243,#65244,#65245,#65246,#65247,#65248,#65249,#65250,#65251,#65252,#65253,
#65254,#65255,#65256,#65257),.UNSPECIFIED.,.F.,.F.,(4,3,3,3,3,3,3,3,3,3,
3,3,3,3,3,3,3,3,3,3,3,3,3,3,3,3,3,3,3,3,3,3,3,3,3,3,3,3,3,3,3,3,3,3,3,3,
3,3,3,3,3,3,3,3,3,3,3,3,3,3,3,3,3,3,3,3,3,3,3,3,3,3,3,3,3,3,3,3,3,3,3,3,
3,3,3,3,3,4),(63.9555017779399,64.0273228485219,64.0990874604196,64.1708067672796,
64.242499811206,64.3141860900314,64.3414835954556,64.4217776112221,64.5022162304088,
64.5867258693361,64.6675004145408,64.748375898319,64.8293859440099,64.840254786118,
64.9147955906901,64.9892604123256,65.0636631423213,65.1380176309775,65.2123376964115,
65.2905201302905,65.3648279193654,65.4391453967353,65.5134850498522,65.5878593755268,
65.662319405382,65.7368292336065,65.8114395065763,65.8377971674429,65.9109502594573,
65.9840155087585,66.057007839811,66.1299421083477,66.202833116744,66.2756956279024,
66.348558241444,66.4214246268581,66.4943081271963,66.5672220966958,66.6402228321809,
66.7132710318568,66.7864302035233,66.8353395487678,66.9108761820243,66.9863269401705,
67.0617047153914,67.1370223521918,67.2122926554366,67.2898663147686,67.3650860090466,
67.4402998249563,67.5155193091636,67.5907560093478,67.6660485392281,67.7413742748641,
67.8167704926212,67.8328819300927,67.9094806718979,67.9860143617395,68.0624926775479,
68.1389168138957,68.2153082200934,68.2916758052387,68.3316531207551,68.4097742707722,
68.4879403364027,68.5661560514746,68.6444625136851,68.7228171709755,68.8012571059632,
68.8304243114176,68.9123931124947,68.9942901248862,69.0780164691847,69.1596733426811,
69.2444344223806,69.3291955020801,69.4028225266105,69.4764443003387,69.5500738061759,
69.623755474427,69.6974644080224,69.771254988521,69.8279666927425,69.9121598020123,
69.9961817097602,70.080066989409,70.1636682981196,70.2386870851195),
 .UNSPECIFIED.);
#3458=B_SPLINE_CURVE_WITH_KNOTS('',3,(#65259,#65260,#65261,#65262,#65263,
#65264,#65265,#65266,#65267,#65268,#65269,#65270,#65271,#65272,#65273,#65274,
#65275,#65276,#65277,#65278,#65279,#65280,#65281,#65282,#65283,#65284,#65285,
#65286,#65287,#65288,#65289,#65290,#65291,#65292,#65293,#65294,#65295,#65296,
#65297,#65298,#65299,#65300,#65301,#65302,#65303,#65304,#65305,#65306,#65307,
#65308,#65309,#65310,#65311,#65312,#65313,#65314,#65315,#65316,#65317,#65318,
#65319,#65320,#65321,#65322,#65323,#65324,#65325,#65326,#65327,#65328,#65329,
#65330,#65331,#65332,#65333,#65334,#65335,#65336,#65337,#65338,#65339,#65340,
#65341,#65342,#65343,#65344,#65345,#65346,#65347,#65348,#65349,#65350,#65351,
#65352,#65353,#65354,#65355,#65356,#65357,#65358,#65359,#65360,#65361,#65362,
#65363,#65364,#65365,#65366,#65367,#65368,#65369,#65370,#65371,#65372,#65373,
#65374,#65375,#65376,#65377,#65378,#65379,#65380,#65381,#65382,#65383,#65384,
#65385,#65386,#65387,#65388,#65389,#65390,#65391,#65392,#65393,#65394,#65395,
#65396,#65397,#65398,#65399,#65400,#65401,#65402,#65403,#65404,#65405,#65406,
#65407,#65408,#65409,#65410,#65411,#65412,#65413,#65414,#65415,#65416,#65417,
#65418,#65419,#65420,#65421,#65422,#65423,#65424,#65425,#65426,#65427,#65428,
#65429,#65430,#65431,#65432,#65433,#65434,#65435,#65436,#65437,#65438,#65439,
#65440,#65441,#65442,#65443,#65444,#65445,#65446,#65447,#65448,#65449,#65450,
#65451,#65452,#65453,#65454,#65455,#65456,#65457,#65458,#65459,#65460,#65461,
#65462,#65463,#65464,#65465,#65466,#65467,#65468,#65469,#65470,#65471,#65472,
#65473,#65474,#65475,#65476,#65477,#65478,#65479,#65480,#65481,#65482,#65483,
#65484,#65485,#65486,#65487,#65488,#65489,#65490,#65491,#65492,#65493,#65494,
#65495,#65496,#65497,#65498,#65499,#65500,#65501,#65502,#65503,#65504,#65505,
#65506,#65507,#65508,#65509,#65510,#65511,#65512,#65513,#65514,#65515,#65516,
#65517,#65518,#65519,#65520,#65521,#65522,#65523,#65524,#65525,#65526,#65527,
#65528,#65529,#65530,#65531,#65532,#65533,#65534,#65535,#65536,#65537,#65538,
#65539,#65540,#65541,#65542,#65543,#65544,#65545,#65546,#65547,#65548,#65549,
#65550,#65551,#65552,#65553,#65554,#65555,#65556,#65557,#65558,#65559,#65560,
#65561,#65562,#65563,#65564,#65565,#65566,#65567,#65568,#65569,#65570,#65571,
#65572,#65573,#65574,#65575,#65576,#65577,#65578,#65579,#65580,#65581,#65582,
#65583,#65584,#65585,#65586,#65587,#65588,#65589,#65590,#65591,#65592,#65593,
#65594,#65595,#65596,#65597,#65598,#65599,#65600,#65601,#65602,#65603,#65604,
#65605,#65606,#65607,#65608,#65609,#65610,#65611,#65612,#65613,#65614,#65615,
#65616,#65617,#65618,#65619,#65620,#65621,#65622,#65623,#65624,#65625,#65626,
#65627,#65628,#65629,#65630,#65631,#65632,#65633,#65634,#65635,#65636,#65637,
#65638,#65639,#65640,#65641,#65642,#65643,#65644,#65645,#65646,#65647,#65648,
#65649,#65650,#65651,#65652,#65653,#65654,#65655,#65656,#65657,#65658,#65659,
#65660,#65661,#65662,#65663,#65664,#65665,#65666,#65667,#65668,#65669,#65670,
#65671,#65672,#65673,#65674,#65675,#65676,#65677,#65678,#65679,#65680,#65681,
#65682,#65683,#65684,#65685,#65686,#65687,#65688,#65689,#65690,#65691,#65692,
#65693,#65694,#65695,#65696,#65697,#65698,#65699,#65700,#65701,#65702,#65703,
#65704,#65705,#65706,#65707,#65708,#65709,#65710,#65711,#65712,#65713,#65714,
#65715,#65716,#65717,#65718,#65719,#65720,#65721,#65722,#65723,#65724,#65725,
#65726,#65727,#65728,#65729,#65730,#65731,#65732,#65733,#65734,#65735,#65736,
#65737,#65738,#65739,#65740,#65741,#65742,#65743,#65744,#65745,#65746,#65747,
#65748,#65749,#65750,#65751,#65752,#65753,#65754,#65755,#65756,#65757,#65758,
#65759,#65760,#65761,#65762,#65763,#65764,#65765,#65766,#65767,#65768,#65769,
#65770,#65771,#65772,#65773,#65774,#65775,#65776,#65777,#65778,#65779,#65780),
 .UNSPECIFIED.,.F.,.F.,(4,2,2,2,2,2,2,2,2,2,2,2,2,2,2,2,2,2,2,2,2,2,2,2,
2,2,2,2,2,2,2,2,2,2,2,2,2,2,2,2,2,2,2,2,2,2,2,2,2,2,2,2,2,2,2,2,2,2,2,2,
2,2,2,2,2,2,2,2,2,2,2,2,2,2,2,2,2,2,2,2,2,2,2,2,2,2,2,2,2,2,2,2,2,2,2,2,
2,2,2,2,2,2,2,2,2,2,2,2,2,2,2,2,2,2,2,2,2,2,2,2,2,2,2,2,2,2,2,2,2,2,2,2,
2,2,2,2,2,2,2,2,2,2,2,2,2,2,2,2,2,2,2,2,2,2,2,2,2,2,2,2,2,2,2,2,2,2,2,2,
2,2,2,2,2,2,2,2,2,2,2,2,2,2,2,2,2,2,2,2,2,2,2,2,2,2,2,2,2,2,2,2,2,2,2,2,
2,2,2,2,2,2,2,2,2,2,2,2,2,2,2,2,2,2,2,2,2,2,2,2,2,2,2,2,2,2,2,2,2,2,2,2,
2,2,2,2,2,2,2,2,2,2,2,2,2,2,2,2,2,2,2,2,4),(0.00129694875898375,0.0515987783487616,
0.0579315983892281,0.0616524198632641,0.0642824509151131,0.0665642669079207,
0.06902096133795,0.0721554590749639,0.0787458653004138,0.122088816665559,
0.135624312393474,0.419309483428982,0.467087289833786,0.475499538648496,
0.47828207959715,0.480078715752738,0.48177095281888,0.483996630800586,0.488757152293363,
0.527324243030715,0.543455291756894,0.580091470747238,0.797912365366847,
0.832480790485467,0.84068344018513,0.845429713381083,0.849567859465754,
0.854522299330115,0.86063168974179,0.866818642413719,0.933367426055363,
1.10932387546117,1.18879389011366,1.2196159892368,1.22421561324367,1.22658034225675,
1.22846901887263,1.23063256464335,1.23430335327822,1.24684569812093,1.46976274739697,
1.5717945851285,1.59870120534138,1.60923697814188,1.61448838982076,1.61767515413441,
1.62057395423146,1.62279988449253,1.62495139618924,1.62795625907131,1.63581026363364,
1.75069202825208,1.84920466485693,1.87552331137487,1.88857500144065,1.91733393988185,
1.9655198522596,2.03240806601917,2.0415369838651,2.04387578268745,2.04525107884274,
2.04646094724078,2.04796604364869,2.05031572992552,2.06148132802729,2.24613624434292,
2.35466482236293,2.42901694218986,2.44162291014305,2.44542580400804,2.44737146881613,
2.44931055266987,2.45175387043991,2.45592747540602,2.47110364085791,2.71894787937801,
2.73413579870909,2.83618901756261,2.84020343702775,2.84195749611482,2.84325310596444,
2.84445254354133,2.84608429095225,2.84928829498566,2.87448314663903,2.93800781358238,
3.15507418905987,3.2511431764564,3.25787932320395,3.2610052890772,3.26337845468242,
3.26562273089915,3.26937390680572,3.27912503611581,3.42928768362734,3.48981763431179,
3.6463159186215,3.65765448635228,3.6613445657696,3.66371318086919,3.66593478039991,
3.6688440210216,3.67374804535977,3.70423679147491,3.86285245162621,4.08476887733537,
4.10468221723066,4.11350560432419,4.12010048011816,4.12628442744884,4.13485785792976,
4.15720585646341,4.30194658241091,4.41163765282002,4.42005267520845,4.42411855427103,
4.42709432328931,4.43029573416651,4.43489238534155,4.44774729924116,4.5733072328144,
4.66618010028589,4.69968711428439,4.72440064207762,4.73515063352563,4.74312685038242,
4.75058599550718,4.7609326441586,4.7885324870106,4.97721827607555,4.98067963655022,
5.1107245669645,5.17340772595675,5.17944812526741,5.18187943361519,5.1839011156992,
5.18597030530872,5.18898462424538,5.19690768784088,5.29996220794026,5.50840655023033,
5.58758229262072,5.59518866361993,5.59829357893385,5.60058716850642,5.60307587179233,
5.60646513034973,5.61423305217746,5.72284503146046,5.80458174649608,5.88149149179126,
5.91713517503595,6.0040878790867,6.00940097908021,6.01154258487026,6.01311486597951,
6.01481151911871,6.0171046920646,6.02228594373892,6.02928164544955,6.1016138812219,
6.24693603180575,6.35915855771817,6.37103000659625,6.37647034996805,6.38065811436151,
6.38516120859008,6.39227313203665,6.41382349175461,6.52782787471184,6.71825792041728,
6.75153948075885,6.75662970314421,6.75909376201621,6.7610100634925,6.76311919601022,
6.76654804963408,6.77831199810844,6.84891065978739,6.9837203477293,7.13845156329159,
7.14836426696517,7.15204709638925,7.15421376584802,7.15625173751565,7.15907136173104,
7.16464473052532,7.20505716797788,7.30445053985152,7.44232976452885,7.5296394986223,
7.57141511572248,7.57528590094398,7.57684344509663,7.57798557582895,7.57921663354673,
7.58088596097316,7.58477232875091,7.68037287778771,7.78937065932108,7.96235823536435,
7.97398041910527,7.97781532979575,7.97995324809147,7.98208768105778,7.98475244937398,
7.98991016706385,8.02335231528796,8.09963760622958,8.23268406182601,8.32823386277435,
8.33811375127778,8.36867050466958,8.37229806711554,8.3739645843572,8.3752503821478,
8.37663344774641,8.37881229585316,8.38567793656397,8.41013789679968,8.46132840621596,
8.5581824132107,8.77244015912746,8.78687343317552,8.79127425252589,8.79391170375441,
8.79602832318765,8.79887966576661,8.80425555941238,8.83509323790803,8.88933565530832,
8.94281250228456,8.95935889398822,9.07181835074182,9.17801279561369,9.18904020936745,
9.19282977290266,9.19498040273328,9.19695547304308,9.19961648847194,9.20245806619031,
9.2133467861147,9.25837098703045,9.3739494212201,9.42683033353842,9.61130835573613,
9.6340927971425,9.64272057285285,9.64891788810083,9.65550601687633,9.66194249681023,
9.6704050576395,9.68385587133202,9.82027766387798,9.87187651067165,9.90044361465627,
9.94465420549725,9.95177921239289,9.9555352402523,9.95748298040422,9.95770791712911),
 .UNSPECIFIED.);
#3459=B_SPLINE_CURVE_WITH_KNOTS('',3,(#65782,#65783,#65784,#65785,#65786,
#65787,#65788,#65789,#65790,#65791,#65792,#65793,#65794,#65795,#65796,#65797,
#65798,#65799,#65800,#65801,#65802,#65803,#65804,#65805,#65806,#65807,#65808,
#65809,#65810,#65811,#65812,#65813,#65814,#65815,#65816,#65817,#65818,#65819,
#65820,#65821,#65822,#65823,#65824,#65825,#65826,#65827,#65828,#65829,#65830,
#65831,#65832,#65833,#65834,#65835,#65836,#65837,#65838,#65839,#65840,#65841,
#65842,#65843,#65844,#65845,#65846,#65847,#65848,#65849,#65850,#65851,#65852,
#65853,#65854,#65855,#65856,#65857,#65858,#65859,#65860,#65861,#65862,#65863,
#65864,#65865,#65866,#65867,#65868,#65869,#65870,#65871,#65872,#65873,#65874,
#65875,#65876,#65877,#65878,#65879,#65880,#65881,#65882,#65883,#65884,#65885,
#65886,#65887,#65888,#65889,#65890,#65891,#65892,#65893,#65894,#65895,#65896,
#65897,#65898,#65899,#65900,#65901,#65902,#65903,#65904,#65905,#65906,#65907,
#65908,#65909,#65910,#65911,#65912,#65913,#65914,#65915,#65916,#65917,#65918,
#65919,#65920,#65921,#65922,#65923,#65924,#65925,#65926,#65927,#65928,#65929,
#65930,#65931,#65932,#65933,#65934,#65935,#65936,#65937,#65938,#65939,#65940,
#65941,#65942,#65943,#65944,#65945,#65946,#65947,#65948,#65949,#65950,#65951,
#65952,#65953,#65954,#65955,#65956,#65957,#65958,#65959,#65960,#65961,#65962,
#65963,#65964,#65965,#65966,#65967,#65968,#65969,#65970,#65971,#65972,#65973,
#65974,#65975,#65976,#65977,#65978,#65979,#65980,#65981,#65982,#65983,#65984,
#65985,#65986,#65987,#65988,#65989,#65990,#65991,#65992,#65993,#65994,#65995,
#65996,#65997,#65998,#65999,#66000,#66001,#66002,#66003,#66004,#66005,#66006,
#66007,#66008,#66009,#66010,#66011,#66012,#66013,#66014,#66015,#66016,#66017,
#66018,#66019,#66020,#66021,#66022,#66023,#66024,#66025,#66026,#66027,#66028,
#66029,#66030,#66031,#66032,#66033,#66034,#66035,#66036,#66037,#66038,#66039,
#66040,#66041,#66042,#66043,#66044,#66045,#66046,#66047,#66048,#66049,#66050,
#66051,#66052,#66053,#66054,#66055,#66056,#66057,#66058,#66059,#66060,#66061,
#66062,#66063,#66064,#66065,#66066,#66067,#66068,#66069,#66070,#66071,#66072,
#66073,#66074,#66075,#66076,#66077,#66078,#66079,#66080,#66081,#66082,#66083,
#66084,#66085,#66086,#66087,#66088,#66089,#66090,#66091,#66092,#66093,#66094,
#66095,#66096,#66097,#66098,#66099,#66100,#66101,#66102,#66103,#66104,#66105,
#66106,#66107,#66108,#66109,#66110,#66111,#66112,#66113,#66114,#66115,#66116,
#66117,#66118,#66119,#66120,#66121,#66122,#66123,#66124,#66125,#66126,#66127,
#66128,#66129,#66130,#66131,#66132,#66133,#66134,#66135,#66136,#66137,#66138,
#66139,#66140,#66141,#66142,#66143,#66144,#66145,#66146,#66147,#66148,#66149,
#66150,#66151,#66152,#66153,#66154,#66155,#66156,#66157,#66158,#66159,#66160,
#66161,#66162,#66163,#66164,#66165,#66166,#66167,#66168,#66169,#66170,#66171,
#66172,#66173,#66174,#66175,#66176,#66177,#66178,#66179,#66180,#66181,#66182,
#66183,#66184,#66185,#66186,#66187,#66188,#66189,#66190,#66191,#66192,#66193,
#66194,#66195,#66196,#66197,#66198,#66199,#66200,#66201,#66202,#66203,#66204,
#66205,#66206,#66207,#66208,#66209,#66210,#66211,#66212,#66213,#66214,#66215,
#66216,#66217,#66218,#66219,#66220,#66221,#66222,#66223,#66224,#66225,#66226,
#66227,#66228,#66229,#66230,#66231,#66232,#66233,#66234,#66235,#66236,#66237,
#66238,#66239,#66240,#66241,#66242,#66243,#66244,#66245,#66246,#66247,#66248,
#66249,#66250,#66251,#66252,#66253,#66254,#66255,#66256,#66257,#66258,#66259,
#66260,#66261,#66262,#66263,#66264,#66265,#66266,#66267,#66268,#66269,#66270,
#66271,#66272,#66273,#66274,#66275,#66276,#66277,#66278,#66279,#66280,#66281,
#66282,#66283,#66284,#66285,#66286,#66287,#66288,#66289,#66290,#66291,#66292,
#66293,#66294,#66295,#66296,#66297,#66298,#66299,#66300,#66301,#66302,#66303,
#66304,#66305,#66306,#66307,#66308,#66309,#66310,#66311,#66312,#66313,#66314,
#66315,#66316,#66317,#66318,#66319,#66320,#66321),.UNSPECIFIED.,.F.,.F.,
(4,2,2,2,2,2,2,2,2,2,2,2,2,2,2,2,2,2,2,2,2,2,2,2,2,2,2,2,2,2,2,2,2,2,2,
2,2,2,2,2,2,2,2,2,2,2,2,2,2,2,2,2,2,2,2,2,2,2,2,2,2,2,2,2,2,2,2,2,2,2,2,
2,2,2,2,2,2,2,2,2,2,2,2,2,2,2,2,2,2,2,2,2,2,2,2,2,2,2,2,2,2,2,2,2,2,2,2,
2,2,2,2,2,2,2,2,2,2,2,2,2,2,2,2,2,2,2,2,2,2,2,2,2,2,2,2,2,2,2,2,2,2,2,2,
2,2,2,2,2,2,2,2,2,2,2,2,2,2,2,2,2,2,2,2,2,2,2,2,2,2,2,2,2,2,2,2,2,2,2,2,
2,2,2,2,2,2,2,2,2,2,2,2,2,2,2,2,2,2,2,2,2,2,2,2,2,2,2,2,2,2,2,2,2,2,2,2,
2,2,2,2,2,2,2,2,2,2,2,2,2,2,2,2,2,2,2,2,2,2,2,2,2,2,2,2,2,2,2,2,2,2,2,2,
2,2,2,2,2,2,2,2,2,2,2,2,2,2,2,2,2,2,4),(0.00194775596412896,0.00381997872219618,
0.00768310839873159,0.0152484757587718,0.0559984597130718,0.083180397964233,
0.141603609062754,0.281568043709847,0.29577685967244,0.305133092997627,
0.312618786027551,0.320391004818619,0.329437010716093,0.344977543044769,
0.407171949186138,0.529569080338524,0.579467614844668,0.695020815505125,
0.740230438163307,0.752480834329959,0.755225656791899,0.757756982232155,
0.759556661349348,0.761443168043385,0.764587308141118,0.772705215194654,
0.885796374400152,0.969917370966717,1.00161701331527,1.04416239589059,1.12860012040994,
1.16571568962566,1.17152115347068,1.17453053933954,1.17673552024678,1.17910825215584,
1.18250918222216,1.19192178345028,1.34399640189478,1.42848146596589,1.52430228347539,
1.56299389590896,1.58214427882464,1.58558882104827,1.58724228565145,1.58893334181055,
1.59051637566891,1.5926977117734,1.59823863487681,1.6836106975509,1.81377528024418,
1.92300136312492,1.94319569010465,1.94972146505349,1.9542342937265,1.95842016276534,
1.96384391559773,1.97553274987955,2.05117404459852,2.22194126280525,2.29747577116899,
2.32769181091046,2.33218901226991,2.33411863593633,2.33606691666687,2.33785543178008,
2.34026602623827,2.34492827465109,2.38304561380264,2.41974028034598,2.59942787629786,
2.71757480409718,2.72498126293383,2.72814885545142,2.73045053862573,2.7325548441317,
2.73537802188319,2.74231579157247,2.80921358088104,2.91722042949577,3.03771079095769,
3.12007098529017,3.14801992030683,3.15119504291634,3.15274836805141,3.15385036369931,
3.15500301689251,3.15661151412765,3.16086680968392,3.22656406429102,3.35973468255457,
3.46249309797955,3.5454151264851,3.55155702939721,3.55441879343791,3.55659616339199,
3.55865874627818,3.56153955503214,3.56906973653488,3.68111098019845,3.83987741549927,
3.89185180635349,3.93909737868554,3.94654593663412,3.94875820402481,3.95014880256214,
3.95143219807736,3.95308261314174,3.95579493363375,3.97061709213312,3.99147548980586,
4.01311132036521,4.0314363943299,4.24606181980214,4.3147854850443,4.35973119812096,
4.36563284404626,4.36859396060057,4.37072452768334,4.37298070659806,4.37615437337573,
4.38271482110138,4.45180781814634,4.67161188739609,4.70366351306464,4.73293746859321,
4.76254526789673,4.76758936827972,4.77025653768783,4.77244480974129,4.7746503277811,
4.77870263311201,4.79178798398156,4.97941733784476,5.08440355178165,5.09870751297555,
5.10738059298268,5.1995394552947,5.21311272659763,5.22150838411226,5.22804364873175,
5.23527609689005,5.24720687966689,5.29198020096143,5.51096158864603,5.52507467095399,
5.530118782356,5.53321490079805,5.53657043262342,5.54113540912274,5.55162621470125,
5.5661978061242,5.60567934643691,5.73534619065898,5.77322221779091,5.82372000327675,
5.83827123717776,5.84702497697012,5.85412325364556,5.86385721463642,5.88317767562645,
5.98996236103159,6.13860502199146,6.22773382494581,6.26026109465342,6.26864373907125,
6.2733967734793,6.28495033187981,6.28857731880631,6.29056134964699,6.29253617205298,
6.29495207591698,6.29954719009276,6.3278445684736,6.36447658544003,6.45893918096176,
6.63025565699961,6.69555549605877,6.70220815601105,6.70546537293365,6.70779878414219,
6.71026337773395,6.71350502023791,6.72047244318536,6.81776823400833,7.04738324766324,
7.11233152381124,7.11694702084774,7.11919145614331,7.12079103842894,7.12230438649885,
7.12441235554195,7.12862919563622,7.16160320049922,7.218982078648,7.36493159850798,
7.46729602080416,7.47875177350771,7.48419284906929,7.48839436964865,7.49286504517853,
7.49982755574733,7.52029443859662,7.62485329577888,7.83262165904118,7.85997588552478,
7.86430148654411,7.8668506429846,7.86878635605074,7.87083924446749,7.87401434139503,
7.88358492332504,7.93326603624882,7.97165775914461,7.99957161640136,8.023535714671,
8.24217625139083,8.25331107998278,8.25820415262086,8.26115111904945,8.26342417841739,
8.2658198612451,8.26954627521727,8.27389293719544,8.28202080286569,8.30095743108379,
8.35247464759818,8.44872518972948,8.66898692388438,8.68169923691979,8.68419037221864,
8.68575037442937,8.68696628511317,8.68830698146203,8.69052277982283,8.69864324276123,
8.75366487971037,8.82837158704511,8.85176347544509,8.9335817840705,8.98575243765326,
9.07662665733073,9.08383235532049,9.08691089921585,9.0891018395348,9.09129764140298,
9.0944770329609,9.10242444577524,9.22764342296318,9.33205812888859,9.47041845508612,
9.47914048175318,9.48158031118098,9.48302198049232,9.48428241132744,9.48586262699845,
9.48894135533289,9.50945390329011,9.5585081271307,9.84612709053324,9.85915041061506,
9.89314019931766,9.89902757463239,9.90202626448096,9.90428597411546,9.90648287202888,
9.90902129607769,9.91262006122599,9.92614792889703,9.95856693167306),
 .UNSPECIFIED.);
#3460=B_SPLINE_CURVE_WITH_KNOTS('',3,(#66323,#66324,#66325,#66326,#66327,
#66328,#66329,#66330,#66331,#66332,#66333,#66334,#66335,#66336,#66337,#66338,
#66339,#66340,#66341,#66342,#66343,#66344,#66345,#66346,#66347,#66348,#66349,
#66350,#66351,#66352,#66353,#66354,#66355,#66356,#66357,#66358,#66359,#66360,
#66361,#66362,#66363,#66364,#66365,#66366,#66367,#66368,#66369,#66370,#66371,
#66372,#66373,#66374,#66375,#66376,#66377,#66378,#66379,#66380,#66381,#66382,
#66383,#66384,#66385,#66386,#66387,#66388,#66389,#66390,#66391,#66392,#66393,
#66394,#66395,#66396,#66397,#66398,#66399,#66400,#66401,#66402,#66403,#66404,
#66405,#66406,#66407,#66408,#66409,#66410,#66411,#66412,#66413,#66414,#66415,
#66416,#66417,#66418,#66419,#66420,#66421,#66422,#66423,#66424,#66425,#66426,
#66427,#66428,#66429,#66430,#66431,#66432,#66433,#66434,#66435,#66436,#66437,
#66438,#66439,#66440,#66441,#66442,#66443,#66444,#66445,#66446,#66447,#66448,
#66449,#66450,#66451,#66452,#66453,#66454,#66455,#66456,#66457,#66458,#66459,
#66460,#66461,#66462,#66463,#66464,#66465,#66466,#66467,#66468,#66469,#66470,
#66471,#66472,#66473,#66474,#66475,#66476,#66477,#66478,#66479,#66480,#66481,
#66482,#66483,#66484,#66485,#66486,#66487,#66488,#66489,#66490,#66491,#66492,
#66493,#66494,#66495,#66496,#66497,#66498,#66499,#66500,#66501,#66502,#66503,
#66504,#66505,#66506,#66507,#66508,#66509,#66510,#66511,#66512,#66513,#66514,
#66515,#66516,#66517,#66518,#66519,#66520,#66521,#66522,#66523,#66524,#66525,
#66526,#66527,#66528,#66529,#66530,#66531,#66532,#66533,#66534,#66535,#66536,
#66537,#66538,#66539,#66540,#66541,#66542,#66543,#66544,#66545,#66546,#66547,
#66548,#66549,#66550,#66551,#66552,#66553,#66554,#66555,#66556,#66557,#66558,
#66559,#66560,#66561,#66562,#66563,#66564,#66565,#66566,#66567,#66568,#66569,
#66570,#66571,#66572,#66573,#66574,#66575,#66576,#66577,#66578,#66579,#66580,
#66581,#66582,#66583,#66584,#66585,#66586,#66587,#66588,#66589,#66590,#66591,
#66592,#66593,#66594,#66595,#66596,#66597,#66598,#66599,#66600,#66601,#66602,
#66603,#66604,#66605,#66606,#66607,#66608,#66609,#66610,#66611,#66612,#66613,
#66614,#66615,#66616,#66617,#66618,#66619,#66620,#66621,#66622,#66623,#66624,
#66625,#66626,#66627,#66628,#66629,#66630,#66631,#66632,#66633,#66634,#66635,
#66636,#66637,#66638,#66639,#66640,#66641,#66642,#66643,#66644,#66645,#66646,
#66647,#66648,#66649,#66650,#66651,#66652,#66653,#66654,#66655,#66656,#66657,
#66658,#66659,#66660,#66661,#66662,#66663,#66664,#66665,#66666,#66667,#66668,
#66669,#66670,#66671,#66672,#66673,#66674,#66675,#66676,#66677,#66678,#66679,
#66680,#66681,#66682,#66683,#66684,#66685,#66686,#66687,#66688,#66689,#66690,
#66691,#66692,#66693,#66694,#66695,#66696,#66697,#66698,#66699,#66700,#66701,
#66702,#66703,#66704,#66705,#66706,#66707,#66708,#66709,#66710,#66711,#66712,
#66713,#66714,#66715,#66716,#66717,#66718,#66719,#66720,#66721,#66722,#66723,
#66724,#66725,#66726,#66727,#66728,#66729,#66730,#66731,#66732,#66733,#66734,
#66735,#66736,#66737,#66738,#66739,#66740,#66741,#66742,#66743,#66744,#66745,
#66746,#66747,#66748,#66749,#66750,#66751,#66752,#66753,#66754,#66755,#66756,
#66757,#66758,#66759,#66760,#66761,#66762,#66763,#66764,#66765,#66766,#66767,
#66768,#66769,#66770,#66771,#66772,#66773,#66774,#66775,#66776,#66777,#66778,
#66779,#66780,#66781,#66782,#66783,#66784,#66785,#66786,#66787,#66788,#66789,
#66790,#66791,#66792,#66793,#66794,#66795,#66796,#66797,#66798,#66799,#66800,
#66801,#66802,#66803,#66804,#66805,#66806,#66807,#66808,#66809,#66810),
 .UNSPECIFIED.,.F.,.F.,(4,2,2,2,2,2,2,2,2,2,2,2,2,2,2,2,2,2,2,2,2,2,2,2,
2,2,2,2,2,2,2,2,2,2,2,2,2,2,2,2,2,2,2,2,2,2,2,2,2,2,2,2,2,2,2,2,2,2,2,2,
2,2,2,2,2,2,2,2,2,2,2,2,2,2,2,2,2,2,2,2,2,2,2,2,2,2,2,2,2,2,2,2,2,2,2,2,
2,2,2,2,2,2,2,2,2,2,2,2,2,2,2,2,2,2,2,2,2,2,2,2,2,2,2,2,2,2,2,2,2,2,2,2,
2,2,2,2,2,2,2,2,2,2,2,2,2,2,2,2,2,2,2,2,2,2,2,2,2,2,2,2,2,2,2,2,2,2,2,2,
2,2,2,2,2,2,2,2,2,2,2,2,2,2,2,2,2,2,2,2,2,2,2,2,2,2,2,2,2,2,2,2,2,2,2,2,
2,2,2,2,2,2,2,2,2,2,2,2,2,2,2,2,2,2,2,2,2,2,2,2,2,2,2,2,2,2,2,2,2,2,2,2,
2,2,2,4),(0.00333856859840685,0.284619736140031,0.310732212505619,0.341204881842414,
0.346286074758269,0.348961341292532,0.35115035079119,0.353351624430859,
0.357381848054998,0.370283360509686,0.512242771930392,0.683425176397613,
0.749100293442828,0.785617124075771,0.79668300737984,0.80372500210769,0.810321021216165,
0.818984859491134,0.825984092719778,0.865776294586179,1.08085965254399,
1.10271545327627,1.10833625502156,1.11189108252888,1.1152290492436,1.11961050853901,
1.12704189247446,1.18023216579261,1.35307036406388,1.38639369448937,1.41100405587999,
1.4217388175445,1.42971493079168,1.43718205057407,1.44755276556001,1.47515165607487,
1.67948408578306,1.79852651386993,1.83136480105587,1.86222139423072,1.86694345415087,
1.86938619252466,1.8713630694055,1.87333105338895,1.87688363769478,1.88780266618339,
2.03694253426517,2.16095073339868,2.24137431025706,2.26508824706165,2.27488746806926,
2.27997815779486,2.28318195949117,2.28614816543039,2.2885408080166,2.29130406454485,
2.29597554833943,2.31181169559806,2.61170011913439,2.6851685037231,2.69213542189016,
2.69740394062439,2.69971397595816,2.70141454983806,2.70298527420405,2.70511697552099,
2.70929076824488,2.74255834148684,2.87103138381762,3.04798852341164,3.05944545251147,
3.0648689488328,3.06904319378483,3.07304054716738,3.07870534618662,3.09046052495392,
3.21877077397897,3.35103580108738,3.41337285182702,3.44089056485544,3.44536334059358,
3.44770222782123,3.44960742422265,3.45179781827585,3.45548919106622,3.46860345086369,
3.64384199356018,3.81612051207427,3.83544714712346,3.83998455119368,3.84258343474566,
3.84460295376569,3.84724512380881,3.85185183240807,3.86984005514159,4.17674663343024,
4.25415149167353,4.2638868468881,4.26627857461073,4.26766642587972,4.26887617021122,
4.2703663933379,4.2726647070277,4.28315059430245,4.55456821585407,4.62928199678382,
4.66235120995652,4.66749733141106,4.67016081181622,4.67231630492058,4.67446258483323,
4.67833406637735,4.69022042633393,4.8671963040303,4.98727923519819,5.05859126307058,
5.06298012073654,5.06466216323046,5.06587504661516,5.0670342207453,5.06866750234386,
5.07200369103419,5.10127021238341,5.15237678373598,5.35326114791585,5.3983550956444,
5.47326243165098,5.48057622775057,5.48356452748619,5.48577296813408,5.4881702066483,
5.49143642960815,5.49892867814273,5.60436596498282,5.72688748951995,5.79064270534328,
5.87616617309477,5.88257971302819,5.88526968560489,5.88751078940089,5.88980663318107,
5.89315489002436,5.90198356407408,5.98747286290205,6.01574022020838,6.17140226368766,
6.23802872166707,6.2503559436341,6.31802460874426,6.33147353202305,6.33911584738048,
6.34554632366637,6.35333683076929,6.36783824853846,6.46141493080208,6.60214365347692,
6.63758686100609,6.64433441644536,6.64814482084694,6.65110085585758,6.65496447424074,
6.66189558421183,6.69560024833733,6.81312269773593,6.93439429375189,6.95019043201198,
6.96015467745225,6.96802870233841,6.97688932558825,6.99166439646711,7.04598141917512,
7.33646679683559,7.39788775490939,7.40391009743869,7.40633950346372,7.40836173379855,
7.41043366147188,7.41339564760077,7.42081395056037,7.52420116356839,7.62398292530944,
7.80645168097928,7.81830261827922,7.82246364043866,7.82484848851303,7.82705216266016,
7.83004067306684,7.83574154049665,7.87026241515591,7.94416352615619,8.13977662323811,
8.22841912104313,8.23436510486817,8.23661351353941,8.23821490069092,8.23972911876566,
8.24134958719679,8.24477750829023,8.26009300085787,8.2893354057991,8.36616526888381,
8.46784621397586,8.58455991286838,8.59651042472393,8.60196840379477,8.60616201397605,
8.61066380508279,8.61775762638676,8.63870261223748,8.72665519044293,8.87099790860996,
8.97540086341416,8.98162602183915,8.98410235528951,8.98590863520523,8.9878468999123,
8.98974446616838,8.99420011229206,9.02232103652388,9.05965205989318,9.11787644591066,
9.30409301029584,9.36882371713917,9.37508255233326,9.37811694411651,9.3802770610686,
9.38231928321416,9.38516132935038,9.39083889647657,9.43460552604944,9.50183645866207,
9.57765477149944,9.61032738298099,9.62679606690743,9.64550862587289,9.79058827780798,
9.80001130044398,9.80246697509114,9.80388342991624,9.80507944683785,9.80652777305202,
9.80925051369668,9.82486059692485,9.96649908929926),.UNSPECIFIED.);
#3461=B_SPLINE_CURVE_WITH_KNOTS('',3,(#66812,#66813,#66814,#66815,#66816,
#66817,#66818,#66819,#66820,#66821,#66822,#66823,#66824,#66825,#66826,#66827,
#66828,#66829,#66830,#66831,#66832,#66833,#66834,#66835,#66836,#66837,#66838,
#66839,#66840,#66841,#66842,#66843,#66844,#66845,#66846,#66847,#66848,#66849,
#66850,#66851,#66852,#66853,#66854,#66855,#66856,#66857,#66858,#66859,#66860,
#66861,#66862,#66863,#66864,#66865,#66866,#66867,#66868,#66869,#66870,#66871,
#66872,#66873,#66874,#66875,#66876,#66877,#66878,#66879,#66880,#66881,#66882,
#66883,#66884,#66885,#66886,#66887,#66888,#66889,#66890,#66891,#66892,#66893,
#66894,#66895,#66896,#66897,#66898,#66899,#66900,#66901,#66902,#66903,#66904,
#66905,#66906,#66907,#66908,#66909,#66910,#66911,#66912,#66913,#66914,#66915,
#66916,#66917,#66918,#66919,#66920,#66921,#66922,#66923,#66924,#66925,#66926,
#66927,#66928,#66929,#66930,#66931,#66932,#66933,#66934,#66935,#66936,#66937,
#66938,#66939,#66940,#66941,#66942,#66943,#66944,#66945,#66946,#66947,#66948,
#66949,#66950,#66951,#66952,#66953,#66954,#66955,#66956,#66957,#66958,#66959,
#66960,#66961,#66962,#66963,#66964,#66965,#66966,#66967,#66968,#66969,#66970,
#66971,#66972,#66973,#66974,#66975,#66976,#66977,#66978,#66979,#66980,#66981,
#66982,#66983,#66984,#66985,#66986,#66987,#66988,#66989,#66990,#66991,#66992,
#66993,#66994,#66995,#66996,#66997,#66998,#66999,#67000,#67001,#67002,#67003,
#67004,#67005,#67006,#67007,#67008,#67009,#67010,#67011,#67012,#67013,#67014,
#67015,#67016,#67017,#67018,#67019,#67020,#67021,#67022,#67023,#67024,#67025,
#67026,#67027,#67028,#67029,#67030,#67031,#67032,#67033,#67034,#67035,#67036,
#67037,#67038,#67039,#67040,#67041,#67042,#67043,#67044,#67045,#67046,#67047,
#67048,#67049,#67050,#67051,#67052,#67053,#67054,#67055,#67056,#67057,#67058,
#67059,#67060,#67061,#67062,#67063,#67064,#67065,#67066,#67067,#67068,#67069,
#67070),.UNSPECIFIED.,.F.,.F.,(4,3,3,3,3,3,3,3,3,3,3,3,3,3,3,3,3,3,3,3,
3,3,3,3,3,3,3,3,3,3,3,3,3,3,3,3,3,3,3,3,3,3,3,3,3,3,3,3,3,3,3,3,3,3,3,3,
3,3,3,3,3,3,3,3,3,3,3,3,3,3,3,3,3,3,3,3,3,3,3,3,3,3,3,3,3,3,4),(107.937798928197,
108.009679787755,108.081504421882,108.153288071956,108.225642008513,108.297402811625,
108.3691705556,108.440958965509,108.513749115235,108.585656546406,108.658888055409,
108.732119564413,108.807656197669,108.883106955815,108.958484731036,109.033802367837,
109.109072671081,109.186646330413,109.261866024691,109.337079840601,109.412299324809,
109.487536024993,109.562828554874,109.63815429051,109.713550508267,109.729661945738,
109.806260687544,109.882794377386,109.959272693195,110.035696829543,110.112088235741,
110.188455820887,110.228433136401,110.306554286418,110.384720352047,110.462936067119,
110.541242529328,110.619597186618,110.698037121605,110.727204327063,110.809173128142,
110.891070140534,110.974796484832,111.056453358329,111.141214438028,111.225975517726,
111.299602542256,111.373224315984,111.44685382182,111.520535490071,111.594244423666,
111.668035004164,111.724746708388,111.801252015151,111.877701493684,111.954106042787,
112.03047652894,112.106823793623,112.183756955634,112.260103916869,112.336461183379,
112.412838607712,112.490201228212,112.566677800309,112.644483445011,112.722289089713,
112.796982177518,112.871595457739,112.946141313354,113.02062162159,113.095063696886,
113.169480525979,113.221060280375,113.301354296142,113.381792915329,113.466302554256,
113.547077099462,113.627952583241,113.708962628932,113.719831471038,113.796253877641,
113.872580080563,113.948820155796,114.024960507632,114.101042441477,114.177062345978,
114.220984235377),.UNSPECIFIED.);
#3462=B_SPLINE_CURVE_WITH_KNOTS('',3,(#67072,#67073,#67074,#67075,#67076,
#67077,#67078,#67079,#67080,#67081,#67082,#67083,#67084,#67085,#67086,#67087,
#67088,#67089,#67090,#67091,#67092,#67093,#67094,#67095,#67096,#67097,#67098,
#67099,#67100,#67101,#67102,#67103,#67104,#67105,#67106,#67107,#67108,#67109,
#67110,#67111,#67112,#67113,#67114,#67115,#67116,#67117,#67118,#67119,#67120,
#67121,#67122,#67123,#67124,#67125,#67126,#67127,#67128,#67129,#67130,#67131,
#67132,#67133,#67134,#67135,#67136,#67137,#67138,#67139,#67140,#67141,#67142,
#67143,#67144,#67145,#67146,#67147,#67148,#67149,#67150,#67151,#67152,#67153,
#67154,#67155,#67156,#67157,#67158,#67159,#67160,#67161,#67162,#67163,#67164,
#67165,#67166,#67167,#67168,#67169,#67170,#67171,#67172,#67173,#67174,#67175,
#67176,#67177,#67178,#67179,#67180,#67181,#67182,#67183,#67184,#67185,#67186,
#67187,#67188,#67189,#67190,#67191,#67192,#67193,#67194,#67195,#67196,#67197,
#67198,#67199,#67200,#67201,#67202,#67203,#67204,#67205,#67206,#67207,#67208,
#67209,#67210,#67211,#67212,#67213,#67214,#67215,#67216,#67217,#67218,#67219,
#67220,#67221,#67222,#67223,#67224,#67225,#67226,#67227,#67228,#67229,#67230,
#67231,#67232,#67233,#67234,#67235,#67236,#67237,#67238,#67239,#67240,#67241,
#67242,#67243,#67244,#67245,#67246,#67247,#67248,#67249,#67250,#67251,#67252,
#67253,#67254,#67255,#67256,#67257,#67258,#67259,#67260,#67261,#67262,#67263,
#67264,#67265,#67266,#67267,#67268,#67269,#67270,#67271,#67272,#67273,#67274,
#67275,#67276,#67277,#67278,#67279,#67280,#67281,#67282,#67283,#67284,#67285,
#67286,#67287,#67288,#67289,#67290,#67291,#67292,#67293,#67294,#67295,#67296,
#67297,#67298,#67299,#67300,#67301,#67302,#67303,#67304,#67305,#67306,#67307,
#67308,#67309,#67310,#67311,#67312,#67313,#67314,#67315,#67316,#67317,#67318,
#67319,#67320,#67321,#67322,#67323,#67324,#67325,#67326,#67327,#67328,#67329,
#67330,#67331,#67332,#67333,#67334,#67335,#67336,#67337,#67338,#67339,#67340,
#67341,#67342,#67343,#67344,#67345,#67346,#67347,#67348,#67349,#67350,#67351,
#67352,#67353,#67354,#67355,#67356,#67357,#67358,#67359,#67360,#67361,#67362,
#67363,#67364,#67365,#67366,#67367,#67368,#67369,#67370,#67371,#67372,#67373,
#67374,#67375,#67376,#67377,#67378,#67379,#67380,#67381,#67382,#67383,#67384,
#67385,#67386,#67387,#67388,#67389,#67390,#67391,#67392,#67393,#67394,#67395,
#67396,#67397,#67398,#67399,#67400,#67401,#67402,#67403,#67404,#67405,#67406,
#67407,#67408,#67409,#67410,#67411,#67412,#67413,#67414,#67415,#67416,#67417,
#67418,#67419,#67420,#67421,#67422,#67423,#67424,#67425,#67426,#67427,#67428,
#67429,#67430,#67431,#67432,#67433,#67434,#67435,#67436,#67437,#67438,#67439,
#67440,#67441,#67442,#67443,#67444,#67445,#67446,#67447,#67448,#67449,#67450,
#67451,#67452,#67453,#67454,#67455,#67456,#67457,#67458,#67459,#67460,#67461,
#67462,#67463,#67464,#67465,#67466,#67467,#67468,#67469,#67470,#67471,#67472,
#67473,#67474,#67475,#67476,#67477,#67478,#67479,#67480,#67481,#67482,#67483,
#67484,#67485,#67486,#67487,#67488,#67489,#67490,#67491,#67492,#67493,#67494,
#67495,#67496,#67497,#67498,#67499,#67500,#67501,#67502,#67503,#67504,#67505,
#67506,#67507,#67508,#67509,#67510,#67511,#67512,#67513,#67514,#67515,#67516,
#67517,#67518,#67519,#67520,#67521,#67522,#67523,#67524,#67525,#67526,#67527,
#67528,#67529,#67530,#67531,#67532,#67533,#67534,#67535,#67536,#67537,#67538,
#67539,#67540,#67541,#67542,#67543,#67544,#67545,#67546,#67547,#67548,#67549,
#67550,#67551,#67552,#67553,#67554,#67555,#67556,#67557,#67558,#67559,#67560,
#67561,#67562,#67563),.UNSPECIFIED.,.F.,.F.,(4,2,2,2,2,2,2,2,2,2,2,2,2,
2,2,2,2,2,2,2,2,2,2,2,2,2,2,2,2,2,2,2,2,2,2,2,2,2,2,2,2,2,2,2,2,2,2,2,2,
2,2,2,2,2,2,2,2,2,2,2,2,2,2,2,2,2,2,2,2,2,2,2,2,2,2,2,2,2,2,2,2,2,2,2,2,
2,2,2,2,2,2,2,2,2,2,2,2,2,2,2,2,2,2,2,2,2,2,2,2,2,2,2,2,2,2,2,2,2,2,2,2,
2,2,2,2,2,2,2,2,2,2,2,2,2,2,2,2,2,2,2,2,2,2,2,2,2,2,2,2,2,2,2,2,2,2,2,2,
2,2,2,2,2,2,2,2,2,2,2,2,2,2,2,2,2,2,2,2,2,2,2,2,2,2,2,2,2,2,2,2,2,2,2,2,
2,2,2,2,2,2,2,2,2,2,2,2,2,2,2,2,2,2,2,2,2,2,2,2,2,2,2,2,2,2,2,2,2,2,2,2,
2,2,2,2,2,2,2,2,2,2,2,2,2,2,2,2,4),(0.00221101600796123,0.294940398990252,
0.344446393877704,0.383713958302492,0.390388737160091,0.392478778912742,
0.393798481889886,0.395020523282386,0.396602589473208,0.400096748693395,
0.428212751745557,0.558443357703154,0.678838207198895,0.783864754714538,
0.791453851911416,0.794574481125808,0.796599252041966,0.798775830731035,
0.801784919286611,0.808617074886337,0.882021864342784,0.950925230679804,
1.0517887987793,1.12987466538263,1.16809382664115,1.18582837742638,1.18870535529707,
1.19024209072519,1.19151147048997,1.19299046703209,1.19553015478069,1.20502108451035,
1.35604567688508,1.47998851801677,1.59760089107955,1.60521262038921,1.6084591886792,
1.61081990271752,1.61324032340629,1.61675119965368,1.62549257913985,1.76785871840477,
1.80078696537217,1.93577640908127,1.95952292585593,1.99759645681226,2.0062113202344,
2.00952694931874,2.01181563835611,2.01406190966798,2.01677594282218,2.02358659409667,
2.12850798601709,2.31861792216491,2.4391981145353,2.45474597810964,2.4627457942354,
2.46861951779537,2.47497550524169,2.4861344979523,2.51943074366916,2.73550553999271,
2.76353848718953,2.76959744638468,2.7732379386688,2.77654758082057,2.78081128979848,
2.78938072039188,2.86515069833341,2.99667471176583,3.06311730216262,3.07828158112576,
3.08716924191958,3.09503657908561,3.10495378619902,3.12071667741521,3.19287518759524,
3.44174246135284,3.49916223168841,3.5243970082556,3.52887999288524,3.53127232918688,
3.53305444193548,3.53528458424103,3.5390279186813,3.55148773864436,3.74367116865347,
3.85336807352492,3.91070505463629,3.93985038186923,3.9452920764229,3.94822467964108,
3.95042189818842,3.95318634924189,3.95786303100498,3.97374424946594,4.25075597417871,
4.35427050102661,4.35924338475827,4.36149920472045,4.36319044892995,4.36477468754753,
4.36695930353944,4.37251713184819,4.46017886987819,4.62492753594253,4.70236122872631,
4.71885994582954,4.72514128982581,4.72946807664061,4.73371359696599,4.73884877938826,
4.75166215720126,4.86467176742369,4.98305744504084,5.09485534761672,5.10451083367231,
5.10781619649007,5.10969073617289,5.11141045676678,5.11372401383544,5.11807811931325,
5.14294296563946,5.19905483631281,5.48389491152695,5.49585394677549,5.50062479700732,
5.50353543078471,5.50580300485759,5.50826448152365,5.5121908905702,5.52498314030815,
5.59893517270499,5.69757744690188,5.73787252713119,5.78212631037049,5.91561031599514,
5.92436788662219,5.92675616407122,5.92815648855939,5.92936409857323,5.93083496231428,
5.93366960720381,5.95187877210987,5.99377298573601,6.07958134449031,6.30933179438556,
6.32398282391089,6.32813507540859,6.3306055775919,6.33275858892246,6.33540675386594,
6.34048526669121,6.371955238811,6.44096127894161,6.5927106648339,6.71383373125756,
6.72160737267125,6.72394614543367,6.7252229402186,6.72649269597564,6.72804281514845,
6.73097927321507,6.74808150382576,6.78295419663718,6.84590352592249,7.05338004988117,
7.1324732241771,7.13988374260119,7.14288771553855,7.14509909415957,7.14749120277648,
7.15073565953597,7.15811415054995,7.25317940958819,7.5025354972263,7.53701136411819,
7.54264958725048,7.5454397677846,7.54755367352287,7.54992771626458,7.55372092425274,
7.55823942865708,7.56698663785587,7.65953860524462,7.82434624940749,7.93837725460838,
7.98038543844159,7.99238532626743,7.99963089933533,8.00551211502852,8.01355308937777,
8.02927349612929,8.04909715424871,8.09413513402357,8.18843500399108,8.22087459838905,
8.29505457010402,8.30282917325925,8.30676644446013,8.30988010404849,8.3135831303279,
8.31978998723772,8.34347473921566,8.38796827401687,8.57107521672241,8.60351769231569,
8.61582974758375,8.62327259492484,8.63125651718348,8.64205364243587,8.66731000722095,
8.75149090683794,8.84003632168467,9.02337590966357,9.0574898588092,9.06272989561353,
9.06527804985395,9.06726536338363,9.06941474496714,9.07282111865078,9.07683786077177,
9.0844296487899,9.10213787841623,9.13612606465791,9.19367068112901,9.45960045680476,
9.47570733634246,9.48040835006537,9.48317750583963,9.4855938413921,9.4886175874711,
9.49449327621657,9.53346434620623,9.62942854047248,9.83601851302572,9.8455306909787,
9.88858657029123,9.89328305854664,9.89546207937708,9.89714650969329,9.89870992134584,
9.90049714337201,9.90301477184182,9.9072952669435,9.96134643791026),
 .UNSPECIFIED.);
#3463=B_SPLINE_CURVE_WITH_KNOTS('',3,(#67565,#67566,#67567,#67568,#67569,
#67570,#67571,#67572,#67573,#67574,#67575,#67576,#67577,#67578,#67579,#67580,
#67581,#67582,#67583,#67584,#67585,#67586,#67587,#67588,#67589,#67590,#67591,
#67592,#67593,#67594,#67595,#67596,#67597,#67598,#67599,#67600,#67601,#67602,
#67603,#67604,#67605,#67606,#67607,#67608,#67609,#67610,#67611,#67612,#67613,
#67614,#67615,#67616,#67617,#67618,#67619,#67620,#67621,#67622,#67623,#67624,
#67625,#67626,#67627,#67628,#67629,#67630,#67631,#67632,#67633,#67634,#67635,
#67636,#67637,#67638,#67639,#67640,#67641,#67642,#67643,#67644,#67645,#67646,
#67647,#67648,#67649,#67650,#67651,#67652,#67653,#67654,#67655,#67656,#67657,
#67658,#67659,#67660,#67661,#67662,#67663,#67664,#67665,#67666,#67667,#67668,
#67669,#67670,#67671,#67672,#67673,#67674,#67675,#67676,#67677,#67678,#67679,
#67680,#67681,#67682,#67683,#67684,#67685,#67686,#67687,#67688,#67689,#67690,
#67691,#67692,#67693,#67694,#67695,#67696,#67697,#67698,#67699,#67700,#67701,
#67702,#67703,#67704,#67705,#67706,#67707,#67708,#67709,#67710,#67711,#67712,
#67713,#67714,#67715,#67716,#67717,#67718,#67719,#67720,#67721,#67722,#67723,
#67724,#67725,#67726,#67727,#67728,#67729,#67730,#67731,#67732,#67733,#67734,
#67735,#67736,#67737,#67738,#67739,#67740,#67741,#67742,#67743,#67744,#67745,
#67746,#67747,#67748,#67749,#67750,#67751,#67752,#67753,#67754,#67755,#67756,
#67757,#67758,#67759,#67760,#67761,#67762,#67763,#67764,#67765,#67766,#67767,
#67768,#67769,#67770,#67771,#67772,#67773,#67774,#67775,#67776,#67777,#67778,
#67779,#67780,#67781,#67782,#67783,#67784,#67785,#67786,#67787,#67788,#67789,
#67790,#67791,#67792,#67793,#67794,#67795,#67796,#67797,#67798,#67799,#67800,
#67801,#67802,#67803,#67804,#67805,#67806,#67807,#67808,#67809,#67810,#67811,
#67812,#67813,#67814,#67815,#67816,#67817,#67818,#67819,#67820,#67821,#67822,
#67823,#67824,#67825,#67826),.UNSPECIFIED.,.F.,.F.,(4,3,3,3,3,3,3,3,3,3,
3,3,3,3,3,3,3,3,3,3,3,3,3,3,3,3,3,3,3,3,3,3,3,3,3,3,3,3,3,3,3,3,3,3,3,3,
3,3,3,3,3,3,3,3,3,3,3,3,3,3,3,3,3,3,3,3,3,3,3,3,3,3,3,3,3,3,3,3,3,3,3,3,
3,3,3,3,3,4),(126.787354849736,126.859442342501,126.931470599143,127.003449731494,
127.075400049158,127.147341795895,127.186653618924,127.26694763469,127.347386253876,
127.431895892803,127.512670438008,127.593545921785,127.674555967475,127.685424809586,
127.759965614158,127.834430435794,127.90883316579,127.983187654446,128.05750771988,
128.135690153759,128.209997942834,128.284315420204,128.358655073321,128.433029398995,
128.507489428851,128.581999257075,128.656609530046,128.682967190911,128.756120282925,
128.829185532227,128.902177863279,128.975112131816,129.048003140213,129.120865651371,
129.193728264913,129.266594650327,129.339478150665,129.412392120165,129.48539285565,
129.558441055326,129.631600226992,129.680509572236,129.756046205493,129.831496963639,
129.90687473886,129.98219237566,130.057462678904,130.135036338236,130.210256032515,
130.285469848424,130.360689332632,130.435926032816,130.511218562696,130.586544298332,
130.661940516089,130.678051953561,130.754650695366,130.831184385207,130.907662701015,
130.984086837362,131.060478243558,131.136845828703,131.176823144223,131.254944294241,
131.333110359872,131.411326074945,131.489632537157,131.567987194449,131.646427129437,
131.675594334886,131.757563135962,131.839460148351,131.923186492651,132.004843366145,
132.089604445847,132.174365525548,132.247992550079,132.321614323809,132.395243829646,
132.468925497898,132.542634431494,132.616425011994,132.673136716211,132.758107903129,
132.842895618683,132.927528471115,133.011843765426,133.070540156915),
 .UNSPECIFIED.);
#3464=B_SPLINE_CURVE_WITH_KNOTS('',3,(#67828,#67829,#67830,#67831,#67832,
#67833,#67834,#67835,#67836,#67837,#67838,#67839,#67840,#67841,#67842,#67843,
#67844,#67845),.UNSPECIFIED.,.F.,.F.,(4,2,2,2,2,2,2,2,4),(133.070540156915,
133.90545706881,134.740373980705,135.5752908926,136.410207804495,137.24512471639,
138.080041628285,138.914958540179,139.353725464095),.UNSPECIFIED.);
#3465=B_SPLINE_CURVE_WITH_KNOTS('',3,(#67847,#67848,#67849,#67850,#67851,
#67852,#67853,#67854,#67855,#67856,#67857,#67858),.UNSPECIFIED.,.F.,.F.,
(4,1,1,1,1,1,1,1,1,4),(139.353725464095,139.655933385485,140.65347576681,
141.152246957472,141.651018148135,142.64856052946,143.646102910785,144.643645292109,
145.142416482772,145.636910654589),.UNSPECIFIED.);
#3466=B_SPLINE_CURVE_WITH_KNOTS('',3,(#67860,#67861,#67862,#67863,#67864,
#67865,#67866,#67867,#67868,#67869,#67870,#67871,#67872,#67873,#67874,#67875,
#67876,#67877,#67878,#67879,#67880,#67881,#67882,#67883,#67884,#67885,#67886,
#67887,#67888,#67889,#67890,#67891,#67892,#67893,#67894,#67895,#67896,#67897,
#67898,#67899,#67900,#67901,#67902,#67903,#67904,#67905,#67906,#67907,#67908,
#67909,#67910,#67911,#67912,#67913,#67914,#67915,#67916,#67917,#67918,#67919,
#67920,#67921,#67922,#67923,#67924,#67925,#67926,#67927,#67928,#67929,#67930,
#67931,#67932,#67933,#67934,#67935,#67936,#67937,#67938,#67939,#67940,#67941,
#67942,#67943,#67944,#67945,#67946,#67947,#67948,#67949,#67950,#67951,#67952,
#67953,#67954,#67955,#67956,#67957,#67958,#67959,#67960,#67961,#67962,#67963,
#67964,#67965,#67966,#67967,#67968,#67969,#67970,#67971,#67972,#67973,#67974,
#67975,#67976,#67977,#67978,#67979,#67980,#67981,#67982,#67983,#67984,#67985,
#67986,#67987,#67988,#67989,#67990,#67991,#67992,#67993,#67994,#67995,#67996,
#67997,#67998,#67999,#68000,#68001,#68002,#68003,#68004,#68005,#68006,#68007,
#68008,#68009,#68010,#68011,#68012,#68013,#68014,#68015,#68016,#68017,#68018,
#68019,#68020,#68021,#68022,#68023,#68024,#68025,#68026,#68027,#68028,#68029,
#68030,#68031,#68032,#68033,#68034,#68035,#68036,#68037,#68038,#68039,#68040,
#68041,#68042,#68043,#68044,#68045,#68046,#68047,#68048,#68049,#68050,#68051,
#68052,#68053,#68054,#68055,#68056,#68057,#68058,#68059,#68060,#68061,#68062,
#68063,#68064,#68065,#68066,#68067,#68068,#68069,#68070,#68071,#68072,#68073,
#68074,#68075,#68076,#68077,#68078,#68079,#68080,#68081,#68082,#68083,#68084,
#68085,#68086,#68087,#68088,#68089,#68090,#68091,#68092,#68093,#68094,#68095,
#68096,#68097,#68098,#68099,#68100,#68101,#68102,#68103,#68104,#68105,#68106,
#68107,#68108,#68109,#68110,#68111,#68112,#68113,#68114,#68115,#68116,#68117,
#68118,#68119,#68120,#68121),.UNSPECIFIED.,.F.,.F.,(4,3,3,3,3,3,3,3,3,3,
3,3,3,3,3,3,3,3,3,3,3,3,3,3,3,3,3,3,3,3,3,3,3,3,3,3,3,3,3,3,3,3,3,3,3,3,
3,3,3,3,3,3,3,3,3,3,3,3,3,3,3,3,3,3,3,3,3,3,3,3,3,3,3,3,3,3,3,3,3,3,3,3,
3,3,3,3,3,4),(145.636910771275,145.641187673434,145.723156474513,145.805053486906,
145.888779831204,145.970436704702,146.0551977844,146.139958864097,146.213585888627,
146.287207662355,146.36083716819,146.434518836441,146.508227770035,146.582018350533,
146.638730054759,146.715235361522,146.791684840055,146.868089389159,146.944459875312,
147.020807139994,147.097740302005,147.17408726324,147.25044452975,147.326821954083,
147.404184574583,147.480661146681,147.558466791382,147.636272436084,147.71096552389,
147.785578804112,147.860124659728,147.934604967965,148.009047043262,148.083463872356,
148.135043626747,148.215337642513,148.295776261699,148.380285900626,148.46106044583,
148.541935929607,148.622945975298,148.633814817409,148.708355621981,148.782820443617,
148.857223173613,148.931577662269,149.005897727703,149.084080161582,149.158387950657,
149.232705428027,149.307045081143,149.381419406818,149.455879436673,149.530389264898,
149.604999537868,149.631357198734,149.704510290748,149.77757554005,149.850567871102,
149.923502139639,149.996393148036,150.069255659195,150.142118272736,150.21498465815,
150.287868158489,150.360782127988,150.433782863474,150.506831063149,150.579990234816,
150.628899580059,150.704436213315,150.779886971462,150.855264746683,150.930582383483,
151.005852686728,151.08342634606,151.158646040338,151.233859856247,151.309079340455,
151.384316040639,151.45960857052,151.534934306156,151.610330523913,151.626441961384,
151.708619166871,151.790681921113,151.872549033798,151.920096078454),
 .UNSPECIFIED.);
#3467=B_SPLINE_CURVE_WITH_KNOTS('',3,(#68123,#68124,#68125,#68126,#68127,
#68128,#68129,#68130,#68131,#68132,#68133,#68134,#68135),.UNSPECIFIED.,
 .F.,.F.,(4,1,1,1,1,1,1,1,1,1,4),(151.920097103546,152.125213152046,152.623984342709,
153.122755533371,153.621526724033,154.619069105358,155.117840296021,155.616611486683,
156.614153868008,157.611696249333,158.203281385634),.UNSPECIFIED.);
#3468=B_SPLINE_CURVE_WITH_KNOTS('',3,(#68137,#68138,#68139,#68140,#68141,
#68142,#68143,#68144,#68145,#68146,#68147,#68148,#68149,#68150,#68151,#68152,
#68153,#68154,#68155,#68156,#68157,#68158,#68159,#68160,#68161,#68162,#68163,
#68164,#68165,#68166,#68167,#68168,#68169,#68170,#68171,#68172,#68173,#68174,
#68175,#68176,#68177,#68178,#68179,#68180,#68181,#68182,#68183,#68184,#68185,
#68186,#68187,#68188,#68189,#68190,#68191,#68192,#68193,#68194,#68195,#68196,
#68197,#68198,#68199,#68200,#68201,#68202,#68203,#68204,#68205,#68206,#68207,
#68208,#68209,#68210,#68211,#68212,#68213,#68214,#68215,#68216,#68217,#68218,
#68219,#68220,#68221,#68222,#68223,#68224,#68225,#68226,#68227,#68228,#68229,
#68230,#68231,#68232,#68233,#68234,#68235,#68236,#68237,#68238,#68239,#68240,
#68241,#68242,#68243,#68244,#68245,#68246,#68247,#68248,#68249,#68250,#68251,
#68252,#68253,#68254,#68255,#68256,#68257,#68258,#68259,#68260,#68261,#68262,
#68263,#68264,#68265,#68266,#68267,#68268,#68269,#68270,#68271,#68272,#68273,
#68274,#68275,#68276,#68277,#68278,#68279,#68280,#68281,#68282,#68283,#68284,
#68285,#68286,#68287,#68288,#68289,#68290,#68291,#68292,#68293,#68294,#68295,
#68296,#68297,#68298,#68299,#68300,#68301,#68302,#68303,#68304,#68305,#68306,
#68307,#68308,#68309,#68310,#68311,#68312,#68313,#68314,#68315,#68316,#68317,
#68318,#68319,#68320,#68321,#68322,#68323,#68324,#68325,#68326,#68327,#68328,
#68329,#68330,#68331,#68332,#68333,#68334,#68335,#68336,#68337,#68338,#68339,
#68340,#68341,#68342,#68343,#68344,#68345,#68346,#68347,#68348,#68349,#68350,
#68351,#68352,#68353,#68354,#68355,#68356,#68357,#68358,#68359,#68360,#68361,
#68362,#68363,#68364,#68365,#68366,#68367,#68368,#68369,#68370,#68371,#68372,
#68373,#68374,#68375,#68376,#68377,#68378,#68379,#68380,#68381,#68382,#68383,
#68384,#68385,#68386,#68387,#68388,#68389,#68390,#68391,#68392,#68393,#68394,
#68395,#68396,#68397,#68398,#68399,#68400,#68401,#68402,#68403,#68404,#68405,
#68406,#68407,#68408,#68409,#68410,#68411,#68412,#68413,#68414,#68415,#68416,
#68417,#68418,#68419,#68420,#68421,#68422,#68423,#68424,#68425,#68426,#68427,
#68428,#68429,#68430,#68431,#68432,#68433,#68434,#68435,#68436,#68437,#68438,
#68439,#68440,#68441,#68442,#68443,#68444,#68445,#68446,#68447,#68448,#68449,
#68450,#68451,#68452,#68453,#68454,#68455,#68456,#68457,#68458,#68459,#68460,
#68461,#68462,#68463,#68464,#68465,#68466,#68467,#68468,#68469,#68470,#68471,
#68472,#68473,#68474,#68475,#68476,#68477,#68478,#68479,#68480,#68481,#68482,
#68483,#68484,#68485,#68486,#68487,#68488,#68489,#68490,#68491,#68492,#68493,
#68494,#68495,#68496,#68497,#68498,#68499,#68500,#68501,#68502,#68503,#68504,
#68505,#68506,#68507,#68508,#68509,#68510,#68511,#68512,#68513,#68514,#68515,
#68516,#68517,#68518,#68519,#68520,#68521,#68522,#68523,#68524,#68525,#68526,
#68527,#68528,#68529,#68530,#68531,#68532,#68533,#68534,#68535,#68536,#68537,
#68538,#68539,#68540,#68541,#68542,#68543,#68544,#68545,#68546,#68547,#68548,
#68549,#68550,#68551,#68552,#68553,#68554,#68555,#68556,#68557,#68558,#68559,
#68560,#68561,#68562,#68563,#68564,#68565,#68566,#68567,#68568,#68569,#68570,
#68571,#68572,#68573,#68574,#68575,#68576,#68577,#68578,#68579,#68580,#68581,
#68582,#68583,#68584,#68585,#68586,#68587,#68588,#68589,#68590,#68591,#68592,
#68593,#68594,#68595,#68596,#68597,#68598,#68599,#68600,#68601,#68602,#68603,
#68604,#68605,#68606,#68607,#68608,#68609,#68610,#68611,#68612,#68613,#68614,
#68615,#68616,#68617,#68618,#68619,#68620,#68621,#68622,#68623,#68624,#68625,
#68626,#68627,#68628,#68629,#68630,#68631,#68632),.UNSPECIFIED.,.F.,.F.,
(4,2,2,2,2,2,2,2,2,2,2,2,2,2,2,2,2,2,2,2,2,2,2,2,2,2,2,2,2,2,2,2,2,2,2,
2,2,2,2,2,2,2,2,2,2,2,2,2,2,2,2,2,2,2,2,2,2,2,2,2,2,2,2,2,2,2,2,2,2,2,2,
2,2,2,2,2,2,2,2,2,2,2,2,2,2,2,2,2,2,2,2,2,2,2,2,2,2,2,2,2,2,2,2,2,2,2,2,
2,2,2,2,2,2,2,2,2,2,2,2,2,2,2,2,2,2,2,2,2,2,2,2,2,2,2,2,2,2,2,2,2,2,2,2,
2,2,2,2,2,2,2,2,2,2,2,2,2,2,2,2,2,2,2,2,2,2,2,2,2,2,2,2,2,2,2,2,2,2,2,2,
2,2,2,2,2,2,2,2,2,2,2,2,2,2,2,2,2,2,2,2,2,2,2,2,2,2,2,2,2,2,2,2,2,2,2,2,
2,2,2,2,2,2,2,2,2,2,2,2,2,2,2,2,2,2,2,2,2,2,2,2,2,2,2,2,2,2,2,2,4),(0.00169003533835,
0.288045268131539,0.3421649754555,0.352897314127812,0.356511362344053,0.35886362064682,
0.361093357559019,0.364047709823501,0.370707227972985,0.442332842734841,
0.553486978526161,0.721924589962906,0.790429699342945,0.803628054006262,
0.811134702086208,0.817631552265838,0.825604117743465,0.840226111381366,
0.925902576319046,1.04179377793575,1.0876109905549,1.11105807856665,1.1168026467886,
1.12038141760047,1.12370929125231,1.12803099258193,1.13525779442268,1.18245076316577,
1.29557218641728,1.39601527720204,1.41981986101972,1.43041383167253,1.43836701163681,
1.44587239467617,1.4563938410042,1.4850127795495,1.73291434717376,1.83583175380349,
1.87060145820998,1.87545827301694,1.87792884037744,1.87988976742142,1.88183871419,
1.88529722956237,1.89551770627139,2.0455736074636,2.16955647699158,2.2499487325598,
2.273656327109,2.28345336733454,2.28854310404211,2.29174640771982,2.29470645520424,
2.29709911169969,2.29986035696478,2.30452354372262,2.32028947619084,2.59743706295665,
2.70094992659311,2.70589756609823,2.70814853753967,2.70983885537649,2.71142420213534,
2.71361346480929,2.719199696416,2.81325162794002,3.0358079018886,3.06296054239148,
3.07052783073283,3.07513371026124,3.07929421316157,3.0846199652116,3.0931293275506,
3.13244813077903,3.18565168884913,3.34177547450781,3.44739244230559,3.4529785443134,
3.45553882922208,3.45746949207241,3.45928520831361,3.4622984099423,3.47000893796097,
3.55858672557251,3.68411785111851,3.76515927735238,3.81648028330425,3.84260563460912,
3.84758289254568,3.85027766461067,3.85250001119127,3.85512658474137,3.85966750128629,
3.87697756782417,4.15856610215374,4.2420145107666,4.27015734919051,4.27333856827254,
4.27489371555689,4.27599656177498,4.27714970603676,4.27875821813101,4.28300957378941,
4.34831745570499,4.54478956791381,4.60133112417586,4.64156248758237,4.66985013688603,
4.67478924687912,4.6774089121329,4.67956154729329,4.68205721528173,4.68631306593921,
4.70192958191256,4.98446823060957,5.06570553957838,5.07053025402685,5.07227614263959,
5.07350638376477,5.07465899674675,5.07624643299506,5.07935678014783,5.10069670862331,
5.16410639704356,5.35903238238304,5.39488458972281,5.48066484784574,5.48823050148015,
5.49126287501233,5.49348284510885,5.49587250632902,5.49909301511976,5.50632976726016,
5.62739806970566,5.73629016666609,5.79419089698692,5.88396812674939,5.88984025441354,
5.89274299618139,5.89483390822586,5.89705320831283,5.89998976572733,5.90637525978894,
6.0376358521255,6.1209643238565,6.31112246315615,6.33407420911135,6.34273009277626,
6.34893844711936,6.35552992995728,6.36430347086444,6.38383794866738,6.46333374718156,
6.56897853803143,6.64390275262583,6.65181980446199,6.65580348478561,6.65908929512506,
6.66291740915685,6.669684170347,6.70072476662585,6.83288257014554,6.89888425020493,
6.94811642061838,6.96254481853922,6.97127493888006,6.9783829702625,6.98816966159238,
7.00656066468097,7.09523491404739,7.21017253699412,7.34725655588969,7.35168892904982,
7.35571884955472,7.36483173529657,7.40613770690696,7.41110727325242,7.41363989236017,
7.41550419290297,7.41752114702744,7.4202044165012,7.42604366359072,7.43376957197959,
7.50320462907729,7.61064298740999,7.81245160560922,7.82549710603779,7.82982382596968,
7.83224183686882,7.83465989409483,7.83768488996447,7.8435601124925,7.88242944237892,
7.97858683471607,8.16314800407253,8.23702651438012,8.24218926455461,8.24430558395608,
8.24587224583045,8.24757536373241,8.2498526634701,8.2549628546333,8.26190975543162,
8.27927792730486,8.34265486956678,8.44570122038853,8.591681994606,8.60387341595175,
8.60937545021437,8.61357591650927,8.61805883459946,8.62506812299598,8.64541119977553,
8.73969685526377,8.89589993370086,8.94583370350186,8.98439969078601,8.98917830281284,
8.99161726783138,8.99341383871419,8.99535848634535,8.99726771833799,9.00183442329845,
9.03305394982638,9.07979359689901,9.12293051843789,9.2918436804488,9.37553913867367,
9.38280018796745,9.38570643089234,9.38783254851848,9.39011971559718,9.39319960740163,
9.40010936714799,9.51573800276529,9.59268743958876,9.62642247510404,9.64352603435034,
9.6626715083179,9.79892639731796,9.80753916787733,9.80991308308417,9.81131045280769,
9.81239815070129,9.81382195085477,9.81642728596756,9.81964282068652,9.96333031754118),
 .UNSPECIFIED.);
#3469=B_SPLINE_CURVE_WITH_KNOTS('',3,(#68634,#68635,#68636,#68637,#68638,
#68639,#68640,#68641,#68642,#68643,#68644,#68645,#68646,#68647,#68648,#68649,
#68650,#68651,#68652,#68653,#68654,#68655,#68656,#68657,#68658,#68659,#68660,
#68661,#68662,#68663,#68664,#68665,#68666,#68667,#68668,#68669,#68670,#68671,
#68672,#68673,#68674,#68675,#68676,#68677,#68678,#68679,#68680,#68681,#68682,
#68683,#68684,#68685,#68686,#68687,#68688,#68689,#68690,#68691,#68692,#68693,
#68694,#68695,#68696,#68697,#68698,#68699,#68700,#68701,#68702,#68703,#68704,
#68705,#68706,#68707,#68708,#68709,#68710,#68711,#68712,#68713,#68714,#68715,
#68716,#68717,#68718,#68719,#68720,#68721,#68722,#68723,#68724,#68725,#68726,
#68727,#68728,#68729,#68730,#68731,#68732,#68733,#68734,#68735,#68736,#68737,
#68738,#68739,#68740,#68741,#68742,#68743,#68744,#68745,#68746,#68747,#68748,
#68749,#68750,#68751,#68752,#68753,#68754,#68755,#68756,#68757,#68758,#68759,
#68760,#68761,#68762,#68763,#68764,#68765,#68766,#68767,#68768,#68769,#68770,
#68771,#68772,#68773,#68774,#68775,#68776,#68777,#68778,#68779,#68780,#68781,
#68782,#68783,#68784,#68785,#68786,#68787,#68788,#68789,#68790,#68791,#68792,
#68793,#68794,#68795,#68796,#68797,#68798,#68799,#68800,#68801,#68802,#68803,
#68804,#68805,#68806,#68807,#68808,#68809,#68810,#68811,#68812,#68813,#68814,
#68815,#68816,#68817,#68818,#68819,#68820,#68821,#68822,#68823,#68824,#68825,
#68826,#68827,#68828,#68829,#68830,#68831,#68832,#68833,#68834,#68835,#68836,
#68837,#68838,#68839,#68840,#68841,#68842,#68843,#68844,#68845,#68846,#68847,
#68848,#68849,#68850,#68851,#68852,#68853,#68854,#68855,#68856,#68857,#68858,
#68859,#68860,#68861,#68862,#68863,#68864,#68865,#68866,#68867,#68868,#68869,
#68870,#68871,#68872,#68873,#68874,#68875,#68876,#68877,#68878,#68879,#68880,
#68881,#68882,#68883,#68884,#68885,#68886,#68887,#68888,#68889,#68890,#68891,
#68892,#68893,#68894,#68895),.UNSPECIFIED.,.F.,.F.,(4,3,3,3,3,3,3,3,3,3,
3,3,3,3,3,3,3,3,3,3,3,3,3,3,3,3,3,3,3,3,3,3,3,3,3,3,3,3,3,3,3,3,3,3,3,3,
3,3,3,3,3,3,3,3,3,3,3,3,3,3,3,3,3,3,3,3,3,3,3,3,3,3,3,3,3,3,3,3,3,3,3,3,
3,3,3,3,3,4),(170.769651999993,170.841525264034,170.913339268465,170.985109276191,
171.059131815152,171.130872259162,171.202617263185,171.274380554809,171.346175885099,
171.418054342032,171.489982494379,171.562008735186,171.577289587882,171.652826221117,
171.728276979241,171.80365475444,171.878972391218,171.954242694441,172.031816353787,
172.107036048043,172.182249863931,172.257469348117,172.332706048281,172.407998578141,
172.483324313756,172.558720531494,172.574831969206,172.651430711188,172.727964401205,
172.804442717187,172.880866853705,172.957258260071,173.033625845381,173.073603159869,
173.151724309452,173.229890374643,173.308106089272,173.386412551037,173.464767207882,
173.543207142429,173.572374350531,173.654343152433,173.736240165645,173.819966509533,
173.901623383812,173.986384462503,174.071145541194,174.144772565293,174.218394338589,
174.292023843992,174.36570551181,174.439414444971,174.513205025037,174.569916731856,
174.646422038254,174.722871516419,174.799276065152,174.875646550934,174.951993815244,
175.028926977486,175.105273938351,175.181631204493,175.258008628461,175.335371249641,
175.411847821384,175.489653467282,175.567459113181,175.642152203854,175.716765486922,
175.79131134536,175.865791656376,175.940233734425,176.014650566224,176.066230303844,
176.146524313229,176.226962925813,176.311472567986,176.392247106257,176.473122583034,
176.554132621711,176.565001494506,176.641798271613,176.718494678783,176.795100070023,
176.871597528246,176.948031146194,177.024393963857,177.052837307172),
 .UNSPECIFIED.);
#3470=B_SPLINE_CURVE_WITH_KNOTS('',3,(#68897,#68898,#68899,#68900,#68901,
#68902,#68903,#68904,#68905,#68906,#68907,#68908,#68909),.UNSPECIFIED.,
 .F.,.F.,(4,1,1,1,1,1,1,1,1,1,4),(177.052840192605,177.562543875831,178.560086257156,
179.557628638481,180.056399829143,180.555171019806,181.053942210468,181.55271340113,
182.550255782455,183.049026973118,183.336022614352),.UNSPECIFIED.);
#3471=B_SPLINE_CURVE_WITH_KNOTS('',3,(#68911,#68912,#68913,#68914,#68915,
#68916,#68917,#68918,#68919,#68920,#68921,#68922,#68923,#68924,#68925,#68926,
#68927,#68928,#68929,#68930,#68931,#68932,#68933,#68934,#68935,#68936,#68937,
#68938,#68939,#68940,#68941,#68942,#68943,#68944,#68945,#68946,#68947,#68948,
#68949,#68950,#68951,#68952,#68953,#68954,#68955,#68956,#68957,#68958,#68959,
#68960,#68961,#68962,#68963,#68964,#68965,#68966,#68967,#68968,#68969,#68970,
#68971,#68972,#68973,#68974,#68975,#68976,#68977,#68978,#68979,#68980,#68981,
#68982,#68983,#68984,#68985,#68986,#68987,#68988,#68989,#68990,#68991,#68992,
#68993,#68994,#68995,#68996,#68997,#68998,#68999,#69000,#69001,#69002,#69003,
#69004,#69005,#69006,#69007,#69008,#69009,#69010,#69011,#69012,#69013,#69014,
#69015,#69016,#69017,#69018,#69019,#69020,#69021,#69022,#69023,#69024,#69025,
#69026,#69027,#69028,#69029,#69030,#69031,#69032,#69033,#69034,#69035,#69036,
#69037,#69038,#69039,#69040,#69041,#69042,#69043,#69044,#69045,#69046,#69047,
#69048,#69049,#69050,#69051,#69052,#69053,#69054,#69055,#69056,#69057,#69058,
#69059,#69060,#69061,#69062,#69063,#69064,#69065,#69066,#69067,#69068,#69069,
#69070,#69071,#69072,#69073,#69074,#69075,#69076,#69077,#69078,#69079,#69080,
#69081,#69082,#69083,#69084,#69085,#69086,#69087,#69088,#69089,#69090,#69091,
#69092,#69093,#69094,#69095,#69096,#69097,#69098,#69099,#69100,#69101,#69102,
#69103,#69104,#69105,#69106,#69107,#69108,#69109,#69110,#69111,#69112,#69113,
#69114,#69115,#69116,#69117,#69118,#69119,#69120,#69121,#69122,#69123,#69124,
#69125,#69126,#69127,#69128,#69129,#69130,#69131,#69132,#69133,#69134,#69135,
#69136,#69137,#69138,#69139,#69140,#69141,#69142,#69143,#69144,#69145,#69146,
#69147,#69148,#69149,#69150,#69151,#69152,#69153,#69154,#69155,#69156,#69157,
#69158,#69159,#69160,#69161,#69162,#69163,#69164,#69165,#69166,#69167,#69168,
#69169,#69170,#69171,#69172,#69173,#69174,#69175,#69176,#69177,#69178,#69179,
#69180,#69181,#69182,#69183,#69184,#69185,#69186,#69187,#69188,#69189,#69190,
#69191,#69192,#69193,#69194,#69195,#69196,#69197,#69198,#69199,#69200,#69201,
#69202,#69203,#69204,#69205,#69206,#69207,#69208,#69209,#69210,#69211,#69212,
#69213,#69214,#69215,#69216,#69217,#69218,#69219,#69220,#69221,#69222,#69223,
#69224,#69225,#69226,#69227,#69228,#69229,#69230,#69231,#69232,#69233,#69234,
#69235,#69236,#69237,#69238,#69239,#69240,#69241,#69242,#69243,#69244,#69245,
#69246,#69247,#69248,#69249,#69250,#69251,#69252,#69253,#69254,#69255,#69256,
#69257,#69258,#69259,#69260,#69261,#69262,#69263,#69264,#69265,#69266,#69267,
#69268,#69269,#69270,#69271,#69272,#69273,#69274,#69275,#69276,#69277,#69278,
#69279,#69280,#69281,#69282,#69283,#69284,#69285,#69286,#69287,#69288,#69289,
#69290,#69291,#69292,#69293,#69294,#69295,#69296,#69297,#69298,#69299,#69300,
#69301,#69302,#69303,#69304,#69305,#69306,#69307,#69308,#69309,#69310,#69311,
#69312,#69313,#69314,#69315,#69316,#69317,#69318,#69319,#69320,#69321,#69322,
#69323,#69324,#69325,#69326,#69327,#69328,#69329,#69330,#69331,#69332,#69333,
#69334,#69335,#69336,#69337,#69338,#69339,#69340,#69341,#69342,#69343,#69344,
#69345,#69346,#69347,#69348,#69349,#69350,#69351,#69352,#69353,#69354,#69355,
#69356,#69357,#69358,#69359,#69360,#69361,#69362,#69363,#69364,#69365,#69366,
#69367,#69368,#69369,#69370,#69371,#69372,#69373,#69374,#69375,#69376,#69377,
#69378,#69379,#69380,#69381,#69382,#69383,#69384,#69385,#69386,#69387,#69388,
#69389,#69390,#69391,#69392,#69393,#69394,#69395,#69396,#69397,#69398,#69399,
#69400,#69401,#69402,#69403,#69404,#69405,#69406,#69407,#69408,#69409,#69410,
#69411,#69412,#69413,#69414,#69415,#69416,#69417,#69418,#69419,#69420,#69421,
#69422,#69423,#69424,#69425,#69426,#69427,#69428,#69429,#69430,#69431,#69432,
#69433,#69434,#69435,#69436),.UNSPECIFIED.,.F.,.F.,(4,2,2,2,2,2,2,2,2,2,
2,2,2,2,2,2,2,2,2,2,2,2,2,2,2,2,2,2,2,2,2,2,2,2,2,2,2,2,2,2,2,2,2,2,2,2,
2,2,2,2,2,2,2,2,2,2,2,2,2,2,2,2,2,2,2,2,2,2,2,2,2,2,2,2,2,2,2,2,2,2,2,2,
2,2,2,2,2,2,2,2,2,2,2,2,2,2,2,2,2,2,2,2,2,2,2,2,2,2,2,2,2,2,2,2,2,2,2,2,
2,2,2,2,2,2,2,2,2,2,2,2,2,2,2,2,2,2,2,2,2,2,2,2,2,2,2,2,2,2,2,2,2,2,2,2,
2,2,2,2,2,2,2,2,2,2,2,2,2,2,2,2,2,2,2,2,2,2,2,2,2,2,2,2,2,2,2,2,2,2,2,2,
2,2,2,2,2,2,2,2,2,2,2,2,2,2,2,2,2,2,2,2,2,2,2,2,2,2,2,2,2,2,2,2,2,2,2,2,
2,2,2,2,2,2,2,2,2,2,2,2,2,2,2,2,2,2,2,2,2,2,2,2,2,2,2,2,2,2,2,2,2,2,2,2,
4),(0.0016813894720157,0.126276306325587,0.13171521603428,0.134813406577695,
0.136946061564364,0.139024362305826,0.140949491087562,0.143435306169637,
0.148776093342873,0.193897711692965,0.246102946707196,0.262390167713752,
0.285794126424522,0.320087296011645,0.390930867775347,0.485193343825969,
0.523841633721814,0.529356059979522,0.532163536424868,0.534199789165854,
0.536371278942309,0.540078880990494,0.55015100646069,0.703271582382227,
0.786515340473811,0.837834333923844,0.898749772576009,0.934487678758292,
0.951930512613121,0.954776619796794,0.956262337919711,0.957470845359138,
0.95885842686672,0.961231062647402,0.97012383177081,1.10932618782953,1.21324590937667,
1.22952058161868,1.28967045517663,1.32228293571319,1.35064336093572,1.3555840756948,
1.35820327475134,1.36014694378895,1.36256792176654,1.3666051285224,1.37982219166346,
1.57974775715462,1.68081352872921,1.72878753413955,1.74858909682943,1.75155845237035,
1.75311421988214,1.75438426268061,1.75565816326952,1.75798093028333,1.76529594289006,
1.88614788006614,2.04264049383793,2.12675154087064,2.1634520484143,2.16907819905463,
2.17198237838747,2.17410521645429,2.17638469223063,2.17964376928181,2.18861168275333,
2.32551285696637,2.40033690502228,2.55668586642739,2.56419023975228,2.57001760980649,
2.57284691400218,2.57505424225381,2.57715459668584,2.58069488373071,2.59008662487545,
2.59956634908852,2.77849466405771,2.97819699447958,2.99951156471404,3.01583034022543,
3.02398112487448,3.02987030007139,3.03704367692439,3.04871724978831,3.08630892509699,
3.29837489785931,3.32565291715049,3.33163007837961,3.33520984563063,3.338470970241,
3.34268134126249,3.34948834652552,3.38865188205523,3.4633678688153,3.57917791198519,
3.61165470575163,3.63566084974347,3.64613919301554,3.65392119967909,3.66120041674774,
3.67129379245727,3.69802893611616,3.89723498840701,4.00078157447208,4.06037241668731,
4.08622825317741,4.09072286391114,4.09310963705833,4.09488254910694,4.09709458467479,
4.10079186163325,4.11296881461358,4.37751463807427,4.49888786919302,4.50600147471296,
4.50926060213944,4.51171744566247,4.5140280226436,4.51722865218343,4.52368818499514,
4.58302392657759,4.78216342476303,4.91459760855396,4.91958658164072,4.92181566607141,
4.92347316137414,4.92501587927965,4.92712775282223,4.93131721565626,4.96700764764638,
4.9783119243875,5.03820072641067,5.14045933275398,5.2687654109915,5.28016785829196,
5.28479123282316,5.28865760875609,5.29263767700519,5.29848486017698,5.31403133582179,
5.38497045258501,5.48997559611325,5.64385776023696,5.66602124321873,5.66989689859193,
5.67223342344906,5.67403846093759,5.6759828719288,5.67905278079114,5.68879275401658,
5.8466369787072,5.98972677624834,6.06231919088305,6.06925759987435,6.07208077907739,
6.07416281593377,6.07641857225871,6.07948443059417,6.08648323198734,6.20155412509249,
6.3562060278163,6.44620500024421,6.45920845028298,6.48651817069122,6.48967901172627,
6.49126137817559,6.49242532117264,6.49368700087476,6.4954022498206,6.49931815638298,
6.59739814063084,6.66030634366478,6.73021428129816,6.87684417251856,6.88655021229513,
6.89020646477263,6.89237166783306,6.89441759817212,6.89726309859609,6.90294131270436,
6.94648917205556,7.01372562470065,7.14419844825498,7.25042281028484,7.27879888185834,
7.28247762272717,7.28420454223694,7.28555417995817,7.28702328333278,7.28937510291162,
7.29710255340587,7.40042222325123,7.56652690397069,7.60680990235306,7.64786719661048,
7.66709479081452,7.67202388171467,7.67485317424848,7.67701711106436,7.67980353641607,
7.68457647867163,7.70432611529756,7.73906828330887,7.82540200164722,7.91621938068956,
8.05378211301946,8.06210642614992,8.06462787814728,8.06598445504395,8.06730768978272,
8.06891519961576,8.07189971496406,8.08972346998265,8.11829715700733,8.21764864857086,
8.31646351631789,8.44515448611735,8.45324832920377,8.45629593936965,8.45846221265475,
8.46050759660477,8.46334985266736,8.46889945219032,8.50890533921324,8.5666422744989,
8.65315760038643,8.84314085372879,8.85448300920299,8.85691016024225,8.85846827826325,
8.85970739684579,8.86109950313883,8.86345756859054,8.87285251805831,8.94423938042643,
9.01678332376981,9.08549889170928,9.08899262232838,9.2019562060884,9.26563155247367,
9.27180455449668,9.274793389,9.27691903974772,9.27892693456711,9.2817184373797,
9.28728458515085,9.32972109297728,9.42295236817236,9.43920789903987,9.45082249532382,
9.48848413968528,9.66150548935551,9.67222315597415,9.67554106896341,9.67734051887701,
9.67910603031286,9.68126471039495,9.68530468990907,9.70776609406871,9.7564964949981,
9.95504525777298),.UNSPECIFIED.);
#3472=B_SPLINE_CURVE_WITH_KNOTS('',3,(#69438,#69439,#69440,#69441,#69442,
#69443,#69444,#69445,#69446,#69447,#69448,#69449,#69450,#69451,#69452,#69453,
#69454,#69455,#69456,#69457,#69458,#69459,#69460,#69461,#69462,#69463,#69464,
#69465,#69466,#69467,#69468,#69469,#69470,#69471,#69472,#69473,#69474,#69475,
#69476,#69477,#69478,#69479,#69480,#69481,#69482,#69483,#69484,#69485,#69486,
#69487,#69488,#69489,#69490,#69491,#69492,#69493,#69494,#69495,#69496,#69497,
#69498,#69499,#69500,#69501,#69502,#69503,#69504,#69505,#69506,#69507,#69508,
#69509,#69510,#69511,#69512,#69513,#69514,#69515,#69516,#69517,#69518,#69519,
#69520,#69521,#69522,#69523,#69524,#69525,#69526,#69527,#69528,#69529,#69530,
#69531,#69532,#69533,#69534,#69535,#69536,#69537,#69538,#69539,#69540,#69541,
#69542,#69543,#69544,#69545,#69546,#69547,#69548,#69549,#69550,#69551,#69552,
#69553,#69554,#69555,#69556,#69557,#69558,#69559,#69560,#69561,#69562,#69563,
#69564,#69565,#69566,#69567,#69568,#69569,#69570,#69571,#69572,#69573,#69574,
#69575,#69576,#69577,#69578,#69579,#69580,#69581,#69582,#69583,#69584,#69585,
#69586,#69587,#69588,#69589,#69590,#69591,#69592,#69593,#69594,#69595,#69596,
#69597,#69598,#69599,#69600,#69601,#69602,#69603,#69604,#69605,#69606,#69607,
#69608,#69609,#69610,#69611,#69612,#69613,#69614,#69615,#69616,#69617,#69618,
#69619,#69620,#69621,#69622,#69623,#69624,#69625,#69626,#69627,#69628,#69629,
#69630,#69631,#69632,#69633,#69634,#69635,#69636,#69637,#69638,#69639,#69640,
#69641,#69642,#69643,#69644,#69645,#69646,#69647,#69648,#69649,#69650,#69651,
#69652,#69653,#69654,#69655,#69656,#69657,#69658,#69659,#69660,#69661,#69662,
#69663,#69664,#69665,#69666,#69667,#69668,#69669,#69670,#69671,#69672,#69673,
#69674,#69675,#69676,#69677,#69678,#69679,#69680,#69681,#69682,#69683,#69684,
#69685,#69686,#69687,#69688,#69689,#69690,#69691,#69692,#69693,#69694,#69695,
#69696,#69697,#69698,#69699,#69700,#69701,#69702,#69703,#69704,#69705,#69706,
#69707,#69708,#69709,#69710,#69711,#69712,#69713,#69714,#69715,#69716,#69717,
#69718,#69719,#69720,#69721,#69722,#69723,#69724,#69725,#69726,#69727,#69728,
#69729,#69730,#69731,#69732,#69733,#69734,#69735,#69736,#69737,#69738,#69739,
#69740,#69741,#69742,#69743,#69744,#69745,#69746,#69747,#69748,#69749,#69750,
#69751,#69752,#69753,#69754,#69755,#69756,#69757,#69758,#69759,#69760,#69761,
#69762,#69763,#69764,#69765,#69766,#69767,#69768,#69769,#69770,#69771,#69772,
#69773,#69774,#69775,#69776,#69777,#69778,#69779,#69780,#69781,#69782,#69783,
#69784,#69785,#69786,#69787,#69788,#69789,#69790,#69791,#69792,#69793,#69794,
#69795,#69796,#69797,#69798,#69799,#69800,#69801,#69802,#69803,#69804,#69805,
#69806,#69807,#69808,#69809,#69810,#69811,#69812,#69813,#69814,#69815,#69816,
#69817,#69818,#69819,#69820,#69821,#69822,#69823,#69824,#69825,#69826,#69827,
#69828,#69829,#69830,#69831,#69832,#69833,#69834,#69835,#69836,#69837,#69838,
#69839,#69840,#69841,#69842,#69843,#69844,#69845,#69846,#69847,#69848,#69849,
#69850,#69851,#69852,#69853,#69854,#69855,#69856,#69857,#69858,#69859,#69860,
#69861,#69862,#69863,#69864,#69865,#69866,#69867,#69868,#69869,#69870,#69871,
#69872,#69873,#69874,#69875,#69876,#69877,#69878,#69879,#69880,#69881,#69882,
#69883,#69884,#69885,#69886,#69887,#69888,#69889,#69890,#69891,#69892,#69893,
#69894,#69895,#69896,#69897,#69898,#69899,#69900,#69901,#69902,#69903,#69904,
#69905,#69906,#69907,#69908,#69909,#69910,#69911,#69912,#69913,#69914,#69915,
#69916,#69917,#69918,#69919,#69920,#69921,#69922,#69923,#69924,#69925,#69926,
#69927),.UNSPECIFIED.,.F.,.F.,(4,2,2,2,2,2,2,2,2,2,2,2,2,2,2,2,2,2,2,2,
2,2,2,2,2,2,2,2,2,2,2,2,2,2,2,2,2,2,2,2,2,2,2,2,2,2,2,2,2,2,2,2,2,2,2,2,
2,2,2,2,2,2,2,2,2,2,2,2,2,2,2,2,2,2,2,2,2,2,2,2,2,2,2,2,2,2,2,2,2,2,2,2,
2,2,2,2,2,2,2,2,2,2,2,2,2,2,2,2,2,2,2,2,2,2,2,2,2,2,2,2,2,2,2,2,2,2,2,2,
2,2,2,2,2,2,2,2,2,2,2,2,2,2,2,2,2,2,2,2,2,2,2,2,2,2,2,2,2,2,2,2,2,2,2,2,
2,2,2,2,2,2,2,2,2,2,2,2,2,2,2,2,2,2,2,2,2,2,2,2,2,2,2,2,2,2,2,2,2,2,2,2,
2,2,2,2,2,2,2,2,2,2,2,2,2,2,2,2,2,2,2,2,2,2,2,2,2,2,2,2,2,2,2,2,2,2,2,2,
2,2,2,2,2,2,2,2,4),(0.0021147162426415,0.0857262217385641,0.0959123132725421,
0.101817668638507,0.105952423517762,0.109510120672382,0.113321414548935,
0.118219462115226,0.128355303510646,0.198457205571982,0.218864102215348,
0.255164213476987,0.455011656366761,0.470031775693596,0.473395464028391,
0.475296187041642,0.476760751229038,0.478410875300978,0.481474133588517,
0.491622758632171,0.662151770789466,0.714975847791071,0.773859001783566,
0.875910873483415,0.882889809062308,0.886123944905947,0.888577389939866,
0.890896201465588,0.894126531781061,0.902525128685859,1.02961162784532,
1.0945067501913,1.20524360683114,1.28553165208685,1.29817116256545,1.30176031498023,
1.30394827115179,1.30592352168945,1.30844611491447,1.31245710765836,1.33283936785151,
1.5691885282616,1.65665791247992,1.72040189980086,1.73512615034882,1.74364682219264,
1.75085877779597,1.75999003059328,1.77694684805219,1.90332017671288,2.03590229083718,
2.04753685223959,2.05606067100292,2.06030458264268,2.06358258447306,2.06667617038536,
2.07101759104478,2.08401702036005,2.18618316659222,2.32731586969064,2.34510604146755,
2.35534739163738,2.36247298112973,2.36928828667622,2.37569464315755,2.38417294501723,
2.39834975895669,2.49607255557145,2.53627412163732,2.70121754018261,2.80311492162715,
2.81229754901474,2.81906637785889,2.82206919057242,2.82429470788258,2.82636000871468,
2.82917824160068,2.83620048021959,2.94636996472043,3.10348583461963,3.21225025704563,
3.21976968678328,3.22303925051097,3.22543566974893,3.22764106093274,3.23062175623667,
3.23789980232397,3.31153014271453,3.3524873607049,3.52832814665662,3.58743433757029,
3.62228162836511,3.63933743746729,3.64227148225394,3.6438209823814,3.64496800991523,
3.64621354827629,3.64801746784966,3.65325286924985,3.74074304237537,3.893129084531,
3.9780306526427,4.01210247075576,4.03111539136288,4.03550078693162,4.03799930145634,
4.03993449712372,4.04245722562997,4.04683288981786,4.06366584341291,4.09538118112343,
4.32176810585032,4.38195140900454,4.43025672223563,4.43776984183809,4.43992504461529,
4.4412527775106,4.44247207562142,4.44403165486226,4.44732324429486,4.46909558516888,
4.51865677483036,4.54506074473599,4.72669198960786,4.78424848556279,4.84701286593956,
4.85853798828355,4.86231304553642,4.86474074815425,4.86702033528734,4.87000798487978,
4.87660151829323,4.92973260715549,4.98045002030486,5.10221443593992,5.24427235548077,
5.25286462314312,5.25648552926838,5.25863738208686,5.26035379641356,5.26265348515541,
5.26694779951379,5.29064318860111,5.3424512558368,5.55487224215899,5.62040553019814,
5.63162385262355,5.63701008483504,5.64117602700476,5.64574583987469,5.6531591034371,
5.67880068867541,5.90227415500722,5.99698321796197,6.0025684084701,6.00475682972833,
6.00634141745119,6.00803078653048,6.01028025482486,6.01522362882187,6.11870399110965,
6.39560652566407,6.41148141879393,6.41615544755748,6.41891814931392,6.42111387769637,
6.42404436306647,6.42948172166862,6.45859474640228,6.51585878091743,6.59837308969972,
6.81737700530157,6.82999182706921,6.83375169501524,6.83598457633156,6.83794438819199,
6.84041241834021,6.84526053629908,6.87981678440402,6.98139824630425,7.14044784617825,
7.19958194660694,7.25317064917875,7.26762837768704,7.27635186016815,7.28424439102001,
7.29442715688286,7.31598237815389,7.39889254138972,7.50522005637645,7.57889164068016,
7.58744346266093,7.59170194898351,7.5950092039627,7.59864875319175,7.60471078440443,
7.63283569665676,7.84915699449695,7.8820564085455,7.8931604814945,7.89950316613594,
7.90537568559607,7.91339087638862,7.92902912279261,8.05170023959194,8.24358712398681,
8.32079868164036,8.34071194170864,8.34982230593964,8.35325066704535,8.35554262923877,
8.35777152310636,8.36077827902947,8.36755214703489,8.52719912658739,8.60332595975835,
8.74182593331619,8.75088262286138,8.75415517434681,8.75643829392326,8.75855997761165,
8.76145559654793,8.7670412572037,8.80270679867144,8.88309602807962,9.01392933675127,
9.08038255757393,9.16777949685675,9.17296213874511,9.17493819556321,9.17626191955968,
9.17752614030541,9.17925754118248,9.18314414459356,9.27023665215949,9.47933248011572,
9.55880443390468,9.56576996403643,9.56855572667082,9.57059288847095,9.572783554419,
9.57573197884494,9.58234014556836,9.69690744402141,9.95834822127454),
 .UNSPECIFIED.);
#3473=B_SPLINE_CURVE_WITH_KNOTS('',3,(#69929,#69930,#69931,#69932,#69933,
#69934,#69935,#69936,#69937,#69938,#69939,#69940,#69941,#69942,#69943,#69944),
 .UNSPECIFIED.,.F.,.F.,(4,3,1,1,1,1,1,1,1,1,1,4),(208.46876384307,208.486357696903,
209.483900078227,209.98267126889,210.481442459552,211.478984840877,211.97775603154,
212.476527222202,212.975298412865,213.474069603527,214.471611984852,214.75194915025),
 .UNSPECIFIED.);
#3474=B_SPLINE_CURVE_WITH_KNOTS('',3,(#69946,#69947,#69948,#69949,#69950,
#69951,#69952,#69953,#69954,#69955,#69956,#69957,#69958,#69959,#69960,#69961,
#69962,#69963),.UNSPECIFIED.,.F.,.F.,(4,2,2,2,2,2,2,2,4),(214.75194915025,
215.586866062145,216.42178297404,217.256699885934,218.091616797829,218.926533709724,
219.761450621619,220.596367533514,221.035134457429),.UNSPECIFIED.);
#3475=B_SPLINE_CURVE_WITH_KNOTS('',3,(#69965,#69966,#69967,#69968,#69969,
#69970,#69971,#69972,#69973,#69974,#69975,#69976,#69977,#69978,#69979,#69980,
#69981,#69982,#69983,#69984,#69985,#69986,#69987,#69988,#69989,#69990,#69991,
#69992,#69993,#69994,#69995,#69996,#69997,#69998,#69999,#70000,#70001,#70002,
#70003,#70004,#70005,#70006,#70007,#70008,#70009,#70010,#70011,#70012,#70013,
#70014,#70015,#70016,#70017,#70018,#70019,#70020,#70021,#70022,#70023,#70024,
#70025,#70026,#70027,#70028,#70029,#70030,#70031,#70032,#70033,#70034,#70035,
#70036,#70037,#70038,#70039,#70040,#70041,#70042,#70043,#70044,#70045,#70046,
#70047,#70048,#70049,#70050,#70051,#70052,#70053,#70054,#70055,#70056,#70057,
#70058,#70059,#70060,#70061,#70062,#70063,#70064,#70065,#70066,#70067,#70068,
#70069,#70070,#70071,#70072,#70073,#70074,#70075,#70076,#70077,#70078,#70079,
#70080,#70081,#70082,#70083,#70084,#70085,#70086,#70087,#70088,#70089,#70090,
#70091,#70092,#70093,#70094,#70095,#70096,#70097,#70098,#70099,#70100,#70101,
#70102,#70103,#70104,#70105,#70106,#70107,#70108,#70109,#70110,#70111,#70112,
#70113,#70114,#70115,#70116,#70117,#70118,#70119,#70120,#70121,#70122,#70123,
#70124,#70125,#70126,#70127,#70128,#70129,#70130,#70131,#70132,#70133,#70134,
#70135,#70136,#70137,#70138,#70139,#70140,#70141,#70142,#70143,#70144,#70145,
#70146,#70147,#70148,#70149,#70150,#70151,#70152,#70153,#70154,#70155,#70156,
#70157,#70158,#70159,#70160,#70161,#70162,#70163,#70164,#70165,#70166,#70167,
#70168,#70169,#70170,#70171,#70172,#70173,#70174,#70175,#70176,#70177,#70178,
#70179,#70180,#70181,#70182,#70183,#70184,#70185,#70186,#70187,#70188,#70189,
#70190,#70191,#70192,#70193,#70194,#70195,#70196,#70197,#70198,#70199,#70200,
#70201,#70202,#70203,#70204,#70205,#70206,#70207,#70208,#70209,#70210,#70211,
#70212,#70213,#70214,#70215,#70216,#70217,#70218,#70219,#70220,#70221,#70222,
#70223,#70224,#70225,#70226,#70227,#70228,#70229,#70230,#70231,#70232,#70233,
#70234,#70235,#70236,#70237,#70238,#70239,#70240,#70241,#70242,#70243,#70244,
#70245,#70246,#70247,#70248,#70249,#70250,#70251,#70252,#70253,#70254,#70255,
#70256,#70257,#70258,#70259,#70260,#70261,#70262,#70263,#70264,#70265,#70266,
#70267,#70268,#70269,#70270,#70271,#70272,#70273,#70274,#70275,#70276,#70277,
#70278,#70279,#70280,#70281,#70282,#70283,#70284,#70285,#70286,#70287,#70288,
#70289,#70290,#70291,#70292,#70293,#70294,#70295,#70296,#70297,#70298,#70299,
#70300,#70301,#70302,#70303,#70304,#70305,#70306,#70307,#70308,#70309,#70310,
#70311,#70312,#70313,#70314,#70315,#70316,#70317,#70318,#70319,#70320,#70321,
#70322,#70323,#70324,#70325,#70326,#70327,#70328,#70329,#70330,#70331,#70332,
#70333,#70334,#70335,#70336,#70337,#70338,#70339,#70340,#70341,#70342,#70343,
#70344,#70345,#70346,#70347,#70348,#70349,#70350,#70351,#70352,#70353,#70354,
#70355,#70356,#70357,#70358,#70359,#70360,#70361,#70362,#70363,#70364,#70365,
#70366,#70367,#70368,#70369,#70370,#70371,#70372,#70373,#70374,#70375,#70376,
#70377,#70378,#70379,#70380,#70381,#70382,#70383,#70384,#70385,#70386,#70387,
#70388,#70389,#70390,#70391,#70392,#70393,#70394,#70395,#70396,#70397,#70398,
#70399,#70400,#70401,#70402,#70403,#70404,#70405,#70406,#70407,#70408,#70409,
#70410,#70411,#70412,#70413,#70414,#70415,#70416,#70417,#70418,#70419,#70420,
#70421,#70422,#70423,#70424,#70425,#70426,#70427,#70428,#70429,#70430,#70431,
#70432,#70433,#70434,#70435,#70436,#70437,#70438,#70439,#70440,#70441,#70442,
#70443,#70444,#70445,#70446,#70447,#70448,#70449,#70450,#70451,#70452,#70453,
#70454,#70455,#70456,#70457,#70458,#70459,#70460,#70461,#70462,#70463,#70464,
#70465,#70466,#70467,#70468,#70469,#70470,#70471,#70472,#70473,#70474,#70475,
#70476),.UNSPECIFIED.,.F.,.F.,(4,2,2,2,2,2,2,2,2,2,2,2,2,2,2,2,2,2,2,2,
2,2,2,2,2,2,2,2,2,2,2,2,2,2,2,2,2,2,2,2,2,2,2,2,2,2,2,2,2,2,2,2,2,2,2,2,
2,2,2,2,2,2,2,2,2,2,2,2,2,2,2,2,2,2,2,2,2,2,2,2,2,2,2,2,2,2,2,2,2,2,2,2,
2,2,2,2,2,2,2,2,2,2,2,2,2,2,2,2,2,2,2,2,2,2,2,2,2,2,2,2,2,2,2,2,2,2,2,2,
2,2,2,2,2,2,2,2,2,2,2,2,2,2,2,2,2,2,2,2,2,2,2,2,2,2,2,2,2,2,2,2,2,2,2,2,
2,2,2,2,2,2,2,2,2,2,2,2,2,2,2,2,2,2,2,2,2,2,2,2,2,2,2,2,2,2,2,2,2,2,2,2,
2,2,2,2,2,2,2,2,2,2,2,2,2,2,2,2,2,2,2,2,2,2,2,2,2,2,2,2,2,2,2,2,2,2,2,2,
2,2,2,2,2,2,2,2,2,2,2,2,2,2,2,2,2,2,2,4),(0.001951533452596,0.265717321319917,
0.317341835588869,0.325376765827814,0.3276862666474,0.329098702429905,0.330376332518678,
0.332010874754853,0.335372120405849,0.358662092625752,0.468281733597388,
0.513763873343083,0.625751409145384,0.678173822325819,0.702169775743808,
0.711754552531524,0.716600773823633,0.71957768741308,0.722301751833663,
0.724427670951214,0.72651042615492,0.730068199531644,0.739742890751326,
0.86679288798981,0.932468076113923,1.06479302989476,1.1148141875318,1.12248808645428,
1.12465969487064,1.12599099474889,1.12720932880081,1.12878788765383,1.13208996362533,
1.15408845654518,1.40067870042842,1.48692095471947,1.52224758592459,1.53520376879134,
1.54415054073146,1.54762243776647,1.54972395080898,1.55199708911254,1.55494587748327,
1.56133228351188,1.60872715456636,1.77046056621364,1.92378574489667,1.93791121758729,
1.94156891021233,1.94372919789255,1.94563596959493,1.94801293825857,1.95167978020016,
1.96833939088765,2.20193778182021,2.29453324672734,2.31356028958412,2.32031261628281,
2.32473663289401,2.32888166679184,2.33373674581061,2.34439136981965,2.41822995509492,
2.61366578679574,2.66276485204052,2.68492429917379,2.68875207706807,2.69077878143689,
2.69244247480863,2.69411840443413,2.69719857924694,2.707096048162,2.86954481235853,
3.00695456765383,3.06509469256782,3.09462892661599,3.10008845123357,3.10302369330253,
3.10521984983143,3.10797896116196,3.11263695265344,3.12837172638961,3.39000425700505,
3.44961594014936,3.50526871698629,3.51563632510471,3.51898307737978,3.52112388466973,
3.52312639600432,3.52574069798841,3.53012854201908,3.55677322438013,3.56187419452147,
3.72388371425758,3.81789483571181,3.92905919796076,3.94875337225157,3.95855780456448,
3.96566268896484,3.97436915348954,3.98871242628505,4.03720416782415,4.20204883044425,
4.26493151031742,4.2729496446515,4.27704190884932,4.28001777630835,4.28365558147312,
4.28970695684892,4.31328579112865,4.33275778340722,4.39638497584167,4.47694045371521,
4.55326950616606,4.57237571540609,4.5810670358198,4.58764122971028,4.59386618453668,
4.60259885639249,4.62618463315842,4.86646835244077,4.9802976591868,5.03008595353589,
5.03621390297851,5.03911228356299,5.0413318367125,5.0437043405124,5.04741303121301,
5.05890604606681,5.21514715136939,5.29002839264698,5.42699189963121,5.4359622488642,
5.43922173549449,5.44150134993598,5.44362420134704,5.44652822038162,5.45215344948398,
5.4888278860254,5.57283460630526,5.66635969382606,5.70968686148662,5.76190687894718,
5.85249190898214,5.85790764595199,5.85996149324299,5.86118160575228,5.86233677909754,
5.86394674216659,5.86718354382573,5.89751972062914,5.9537159215645,6.14691719609207,
6.22524993965214,6.24723500148468,6.25162210435026,6.25438569981103,6.25654944593365,
6.25894548235369,6.26287313209285,6.27665186113409,6.3624633135438,6.52541776152828,
6.59335055712837,6.65118777322531,6.65531443229296,6.65690161242639,6.65804871462973,
6.65927607772336,6.66091672090075,6.66454590252395,6.73263988988279,6.90637352692446,
7.06513602481122,7.07535705906912,7.07908685011856,7.08126242001413,7.08329678031912,
7.08609274200448,7.09155331373573,7.12867475289864,7.22220798761413,7.36833388769845,
7.46380067968375,7.47093998728375,7.47356285250664,7.47540687358606,7.47713128231082,
7.47950171757497,7.48413211656161,7.51535882400722,7.59744225875962,7.68971340294352,
7.74131872925907,7.83500813165633,7.84610484627746,7.85159682793949,7.85554550976842,
7.85973585256492,7.86518099353552,7.87685990441749,7.89214738329876,8.11574406924228,
8.21324159148531,8.21883332103305,8.22102267943941,8.22260738279229,8.22429635074362,
8.22654438819321,8.23148101705829,8.23791374389157,8.25343561837247,8.31302842062166,
8.41634128144384,8.61536988972848,8.62804401933215,8.63231778230145,8.63472345864302,
8.63691981004058,8.63985893388704,8.64533726327819,8.67524077685549,8.73408589683472,
8.77386514206112,8.84503634559689,8.90114113979982,9.03541020197952,9.04595398625163,
9.04945487878885,9.05141149103592,9.05338834388455,9.05584819133908,9.06065792786725,
9.09346093759942,9.18355932857806,9.25345509573954,9.36880202776115,9.45790793168817,
9.47860278410875,9.48859631016876,9.49646600978707,9.5037870682281,9.51239369813437,
9.5377496250476,9.608828896354,9.67154750433572,9.69699547766963,9.79426533363515,
9.80272985902464,9.80696967029066,9.81027419058992,9.81333205485562,9.81687702618506,
9.82198829068213,9.84212776085011,9.95551597770185),.UNSPECIFIED.);
#3476=B_SPLINE_CURVE_WITH_KNOTS('',3,(#70478,#70479,#70480,#70481,#70482,
#70483,#70484,#70485,#70486,#70487,#70488,#70489),.UNSPECIFIED.,.F.,.F.,
(4,1,1,1,1,1,1,1,1,4),(233.601505071788,233.923688420687,234.42245961135,
235.420001992675,236.417544374,237.415086755324,237.913857945987,238.412629136649,
239.410171517974,239.884387681578),.UNSPECIFIED.);
#3477=B_SPLINE_CURVE_WITH_KNOTS('',3,(#70491,#70492,#70493,#70494,#70495,
#70496,#70497,#70498,#70499,#70500,#70501,#70502,#70503,#70504,#70505,#70506,
#70507,#70508,#70509,#70510,#70511,#70512,#70513,#70514,#70515,#70516,#70517,
#70518,#70519,#70520,#70521,#70522,#70523,#70524,#70525,#70526,#70527,#70528,
#70529,#70530,#70531,#70532,#70533,#70534,#70535,#70536,#70537,#70538,#70539,
#70540,#70541,#70542,#70543,#70544,#70545,#70546,#70547,#70548,#70549,#70550,
#70551,#70552,#70553,#70554,#70555,#70556,#70557,#70558,#70559,#70560,#70561,
#70562,#70563,#70564,#70565,#70566,#70567,#70568,#70569,#70570,#70571,#70572,
#70573,#70574,#70575,#70576,#70577,#70578,#70579,#70580,#70581,#70582,#70583,
#70584,#70585,#70586,#70587,#70588,#70589,#70590,#70591,#70592,#70593,#70594,
#70595,#70596,#70597,#70598,#70599,#70600,#70601,#70602,#70603,#70604,#70605,
#70606,#70607,#70608,#70609,#70610,#70611,#70612,#70613,#70614,#70615,#70616,
#70617,#70618,#70619,#70620,#70621,#70622,#70623,#70624,#70625,#70626,#70627,
#70628,#70629,#70630,#70631,#70632,#70633,#70634,#70635,#70636,#70637,#70638,
#70639,#70640,#70641,#70642,#70643,#70644,#70645,#70646,#70647,#70648,#70649,
#70650,#70651,#70652,#70653,#70654,#70655,#70656,#70657,#70658,#70659,#70660,
#70661,#70662,#70663,#70664,#70665,#70666,#70667,#70668,#70669,#70670,#70671,
#70672,#70673,#70674,#70675,#70676,#70677,#70678,#70679,#70680,#70681,#70682,
#70683,#70684,#70685,#70686,#70687,#70688,#70689,#70690,#70691,#70692,#70693,
#70694,#70695,#70696,#70697,#70698,#70699,#70700,#70701,#70702,#70703,#70704,
#70705,#70706,#70707,#70708,#70709,#70710,#70711,#70712,#70713,#70714,#70715,
#70716,#70717,#70718,#70719,#70720,#70721,#70722,#70723,#70724,#70725,#70726,
#70727,#70728,#70729,#70730,#70731,#70732,#70733,#70734,#70735,#70736,#70737,
#70738,#70739,#70740,#70741,#70742,#70743,#70744,#70745,#70746,#70747,#70748,
#70749,#70750,#70751,#70752,#70753,#70754,#70755,#70756,#70757,#70758,#70759,
#70760,#70761,#70762,#70763,#70764,#70765,#70766,#70767,#70768,#70769,#70770,
#70771,#70772,#70773,#70774,#70775,#70776,#70777,#70778,#70779,#70780,#70781,
#70782,#70783,#70784,#70785,#70786,#70787,#70788,#70789,#70790,#70791,#70792,
#70793,#70794,#70795,#70796,#70797,#70798,#70799,#70800,#70801,#70802,#70803,
#70804,#70805,#70806,#70807,#70808,#70809,#70810,#70811,#70812,#70813,#70814,
#70815,#70816,#70817,#70818,#70819,#70820,#70821,#70822,#70823,#70824,#70825,
#70826,#70827,#70828,#70829,#70830,#70831,#70832,#70833,#70834,#70835,#70836,
#70837,#70838,#70839,#70840,#70841,#70842,#70843,#70844,#70845,#70846,#70847,
#70848,#70849,#70850,#70851,#70852,#70853,#70854,#70855,#70856,#70857,#70858,
#70859,#70860,#70861,#70862,#70863,#70864,#70865,#70866,#70867,#70868,#70869,
#70870,#70871,#70872,#70873,#70874,#70875,#70876,#70877,#70878,#70879,#70880,
#70881,#70882,#70883,#70884,#70885,#70886,#70887,#70888,#70889,#70890,#70891,
#70892,#70893,#70894,#70895,#70896,#70897,#70898,#70899,#70900,#70901,#70902,
#70903,#70904,#70905,#70906,#70907,#70908,#70909,#70910,#70911,#70912,#70913,
#70914,#70915,#70916,#70917,#70918,#70919,#70920,#70921,#70922,#70923,#70924,
#70925,#70926,#70927,#70928,#70929,#70930,#70931,#70932,#70933,#70934,#70935,
#70936,#70937,#70938,#70939,#70940,#70941,#70942,#70943,#70944,#70945,#70946,
#70947,#70948,#70949,#70950,#70951,#70952,#70953,#70954,#70955,#70956,#70957,
#70958,#70959,#70960,#70961,#70962,#70963,#70964,#70965,#70966,#70967,#70968,
#70969,#70970,#70971,#70972,#70973,#70974,#70975,#70976,#70977,#70978,#70979,
#70980,#70981,#70982,#70983,#70984,#70985,#70986,#70987,#70988,#70989,#70990,
#70991,#70992,#70993,#70994,#70995,#70996,#70997,#70998,#70999,#71000,#71001,
#71002,#71003,#71004,#71005,#71006,#71007,#71008,#71009,#71010,#71011,#71012,
#71013,#71014,#71015,#71016,#71017,#71018,#71019,#71020),.UNSPECIFIED.,
 .F.,.F.,(4,2,2,2,2,2,2,2,2,2,2,2,2,2,2,2,2,2,2,2,2,2,2,2,2,2,2,2,2,2,2,
2,2,2,2,2,2,2,2,2,2,2,2,2,2,2,2,2,2,2,2,2,2,2,2,2,2,2,2,2,2,2,2,2,2,2,2,
2,2,2,2,2,2,2,2,2,2,2,2,2,2,2,2,2,2,2,2,2,2,2,2,2,2,2,2,2,2,2,2,2,2,2,2,
2,2,2,2,2,2,2,2,2,2,2,2,2,2,2,2,2,2,2,2,2,2,2,2,2,2,2,2,2,2,2,2,2,2,2,2,
2,2,2,2,2,2,2,2,2,2,2,2,2,2,2,2,2,2,2,2,2,2,2,2,2,2,2,2,2,2,2,2,2,2,2,2,
2,2,2,2,2,2,2,2,2,2,2,2,2,2,2,2,2,2,2,2,2,2,2,2,2,2,2,2,2,2,2,2,2,2,2,2,
2,2,2,2,2,2,2,2,2,2,2,2,2,2,2,2,2,2,2,2,2,2,2,2,2,2,2,2,2,2,2,2,2,2,2,2,
2,2,2,2,2,2,2,2,2,2,2,2,2,2,2,2,2,4),(0.00168357070064361,0.043274643150003,
0.0685334213659095,0.0790143023288335,0.0868883847257787,0.0944095737450267,
0.101794669849645,0.111844750673594,0.137179843959166,0.187514130969224,
0.348804161845356,0.395630614416885,0.401053194682952,0.40476130467354,
0.407874528067813,0.410826942683271,0.414759726605491,0.422149101631073,
0.473392987687212,0.599416728122072,0.659951264051369,0.684273679179953,
0.70264868932782,0.711167356501013,0.71736127507081,0.723515572225275,0.733619732738534,
0.759806628156653,1.00552198108395,1.11994345884837,1.1614787140408,1.16694204752024,
1.16969627850224,1.1716832892601,1.17379299161084,1.17737463862252,1.18698109954257,
1.33744860748507,1.43810358227347,1.55707301404325,1.56638839060558,1.56995495490699,
1.57240962086844,1.57481237876229,1.57770526665601,1.58491466487181,1.65048588343432,
1.76165733730261,1.91767263470405,1.96617116888262,1.98654282058554,1.98961633476199,
1.99119548508848,1.99245584574268,1.9938982926654,1.99634151682156,2.00509666039586,
2.14264997082273,2.23057096430205,2.32100147617026,2.37068103478181,2.37721333124266,
2.38241336843127,2.38508732538944,2.38703755530943,2.38912752643311,2.39210847017446,
2.4002663549463,2.52979483294095,2.68438994542906,2.74044181455745,2.77885985730339,
2.78538427343791,2.78743033279388,2.78873513635092,2.78996287069773,2.79157541648948,
2.79501400647715,2.82140638814894,2.82751990163162,2.83660450070032,2.95132069539436,
3.09341302873435,3.20116883242843,3.20774986988387,3.21076815783328,3.21304461862589,
3.21518639661658,3.21815446026977,3.22414855576671,3.27924054223989,3.33239290271546,
3.4968045191568,3.58737237586432,3.60050340732827,3.60407006443767,3.60621030717788,
3.6081206209944,3.61053039058114,3.61430227953695,3.63234109374042,3.84101922941899,
3.95384819270381,3.97526619925623,3.98236072417324,3.98686041628649,3.99105030173818,
3.99650091327692,4.00842509728725,4.12389661021933,4.261496858014,4.337810877864,
4.34869478025052,4.3517550751624,4.35361346850431,4.35528628656936,4.35741553140064,
4.3617373398443,4.39204436367251,4.64932441583501,4.75392478935123,4.76165115962004,
4.76503283428499,4.76752005624028,4.76981515934972,4.77292650576448,4.78057040761326,
4.86136463807988,4.98004174955559,5.16637169849527,5.17766385897107,5.18126343289091,
5.18324027520222,5.1852149745882,5.18763867139315,5.19227328777566,5.22094577653925,
5.28986735475889,5.45380212274526,5.50673042731537,5.59144336014785,5.61097632404609,
5.62087719515763,5.62873961860188,5.63763025679442,5.65282088438884,5.71976501883445,
5.84884556444085,5.92631971252463,5.93489428125943,5.93915785682697,5.94246613149657,
5.94610384682777,5.95215469550854,5.9800910435969,6.19580005924466,6.22937383641455,
6.24056460513399,6.24692477810978,6.25279384330619,6.26077430473703,6.27623871959087,
6.39512736434397,6.58371822501153,6.64730144268971,6.69278254782892,6.69885602671975,
6.70170066128268,6.70391174563339,6.70630770680104,6.71012212382932,6.72251131492311,
6.88945756757099,7.08501760065372,7.09748773553116,7.10163853312632,7.10396184639994,
7.1060750799815,7.10889132043101,7.11410353876239,7.1417033118507,7.19542408957702,
7.29841788700904,7.45353450326594,7.51654393343234,7.52098954510073,7.52269013153598,
7.52390737952985,7.52506365398733,7.52663701096129,7.52954974089529,7.53336257806554,
7.68846427894584,7.76416277075836,7.90316101507657,7.91248538292321,7.91598820482693,
7.91805971104074,7.92001519078334,7.92273178028472,7.92814120193399,7.96902508966463,
8.07295424057414,8.21097632125331,8.3106574593564,8.31717035203294,8.31929913182466,
8.32048872185174,8.32157872486837,8.32304297502124,8.32573374116278,8.34001488629136,
8.36888139613217,8.42697714040849,8.48700246648982,8.57220064211512,8.72784692789641,
8.73790840655419,8.74161403909164,8.74378491614204,8.74582094258979,8.74862865194153,
8.75414546465156,8.79288417693994,8.88749002208078,8.93480333594175,8.95079901121166,
8.96468383112629,8.97690411286408,8.98778701709875,9.09277672768747,9.10323636555463,
9.12278109258072,9.13251740174098,9.13583582760789,9.13771132707051,9.13959166752094,
9.14192552192337,9.14641871298226,9.15215657573219,9.16490875767532,9.20349591930505,
9.26140221976965,9.3785123105631,9.49672382518336,9.50962581335401,9.5147745998946,
9.51902209129393,9.52334155339519,9.52959537643696,9.54592576675249,9.62206746974412,
9.80168187512738,9.81350051881362,9.855726000521,9.86261140856199,9.87880304855279,
9.88213450575607,9.88425196908999,9.88592334351232,9.88748078326666,9.88930186190153,
9.89190202184739,9.89635244352137,9.95673900561715),.UNSPECIFIED.);
#3478=B_SPLINE_CURVE_WITH_KNOTS('',3,(#71022,#71023,#71024,#71025,#71026,
#71027,#71028,#71029,#71030,#71031,#71032,#71033,#71034,#71035,#71036,#71037,
#71038,#71039,#71040,#71041,#71042,#71043,#71044,#71045,#71046,#71047,#71048,
#71049,#71050,#71051,#71052,#71053,#71054,#71055,#71056,#71057,#71058,#71059,
#71060,#71061,#71062,#71063,#71064,#71065,#71066,#71067,#71068,#71069,#71070,
#71071,#71072,#71073,#71074,#71075,#71076,#71077,#71078,#71079,#71080,#71081,
#71082,#71083,#71084,#71085,#71086,#71087,#71088,#71089,#71090,#71091,#71092,
#71093,#71094,#71095,#71096,#71097,#71098,#71099,#71100,#71101,#71102,#71103,
#71104,#71105,#71106,#71107,#71108,#71109,#71110,#71111,#71112,#71113,#71114,
#71115,#71116,#71117,#71118,#71119,#71120,#71121,#71122,#71123,#71124,#71125,
#71126,#71127,#71128,#71129,#71130,#71131,#71132,#71133,#71134,#71135,#71136,
#71137,#71138,#71139,#71140,#71141,#71142,#71143,#71144,#71145,#71146,#71147,
#71148,#71149,#71150,#71151,#71152,#71153,#71154,#71155,#71156,#71157,#71158,
#71159,#71160,#71161,#71162,#71163,#71164,#71165,#71166,#71167,#71168,#71169,
#71170,#71171,#71172,#71173,#71174,#71175,#71176,#71177,#71178,#71179,#71180,
#71181,#71182,#71183,#71184,#71185,#71186,#71187,#71188,#71189,#71190,#71191,
#71192,#71193,#71194,#71195,#71196,#71197,#71198,#71199,#71200,#71201,#71202,
#71203,#71204,#71205,#71206,#71207,#71208,#71209,#71210,#71211,#71212,#71213,
#71214,#71215,#71216,#71217,#71218,#71219,#71220,#71221,#71222,#71223,#71224,
#71225,#71226,#71227,#71228,#71229,#71230,#71231,#71232,#71233,#71234,#71235,
#71236,#71237,#71238,#71239,#71240,#71241,#71242,#71243,#71244,#71245,#71246,
#71247,#71248,#71249,#71250,#71251,#71252,#71253,#71254,#71255,#71256,#71257,
#71258,#71259,#71260,#71261,#71262,#71263,#71264,#71265,#71266,#71267,#71268,
#71269,#71270,#71271,#71272,#71273,#71274,#71275,#71276,#71277,#71278,#71279,
#71280,#71281,#71282,#71283,#71284,#71285,#71286,#71287,#71288,#71289,#71290,
#71291,#71292,#71293,#71294,#71295,#71296,#71297,#71298,#71299,#71300,#71301,
#71302,#71303,#71304,#71305,#71306,#71307,#71308,#71309,#71310,#71311,#71312,
#71313,#71314,#71315,#71316,#71317,#71318,#71319,#71320,#71321,#71322,#71323,
#71324,#71325,#71326,#71327,#71328,#71329,#71330,#71331,#71332,#71333,#71334,
#71335,#71336,#71337,#71338,#71339,#71340,#71341,#71342,#71343,#71344,#71345,
#71346,#71347,#71348,#71349,#71350,#71351,#71352,#71353,#71354,#71355,#71356,
#71357,#71358,#71359,#71360,#71361,#71362,#71363,#71364,#71365,#71366,#71367,
#71368,#71369,#71370,#71371,#71372,#71373,#71374,#71375,#71376,#71377,#71378,
#71379,#71380,#71381,#71382,#71383,#71384,#71385,#71386,#71387,#71388,#71389,
#71390,#71391,#71392,#71393,#71394,#71395,#71396,#71397,#71398,#71399,#71400,
#71401,#71402,#71403,#71404,#71405,#71406,#71407,#71408,#71409,#71410,#71411,
#71412,#71413,#71414,#71415,#71416,#71417,#71418,#71419,#71420,#71421,#71422,
#71423,#71424,#71425,#71426,#71427,#71428,#71429,#71430,#71431,#71432,#71433,
#71434,#71435,#71436,#71437,#71438,#71439,#71440,#71441,#71442,#71443,#71444,
#71445,#71446,#71447,#71448,#71449,#71450,#71451,#71452,#71453,#71454,#71455,
#71456,#71457,#71458,#71459,#71460,#71461,#71462,#71463,#71464,#71465,#71466,
#71467,#71468,#71469,#71470,#71471,#71472,#71473,#71474,#71475,#71476,#71477,
#71478,#71479,#71480,#71481,#71482,#71483,#71484,#71485,#71486,#71487,#71488,
#71489,#71490,#71491,#71492,#71493,#71494,#71495,#71496,#71497,#71498,#71499,
#71500,#71501,#71502,#71503,#71504,#71505,#71506,#71507,#71508,#71509,#71510,
#71511,#71512,#71513,#71514,#71515,#71516,#71517,#71518,#71519,#71520,#71521,
#71522,#71523,#71524,#71525),.UNSPECIFIED.,.F.,.F.,(4,2,2,2,2,2,2,2,2,2,
2,2,2,2,2,2,2,2,2,2,2,2,2,2,2,2,2,2,2,2,2,2,2,2,2,2,2,2,2,2,2,2,2,2,2,2,
2,2,2,2,2,2,2,2,2,2,2,2,2,2,2,2,2,2,2,2,2,2,2,2,2,2,2,2,2,2,2,2,2,2,2,2,
2,2,2,2,2,2,2,2,2,2,2,2,2,2,2,2,2,2,2,2,2,2,2,2,2,2,2,2,2,2,2,2,2,2,2,2,
2,2,2,2,2,2,2,2,2,2,2,2,2,2,2,2,2,2,2,2,2,2,2,2,2,2,2,2,2,2,2,2,2,2,2,2,
2,2,2,2,2,2,2,2,2,2,2,2,2,2,2,2,2,2,2,2,2,2,2,2,2,2,2,2,2,2,2,2,2,2,2,2,
2,2,2,2,2,2,2,2,2,2,2,2,2,2,2,2,2,2,2,2,2,2,2,2,2,2,2,2,2,2,2,2,2,2,2,2,
2,2,2,2,2,2,2,2,2,2,2,2,2,2,2,2,2,2,2,2,2,2,2,2,2,4),(0.00251010222491945,
0.243787391938942,0.303585856625084,0.334265125341356,0.339783302168653,
0.342731196990903,0.344928651576325,0.347678715786094,0.3522958866643,0.367677234091077,
0.665375547270404,0.719529836939747,0.753106403301528,0.757805985350203,
0.760250090460091,0.76217375969946,0.764103766158577,0.76746238785199,0.776997208265284,
0.821072968260817,0.827425971333189,0.993027291007421,1.09349735049628,
1.16892839688559,1.1888067752484,1.19864822603004,1.20575936414824,1.21336448320816,
1.22653290570935,1.2649723820318,1.42001696008981,1.47913703997041,1.50759999993778,
1.5141869737241,1.51797399058619,1.52101238571232,1.52481872651664,1.5318846130407,
1.57414022287303,1.70078210174418,1.76721092418276,1.79310006757511,1.81253704887497,
1.82128950858579,1.82787420813396,1.8340828171777,1.84274982024407,1.86581413092087,
2.05981437474254,2.14034417212541,2.26694614174772,2.27276444203969,2.27742084528508,
2.27988431817427,2.28202981459984,2.28421901795791,2.28819874845734,2.30064121003661,
2.54839057286477,2.66730110349389,2.67668283694365,2.68025928556359,2.68271579951296,
2.68511649989536,2.68800225265757,2.69516952013211,2.75933417950786,2.88413027690822,
2.99667146727563,3.09510287243425,3.09927062972646,3.10105921414451,3.10236081307502,
3.10355184308957,3.10515108928364,3.10904212056815,3.15223125590808,3.36090907023271,
3.45193753704296,3.48750015054709,3.49273659358103,3.49541773321685,3.4973685061179,
3.49945461486889,3.50303073822689,3.51282882315481,3.66019078512744,3.74152808340484,
3.88874758038838,3.89558483034534,3.89766658668889,3.8989786908732,3.90020300531344,
3.90179632911577,3.90514044211941,3.92912546097264,4.00784067621214,4.21752717165338,
4.2823982203165,4.31359471287522,4.31882072478056,4.3215676574711,4.32359623307228,
4.32579446509543,4.32897150358384,4.33793103731674,4.47446455387964,4.54935502043155,
4.70042907417598,4.7111671047788,4.71448236650469,4.71656580958623,4.71848878622497,
4.72096259656022,4.72503398324502,4.74764638332562,4.86333868376048,4.98068554299978,
5.07608863377555,5.08723110589535,5.09273514103766,5.09668712426034,5.10087604412859,
5.10642261388538,5.11854635663474,5.27017147221037,5.43419298400449,5.4365305035406,
5.45685573816647,5.4604520103869,5.46262621580172,5.46430952145124,5.46612643741112,
5.46900275353824,5.47819225007716,5.53407272110727,5.60032482683932,5.65840683785703,
5.85671900096459,5.86912187188425,5.8733587166141,5.87575701510525,5.87795477467401,
5.88090786164873,5.88645125552013,5.91764970183465,5.97721099953278,6.15247583005955,
6.1946485071903,6.28093150267365,6.28816864312843,6.2908622399433,6.29276755757812,
6.29455863897503,6.29703568431977,6.30192831496201,6.3379244699221,6.4493918238998,
6.68995834198289,6.71660076234272,6.72682798178216,6.73425510724238,6.7422474801572,
6.75310850774865,6.77849032336773,6.81317417511326,6.91167960312419,7.02881368071915,
7.04204919188353,7.04670177144201,7.04991790532169,7.05288858733531,7.05691898099624,
7.06512729949014,7.07610674974359,7.20439964912853,7.330927269013,7.34601481188863,
7.35391560012106,7.36042224379344,7.36779311781667,7.38037858621192,7.43635714613673,
7.61417255428127,7.77095324968326,7.80275128373853,7.80771547691403,7.81064176492888,
7.81286564864252,7.8152263839659,7.81888312459723,7.8299603614273,7.88694314649619,
7.92111440052267,7.94682652387992,8.15137793326954,8.202012073061,8.20871835137869,
8.2118039707384,8.21417809096293,8.21667465695087,8.22054175137566,8.22505071786973,
8.23346362786466,8.25301875274464,8.30911523315822,8.38817373028602,8.53488096606999,
8.60600104584896,8.62697798083178,8.63034524485487,8.63198361762719,8.6332610889448,
8.63467014239525,8.63696687632437,8.64528009632667,8.70207682131942,8.77152871803475,
8.7920770617834,8.88521330564611,9.01157424389431,9.02096127464029,9.02447339770842,
9.02654638867801,9.02863016613432,9.03135243079927,9.03685380321987,9.04392303384984,
9.05987136615499,9.10697552250956,9.16472826375648,9.29460673284835,9.38594217404497,
9.42282230595951,9.42658272608822,9.42806498559548,9.42929890458283,9.43056714537261,
9.43242347950637,9.43734521202508,9.53928660437817,9.74725342253797,9.75959851262685,
9.84016579236699,9.84738741128452,9.85028499635874,9.8524073356124,9.85455428594291,
9.85677670138773,9.8596816472686,9.86426249311313,9.95742286907103),
 .UNSPECIFIED.);
#3479=B_SPLINE_CURVE_WITH_KNOTS('',3,(#71527,#71528,#71529,#71530,#71531,
#71532,#71533,#71534,#71535,#71536,#71537,#71538,#71539,#71540,#71541,#71542,
#71543,#71544,#71545,#71546,#71547,#71548,#71549,#71550,#71551,#71552,#71553,
#71554,#71555,#71556,#71557,#71558,#71559,#71560,#71561,#71562,#71563,#71564,
#71565,#71566,#71567,#71568,#71569,#71570,#71571,#71572,#71573,#71574,#71575,
#71576,#71577,#71578,#71579,#71580,#71581,#71582,#71583,#71584,#71585,#71586,
#71587,#71588,#71589,#71590,#71591,#71592,#71593,#71594,#71595,#71596,#71597,
#71598,#71599,#71600,#71601,#71602,#71603,#71604,#71605,#71606,#71607,#71608,
#71609,#71610,#71611,#71612,#71613,#71614,#71615,#71616,#71617,#71618,#71619,
#71620,#71621,#71622,#71623,#71624,#71625,#71626,#71627,#71628,#71629,#71630,
#71631,#71632,#71633,#71634,#71635,#71636,#71637,#71638,#71639,#71640,#71641,
#71642,#71643,#71644,#71645,#71646,#71647,#71648,#71649,#71650,#71651,#71652,
#71653,#71654,#71655,#71656,#71657,#71658,#71659,#71660,#71661,#71662,#71663,
#71664,#71665,#71666,#71667,#71668,#71669,#71670,#71671,#71672,#71673,#71674,
#71675,#71676,#71677,#71678,#71679,#71680,#71681,#71682,#71683,#71684,#71685,
#71686,#71687,#71688,#71689,#71690,#71691,#71692,#71693,#71694,#71695,#71696,
#71697,#71698,#71699,#71700,#71701,#71702,#71703,#71704,#71705,#71706,#71707,
#71708,#71709,#71710,#71711,#71712,#71713,#71714,#71715,#71716,#71717,#71718,
#71719,#71720,#71721,#71722,#71723,#71724,#71725,#71726,#71727,#71728,#71729,
#71730,#71731,#71732,#71733,#71734,#71735,#71736,#71737,#71738,#71739,#71740,
#71741,#71742,#71743,#71744,#71745,#71746,#71747,#71748,#71749,#71750,#71751,
#71752,#71753,#71754,#71755,#71756,#71757,#71758,#71759,#71760,#71761,#71762,
#71763,#71764,#71765,#71766,#71767,#71768,#71769,#71770,#71771,#71772,#71773,
#71774,#71775,#71776,#71777,#71778,#71779,#71780,#71781,#71782,#71783,#71784,
#71785,#71786,#71787,#71788,#71789,#71790,#71791,#71792,#71793,#71794,#71795,
#71796,#71797,#71798,#71799,#71800,#71801,#71802,#71803,#71804,#71805,#71806,
#71807,#71808,#71809,#71810,#71811,#71812,#71813,#71814,#71815,#71816,#71817,
#71818,#71819,#71820,#71821,#71822,#71823,#71824,#71825,#71826,#71827,#71828,
#71829,#71830,#71831,#71832,#71833,#71834,#71835,#71836,#71837,#71838,#71839,
#71840,#71841,#71842,#71843,#71844,#71845,#71846,#71847,#71848,#71849,#71850,
#71851,#71852,#71853,#71854,#71855,#71856,#71857,#71858,#71859,#71860,#71861,
#71862,#71863,#71864,#71865,#71866,#71867,#71868,#71869,#71870,#71871,#71872,
#71873,#71874,#71875,#71876,#71877,#71878,#71879,#71880,#71881,#71882,#71883,
#71884,#71885,#71886,#71887,#71888,#71889,#71890,#71891,#71892,#71893,#71894,
#71895,#71896,#71897,#71898,#71899,#71900,#71901,#71902,#71903,#71904,#71905,
#71906,#71907,#71908,#71909,#71910,#71911,#71912,#71913,#71914,#71915,#71916,
#71917,#71918,#71919,#71920,#71921,#71922,#71923,#71924,#71925,#71926,#71927,
#71928,#71929,#71930,#71931,#71932,#71933,#71934,#71935,#71936,#71937,#71938,
#71939,#71940,#71941,#71942,#71943,#71944,#71945,#71946,#71947,#71948,#71949,
#71950,#71951,#71952,#71953,#71954,#71955,#71956,#71957,#71958,#71959,#71960,
#71961,#71962,#71963,#71964,#71965,#71966,#71967,#71968,#71969,#71970,#71971,
#71972,#71973,#71974,#71975,#71976,#71977,#71978,#71979,#71980,#71981,#71982,
#71983,#71984,#71985,#71986,#71987,#71988,#71989,#71990,#71991,#71992,#71993,
#71994,#71995,#71996,#71997,#71998,#71999,#72000,#72001,#72002,#72003,#72004,
#72005,#72006,#72007,#72008,#72009,#72010,#72011,#72012,#72013,#72014,#72015,
#72016,#72017,#72018,#72019,#72020,#72021,#72022,#72023,#72024,#72025,#72026,
#72027,#72028,#72029,#72030,#72031,#72032,#72033,#72034,#72035,#72036,#72037,
#72038,#72039,#72040,#72041,#72042,#72043,#72044,#72045,#72046,#72047,#72048,
#72049,#72050,#72051,#72052,#72053,#72054,#72055,#72056),.UNSPECIFIED.,
 .F.,.F.,(4,2,2,2,2,2,2,2,2,2,2,2,2,2,2,2,2,2,2,2,2,2,2,2,2,2,2,2,2,2,2,
2,2,2,2,2,2,2,2,2,2,2,2,2,2,2,2,2,2,2,2,2,2,2,2,2,2,2,2,2,2,2,2,2,2,2,2,
2,2,2,2,2,2,2,2,2,2,2,2,2,2,2,2,2,2,2,2,2,2,2,2,2,2,2,2,2,2,2,2,2,2,2,2,
2,2,2,2,2,2,2,2,2,2,2,2,2,2,2,2,2,2,2,2,2,2,2,2,2,2,2,2,2,2,2,2,2,2,2,2,
2,2,2,2,2,2,2,2,2,2,2,2,2,2,2,2,2,2,2,2,2,2,2,2,2,2,2,2,2,2,2,2,2,2,2,2,
2,2,2,2,2,2,2,2,2,2,2,2,2,2,2,2,2,2,2,2,2,2,2,2,2,2,2,2,2,2,2,2,2,2,2,2,
2,2,2,2,2,2,2,2,2,2,2,2,2,2,2,2,2,2,2,2,2,2,2,2,2,2,2,2,2,2,2,2,2,2,2,2,
2,2,2,2,2,2,2,2,2,2,2,2,2,2,2,2,2,4),(0.00309469634645156,0.224719887751486,
0.262433627837547,0.285214875920883,0.289466113176118,0.291757187350233,
0.293474235860959,0.295359849641409,0.298722341888027,0.308803625459528,
0.549626391594619,0.642918507831922,0.662033156729555,0.668799520237496,
0.673227324591152,0.67735443317442,0.682852864260989,0.694580657859646,
0.812759013597112,1.01883049575864,1.03426833278783,1.03771171899465,1.0396554936354,
1.04115232103902,1.04309216526864,1.04642720178532,1.0592142306045,1.28282484245239,
1.35265975418497,1.41249861493508,1.43278181691983,1.44150342361149,1.44817114029072,
1.45134673197699,1.45381104455684,1.45614459990585,1.4594026790858,1.46605918984373,
1.53151068475513,1.66512180306669,1.76645673300713,1.85877163432735,1.86537200414604,
1.86817197563305,1.87019871776286,1.87204727014748,1.87452132427924,1.88082548367989,
1.98034717375737,2.10112255881258,2.27221666046685,2.29546951003967,2.30592719309536,
2.31385709756275,2.32219156103465,2.33522503618132,2.37459332398833,2.5286672647815,
2.61108190335055,2.62064894285417,2.62504537978011,2.62837252159074,2.63151223062196,
2.63590168280702,2.64900532091202,2.78209897772558,2.90815257233216,2.92330003024977,
2.93122200645702,2.93708820872066,2.94421158040537,2.9558308356711,2.99638804728661,
3.11090925815809,3.27623062293508,3.37678768202605,3.38416999129581,3.38728417606207,
3.38953251963091,3.3915778656314,3.39430741218754,3.40095041360982,3.46486382262876,
3.68947080484061,3.74907612239742,3.78107720553494,3.78650640920955,3.78936881130532,
3.79171218456978,3.79441929102231,3.79901266879074,3.81564653179389,4.11578768838679,
4.1637054322703,4.20058417583274,4.20711678014725,4.2092549857036,4.21062907802626,
4.21191845006874,4.2136066843205,4.21735441760319,4.25182846441527,4.49704387422664,
4.56526773305332,4.59653605460805,4.60160542766454,4.60425137813528,4.60640387838646,
4.60855647492885,4.61246543439191,4.62465802407176,4.811918192958,4.93023847044749,
4.98209070115221,5.00243293872193,5.00561094204973,5.007149990671,5.00836273374973,
5.00971628922986,5.01195907799621,5.02005971781845,5.07391517684984,5.13239006679914,
5.35824453427294,5.41978632594383,5.42666026502501,5.42942482998162,5.43172342319774,
5.43407408342837,5.43749381958586,5.44644882676684,5.56309423210432,5.78056665645007,
5.81695700212397,5.82208040794227,5.82452443071683,5.8264434546441,5.82854181405301,
5.83192278327131,5.843248492938,5.91829036322231,6.05515733954,6.18411661874727,
6.19587202496579,6.2015348668477,6.20552982875455,6.20970067724296,6.21511829421865,
6.22655730815366,6.40117302670314,6.52695079547495,6.53299776476238,6.56501597657014,
6.56959898718664,6.57175640007582,6.57343740542144,6.57526257129168,6.57817498867056,
6.58767707680309,6.64701878425076,6.82690648528476,6.9697968914167,6.97925218850127,
6.98265892355394,6.98503275984224,6.98723645608052,6.99024055115944,6.99602375843549,
7.03261853306109,7.11511872343908,7.26404271985294,7.3889518932205,7.39704502058058,
7.40018454020166,7.40206974185838,7.40406969127019,7.40671417659079,7.41245584296766,
7.52905549586341,7.61604258409039,7.79764505975827,7.82524305582067,7.83560981363484,
7.84307294750416,7.85026364059302,7.86029388583745,7.87127442237592,7.88940235554483,
8.01638831306692,8.13822056002897,8.15122007998795,8.15583773937631,8.15904445601183,
8.16201788539676,8.16515289989451,8.17150897411593,8.20866382550621,8.30871545843223,
8.44012717552391,8.45391861469426,8.46230348423881,8.46869222771516,8.46872718864108,
8.46876105285513,8.46879384137152,8.4688255952888,8.46885635440215,8.46888615175129,
8.46890916974447,8.46893201552123,8.468954689056,8.46897719200031,8.46899952597806,
8.46902169262842,8.46904369352656,8.46906553025354,8.46908720432959,8.46910871734257,
8.4691300708164,8.46915126624619,8.46917230513227,8.46919318894168,8.46921391910887,
8.46923449708225,8.46925492429996,8.47621949401905,8.48770710851714,8.50159772175201,
8.52958141995862,8.61050599383194,8.71797921403125,8.89001164282994,8.89591080933983,
8.90534597246996,8.91536689607916,8.91900733887831,8.92113024104654,8.92311505307131,
8.92584282379479,8.93117600392541,8.96899290060652,9.01363917538949,9.07123810151026,
9.12804824249409,9.30504596556728,9.31609810353664,9.32004985896535,9.32233348697841,
9.32445534686691,9.32735075169056,9.33293444719636,9.36853840224448,9.46500284625107,
9.4967972322281,9.52913341068263,9.71290888733782,9.73640839333331,9.73989425423439,
9.74153865014484,9.742821111323,9.74421446735353,9.74643924439886,9.75400969021246,
9.80253514951666,9.95802914947034),.UNSPECIFIED.);
#3480=B_SPLINE_CURVE_WITH_KNOTS('',3,(#72058,#72059,#72060,#72061,#72062,
#72063,#72064,#72065,#72066,#72067,#72068,#72069,#72070,#72071,#72072,#72073,
#72074,#72075),.UNSPECIFIED.,.F.,.F.,(4,2,2,2,2,2,2,2,4),(277.583802222045,
278.41871913394,279.253636045835,280.08855295773,280.923469869625,281.75838678152,
282.593303693415,283.42822060531,283.866987529225),.UNSPECIFIED.);
#3481=B_SPLINE_CURVE_WITH_KNOTS('',3,(#72077,#72078,#72079,#72080,#72081,
#72082,#72083,#72084,#72085,#72086,#72087,#72088,#72089,#72090,#72091,#72092,
#72093,#72094,#72095,#72096,#72097,#72098,#72099,#72100,#72101,#72102,#72103,
#72104,#72105,#72106,#72107,#72108,#72109,#72110,#72111,#72112,#72113,#72114,
#72115,#72116,#72117,#72118,#72119,#72120,#72121,#72122,#72123,#72124,#72125,
#72126,#72127,#72128,#72129,#72130,#72131,#72132,#72133,#72134,#72135,#72136,
#72137,#72138,#72139,#72140,#72141,#72142,#72143,#72144,#72145,#72146,#72147,
#72148,#72149,#72150,#72151,#72152,#72153,#72154,#72155,#72156,#72157,#72158,
#72159,#72160,#72161,#72162,#72163,#72164,#72165,#72166,#72167,#72168,#72169,
#72170,#72171,#72172,#72173,#72174,#72175,#72176,#72177,#72178,#72179,#72180,
#72181,#72182,#72183,#72184,#72185,#72186,#72187,#72188,#72189,#72190,#72191,
#72192,#72193,#72194,#72195,#72196,#72197,#72198,#72199,#72200,#72201,#72202,
#72203,#72204,#72205,#72206,#72207,#72208,#72209,#72210,#72211,#72212,#72213,
#72214,#72215,#72216,#72217,#72218,#72219,#72220,#72221,#72222,#72223,#72224,
#72225,#72226,#72227,#72228,#72229,#72230,#72231,#72232,#72233,#72234,#72235,
#72236,#72237,#72238,#72239,#72240,#72241,#72242,#72243,#72244,#72245,#72246,
#72247,#72248,#72249,#72250,#72251,#72252,#72253,#72254,#72255,#72256,#72257,
#72258,#72259,#72260,#72261,#72262,#72263,#72264,#72265,#72266,#72267,#72268,
#72269,#72270,#72271,#72272,#72273,#72274,#72275,#72276,#72277,#72278,#72279,
#72280,#72281,#72282,#72283,#72284,#72285,#72286,#72287,#72288,#72289,#72290,
#72291,#72292,#72293,#72294,#72295,#72296,#72297,#72298,#72299,#72300,#72301,
#72302,#72303,#72304,#72305,#72306,#72307,#72308,#72309,#72310,#72311,#72312,
#72313,#72314,#72315,#72316,#72317,#72318,#72319,#72320,#72321,#72322,#72323,
#72324,#72325,#72326,#72327,#72328,#72329,#72330,#72331,#72332,#72333,#72334,
#72335,#72336,#72337,#72338,#72339,#72340,#72341,#72342,#72343,#72344,#72345,
#72346,#72347,#72348,#72349,#72350,#72351,#72352,#72353,#72354,#72355,#72356,
#72357,#72358,#72359,#72360,#72361,#72362,#72363,#72364,#72365,#72366,#72367,
#72368,#72369,#72370,#72371,#72372,#72373,#72374,#72375,#72376,#72377,#72378,
#72379,#72380,#72381,#72382,#72383,#72384,#72385,#72386,#72387,#72388,#72389,
#72390,#72391,#72392,#72393,#72394,#72395,#72396,#72397,#72398,#72399,#72400,
#72401,#72402,#72403,#72404,#72405,#72406,#72407,#72408,#72409,#72410,#72411,
#72412,#72413,#72414,#72415,#72416,#72417,#72418,#72419,#72420,#72421,#72422,
#72423,#72424,#72425,#72426,#72427,#72428,#72429,#72430,#72431,#72432,#72433,
#72434,#72435,#72436,#72437,#72438,#72439,#72440,#72441,#72442,#72443,#72444,
#72445,#72446,#72447,#72448,#72449,#72450,#72451,#72452,#72453,#72454,#72455,
#72456,#72457,#72458,#72459,#72460,#72461,#72462,#72463,#72464,#72465,#72466,
#72467,#72468,#72469,#72470,#72471,#72472,#72473,#72474,#72475,#72476,#72477,
#72478,#72479,#72480,#72481,#72482,#72483,#72484,#72485,#72486,#72487,#72488,
#72489,#72490,#72491,#72492,#72493,#72494,#72495,#72496,#72497,#72498,#72499,
#72500,#72501,#72502,#72503,#72504,#72505,#72506,#72507,#72508,#72509,#72510,
#72511,#72512,#72513,#72514,#72515,#72516,#72517,#72518,#72519,#72520,#72521,
#72522,#72523,#72524,#72525,#72526,#72527,#72528,#72529,#72530,#72531,#72532,
#72533,#72534,#72535,#72536,#72537,#72538,#72539,#72540,#72541,#72542,#72543,
#72544,#72545,#72546,#72547,#72548,#72549,#72550,#72551,#72552,#72553,#72554,
#72555,#72556,#72557,#72558,#72559,#72560,#72561,#72562,#72563,#72564,#72565,
#72566,#72567,#72568,#72569,#72570,#72571,#72572,#72573,#72574,#72575,#72576,
#72577,#72578,#72579,#72580,#72581,#72582,#72583,#72584,#72585,#72586,#72587,
#72588,#72589,#72590,#72591,#72592,#72593,#72594,#72595,#72596,#72597,#72598,
#72599,#72600,#72601,#72602),.UNSPECIFIED.,.F.,.F.,(4,2,2,2,2,2,2,2,2,2,
2,2,2,2,2,2,2,2,2,2,2,2,2,2,2,2,2,2,2,2,2,2,2,2,2,2,2,2,2,2,2,2,2,2,2,2,
2,2,2,2,2,2,2,2,2,2,2,2,2,2,2,2,2,2,2,2,2,2,2,2,2,2,2,2,2,2,2,2,2,2,2,2,
2,2,2,2,2,2,2,2,2,2,2,2,2,2,2,2,2,2,2,2,2,2,2,2,2,2,2,2,2,2,2,2,2,2,2,2,
2,2,2,2,2,2,2,2,2,2,2,2,2,2,2,2,2,2,2,2,2,2,2,2,2,2,2,2,2,2,2,2,2,2,2,2,
2,2,2,2,2,2,2,2,2,2,2,2,2,2,2,2,2,2,2,2,2,2,2,2,2,2,2,2,2,2,2,2,2,2,2,2,
2,2,2,2,2,2,2,2,2,2,2,2,2,2,2,2,2,2,2,2,2,2,2,2,2,2,2,2,2,2,2,2,2,2,2,2,
2,2,2,2,2,2,2,2,2,2,2,2,2,2,2,2,2,2,2,2,2,2,2,2,2,2,2,2,2,2,2,2,2,2,2,2,
4),(0.00198225243763518,0.266615072056633,0.314441300500113,0.334641517799556,
0.337708435595375,0.339286156902143,0.34043680491537,0.341669770816142,
0.343427590865343,0.348341092477681,0.430473500897858,0.483897354527935,
0.60921972497755,0.712024641181708,0.722038038549978,0.727042778428079,
0.730085961804466,0.732856084557811,0.734989039660594,0.737054349361429,
0.739944730530766,0.747532377017718,0.862309904946988,0.924634325421874,
1.03559976262637,1.13064497942464,1.13430874801485,1.13593891570679,1.13716391827038,
1.13831649649319,1.13991360821256,1.14313898836948,1.17228018560106,1.21761096157214,
1.4459763678948,1.5183423097778,1.54000712921983,1.54899459573558,1.5536716600765,
1.55758630132628,1.56004427966134,1.56229971101897,1.56516709850484,1.56969331072979,
1.59192903224698,1.75936817351546,1.87253162650479,1.92331778826061,1.94727193321419,
1.95158208883212,1.9538857748097,1.95578821732426,1.95800480438475,1.96181298087984,
1.97613406469955,2.12485827810235,2.23372919887249,2.30804055964423,2.32472192340326,
2.33110904665255,2.33545633208363,2.33965478370078,2.34470846983821,2.3564289454588,
2.47462750722216,2.680710954984,2.69615950032377,2.69960385795793,2.70154795524276,
2.70304492550759,2.70473051940944,2.70785668537208,2.71814549595555,2.87832043608914,
3.0144889970319,3.07435018640052,3.10522771842819,3.11075707410745,3.11370794239236,
3.11590631965682,3.11865585281012,3.12326811748487,3.13859965815366,3.3976220229261,
3.45822810659263,3.51584845164515,3.52643624975621,3.52981042887143,3.53195783349664,
3.53395884418568,3.53656025493411,3.54090255764027,3.56664961729996,3.77085053262592,
3.93525659107231,3.95824445959824,3.96865763316827,3.97658295715926,3.98413755300539,
3.9970411790911,4.03365134483239,4.04020249684436,4.13416726246233,4.24056174647398,
4.26004278481672,4.27339291106414,4.2831935789027,4.28763405210317,4.29096872969093,
4.29409671977725,4.29843686622211,4.31102664746692,4.43651056067615,4.57075285843747,
4.58598576323042,4.59392662578966,4.59979612478252,4.60618422209085,4.61749963670284,
4.65262195319419,4.86021660274821,4.98116045187684,5.04111614054903,5.04757498980902,
5.05049251097247,5.05271575208749,5.05508160058148,5.05875810647169,5.06998444302561,
5.22674932224136,5.30159467473023,5.43852673742968,5.44749505364594,5.45075479126959,
5.45303488796546,5.45515843067035,5.45806376850237,5.4636928368299,5.50043471317159,
5.58466896581577,5.67639352389981,5.7188608708688,5.7698112880867,5.82148422408315,
5.82742769798544,5.86621604705074,5.8702289973981,5.87181440906204,5.87300224097223,
5.87430740876504,5.87611457455958,5.88044499963987,5.9769466772595,6.16188931190439,
6.20406072287318,6.25658624508628,6.26233272291347,6.26517834142509,6.26723170262753,
6.26941409851677,6.27230741377316,6.27861468613636,6.3813668760207,6.54084947979132,
6.61003418774181,6.62354643585024,6.63384254405937,6.66400913015447,6.66757269096298,
6.66916728573966,6.67039116971523,6.67170539942978,6.67377107641829,6.68024182919464,
6.71759161580657,6.7722359060442,6.92261475698076,7.07730472686564,7.08736225664695,
7.09106793264123,7.09323924909741,7.09527595478646,7.09808501897963,7.10360597228759,
7.14243030451987,7.23734819603142,7.38358283627325,7.47567261873065,7.48297160925171,
7.48561972276589,7.4874711020023,7.489194170405,7.49155007210844,7.49601658005833,
7.5238281934931,7.58604186629975,7.83506009462097,7.85611928487344,7.86344239835313,
7.8675385485098,7.87126845106183,7.87615153375793,7.88506898416066,7.89607581049333,
7.97269604367384,8.11205672686641,8.17961394039693,8.21188191530798,8.21793454416393,
8.2295247890045,8.23276036223944,8.23467649113636,8.23634112964606,8.23838203712901,
8.24227615455492,8.24708830857299,8.2574063793657,8.28836137685172,8.32992307416076,
8.42689301207743,8.62756784135761,8.64049819772866,8.64480723530506,8.64722034940708,
8.64941605330347,8.65234340316962,8.65776510825396,8.68657565691866,8.74316135186546,
8.78404525961025,8.86783976403443,8.91949911711619,9.04951659666925,9.05889847716958,
9.06223723304688,9.0641616489134,9.0659473004337,9.06838078613387,9.07306261287258,
9.10239780555826,9.17284454773263,9.24973913035732,9.36264035722129,9.38650447145289,
9.4718304670089,9.49149272889614,9.50141955536032,9.50928400021423,9.51661192825482,
9.52526030213393,9.55106232405648,9.62837413482203,9.69183076576367,9.79954507771061,
9.81309704146065,9.81831218670084,9.82144892687799,9.82458699357909,9.82779203661205,
9.83193125727591,9.83870063406499,9.85258264854099,9.95778309923622),
 .UNSPECIFIED.);
#3482=B_SPLINE_CURVE_WITH_KNOTS('',3,(#72604,#72605,#72606,#72607,#72608,
#72609,#72610,#72611,#72612,#72613,#72614,#72615),.UNSPECIFIED.,.F.,.F.,
(4,1,1,1,1,1,1,1,1,4),(296.433358143584,296.768858444156,297.267629634818,
298.265172016143,299.262714397468,300.260256778793,300.759027969455,301.257799160118,
302.255341541442,302.716255299813),.UNSPECIFIED.);
#3483=B_SPLINE_CURVE_WITH_KNOTS('',3,(#72617,#72618,#72619,#72620,#72621,
#72622,#72623,#72624,#72625,#72626,#72627,#72628,#72629,#72630,#72631,#72632,
#72633,#72634,#72635,#72636,#72637,#72638,#72639,#72640,#72641,#72642,#72643,
#72644,#72645,#72646,#72647,#72648,#72649,#72650,#72651,#72652,#72653,#72654,
#72655,#72656,#72657,#72658,#72659,#72660,#72661,#72662,#72663,#72664,#72665,
#72666,#72667,#72668,#72669,#72670,#72671,#72672,#72673,#72674,#72675,#72676,
#72677,#72678,#72679,#72680,#72681,#72682,#72683,#72684,#72685,#72686,#72687,
#72688,#72689,#72690,#72691,#72692,#72693,#72694,#72695,#72696,#72697,#72698,
#72699,#72700,#72701,#72702,#72703,#72704,#72705,#72706,#72707,#72708,#72709,
#72710,#72711,#72712,#72713,#72714,#72715,#72716,#72717,#72718,#72719,#72720,
#72721,#72722,#72723,#72724,#72725,#72726,#72727,#72728,#72729,#72730,#72731,
#72732,#72733,#72734,#72735,#72736,#72737,#72738,#72739,#72740,#72741,#72742,
#72743,#72744,#72745,#72746,#72747,#72748,#72749,#72750,#72751,#72752,#72753,
#72754,#72755,#72756,#72757,#72758,#72759,#72760,#72761,#72762,#72763,#72764,
#72765,#72766,#72767,#72768,#72769,#72770,#72771,#72772,#72773,#72774,#72775,
#72776,#72777,#72778,#72779,#72780,#72781,#72782,#72783,#72784,#72785,#72786,
#72787,#72788,#72789,#72790,#72791,#72792,#72793,#72794,#72795,#72796,#72797,
#72798,#72799,#72800,#72801,#72802,#72803,#72804,#72805,#72806,#72807,#72808,
#72809,#72810,#72811,#72812,#72813,#72814,#72815,#72816,#72817,#72818,#72819,
#72820,#72821,#72822,#72823,#72824,#72825,#72826,#72827,#72828,#72829,#72830,
#72831,#72832,#72833,#72834,#72835,#72836,#72837,#72838,#72839,#72840,#72841,
#72842,#72843,#72844,#72845,#72846,#72847,#72848,#72849,#72850,#72851,#72852,
#72853,#72854,#72855,#72856,#72857,#72858,#72859,#72860,#72861,#72862,#72863,
#72864,#72865,#72866,#72867,#72868,#72869,#72870,#72871,#72872,#72873,#72874,
#72875,#72876,#72877,#72878,#72879,#72880,#72881,#72882,#72883,#72884,#72885,
#72886,#72887,#72888,#72889,#72890,#72891,#72892,#72893,#72894,#72895,#72896,
#72897,#72898,#72899,#72900,#72901,#72902,#72903,#72904,#72905,#72906,#72907,
#72908,#72909,#72910,#72911,#72912,#72913,#72914,#72915,#72916,#72917,#72918,
#72919,#72920,#72921,#72922,#72923,#72924,#72925,#72926,#72927,#72928,#72929,
#72930,#72931,#72932,#72933,#72934,#72935,#72936,#72937,#72938,#72939,#72940,
#72941,#72942,#72943,#72944,#72945,#72946,#72947,#72948,#72949,#72950,#72951,
#72952,#72953,#72954,#72955,#72956,#72957,#72958,#72959,#72960,#72961,#72962,
#72963,#72964,#72965,#72966,#72967,#72968,#72969,#72970,#72971,#72972,#72973,
#72974,#72975,#72976,#72977,#72978,#72979,#72980,#72981,#72982,#72983,#72984,
#72985,#72986,#72987,#72988,#72989,#72990,#72991,#72992,#72993,#72994,#72995,
#72996,#72997,#72998,#72999,#73000,#73001,#73002,#73003,#73004,#73005,#73006,
#73007,#73008,#73009,#73010,#73011,#73012,#73013,#73014,#73015,#73016,#73017,
#73018,#73019,#73020,#73021,#73022,#73023,#73024,#73025,#73026,#73027,#73028,
#73029,#73030,#73031,#73032,#73033,#73034,#73035,#73036,#73037,#73038,#73039,
#73040,#73041,#73042,#73043,#73044,#73045,#73046,#73047,#73048,#73049,#73050,
#73051,#73052,#73053,#73054,#73055,#73056,#73057,#73058,#73059,#73060,#73061,
#73062,#73063,#73064,#73065,#73066,#73067,#73068,#73069,#73070,#73071,#73072,
#73073,#73074,#73075,#73076,#73077,#73078,#73079,#73080,#73081,#73082,#73083,
#73084,#73085,#73086,#73087,#73088,#73089,#73090,#73091,#73092,#73093,#73094,
#73095,#73096,#73097,#73098,#73099,#73100,#73101,#73102,#73103,#73104,#73105,
#73106,#73107,#73108,#73109,#73110,#73111,#73112,#73113,#73114,#73115,#73116,
#73117,#73118,#73119,#73120,#73121,#73122,#73123,#73124,#73125,#73126,#73127,
#73128,#73129,#73130,#73131,#73132,#73133,#73134,#73135,#73136,#73137,#73138,
#73139,#73140,#73141,#73142,#73143,#73144,#73145,#73146,#73147,#73148,#73149,
#73150,#73151,#73152,#73153,#73154,#73155,#73156,#73157,#73158,#73159,#73160,
#73161,#73162,#73163,#73164,#73165,#73166,#73167,#73168,#73169,#73170,#73171,
#73172,#73173,#73174,#73175,#73176,#73177,#73178,#73179,#73180),
 .UNSPECIFIED.,.F.,.F.,(4,2,2,2,2,2,2,2,2,2,2,2,2,2,2,2,2,2,2,2,2,2,2,2,
2,2,2,2,2,2,2,2,2,2,2,2,2,2,2,2,2,2,2,2,2,2,2,2,2,2,2,2,2,2,2,2,2,2,2,2,
2,2,2,2,2,2,2,2,2,2,2,2,2,2,2,2,2,2,2,2,2,2,2,2,2,2,2,2,2,2,2,2,2,2,2,2,
2,2,2,2,2,2,2,2,2,2,2,2,2,2,2,2,2,2,2,2,2,2,2,2,2,2,2,2,2,2,2,2,2,2,2,2,
2,2,2,2,2,2,2,2,2,2,2,2,2,2,2,2,2,2,2,2,2,2,2,2,2,2,2,2,2,2,2,2,2,2,2,2,
2,2,2,2,2,2,2,2,2,2,2,2,2,2,2,2,2,2,2,2,2,2,2,2,2,2,2,2,2,2,2,2,2,2,2,2,
2,2,2,2,2,2,2,2,2,2,2,2,2,2,2,2,2,2,2,2,2,2,2,2,2,2,2,2,2,2,2,2,2,2,2,2,
2,2,2,2,2,2,2,2,2,2,2,2,2,2,2,2,2,2,2,2,2,2,2,2,2,2,2,2,2,2,2,2,2,2,2,2,
2,2,2,2,2,4),(0.00168353385591401,0.0498777725783733,0.079003186553249,
0.0895156419589813,0.0974007412312368,0.104915212734958,0.112289681583754,
0.124232755713915,0.154184803611029,0.204113212361754,0.390295019998446,
0.409493031083788,0.413812283128153,0.417094354289524,0.420423817961922,
0.423560710051339,0.427937381600568,0.440899503587822,0.545448952708169,
0.629479438484531,0.67755807686016,0.698309917290908,0.714482280281196,
0.722576845810815,0.728897071836187,0.735237297706495,0.746310083480894,
0.779527291000484,1.01324258215097,1.13599247224734,1.17232186988904,1.17762337879856,
1.18034426807877,1.18232680519458,1.18445023670214,1.18810136647382,1.19816950966103,
1.34640236540742,1.44865603901265,1.5675992262831,1.57695568485988,1.58052855253191,
1.58298454179852,1.58538623977395,1.58827501156116,1.59545928201116,1.66017201985687,
1.76921009663314,1.89063114455488,1.97243364729558,1.99685057948197,2.00005878378817,
2.00166569926628,2.00282040079342,2.00404168752873,2.00610208564028,2.01170845117154,
2.10070766806404,2.10077395529731,2.10091211990214,2.101187452584,2.10169349540269,
2.10251776573483,2.10368731986464,2.10516188595958,2.10687849259004,2.16980160606017,
2.28622622708861,2.37580530142592,2.38973034856071,2.39378866124825,2.39621455204496,
2.39837368431185,2.40108880468321,2.40531683540522,2.42510133383884,2.50604430803166,
2.53979261107383,2.68836841443852,2.74615531093579,2.77854810093646,2.79455970257573,
2.79730056715374,2.79875229629633,2.79994796798825,2.80136036330358,2.80379996790127,
2.81306464078964,2.95661978409542,3.09012507541166,3.14572114533918,3.20536908080192,
3.21652977092373,3.22025913287162,3.22267704257178,3.22496154657145,3.2279762319077,
3.23471489081541,3.29227508613932,3.35229405093857,3.52397726557653,3.59902294881875,
3.61115988384797,3.61462809852094,3.61674631861868,3.61866099038122,3.62110923163744,
3.62611839070542,3.65758831406184,3.840940533774,3.96295214523924,3.9853897282661,
3.99262099900004,3.99715105393213,4.00133071207611,4.00671403653279,4.0182776372746,
4.11500547720755,4.24014635113042,4.2790064466594,4.34882749600617,4.35568774037037,
4.36078926225323,4.36306815486034,4.36476261847292,4.36633886777264,4.36849514971075,
4.37275971680104,4.4176221802148,4.41952602532707,4.66314860298935,4.73354229690831,
4.76741381591787,4.77308291044379,4.77606327952662,4.77826454219667,4.78065027084908,
4.78482191023632,4.79676045438706,4.97994016275531,5.17538295130353,5.18789307138019,
5.19164138272884,5.19387207417756,5.19565326728428,5.19804262159615,5.20251436275363,
5.22754477696715,5.28427901639821,5.4901758164607,5.49888674407132,5.56953400597466,
5.59328173306116,5.61847426478226,5.62846629335407,5.63583652377428,5.64387655236454,
5.65500081752022,5.68197162116042,5.81136460128152,5.93029902217239,5.94345903054978,
5.94810132611293,5.95131527057692,5.954287739056,5.9583263358495,5.96657811711028,
5.97763113072634,6.10022074232059,6.23253370119179,6.24631816563436,6.25470193609506,
6.26125326417265,6.26841682978343,6.28004742930654,6.32259183306286,6.51678739911555,
6.66559673606709,6.69896007466199,6.70809118169648,6.7115927283139,6.71368805519725,
6.71590340827373,6.71882317805519,6.72512592889425,6.87167365461539,7.09459737471727,
7.10811816849245,7.11240626760737,7.11475750211263,7.11710211855158,7.11997486685529,
7.12545052913383,7.1584559018588,7.22847409834317,7.4551879189228,7.47858769823266,
7.51195871758507,7.522769412867,7.53106992517631,7.53351145478206,7.53480945510939,
7.5359515105539,7.53737866264054,7.53983876033695,7.55016936974492,7.64627327967203,
7.90652536288647,7.9225139827139,7.92680587190077,7.92930889939954,7.931459552461,
7.93406646017141,7.93895084429497,7.96616590176265,8.01841922259449,8.05164230803548,
8.07578157943914,8.22746345528132,8.30300532163895,8.32681226677966,8.3301004256536,
8.33166704303511,8.33288653224296,8.33421261027509,8.33628991055581,8.34283483538172,
8.35311217620763,8.38514955306603,8.47970781201078,8.67792042524294,8.7441485597068,
8.75045795653661,8.75350386494422,8.75566604118089,8.75770514333178,8.76053483818278,
8.76615843540553,8.80824886870022,8.91619915555595,8.93775711878854,8.95584827275764,
8.97141534766263,8.98504177726917,8.99713095477215,9.00799735478284,9.12288842701972,
9.14252623037617,9.14642127403559,9.14887136066608,9.15078580291964,9.15285952187365,
9.15619593669478,9.16017138664598,9.16787948793886,9.18699026160615,9.2423309841501,
9.37872978869866,9.47119618921288,9.47744072684706,9.51438152226805,9.52270159349194,
9.5279676107825,9.53211959901976,9.53675557002965,9.54446428009804,9.57313598191909,
9.71969638076577,9.8260614980944,9.83730722237228,9.84572006054629,9.85472697793631,
9.85935372777375,9.88924730077025,9.89374171754815,9.89590502436992,9.89758176239949,
9.89913672284857,9.9009334025763,9.90347438119731,9.907782335338,9.95796125064517),
 .UNSPECIFIED.);
#3484=B_SPLINE_CURVE_WITH_KNOTS('',3,(#73182,#73183,#73184,#73185,#73186,
#73187,#73188,#73189,#73190,#73191,#73192,#73193),.UNSPECIFIED.,.F.,.F.,
(4,1,1,1,1,1,1,1,1,4),(315.282914065123,316.220934879991,316.719706070653,
317.218477261316,317.717248451978,318.216019642641,319.213562023966,320.211104405291,
321.208646786615,321.566097918198),.UNSPECIFIED.);
#3485=B_SPLINE_CURVE_WITH_KNOTS('',3,(#73195,#73196,#73197,#73198,#73199,
#73200,#73201,#73202,#73203,#73204,#73205,#73206,#73207,#73208,#73209,#73210,
#73211,#73212,#73213,#73214,#73215,#73216,#73217,#73218,#73219,#73220,#73221,
#73222,#73223,#73224,#73225,#73226,#73227,#73228,#73229,#73230,#73231,#73232,
#73233,#73234,#73235,#73236,#73237,#73238,#73239,#73240,#73241,#73242,#73243,
#73244,#73245,#73246,#73247,#73248,#73249,#73250,#73251,#73252,#73253,#73254,
#73255,#73256,#73257,#73258,#73259,#73260,#73261,#73262,#73263,#73264,#73265,
#73266,#73267,#73268,#73269,#73270,#73271,#73272,#73273,#73274,#73275,#73276,
#73277,#73278,#73279,#73280,#73281,#73282,#73283,#73284,#73285,#73286,#73287,
#73288,#73289,#73290,#73291,#73292,#73293,#73294,#73295,#73296,#73297,#73298,
#73299,#73300,#73301,#73302,#73303,#73304,#73305,#73306,#73307,#73308,#73309,
#73310,#73311,#73312,#73313,#73314,#73315,#73316,#73317,#73318,#73319,#73320,
#73321,#73322,#73323,#73324,#73325,#73326,#73327,#73328,#73329,#73330,#73331,
#73332,#73333,#73334,#73335,#73336,#73337,#73338,#73339,#73340,#73341,#73342,
#73343,#73344,#73345,#73346,#73347,#73348,#73349,#73350,#73351,#73352,#73353,
#73354,#73355,#73356,#73357,#73358,#73359,#73360,#73361,#73362,#73363,#73364,
#73365,#73366,#73367,#73368,#73369,#73370,#73371,#73372,#73373,#73374,#73375,
#73376,#73377,#73378,#73379,#73380,#73381,#73382,#73383,#73384,#73385,#73386,
#73387,#73388,#73389,#73390,#73391,#73392,#73393,#73394,#73395,#73396,#73397,
#73398,#73399,#73400,#73401,#73402,#73403,#73404,#73405,#73406,#73407,#73408,
#73409,#73410,#73411,#73412,#73413,#73414,#73415,#73416,#73417,#73418,#73419,
#73420,#73421,#73422,#73423,#73424,#73425,#73426,#73427,#73428,#73429,#73430,
#73431,#73432,#73433,#73434,#73435,#73436,#73437,#73438,#73439,#73440,#73441,
#73442,#73443,#73444,#73445,#73446,#73447,#73448,#73449,#73450,#73451,#73452,
#73453),.UNSPECIFIED.,.F.,.F.,(4,3,3,3,3,3,3,3,3,3,3,3,3,3,3,3,3,3,3,3,
3,3,3,3,3,3,3,3,3,3,3,3,3,3,3,3,3,3,3,3,3,3,3,3,3,3,3,3,3,3,3,3,3,3,3,3,
3,3,3,3,3,3,3,3,3,3,3,3,3,3,3,3,3,3,3,3,3,3,3,3,3,3,3,3,3,3,4),(321.566099372302,
321.639562907717,321.707417977278,321.781834369621,321.856267530736,321.930729723134,
322.005273658581,322.07986197705,322.154554403333,322.20618916794,322.282764990038,
322.359273326325,322.43572511814,322.512131266634,322.588502640109,322.665406253753,
322.741748751244,322.818090793491,322.894442226529,322.971764557213,323.048188724363,
323.125960136814,323.203731549265,323.277523615233,323.351253473926,323.424934185762,
323.498579583122,323.572203530935,323.645831596629,323.702502739928,323.783929205766,
323.865490499842,323.949436357529,324.031269866712,324.116271898651,324.20127393059,
324.279707563597,324.358071614971,324.43637092051,324.514591494691,324.592762239732,
324.670875258101,324.700045121253,324.776415149011,324.852802028157,324.929215329136,
325.005697368984,325.082216747814,325.158818071272,325.198816311915,325.274202690607,
325.349527667363,325.42480405076,325.500044616947,325.575262117461,325.652899189433,
325.728126958421,325.803371452636,325.878644229176,325.953956858419,326.029358435394,
326.104812705547,326.180364874505,326.19635869324,326.269516707425,326.342586099395,
326.415581797685,326.488518661238,326.561411494871,326.634275063227,326.707137573486,
326.780003140076,326.852885105631,326.92579682345,326.99879421002,327.071838442305,
327.144992679506,327.193901074565,327.26973914768,327.345446257123,327.421075129875,
327.496636972093,327.572142950378,327.647597845216,327.723022264868,327.798430624931,
327.849284679482),.UNSPECIFIED.);
#3486=B_SPLINE_CURVE_WITH_KNOTS('',3,(#73455,#73456,#73457,#73458,#73459,
#73460,#73461,#73462,#73463,#73464,#73465,#73466,#73467,#73468,#73469,#73470,
#73471,#73472,#73473,#73474,#73475,#73476,#73477,#73478,#73479,#73480,#73481,
#73482,#73483,#73484,#73485,#73486,#73487,#73488,#73489,#73490,#73491,#73492,
#73493,#73494,#73495,#73496,#73497,#73498,#73499,#73500,#73501,#73502,#73503,
#73504,#73505,#73506,#73507,#73508,#73509,#73510,#73511,#73512,#73513,#73514,
#73515,#73516,#73517,#73518,#73519,#73520,#73521,#73522,#73523,#73524,#73525,
#73526,#73527,#73528,#73529,#73530,#73531,#73532,#73533,#73534,#73535,#73536,
#73537,#73538,#73539,#73540,#73541,#73542,#73543,#73544,#73545,#73546,#73547,
#73548,#73549,#73550,#73551,#73552,#73553,#73554,#73555,#73556,#73557,#73558,
#73559,#73560,#73561,#73562,#73563,#73564,#73565,#73566,#73567,#73568,#73569,
#73570,#73571,#73572,#73573,#73574,#73575,#73576,#73577,#73578,#73579,#73580,
#73581,#73582,#73583,#73584,#73585,#73586,#73587,#73588,#73589,#73590,#73591,
#73592,#73593,#73594,#73595,#73596,#73597,#73598,#73599,#73600,#73601,#73602,
#73603,#73604,#73605,#73606,#73607,#73608,#73609,#73610,#73611,#73612,#73613,
#73614,#73615,#73616,#73617,#73618,#73619,#73620,#73621,#73622,#73623,#73624,
#73625,#73626,#73627,#73628,#73629,#73630,#73631,#73632,#73633,#73634,#73635,
#73636,#73637,#73638,#73639,#73640,#73641,#73642,#73643,#73644,#73645,#73646,
#73647,#73648,#73649,#73650,#73651,#73652,#73653,#73654,#73655,#73656,#73657,
#73658,#73659,#73660,#73661,#73662,#73663,#73664,#73665,#73666,#73667,#73668,
#73669,#73670,#73671,#73672,#73673,#73674,#73675,#73676,#73677,#73678,#73679,
#73680,#73681,#73682,#73683,#73684,#73685,#73686,#73687,#73688,#73689,#73690,
#73691,#73692,#73693,#73694,#73695,#73696,#73697,#73698,#73699,#73700,#73701,
#73702,#73703,#73704,#73705,#73706,#73707,#73708,#73709,#73710,#73711,#73712,
#73713,#73714,#73715,#73716,#73717,#73718,#73719,#73720,#73721,#73722,#73723,
#73724,#73725,#73726,#73727,#73728,#73729,#73730,#73731,#73732,#73733,#73734,
#73735,#73736,#73737,#73738,#73739,#73740,#73741,#73742,#73743,#73744,#73745,
#73746,#73747,#73748,#73749,#73750,#73751,#73752,#73753,#73754,#73755,#73756,
#73757,#73758,#73759,#73760,#73761,#73762,#73763,#73764,#73765,#73766,#73767,
#73768,#73769,#73770,#73771,#73772,#73773,#73774,#73775,#73776,#73777,#73778,
#73779,#73780,#73781,#73782,#73783,#73784,#73785,#73786,#73787,#73788,#73789,
#73790,#73791,#73792,#73793,#73794,#73795,#73796,#73797,#73798,#73799,#73800,
#73801,#73802,#73803,#73804,#73805,#73806,#73807,#73808,#73809,#73810,#73811,
#73812,#73813,#73814,#73815,#73816,#73817,#73818,#73819,#73820,#73821,#73822,
#73823,#73824,#73825,#73826,#73827,#73828,#73829,#73830,#73831,#73832,#73833,
#73834,#73835,#73836,#73837,#73838,#73839,#73840,#73841,#73842,#73843,#73844,
#73845,#73846,#73847,#73848,#73849,#73850,#73851,#73852,#73853,#73854,#73855,
#73856,#73857,#73858,#73859,#73860,#73861,#73862,#73863,#73864,#73865,#73866,
#73867,#73868,#73869,#73870,#73871,#73872,#73873,#73874,#73875,#73876,#73877,
#73878,#73879,#73880,#73881,#73882,#73883,#73884,#73885,#73886,#73887,#73888,
#73889,#73890,#73891,#73892,#73893,#73894,#73895,#73896,#73897,#73898,#73899,
#73900,#73901,#73902,#73903,#73904,#73905,#73906,#73907,#73908,#73909,#73910,
#73911,#73912,#73913,#73914,#73915,#73916,#73917,#73918,#73919,#73920,#73921,
#73922,#73923,#73924,#73925,#73926,#73927,#73928,#73929,#73930,#73931,#73932,
#73933,#73934,#73935,#73936,#73937,#73938,#73939,#73940,#73941,#73942,#73943,
#73944,#73945,#73946,#73947,#73948,#73949,#73950),.UNSPECIFIED.,.F.,.F.,
(4,2,2,2,2,2,2,2,2,2,2,2,2,2,2,2,2,2,2,2,2,2,2,2,2,2,2,2,2,2,2,2,2,2,2,
2,2,2,2,2,2,2,2,2,2,2,2,2,2,2,2,2,2,2,2,2,2,2,2,2,2,2,2,2,2,2,2,2,2,2,2,
2,2,2,2,2,2,2,2,2,2,2,2,2,2,2,2,2,2,2,2,2,2,2,2,2,2,2,2,2,2,2,2,2,2,2,2,
2,2,2,2,2,2,2,2,2,2,2,2,2,2,2,2,2,2,2,2,2,2,2,2,2,2,2,2,2,2,2,2,2,2,2,2,
2,2,2,2,2,2,2,2,2,2,2,2,2,2,2,2,2,2,2,2,2,2,2,2,2,2,2,2,2,2,2,2,2,2,2,2,
2,2,2,2,2,2,2,2,2,2,2,2,2,2,2,2,2,2,2,2,2,2,2,2,2,2,2,2,2,2,2,2,2,2,2,2,
2,2,2,2,2,2,2,2,2,2,2,2,2,2,2,2,2,2,2,2,2,2,2,2,2,2,2,2,2,2,2,2,4),(0.00198922818128111,
0.236183877542624,0.272854307600681,0.294822807650427,0.299030406213339,
0.301312088887494,0.303028329272993,0.30491931832674,0.308308476588276,
0.318584789539833,0.559208678639797,0.652459493438587,0.67156912176654,
0.678334765277876,0.682762433727734,0.686889650910601,0.692388579016866,
0.704118744927879,0.822382316496041,1.02860731611399,1.04383306888064,1.04726138975409,
1.04920185227845,1.05069856678751,1.05264169890295,1.0559908342161,1.06894166926308,
1.30639838012157,1.3939299335222,1.43253332457032,1.44661779578641,1.45643706072953,
1.4601553805191,1.4624361584321,1.46490890829546,1.46814748561117,1.47528654622001,
1.53269229438039,1.68098511292506,1.79909040532422,1.84223199734028,1.87143150913627,
1.87605932057005,1.87848197893651,1.88045701740972,1.88243681468299,1.88604344122846,
1.8974279115671,2.05854355971327,2.18991595825875,2.28905433085235,2.30767206141563,
2.31726643519325,2.32434806478356,2.33318985934922,2.34753042178583,2.39885191546709,
2.40512897751166,2.49853317154152,2.588456026089,2.60745601719949,2.6205802810811,
2.63025107918723,2.63466719100882,2.63799770453316,2.64113213820639,2.6454993194314,
2.65837529646984,2.76719764834364,2.91729375116296,2.93278328648167,2.9407762474667,
2.9466508643795,2.95373159719259,2.96516426117223,3.00376511867622,3.21178573994249,
3.25897309158952,3.37706979077462,3.38446558967613,3.39344689395539,3.39681685337303,
3.39911628918255,3.40135218509615,3.40402551600192,3.41060475931895,3.50973555301615,
3.63104127870229,3.74590361341228,3.79008372879148,3.79596218226843,3.79891878581283,
3.8010488771777,3.80330714313027,3.80648785107587,3.81307509940703,3.88260556633153,
4.05562322016617,4.2040097025033,4.21541741319343,4.21802142936888,4.21949956439709,
4.22064155763814,4.22212632891757,4.22469123363908,4.23506271096358,4.41329212317539,
4.52199816333728,4.60387237982322,4.61000243473734,4.6128619386028,4.61503898019725,
4.61710227060373,4.61998570609533,4.62753195724338,4.73936091549275,4.92276967741616,
4.98071285511311,5.01094685390791,5.01451238828769,5.0161072648194,5.01733111634852,
5.01864507514235,5.02070983223992,5.02717379164662,5.0644619037052,5.1189502509723,
5.34045677191975,5.42803574855811,5.43541096081708,5.4383356882947,5.44046576788778,
5.44274815766424,5.44580575853961,5.45260005077582,5.61661074564287,5.81665138729238,
5.8287898116107,5.83241363952725,5.83456638341725,5.83628303512172,5.83858243497155,
5.84287425935348,5.86650944873605,5.91812446072802,6.13359423381958,6.19658530492327,
6.20752542067062,6.21287492770743,6.21704856225871,6.2215934740388,6.22889288984193,
6.25344306470296,6.47680113779414,6.57295769993393,6.57854740615174,6.58073665153315,
6.58232150842026,6.58401085926164,6.58625978128018,6.59119985802725,6.6946889010257,
6.84660903857566,6.98032329318788,6.98910616799941,6.99240792195616,6.99475325509561,
6.99696645441848,7.0000399965982,7.00615702996334,7.05242662136879,7.12328351322218,
7.2802246409017,7.29444222228421,7.40066858456703,7.40728160689274,7.40987433864081,
7.41175291418941,7.41375694874064,7.41642580659961,7.42229618074848,7.43016200465765,
7.51158729562236,7.61121233767283,7.80743060968919,7.83504689160474,7.84539478393793,
7.85285393545266,7.86067023627787,7.87104298152544,7.88252912544297,7.90189377934439,
7.94261746555521,8.09148070970994,8.15488619146199,8.16327541451296,8.16750021120826,
8.17080389293221,8.17386363203754,8.17925342636621,8.19857936923149,8.23324694023105,
8.43769230459801,8.46089409090767,8.46960139265026,8.47582013150466,8.48226225872685,
8.49010033441227,8.5068702301573,8.52925831275699,8.58669913376713,8.7465037095287,
8.90657701057071,8.91604544717839,8.92549838760043,8.92905162308387,8.93115696268724,
8.93336756206607,8.93625562121796,8.94239292077128,8.97396052408427,9.00026170834061,
9.06687491676023,9.12609830984473,9.22412600025835,9.23160590966397,9.23705958717135,
9.31970204207281,9.32716434948363,9.33017709377742,9.33239051371326,9.33478061134552,
9.33801503840048,9.34533944247983,9.4634722039409,9.50705389168326,9.52698316382605,
9.55023543880307,9.7363667131148,9.74732266012034,9.74976205280237,9.7513463374906,
9.75261827946431,9.75406013419233,9.75650244224091,9.76652286260011,9.85174569816709,
9.95699582782369),.UNSPECIFIED.);
#3487=B_SPLINE_CURVE_WITH_KNOTS('',3,(#73952,#73953,#73954,#73955,#73956,
#73957,#73958,#73959,#73960,#73961,#73962,#73963,#73964,#73965,#73966,#73967,
#73968,#73969),.UNSPECIFIED.,.F.,.F.,(4,2,2,2,2,2,2,2,4),(340.415655293841,
341.250572205736,342.085489117631,342.920406029526,343.755322941421,344.590239853315,
345.42515676521,346.260073677105,346.698840601021),.UNSPECIFIED.);
#3488=B_SPLINE_CURVE_WITH_KNOTS('',3,(#73971,#73972,#73973,#73974,#73975,
#73976,#73977,#73978,#73979,#73980,#73981,#73982,#73983,#73984,#73985,#73986,
#73987,#73988,#73989,#73990,#73991,#73992,#73993,#73994,#73995,#73996,#73997,
#73998,#73999,#74000,#74001,#74002,#74003,#74004,#74005,#74006,#74007,#74008,
#74009,#74010,#74011,#74012,#74013,#74014,#74015,#74016,#74017,#74018,#74019,
#74020,#74021,#74022,#74023,#74024,#74025,#74026,#74027,#74028,#74029,#74030,
#74031,#74032,#74033,#74034,#74035,#74036,#74037,#74038,#74039,#74040,#74041,
#74042,#74043,#74044,#74045,#74046,#74047,#74048,#74049,#74050,#74051,#74052,
#74053,#74054,#74055,#74056,#74057,#74058,#74059,#74060,#74061,#74062,#74063,
#74064,#74065,#74066,#74067,#74068,#74069,#74070,#74071,#74072,#74073,#74074,
#74075,#74076,#74077,#74078,#74079,#74080,#74081,#74082,#74083,#74084,#74085,
#74086,#74087,#74088,#74089,#74090,#74091,#74092,#74093,#74094,#74095,#74096,
#74097,#74098,#74099,#74100,#74101,#74102,#74103,#74104,#74105,#74106,#74107,
#74108,#74109,#74110,#74111,#74112,#74113,#74114,#74115,#74116,#74117,#74118,
#74119,#74120,#74121,#74122,#74123,#74124,#74125,#74126,#74127,#74128,#74129,
#74130,#74131,#74132,#74133,#74134,#74135,#74136,#74137,#74138,#74139,#74140,
#74141,#74142,#74143,#74144,#74145,#74146,#74147,#74148,#74149,#74150,#74151,
#74152,#74153,#74154,#74155,#74156,#74157,#74158,#74159,#74160,#74161,#74162,
#74163,#74164,#74165,#74166,#74167,#74168,#74169,#74170,#74171,#74172,#74173,
#74174,#74175,#74176,#74177,#74178,#74179,#74180,#74181,#74182,#74183,#74184,
#74185,#74186,#74187,#74188,#74189,#74190,#74191,#74192,#74193,#74194,#74195,
#74196,#74197,#74198,#74199,#74200,#74201,#74202,#74203,#74204,#74205,#74206,
#74207,#74208,#74209,#74210,#74211,#74212,#74213,#74214,#74215,#74216,#74217,
#74218,#74219,#74220,#74221,#74222,#74223,#74224,#74225,#74226,#74227,#74228,
#74229,#74230,#74231,#74232,#74233,#74234,#74235,#74236,#74237,#74238,#74239,
#74240,#74241,#74242,#74243,#74244,#74245,#74246,#74247,#74248,#74249,#74250,
#74251,#74252,#74253,#74254,#74255,#74256,#74257,#74258,#74259,#74260,#74261,
#74262,#74263,#74264,#74265,#74266,#74267,#74268,#74269,#74270,#74271,#74272,
#74273,#74274,#74275,#74276,#74277,#74278,#74279,#74280,#74281,#74282,#74283,
#74284,#74285,#74286,#74287,#74288,#74289,#74290,#74291,#74292,#74293,#74294,
#74295,#74296,#74297,#74298,#74299,#74300,#74301,#74302,#74303,#74304,#74305,
#74306,#74307,#74308,#74309,#74310,#74311,#74312,#74313,#74314,#74315,#74316,
#74317,#74318,#74319,#74320,#74321,#74322,#74323,#74324,#74325,#74326,#74327,
#74328,#74329,#74330,#74331,#74332,#74333,#74334,#74335,#74336,#74337,#74338,
#74339,#74340,#74341,#74342,#74343,#74344,#74345,#74346,#74347,#74348,#74349,
#74350,#74351,#74352,#74353,#74354,#74355,#74356,#74357,#74358,#74359,#74360,
#74361,#74362,#74363,#74364,#74365,#74366,#74367,#74368,#74369,#74370,#74371,
#74372,#74373,#74374,#74375,#74376,#74377,#74378,#74379,#74380,#74381,#74382,
#74383,#74384,#74385,#74386,#74387,#74388,#74389,#74390,#74391,#74392,#74393,
#74394,#74395,#74396,#74397,#74398,#74399,#74400,#74401,#74402,#74403,#74404,
#74405,#74406,#74407,#74408,#74409,#74410,#74411,#74412,#74413,#74414,#74415,
#74416,#74417,#74418,#74419,#74420,#74421,#74422,#74423,#74424,#74425,#74426,
#74427,#74428,#74429,#74430,#74431,#74432,#74433,#74434,#74435,#74436,#74437,
#74438,#74439,#74440,#74441,#74442,#74443,#74444,#74445,#74446,#74447,#74448,
#74449,#74450,#74451,#74452,#74453,#74454,#74455,#74456,#74457,#74458,#74459,
#74460,#74461,#74462,#74463,#74464,#74465,#74466,#74467,#74468,#74469,#74470,
#74471,#74472,#74473,#74474,#74475,#74476,#74477,#74478,#74479,#74480,#74481,
#74482,#74483,#74484,#74485,#74486),.UNSPECIFIED.,.F.,.F.,(4,2,2,2,2,2,
2,2,2,2,2,2,2,2,2,2,2,2,2,2,2,2,2,2,2,2,2,2,2,2,2,2,2,2,2,2,2,2,2,2,2,2,
2,2,2,2,2,2,2,2,2,2,2,2,2,2,2,2,2,2,2,2,2,2,2,2,2,2,2,2,2,2,2,2,2,2,2,2,
2,2,2,2,2,2,2,2,2,2,2,2,2,2,2,2,2,2,2,2,2,2,2,2,2,2,2,2,2,2,2,2,2,2,2,2,
2,2,2,2,2,2,2,2,2,2,2,2,2,2,2,2,2,2,2,2,2,2,2,2,2,2,2,2,2,2,2,2,2,2,2,2,
2,2,2,2,2,2,2,2,2,2,2,2,2,2,2,2,2,2,2,2,2,2,2,2,2,2,2,2,2,2,2,2,2,2,2,2,
2,2,2,2,2,2,2,2,2,2,2,2,2,2,2,2,2,2,2,2,2,2,2,2,2,2,2,2,2,2,2,2,2,2,2,2,
2,2,2,2,2,2,2,2,2,2,2,2,2,2,2,2,2,2,2,2,2,2,2,2,2,2,2,2,2,2,2,2,2,2,2,4),
(0.00201172098188263,0.26785772850997,0.336857823383509,0.346341844779204,
0.348790531623013,0.350234150731159,0.35150641770642,0.353089494729013,
0.355522927949294,0.367173556294413,0.61641885642891,0.732383385343184,
0.740170432410955,0.74332318988102,0.745513237332233,0.747708768708506,
0.750811159704312,0.758150621232473,0.856660079940925,0.915920330777643,
1.01131517256049,1.0872275531088,1.13635125872654,1.14394057562209,1.1461031432124,
1.14743227276947,1.14865076128787,1.15020643452794,1.15347907616869,1.17485044651468,
1.42262349848926,1.50584868045553,1.54279547640015,1.55619405281239,1.5624737103579,
1.56750517355141,1.57019711971199,1.57243428466372,1.57468451831813,1.5787871612878,
1.59171101200624,1.78669000326812,1.94811466511878,1.95971868454392,1.96312974970139,
1.9652344312891,1.96715099015463,1.96962142125009,1.97474648119242,2.0088629671186,
2.02595144789495,2.14118090651002,2.30773034059313,2.33290597661399,2.34047794924219,
2.34508209565747,2.34923912489801,2.3543968663223,2.3645024658482,2.42490062362265,
2.63501688132774,2.68385780569144,2.70592756902931,2.70975065833207,2.71177614841906,
2.71343950102428,2.71511564282012,2.71819780833977,2.72811504021162,2.89581916126414,
3.03810262379446,3.1057656921007,3.11815354878818,3.12223321602547,3.12486288116367,
3.12733654813598,3.13058510284429,3.1360700444179,3.16969808690455,3.45296143876884,
3.52434995656347,3.53630651696089,3.53983508604457,3.54201619766115,3.54400521418938,
3.54657339107814,3.55191870659064,3.58862326122928,3.59112629064559,3.5941580942748,
3.60589132120185,3.60804128041258,3.61062450907206,3.72820514770246,3.93957400625043,
3.96649696857761,3.9775564112426,3.98558204304256,3.99295830280372,4.00492030425341,
4.03495101972908,4.19845562922461,4.25942722184311,4.28843584675888,4.29506018532236,
4.2988546586122,4.30180604973414,4.30567928455193,4.3127602458724,4.35465198551136,
4.39648202516114,4.49634347355929,4.57408995776118,4.59338435610224,4.60210937166159,
4.60868817207238,4.6149020810814,4.62359414162019,4.64686757126827,4.84700225921339,
4.98014546872586,5.0503407855483,5.05697759015036,5.05992698481809,5.06215502858731,
5.06450744202789,5.06812562234812,5.07889829876476,5.13336633417323,5.19116823361091,
5.44053566966038,5.4553627135643,5.45980899203634,5.46245607750361,5.46457057284833,
5.46740620449709,5.47271105002696,5.50210821774037,5.55864007014396,5.67191545187263,
5.71919451972143,5.77378411346617,5.85521600423813,5.87647321545384,5.87985435183502,
5.88149547809999,5.88277328780646,5.88418088049476,5.8864711188375,5.89471523202358,
5.95069907347356,6.04945136834659,6.16188021070765,6.20717207483633,6.26524119445543,
6.27114320731447,6.27402671579624,6.27608941466102,6.27826524853656,6.28112222820834,
6.2872432673312,6.36837618381505,6.54132711455869,6.60722517412876,6.67161264542583,
6.67584617814019,6.67745079435046,6.67860212432523,6.67970401266425,6.68125908222952,
6.68444499569772,6.71292051338696,6.79899987135283,6.93507335710241,7.08563288839093,
7.09576935119661,7.09948584939378,7.10165848778219,7.10369320427128,7.1064944826526,
7.11198237196928,7.14990676712809,7.24266649478576,7.39314191534718,7.4838138174065,
7.49116657838417,7.49382205924072,7.49567484370405,7.49739627132081,7.49974540373852,
7.5041839075335,7.53136198294643,7.59330462925065,7.82726968508707,7.8610618831827,
7.86910390750369,7.87428252257254,7.87842405211085,7.88229674326543,7.88924415942943,
7.91089580081731,8.03356739936528,8.15266598084587,8.1852523471671,8.19747536371011,
8.20034717474997,8.23490581711722,8.23911935969333,8.24125983362429,8.24283145486047,
8.2445276718186,8.24682237612872,8.25173469297441,8.25827461499044,8.2741862114308,
8.31447112604205,8.42791900126448,8.6343598522704,8.64785971055778,8.65224260197667,
8.65466964122223,8.65710543600497,8.6601129411165,8.6659171427816,8.70310007140037,
8.78782717693791,8.86041969121024,8.92383943212682,9.05499123177181,9.06577426419802,
9.06930660433383,9.07126906258101,9.07324411601817,9.07569016843109,9.08043619647743,
9.11149746112447,9.15785056291941,9.24268266709482,9.3545572047712,9.472130522821,
9.49621907773396,9.5059188575557,9.51394201092931,9.52127052255671,9.52927707275944,
9.54859043813267,9.64010979152572,9.70678561614486,9.76949118288661,9.8148868318222,
9.82204284743874,9.82634158260985,9.82966314592016,9.83271634113912,9.83619805523396,
9.84112763116791,9.86117115424333,9.95401133408935),.UNSPECIFIED.);
#3489=B_SPLINE_CURVE_WITH_KNOTS('',3,(#74488,#74489,#74490,#74491,#74492,
#74493,#74494,#74495,#74496,#74497,#74498,#74499),.UNSPECIFIED.,.F.,.F.,
(4,1,1,1,1,1,1,1,1,4),(359.26521121538,359.614028467624,360.112799658286,
361.110342039611,362.107884420936,363.105426802261,363.604197992924,364.102969183586,
365.100511564911,365.54819074432),.UNSPECIFIED.);
#3490=B_SPLINE_CURVE_WITH_KNOTS('',3,(#74501,#74502,#74503,#74504,#74505,
#74506,#74507,#74508,#74509,#74510,#74511,#74512,#74513,#74514,#74515,#74516,
#74517,#74518),.UNSPECIFIED.,.F.,.F.,(4,2,2,2,2,2,2,2,4),(365.548432642184,
366.383313434454,367.218230346349,368.053147258244,368.888064170139,369.722981082033,
370.557897993928,371.392814905823,371.831581829739),.UNSPECIFIED.);
#3491=B_SPLINE_CURVE_WITH_KNOTS('',3,(#74520,#74521,#74522,#74523,#74524,
#74525,#74526,#74527,#74528,#74529,#74530,#74531,#74532,#74533,#74534,#74535),
 .UNSPECIFIED.,.F.,.F.,(4,2,2,2,2,2,2,4),(371.831581829739,372.666498741634,
373.501415653529,374.336332565424,375.171249477318,376.006166389213,376.841083301108,
376.991118430775),.UNSPECIFIED.);
#3492=B_SPLINE_CURVE_WITH_KNOTS('',3,(#74539,#74540,#74541,#74542,#74543,
#74544,#74545,#74546,#74547,#74548,#74549,#74550,#74551,#74552,#74553,#74554,
#74555,#74556,#74557,#74558,#74559,#74560,#74561,#74562,#74563,#74564,#74565,
#74566,#74567,#74568,#74569,#74570,#74571,#74572,#74573,#74574,#74575,#74576,
#74577,#74578,#74579,#74580,#74581,#74582,#74583,#74584,#74585,#74586,#74587,
#74588,#74589,#74590,#74591,#74592,#74593,#74594,#74595,#74596,#74597,#74598,
#74599,#74600,#74601,#74602,#74603,#74604,#74605,#74606,#74607,#74608,#74609,
#74610,#74611,#74612,#74613,#74614,#74615,#74616,#74617,#74618,#74619,#74620,
#74621,#74622,#74623,#74624,#74625,#74626,#74627,#74628,#74629,#74630,#74631,
#74632,#74633,#74634,#74635,#74636,#74637,#74638,#74639,#74640,#74641,#74642,
#74643,#74644,#74645,#74646,#74647,#74648,#74649,#74650,#74651,#74652,#74653,
#74654,#74655,#74656,#74657,#74658,#74659,#74660,#74661,#74662,#74663,#74664,
#74665,#74666,#74667,#74668,#74669,#74670,#74671,#74672,#74673,#74674,#74675,
#74676,#74677,#74678,#74679,#74680,#74681,#74682,#74683,#74684,#74685,#74686,
#74687,#74688,#74689,#74690,#74691,#74692,#74693,#74694,#74695,#74696,#74697,
#74698,#74699,#74700,#74701,#74702,#74703,#74704,#74705,#74706,#74707,#74708,
#74709,#74710),.UNSPECIFIED.,.F.,.F.,(4,3,3,3,3,3,3,3,3,3,3,3,3,3,3,3,3,
3,3,3,3,3,3,3,3,3,3,3,3,3,3,3,3,3,3,3,3,3,3,3,3,3,3,3,3,3,3,3,3,3,3,3,3,
3,3,3,3,4),(-379.066104903459,-378.984591704675,-378.90305453626,-378.819124330394,
-378.737584607012,-378.652459159905,-378.567333712797,-378.493243868417,
-378.41917720065,-378.345120941409,-378.271041497686,-378.196950707724,
-378.122805283221,-378.068562522134,-377.984413927215,-377.90024800538,
-377.816140290729,-377.732108414648,-377.648267189574,-377.569791331472,
-377.494854902038,-377.419925132161,-377.34499010411,-377.270011093797,
-377.195008711992,-377.119937164651,-377.071020140809,-376.995535332464,
-376.92010901322,-376.844728552861,-376.769381352133,-376.69405483498,-376.616482700543,
-376.541140898997,-376.46578071888,-376.390390754318,-376.311162505609,
-376.235638571276,-376.160060519903,-376.08438514796,-376.073477759484,
-376.000482344579,-375.927575454631,-375.854742076552,-375.781967271272,
-375.709236157044,-375.636533894427,-375.563831707361,-375.491125918639,
-375.418403117554,-375.345649881171,-375.272809217739,-375.199921024411,
-375.126920336245,-375.07593537816,-374.972030919384,-374.871429316071,
-374.800863543725),.UNSPECIFIED.);
#3493=B_SPLINE_CURVE_WITH_KNOTS('',3,(#74712,#74713,#74714,#74715,#74716,
#74717,#74718,#74719,#74720,#74721,#74722,#74723,#74724,#74725,#74726,#74727,
#74728,#74729),.UNSPECIFIED.,.F.,.F.,(4,2,2,2,2,2,2,2,4),(-374.800863543725,
-373.965946631831,-373.131029719936,-372.296112808041,-371.461195896146,
-370.626278984251,-369.791362072357,-368.956445160462,-368.517678236546),
 .UNSPECIFIED.);
#3494=B_SPLINE_CURVE_WITH_KNOTS('',3,(#74731,#74732,#74733,#74734,#74735,
#74736,#74737,#74738,#74739,#74740,#74741,#74742,#74743),.UNSPECIFIED.,
 .F.,.F.,(4,1,1,1,1,1,1,1,1,1,4),(-368.517678236546,-368.093138708885,-367.09559632756,
-366.596825136898,-366.098053946236,-365.599282755573,-365.100511564911,
-364.102969183586,-363.604197992923,-363.105426802261,-362.234492929366),
 .UNSPECIFIED.);
#3495=B_SPLINE_CURVE_WITH_KNOTS('',3,(#74745,#74746,#74747,#74748,#74749,
#74750,#74751,#74752,#74753,#74754,#74755,#74756,#74757,#74758),
 .UNSPECIFIED.,.F.,.F.,(4,1,1,1,1,1,1,1,1,1,1,4),(-362.234492929366,-362.107884420936,
-361.110342039611,-360.112799658286,-359.614028467624,-359.115257276961,
-358.616486086299,-358.117714895636,-357.120172514312,-356.621401323649,
-356.122630132987,-355.951307622187),.UNSPECIFIED.);
#3496=B_SPLINE_CURVE_WITH_KNOTS('',3,(#74760,#74761,#74762,#74763,#74764,
#74765,#74766,#74767,#74768,#74769,#74770,#74771),.UNSPECIFIED.,.F.,.F.,
(4,1,1,1,1,1,1,1,1,4),(-355.951307622187,-355.125087751662,-354.127545370337,
-353.130002989012,-352.631231798349,-352.132460607687,-351.633689417025,
-351.134918226362,-350.137375845037,-349.668188319012),.UNSPECIFIED.);
#3497=B_SPLINE_CURVE_WITH_KNOTS('',3,(#74773,#74774,#74775,#74776,#74777,
#74778,#74779,#74780,#74781,#74782,#74783,#74784,#74785,#74786,#74787,#74788,
#74789,#74790),.UNSPECIFIED.,.F.,.F.,(4,2,2,2,2,2,2,2,4),(-349.668100404495,
-348.833205403112,-347.998288491218,-347.163371579323,-346.328454667428,
-345.493537755533,-344.658620843638,-343.823703931743,-343.384937007828),
 .UNSPECIFIED.);
#3498=B_SPLINE_CURVE_WITH_KNOTS('',3,(#74792,#74793,#74794,#74795,#74796,
#74797,#74798,#74799,#74800,#74801,#74802,#74803,#74804,#74805,#74806,#74807,
#74808,#74809),.UNSPECIFIED.,.F.,.F.,(4,2,2,2,2,2,2,2,4),(-343.384937007828,
-342.550020095933,-341.715103184038,-340.880186272143,-340.045269360248,
-339.210352448353,-338.375435536458,-337.540518624564,-337.101751700648),
 .UNSPECIFIED.);
#3499=B_SPLINE_CURVE_WITH_KNOTS('',3,(#74811,#74812,#74813,#74814,#74815,
#74816,#74817,#74818,#74819,#74820,#74821,#74822,#74823,#74824,#74825,#74826,
#74827,#74828),.UNSPECIFIED.,.F.,.F.,(4,2,2,2,2,2,2,2,4),(-337.101751700648,
-336.266834788753,-335.431917876858,-334.597000964963,-333.762084053069,
-332.927167141174,-332.092250229279,-331.257333317384,-330.818566393468),
 .UNSPECIFIED.);
#3500=B_SPLINE_CURVE_WITH_KNOTS('',3,(#74830,#74831,#74832,#74833,#74834,
#74835,#74836,#74837,#74838,#74839,#74840,#74841,#74842,#74843,#74844,#74845,
#74846,#74847),.UNSPECIFIED.,.F.,.F.,(4,2,2,2,2,2,2,2,4),(-330.818566393468,
-329.983649481574,-329.148732569679,-328.313815657784,-327.478898745889,
-326.643981833994,-325.809064922099,-324.974148010204,-324.535381086289),
 .UNSPECIFIED.);
#3501=B_SPLINE_CURVE_WITH_KNOTS('',3,(#74849,#74850,#74851,#74852,#74853,
#74854,#74855,#74856,#74857,#74858,#74859,#74860),.UNSPECIFIED.,.F.,.F.,
(4,1,1,1,1,1,1,1,1,4),(-324.535381086289,-324.20127393059,-323.702502739928,
-323.203731549265,-322.20618916794,-321.707417977278,-321.208646786615,
-320.21110440529,-319.213562023966,-318.252195779109),.UNSPECIFIED.);
#3502=B_SPLINE_CURVE_WITH_KNOTS('',3,(#74862,#74863,#74864,#74865,#74866,
#74867,#74868,#74869,#74870,#74871,#74872,#74873,#74874,#74875,#74876),
 .UNSPECIFIED.,.F.,.F.,(4,2,1,1,1,1,1,1,1,1,1,4),(-318.252195779109,-318.216019642641,
-317.717248451978,-317.218477261316,-316.719706070653,-316.220934879991,
-315.223392498666,-314.724621308004,-314.225850117341,-313.228307736016,
-312.230765354691,-311.96901047193),.UNSPECIFIED.);
#3503=B_SPLINE_CURVE_WITH_KNOTS('',3,(#74878,#74879,#74880,#74881,#74882,
#74883,#74884,#74885,#74886,#74887,#74888,#74889,#74890,#74891,#74892,#74893,
#74894,#74895),.UNSPECIFIED.,.F.,.F.,(4,2,2,2,2,2,2,2,4),(-311.96901047193,
-311.134093560035,-310.29917664814,-309.464259736245,-308.62934282435,-307.794425912455,
-306.959509000561,-306.124592088666,-305.68582516475),.UNSPECIFIED.);
#3504=B_SPLINE_CURVE_WITH_KNOTS('',3,(#74897,#74898,#74899,#74900,#74901,
#74902,#74903,#74904,#74905,#74906,#74907,#74908,#74909),.UNSPECIFIED.,
 .F.,.F.,(4,1,1,1,1,1,1,1,1,1,4),(-305.68582516475,-305.247968685417,-304.250426304092,
-303.75165511343,-303.252883922767,-302.754112732105,-302.255341541442,
-301.257799160117,-300.759027969455,-300.260256778793,-299.402639857571),
 .UNSPECIFIED.);
#3505=B_SPLINE_CURVE_WITH_KNOTS('',3,(#74911,#74912,#74913,#74914,#74915,
#74916,#74917,#74918,#74919,#74920,#74921,#74922,#74923,#74924),
 .UNSPECIFIED.,.F.,.F.,(4,1,1,1,1,1,1,1,1,1,1,4),(-299.402639857571,-299.262714397468,
-298.265172016143,-297.267629634818,-296.768858444155,-296.270087253493,
-295.771316062831,-295.272544872168,-294.275002490843,-293.776231300181,
-293.277460109518,-293.119454550391),.UNSPECIFIED.);
#3506=B_SPLINE_CURVE_WITH_KNOTS('',3,(#74926,#74927,#74928,#74929,#74930,
#74931,#74932,#74933,#74934,#74935,#74936,#74937),.UNSPECIFIED.,.F.,.F.,
(4,1,1,1,1,1,1,1,1,4),(-293.119454550391,-292.279917728194,-291.282375346869,
-290.284832965544,-289.786061774881,-289.287290584219,-288.788519393556,
-288.289748202894,-287.292205821569,-286.836289777759),.UNSPECIFIED.);
#3507=B_SPLINE_CURVE_WITH_KNOTS('',3,(#74939,#74940,#74941,#74942,#74943,
#74944,#74945,#74946,#74947,#74948,#74949,#74950,#74951,#74952,#74953,#74954,
#74955,#74956),.UNSPECIFIED.,.F.,.F.,(4,2,2,2,2,2,2,2,4),(-286.836262713003,
-286.001352331317,-285.166435419422,-284.331518507527,-283.496601595632,
-282.661684683737,-281.826767771843,-280.991850859948,-280.553083936032),
 .UNSPECIFIED.);
#3508=B_SPLINE_CURVE_WITH_KNOTS('',3,(#74958,#74959,#74960,#74961,#74962,
#74963,#74964,#74965,#74966,#74967,#74968,#74969,#74970,#74971,#74972,#74973,
#74974,#74975),.UNSPECIFIED.,.F.,.F.,(4,2,2,2,2,2,2,2,4),(-280.553083936032,
-279.718167024137,-278.883250112242,-278.048333200347,-277.213416288452,
-276.378499376558,-275.543582464663,-274.708665552768,-274.269898628852),
 .UNSPECIFIED.);
#3509=B_SPLINE_CURVE_WITH_KNOTS('',3,(#74977,#74978,#74979,#74980,#74981,
#74982,#74983,#74984,#74985,#74986,#74987,#74988,#74989,#74990,#74991,#74992,
#74993,#74994),.UNSPECIFIED.,.F.,.F.,(4,2,2,2,2,2,2,2,4),(-274.269898628852,
-273.434981716958,-272.600064805063,-271.765147893168,-270.930230981273,
-270.095314069378,-269.260397157483,-268.425480245589,-267.986713321673),
 .UNSPECIFIED.);
#3510=B_SPLINE_CURVE_WITH_KNOTS('',3,(#74996,#74997,#74998,#74999,#75000,
#75001,#75002,#75003,#75004,#75005,#75006,#75007,#75008,#75009,#75010,#75011,
#75012,#75013),.UNSPECIFIED.,.F.,.F.,(4,2,2,2,2,2,2,2,4),(-267.986713321673,
-267.151796409778,-266.316879497883,-265.481962585988,-264.647045674093,
-263.812128762198,-262.977211850304,-262.142294938409,-261.703528014493),
 .UNSPECIFIED.);
#3511=B_SPLINE_CURVE_WITH_KNOTS('',3,(#75015,#75016,#75017,#75018,#75019,
#75020,#75021,#75022,#75023,#75024,#75025,#75026),.UNSPECIFIED.,.F.,.F.,
(4,1,1,1,1,1,1,1,1,4),(-261.703528014493,-261.356103907122,-260.857332716459,
-260.358561525797,-259.361019144472,-258.86224795381,-258.363476763147,
-257.365934381822,-256.368392000497,-255.420342707314),.UNSPECIFIED.);
#3512=B_SPLINE_CURVE_WITH_KNOTS('',3,(#75028,#75029,#75030,#75031,#75032,
#75033,#75034,#75035,#75036,#75037,#75038,#75039,#75040,#75041,#75042),
 .UNSPECIFIED.,.F.,.F.,(4,2,1,1,1,1,1,1,1,1,1,4),(-255.420342707314,-255.370849619172,
-254.87207842851,-254.373307237848,-253.874536047185,-253.375764856523,
-252.378222475198,-251.879451284535,-251.380680093873,-250.383137712548,
-249.385595331223,-249.137157400134),.UNSPECIFIED.);
#3513=B_SPLINE_CURVE_WITH_KNOTS('',3,(#75044,#75045,#75046,#75047,#75048,
#75049,#75050,#75051,#75052,#75053,#75054,#75055,#75056,#75057,#75058,#75059,
#75060,#75061),.UNSPECIFIED.,.F.,.F.,(4,2,2,2,2,2,2,2,4),(-249.137157400134,
-248.302240488239,-247.467323576344,-246.632406664449,-245.797489752555,
-244.96257284066,-244.127655928765,-243.29273901687,-242.853972092955),
 .UNSPECIFIED.);
#3514=B_SPLINE_CURVE_WITH_KNOTS('',3,(#75063,#75064,#75065,#75066,#75067,
#75068,#75069,#75070,#75071,#75072,#75073,#75074,#75075),.UNSPECIFIED.,
 .F.,.F.,(4,1,1,1,1,1,1,1,1,1,4),(-242.853972092955,-242.402798661949,-241.405256280624,
-240.906485089962,-240.407713899299,-239.908942708637,-239.410171517974,
-238.412629136649,-237.913857945987,-237.415086755324,-236.570786785775),
 .UNSPECIFIED.);
#3515=B_SPLINE_CURVE_WITH_KNOTS('',3,(#75077,#75078,#75079,#75080,#75081,
#75082,#75083,#75084,#75085,#75086,#75087,#75088,#75089,#75090),
 .UNSPECIFIED.,.F.,.F.,(4,1,1,1,1,1,1,1,1,1,1,4),(-236.570786785775,-236.417544374,
-235.420001992675,-234.42245961135,-233.923688420687,-233.424917230025,
-232.926146039362,-232.4273748487,-231.429832467375,-230.931061276713,-230.43229008605,
-230.287601478595),.UNSPECIFIED.);
#3516=B_SPLINE_CURVE_WITH_KNOTS('',3,(#75092,#75093,#75094,#75095,#75096,
#75097,#75098,#75099,#75100,#75101,#75102,#75103),.UNSPECIFIED.,.F.,.F.,
(4,1,1,1,1,1,1,1,1,4),(-230.287601478595,-229.434747704725,-228.4372053234,
-227.439662942076,-226.940891751413,-226.442120560751,-225.943349370088,
-225.444578179426,-224.447035798101,-224.004416171416),.UNSPECIFIED.);
#3517=B_SPLINE_CURVE_WITH_KNOTS('',3,(#75105,#75106,#75107,#75108,#75109,
#75110,#75111,#75112,#75113,#75114,#75115,#75116,#75117,#75118,#75119,#75120,
#75121,#75122),.UNSPECIFIED.,.F.,.F.,(4,2,2,2,2,2,2,2,4),(-224.004416171416,
-223.169499259521,-222.334582347626,-221.499665435731,-220.664748523836,
-219.829831611942,-218.994914700047,-218.159997788152,-217.721230864236),
 .UNSPECIFIED.);
#3518=B_SPLINE_CURVE_WITH_KNOTS('',3,(#75124,#75125,#75126,#75127,#75128,
#75129,#75130,#75131,#75132,#75133,#75134,#75135,#75136,#75137,#75138,#75139,
#75140,#75141),.UNSPECIFIED.,.F.,.F.,(4,2,2,2,2,2,2,2,4),(-217.721230864236,
-216.886313952342,-216.051397040447,-215.216480128552,-214.381563216657,
-213.546646304762,-212.711729392867,-211.876812480973,-211.438045557057),
 .UNSPECIFIED.);
#3519=B_SPLINE_CURVE_WITH_KNOTS('',3,(#75143,#75144,#75145,#75146,#75147,
#75148,#75149,#75150,#75151,#75152,#75153,#75154,#75155,#75156,#75157,#75158,
#75159,#75160),.UNSPECIFIED.,.F.,.F.,(4,2,2,2,2,2,2,2,4),(-211.438045557057,
-210.603128645162,-209.768211733267,-208.933294821372,-208.098377909478,
-207.263460997583,-206.428544085688,-205.593627173793,-205.154860249877),
 .UNSPECIFIED.);
#3520=B_SPLINE_CURVE_WITH_KNOTS('',3,(#75162,#75163,#75164,#75165,#75166,
#75167,#75168,#75169,#75170,#75171,#75172,#75173,#75174,#75175,#75176,#75177,
#75178,#75179),.UNSPECIFIED.,.F.,.F.,(4,2,2,2,2,2,2,2,4),(-205.154860249877,
-204.319943337982,-203.485026426088,-202.650109514193,-201.815192602298,
-200.980275690403,-200.145358778508,-199.310441866613,-198.871674942698),
 .UNSPECIFIED.);
#3521=B_SPLINE_CURVE_WITH_KNOTS('',3,(#75181,#75182,#75183,#75184,#75185,
#75186,#75187,#75188,#75189,#75190,#75191,#75192),.UNSPECIFIED.,.F.,.F.,
(4,1,1,1,1,1,1,1,1,4),(-198.871674942698,-198.510933883654,-198.012162692991,
-197.513391502329,-196.515849121004,-196.017077930341,-195.518306739679,
-194.520764358354,-193.523221977029,-192.588489635518),.UNSPECIFIED.);
#3522=B_SPLINE_CURVE_WITH_KNOTS('',3,(#75194,#75195,#75196,#75197,#75198,
#75199,#75200,#75201,#75202,#75203,#75204,#75205,#75206,#75207),
 .UNSPECIFIED.,.F.,.F.,(4,1,1,1,1,1,1,1,1,1,1,4),(-192.588489635518,-192.525679595704,
-191.528137214379,-190.530594833054,-190.031823642392,-189.53305245173,
-188.535510070405,-188.036738879742,-187.53796768908,-187.039196498417,
-186.540425307755,-186.305304328339),.UNSPECIFIED.);
#3523=B_SPLINE_CURVE_WITH_KNOTS('',3,(#75209,#75210,#75211,#75212,#75213,
#75214,#75215,#75216,#75217,#75218,#75219,#75220,#75221),.UNSPECIFIED.,
 .F.,.F.,(4,1,1,1,1,1,1,1,1,1,4),(-186.305304328339,-185.54288292643,-184.545340545105,
-183.54779816378,-183.049026973118,-182.550255782455,-181.55271340113,-181.053942210468,
-180.555171019806,-180.056399829143,-180.022119021159),.UNSPECIFIED.);
#3524=B_SPLINE_CURVE_WITH_KNOTS('',3,(#75223,#75224,#75225,#75226,#75227,
#75228,#75229,#75230,#75231,#75232,#75233,#75234,#75235,#75236,#75237,#75238,
#75239,#75240),.UNSPECIFIED.,.F.,.F.,(4,2,2,2,2,2,2,2,4),(-180.022119021159,
-179.187202109264,-178.352285197369,-177.517368285475,-176.68245137358,
-175.847534461685,-175.01261754979,-174.177700637896,-173.738933713979),
 .UNSPECIFIED.);
#3525=B_SPLINE_CURVE_WITH_KNOTS('',3,(#75242,#75243,#75244,#75245,#75246,
#75247,#75248,#75249,#75250,#75251,#75252,#75253,#75254,#75255,#75256,#75257,
#75258,#75259),.UNSPECIFIED.,.F.,.F.,(4,2,2,2,2,2,2,2,4),(-173.738933713979,
-172.904016802084,-172.06909989019,-171.234182978295,-170.3992660664,-169.564349154505,
-168.72943224261,-167.894515330715,-167.4557484068),.UNSPECIFIED.);
#3526=B_SPLINE_CURVE_WITH_KNOTS('',3,(#75261,#75262,#75263,#75264,#75265,
#75266,#75267,#75268,#75269,#75270,#75271,#75272,#75273,#75274,#75275,#75276,
#75277,#75278),.UNSPECIFIED.,.F.,.F.,(4,2,2,2,2,2,2,2,4),(-167.4557484068,
-166.620831494905,-165.78591458301,-164.950997671115,-164.116080759221,
-163.281163847326,-162.446246935431,-161.611330023536,-161.172570307997),
 .UNSPECIFIED.);
#3527=B_SPLINE_CURVE_WITH_KNOTS('',3,(#75280,#75281,#75282,#75283,#75284,
#75285,#75286,#75287,#75288,#75289,#75290,#75291,#75292,#75293,#75294,#75295,
#75296,#75297,#75298,#75299,#75300,#75301,#75302,#75303,#75304,#75305,#75306,
#75307,#75308,#75309,#75310,#75311,#75312,#75313,#75314,#75315,#75316,#75317,
#75318,#75319,#75320,#75321,#75322,#75323,#75324,#75325,#75326,#75327,#75328,
#75329,#75330,#75331,#75332,#75333,#75334,#75335,#75336,#75337,#75338,#75339,
#75340,#75341,#75342,#75343,#75344,#75345,#75346,#75347,#75348,#75349,#75350,
#75351,#75352,#75353,#75354,#75355,#75356,#75357,#75358,#75359,#75360,#75361,
#75362,#75363,#75364,#75365,#75366,#75367,#75368,#75369,#75370,#75371,#75372,
#75373,#75374,#75375,#75376,#75377,#75378,#75379,#75380,#75381,#75382,#75383,
#75384,#75385,#75386,#75387,#75388,#75389,#75390,#75391,#75392,#75393,#75394,
#75395,#75396,#75397,#75398,#75399,#75400,#75401,#75402,#75403,#75404,#75405,
#75406,#75407,#75408,#75409,#75410,#75411,#75412,#75413,#75414,#75415,#75416,
#75417,#75418,#75419,#75420,#75421,#75422,#75423,#75424,#75425,#75426,#75427,
#75428,#75429,#75430,#75431,#75432,#75433,#75434,#75435,#75436,#75437,#75438,
#75439,#75440,#75441,#75442,#75443,#75444,#75445,#75446,#75447,#75448,#75449,
#75450,#75451,#75452,#75453,#75454,#75455,#75456,#75457,#75458,#75459,#75460,
#75461,#75462,#75463,#75464,#75465,#75466,#75467,#75468,#75469,#75470,#75471,
#75472,#75473,#75474,#75475,#75476,#75477,#75478,#75479,#75480,#75481,#75482,
#75483,#75484,#75485,#75486,#75487,#75488,#75489,#75490,#75491,#75492,#75493,
#75494,#75495,#75496,#75497,#75498,#75499,#75500,#75501,#75502),
 .UNSPECIFIED.,.F.,.F.,(4,3,3,3,3,3,3,3,3,3,3,3,3,3,3,3,3,3,3,3,3,3,3,3,
3,3,3,3,3,3,3,3,3,3,3,3,3,3,3,3,3,3,3,3,3,3,3,3,3,3,3,3,3,3,3,3,3,3,3,3,
3,3,3,3,3,3,3,3,3,3,3,3,3,3,4),(-161.172534268608,-161.076875819595,-160.980846673946,
-160.8848438716,-160.789080703855,-160.693626747646,-160.605015379132,-160.510966660752,
-160.462380492166,-160.400013339945,-160.337646187725,-160.179613361151,
-160.105498696632,-159.942312798227,-159.774631179198,-159.60694956017,
-159.502729275831,-159.390898384637,-159.276901723327,-159.160779303066,
-159.108140809998,-158.992014088384,-158.877377248298,-158.767600041595,
-158.667812363936,-158.60923644261,-158.511423045628,-158.413466381551,
-158.315490462468,-158.250353907988,-158.160753613792,-158.071253574473,
-157.982706110331,-157.896329266241,-157.832895452041,-157.737989653359,
-157.644824200271,-157.612044871271,-157.517597734643,-157.422345400126,
-157.327747638583,-157.251013998931,-157.176302298935,-157.101083416223,
-157.02585745876,-156.997978540146,-156.920734393649,-156.843609945958,
-156.766681221241,-156.689979154557,-156.614102931111,-156.53741871234,
-156.461002677123,-156.416097087036,-156.34345143238,-156.270329100991,
-156.196539751135,-156.163061628251,-156.065396634053,-155.967246292825,
-155.868970620973,-155.770933922614,-155.673436224496,-155.616863151268,
-155.52069496055,-155.461230458469,-155.401501838647,-155.341815438617,
-155.328144716356,-155.234430212384,-155.139022723453,-155.118013022302,
-155.022163018909,-154.927201558076,-154.889377792441),.UNSPECIFIED.);
#3528=B_SPLINE_CURVE_WITH_KNOTS('',3,(#75504,#75505,#75506,#75507,#75508,
#75509,#75510,#75511,#75512,#75513,#75514,#75515,#75516),.UNSPECIFIED.,
 .F.,.F.,(4,1,1,1,1,1,1,1,1,1,4),(-154.889377792441,-154.619069105358,-153.621526724033,
-153.122755533371,-152.623984342709,-152.125213152046,-151.626441961384,
-150.628899580059,-149.631357198734,-148.633814817409,-148.60619306022),
 .UNSPECIFIED.);
#3529=B_SPLINE_CURVE_WITH_KNOTS('',3,(#75518,#75519,#75520,#75521,#75522,
#75523,#75524,#75525,#75526,#75527,#75528,#75529,#75530,#75531,#75532,#75533,
#75534,#75535,#75536,#75537,#75538,#75539,#75540,#75541,#75542,#75543,#75544,
#75545,#75546,#75547,#75548,#75549,#75550,#75551,#75552,#75553,#75554,#75555,
#75556,#75557,#75558,#75559,#75560,#75561,#75562,#75563,#75564,#75565,#75566,
#75567,#75568,#75569,#75570,#75571,#75572,#75573,#75574,#75575,#75576,#75577,
#75578,#75579,#75580,#75581,#75582,#75583,#75584,#75585,#75586,#75587,#75588,
#75589,#75590,#75591,#75592,#75593,#75594,#75595,#75596,#75597,#75598,#75599,
#75600,#75601,#75602,#75603,#75604,#75605,#75606,#75607,#75608,#75609,#75610,
#75611,#75612,#75613,#75614,#75615,#75616,#75617,#75618,#75619,#75620,#75621,
#75622,#75623,#75624,#75625,#75626,#75627,#75628,#75629,#75630,#75631,#75632,
#75633,#75634,#75635,#75636,#75637,#75638,#75639,#75640,#75641,#75642,#75643,
#75644,#75645,#75646,#75647,#75648,#75649,#75650,#75651,#75652,#75653,#75654,
#75655,#75656,#75657,#75658,#75659,#75660,#75661,#75662,#75663,#75664,#75665,
#75666,#75667,#75668,#75669,#75670,#75671,#75672,#75673,#75674,#75675,#75676,
#75677,#75678,#75679,#75680,#75681,#75682,#75683,#75684,#75685,#75686,#75687,
#75688,#75689,#75690,#75691,#75692,#75693,#75694,#75695,#75696,#75697,#75698,
#75699,#75700,#75701,#75702,#75703,#75704,#75705,#75706,#75707,#75708,#75709,
#75710,#75711,#75712,#75713,#75714,#75715,#75716,#75717,#75718,#75719,#75720,
#75721,#75722,#75723,#75724,#75725,#75726,#75727,#75728,#75729,#75730,#75731,
#75732,#75733,#75734,#75735,#75736,#75737,#75738,#75739,#75740,#75741,#75742,
#75743,#75744,#75745,#75746,#75747,#75748,#75749,#75750,#75751,#75752,#75753,
#75754,#75755,#75756,#75757,#75758,#75759,#75760,#75761,#75762,#75763,#75764,
#75765,#75766,#75767,#75768,#75769,#75770,#75771,#75772,#75773),
 .UNSPECIFIED.,.F.,.F.,(4,3,3,3,3,3,3,3,3,3,3,3,3,3,3,3,3,3,3,3,3,3,3,3,
3,3,3,3,3,3,3,3,3,3,3,3,3,3,3,3,3,3,3,3,3,3,3,3,3,3,3,3,3,3,3,3,3,3,3,3,
3,3,3,3,3,3,3,3,3,3,3,3,3,3,3,3,3,3,3,3,3,3,3,3,3,4),(-148.606192485261,
-148.52636985924,-148.446664288587,-148.367133225438,-148.28770796962,-148.208444972183,
-148.135043626747,-148.0606272344,-147.986194073281,-147.911731880879,-147.837187945428,
-147.762599626954,-147.687907200668,-147.636272436084,-147.559696613986,
-147.4831882777,-147.406736485885,-147.330330337391,-147.253958963917,-147.177055350273,
-147.100712852782,-147.024370810536,-146.948019377498,-146.870697046813,
-146.794272879664,-146.716501467211,-146.638730054759,-146.564937988792,
-146.491208130101,-146.417527418265,-146.343882020907,-146.270258073095,
-146.196630007403,-146.139958864097,-146.058532398256,-145.976971104177,
-145.893025246491,-145.811191737305,-145.72618970537,-145.641187673434,
-145.562754040429,-145.484389989058,-145.40609068352,-145.327870109342,
-145.249699364303,-145.171586345936,-145.142416482772,-145.066046455012,
-144.989659575864,-144.913246274884,-144.836764235035,-144.760244856203,
-144.683643532744,-144.643645292109,-144.568258913417,-144.492933936661,
-144.417657553264,-144.342416987077,-144.267199486563,-144.189562414591,
-144.114334645603,-144.039090151388,-143.963817374849,-143.888504745606,
-143.813103168631,-143.737648898478,-143.662096729519,-143.646102910784,
-143.5729448966,-143.49987550463,-143.42687980634,-143.353942942787,-143.281050109155,
-143.2081865408,-143.135324030541,-143.062458463952,-142.989576498397,-142.916664780578,
-142.843667394008,-142.770623161723,-142.697468924523,-142.64856052946,
-142.555235922819,-142.462568780342,-142.371289963649,-142.323007313817),
 .UNSPECIFIED.);
#3530=B_SPLINE_CURVE_WITH_KNOTS('',3,(#75775,#75776,#75777,#75778,#75779,
#75780,#75781,#75782,#75783,#75784,#75785,#75786,#75787),.UNSPECIFIED.,
 .F.,.F.,(4,1,1,1,1,1,1,1,1,1,4),(-142.323007178082,-141.651018148135,-141.152246957472,
-140.65347576681,-139.655933385485,-139.157162194822,-138.65839100416,-138.159619813498,
-137.660848622835,-136.66330624151,-136.039821870902),.UNSPECIFIED.);
#3531=B_SPLINE_CURVE_WITH_KNOTS('',3,(#75789,#75790,#75791,#75792,#75793,
#75794,#75795,#75796,#75797,#75798,#75799,#75800,#75801),.UNSPECIFIED.,
 .F.,.F.,(4,1,1,1,1,1,1,1,1,1,4),(-136.039821870902,-135.665763860185,-134.66822147886,
-134.169450288198,-133.670679097536,-132.673136716211,-132.174365525548,
-131.675594334886,-131.176823144223,-130.678051953561,-129.756636563722),
 .UNSPECIFIED.);
#3532=B_SPLINE_CURVE_WITH_KNOTS('',3,(#75803,#75804,#75805,#75806,#75807,
#75808,#75809,#75810,#75811,#75812,#75813,#75814,#75815,#75816,#75817),
 .UNSPECIFIED.,.F.,.F.,(4,2,1,1,1,1,1,1,1,1,1,4),(-129.756636563722,-129.680509572236,
-128.682967190911,-127.685424809586,-127.186653618924,-126.687882428261,
-125.690340046936,-125.191568856274,-124.692797665612,-124.194026474949,
-123.695255284287,-123.473451256543),.UNSPECIFIED.);
#3533=B_SPLINE_CURVE_WITH_KNOTS('',3,(#75819,#75820,#75821,#75822,#75823,
#75824,#75825,#75826,#75827,#75828,#75829,#75830,#75831),.UNSPECIFIED.,
 .F.,.F.,(4,1,1,1,1,1,1,1,1,1,4),(-123.473451256543,-122.697712902962,-121.700170521637,
-120.702628140312,-120.20385694965,-119.705085758987,-118.707543377662,
-118.208772187,-117.710000996337,-117.211229805675,-117.190265949363),
 .UNSPECIFIED.);
#3534=B_SPLINE_CURVE_WITH_KNOTS('',3,(#75833,#75834,#75835,#75836,#75837,
#75838,#75839,#75840,#75841,#75842,#75843,#75844,#75845,#75846,#75847,#75848,
#75849,#75850),.UNSPECIFIED.,.F.,.F.,(4,2,2,2,2,2,2,2,4),(-117.190265949363,
-116.355349037468,-115.520432125574,-114.685515213679,-113.850598301784,
-113.015681389889,-112.180764477994,-111.345847566099,-110.907080642184),
 .UNSPECIFIED.);
#3535=B_SPLINE_CURVE_WITH_KNOTS('',3,(#75852,#75853,#75854,#75855,#75856,
#75857,#75858,#75859,#75860,#75861,#75862,#75863,#75864,#75865,#75866,#75867,
#75868,#75869),.UNSPECIFIED.,.F.,.F.,(4,2,2,2,2,2,2,2,4),(-110.907080642184,
-110.072163730289,-109.237246818394,-108.402329906499,-107.567412994604,
-106.732496082709,-105.897579170815,-105.06266225892,-104.623895335004),
 .UNSPECIFIED.);
#3536=B_SPLINE_CURVE_WITH_KNOTS('',3,(#75871,#75872,#75873,#75874,#75875,
#75876,#75877,#75878,#75879,#75880,#75881,#75882,#75883,#75884,#75885,#75886,
#75887,#75888),.UNSPECIFIED.,.F.,.F.,(4,2,2,2,2,2,2,2,4),(-104.623895335004,
-103.788978423109,-102.954061511214,-102.119144599319,-101.284227687425,
-100.44931077553,-99.6143938636348,-98.7794769517399,-98.3407182225155),
 .UNSPECIFIED.);
#3537=B_SPLINE_CURVE_WITH_KNOTS('',3,(#75890,#75891,#75892,#75893,#75894,
#75895,#75896,#75897,#75898,#75899,#75900,#75901,#75902,#75903,#75904,#75905,
#75906,#75907,#75908,#75909,#75910,#75911,#75912,#75913,#75914,#75915,#75916,
#75917,#75918,#75919,#75920,#75921,#75922,#75923,#75924,#75925,#75926,#75927,
#75928,#75929,#75930,#75931,#75932,#75933,#75934,#75935,#75936,#75937,#75938,
#75939,#75940,#75941,#75942,#75943,#75944,#75945,#75946,#75947,#75948,#75949,
#75950,#75951,#75952,#75953,#75954,#75955,#75956,#75957,#75958,#75959,#75960,
#75961,#75962,#75963,#75964,#75965,#75966,#75967,#75968,#75969,#75970,#75971,
#75972,#75973,#75974,#75975,#75976,#75977,#75978,#75979,#75980,#75981,#75982,
#75983,#75984,#75985,#75986,#75987,#75988,#75989,#75990,#75991,#75992,#75993,
#75994,#75995,#75996,#75997,#75998,#75999,#76000,#76001,#76002,#76003,#76004,
#76005,#76006,#76007,#76008,#76009,#76010,#76011,#76012,#76013,#76014,#76015,
#76016,#76017,#76018,#76019,#76020,#76021,#76022,#76023,#76024,#76025,#76026,
#76027,#76028,#76029,#76030,#76031,#76032,#76033,#76034,#76035,#76036,#76037,
#76038,#76039,#76040,#76041,#76042,#76043,#76044,#76045,#76046,#76047,#76048,
#76049,#76050,#76051,#76052,#76053,#76054,#76055,#76056,#76057,#76058,#76059,
#76060,#76061,#76062,#76063,#76064,#76065,#76066,#76067,#76068,#76069,#76070,
#76071,#76072,#76073,#76074,#76075,#76076,#76077,#76078,#76079,#76080,#76081,
#76082,#76083,#76084,#76085,#76086,#76087,#76088,#76089,#76090,#76091,#76092,
#76093,#76094,#76095,#76096,#76097,#76098,#76099,#76100,#76101,#76102,#76103,
#76104,#76105,#76106,#76107,#76108,#76109,#76110,#76111,#76112,#76113,#76114,
#76115),.UNSPECIFIED.,.F.,.F.,(4,3,3,3,3,3,3,3,3,3,3,3,3,3,3,3,3,3,3,3,
3,3,3,3,3,3,3,3,3,3,3,3,3,3,3,3,3,3,3,3,3,3,3,3,3,3,3,3,3,3,3,3,3,3,3,3,
3,3,3,3,3,3,3,3,3,3,3,3,3,3,3,3,3,3,3,4),(-98.3406829019419,-98.2437434225405,
-98.1464170814034,-98.0490921798296,-97.952002419303,-97.8552294380063,
-97.7598399901283,-97.6646221079338,-97.6235044607133,-97.5640891355954,
-97.5057931159296,-97.3426521359185,-97.2603547490666,-97.0941106891489,
-96.9279359782203,-96.7712320269567,-96.7617612672917,-96.6708762040348,
-96.5585454252642,-96.4438414670671,-96.3267705129137,-96.2629476276435,
-96.1459381539855,-96.0305291061737,-95.9199121328771,-95.8359592921399,
-95.7640576214475,-95.6654509547965,-95.566675161101,-95.4678165237561,
-95.4185008361925,-95.3290566577505,-95.2394267731222,-95.1506720310447,
-95.0641128465456,-95.0010423802451,-94.9076334079712,-94.8159559204494,
-94.7668960523893,-94.6740601804583,-94.5804783923981,-94.487591502431,
-94.4191609271352,-94.3450524977225,-94.2703865386836,-94.1955565765706,
-94.1661254683502,-94.0887540337746,-94.0088013892139,-93.9316962686835,
-93.854758696316,-93.7779778643584,-93.768943455532,-93.6921690976646,-93.6157128298723,
-93.5842440152404,-93.5061151209651,-93.4272088502916,-93.3472535258137,
-93.3312085564554,-93.2277417440618,-93.1234262934822,-93.0189022010898,
-92.9146773684954,-92.8109975883665,-92.7717831578707,-92.6695455287042,
-92.5794481812869,-92.5275488857113,-92.4962916445605,-92.4021323038907,
-92.3061118569842,-92.2728410231873,-92.1763014953801,-92.0805228281303,
-92.0575247206449),.UNSPECIFIED.);
#3538=B_SPLINE_CURVE_WITH_KNOTS('',3,(#76117,#76118,#76119,#76120,#76121,
#76122,#76123,#76124,#76125,#76126,#76127,#76128,#76129),.UNSPECIFIED.,
 .F.,.F.,(4,1,1,1,1,1,1,1,1,1,4),(-92.0575247206449,-91.7738990818901,-90.7763567005652,
-90.2775855099027,-89.7788143192403,-89.2800431285779,-88.7812719379154,
-87.7837295565905,-86.7861871752656,-85.7886447939407,-85.7743411505574),
 .UNSPECIFIED.);
#3539=B_SPLINE_CURVE_WITH_KNOTS('',3,(#76131,#76132,#76133,#76134,#76135,
#76136,#76137,#76138,#76139,#76140,#76141,#76142,#76143,#76144,#76145,#76146,
#76147,#76148,#76149,#76150,#76151,#76152,#76153,#76154,#76155,#76156,#76157,
#76158,#76159,#76160,#76161,#76162,#76163,#76164,#76165,#76166,#76167,#76168,
#76169,#76170,#76171,#76172,#76173,#76174,#76175,#76176,#76177,#76178,#76179,
#76180,#76181,#76182,#76183,#76184,#76185,#76186,#76187,#76188,#76189,#76190,
#76191,#76192,#76193,#76194,#76195,#76196,#76197,#76198,#76199,#76200,#76201,
#76202,#76203,#76204,#76205,#76206,#76207,#76208,#76209,#76210,#76211,#76212,
#76213,#76214,#76215,#76216,#76217,#76218,#76219,#76220,#76221,#76222,#76223,
#76224,#76225,#76226,#76227,#76228,#76229,#76230,#76231,#76232,#76233,#76234,
#76235,#76236,#76237,#76238,#76239,#76240,#76241,#76242,#76243,#76244,#76245,
#76246,#76247,#76248,#76249,#76250,#76251,#76252,#76253,#76254,#76255,#76256,
#76257,#76258,#76259,#76260,#76261,#76262,#76263,#76264,#76265,#76266,#76267,
#76268,#76269,#76270,#76271,#76272,#76273,#76274,#76275,#76276,#76277,#76278,
#76279,#76280,#76281,#76282,#76283,#76284,#76285,#76286,#76287,#76288,#76289,
#76290,#76291,#76292,#76293,#76294,#76295,#76296,#76297,#76298,#76299,#76300,
#76301,#76302,#76303,#76304,#76305,#76306,#76307,#76308,#76309,#76310,#76311,
#76312,#76313,#76314,#76315,#76316,#76317,#76318,#76319,#76320,#76321,#76322,
#76323,#76324,#76325,#76326,#76327,#76328,#76329,#76330,#76331,#76332,#76333,
#76334,#76335,#76336,#76337,#76338,#76339,#76340,#76341,#76342,#76343,#76344,
#76345,#76346,#76347,#76348,#76349,#76350,#76351,#76352,#76353,#76354,#76355,
#76356,#76357,#76358,#76359,#76360,#76361,#76362,#76363,#76364,#76365,#76366,
#76367,#76368,#76369,#76370,#76371,#76372,#76373,#76374,#76375,#76376,#76377,
#76378,#76379,#76380,#76381,#76382,#76383,#76384,#76385,#76386),
 .UNSPECIFIED.,.F.,.F.,(4,3,3,3,3,3,3,3,3,3,3,3,3,3,3,3,3,3,3,3,3,3,3,3,
3,3,3,3,3,3,3,3,3,3,3,3,3,3,3,3,3,3,3,3,3,3,3,3,3,3,3,3,3,3,3,3,3,3,3,3,
3,3,3,3,3,3,3,3,3,3,3,3,3,3,3,3,3,3,3,3,3,3,3,3,3,4),(-85.7743394134653,
-85.6939733990312,-85.6137248761189,-85.5327620579087,-85.4528102675906,
-85.3713419354345,-85.2898736032783,-85.2154572109321,-85.1410240498145,
-85.0665618574138,-84.9920179219637,-84.9174296034911,-84.8427371772053,
-84.7911024126159,-84.7145265905183,-84.6380182542315,-84.5615664624167,
-84.4851603139229,-84.4087889404489,-84.3318853268042,-84.2555428293141,
-84.1792007870672,-84.1028493540296,-84.0255270233449,-83.9491028561956,
-83.8713314437433,-83.793560031291,-83.7197679653234,-83.6460381066311,
-83.572357394795,-83.4987119974357,-83.425088049623,-83.3514599839301,-83.2947888406285,
-83.213362374789,-83.1318010807113,-83.047855223025,-82.9660217138412,-82.8810196819036,
-82.7960176499661,-82.7175840169603,-82.6392199655877,-82.5609206600491,
-82.4827000858693,-82.4045293408292,-82.3264163224614,-82.2972464593036,
-82.2208764315444,-82.1444895523973,-82.0680762514176,-81.9915942115689,
-81.9150748327382,-81.8384735092794,-81.7984752686412,-81.7230888899497,
-81.6477639131932,-81.5724875297967,-81.4972469636097,-81.4220294630957,
-81.3443923911233,-81.269164622136,-81.193920127921,-81.1186473513818,-81.0433347221388,
-80.9679331451636,-80.8924788750111,-80.8169267060524,-80.8009328873163,
-80.7277748731317,-80.6547054811617,-80.5817097828716,-80.5087729193186,
-80.4358800856856,-80.3630165173305,-80.2901540070714,-80.2172884404815,
-80.1444064749265,-80.0714947571072,-79.9984973705371,-79.9254531382524,
-79.8522989010521,-79.8033905059914,-79.7082675746029,-79.6139520835005,
-79.5212737556616,-79.4911542246076),.UNSPECIFIED.);
#3540=B_SPLINE_CURVE_WITH_KNOTS('',3,(#76388,#76389,#76390,#76391,#76392,
#76393,#76394,#76395,#76396,#76397,#76398,#76399,#76400),.UNSPECIFIED.,
 .F.,.F.,(4,1,1,1,1,1,1,1,1,1,4),(-79.4911541062857,-78.8058481246665,-78.3070769340041,
-77.8083057433416,-76.8107633620167,-76.3119921713543,-75.8132209806918,
-75.3144497900294,-74.8156785993669,-73.818136218042,-73.2079687991061),
 .UNSPECIFIED.);
#3541=B_SPLINE_CURVE_WITH_KNOTS('',3,(#76402,#76403,#76404,#76405,#76406,
#76407,#76408,#76409,#76410,#76411,#76412,#76413,#76414),.UNSPECIFIED.,
 .F.,.F.,(4,1,1,1,1,1,1,1,1,1,4),(-73.2079687991061,-72.8205938367171,-71.8230514553922,
-71.3242802647298,-70.8255090740674,-69.8279666927425,-69.32919550208,-68.8304243114176,
-68.3316531207551,-67.8328819300927,-66.9247834919265),.UNSPECIFIED.);
#3542=B_SPLINE_CURVE_WITH_KNOTS('',3,(#76416,#76417,#76418,#76419,#76420,
#76421,#76422,#76423,#76424,#76425,#76426,#76427,#76428,#76429),
 .UNSPECIFIED.,.F.,.F.,(4,1,1,1,1,1,1,1,1,1,1,4),(-66.9247834919265,-66.8353395487678,
-65.8377971674429,-64.840254786118,-64.3414835954556,-63.8427124047931,
-62.8451700234682,-62.3463988328058,-61.8476276421433,-61.3488564514809,
-60.8500852608184,-60.6415981847469),.UNSPECIFIED.);
#3543=B_SPLINE_CURVE_WITH_KNOTS('',3,(#76431,#76432,#76433,#76434,#76435,
#76436,#76437,#76438,#76439,#76440,#76441,#76442,#76443),.UNSPECIFIED.,
 .F.,.F.,(4,1,1,1,1,1,1,1,1,1,4),(-60.6415981847469,-59.8525428794935,-58.8550004981687,
-57.8574581168438,-57.3586869261813,-56.8599157355189,-55.862373354194,
-55.3636021635315,-54.8648309728691,-54.3660597822066,-54.3584128775673),
 .UNSPECIFIED.);
#3544=B_SPLINE_CURVE_WITH_KNOTS('',3,(#76445,#76446,#76447,#76448,#76449,
#76450,#76451,#76452,#76453,#76454,#76455,#76456,#76457,#76458,#76459,#76460,
#76461,#76462),.UNSPECIFIED.,.F.,.F.,(4,2,2,2,2,2,2,2,4),(-54.3584128775673,
-53.5234959656725,-52.6885790537776,-51.8536621418828,-51.0187452299879,
-50.183828318093,-49.3489114061982,-48.5139944943033,-48.0752275703878),
 .UNSPECIFIED.);
#3545=B_SPLINE_CURVE_WITH_KNOTS('',3,(#76464,#76465,#76466,#76467,#76468,
#76469,#76470,#76471,#76472,#76473,#76474,#76475,#76476,#76477,#76478,#76479,
#76480,#76481),.UNSPECIFIED.,.F.,.F.,(4,2,2,2,2,2,2,2,4),(-48.0752275703878,
-47.2403106584929,-46.405393746598,-45.5704768347032,-44.7355599228083,
-43.9006430109135,-43.0657260990186,-42.2308091871237,-41.7920422632082),
 .UNSPECIFIED.);
#3546=B_SPLINE_CURVE_WITH_KNOTS('',3,(#76483,#76484,#76485,#76486,#76487,
#76488,#76489,#76490,#76491,#76492,#76493,#76494,#76495,#76496,#76497,#76498,
#76499,#76500),.UNSPECIFIED.,.F.,.F.,(4,2,2,2,2,2,2,2,4),(-41.7920422632082,
-40.9571253513133,-40.1222084394185,-39.2872915275236,-38.4523746156287,
-37.6174577037339,-36.782540791839,-35.9476238799442,-35.5088569560286),
 .UNSPECIFIED.);
#3547=B_SPLINE_CURVE_WITH_KNOTS('',3,(#76502,#76503,#76504,#76505,#76506,
#76507,#76508,#76509,#76510,#76511,#76512,#76513,#76514,#76515,#76516,#76517,
#76518,#76519),.UNSPECIFIED.,.F.,.F.,(4,2,2,2,2,2,2,2,4),(-35.5088569560286,
-34.6739400441337,-33.8390231322389,-33.004106220344,-32.1691893084491,
-31.3342723965543,-30.4993554846594,-29.6644385727646,-29.225671648849),
 .UNSPECIFIED.);
#3548=B_SPLINE_CURVE_WITH_KNOTS('',3,(#76521,#76522,#76523,#76524,#76525,
#76526,#76527,#76528,#76529,#76530,#76531,#76532,#76533),.UNSPECIFIED.,
 .F.,.F.,(4,1,1,1,1,1,1,1,2,4),(-29.225671648849,-28.9287290584219,-27.931186677097,
-27.4324154864345,-26.9336442957721,-26.4348731051097,-25.9361019144472,
-24.9385595331223,-23.9410171517974,-22.9424863416694),.UNSPECIFIED.);
#3549=B_SPLINE_CURVE_WITH_KNOTS('',3,(#76535,#76536,#76537,#76538,#76539,
#76540,#76541,#76542,#76543,#76544,#76545,#76546,#76547),.UNSPECIFIED.,
 .F.,.F.,(4,1,1,1,1,1,1,1,1,1,4),(-22.9424863416694,-22.4447035798101,-21.9459323891476,
-20.9483900078227,-20.4496188171603,-19.9508476264979,-19.4520764358354,
-18.953305245173,-17.9557628638481,-16.9582204825232,-16.6593010344898),
 .UNSPECIFIED.);
#3550=B_SPLINE_CURVE_WITH_KNOTS('',3,(#76549,#76550,#76551,#76552,#76553,
#76554,#76555,#76556,#76557,#76558,#76559,#76560,#76561),.UNSPECIFIED.,
 .F.,.F.,(4,1,1,1,1,1,1,1,1,1,4),(-16.6593010344898,-15.9606781011983,-15.4619069105358,
-14.9631357198734,-13.9655933385485,-13.4668221478861,-12.9680509572236,
-12.4692797665612,-11.9705085758987,-10.9729661945738,-10.3761157273102),
 .UNSPECIFIED.);
#3551=B_SPLINE_CURVE_WITH_KNOTS('',3,(#76562,#76563,#76564,#76565,#76566,
#76567,#76568,#76569,#76570,#76571,#76572,#76573,#76574,#76575,#76576,#76577,
#76578,#76579,#76580,#76581,#76582,#76583,#76584,#76585,#76586,#76587,#76588,
#76589,#76590,#76591,#76592,#76593,#76594,#76595,#76596,#76597,#76598,#76599,
#76600,#76601,#76602,#76603,#76604,#76605,#76606,#76607,#76608,#76609,#76610,
#76611,#76612,#76613,#76614,#76615,#76616,#76617,#76618,#76619,#76620,#76621,
#76622,#76623,#76624,#76625,#76626,#76627,#76628,#76629,#76630,#76631,#76632,
#76633,#76634,#76635,#76636,#76637,#76638,#76639,#76640,#76641,#76642,#76643,
#76644,#76645,#76646,#76647,#76648,#76649,#76650,#76651,#76652,#76653,#76654,
#76655,#76656,#76657,#76658,#76659,#76660,#76661,#76662,#76663,#76664,#76665,
#76666,#76667,#76668,#76669,#76670,#76671,#76672,#76673,#76674,#76675,#76676,
#76677,#76678,#76679,#76680,#76681,#76682,#76683,#76684,#76685,#76686,#76687,
#76688,#76689,#76690,#76691,#76692,#76693,#76694,#76695,#76696,#76697,#76698,
#76699,#76700,#76701,#76702,#76703,#76704,#76705,#76706,#76707,#76708,#76709,
#76710,#76711,#76712,#76713,#76714,#76715,#76716,#76717,#76718,#76719,#76720,
#76721,#76722,#76723,#76724,#76725,#76726,#76727,#76728,#76729,#76730,#76731,
#76732,#76733,#76734,#76735,#76736,#76737,#76738,#76739,#76740,#76741,#76742,
#76743,#76744,#76745,#76746,#76747,#76748,#76749,#76750,#76751,#76752,#76753,
#76754,#76755,#76756,#76757,#76758,#76759,#76760,#76761,#76762,#76763,#76764,
#76765,#76766,#76767,#76768,#76769,#76770,#76771,#76772,#76773,#76774,#76775,
#76776,#76777,#76778,#76779,#76780,#76781,#76782,#76783,#76784,#76785,#76786,
#76787,#76788,#76789,#76790,#76791,#76792,#76793,#76794,#76795,#76796,#76797,
#76798,#76799,#76800,#76801,#76802,#76803,#76804,#76805,#76806,#76807,#76808,
#76809,#76810,#76811,#76812,#76813,#76814,#76815,#76816,#76817),
 .UNSPECIFIED.,.F.,.F.,(4,3,3,3,3,3,3,3,3,3,3,3,3,3,3,3,3,3,3,3,3,3,3,3,
3,3,3,3,3,3,3,3,3,3,3,3,3,3,3,3,3,3,3,3,3,3,3,3,3,3,3,3,3,3,3,3,3,3,3,3,
3,3,3,3,3,3,3,3,3,3,3,3,3,3,3,3,3,3,3,3,3,3,3,3,3,4),(-10.3761155991787,
-10.295606520528,-10.2146913962069,-10.133569882389,-10.0521153589786,-9.97542381324893,
-9.90082242327339,-9.82630646970646,-9.75186202983587,-9.67747522823774,
-9.60313222764775,-9.52497587818229,-9.45066896650611,-9.37636110658798,
-9.3020398161475,-9.22769260816435,-9.15327268902442,-9.07881051078405,
-9.00425886052311,-8.97788143192403,-8.89691300520634,-8.81606084545914,
-8.73182319440975,-8.65128703682939,-8.57087370924006,-8.49063373416483,
-8.47911024126159,-8.40467232653595,-8.33021746049187,-8.25573340166718,
-8.18116743951215,-8.10655699125635,-8.03184239740111,-7.98033905059914,
-7.90377167175971,-7.82727181501515,-7.75082852206479,-7.67443087479399,
-7.59806798792931,-7.52115907309743,-7.44482494298547,-7.36849119936814,
-7.29214798104616,-7.21481015310318,-7.13839390388424,-7.06059528657925,
-6.98279666927425,-6.9090272294558,-6.83532000708233,-6.761661926602,-6.68803909799174,
-6.61443769154234,-6.54083204558264,-6.4840254786118,-6.40241867513602,
-6.32067125792403,-6.23681701543036,-6.15479073653799,-6.07002251224367,
-5.98525428794935,-5.90721271412927,-5.82923946759867,-5.75132842618543,
-5.67348967314702,-5.59569614859377,-5.51795162298141,-5.48648309728691,
-5.40960063427011,-5.33269517011168,-5.25575826443357,-5.17874823782564,
-5.101698651857,-5.02456717534387,-4.98771190662446,-4.91378147830581,-4.83991642829119,
-4.76610243408189,-4.69232520981352,-4.61740086548968,-4.54364068820302,
-4.46987217167397,-4.39608241444794,-4.32029442464165,-4.24638719604415,
-4.16965882563346,-4.09293045522277),.UNSPECIFIED.);
#3552=B_SPLINE_CURVE_WITH_KNOTS('',3,(#76820,#76821,#76822,#76823,#76824,
#76825,#76826,#76827,#76828,#76829,#76830,#76831,#76832,#76833,#76834,#76835,
#76836,#76837,#76838,#76839,#76840,#76841,#76842,#76843,#76844,#76845,#76846,
#76847,#76848,#76849,#76850,#76851,#76852,#76853,#76854,#76855,#76856,#76857,
#76858,#76859,#76860,#76861,#76862,#76863,#76864,#76865,#76866,#76867,#76868,
#76869,#76870,#76871,#76872,#76873,#76874,#76875,#76876,#76877,#76878,#76879,
#76880,#76881,#76882,#76883,#76884,#76885,#76886,#76887,#76888,#76889,#76890,
#76891,#76892,#76893,#76894,#76895),.UNSPECIFIED.,.F.,.F.,(4,3,3,3,3,3,
3,3,3,3,3,3,3,3,3,3,3,3,3,3,3,3,3,3,3,4),(384.369389342789,384.451850946519,
384.534311884371,384.616772183743,384.699231872031,384.78169097663,384.86414952493,
384.946607544323,385.029065062195,385.11574202028,385.198208805821,385.280673918889,
385.363137469137,385.445599566196,385.528060319677,385.610519839173,385.692978234258,
385.775435614492,385.857902000178,385.940365201686,386.022825657536,386.105283806091,
386.187749409844,386.270209288232,386.352673399484,386.415896391544),
 .UNSPECIFIED.);
#3553=B_SPLINE_CURVE_WITH_KNOTS('',3,(#76897,#76898,#76899,#76900,#76901,
#76902,#76903,#76904,#76905,#76906,#76907,#76908,#76909,#76910,#76911,#76912,
#76913,#76914,#76915,#76916,#76917,#76918,#76919,#76920,#76921,#76922,#76923,
#76924,#76925,#76926,#76927,#76928,#76929,#76930,#76931,#76932,#76933,#76934,
#76935,#76936,#76937,#76938,#76939,#76940,#76941,#76942,#76943,#76944,#76945,
#76946,#76947,#76948,#76949,#76950,#76951,#76952,#76953,#76954,#76955,#76956,
#76957,#76958,#76959,#76960,#76961,#76962,#76963,#76964,#76965,#76966,#76967,
#76968,#76969,#76970,#76971,#76972,#76973,#76974,#76975,#76976,#76977,#76978,
#76979,#76980,#76981,#76982,#76983,#76984),.UNSPECIFIED.,.F.,.F.,(4,3,3,
3,3,3,3,3,3,3,3,3,3,3,3,3,3,3,3,3,3,3,3,3,3,3,3,3,3,4),(386.415896391544,
386.519916896913,386.627595730804,386.690968225979,386.766875587204,386.842686706208,
386.918418464482,386.994087656886,387.069711011893,387.14706096132,387.222657598836,
387.298261456307,387.373887613424,387.452543361894,387.528302185255,387.604118054994,
387.680040881299,387.688510607304,387.766536949769,387.844470266106,387.9223257434,
388.000118514048,388.077861083107,388.155576186865,388.233277447859,388.310978478188,
388.388721898678,388.466486616982,388.544326454714,388.606135786806),
 .UNSPECIFIED.);
#3554=B_SPLINE_CURVE_WITH_KNOTS('',3,(#76988,#76989,#76990,#76991,#76992,
#76993,#76994,#76995,#76996,#76997,#76998,#76999,#77000,#77001,#77002,#77003,
#77004,#77005,#77006,#77007,#77008,#77009,#77010,#77011,#77012,#77013,#77014,
#77015,#77016,#77017,#77018,#77019,#77020,#77021,#77022,#77023,#77024),
 .UNSPECIFIED.,.F.,.F.,(4,3,3,3,3,3,3,3,3,3,3,3,4),(386.416228946818,386.492961263492,
386.569655033906,386.646335793747,386.723006668584,386.799707977879,386.868462967424,
386.953194636385,387.037962795978,387.122762791903,387.207557598771,387.292327469878,
387.367234158086),.UNSPECIFIED.);
#3555=B_SPLINE_CURVE_WITH_KNOTS('',3,(#77025,#77026,#77027,#77028,#77029,
#77030,#77031,#77032,#77033,#77034,#77035,#77036,#77037,#77038,#77039,#77040,
#77041,#77042,#77043,#77044,#77045,#77046,#77047,#77048,#77049,#77050,#77051,
#77052,#77053,#77054,#77055,#77056,#77057,#77058,#77059,#77060,#77061,#77062,
#77063,#77064,#77065,#77066,#77067,#77068,#77069,#77070,#77071,#77072,#77073,
#77074,#77075,#77076,#77077,#77078,#77079,#77080,#77081,#77082,#77083,#77084,
#77085,#77086,#77087,#77088,#77089,#77090,#77091,#77092,#77093,#77094,#77095,
#77096,#77097,#77098,#77099,#77100),.UNSPECIFIED.,.F.,.F.,(4,3,3,3,3,3,
3,3,3,3,3,3,3,3,3,3,3,3,3,3,3,3,3,3,3,4),(384.36938934279,384.45185094652,
384.534311884372,384.616772183744,384.699231872032,384.78169097663,384.864149524931,
384.946607544324,385.029065062196,385.115742020281,385.198208805822,385.28067391889,
385.363137469137,385.445599566197,385.528060319678,385.610519839174,385.69297823426,
385.775435614493,385.857902000179,385.940365201687,386.022825657537,386.105283806092,
386.187749409845,386.270209288233,386.352673399486,386.415896391545),
 .UNSPECIFIED.);
#3556=B_SPLINE_CURVE_WITH_KNOTS('',3,(#79285,#79286,#79287,#79288,#79289,
#79290,#79291,#79292,#79293,#79294,#79295,#79296,#79297,#79298,#79299,#79300,
#79301,#79302,#79303,#79304,#79305,#79306,#79307,#79308,#79309,#79310,#79311,
#79312,#79313,#79314,#79315,#79316,#79317,#79318,#79319,#79320,#79321,#79322,
#79323,#79324,#79325,#79326,#79327,#79328,#79329,#79330,#79331,#79332,#79333,
#79334,#79335,#79336,#79337,#79338,#79339,#79340,#79341,#79342,#79343,#79344,
#79345,#79346,#79347,#79348,#79349,#79350,#79351,#79352,#79353,#79354,#79355,
#79356,#79357,#79358,#79359,#79360,#79361,#79362,#79363,#79364,#79365,#79366,
#79367,#79368,#79369,#79370,#79371,#79372,#79373,#79374,#79375,#79376,#79377,
#79378,#79379,#79380,#79381,#79382,#79383,#79384,#79385,#79386,#79387,#79388,
#79389,#79390,#79391,#79392,#79393,#79394,#79395,#79396),.UNSPECIFIED.,
 .F.,.F.,(4,3,3,3,3,3,3,3,3,3,3,3,3,3,3,3,3,3,3,3,3,3,3,3,3,3,3,3,3,3,3,
3,3,3,3,3,3,4),(-1.5287061066451,-1.46563278609545,-1.40366848264018,-1.34172139311797,
-1.32648945379474,-1.31592687441394,-1.25478040828007,-1.1937868575411,
-1.13659146157303,-1.12365124112427,-1.11392990179138,-1.07958806715143,
-1.0175020583394,-0.95735980222339,-0.897594901146072,-0.838755474514921,
-0.831244031903299,-0.822278048496474,-0.763680893830734,-0.706297406799082,
-0.647448671960985,-0.588997675249399,-0.558591305544723,-0.547035837801617,
-0.538520796827503,-0.481016200558624,-0.423876489176745,-0.367086474483784,
-0.346349267967161,-0.288951741053603,-0.28370495096647,-0.272562553273686,
-0.262826912836319,-0.20680074940186,-0.150577776627783,-0.0947036602514006,
-0.039876806877971,0.),.UNSPECIFIED.);
#3557=B_SPLINE_CURVE_WITH_KNOTS('',3,(#79397,#79398,#79399,#79400,#79401,
#79402,#79403,#79404,#79405,#79406,#79407,#79408,#79409,#79410,#79411,#79412,
#79413,#79414,#79415,#79416,#79417,#79418,#79419,#79420,#79421,#79422,#79423,
#79424,#79425,#79426,#79427,#79428,#79429,#79430,#79431,#79432,#79433,#79434,
#79435,#79436,#79437,#79438,#79439,#79440,#79441,#79442,#79443,#79444,#79445,
#79446,#79447,#79448,#79449,#79450,#79451,#79452,#79453,#79454,#79455,#79456,
#79457,#79458,#79459,#79460,#79461,#79462,#79463,#79464,#79465,#79466,#79467,
#79468,#79469,#79470,#79471,#79472,#79473,#79474,#79475,#79476,#79477,#79478,
#79479,#79480,#79481,#79482,#79483,#79484,#79485,#79486,#79487,#79488,#79489,
#79490,#79491,#79492,#79493,#79494,#79495,#79496,#79497,#79498,#79499,#79500,
#79501,#79502,#79503,#79504,#79505,#79506,#79507,#79508),.UNSPECIFIED.,
 .F.,.F.,(4,3,3,3,3,3,3,3,3,3,3,3,3,3,3,3,3,3,3,3,3,3,3,3,3,3,3,3,3,3,3,
3,3,3,3,3,3,4),(0.,0.0545106824407012,0.108992246219552,0.164300448223578,
0.220448606574958,0.265804300761185,0.27240010972656,0.328717061982265,
0.386064106174773,0.403165036736809,0.460671233468054,0.518311395019354,
0.53396435510986,0.542259344152256,0.549928427684927,0.608631374891456,
0.667610836158375,0.726335850589568,0.765244330794922,0.809377107743138,
0.821963747402437,0.832575451855005,0.890877486210268,0.950588397110567,
1.01065953636793,1.07043858295781,1.11830654638065,1.12643018240209,1.14048721636953,
1.20067707539853,1.26153051799682,1.29492746657787,1.31795046485262,1.32913658579,
1.39094257766379,1.45298891535971,1.51475741177567,1.5287061066452),
 .UNSPECIFIED.);
#3558=B_SPLINE_CURVE_WITH_KNOTS('',3,(#81693,#81694,#81695,#81696,#81697,
#81698,#81699,#81700,#81701,#81702,#81703,#81704,#81705,#81706,#81707,#81708,
#81709,#81710,#81711,#81712,#81713,#81714,#81715,#81716,#81717,#81718,#81719,
#81720,#81721,#81722,#81723,#81724,#81725,#81726,#81727,#81728,#81729,#81730,
#81731,#81732,#81733,#81734,#81735,#81736,#81737,#81738,#81739,#81740,#81741,
#81742,#81743,#81744,#81745,#81746,#81747,#81748,#81749,#81750,#81751,#81752,
#81753,#81754,#81755,#81756,#81757,#81758,#81759,#81760,#81761,#81762,#81763,
#81764,#81765,#81766,#81767,#81768,#81769,#81770,#81771,#81772,#81773,#81774,
#81775,#81776,#81777,#81778,#81779,#81780,#81781,#81782,#81783,#81784,#81785,
#81786,#81787,#81788,#81789,#81790,#81791,#81792,#81793,#81794,#81795,#81796,
#81797,#81798),.UNSPECIFIED.,.F.,.F.,(4,3,3,3,3,3,3,3,3,3,3,3,3,3,3,3,3,
3,3,3,3,3,3,3,3,3,3,3,3,3,3,3,3,3,3,4),(-1.5337369924873,-1.47910110659077,
-1.42364061709559,-1.3681801276004,-1.35627281297634,-1.3472470912004,-1.29117883986854,
-1.23440724571817,-1.17721536336885,-1.16839365668255,-1.16075205045248,
-1.13001159231546,-1.07138046030213,-1.01314818419106,-0.954317624226592,
-0.895487064262123,-0.888451348769209,-0.881320522452671,-0.821738837487018,
-0.766771277739479,-0.708056182374627,-0.648681097977743,-0.602036123386777,
-0.595834923297491,-0.535881606952541,-0.475330179668211,-0.414610032838359,
-0.390005676689811,-0.329435956673073,-0.309660837375982,-0.299293319274086,
-0.238580681129937,-0.176748134609211,-0.114706770089442,-0.0530932525039872,
0.),.UNSPECIFIED.);
#3559=B_SPLINE_CURVE_WITH_KNOTS('',3,(#81799,#81800,#81801,#81802,#81803,
#81804,#81805,#81806,#81807,#81808,#81809,#81810,#81811,#81812,#81813,#81814,
#81815,#81816,#81817,#81818,#81819,#81820,#81821,#81822,#81823,#81824,#81825,
#81826,#81827,#81828,#81829,#81830,#81831,#81832,#81833,#81834,#81835,#81836,
#81837,#81838,#81839,#81840,#81841,#81842,#81843,#81844,#81845,#81846,#81847,
#81848,#81849,#81850,#81851,#81852,#81853,#81854,#81855,#81856,#81857,#81858,
#81859,#81860,#81861,#81862,#81863,#81864,#81865,#81866,#81867,#81868,#81869,
#81870,#81871,#81872,#81873,#81874,#81875,#81876,#81877,#81878,#81879,#81880,
#81881,#81882,#81883,#81884,#81885,#81886,#81887,#81888,#81889,#81890,#81891,
#81892,#81893,#81894,#81895,#81896,#81897,#81898,#81899,#81900,#81901,#81902,
#81903,#81904,#81905,#81906,#81907,#81908,#81909,#81910,#81911,#81912,#81913),
 .UNSPECIFIED.,.F.,.F.,(4,3,3,3,3,3,3,3,3,3,3,3,3,3,3,3,3,3,3,3,3,3,3,3,
3,3,3,3,3,3,3,3,3,3,3,3,3,3,4),(0.,0.0633019324654129,0.12491271385973,
0.186949391078483,0.248706534299387,0.299397460630789,0.309169279515443,
0.369823137865797,0.43050954289667,0.451329337802415,0.512095985193222,
0.572332100986119,0.588852907602698,0.599399630443956,0.607101257943028,
0.623405281176508,0.68288782162807,0.742060156956974,0.800329933464109,
0.82591160309259,0.86860772496703,0.880796950572916,0.888966192736701,0.902581013409931,
0.960529646986361,1.01866415529143,1.07634930727061,1.13279238012094,1.16748057808811,
1.18322808695813,1.18681525711862,1.24385416478557,1.3008962452759,1.3498146643194,
1.35813634882905,1.41433556809954,1.46986785043297,1.52519276368421,1.53373699248745),
 .UNSPECIFIED.);
#3560=B_SPLINE_CURVE_WITH_KNOTS('',3,(#81965,#81966,#81967,#81968,#81969,
#81970,#81971,#81972,#81973,#81974,#81975,#81976,#81977,#81978,#81979,#81980,
#81981,#81982,#81983,#81984,#81985,#81986,#81987,#81988,#81989,#81990,#81991,
#81992,#81993,#81994,#81995,#81996,#81997,#81998,#81999,#82000,#82001,#82002,
#82003,#82004,#82005,#82006,#82007,#82008,#82009,#82010,#82011,#82012,#82013,
#82014,#82015,#82016,#82017,#82018,#82019,#82020,#82021,#82022,#82023,#82024,
#82025,#82026,#82027,#82028),.UNSPECIFIED.,.F.,.F.,(4,3,3,3,3,3,3,3,3,3,
3,3,3,3,3,3,3,3,3,3,3,4),(0.479292617177209,0.505000840917307,0.530713137629105,
0.547756394224347,0.57336762750038,0.598976297476449,0.62458735299975,0.650198139465077,
0.675813884972614,0.684683947910694,0.710199819641625,0.735710769342924,
0.761221509088754,0.786730721796191,0.812243799751802,0.821611501597041,
0.847360903592922,0.873107128637788,0.898853495292093,0.924597895094032,
0.95034373058283,0.958539055283388),.UNSPECIFIED.);
#3561=B_SPLINE_CURVE_WITH_KNOTS('',3,(#82030,#82031,#82032,#82033,#82034,
#82035,#82036,#82037,#82038,#82039,#82040,#82041,#82042,#82043,#82044,#82045,
#82046,#82047,#82048,#82049,#82050,#82051,#82052,#82053,#82054,#82055,#82056,
#82057,#82058,#82059,#82060,#82061,#82062,#82063,#82064,#82065,#82066,#82067,
#82068,#82069,#82070,#82071,#82072,#82073,#82074,#82075,#82076,#82077,#82078,
#82079,#82080,#82081,#82082,#82083,#82084,#82085,#82086,#82087,#82088,#82089,
#82090,#82091,#82092,#82093,#82094,#82095,#82096,#82097,#82098,#82099,#82100,
#82101,#82102,#82103,#82104,#82105,#82106,#82107,#82108,#82109,#82110,#82111,
#82112,#82113,#82114,#82115,#82116,#82117,#82118,#82119,#82120,#82121,#82122,
#82123,#82124,#82125,#82126,#82127,#82128,#82129,#82130,#82131,#82132),
 .UNSPECIFIED.,.F.,.F.,(4,3,3,3,3,3,3,3,3,3,3,3,3,3,3,3,3,3,3,3,3,3,3,3,
3,3,3,3,3,3,3,3,3,3,4),(0.,0.0255611682442398,0.0511196475252543,0.0766807791052086,
0.102241920428134,0.127808798952552,0.136937787707076,0.162568577806161,
0.188195056364783,0.213821211828165,0.23944549133029,0.265072298366607,
0.273875575414151,0.299433431887937,0.32498835629455,0.350545625560006,
0.376102741264404,0.401665398667488,0.410813363121227,0.436405033823088,
0.461991883117399,0.487578024623893,0.513162172427522,0.538748975424076,
0.547751150828302,0.573364266367873,0.59897482287007,0.624587772130241,
0.650200456525016,0.675818106794432,0.684688938535378,0.710236075973954,
0.735777726404149,0.761318556176312,0.780281541707351),.UNSPECIFIED.);
#3562=B_SPLINE_CURVE_WITH_KNOTS('',3,(#82136,#82137,#82138,#82139,#82140,
#82141),.UNSPECIFIED.,.F.,.F.,(4,2,4),(0.,0.216145308133088,0.432258182334419),
 .UNSPECIFIED.);
#3563=B_SPLINE_CURVE_WITH_KNOTS('',3,(#82142,#82143,#82144,#82145,#82146,
#82147,#82148,#82149,#82150,#82151,#82152,#82153,#82154,#82155,#82156,#82157,
#82158,#82159,#82160,#82161,#82162,#82163,#82164,#82165,#82166,#82167,#82168,
#82169,#82170,#82171,#82172,#82173,#82174,#82175,#82176,#82177,#82178,#82179,
#82180,#82181,#82182,#82183,#82184,#82185,#82186,#82187,#82188,#82189,#82190,
#82191,#82192,#82193,#82194,#82195,#82196,#82197,#82198,#82199,#82200,#82201,
#82202,#82203,#82204,#82205),.UNSPECIFIED.,.F.,.F.,(4,3,3,3,3,3,3,3,3,3,
3,3,3,3,3,3,3,3,3,3,3,4),(0.,0.0257479719507909,0.0514943137831926,0.0772430807474856,
0.102991209339309,0.12874269019043,0.136940747823198,0.162456524286232,
0.18796862101097,0.213482344429356,0.23899560263191,0.264514271518437,0.273881495646396,
0.299499689510765,0.325113349245822,0.350726484436241,0.376337663430009,
0.401951356406392,0.410822243469594,0.436536016946579,0.462248012834959,
0.47929261717721),.UNSPECIFIED.);
#3564=B_SPLINE_CURVE_WITH_KNOTS('',3,(#82211,#82212,#82213,#82214,#82215,
#82216,#82217,#82218,#82219,#82220,#82221,#82222,#82223,#82224,#82225,#82226,
#82227,#82228,#82229,#82230,#82231,#82232,#82233,#82234,#82235,#82236,#82237,
#82238,#82239,#82240,#82241,#82242,#82243,#82244,#82245,#82246,#82247,#82248,
#82249,#82250,#82251,#82252,#82253,#82254,#82255,#82256,#82257,#82258,#82259,
#82260,#82261,#82262,#82263,#82264,#82265,#82266,#82267,#82268,#82269,#82270,
#82271,#82272,#82273,#82274),.UNSPECIFIED.,.F.,.F.,(4,3,3,3,3,3,3,3,3,3,
3,3,3,3,3,3,3,3,3,3,3,4),(0.479292617177209,0.505001327382096,0.530714120836313,
0.547756394224347,0.573367708107215,0.5989764517365,0.624587569678354,0.650198411765993,
0.675814202278988,0.684683947910694,0.710199270596006,0.735709680648712,
0.761219898903124,0.786728601757571,0.812241190362207,0.82161150159704,
0.847361553520347,0.873108430011801,0.89885544393772,0.92460048661686,0.950346953615207,
0.958539055283387),.UNSPECIFIED.);
#3565=B_SPLINE_CURVE_WITH_KNOTS('',3,(#82276,#82277,#82278,#82279,#82280,
#82281,#82282,#82283,#82284,#82285,#82286,#82287,#82288,#82289,#82290,#82291,
#82292,#82293,#82294,#82295,#82296,#82297,#82298,#82299,#82300,#82301,#82302,
#82303,#82304,#82305,#82306,#82307,#82308,#82309,#82310,#82311,#82312,#82313,
#82314,#82315,#82316,#82317,#82318,#82319,#82320,#82321,#82322,#82323,#82324,
#82325,#82326,#82327,#82328,#82329,#82330,#82331,#82332,#82333,#82334,#82335,
#82336,#82337,#82338,#82339,#82340,#82341,#82342,#82343,#82344,#82345,#82346,
#82347,#82348,#82349,#82350,#82351,#82352,#82353,#82354,#82355,#82356,#82357,
#82358,#82359,#82360,#82361,#82362,#82363,#82364,#82365,#82366,#82367,#82368,
#82369,#82370,#82371,#82372,#82373,#82374,#82375,#82376,#82377,#82378,#82379,
#82380,#82381,#82382,#82383,#82384,#82385,#82386,#82387,#82388,#82389,#82390,
#82391,#82392,#82393,#82394,#82395,#82396,#82397,#82398,#82399,#82400,#82401,
#82402),.UNSPECIFIED.,.F.,.F.,(4,3,3,3,3,3,3,3,3,3,3,3,3,3,3,3,3,3,3,3,
3,3,3,3,3,3,3,3,3,3,3,3,3,3,3,3,3,3,3,3,3,3,4),(0.,0.0255611464246521,0.05111961735306,
0.0766807545207074,0.102241907980011,0.127808803185896,0.13693415075477,
0.162564198332204,0.188189930450198,0.21381533459465,0.239438860313218,
0.265064910696906,0.273868301509539,0.299425506394592,0.324979768153375,
0.35053635819426,0.376092785100791,0.401654739600194,0.410802452264309,
0.436393221748823,0.46197917265453,0.487564421430711,0.513147680282411,
0.538733601021664,0.547736603019078,0.573349086037912,0.598959003993817,
0.62457130498956,0.650183335334688,0.675800322512345,0.684670753773848,
0.710187725086894,0.73569977633771,0.761211621888362,0.786721943062233,
0.812236134492197,0.821604904528618,0.847355702730773,0.873103324254661,
0.89885108648345,0.924596880763502,0.9503441081478,0.958539055283387),
 .UNSPECIFIED.);
#3566=B_SPLINE_CURVE_WITH_KNOTS('',3,(#82403,#82404,#82405,#82406,#82407,
#82408,#82409,#82410,#82411,#82412,#82413,#82414,#82415,#82416,#82417,#82418,
#82419,#82420,#82421,#82422,#82423,#82424,#82425,#82426,#82427,#82428,#82429,
#82430,#82431,#82432,#82433,#82434,#82435,#82436,#82437,#82438,#82439,#82440,
#82441,#82442,#82443,#82444,#82445,#82446,#82447,#82448,#82449,#82450,#82451,
#82452,#82453,#82454,#82455,#82456,#82457,#82458,#82459,#82460,#82461,#82462,
#82463,#82464,#82465,#82466),.UNSPECIFIED.,.F.,.F.,(4,3,3,3,3,3,3,3,3,3,
3,3,3,3,3,3,3,3,3,3,3,4),(0.,0.0255621962959842,0.0511217133779092,0.0766838931244148,
0.102246087451785,0.12781402264808,0.136940747823198,0.162572051839977,
0.188199041285704,0.213825704029898,0.239450488906111,0.265077799247033,
0.273881495646396,0.299439922937785,0.324995409932617,0.35055322974378,
0.376110888981581,0.401674079835378,0.410822243469594,0.436808285767853,
0.462788710530963,0.479292617177209),.UNSPECIFIED.);
#3567=B_SPLINE_CURVE_WITH_KNOTS('',3,(#82468,#82469,#82470,#82471,#82472,
#82473,#82474,#82475,#82476,#82477,#82478,#82479,#82480,#82481,#82482,#82483,
#82484,#82485,#82486,#82487,#82488,#82489,#82490,#82491,#82492,#82493,#82494,
#82495,#82496,#82497,#82498,#82499,#82500,#82501,#82502,#82503,#82504,#82505,
#82506,#82507,#82508,#82509,#82510,#82511,#82512,#82513,#82514,#82515,#82516,
#82517,#82518,#82519,#82520,#82521,#82522,#82523,#82524,#82525,#82526,#82527,
#82528,#82529,#82530,#82531),.UNSPECIFIED.,.F.,.F.,(4,3,3,3,3,3,3,3,3,3,
3,3,3,3,3,3,3,3,3,3,3,4),(0.47929261717721,0.50526908884444,0.531253388712084,
0.547756394224346,0.573317123506841,0.598872836724378,0.624427812859824,
0.649980850854883,0.675536835901665,0.684683947910693,0.710308819151011,
0.735931126543647,0.761555691319374,0.787179876706826,0.812808757477038,
0.82161150159704,0.847176507707005,0.872736342186476,0.898295157372897,
0.923851855982624,0.949411200600672,0.958539055283387),.UNSPECIFIED.);
#3568=B_SPLINE_CURVE_WITH_KNOTS('',3,(#82533,#82534,#82535,#82536,#82537,
#82538,#82539,#82540,#82541,#82542,#82543,#82544,#82545,#82546,#82547,#82548,
#82549,#82550,#82551,#82552,#82553,#82554,#82555,#82556,#82557,#82558,#82559,
#82560,#82561,#82562,#82563,#82564,#82565,#82566,#82567,#82568,#82569,#82570,
#82571,#82572,#82573,#82574,#82575,#82576,#82577,#82578,#82579,#82580,#82581,
#82582,#82583,#82584,#82585,#82586,#82587,#82588,#82589,#82590,#82591,#82592,
#82593,#82594,#82595,#82596,#82597,#82598,#82599,#82600,#82601,#82602,#82603,
#82604,#82605,#82606,#82607,#82608,#82609,#82610,#82611,#82612,#82613,#82614,
#82615,#82616,#82617,#82618,#82619,#82620,#82621,#82622,#82623,#82624,#82625,
#82626,#82627,#82628,#82629,#82630,#82631,#82632,#82633,#82634,#82635,#82636,
#82637,#82638,#82639,#82640,#82641,#82642,#82643,#82644,#82645,#82646,#82647,
#82648,#82649,#82650,#82651,#82652,#82653,#82654,#82655,#82656,#82657,#82658,
#82659),.UNSPECIFIED.,.F.,.F.,(4,3,3,3,3,3,3,3,3,3,3,3,3,3,3,3,3,3,3,3,
3,3,3,3,3,3,3,3,3,3,3,3,3,3,3,3,3,3,3,3,3,3,4),(0.,0.0257468698833424,0.0514921116641796,
0.0772397799040712,0.102986810214673,0.128737192099745,0.136934150754769,
0.162448594603267,0.187959355420383,0.213471738614108,0.238983654397716,
0.264500978128848,0.273868301509539,0.299485263220318,0.32509769272638,
0.350709600094688,0.376319552699293,0.401932020998882,0.410802452264308,
0.436388483272024,0.461971827501006,0.48755761887005,0.513143244771744,
0.538734180026944,0.547736603019078,0.573298556820878,0.598855497016331,
0.624411704087103,0.649965975236065,0.675523196940356,0.684670753773847,
0.710296844933874,0.735920372698376,0.761546159030797,0.787171566648004,
0.812801671053547,0.821604904528617,0.847171306528443,0.872732535722516,
0.898292742853538,0.923850831355127,0.949411562047455,0.958539055283386),
 .UNSPECIFIED.);
#3569=B_SPLINE_CURVE_WITH_KNOTS('',3,(#82660,#82661,#82662,#82663,#82664,
#82665,#82666,#82667,#82668,#82669,#82670,#82671,#82672,#82673,#82674,#82675,
#82676,#82677,#82678,#82679,#82680,#82681,#82682,#82683,#82684,#82685,#82686,
#82687,#82688,#82689,#82690,#82691,#82692,#82693,#82694,#82695,#82696,#82697,
#82698,#82699,#82700,#82701,#82702,#82703,#82704,#82705,#82706,#82707,#82708,
#82709,#82710,#82711,#82712,#82713,#82714,#82715,#82716,#82717,#82718,#82719,
#82720,#82721,#82722,#82723),.UNSPECIFIED.,.F.,.F.,(4,3,3,3,3,3,3,3,3,3,
3,3,3,3,3,3,3,3,3,3,3,4),(0.,0.0257485479088003,0.0514954739738495,0.0772448314910723,
0.102993552532202,0.128745623912882,0.136940747823198,0.16245608850035,
0.187967734750382,0.213480989744456,0.23899377013341,0.264511950710105,
0.273881495646396,0.299499709480288,0.3251133965368,0.35072656922542,0.376337791412174,
0.401951535304368,0.410822243469594,0.436536442242556,0.462248854910223,
0.47929261717721),.UNSPECIFIED.);
#3570=B_SPLINE_CURVE_WITH_KNOTS('',3,(#82729,#82730,#82731,#82732,#82733,
#82734,#82735,#82736,#82737,#82738,#82739,#82740,#82741,#82742,#82743,#82744,
#82745,#82746,#82747,#82748,#82749,#82750,#82751,#82752,#82753,#82754,#82755,
#82756,#82757,#82758,#82759,#82760,#82761,#82762,#82763,#82764,#82765,#82766,
#82767,#82768,#82769,#82770,#82771,#82772,#82773,#82774,#82775,#82776,#82777,
#82778,#82779,#82780,#82781,#82782,#82783,#82784,#82785,#82786,#82787,#82788,
#82789,#82790,#82791,#82792),.UNSPECIFIED.,.F.,.F.,(4,3,3,3,3,3,3,3,3,3,
3,3,3,3,3,3,3,3,3,3,3,4),(0.479292617177209,0.505001679057846,0.530714831987189,
0.547756394224347,0.573367782262073,0.598976595249061,0.624587774647072,
0.650198673372923,0.675814512887766,0.684683947910694,0.710198896452721,
0.735708938883533,0.761218802071892,0.78672715789912,0.812239413611988,
0.82161150159704,0.84736198318122,0.873109289958388,0.898856730869144,0.924602197319219,
0.950349080143881,0.958539055283387),.UNSPECIFIED.);
#3571=B_SPLINE_CURVE_WITH_KNOTS('',3,(#82794,#82795,#82796,#82797,#82798,
#82799,#82800,#82801,#82802,#82803,#82804,#82805,#82806,#82807,#82808,#82809,
#82810,#82811,#82812,#82813,#82814,#82815,#82816,#82817,#82818,#82819,#82820,
#82821,#82822,#82823,#82824,#82825,#82826,#82827,#82828,#82829,#82830,#82831,
#82832,#82833,#82834,#82835,#82836,#82837,#82838,#82839,#82840,#82841,#82842,
#82843,#82844,#82845,#82846,#82847,#82848,#82849,#82850,#82851,#82852,#82853,
#82854,#82855,#82856,#82857,#82858,#82859,#82860,#82861,#82862,#82863,#82864,
#82865,#82866,#82867,#82868,#82869,#82870,#82871,#82872,#82873,#82874,#82875,
#82876,#82877,#82878,#82879,#82880,#82881,#82882,#82883,#82884,#82885,#82886,
#82887,#82888,#82889,#82890,#82891,#82892,#82893,#82894,#82895,#82896,#82897,
#82898,#82899,#82900,#82901,#82902,#82903,#82904,#82905,#82906,#82907,#82908,
#82909,#82910,#82911,#82912,#82913,#82914,#82915,#82916,#82917,#82918,#82919,
#82920),.UNSPECIFIED.,.F.,.F.,(4,3,3,3,3,3,3,3,3,3,3,3,3,3,3,3,3,3,3,3,
3,3,3,3,3,3,3,3,3,3,3,3,3,3,3,3,3,3,3,3,3,3,4),(0.,0.0255619939227406,0.0511213281374935,
0.0766833444398237,0.102245384185567,0.127813169841507,0.13693415075477,
0.162564057304859,0.188189643439327,0.213814896138194,0.239438267791297,
0.265064161788029,0.273868301509539,0.299425560181825,0.324979862788474,
0.350536474274596,0.376092911315033,0.401654859286199,0.410802452264309,
0.436392939165486,0.461978611441267,0.487563589554087,0.513146582949068,
0.538732247536879,0.547736603019078,0.573349179912026,0.598959184439744,
0.624571560133446,0.650183657974615,0.67580070134257,0.684670753773848,
0.71018715005693,0.735698636171859,0.761209935684971,0.786719723058999,
0.812233402235842,0.821604904528618,0.847356377225811,0.873104674637665,
0.898853108159833,0.924599569023129,0.950347450985566,0.958539055283387),
 .UNSPECIFIED.);
#3572=B_SPLINE_CURVE_WITH_KNOTS('',3,(#82921,#82922,#82923,#82924,#82925,
#82926,#82927,#82928,#82929,#82930,#82931,#82932,#82933,#82934,#82935,#82936,
#82937,#82938,#82939,#82940,#82941,#82942,#82943,#82944,#82945,#82946,#82947,
#82948,#82949,#82950,#82951,#82952,#82953,#82954,#82955,#82956,#82957,#82958,
#82959,#82960,#82961,#82962,#82963,#82964,#82965,#82966,#82967,#82968,#82969,
#82970,#82971,#82972,#82973,#82974,#82975,#82976,#82977,#82978,#82979,#82980,
#82981,#82982,#82983,#82984),.UNSPECIFIED.,.F.,.F.,(4,3,3,3,3,3,3,3,3,3,
3,3,3,3,3,3,3,3,3,3,3,4),(0.,0.0255629888202805,0.0511233135427478,0.0766863162753848,
0.102249340582942,0.127818110100948,0.136940747823198,0.162571934653423,
0.188198802218777,0.213825337772865,0.239449992859417,0.265077170929289,
0.273881495646396,0.299439968602179,0.3249954888192,0.350553323253718,0.376110986287893,
0.401674165036479,0.410822243469594,0.436807223890087,0.4627865956417,0.479292617174637),
 .UNSPECIFIED.);
#3573=B_SPLINE_CURVE_WITH_KNOTS('',3,(#82986,#82987,#82988,#82989,#82990,
#82991,#82992,#82993,#82994,#82995,#82996,#82997,#82998,#82999,#83000,#83001,
#83002,#83003,#83004,#83005,#83006,#83007,#83008,#83009,#83010,#83011,#83012,
#83013,#83014,#83015,#83016,#83017,#83018,#83019,#83020,#83021,#83022,#83023,
#83024,#83025,#83026,#83027,#83028,#83029,#83030,#83031,#83032,#83033,#83034,
#83035,#83036,#83037,#83038,#83039,#83040,#83041,#83042,#83043,#83044,#83045,
#83046,#83047,#83048,#83049),.UNSPECIFIED.,.F.,.F.,(4,3,3,3,3,3,3,3,3,3,
3,3,3,3,3,3,3,3,3,3,3,4),(0.47929261717721,0.505268190015835,0.53125158411797,
0.547756394224346,0.573317100440759,0.598872801966681,0.624427783168165,
0.649980835915105,0.675536849746693,0.684683947910693,0.710308737821271,
0.735930966056476,0.761555456007261,0.78717956941456,0.812808383216706,
0.82161150159704,0.847177217066114,0.872737757364608,0.898297267271713,
0.923854652547247,0.949414667311442,0.958539055283387),.UNSPECIFIED.);
#3574=B_SPLINE_CURVE_WITH_KNOTS('',3,(#83051,#83052,#83053,#83054,#83055,
#83056,#83057,#83058,#83059,#83060,#83061,#83062,#83063,#83064,#83065,#83066,
#83067,#83068,#83069,#83070,#83071,#83072,#83073,#83074,#83075,#83076,#83077,
#83078,#83079,#83080,#83081,#83082,#83083,#83084,#83085,#83086,#83087,#83088,
#83089,#83090,#83091,#83092,#83093,#83094,#83095,#83096,#83097,#83098,#83099,
#83100,#83101,#83102,#83103,#83104,#83105,#83106,#83107,#83108,#83109,#83110,
#83111,#83112,#83113,#83114,#83115,#83116,#83117,#83118,#83119,#83120,#83121,
#83122,#83123,#83124,#83125,#83126,#83127,#83128,#83129,#83130,#83131,#83132,
#83133,#83134,#83135,#83136,#83137,#83138,#83139,#83140,#83141,#83142,#83143,
#83144,#83145,#83146,#83147,#83148,#83149,#83150,#83151,#83152,#83153,#83154,
#83155,#83156,#83157,#83158,#83159,#83160,#83161,#83162,#83163,#83164,#83165,
#83166,#83167,#83168,#83169,#83170,#83171,#83172,#83173,#83174,#83175,#83176,
#83177),.UNSPECIFIED.,.F.,.F.,(4,3,3,3,3,3,3,3,3,3,3,3,3,3,3,3,3,3,3,3,
3,3,3,3,3,3,3,3,3,3,3,3,3,3,3,3,3,3,3,3,3,3,4),(0.,0.0257474663313306,0.051493313275948,
0.0772415934420302,0.102989237768966,0.128740231865067,0.136934150754769,
0.162448139512518,0.187958429852175,0.213470323759636,0.238981740416334,
0.264498554012216,0.273868301509539,0.299485292022666,0.325097758125654,
0.350709712822948,0.376319718744946,0.401932248431029,0.410802452264308,
0.436388264300392,0.461971383426754,0.487556942438714,0.513142332269183,
0.538733027566822,0.547736603019078,0.573298537314448,0.598855469883609,
0.624411686786277,0.64996597784542,0.675523234025067,0.684670753773847,
0.710296746065935,0.735920177050789,0.76154587098572,0.787171189128425,
0.812801209325657,0.821604904528617,0.847172060057425,0.872734039337613,
0.898294985218545,0.923853804170973,0.949415248127543,0.958539055283386),
 .UNSPECIFIED.);
#3575=B_SPLINE_CURVE_WITH_KNOTS('',3,(#83178,#83179,#83180,#83181,#83182,
#83183,#83184,#83185,#83186,#83187,#83188,#83189,#83190,#83191,#83192,#83193,
#83194,#83195,#83196,#83197,#83198,#83199,#83200,#83201,#83202,#83203,#83204,
#83205,#83206,#83207,#83208,#83209,#83210,#83211,#83212,#83213,#83214,#83215,
#83216,#83217,#83218,#83219,#83220,#83221,#83222,#83223,#83224,#83225,#83226,
#83227,#83228,#83229,#83230,#83231,#83232,#83233,#83234,#83235,#83236,#83237,
#83238,#83239,#83240,#83241),.UNSPECIFIED.,.F.,.F.,(4,3,3,3,3,3,3,3,3,3,
3,3,3,3,3,3,3,3,3,3,3,4),(0.,0.0257492105713833,0.0514968095059438,0.0772468481796215,
0.102996253150109,0.12874900710514,0.136940747823198,0.162455568546276,
0.187966677069076,0.213479372579753,0.238991582093521,0.264509179016115,
0.273881495646396,0.299499769501555,0.325113525936777,0.350726780699462,
0.376338091987283,0.401951934277687,0.410822243469594,0.436536985254516,
0.462249929267478,0.47929261717721),.UNSPECIFIED.);
#3576=B_SPLINE_CURVE_WITH_KNOTS('',3,(#83247,#83248,#83249,#83250,#83251,
#83252,#83253,#83254,#83255,#83256,#83257,#83258,#83259,#83260,#83261,#83262,
#83263,#83264,#83265,#83266,#83267,#83268,#83269,#83270,#83271,#83272,#83273,
#83274,#83275,#83276,#83277,#83278,#83279,#83280,#83281,#83282,#83283,#83284,
#83285,#83286,#83287,#83288,#83289,#83290,#83291,#83292,#83293,#83294,#83295,
#83296,#83297,#83298,#83299,#83300,#83301,#83302,#83303,#83304,#83305,#83306,
#83307,#83308,#83309,#83310),.UNSPECIFIED.,.F.,.F.,(4,3,3,3,3,3,3,3,3,3,
3,3,3,3,3,3,3,3,3,3,3,4),(0.479292617177209,0.505001112402896,0.530713686248326,
0.547756394224347,0.573367668816933,0.598976376178496,0.624587462770878,
0.650198276493159,0.675814043328,0.684683947910694,0.710199508692036,0.735710152743036,
0.761220597085833,0.786729520960406,0.812242321661702,0.82161150159704,
0.847361274447889,0.873107871298353,0.898854607494945,0.924599374399674,
0.950345570599475,0.958539055283387),.UNSPECIFIED.);
#3577=B_SPLINE_CURVE_WITH_KNOTS('',3,(#83312,#83313,#83314,#83315,#83316,
#83317,#83318,#83319,#83320,#83321,#83322,#83323,#83324,#83325,#83326,#83327,
#83328,#83329,#83330,#83331,#83332,#83333,#83334,#83335,#83336,#83337,#83338,
#83339,#83340,#83341,#83342,#83343,#83344,#83345,#83346,#83347,#83348,#83349,
#83350,#83351,#83352,#83353,#83354,#83355,#83356,#83357,#83358,#83359,#83360,
#83361,#83362,#83363,#83364,#83365,#83366,#83367,#83368,#83369,#83370,#83371,
#83372,#83373,#83374,#83375,#83376,#83377,#83378,#83379,#83380,#83381,#83382,
#83383,#83384,#83385,#83386,#83387,#83388,#83389,#83390,#83391,#83392,#83393,
#83394,#83395,#83396,#83397,#83398,#83399,#83400,#83401,#83402,#83403,#83404,
#83405,#83406,#83407,#83408,#83409,#83410,#83411,#83412,#83413,#83414,#83415,
#83416,#83417,#83418,#83419,#83420,#83421,#83422,#83423,#83424,#83425,#83426,
#83427,#83428,#83429,#83430,#83431,#83432,#83433,#83434,#83435,#83436,#83437,
#83438),.UNSPECIFIED.,.F.,.F.,(4,3,3,3,3,3,3,3,3,3,3,3,3,3,3,3,3,3,3,3,
3,3,3,3,3,3,3,3,3,3,3,3,3,3,3,3,3,3,3,3,3,3,4),(0.,0.02556233511759,0.0511220164970866,
0.0766843857678656,0.102246781025239,0.127814923376965,0.13693415075477,
0.162563984146602,0.188189495193546,0.213814670831708,0.239437964536715,
0.265063779997811,0.273868301509539,0.299425587203,0.324979912003907,0.350536538379918,
0.376092986033964,0.401654938265957,0.410802452264309,0.436392827093722,
0.461978389004138,0.487563260120719,0.513146148707476,0.538731712359866,
0.547736603019078,0.573349224994543,0.598959271795233,0.624571685120951,
0.650183817761065,0.675800891428116,0.684670753773848,0.710186931607258,
0.735698203093025,0.761209295327788,0.786718880128828,0.812232365003339,
0.821604904528618,0.847356626751991,0.873105174015333,0.898853855418756,
0.924600562266398,0.950348685556951,0.958539055283387),.UNSPECIFIED.);
#3578=B_SPLINE_CURVE_WITH_KNOTS('',3,(#83439,#83440,#83441,#83442,#83443,
#83444,#83445,#83446,#83447,#83448,#83449,#83450,#83451,#83452,#83453,#83454,
#83455,#83456,#83457,#83458,#83459,#83460,#83461,#83462,#83463,#83464,#83465,
#83466,#83467,#83468,#83469,#83470,#83471,#83472,#83473,#83474,#83475,#83476,
#83477,#83478,#83479,#83480,#83481,#83482,#83483,#83484,#83485,#83486,#83487,
#83488,#83489,#83490,#83491,#83492,#83493,#83494,#83495,#83496,#83497,#83498,
#83499,#83500,#83501,#83502),.UNSPECIFIED.,.F.,.F.,(4,3,3,3,3,3,3,3,3,3,
3,3,3,3,3,3,3,3,3,3,3,4),(0.,0.0255635666326801,0.0511244793994705,0.076688080187019,
0.102251706962356,0.127821081108941,0.136940747823198,0.162571815981994,
0.188198561587646,0.213824971768371,0.239449499925226,0.265076549959684,
0.273881495646396,0.299440012611685,0.324995568541792,0.350553426157864,
0.376111105043384,0.401674288772044,0.410822243469594,0.43680646043743,
0.462785075549229,0.479292617177209),.UNSPECIFIED.);
#3579=B_SPLINE_CURVE_WITH_KNOTS('',3,(#83504,#83505,#83506,#83507,#83508,
#83509,#83510,#83511,#83512,#83513,#83514,#83515,#83516,#83517,#83518,#83519,
#83520,#83521,#83522,#83523,#83524,#83525,#83526,#83527,#83528,#83529,#83530,
#83531,#83532,#83533,#83534,#83535,#83536,#83537,#83538,#83539,#83540,#83541,
#83542,#83543,#83544,#83545,#83546,#83547,#83548,#83549,#83550,#83551,#83552,
#83553,#83554,#83555,#83556,#83557,#83558,#83559,#83560,#83561,#83562,#83563,
#83564,#83565,#83566,#83567),.UNSPECIFIED.,.F.,.F.,(4,3,3,3,3,3,3,3,3,3,
3,3,3,3,3,3,3,3,3,3,3,4),(0.479292617179906,0.505267046530367,0.531249287460817,
0.547756394224346,0.573317095800904,0.598872806297043,0.62442781629965,
0.649980909248029,0.675536979617555,0.684683947910693,0.71030857285459,
0.735930637841139,0.761554969027824,0.787178926838093,0.812807591189663,
0.82161150159704,0.847178127100071,0.872739574414869,0.89829997927434,0.923858250403141,
0.949419131562034,0.958539055283387),.UNSPECIFIED.);
#3580=B_SPLINE_CURVE_WITH_KNOTS('',3,(#83569,#83570,#83571,#83572,#83573,
#83574,#83575,#83576,#83577,#83578,#83579,#83580,#83581,#83582,#83583,#83584,
#83585,#83586,#83587,#83588,#83589,#83590,#83591,#83592,#83593,#83594,#83595,
#83596,#83597,#83598,#83599,#83600,#83601,#83602,#83603,#83604,#83605,#83606,
#83607,#83608,#83609,#83610,#83611,#83612,#83613,#83614,#83615,#83616,#83617,
#83618,#83619,#83620,#83621,#83622,#83623,#83624,#83625,#83626,#83627,#83628,
#83629,#83630,#83631,#83632,#83633,#83634,#83635,#83636,#83637,#83638,#83639,
#83640,#83641,#83642,#83643,#83644,#83645,#83646,#83647,#83648,#83649,#83650,
#83651,#83652,#83653,#83654,#83655,#83656,#83657,#83658,#83659,#83660,#83661,
#83662,#83663,#83664,#83665,#83666,#83667,#83668,#83669,#83670,#83671,#83672,
#83673,#83674,#83675,#83676,#83677,#83678,#83679,#83680,#83681,#83682,#83683,
#83684,#83685,#83686,#83687,#83688,#83689,#83690,#83691,#83692,#83693,#83694,
#83695),.UNSPECIFIED.,.F.,.F.,(4,3,3,3,3,3,3,3,3,3,3,3,3,3,3,3,3,3,3,3,
3,3,3,3,3,3,3,3,3,3,3,3,3,3,3,3,3,3,3,3,3,3,4),(0.,0.0257481533409456,0.0514946980789381,
0.0772436849279218,0.102992038986384,0.128743741659937,0.136934150754769,
0.162447594607815,0.187957321333388,0.213468628709931,0.238979446831854,
0.264495648410872,0.273868301509539,0.299485364667177,0.325097913405818,
0.350709964231731,0.376320073731763,0.401932716793888,0.410802452264308,
0.436387986336631,0.461970819036555,0.487556081452547,0.513141169428889,
0.538731557184643,0.547736603019078,0.573298539642115,0.598855488832839,
0.624411743116122,0.649966083470479,0.675523405962016,0.684670753773847,
0.710296552579017,0.735919791615974,0.761545298101024,0.787170432048045,
0.812800274548105,0.821604904528617,0.84717303404939,0.872735984507688,
0.898297889248134,0.92385765765822,0.949420030719154,0.958539055283386),
 .UNSPECIFIED.);
#3581=B_SPLINE_CURVE_WITH_KNOTS('',3,(#83696,#83697,#83698,#83699,#83700,
#83701,#83702,#83703,#83704,#83705,#83706,#83707,#83708,#83709,#83710,#83711,
#83712,#83713,#83714,#83715,#83716,#83717,#83718,#83719,#83720,#83721,#83722,
#83723,#83724,#83725,#83726,#83727,#83728,#83729,#83730,#83731,#83732,#83733,
#83734,#83735,#83736,#83737,#83738,#83739,#83740,#83741,#83742,#83743,#83744,
#83745,#83746,#83747,#83748,#83749,#83750,#83751,#83752,#83753,#83754,#83755,
#83756,#83757,#83758,#83759),.UNSPECIFIED.,.F.,.F.,(4,3,3,3,3,3,3,3,3,3,
3,3,3,3,3,3,3,3,3,3,3,4),(0.,0.0257491523438341,0.0514966921238077,0.0772466708701257,
0.102996015643584,0.128748709483213,0.136940747823198,0.162455615107776,
0.187966771796078,0.21347951743795,0.238991778112778,0.264509427354194,
0.273881495646396,0.299499762668791,0.325113511405751,0.350726757305157,
0.376338059087739,0.401951891032166,0.410822243469593,0.436536934850327,
0.462249829569396,0.47929261717721),.UNSPECIFIED.);
#3582=B_SPLINE_CURVE_WITH_KNOTS('',3,(#83765,#83766,#83767,#83768,#83769,
#83770,#83771,#83772,#83773,#83774,#83775,#83776,#83777,#83778,#83779,#83780,
#83781,#83782,#83783,#83784,#83785,#83786,#83787,#83788,#83789,#83790,#83791,
#83792,#83793,#83794,#83795,#83796,#83797,#83798,#83799,#83800,#83801,#83802,
#83803,#83804,#83805,#83806,#83807,#83808,#83809,#83810,#83811,#83812,#83813,
#83814,#83815,#83816,#83817,#83818,#83819,#83820,#83821,#83822,#83823,#83824,
#83825,#83826,#83827,#83828),.UNSPECIFIED.,.F.,.F.,(4,3,3,3,3,3,3,3,3,3,
3,3,3,3,3,3,3,3,3,3,3,4),(0.479292617177209,0.505000671870075,0.530712796156197,
0.547756394224347,0.573367607382753,0.598976259761798,0.624587301684935,
0.650198076948859,0.67581381494733,0.684683947910694,0.710200019009184,
0.735711164707781,0.761222093924401,0.786731491916345,0.812244747773555,
0.82161150159704,0.847360662097727,0.873106644909574,0.898852770635322,
0.924596931000677,0.950342531080525,0.958539055283387),.UNSPECIFIED.);
#3583=B_SPLINE_CURVE_WITH_KNOTS('',3,(#83830,#83831,#83832,#83833,#83834,
#83835,#83836,#83837,#83838,#83839,#83840,#83841,#83842,#83843,#83844,#83845,
#83846,#83847,#83848,#83849,#83850,#83851,#83852,#83853,#83854,#83855,#83856,
#83857,#83858,#83859,#83860,#83861,#83862,#83863,#83864,#83865,#83866,#83867,
#83868,#83869,#83870,#83871,#83872,#83873,#83874,#83875,#83876,#83877,#83878,
#83879,#83880,#83881,#83882,#83883,#83884,#83885,#83886,#83887,#83888,#83889,
#83890,#83891,#83892,#83893,#83894,#83895,#83896,#83897,#83898,#83899,#83900,
#83901,#83902,#83903,#83904,#83905,#83906,#83907,#83908,#83909,#83910,#83911,
#83912,#83913,#83914,#83915,#83916,#83917,#83918,#83919,#83920,#83921,#83922,
#83923,#83924,#83925,#83926,#83927,#83928,#83929,#83930,#83931,#83932,#83933,
#83934,#83935,#83936,#83937,#83938,#83939,#83940,#83941,#83942,#83943,#83944,
#83945,#83946,#83947,#83948,#83949,#83950,#83951,#83952,#83953,#83954,#83955,
#83956),.UNSPECIFIED.,.F.,.F.,(4,3,3,3,3,3,3,3,3,3,3,3,3,3,3,3,3,3,3,3,
3,3,3,3,3,3,3,3,3,3,3,3,3,3,3,3,3,3,3,3,3,3,4),(0.,0.0255614058406569,0.0511201411777619,
0.0766815478440569,0.102242973130247,0.127810141641151,0.13693415075477,
0.162564161855662,0.18818985595306,0.213815220313041,0.239438705376993,
0.265064714254088,0.273868301509539,0.299425520738351,0.324979792724313,
0.350536386846161,0.376092814257761,0.401654764016234,0.410802452264309,
0.436393134716681,0.461978999751451,0.487564165024772,0.513147341926946,
0.53873318350802,0.547736603019078,0.573349111543881,0.598959052713892,
0.624571373229419,0.650183420861739,0.675800421845165,0.684670753773848,
0.710187543876092,0.735699417010997,0.761211090428249,0.78672124330388,
0.81223527319308,0.821604904528618,0.847355917984526,0.873103755286946,
0.898851731942261,0.924597739210931,0.950345175843443,0.958539055283387),
 .UNSPECIFIED.);
#3584=B_SPLINE_CURVE_WITH_KNOTS('',3,(#83957,#83958,#83959,#83960,#83961,
#83962,#83963,#83964,#83965,#83966,#83967,#83968,#83969,#83970,#83971,#83972,
#83973,#83974,#83975,#83976,#83977,#83978,#83979,#83980,#83981,#83982,#83983,
#83984,#83985,#83986,#83987,#83988,#83989,#83990,#83991,#83992,#83993,#83994,
#83995,#83996,#83997,#83998,#83999,#84000,#84001,#84002,#84003,#84004,#84005,
#84006,#84007,#84008,#84009,#84010,#84011,#84012,#84013,#84014,#84015,#84016,
#84017,#84018,#84019,#84020),.UNSPECIFIED.,.F.,.F.,(4,3,3,3,3,3,3,3,3,3,
3,3,3,3,3,3,3,3,3,3,3,4),(0.,0.0255626373109835,0.0511226039897656,0.0766852421264175,
0.102247898883866,0.127816299142739,0.136940747823198,0.162571993699622,
0.188198922364561,0.213825521276229,0.239450240801314,0.265077484261085,
0.273881495646396,0.299439946143816,0.324995449256306,0.350553274616682,
0.376110933258725,0.401674114513703,0.410822243469594,0.436807692773927,
0.462787529398712,0.479292617174633),.UNSPECIFIED.);
#3585=B_SPLINE_CURVE_WITH_KNOTS('',3,(#84022,#84023,#84024,#84025,#84026,
#84027,#84028,#84029,#84030,#84031,#84032,#84033,#84034,#84035,#84036,#84037,
#84038,#84039,#84040,#84041,#84042,#84043,#84044,#84045,#84046,#84047,#84048,
#84049,#84050,#84051,#84052,#84053,#84054,#84055,#84056,#84057,#84058,#84059,
#84060,#84061,#84062,#84063,#84064,#84065,#84066,#84067,#84068,#84069,#84070,
#84071,#84072,#84073,#84074,#84075,#84076,#84077,#84078,#84079,#84080,#84081,
#84082,#84083,#84084,#84085),.UNSPECIFIED.,.F.,.F.,(4,3,3,3,3,3,3,3,3,3,
3,3,3,3,3,3,3,3,3,3,3,4),(0.47929261717721,0.505267152182088,0.531249499696255,
0.547756394224346,0.573317095142505,0.598872803757218,0.624427810106277,
0.649980898385333,0.675536962638426,0.684683947910693,0.710308590703365,
0.735930673424052,0.761555021973375,0.787178996872414,0.812807677753939,
0.82161150159704,0.84717804259122,0.872739405615204,0.898299727215526,0.923857915879837,
0.949418716310487,0.958539055283387),.UNSPECIFIED.);
#3586=B_SPLINE_CURVE_WITH_KNOTS('',3,(#84087,#84088,#84089,#84090,#84091,
#84092,#84093,#84094,#84095,#84096,#84097,#84098,#84099,#84100,#84101,#84102,
#84103,#84104,#84105,#84106,#84107,#84108,#84109,#84110,#84111,#84112,#84113,
#84114,#84115,#84116,#84117,#84118,#84119,#84120,#84121,#84122,#84123,#84124,
#84125,#84126,#84127,#84128,#84129,#84130,#84131,#84132,#84133,#84134,#84135,
#84136,#84137,#84138,#84139,#84140,#84141,#84142,#84143,#84144,#84145,#84146,
#84147,#84148,#84149,#84150,#84151,#84152,#84153,#84154,#84155,#84156,#84157,
#84158,#84159,#84160,#84161,#84162,#84163,#84164,#84165,#84166,#84167,#84168,
#84169,#84170,#84171,#84172,#84173,#84174,#84175,#84176,#84177,#84178,#84179,
#84180,#84181,#84182,#84183,#84184,#84185,#84186,#84187,#84188,#84189,#84190,
#84191,#84192,#84193,#84194,#84195,#84196,#84197,#84198,#84199,#84200,#84201,
#84202,#84203,#84204,#84205,#84206,#84207,#84208,#84209,#84210,#84211,#84212,
#84213),.UNSPECIFIED.,.F.,.F.,(4,3,3,3,3,3,3,3,3,3,3,3,3,3,3,3,3,3,3,3,
3,3,3,3,3,3,3,3,3,3,3,3,3,3,3,3,3,3,3,3,3,3,4),(0.,0.0257479118882393,0.0514942112903244,
0.0772429495412298,0.102991053849869,0.128742507063266,0.136934150754769,
0.162447788870315,0.1879577165684,0.213469233143456,0.238980264774859,0.264496684713239,
0.273868301509539,0.299485334381649,0.325097849185929,0.350709861176942,
0.376319929144802,0.401932527152614,0.410802452264308,0.436388087284282,
0.461971024086556,0.487556394413245,0.513141592275077,0.538732092072625,
0.547736603019078,0.57329853543293,0.59885547530275,0.6244117128732,0.649966032281209,
0.675523327806675,0.684670753773847,0.710296631142861,0.735919948316494,
0.761545531427997,0.787170740871235,0.812800656523678,0.821604904528617,
0.847172677299873,0.872735271851408,0.898296824929134,0.923856244968091,
0.94941827689922,0.958539055283386),.UNSPECIFIED.);
#3587=B_SPLINE_CURVE_WITH_KNOTS('',3,(#84214,#84215,#84216,#84217,#84218,
#84219,#84220,#84221,#84222,#84223,#84224,#84225,#84226,#84227,#84228,#84229,
#84230,#84231,#84232,#84233,#84234,#84235,#84236,#84237,#84238,#84239,#84240,
#84241,#84242,#84243,#84244,#84245,#84246,#84247,#84248,#84249,#84250,#84251,
#84252,#84253,#84254,#84255,#84256,#84257,#84258,#84259,#84260,#84261,#84262,
#84263,#84264,#84265,#84266,#84267,#84268,#84269,#84270,#84271,#84272,#84273,
#84274,#84275,#84276,#84277),.UNSPECIFIED.,.F.,.F.,(4,3,3,3,3,3,3,3,3,3,
3,3,3,3,3,3,3,3,3,3,3,4),(0.,0.0257484974013576,0.05149537221129,0.077244677886759,
0.102993346900836,0.128745366395548,0.136940747823198,0.162456127284197,
0.187967813632376,0.213481110331621,0.23899393326664,0.264512157330573,
0.273881495646396,0.29949970651347,0.325113389931437,0.350726558060159,
0.376337775174149,0.401951513305493,0.410822243469593,0.436536403375429,
0.462248777981185,0.47929261717721),.UNSPECIFIED.);
#3588=B_SPLINE_CURVE_WITH_KNOTS('',3,(#84285,#84286,#84287,#84288,#84289,
#84290),.UNSPECIFIED.,.F.,.F.,(4,2,4),(0.,0.216145052008235,0.432257670232604),
 .UNSPECIFIED.);
#3589=B_SPLINE_CURVE_WITH_KNOTS('',3,(#84292,#84293,#84294,#84295,#84296,
#84297,#84298,#84299,#84300,#84301,#84302,#84303,#84304,#84305,#84306,#84307,
#84308,#84309,#84310,#84311,#84312,#84313,#84314,#84315,#84316,#84317,#84318,
#84319,#84320,#84321,#84322,#84323,#84324,#84325,#84326,#84327,#84328,#84329,
#84330,#84331,#84332,#84333,#84334,#84335,#84336,#84337,#84338,#84339,#84340,
#84341,#84342,#84343,#84344,#84345,#84346,#84347,#84348,#84349,#84350,#84351,
#84352,#84353,#84354,#84355,#84356,#84357,#84358,#84359,#84360,#84361,#84362,
#84363,#84364,#84365,#84366,#84367,#84368,#84369,#84370,#84371,#84372,#84373,
#84374,#84375,#84376,#84377,#84378,#84379,#84380,#84381,#84382,#84383,#84384,
#84385,#84386,#84387,#84388,#84389,#84390,#84391,#84392,#84393,#84394,#84395,
#84396,#84397,#84398,#84399,#84400,#84401,#84402,#84403,#84404,#84405,#84406,
#84407,#84408,#84409,#84410,#84411,#84412,#84413,#84414,#84415,#84416,#84417,
#84418),.UNSPECIFIED.,.F.,.F.,(4,3,3,3,3,3,3,3,3,3,3,3,3,3,3,3,3,3,3,3,
3,3,3,3,3,3,3,3,3,3,3,3,3,3,3,3,3,3,3,3,3,3,4),(0.,0.0255606924572304,0.0511187002880486,
0.0766793648644971,0.102240041316473,0.127806456428402,0.13693415075477,
0.162564246062696,0.18819002867775,0.213815486626741,0.239439067836035,
0.265065175540469,0.273868301509539,0.299425486139408,0.324979735220857,
0.350536323838371,0.376092755852858,0.401654724993392,0.410802452264309,
0.436393374733914,0.461979476717824,0.487564872613919,0.513148275975265,
0.538734336496269,0.547736603019078,0.573349050106841,0.59895893629183,
0.624571212136073,0.650183221308245,0.675800193454039,0.684670753773848,
0.710188054217764,0.735700429024432,0.761212587338756,0.786723214354636,
0.812237699421663,0.821604904528618,0.847355305604822,0.873102528839054,
0.898849894994097,0.924595295694261,0.950342136178106,0.958539055283387),
 .UNSPECIFIED.);
#3590=B_SPLINE_CURVE_WITH_KNOTS('',3,(#84419,#84420,#84421,#84422,#84423,
#84424,#84425,#84426,#84427,#84428,#84429,#84430,#84431,#84432,#84433,#84434,
#84435,#84436,#84437,#84438,#84439,#84440,#84441,#84442,#84443,#84444,#84445,
#84446,#84447,#84448,#84449,#84450,#84451,#84452,#84453,#84454,#84455,#84456,
#84457,#84458,#84459,#84460,#84461,#84462,#84463,#84464,#84465,#84466,#84467,
#84468,#84469,#84470,#84471,#84472,#84473,#84474,#84475,#84476,#84477,#84478,
#84479,#84480,#84481,#84482),.UNSPECIFIED.,.F.,.F.,(4,3,3,3,3,3,3,3,3,3,
3,3,3,3,3,3,3,3,3,3,3,4),(0.,0.0255619238931804,0.0511211630306363,0.0766830590417173,
0.102244966928892,0.127812613752488,0.136940747823198,0.162572077910745,
0.188199095097715,0.213825787602894,0.239450603277954,0.265077945569875,
0.273881495646396,0.299439911543206,0.324995391750202,0.350553211605967,
0.376110874851102,0.401674075489097,0.410822243469594,0.436808654596317,
0.46278944530477,0.479292617174629),.UNSPECIFIED.);
#3591=B_SPLINE_CURVE_WITH_KNOTS('',3,(#84484,#84485,#84486,#84487,#84488,
#84489,#84490,#84491,#84492,#84493,#84494,#84495,#84496,#84497,#84498,#84499,
#84500,#84501,#84502,#84503,#84504,#84505,#84506,#84507,#84508,#84509,#84510,
#84511,#84512,#84513,#84514,#84515,#84516,#84517,#84518,#84519,#84520,#84521,
#84522,#84523,#84524,#84525,#84526,#84527,#84528,#84529,#84530,#84531,#84532,
#84533,#84534,#84535,#84536,#84537,#84538,#84539,#84540,#84541,#84542,#84543,
#84544,#84545,#84546,#84547),.UNSPECIFIED.,.F.,.F.,(4,3,3,3,3,3,3,3,3,3,
3,3,3,3,3,3,3,3,3,3,3,4),(0.47929261717721,0.505268272173354,0.531251749094228,
0.547756394224346,0.57331710180848,0.598872803689831,0.62442778376179,0.649980834522848,
0.675536845133206,0.684683947910693,0.710308747141793,0.735930984531055,
0.761555483271823,0.787179605223059,0.812808427118386,0.82161150159704,
0.84717715204078,0.872737627590923,0.898297073699267,0.923854395875952,
0.949414349001511,0.958539055283387),.UNSPECIFIED.);
#3592=B_SPLINE_CURVE_WITH_KNOTS('',3,(#84549,#84550,#84551,#84552,#84553,
#84554,#84555,#84556,#84557,#84558,#84559,#84560,#84561,#84562,#84563,#84564,
#84565,#84566,#84567,#84568,#84569,#84570,#84571,#84572,#84573,#84574,#84575,
#84576,#84577,#84578,#84579,#84580,#84581,#84582,#84583,#84584,#84585,#84586,
#84587,#84588,#84589,#84590,#84591,#84592,#84593,#84594,#84595,#84596,#84597,
#84598,#84599,#84600,#84601,#84602,#84603,#84604,#84605,#84606,#84607,#84608,
#84609,#84610,#84611,#84612,#84613,#84614,#84615,#84616,#84617,#84618,#84619,
#84620,#84621,#84622,#84623,#84624,#84625,#84626,#84627,#84628,#84629,#84630,
#84631,#84632,#84633,#84634,#84635,#84636,#84637,#84638,#84639,#84640,#84641,
#84642,#84643,#84644,#84645,#84646,#84647,#84648,#84649,#84650,#84651,#84652,
#84653,#84654,#84655,#84656,#84657,#84658,#84659,#84660,#84661,#84662,#84663,
#84664,#84665,#84666,#84667,#84668,#84669,#84670,#84671,#84672,#84673,#84674,
#84675),.UNSPECIFIED.,.F.,.F.,(4,3,3,3,3,3,3,3,3,3,3,3,3,3,3,3,3,3,3,3,
3,3,3,3,3,3,3,3,3,3,3,3,3,3,3,3,3,3,3,3,3,3,4),(0.,0.0257472569772838,0.0514928914413629,
0.0772409566538184,0.102988385235593,0.12873916413656,0.136934150754769,
0.162448301022051,0.187958758354364,0.213470825960218,0.23898241982469,
0.264499414557891,0.273868301509539,0.299485278229076,0.325097727717576,
0.350709661941676,0.376319645244957,0.401932149444248,0.410802452264308,
0.436388343469677,0.461971544040781,0.487557187203235,0.513142662573877,
0.538733444881708,0.547736603019078,0.573298542099209,0.598855475235286,
0.624411686527281,0.649965968415386,0.675523210295452,0.684670753773847,
0.710296787588882,0.735920259438635,0.76154599274883,0.78717134925136,0.812801405924429,
0.821604904528617,0.847171786706504,0.872733493741441,0.898294171285005,
0.923852724794528,0.949413909379723,0.958539055283386),.UNSPECIFIED.);
#3593=B_SPLINE_CURVE_WITH_KNOTS('',3,(#84676,#84677,#84678,#84679,#84680,
#84681,#84682,#84683,#84684,#84685,#84686,#84687,#84688,#84689,#84690,#84691,
#84692,#84693,#84694,#84695,#84696,#84697,#84698,#84699,#84700,#84701,#84702,
#84703,#84704,#84705,#84706,#84707,#84708,#84709,#84710,#84711,#84712,#84713,
#84714,#84715,#84716,#84717,#84718,#84719,#84720,#84721,#84722,#84723,#84724,
#84725,#84726,#84727,#84728,#84729,#84730,#84731,#84732,#84733,#84734,#84735,
#84736,#84737,#84738,#84739),.UNSPECIFIED.,.F.,.F.,(4,3,3,3,3,3,3,3,3,3,
3,3,3,3,3,3,3,3,3,3,3,4),(0.,0.0257479279250796,0.0514942251218129,0.0772429470007209,
0.102991030381649,0.128742466196639,0.136940747823198,0.162456557033928,
0.187968687603579,0.213482446206961,0.238995740295273,0.264514445849957,
0.273881495646396,0.299499689255512,0.325113348199751,0.350726481849042,
0.376337658878936,0.401951349310238,0.410822243469593,0.436535985935545,
0.462247951405,0.47929261717721),.UNSPECIFIED.);
#3594=B_SPLINE_CURVE_WITH_KNOTS('',3,(#84742,#84743,#84744,#84745,#84746,
#84747,#84748,#84749,#84750,#84751,#84752,#84753,#84754,#84755,#84756,#84757,
#84758,#84759,#84760,#84761,#84762,#84763,#84764,#84765,#84766,#84767,#84768,
#84769,#84770,#84771,#84772,#84773,#84774,#84775,#84776,#84777,#84778,#84779,
#84780,#84781),.UNSPECIFIED.,.F.,.F.,(4,3,3,3,3,3,3,3,3,3,3,3,3,4),(0.479292617179918,
0.505270201534281,0.531255614881935,0.547759154438251,0.573320916637539,
0.598877661713949,0.624433668411704,0.649987736156769,0.675544750003459,
0.684692228552392,0.710230981397045,0.735766124290673,0.761303447116751,
0.780281286407365),.UNSPECIFIED.);
#3595=B_SPLINE_CURVE_WITH_KNOTS('',3,(#84786,#84787,#84788,#84789,#84790,
#84791,#84792,#84793,#84794,#84795,#84796,#84797,#84798,#84799,#84800,#84801,
#84802,#84803,#84804,#84805,#84806,#84807,#84808,#84809,#84810,#84811,#84812,
#84813,#84814,#84815,#84816,#84817,#84818,#84819,#84820,#84821,#84822),
 .UNSPECIFIED.,.F.,.F.,(4,3,3,3,3,3,3,3,3,3,3,3,4),(-0.587674682252879,
-0.522275543829995,-0.458090181278496,-0.394772087238499,-0.332851241040222,
-0.290582655255106,-0.278920555202013,-0.270271621870392,-0.211810705909702,
-0.154597029996384,-0.0981542104956995,-0.0429508698655889,0.),
 .UNSPECIFIED.);
#3596=B_SPLINE_CURVE_WITH_KNOTS('',3,(#84824,#84825,#84826,#84827,#84828,
#84829,#84830,#84831,#84832,#84833,#84834,#84835,#84836,#84837,#84838,#84839,
#84840,#84841,#84842,#84843,#84844,#84845,#84846,#84847,#84848,#84849,#84850,
#84851,#84852,#84853,#84854,#84855,#84856,#84857,#84858,#84859,#84860,#84861,
#84862,#84863,#84864,#84865,#84866,#84867,#84868,#84869,#84870,#84871,#84872,
#84873,#84874,#84875,#84876,#84877,#84878,#84879,#84880,#84881,#84882,#84883,
#84884,#84885,#84886,#84887,#84888,#84889,#84890,#84891,#84892,#84893,#84894,
#84895,#84896,#84897,#84898,#84899,#84900,#84901,#84902,#84903,#84904,#84905,
#84906,#84907,#84908,#84909,#84910,#84911,#84912,#84913,#84914,#84915,#84916,
#84917,#84918,#84919,#84920,#84921,#84922,#84923,#84924,#84925,#84926,#84927,
#84928,#84929,#84930,#84931,#84932,#84933,#84934,#84935,#84936,#84937,#84938,
#84939,#84940,#84941),.UNSPECIFIED.,.F.,.F.,(4,3,3,3,3,3,3,3,3,3,3,3,3,
3,3,3,3,3,3,3,3,3,3,3,3,3,3,3,3,3,3,3,3,3,3,3,3,3,3,4),(-2.21853380163141,
-2.14169700900979,-2.06000622499644,-1.98211684071596,-1.94032109877607,
-1.92940218041483,-1.89664180199272,-1.81493387295641,-1.73704918283534,
-1.65550918141576,-1.64157430304436,-1.63094960942268,-1.55302694654912,
-1.47530023545016,-1.410889177157,-1.33294761057228,-1.25462606115837,-1.23895063150748,
-1.22943147765607,-1.21204834416161,-1.13439080518558,-1.05606095724006,
-0.977636631083868,-0.899720638530548,-0.825388030509179,-0.812979956321517,
-0.734650421044989,-0.656887708961902,-0.602390206445073,-0.524409242543717,
-0.460391483368985,-0.43238371373004,-0.413066499848313,-0.402820754727463,
-0.325843178167182,-0.247449175911852,-0.169023585066473,-0.0906453771061667,
-0.01226716914586,-3.85504356227988E-5),.UNSPECIFIED.);
#3597=B_SPLINE_CURVE_WITH_KNOTS('',3,(#84944,#84945,#84946,#84947,#84948,
#84949,#84950,#84951,#84952,#84953,#84954,#84955,#84956,#84957,#84958,#84959,
#84960,#84961,#84962,#84963,#84964,#84965,#84966,#84967,#84968,#84969,#84970,
#84971,#84972,#84973,#84974,#84975,#84976,#84977,#84978,#84979,#84980,#84981,
#84982,#84983,#84984,#84985,#84986,#84987,#84988,#84989),.UNSPECIFIED.,
 .F.,.F.,(4,3,3,3,3,3,3,3,3,3,3,3,3,3,3,4),(-0.593406414910134,-0.551632623974457,
-0.508637403999538,-0.476718450480326,-0.455431999029698,-0.441536524705485,
-0.395342652559364,-0.347935919259055,-0.308483973940118,-0.294081551185092,
-0.243706144295089,-0.192379500820218,-0.139588002045789,-0.0860358862173692,
-0.0315002188398129,0.),.UNSPECIFIED.);
#3598=B_SPLINE_CURVE_WITH_KNOTS('',3,(#84990,#84991,#84992,#84993,#84994,
#84995,#84996,#84997,#84998,#84999,#85000,#85001,#85002,#85003,#85004,#85005,
#85006,#85007,#85008,#85009,#85010,#85011,#85012,#85013,#85014,#85015,#85016,
#85017,#85018,#85019,#85020,#85021,#85022,#85023,#85024,#85025,#85026),
 .UNSPECIFIED.,.F.,.F.,(4,3,3,3,3,3,3,3,3,3,3,3,4),(-0.47345883347035,-0.421785176279112,
-0.371368479159938,-0.321739753842847,-0.273397162061595,-0.229764201701003,
-0.222185125570855,-0.176965222652948,-0.132800326254763,-0.0998029709030014,
-0.057155654322561,-0.0156176608406257,-1.17079676490498E-5),
 .UNSPECIFIED.);
#3599=B_SPLINE_CURVE_WITH_KNOTS('',3,(#85087,#85088,#85089,#85090,#85091,
#85092,#85093,#85094),.UNSPECIFIED.,.F.,.F.,(4,1,1,1,1,4),(0.144829272278474,
0.266996519095835,0.389163765913196,0.633498259547918,0.877832753182639,
1.),.UNSPECIFIED.);
#3600=B_SPLINE_CURVE_WITH_KNOTS('',3,(#85129,#85130,#85131,#85132,#85133,
#85134,#85135,#85136,#85137,#85138,#85139,#85140,#85141,#85142,#85143,#85144,
#85145,#85146,#85147),.UNSPECIFIED.,.F.,.F.,(4,3,3,3,3,3,4),(0.815535452893383,
0.847523529162131,0.877832753182639,0.913211852549041,0.948843428238211,
0.98416694468468,1.),.UNSPECIFIED.);
#3601=B_SPLINE_CURVE_WITH_KNOTS('',3,(#85151,#85152,#85153,#85154,#85155,
#85156,#85157,#85158,#85159,#85160,#85161,#85162,#85163,#85164,#85165,#85166,
#85167,#85168,#85169,#85170,#85171,#85172,#85173,#85174,#85175,#85176,#85177,
#85178,#85179,#85180,#85181,#85182,#85183,#85184,#85185,#85186,#85187),
 .UNSPECIFIED.,.F.,.F.,(4,3,3,3,3,3,3,3,3,3,3,3,4),(-0.473459590222709,
-0.421790762051377,-0.37138598180264,-0.321768833120639,-0.273433624494914,
-0.229795000551108,-0.221386012412719,-0.176179340889983,-0.132023266728005,
-0.099803605201648,-0.0571527054274905,-0.0156155844320621,-1.1601141627616E-5),
 .UNSPECIFIED.);
#3602=B_SPLINE_CURVE_WITH_KNOTS('',3,(#85189,#85190,#85191,#85192,#85193,
#85194,#85195,#85196,#85197,#85198,#85199,#85200,#85201,#85202,#85203,#85204,
#85205,#85206,#85207,#85208,#85209,#85210,#85211,#85212,#85213,#85214,#85215,
#85216,#85217,#85218,#85219,#85220,#85221,#85222),.UNSPECIFIED.,.F.,.F.,
(4,3,3,3,3,3,3,3,3,3,3,4),(-0.587778750364654,-0.522392013442643,-0.458246883948291,
-0.39497298076002,-0.333146586530125,-0.280267059023603,-0.270271030376407,
-0.21181010441986,-0.154596418410281,-0.0981535891351624,-0.0429502360987486,
0.),.UNSPECIFIED.);
#3603=B_SPLINE_CURVE_WITH_KNOTS('',3,(#85224,#85225,#85226,#85227,#85228,
#85229,#85230,#85231,#85232,#85233,#85234,#85235,#85236,#85237,#85238,#85239,
#85240,#85241,#85242,#85243,#85244,#85245,#85246,#85247,#85248,#85249,#85250,
#85251,#85252,#85253,#85254,#85255,#85256,#85257,#85258,#85259,#85260,#85261,
#85262,#85263,#85264,#85265,#85266,#85267,#85268,#85269,#85270,#85271,#85272,
#85273,#85274,#85275,#85276,#85277,#85278,#85279,#85280,#85281,#85282,#85283,
#85284,#85285,#85286,#85287,#85288,#85289,#85290,#85291,#85292,#85293,#85294,
#85295,#85296,#85297,#85298,#85299,#85300,#85301,#85302,#85303,#85304,#85305,
#85306,#85307,#85308,#85309,#85310,#85311,#85312,#85313,#85314,#85315,#85316,
#85317,#85318,#85319,#85320,#85321,#85322,#85323,#85324,#85325,#85326,#85327,
#85328,#85329,#85330,#85331,#85332,#85333,#85334,#85335,#85336,#85337,#85338,
#85339,#85340,#85341),.UNSPECIFIED.,.F.,.F.,(4,3,3,3,3,3,3,3,3,3,3,3,3,
3,3,3,3,3,3,3,3,3,3,3,3,3,3,3,3,3,3,3,3,3,3,3,3,3,3,4),(-2.21853380163141,
-2.14147687580222,-2.05984115648833,-1.98219940142569,-1.94038305070594,
-1.92982950632801,-1.90569661828717,-1.82789475155552,-1.81493399854668,
-1.73723203187215,-1.65564638113919,-1.64262516049492,-1.63166177462369,
-1.55405438820831,-1.47598659309221,-1.4108894289403,-1.33296387367606,
-1.25559958045839,-1.2374200788259,-1.22345195044101,-1.14563978964884,
-1.06790309904323,-1.00663999520165,-0.928722650056018,-0.850384574996885,
-0.829262259425257,-0.819802210939349,-0.798261686933839,-0.720531563347699,
-0.642165018867216,-0.563716269145714,-0.485760922111857,-0.413856073237234,
-0.404560305583847,-0.326120745631757,-0.248239195955339,-0.198141526613365,
-0.120433480757384,-0.0425282133148996,0.),.UNSPECIFIED.);
#3604=B_SPLINE_CURVE_WITH_KNOTS('',3,(#85344,#85345,#85346,#85347,#85348,
#85349,#85350,#85351,#85352,#85353,#85354,#85355,#85356,#85357,#85358,#85359,
#85360,#85361,#85362,#85363,#85364,#85365,#85366,#85367,#85368,#85369,#85370,
#85371,#85372,#85373,#85374,#85375,#85376,#85377,#85378,#85379,#85380,#85381,
#85382,#85383,#85384,#85385,#85386,#85387,#85388,#85389,#85390,#85391,#85392),
 .UNSPECIFIED.,.F.,.F.,(4,3,3,3,3,3,3,3,3,3,3,3,3,3,3,3,4),(-0.593405610245497,
-0.551428083606103,-0.508498879669832,-0.476717699690467,-0.458169903899235,
-0.442929634384365,-0.396892175868468,-0.34991960007854,-0.31930222027659,
-0.303005267879666,-0.289328418066246,-0.238863157543073,-0.187445469095536,
-0.134580054596664,-0.0809600612898856,-0.0263940066113425,0.),
 .UNSPECIFIED.);
#3605=B_SPLINE_CURVE_WITH_KNOTS('',3,(#85432,#85433,#85434,#85435,#85436,
#85437,#85438,#85439,#85440,#85441,#85442,#85443,#85444,#85445,#85446,#85447,
#85448,#85449,#85450,#85451,#85452,#85453),.UNSPECIFIED.,.F.,.F.,(4,3,3,
3,3,3,3,4),(0.,0.0333176175948162,0.0669610730078588,0.100473730255888,
0.12216720883009,0.147816659999738,0.173346358925325,0.184428015042582),
 .UNSPECIFIED.);
#3606=B_SPLINE_CURVE_WITH_KNOTS('',3,(#85456,#85457,#85458,#85459,#85460,
#85461,#85462,#85463,#85464),.UNSPECIFIED.,.F.,.F.,(4,1,1,1,1,1,4),(0.,
0.12216720883009,0.24433441766018,0.488668835320359,0.610836044150449,0.733003252980539,
0.855170461810629),.UNSPECIFIED.);
#3607=B_SPLINE_CURVE_WITH_KNOTS('',3,(#85524,#85525,#85526,#85527,#85528,
#85529,#85530,#85531,#85532,#85533),.UNSPECIFIED.,.F.,.F.,(4,1,1,1,1,1,
1,4),(0.,0.142857142857143,0.285714285714286,0.428571428571429,0.571428571428571,
0.714285714285714,0.857142857142857,1.),.UNSPECIFIED.);
#3608=B_SPLINE_CURVE_WITH_KNOTS('',3,(#85602,#85603,#85604,#85605,#85606,
#85607,#85608,#85609,#85610,#85611),.UNSPECIFIED.,.F.,.F.,(4,1,1,1,1,1,
1,4),(0.,0.142857142857143,0.285714285714286,0.428571428571429,0.571428571428571,
0.714285714285714,0.857142857142857,1.),.UNSPECIFIED.);
#3609=B_SPLINE_CURVE_WITH_KNOTS('',3,(#85697,#85698,#85699,#85700,#85701,
#85702,#85703,#85704,#85705,#85706),.UNSPECIFIED.,.F.,.F.,(4,1,1,1,1,1,
1,4),(0.,0.142857142857143,0.285714285714286,0.428571428571429,0.571428571428571,
0.714285714285714,0.857142857142857,1.),.UNSPECIFIED.);
#3610=B_SPLINE_CURVE_WITH_KNOTS('',3,(#85751,#85752,#85753,#85754,#85755,
#85756,#85757,#85758,#85759,#85760),.UNSPECIFIED.,.F.,.F.,(4,1,1,1,1,1,
1,4),(0.,0.142857142857143,0.285714285714286,0.428571428571429,0.571428571428571,
0.714285714285714,0.857142857142857,1.),.UNSPECIFIED.);
#3611=B_SPLINE_CURVE_WITH_KNOTS('',3,(#85847,#85848,#85849,#85850,#85851,
#85852,#85853,#85854,#85855,#85856),.UNSPECIFIED.,.F.,.F.,(4,1,1,1,1,1,
1,4),(0.,0.142857142857143,0.285714285714286,0.428571428571429,0.571428571428571,
0.714285714285714,0.857142857142857,1.),.UNSPECIFIED.);
#3612=B_SPLINE_CURVE_WITH_KNOTS('',3,(#85901,#85902,#85903,#85904,#85905,
#85906,#85907,#85908,#85909,#85910,#85911,#85912,#85913,#85914,#85915,#85916,
#85917,#85918),.UNSPECIFIED.,.F.,.F.,(4,2,2,2,2,2,2,2,4),(0.,0.411606409146398,
0.882606331055097,1.58532698900216,2.58333249194717,3.58155989188507,4.32087044195073,
4.8178921514512,5.24318392699258),.UNSPECIFIED.);
#3613=B_SPLINE_CURVE_WITH_KNOTS('',3,(#86005,#86006,#86007,#86008,#86009,
#86010,#86011,#86012,#86013,#86014,#86015,#86016,#86017,#86018,#86019,#86020,
#86021,#86022,#86023,#86024,#86025,#86026),.UNSPECIFIED.,.F.,.F.,(4,3,3,
3,3,3,3,4),(0.,0.142857142857143,0.285714285714286,0.428571428571429,0.571428571428571,
0.714285714285714,0.857142857142857,1.),.UNSPECIFIED.);
#3614=B_SPLINE_CURVE_WITH_KNOTS('',3,(#86071,#86072,#86073,#86074,#86075,
#86076,#86077,#86078,#86079,#86080),.UNSPECIFIED.,.F.,.F.,(4,1,1,1,1,1,
1,4),(0.,0.142857142857143,0.285714285714286,0.428571428571429,0.571428571428571,
0.714285714285714,0.857142857142857,1.),.UNSPECIFIED.);
#3615=B_SPLINE_CURVE_WITH_KNOTS('',3,(#86167,#86168,#86169,#86170,#86171,
#86172,#86173,#86174,#86175,#86176,#86177,#86178,#86179,#86180,#86181,#86182,
#86183,#86184,#86185,#86186,#86187,#86188),.UNSPECIFIED.,.F.,.F.,(4,3,3,
3,3,3,3,4),(0.,0.142857142857143,0.285714285714286,0.428571428571429,0.571428571428571,
0.714285714285714,0.857142857142857,1.),.UNSPECIFIED.);
#3616=B_SPLINE_CURVE_WITH_KNOTS('',3,(#86233,#86234,#86235,#86236,#86237,
#86238,#86239,#86240,#86241,#86242),.UNSPECIFIED.,.F.,.F.,(4,1,1,1,1,1,
1,4),(0.,0.142857142857143,0.285714285714286,0.428571428571429,0.571428571428571,
0.714285714285714,0.857142857142857,1.),.UNSPECIFIED.);
#3617=B_SPLINE_CURVE_WITH_KNOTS('',3,(#86383,#86384,#86385,#86386,#86387,
#86388,#86389,#86390,#86391,#86392),.UNSPECIFIED.,.F.,.F.,(4,1,1,1,1,1,
1,4),(0.,0.142857142857143,0.285714285714286,0.428571428571429,0.571428571428571,
0.714285714285714,0.857142857142857,1.),.UNSPECIFIED.);
#3618=B_SPLINE_CURVE_WITH_KNOTS('',3,(#86433,#86434,#86435,#86436,#86437,
#86438,#86439,#86440,#86441,#86442),.UNSPECIFIED.,.F.,.F.,(4,1,1,1,1,1,
1,4),(0.,0.142857142857143,0.285714285714286,0.428571428571429,0.571428571428571,
0.714285714285714,0.857142857142857,1.),.UNSPECIFIED.);
#3619=B_SPLINE_CURVE_WITH_KNOTS('',3,(#86523,#86524,#86525,#86526,#86527,
#86528,#86529,#86530,#86531,#86532),.UNSPECIFIED.,.F.,.F.,(4,1,1,1,1,1,
1,4),(0.,0.142857142857143,0.285714285714286,0.428571428571429,0.571428571428571,
0.714285714285714,0.857142857142857,1.),.UNSPECIFIED.);
#3620=B_SPLINE_CURVE_WITH_KNOTS('',3,(#86573,#86574,#86575,#86576,#86577,
#86578,#86579,#86580,#86581,#86582,#86583,#86584,#86585,#86586,#86587,#86588,
#86589,#86590),.UNSPECIFIED.,.F.,.F.,(4,2,2,2,2,2,2,2,4),(0.,0.411606409146402,
0.882606331055175,1.58532698900237,2.58333249194715,3.5815598918848,4.32087044194964,
4.8178921514492,5.24318392698968),.UNSPECIFIED.);
#3621=B_SPLINE_CURVE_WITH_KNOTS('',3,(#86671,#86672,#86673,#86674,#86675,
#86676,#86677,#86678,#86679,#86680,#86681,#86682,#86683,#86684,#86685,#86686,
#86687,#86688),.UNSPECIFIED.,.F.,.F.,(4,2,2,2,2,2,2,2,4),(-5.06897673155691,
-4.67104605560332,-4.21569535708223,-3.5363229670094,-2.57147642457375,
-1.60641534306576,-0.891668820224186,-0.411161088211719,0.),
 .UNSPECIFIED.);
#3622=B_SPLINE_CURVE_WITH_KNOTS('',3,(#86729,#86730,#86731,#86732,#86733,
#86734,#86735,#86736,#86737,#86738),.UNSPECIFIED.,.F.,.F.,(4,1,1,1,1,1,
1,4),(0.,0.142857142857143,0.285714285714286,0.428571428571429,0.571428571428571,
0.714285714285714,0.857142857142857,1.),.UNSPECIFIED.);
#3623=B_SPLINE_CURVE_WITH_KNOTS('',3,(#86819,#86820,#86821,#86822,#86823,
#86824,#86825,#86826,#86827,#86828,#86829,#86830,#86831,#86832,#86833,#86834,
#86835,#86836,#86837,#86838,#86839,#86840),.UNSPECIFIED.,.F.,.F.,(4,3,3,
3,3,3,3,4),(0.,0.142857142857143,0.285714285714286,0.428571428571429,0.571428571428571,
0.714285714285714,0.857142857142857,1.),.UNSPECIFIED.);
#3624=B_SPLINE_CURVE_WITH_KNOTS('',3,(#86881,#86882,#86883,#86884,#86885,
#86886,#86887,#86888,#86889,#86890),.UNSPECIFIED.,.F.,.F.,(4,1,1,1,1,1,
1,4),(0.,0.142857142857143,0.285714285714286,0.428571428571429,0.571428571428571,
0.714285714285714,0.857142857142857,1.),.UNSPECIFIED.);
#3625=B_SPLINE_CURVE_WITH_KNOTS('',3,(#86971,#86972,#86973,#86974,#86975,
#86976,#86977,#86978,#86979,#86980,#86981,#86982,#86983,#86984,#86985,#86986,
#86987,#86988,#86989,#86990,#86991,#86992),.UNSPECIFIED.,.F.,.F.,(4,3,3,
3,3,3,3,4),(0.,0.142857142857143,0.285714285714286,0.428571428571429,0.571428571428571,
0.714285714285714,0.857142857142857,1.),.UNSPECIFIED.);
#3626=B_SPLINE_CURVE_WITH_KNOTS('',3,(#87033,#87034,#87035,#87036,#87037,
#87038,#87039,#87040,#87041,#87042),.UNSPECIFIED.,.F.,.F.,(4,1,1,1,1,1,
1,4),(0.,0.142857142857143,0.285714285714286,0.428571428571429,0.571428571428571,
0.714285714285714,0.857142857142857,1.),.UNSPECIFIED.);
#3627=B_SPLINE_CURVE_WITH_KNOTS('',3,(#87301,#87302,#87303,#87304,#87305,
#87306,#87307,#87308,#87309,#87310,#87311,#87312,#87313,#87314,#87315,#87316,
#87317,#87318,#87319,#87320,#87321,#87322,#87323,#87324,#87325,#87326,#87327,
#87328,#87329,#87330,#87331,#87332,#87333,#87334,#87335,#87336,#87337,#87338,
#87339,#87340,#87341,#87342,#87343,#87344,#87345,#87346,#87347,#87348,#87349,
#87350,#87351,#87352,#87353,#87354,#87355,#87356,#87357,#87358,#87359),
 .UNSPECIFIED.,.F.,.F.,(4,2,2,2,2,2,2,2,2,2,2,2,2,2,3,2,2,2,2,2,2,2,2,2,
2,2,2,2,4),(-4.85232699494737,-4.58025935130269,-4.21243389208218,-3.93854775205376,
-3.66466161202534,-3.25326473825372,-2.84186786448211,-2.43047099071049,
-2.01907411693888,-1.74518797691046,-1.47130183688203,-1.10347637766153,
-0.735650918441017,-0.367825459220508,0.,0.367825459220509,0.735650918441017,
1.10347637766153,1.47130183688203,1.74518797691046,2.01907411693888,2.43047099071049,
2.84186786448211,3.25326473825372,3.66466161202534,3.93854775205376,4.21243389208218,
4.58025935130269,4.85232699494738),.UNSPECIFIED.);
#3628=B_SPLINE_CURVE_WITH_KNOTS('',3,(#87390,#87391,#87392,#87393,#87394,
#87395,#87396,#87397,#87398,#87399,#87400,#87401,#87402,#87403),
 .UNSPECIFIED.,.F.,.F.,(4,2,2,2,2,2,4),(8.79034115467969,9.02147795200396,
9.25261474932822,9.57656340840008,9.90051206747193,10.2244607265438,10.5484093856156),
 .UNSPECIFIED.);
#3629=B_SPLINE_CURVE_WITH_KNOTS('',3,(#87405,#87406,#87407,#87408,#87409,
#87410,#87411,#87412,#87413,#87414,#87415,#87416,#87417,#87418),
 .UNSPECIFIED.,.F.,.F.,(4,2,2,2,2,2,4),(3.51613646187188,3.84008512094373,
4.16403378001558,4.48798243908744,4.81193109815929,5.04306789548355,5.27420469280782),
 .UNSPECIFIED.);
#3630=B_SPLINE_CURVE_WITH_KNOTS('',3,(#87422,#87423,#87424,#87425,#87426,
#87427,#87428,#87429,#87430,#87431,#87432,#87433,#87434,#87435,#87436,#87437,
#87438,#87439,#87440,#87441,#87442,#87443,#87444,#87445,#87446,#87447,#87448),
 .UNSPECIFIED.,.F.,.F.,(4,2,2,2,2,2,3,2,2,2,2,2,4),(5.27420469280782,5.50534149013208,
5.73647828745635,6.0604269465282,6.38437560560005,6.7083242646719,7.03227292374376,
7.35622158281561,7.68017024188746,8.00411890095931,8.32806756003117,8.55920435735543,
8.79034115467969),.UNSPECIFIED.);
#3631=B_SPLINE_CURVE_WITH_KNOTS('',3,(#87783,#87784,#87785,#87786,#87787,
#87788,#87789),.UNSPECIFIED.,.F.,.F.,(4,3,4),(0.000674089299982974,0.00549718988211594,
0.00902105606223609),.UNSPECIFIED.);
#3632=B_SPLINE_CURVE_WITH_KNOTS('',3,(#87796,#87797,#87798,#87799,#87800,
#87801,#87802),.UNSPECIFIED.,.F.,.F.,(4,3,4),(0.000736267499631611,0.00549718958832386,
0.00908323445073435),.UNSPECIFIED.);
#3633=B_SPLINE_CURVE_WITH_KNOTS('',3,(#87808,#87809,#87810,#87811,#87812,
#87813,#87814),.UNSPECIFIED.,.F.,.F.,(4,3,4),(0.000674089299982975,0.00549718988211594,
0.00902105608511028),.UNSPECIFIED.);
#3634=B_SPLINE_CURVE_WITH_KNOTS('',3,(#87817,#87818,#87819,#87820,#87821,
#87822,#87823),.UNSPECIFIED.,.F.,.F.,(4,3,4),(0.000300808474506944,0.00549718960300923,
0.0086477753818904),.UNSPECIFIED.);
#3635=B_SPLINE_CURVE_WITH_KNOTS('',3,(#87828,#87829,#87830,#87831,#87832,
#87833,#87834),.UNSPECIFIED.,.F.,.F.,(4,3,4),(0.00073626749963161,0.00549718958832386,
0.00908323445073435),.UNSPECIFIED.);
#3636=B_SPLINE_CURVE_WITH_KNOTS('',3,(#87837,#87838,#87839,#87840,#87841,
#87842,#87843),.UNSPECIFIED.,.F.,.F.,(4,3,4),(0.000674089299982974,0.00549718988211594,
0.00902105608511028),.UNSPECIFIED.);
#3637=B_SPLINE_CURVE_WITH_KNOTS('',3,(#87848,#87849,#87850,#87851,#87852,
#87853,#87854),.UNSPECIFIED.,.F.,.F.,(4,3,4),(0.000736267499631611,0.00549718958832386,
0.00908323445073436),.UNSPECIFIED.);
#3638=B_SPLINE_CURVE_WITH_KNOTS('',3,(#87857,#87858,#87859,#87860,#87861,
#87862,#87863),.UNSPECIFIED.,.F.,.F.,(4,3,4),(0.000674089299982974,0.00549718988211594,
0.00902105608511028),.UNSPECIFIED.);
#3639=B_SPLINE_CURVE_WITH_KNOTS('',3,(#87868,#87869,#87870,#87871,#87872,
#87873,#87874),.UNSPECIFIED.,.F.,.F.,(4,3,4),(0.00073626749963161,0.00549718958832386,
0.00908323445073435),.UNSPECIFIED.);
#3640=B_SPLINE_CURVE_WITH_KNOTS('',3,(#87877,#87878,#87879,#87880,#87881,
#87882,#87883),.UNSPECIFIED.,.F.,.F.,(4,3,4),(0.000674089299982977,0.00549718988211594,
0.00902105608511028),.UNSPECIFIED.);
#3641=B_SPLINE_CURVE_WITH_KNOTS('',3,(#87888,#87889,#87890,#87891,#87892,
#87893,#87894),.UNSPECIFIED.,.F.,.F.,(4,3,4),(0.000736267499631609,0.00549718958832386,
0.00908323445073436),.UNSPECIFIED.);
#3642=B_SPLINE_CURVE_WITH_KNOTS('',3,(#87897,#87898,#87899,#87900,#87901,
#87902,#87903),.UNSPECIFIED.,.F.,.F.,(4,3,4),(0.000674089299982975,0.00549718988211594,
0.00902105608511028),.UNSPECIFIED.);
#3643=B_SPLINE_CURVE_WITH_KNOTS('',3,(#87908,#87909,#87910,#87911,#87912,
#87913,#87914),.UNSPECIFIED.,.F.,.F.,(4,3,4),(0.00073626749963161,0.00549718958832386,
0.00908323445073436),.UNSPECIFIED.);
#3644=B_SPLINE_CURVE_WITH_KNOTS('',3,(#87917,#87918,#87919,#87920,#87921,
#87922,#87923),.UNSPECIFIED.,.F.,.F.,(4,3,4),(0.000674089299982974,0.00549718988211594,
0.00902105608511028),.UNSPECIFIED.);
#3645=B_SPLINE_CURVE_WITH_KNOTS('',3,(#87928,#87929,#87930,#87931,#87932,
#87933,#87934),.UNSPECIFIED.,.F.,.F.,(4,3,4),(0.00073626749963161,0.00549718958832386,
0.00908323445073435),.UNSPECIFIED.);
#3646=B_SPLINE_CURVE_WITH_KNOTS('',3,(#87937,#87938,#87939,#87940,#87941,
#87942,#87943),.UNSPECIFIED.,.F.,.F.,(4,3,4),(0.000674089299982975,0.00549718988211594,
0.00902105608511028),.UNSPECIFIED.);
#3647=B_SPLINE_CURVE_WITH_KNOTS('',3,(#87948,#87949,#87950,#87951,#87952,
#87953,#87954),.UNSPECIFIED.,.F.,.F.,(4,3,4),(0.00073626749963161,0.00549718958832386,
0.00908323445073435),.UNSPECIFIED.);
#3648=B_SPLINE_CURVE_WITH_KNOTS('',3,(#87957,#87958,#87959,#87960,#87961,
#87962,#87963),.UNSPECIFIED.,.F.,.F.,(4,3,4),(0.000674089299982974,0.00549718988211594,
0.00902105608511028),.UNSPECIFIED.);
#3649=B_SPLINE_CURVE_WITH_KNOTS('',3,(#87968,#87969,#87970,#87971,#87972,
#87973,#87974),.UNSPECIFIED.,.F.,.F.,(4,3,4),(0.000736267499631611,0.00549718958832386,
0.00908323445073436),.UNSPECIFIED.);
#3650=B_SPLINE_CURVE_WITH_KNOTS('',3,(#87977,#87978,#87979,#87980,#87981,
#87982,#87983),.UNSPECIFIED.,.F.,.F.,(4,3,4),(0.000674089299982975,0.00549718988211594,
0.00902105608511028),.UNSPECIFIED.);
#3651=B_SPLINE_CURVE_WITH_KNOTS('',3,(#87988,#87989,#87990,#87991,#87992,
#87993,#87994),.UNSPECIFIED.,.F.,.F.,(4,3,4),(0.000736267499631609,0.00549718958832386,
0.00908323445073436),.UNSPECIFIED.);
#3652=B_SPLINE_CURVE_WITH_KNOTS('',3,(#87997,#87998,#87999,#88000,#88001,
#88002,#88003),.UNSPECIFIED.,.F.,.F.,(4,3,4),(0.000674089299982975,0.00549718988211594,
0.00902105608511028),.UNSPECIFIED.);
#3653=B_SPLINE_CURVE_WITH_KNOTS('',3,(#88010,#88011,#88012,#88013,#88014,
#88015,#88016),.UNSPECIFIED.,.F.,.F.,(4,3,4),(0.0010048444099522,0.00549718948033446,
0.00935178896934134),.UNSPECIFIED.);
#3654=B_SPLINE_CURVE_WITH_KNOTS('',3,(#88023,#88024,#88025,#88026,#88027,
#88028,#88029),.UNSPECIFIED.,.F.,.F.,(4,3,4),(0.000402895054555106,0.00549718967396158,
0.00874983950741581),.UNSPECIFIED.);
#3655=B_SPLINE_CURVE_WITH_KNOTS('',3,(#88035,#88036,#88037,#88038,#88039,
#88040,#88041),.UNSPECIFIED.,.F.,.F.,(4,3,4),(0.000402895054555106,0.00549718967396158,
0.00874983950741581),.UNSPECIFIED.);
#3656=B_SPLINE_CURVE_WITH_KNOTS('',3,(#88044,#88045,#88046,#88047,#88048,
#88049,#88050),.UNSPECIFIED.,.F.,.F.,(4,3,4),(0.0010048444099522,0.00549718948033446,
0.00935178896934134),.UNSPECIFIED.);
#3657=B_SPLINE_CURVE_WITH_KNOTS('',3,(#88055,#88056,#88057,#88058,#88059,
#88060,#88061),.UNSPECIFIED.,.F.,.F.,(4,3,4),(0.000514450719951176,0.00549718949135943,
0.00886139524895251),.UNSPECIFIED.);
#3658=B_SPLINE_CURVE_WITH_KNOTS('',3,(#88064,#88065,#88066,#88067,#88068,
#88069,#88070),.UNSPECIFIED.,.F.,.F.,(4,3,4),(0.000402895054555106,0.00549718967396158,
0.00874983950741581),.UNSPECIFIED.);
#3659=B_SPLINE_CURVE_WITH_KNOTS('',3,(#88075,#88076,#88077,#88078,#88079,
#88080,#88081),.UNSPECIFIED.,.F.,.F.,(4,3,4),(0.000595284717236738,0.00549718948949992,
0.00894222925114684),.UNSPECIFIED.);
#3660=B_SPLINE_CURVE_WITH_KNOTS('',3,(#88084,#88085,#88086,#88087,#88088,
#88089,#88090),.UNSPECIFIED.,.F.,.F.,(4,3,4),(0.000402895054555105,0.00549718967396158,
0.00874983950741581),.UNSPECIFIED.);
#3661=B_SPLINE_CURVE_WITH_KNOTS('',3,(#88095,#88096,#88097,#88098,#88099,
#88100,#88101),.UNSPECIFIED.,.F.,.F.,(4,3,4),(0.0010048444099522,0.00549718948033446,
0.00935178896934135),.UNSPECIFIED.);
#3662=B_SPLINE_CURVE_WITH_KNOTS('',3,(#88104,#88105,#88106,#88107,#88108,
#88109,#88110),.UNSPECIFIED.,.F.,.F.,(4,3,4),(0.000402895054555106,0.00549718967396158,
0.00874983949247052),.UNSPECIFIED.);
#3663=B_SPLINE_CURVE_WITH_KNOTS('',3,(#88115,#88116,#88117,#88118,#88119,
#88120,#88121),.UNSPECIFIED.,.F.,.F.,(4,3,4),(0.0010048444099522,0.00549718948033446,
0.00935178896934134),.UNSPECIFIED.);
#3664=B_SPLINE_CURVE_WITH_KNOTS('',3,(#88124,#88125,#88126,#88127,#88128,
#88129,#88130),.UNSPECIFIED.,.F.,.F.,(4,3,4),(0.000402895054555107,0.00549718967396158,
0.0087498394949498),.UNSPECIFIED.);
#3665=B_SPLINE_CURVE_WITH_KNOTS('',3,(#88135,#88136,#88137,#88138,#88139,
#88140,#88141),.UNSPECIFIED.,.F.,.F.,(4,3,4),(0.0010048444099522,0.00549718948033446,
0.00935178896934135),.UNSPECIFIED.);
#3666=B_SPLINE_CURVE_WITH_KNOTS('',3,(#88144,#88145,#88146,#88147,#88148,
#88149,#88150),.UNSPECIFIED.,.F.,.F.,(4,3,4),(0.000402895054555106,0.00549718967396158,
0.00874983947706886),.UNSPECIFIED.);
#3667=B_SPLINE_CURVE_WITH_KNOTS('',3,(#88155,#88156,#88157,#88158,#88159,
#88160,#88161),.UNSPECIFIED.,.F.,.F.,(4,3,4),(1.68383824729309E-5,0.00549718950318958,
0.00836378288127802),.UNSPECIFIED.);
#3668=B_SPLINE_CURVE_WITH_KNOTS('',3,(#88164,#88165,#88166,#88167,#88168,
#88169,#88170),.UNSPECIFIED.,.F.,.F.,(4,3,4),(0.000402895054555107,0.00549718967396158,
0.00874983950741581),.UNSPECIFIED.);
#3669=B_SPLINE_CURVE_WITH_KNOTS('',3,(#88175,#88176,#88177,#88178,#88179,
#88180,#88181),.UNSPECIFIED.,.F.,.F.,(4,3,4),(0.0010048444099522,0.00549718948033446,
0.00935178896934135),.UNSPECIFIED.);
#3670=B_SPLINE_CURVE_WITH_KNOTS('',3,(#88184,#88185,#88186,#88187,#88188,
#88189,#88190),.UNSPECIFIED.,.F.,.F.,(4,3,4),(0.000402895054555113,0.00549718967396158,
0.00874983950741582),.UNSPECIFIED.);
#3671=B_SPLINE_CURVE_WITH_KNOTS('',3,(#88195,#88196,#88197,#88198,#88199,
#88200,#88201),.UNSPECIFIED.,.F.,.F.,(4,3,4),(0.000117964457281399,0.00549718950073096,
0.00846490896228074),.UNSPECIFIED.);
#3672=B_SPLINE_CURVE_WITH_KNOTS('',3,(#88204,#88205,#88206,#88207,#88208,
#88209,#88210),.UNSPECIFIED.,.F.,.F.,(4,3,4),(0.000402895054555107,0.00549718967396158,
0.00874983950741581),.UNSPECIFIED.);
#3673=B_SPLINE_CURVE_WITH_KNOTS('',3,(#88215,#88216,#88217,#88218,#88219,
#88220,#88221),.UNSPECIFIED.,.F.,.F.,(4,3,4),(0.0010048444099522,0.00549718948033446,
0.00935178896934134),.UNSPECIFIED.);
#3674=B_SPLINE_CURVE_WITH_KNOTS('',3,(#88224,#88225,#88226,#88227,#88228,
#88229,#88230),.UNSPECIFIED.,.F.,.F.,(4,3,4),(0.000402895054555106,0.00549718967396158,
0.00874983948021838),.UNSPECIFIED.);
#3675=LINE('',#17358,#4145);
#3676=LINE('',#17382,#4146);
#3677=LINE('',#17752,#4147);
#3678=LINE('',#18130,#4148);
#3679=LINE('',#18586,#4149);
#3680=LINE('',#18970,#4150);
#3681=LINE('',#19422,#4151);
#3682=LINE('',#19806,#4152);
#3683=LINE('',#20104,#4153);
#3684=LINE('',#20396,#4154);
#3685=LINE('',#20692,#4155);
#3686=LINE('',#20989,#4156);
#3687=LINE('',#21186,#4157);
#3688=LINE('',#21289,#4158);
#3689=LINE('',#21481,#4159);
#3690=LINE('',#21773,#4160);
#3691=LINE('',#22068,#4161);
#3692=LINE('',#22363,#4162);
#3693=LINE('',#22659,#4163);
#3694=LINE('',#23075,#4164);
#3695=LINE('',#23264,#4165);
#3696=LINE('',#23678,#4166);
#3697=LINE('',#23979,#4167);
#3698=LINE('',#24393,#4168);
#3699=LINE('',#26899,#4169);
#3700=LINE('',#26903,#4170);
#3701=LINE('',#26907,#4171);
#3702=LINE('',#26911,#4172);
#3703=LINE('',#26915,#4173);
#3704=LINE('',#26919,#4174);
#3705=LINE('',#26923,#4175);
#3706=LINE('',#26927,#4176);
#3707=LINE('',#26931,#4177);
#3708=LINE('',#26935,#4178);
#3709=LINE('',#26939,#4179);
#3710=LINE('',#26943,#4180);
#3711=LINE('',#26947,#4181);
#3712=LINE('',#26951,#4182);
#3713=LINE('',#26955,#4183);
#3714=LINE('',#26959,#4184);
#3715=LINE('',#26963,#4185);
#3716=LINE('',#26967,#4186);
#3717=LINE('',#26971,#4187);
#3718=LINE('',#26975,#4188);
#3719=LINE('',#26979,#4189);
#3720=LINE('',#26983,#4190);
#3721=LINE('',#26987,#4191);
#3722=LINE('',#26991,#4192);
#3723=LINE('',#26995,#4193);
#3724=LINE('',#26999,#4194);
#3725=LINE('',#27003,#4195);
#3726=LINE('',#27007,#4196);
#3727=LINE('',#27011,#4197);
#3728=LINE('',#27015,#4198);
#3729=LINE('',#27019,#4199);
#3730=LINE('',#27023,#4200);
#3731=LINE('',#27027,#4201);
#3732=LINE('',#27031,#4202);
#3733=LINE('',#27035,#4203);
#3734=LINE('',#27038,#4204);
#3735=LINE('',#27042,#4205);
#3736=LINE('',#27046,#4206);
#3737=LINE('',#27051,#4207);
#3738=LINE('',#27055,#4208);
#3739=LINE('',#27060,#4209);
#3740=LINE('',#27064,#4210);
#3741=LINE('',#27069,#4211);
#3742=LINE('',#27073,#4212);
#3743=LINE('',#27078,#4213);
#3744=LINE('',#27082,#4214);
#3745=LINE('',#27087,#4215);
#3746=LINE('',#27091,#4216);
#3747=LINE('',#27096,#4217);
#3748=LINE('',#27100,#4218);
#3749=LINE('',#27105,#4219);
#3750=LINE('',#27109,#4220);
#3751=LINE('',#27114,#4221);
#3752=LINE('',#27118,#4222);
#3753=LINE('',#27123,#4223);
#3754=LINE('',#27127,#4224);
#3755=LINE('',#27132,#4225);
#3756=LINE('',#27136,#4226);
#3757=LINE('',#27141,#4227);
#3758=LINE('',#27145,#4228);
#3759=LINE('',#27150,#4229);
#3760=LINE('',#27154,#4230);
#3761=LINE('',#27159,#4231);
#3762=LINE('',#27163,#4232);
#3763=LINE('',#27168,#4233);
#3764=LINE('',#27172,#4234);
#3765=LINE('',#27177,#4235);
#3766=LINE('',#27181,#4236);
#3767=LINE('',#27186,#4237);
#3768=LINE('',#27190,#4238);
#3769=LINE('',#27195,#4239);
#3770=LINE('',#27199,#4240);
#3771=LINE('',#27207,#4241);
#3772=LINE('',#27227,#4242);
#3773=LINE('',#27234,#4243);
#3774=LINE('',#27254,#4244);
#3775=LINE('',#27261,#4245);
#3776=LINE('',#27279,#4246);
#3777=LINE('',#27286,#4247);
#3778=LINE('',#27306,#4248);
#3779=LINE('',#27313,#4249);
#3780=LINE('',#27333,#4250);
#3781=LINE('',#27340,#4251);
#3782=LINE('',#27360,#4252);
#3783=LINE('',#27367,#4253);
#3784=LINE('',#27385,#4254);
#3785=LINE('',#27392,#4255);
#3786=LINE('',#27412,#4256);
#3787=LINE('',#27419,#4257);
#3788=LINE('',#27439,#4258);
#3789=LINE('',#27446,#4259);
#3790=LINE('',#27466,#4260);
#3791=LINE('',#27473,#4261);
#3792=LINE('',#27491,#4262);
#3793=LINE('',#27498,#4263);
#3794=LINE('',#27518,#4264);
#3795=LINE('',#27525,#4265);
#3796=LINE('',#27545,#4266);
#3797=LINE('',#27552,#4267);
#3798=LINE('',#27572,#4268);
#3799=LINE('',#27579,#4269);
#3800=LINE('',#27599,#4270);
#3801=LINE('',#27606,#4271);
#3802=LINE('',#27626,#4272);
#3803=LINE('',#27633,#4273);
#3804=LINE('',#27653,#4274);
#3805=LINE('',#27660,#4275);
#3806=LINE('',#27680,#4276);
#3807=LINE('',#27690,#4277);
#3808=LINE('',#27713,#4278);
#3809=LINE('',#27723,#4279);
#3810=LINE('',#27746,#4280);
#3811=LINE('',#27756,#4281);
#3812=LINE('',#27781,#4282);
#3813=LINE('',#27791,#4283);
#3814=LINE('',#27812,#4284);
#3815=LINE('',#27822,#4285);
#3816=LINE('',#27847,#4286);
#3817=LINE('',#27857,#4287);
#3818=LINE('',#27882,#4288);
#3819=LINE('',#27892,#4289);
#3820=LINE('',#27915,#4290);
#3821=LINE('',#27925,#4291);
#3822=LINE('',#27948,#4292);
#3823=LINE('',#27958,#4293);
#3824=LINE('',#27983,#4294);
#3825=LINE('',#27993,#4295);
#3826=LINE('',#28018,#4296);
#3827=LINE('',#28028,#4297);
#3828=LINE('',#28051,#4298);
#3829=LINE('',#28061,#4299);
#3830=LINE('',#28084,#4300);
#3831=LINE('',#28094,#4301);
#3832=LINE('',#28117,#4302);
#3833=LINE('',#28127,#4303);
#3834=LINE('',#28152,#4304);
#3835=LINE('',#28162,#4305);
#3836=LINE('',#28187,#4306);
#3837=LINE('',#28197,#4307);
#3838=LINE('',#28220,#4308);
#3839=LINE('',#28230,#4309);
#3840=LINE('',#28253,#4310);
#3841=LINE('',#28263,#4311);
#3842=LINE('',#28284,#4312);
#3843=LINE('',#28287,#4313);
#3844=LINE('',#28289,#4314);
#3845=LINE('',#28293,#4315);
#3846=LINE('',#28295,#4316);
#3847=LINE('',#28299,#4317);
#3848=LINE('',#28301,#4318);
#3849=LINE('',#28305,#4319);
#3850=LINE('',#28307,#4320);
#3851=LINE('',#28311,#4321);
#3852=LINE('',#28313,#4322);
#3853=LINE('',#28317,#4323);
#3854=LINE('',#28319,#4324);
#3855=LINE('',#28323,#4325);
#3856=LINE('',#28325,#4326);
#3857=LINE('',#28329,#4327);
#3858=LINE('',#28331,#4328);
#3859=LINE('',#28335,#4329);
#3860=LINE('',#28337,#4330);
#3861=LINE('',#28341,#4331);
#3862=LINE('',#28343,#4332);
#3863=LINE('',#28347,#4333);
#3864=LINE('',#28349,#4334);
#3865=LINE('',#28353,#4335);
#3866=LINE('',#28355,#4336);
#3867=LINE('',#28359,#4337);
#3868=LINE('',#28361,#4338);
#3869=LINE('',#28365,#4339);
#3870=LINE('',#28367,#4340);
#3871=LINE('',#28371,#4341);
#3872=LINE('',#28373,#4342);
#3873=LINE('',#28377,#4343);
#3874=LINE('',#28379,#4344);
#3875=LINE('',#28383,#4345);
#3876=LINE('',#28385,#4346);
#3877=LINE('',#28389,#4347);
#3878=LINE('',#28391,#4348);
#3879=LINE('',#31480,#4349);
#3880=LINE('',#31544,#4350);
#3881=LINE('',#31607,#4351);
#3882=LINE('',#31628,#4352);
#3883=LINE('',#31662,#4353);
#3884=LINE('',#31706,#4354);
#3885=LINE('',#31731,#4355);
#3886=LINE('',#31733,#4356);
#3887=LINE('',#31736,#4357);
#3888=LINE('',#31738,#4358);
#3889=LINE('',#31741,#4359);
#3890=LINE('',#31743,#4360);
#3891=LINE('',#31746,#4361);
#3892=LINE('',#31748,#4362);
#3893=LINE('',#31751,#4363);
#3894=LINE('',#31753,#4364);
#3895=LINE('',#31756,#4365);
#3896=LINE('',#31758,#4366);
#3897=LINE('',#31761,#4367);
#3898=LINE('',#31763,#4368);
#3899=LINE('',#31766,#4369);
#3900=LINE('',#31768,#4370);
#3901=LINE('',#31771,#4371);
#3902=LINE('',#31773,#4372);
#3903=LINE('',#31776,#4373);
#3904=LINE('',#31778,#4374);
#3905=LINE('',#31781,#4375);
#3906=LINE('',#31783,#4376);
#3907=LINE('',#31786,#4377);
#3908=LINE('',#31788,#4378);
#3909=LINE('',#31791,#4379);
#3910=LINE('',#31793,#4380);
#3911=LINE('',#31796,#4381);
#3912=LINE('',#31798,#4382);
#3913=LINE('',#31801,#4383);
#3914=LINE('',#31802,#4384);
#3915=LINE('',#32981,#4385);
#3916=LINE('',#32987,#4386);
#3917=LINE('',#32993,#4387);
#3918=LINE('',#33005,#4388);
#3919=LINE('',#33013,#4389);
#3920=LINE('',#33019,#4390);
#3921=LINE('',#33241,#4391);
#3922=LINE('',#33740,#4392);
#3923=LINE('',#34236,#4393);
#3924=LINE('',#34744,#4394);
#3925=LINE('',#35252,#4395);
#3926=LINE('',#35748,#4396);
#3927=LINE('',#36250,#4397);
#3928=LINE('',#36746,#4398);
#3929=LINE('',#37233,#4399);
#3930=LINE('',#37732,#4400);
#3931=LINE('',#38240,#4401);
#3932=LINE('',#38733,#4402);
#3933=LINE('',#39229,#4403);
#3934=LINE('',#39737,#4404);
#3935=LINE('',#40245,#4405);
#3936=LINE('',#40744,#4406);
#3937=LINE('',#41240,#4407);
#3938=LINE('',#41733,#4408);
#3939=LINE('',#42220,#4409);
#3940=LINE('',#42722,#4410);
#3941=LINE('',#43230,#4411);
#3942=LINE('',#43723,#4412);
#3943=LINE('',#44225,#4413);
#3944=LINE('',#44733,#4414);
#3945=LINE('',#45238,#4415);
#3946=LINE('',#45734,#4416);
#3947=LINE('',#46230,#4417);
#3948=LINE('',#46723,#4418);
#3949=LINE('',#47207,#4419);
#3950=LINE('',#47709,#4420);
#3951=LINE('',#48217,#4421);
#3952=LINE('',#48722,#4422);
#3953=LINE('',#49215,#4423);
#3954=LINE('',#49714,#4424);
#3955=LINE('',#50198,#4425);
#3956=LINE('',#50679,#4426);
#3957=LINE('',#51181,#4427);
#3958=LINE('',#51683,#4428);
#3959=LINE('',#52188,#4429);
#3960=LINE('',#52675,#4430);
#3961=LINE('',#53168,#4431);
#3962=LINE('',#53679,#4432);
#3963=LINE('',#54172,#4433);
#3964=LINE('',#54671,#4434);
#3965=LINE('',#55155,#4435);
#3966=LINE('',#55636,#4436);
#3967=LINE('',#56135,#4437);
#3968=LINE('',#56640,#4438);
#3969=LINE('',#57136,#4439);
#3970=LINE('',#57629,#4440);
#3971=LINE('',#58125,#4441);
#3972=LINE('',#58633,#4442);
#3973=LINE('',#59120,#4443);
#3974=LINE('',#59625,#4444);
#3975=LINE('',#60109,#4445);
#3976=LINE('',#60587,#4446);
#3977=LINE('',#61086,#4447);
#3978=LINE('',#61591,#4448);
#3979=LINE('',#62087,#4449);
#3980=LINE('',#81918,#4450);
#3981=LINE('',#81924,#4451);
#3982=LINE('',#81930,#4452);
#3983=LINE('',#81936,#4453);
#3984=LINE('',#81951,#4454);
#3985=LINE('',#81963,#4455);
#3986=LINE('',#82209,#4456);
#3987=LINE('',#82727,#4457);
#3988=LINE('',#83245,#4458);
#3989=LINE('',#83763,#4459);
#3990=LINE('',#84281,#4460);
#3991=LINE('',#85045,#4461);
#3992=LINE('',#85095,#4462);
#3993=LINE('',#85148,#4463);
#3994=LINE('',#85455,#4464);
#3995=LINE('',#85481,#4465);
#3996=LINE('',#85523,#4466);
#3997=LINE('',#85537,#4467);
#3998=LINE('',#85540,#4468);
#3999=LINE('',#85559,#4469);
#4000=LINE('',#85600,#4470);
#4001=LINE('',#85612,#4471);
#4002=LINE('',#85653,#4472);
#4003=LINE('',#85695,#4473);
#4004=LINE('',#85707,#4474);
#4005=LINE('',#85749,#4475);
#4006=LINE('',#85761,#4476);
#4007=LINE('',#85802,#4477);
#4008=LINE('',#85803,#4478);
#4009=LINE('',#85845,#4479);
#4010=LINE('',#85857,#4480);
#4011=LINE('',#85899,#4481);
#4012=LINE('',#85919,#4482);
#4013=LINE('',#85960,#4483);
#4014=LINE('',#85961,#4484);
#4015=LINE('',#86003,#4485);
#4016=LINE('',#86027,#4486);
#4017=LINE('',#86069,#4487);
#4018=LINE('',#86081,#4488);
#4019=LINE('',#86122,#4489);
#4020=LINE('',#86123,#4490);
#4021=LINE('',#86165,#4491);
#4022=LINE('',#86189,#4492);
#4023=LINE('',#86231,#4493);
#4024=LINE('',#86243,#4494);
#4025=LINE('',#86284,#4495);
#4026=LINE('',#86285,#4496);
#4027=LINE('',#86302,#4497);
#4028=LINE('',#87095,#4498);
#4029=LINE('',#87110,#4499);
#4030=LINE('',#87114,#4500);
#4031=LINE('',#87118,#4501);
#4032=LINE('',#87122,#4502);
#4033=LINE('',#87127,#4503);
#4034=LINE('',#87134,#4504);
#4035=LINE('',#87141,#4505);
#4036=LINE('',#87148,#4506);
#4037=LINE('',#87155,#4507);
#4038=LINE('',#87162,#4508);
#4039=LINE('',#87168,#4509);
#4040=LINE('',#87175,#4510);
#4041=LINE('',#87182,#4511);
#4042=LINE('',#87189,#4512);
#4043=LINE('',#87195,#4513);
#4044=LINE('',#87201,#4514);
#4045=LINE('',#87207,#4515);
#4046=LINE('',#87214,#4516);
#4047=LINE('',#87217,#4517);
#4048=LINE('',#87220,#4518);
#4049=LINE('',#87224,#4519);
#4050=LINE('',#87228,#4520);
#4051=LINE('',#87230,#4521);
#4052=LINE('',#87232,#4522);
#4053=LINE('',#87234,#4523);
#4054=LINE('',#87236,#4524);
#4055=LINE('',#87242,#4525);
#4056=LINE('',#87244,#4526);
#4057=LINE('',#87246,#4527);
#4058=LINE('',#87248,#4528);
#4059=LINE('',#87250,#4529);
#4060=LINE('',#87253,#4530);
#4061=LINE('',#87256,#4531);
#4062=LINE('',#87257,#4532);
#4063=LINE('',#87261,#4533);
#4064=LINE('',#87266,#4534);
#4065=LINE('',#87267,#4535);
#4066=LINE('',#87269,#4536);
#4067=LINE('',#87271,#4537);
#4068=LINE('',#87272,#4538);
#4069=LINE('',#87276,#4539);
#4070=LINE('',#87278,#4540);
#4071=LINE('',#87281,#4541);
#4072=LINE('',#87284,#4542);
#4073=LINE('',#87287,#4543);
#4074=LINE('',#87288,#4544);
#4075=LINE('',#87292,#4545);
#4076=LINE('',#87295,#4546);
#4077=LINE('',#87299,#4547);
#4078=LINE('',#87361,#4548);
#4079=LINE('',#87364,#4549);
#4080=LINE('',#87366,#4550);
#4081=LINE('',#87369,#4551);
#4082=LINE('',#87371,#4552);
#4083=LINE('',#87378,#4553);
#4084=LINE('',#87385,#4554);
#4085=LINE('',#87388,#4555);
#4086=LINE('',#87420,#4556);
#4087=LINE('',#87454,#4557);
#4088=LINE('',#87460,#4558);
#4089=LINE('',#87468,#4559);
#4090=LINE('',#87474,#4560);
#4091=LINE('',#87480,#4561);
#4092=LINE('',#87493,#4562);
#4093=LINE('',#87499,#4563);
#4094=LINE('',#87514,#4564);
#4095=LINE('',#87521,#4565);
#4096=LINE('',#87525,#4566);
#4097=LINE('',#87538,#4567);
#4098=LINE('',#87541,#4568);
#4099=LINE('',#87561,#4569);
#4100=LINE('',#87572,#4570);
#4101=LINE('',#87577,#4571);
#4102=LINE('',#87585,#4572);
#4103=LINE('',#87591,#4573);
#4104=LINE('',#87599,#4574);
#4105=LINE('',#87607,#4575);
#4106=LINE('',#87611,#4576);
#4107=LINE('',#87618,#4577);
#4108=LINE('',#87623,#4578);
#4109=LINE('',#87627,#4579);
#4110=LINE('',#87633,#4580);
#4111=LINE('',#87639,#4581);
#4112=LINE('',#87643,#4582);
#4113=LINE('',#87650,#4583);
#4114=LINE('',#87689,#4584);
#4115=LINE('',#87697,#4585);
#4116=LINE('',#87709,#4586);
#4117=LINE('',#87713,#4587);
#4118=LINE('',#87735,#4588);
#4119=LINE('',#87738,#4589);
#4120=LINE('',#87747,#4590);
#4121=LINE('',#87757,#4591);
#4122=LINE('',#87774,#4592);
#4123=LINE('',#87776,#4593);
#4124=LINE('',#87779,#4594);
#4125=LINE('',#87792,#4595);
#4126=LINE('',#88006,#4596);
#4127=LINE('',#88019,#4597);
#4128=LINE('',#88337,#4598);
#4129=LINE('',#88345,#4599);
#4130=LINE('',#88349,#4600);
#4131=LINE('',#88353,#4601);
#4132=LINE('',#88356,#4602);
#4133=LINE('',#88360,#4603);
#4134=LINE('',#88367,#4604);
#4135=LINE('',#88375,#4605);
#4136=LINE('',#88383,#4606);
#4137=LINE('',#88391,#4607);
#4138=LINE('',#88399,#4608);
#4139=LINE('',#88407,#4609);
#4140=LINE('',#88415,#4610);
#4141=LINE('',#88423,#4611);
#4142=LINE('',#88431,#4612);
#4143=LINE('',#88439,#4613);
#4144=LINE('',#88447,#4614);
#4145=VECTOR('',#14385,8.12525);
#4146=VECTOR('',#14390,8.12525);
#4147=VECTOR('',#14393,8.12525);
#4148=VECTOR('',#14396,8.12525);
#4149=VECTOR('',#14399,8.12525);
#4150=VECTOR('',#14402,8.12525);
#4151=VECTOR('',#14405,8.12525);
#4152=VECTOR('',#14408,8.12525);
#4153=VECTOR('',#14411,8.12525);
#4154=VECTOR('',#14414,8.12525);
#4155=VECTOR('',#14417,8.12525);
#4156=VECTOR('',#14420,8.12525);
#4157=VECTOR('',#14425,7.01125);
#4158=VECTOR('',#14430,7.01125);
#4159=VECTOR('',#14433,7.01125);
#4160=VECTOR('',#14436,7.01125);
#4161=VECTOR('',#14439,7.01125);
#4162=VECTOR('',#14442,7.01125);
#4163=VECTOR('',#14445,7.01125);
#4164=VECTOR('',#14448,7.01125);
#4165=VECTOR('',#14451,7.01125);
#4166=VECTOR('',#14454,7.01125);
#4167=VECTOR('',#14457,7.01125);
#4168=VECTOR('',#14460,7.01125);
#4169=VECTOR('',#14471,10.);
#4170=VECTOR('',#14474,10.);
#4171=VECTOR('',#14477,10.);
#4172=VECTOR('',#14480,10.);
#4173=VECTOR('',#14483,10.);
#4174=VECTOR('',#14486,10.);
#4175=VECTOR('',#14489,10.);
#4176=VECTOR('',#14492,10.);
#4177=VECTOR('',#14495,10.);
#4178=VECTOR('',#14498,10.);
#4179=VECTOR('',#14501,10.);
#4180=VECTOR('',#14504,10.);
#4181=VECTOR('',#14507,10.);
#4182=VECTOR('',#14510,10.);
#4183=VECTOR('',#14513,10.);
#4184=VECTOR('',#14516,10.);
#4185=VECTOR('',#14519,10.);
#4186=VECTOR('',#14522,10.);
#4187=VECTOR('',#14525,10.);
#4188=VECTOR('',#14528,10.);
#4189=VECTOR('',#14531,10.);
#4190=VECTOR('',#14534,10.);
#4191=VECTOR('',#14537,10.);
#4192=VECTOR('',#14540,10.);
#4193=VECTOR('',#14543,10.);
#4194=VECTOR('',#14546,10.);
#4195=VECTOR('',#14549,10.);
#4196=VECTOR('',#14552,10.);
#4197=VECTOR('',#14555,10.);
#4198=VECTOR('',#14558,10.);
#4199=VECTOR('',#14561,10.);
#4200=VECTOR('',#14564,10.);
#4201=VECTOR('',#14567,10.);
#4202=VECTOR('',#14570,10.);
#4203=VECTOR('',#14573,10.);
#4204=VECTOR('',#14576,10.);
#4205=VECTOR('',#14579,10.);
#4206=VECTOR('',#14582,10.);
#4207=VECTOR('',#14587,10.);
#4208=VECTOR('',#14590,10.);
#4209=VECTOR('',#14595,10.);
#4210=VECTOR('',#14598,10.);
#4211=VECTOR('',#14603,10.);
#4212=VECTOR('',#14606,10.);
#4213=VECTOR('',#14611,10.);
#4214=VECTOR('',#14614,10.);
#4215=VECTOR('',#14619,10.);
#4216=VECTOR('',#14622,10.);
#4217=VECTOR('',#14627,10.);
#4218=VECTOR('',#14630,10.);
#4219=VECTOR('',#14635,10.);
#4220=VECTOR('',#14638,10.);
#4221=VECTOR('',#14643,10.);
#4222=VECTOR('',#14646,10.);
#4223=VECTOR('',#14651,10.);
#4224=VECTOR('',#14654,10.);
#4225=VECTOR('',#14659,10.);
#4226=VECTOR('',#14662,10.);
#4227=VECTOR('',#14667,10.);
#4228=VECTOR('',#14670,10.);
#4229=VECTOR('',#14675,10.);
#4230=VECTOR('',#14678,10.);
#4231=VECTOR('',#14683,10.);
#4232=VECTOR('',#14686,10.);
#4233=VECTOR('',#14691,10.);
#4234=VECTOR('',#14694,10.);
#4235=VECTOR('',#14699,10.);
#4236=VECTOR('',#14702,10.);
#4237=VECTOR('',#14707,10.);
#4238=VECTOR('',#14710,10.);
#4239=VECTOR('',#14715,10.);
#4240=VECTOR('',#14718,10.);
#4241=VECTOR('',#14727,10.);
#4242=VECTOR('',#14728,10.);
#4243=VECTOR('',#14735,10.);
#4244=VECTOR('',#14736,10.);
#4245=VECTOR('',#14743,10.);
#4246=VECTOR('',#14744,10.);
#4247=VECTOR('',#14751,10.);
#4248=VECTOR('',#14752,10.);
#4249=VECTOR('',#14759,10.);
#4250=VECTOR('',#14760,10.);
#4251=VECTOR('',#14767,10.);
#4252=VECTOR('',#14768,10.);
#4253=VECTOR('',#14775,10.);
#4254=VECTOR('',#14776,10.);
#4255=VECTOR('',#14783,10.);
#4256=VECTOR('',#14784,10.);
#4257=VECTOR('',#14791,10.);
#4258=VECTOR('',#14792,10.);
#4259=VECTOR('',#14799,10.);
#4260=VECTOR('',#14800,10.);
#4261=VECTOR('',#14807,10.);
#4262=VECTOR('',#14808,10.);
#4263=VECTOR('',#14815,10.);
#4264=VECTOR('',#14816,10.);
#4265=VECTOR('',#14823,10.);
#4266=VECTOR('',#14824,10.);
#4267=VECTOR('',#14831,10.);
#4268=VECTOR('',#14832,10.);
#4269=VECTOR('',#14839,10.);
#4270=VECTOR('',#14840,10.);
#4271=VECTOR('',#14847,10.);
#4272=VECTOR('',#14848,10.);
#4273=VECTOR('',#14855,10.);
#4274=VECTOR('',#14856,10.);
#4275=VECTOR('',#14863,10.);
#4276=VECTOR('',#14864,10.);
#4277=VECTOR('',#14873,10.);
#4278=VECTOR('',#14876,10.);
#4279=VECTOR('',#14885,10.);
#4280=VECTOR('',#14888,10.);
#4281=VECTOR('',#14897,10.);
#4282=VECTOR('',#14900,10.);
#4283=VECTOR('',#14909,10.);
#4284=VECTOR('',#14912,10.);
#4285=VECTOR('',#14921,10.);
#4286=VECTOR('',#14924,10.);
#4287=VECTOR('',#14933,10.);
#4288=VECTOR('',#14936,10.);
#4289=VECTOR('',#14945,10.);
#4290=VECTOR('',#14948,10.);
#4291=VECTOR('',#14957,10.);
#4292=VECTOR('',#14960,10.);
#4293=VECTOR('',#14969,10.);
#4294=VECTOR('',#14972,10.);
#4295=VECTOR('',#14981,10.);
#4296=VECTOR('',#14984,10.);
#4297=VECTOR('',#14993,10.);
#4298=VECTOR('',#14996,10.);
#4299=VECTOR('',#15005,10.);
#4300=VECTOR('',#15008,10.);
#4301=VECTOR('',#15017,10.);
#4302=VECTOR('',#15020,10.);
#4303=VECTOR('',#15029,10.);
#4304=VECTOR('',#15032,10.);
#4305=VECTOR('',#15041,10.);
#4306=VECTOR('',#15044,10.);
#4307=VECTOR('',#15053,10.);
#4308=VECTOR('',#15056,10.);
#4309=VECTOR('',#15065,10.);
#4310=VECTOR('',#15068,10.);
#4311=VECTOR('',#15077,10.);
#4312=VECTOR('',#15080,10.);
#4313=VECTOR('',#15083,10.);
#4314=VECTOR('',#15084,10.);
#4315=VECTOR('',#15089,10.);
#4316=VECTOR('',#15090,10.);
#4317=VECTOR('',#15095,10.);
#4318=VECTOR('',#15096,10.);
#4319=VECTOR('',#15101,10.);
#4320=VECTOR('',#15102,10.);
#4321=VECTOR('',#15107,10.);
#4322=VECTOR('',#15108,10.);
#4323=VECTOR('',#15113,10.);
#4324=VECTOR('',#15114,10.);
#4325=VECTOR('',#15119,10.);
#4326=VECTOR('',#15120,10.);
#4327=VECTOR('',#15125,10.);
#4328=VECTOR('',#15126,10.);
#4329=VECTOR('',#15131,10.);
#4330=VECTOR('',#15132,10.);
#4331=VECTOR('',#15137,10.);
#4332=VECTOR('',#15138,10.);
#4333=VECTOR('',#15143,10.);
#4334=VECTOR('',#15144,10.);
#4335=VECTOR('',#15149,10.);
#4336=VECTOR('',#15150,10.);
#4337=VECTOR('',#15155,10.);
#4338=VECTOR('',#15156,10.);
#4339=VECTOR('',#15161,10.);
#4340=VECTOR('',#15162,10.);
#4341=VECTOR('',#15167,10.);
#4342=VECTOR('',#15168,10.);
#4343=VECTOR('',#15173,10.);
#4344=VECTOR('',#15174,10.);
#4345=VECTOR('',#15179,10.);
#4346=VECTOR('',#15180,10.);
#4347=VECTOR('',#15185,10.);
#4348=VECTOR('',#15186,10.);
#4349=VECTOR('',#15681,10.);
#4350=VECTOR('',#15682,10.);
#4351=VECTOR('',#15691,10.);
#4352=VECTOR('',#15692,10.);
#4353=VECTOR('',#15693,10.);
#4354=VECTOR('',#15694,10.);
#4355=VECTOR('',#15701,10.);
#4356=VECTOR('',#15702,10.);
#4357=VECTOR('',#15705,10.);
#4358=VECTOR('',#15706,10.);
#4359=VECTOR('',#15709,10.);
#4360=VECTOR('',#15710,10.);
#4361=VECTOR('',#15713,10.);
#4362=VECTOR('',#15714,10.);
#4363=VECTOR('',#15717,10.);
#4364=VECTOR('',#15718,10.);
#4365=VECTOR('',#15721,10.);
#4366=VECTOR('',#15722,10.);
#4367=VECTOR('',#15725,10.);
#4368=VECTOR('',#15726,10.);
#4369=VECTOR('',#15729,10.);
#4370=VECTOR('',#15730,10.);
#4371=VECTOR('',#15733,10.);
#4372=VECTOR('',#15734,10.);
#4373=VECTOR('',#15737,10.);
#4374=VECTOR('',#15738,10.);
#4375=VECTOR('',#15741,10.);
#4376=VECTOR('',#15742,10.);
#4377=VECTOR('',#15745,10.);
#4378=VECTOR('',#15746,10.);
#4379=VECTOR('',#15749,10.);
#4380=VECTOR('',#15750,10.);
#4381=VECTOR('',#15753,10.);
#4382=VECTOR('',#15754,10.);
#4383=VECTOR('',#15757,10.);
#4384=VECTOR('',#15758,10.);
#4385=VECTOR('',#15797,1.);
#4386=VECTOR('',#15804,1.);
#4387=VECTOR('',#15811,1.);
#4388=VECTOR('',#15826,13.5);
#4389=VECTOR('',#15837,5.5);
#4390=VECTOR('',#15844,6.767);
#4391=VECTOR('',#15849,6.767);
#4392=VECTOR('',#15852,6.767);
#4393=VECTOR('',#15855,6.767);
#4394=VECTOR('',#15858,6.767);
#4395=VECTOR('',#15861,6.767);
#4396=VECTOR('',#15864,6.767);
#4397=VECTOR('',#15867,6.767);
#4398=VECTOR('',#15870,6.767);
#4399=VECTOR('',#15873,6.767);
#4400=VECTOR('',#15876,6.767);
#4401=VECTOR('',#15879,6.767);
#4402=VECTOR('',#15882,6.767);
#4403=VECTOR('',#15885,6.767);
#4404=VECTOR('',#15888,6.767);
#4405=VECTOR('',#15891,6.767);
#4406=VECTOR('',#15894,6.767);
#4407=VECTOR('',#15897,6.767);
#4408=VECTOR('',#15900,6.767);
#4409=VECTOR('',#15903,6.767);
#4410=VECTOR('',#15906,6.767);
#4411=VECTOR('',#15909,6.767);
#4412=VECTOR('',#15912,6.767);
#4413=VECTOR('',#15915,6.767);
#4414=VECTOR('',#15918,6.767);
#4415=VECTOR('',#15921,6.767);
#4416=VECTOR('',#15924,6.767);
#4417=VECTOR('',#15927,6.767);
#4418=VECTOR('',#15930,6.767);
#4419=VECTOR('',#15933,6.767);
#4420=VECTOR('',#15936,6.767);
#4421=VECTOR('',#15939,6.767);
#4422=VECTOR('',#15942,6.767);
#4423=VECTOR('',#15945,6.767);
#4424=VECTOR('',#15948,6.767);
#4425=VECTOR('',#15951,6.767);
#4426=VECTOR('',#15954,6.767);
#4427=VECTOR('',#15957,6.767);
#4428=VECTOR('',#15960,6.767);
#4429=VECTOR('',#15963,6.767);
#4430=VECTOR('',#15966,6.767);
#4431=VECTOR('',#15969,6.767);
#4432=VECTOR('',#15972,6.767);
#4433=VECTOR('',#15975,6.767);
#4434=VECTOR('',#15978,6.767);
#4435=VECTOR('',#15981,6.767);
#4436=VECTOR('',#15984,6.767);
#4437=VECTOR('',#15987,6.767);
#4438=VECTOR('',#15990,6.767);
#4439=VECTOR('',#15993,6.767);
#4440=VECTOR('',#15996,6.767);
#4441=VECTOR('',#15999,6.767);
#4442=VECTOR('',#16002,6.767);
#4443=VECTOR('',#16005,6.767);
#4444=VECTOR('',#16008,6.767);
#4445=VECTOR('',#16011,6.767);
#4446=VECTOR('',#16014,6.767);
#4447=VECTOR('',#16017,6.767);
#4448=VECTOR('',#16020,6.767);
#4449=VECTOR('',#16023,6.767);
#4450=VECTOR('',#16038,2.);
#4451=VECTOR('',#16045,2.);
#4452=VECTOR('',#16052,2.);
#4453=VECTOR('',#16059,2.);
#4454=VECTOR('',#16078,20.);
#4455=VECTOR('',#16095,6.);
#4456=VECTOR('',#16100,6.);
#4457=VECTOR('',#16103,6.);
#4458=VECTOR('',#16106,6.);
#4459=VECTOR('',#16109,6.);
#4460=VECTOR('',#16112,6.);
#4461=VECTOR('',#16125,20.);
#4462=VECTOR('',#16126,20.);
#4463=VECTOR('',#16127,20.);
#4464=VECTOR('',#16134,20.);
#4465=VECTOR('',#16135,20.);
#4466=VECTOR('',#16136,20.);
#4467=VECTOR('',#16141,4.5);
#4468=VECTOR('',#16144,4.5);
#4469=VECTOR('',#16149,20.);
#4470=VECTOR('',#16150,20.);
#4471=VECTOR('',#16151,20.);
#4472=VECTOR('',#16152,20.);
#4473=VECTOR('',#16153,20.);
#4474=VECTOR('',#16154,20.);
#4475=VECTOR('',#16155,20.);
#4476=VECTOR('',#16156,20.);
#4477=VECTOR('',#16157,20.);
#4478=VECTOR('',#16158,20.);
#4479=VECTOR('',#16159,20.);
#4480=VECTOR('',#16160,20.);
#4481=VECTOR('',#16161,20.);
#4482=VECTOR('',#16162,20.);
#4483=VECTOR('',#16163,20.);
#4484=VECTOR('',#16164,20.);
#4485=VECTOR('',#16165,20.);
#4486=VECTOR('',#16166,20.);
#4487=VECTOR('',#16167,20.);
#4488=VECTOR('',#16168,20.);
#4489=VECTOR('',#16169,20.);
#4490=VECTOR('',#16170,20.);
#4491=VECTOR('',#16171,20.);
#4492=VECTOR('',#16172,20.);
#4493=VECTOR('',#16173,20.);
#4494=VECTOR('',#16174,20.);
#4495=VECTOR('',#16175,20.);
#4496=VECTOR('',#16176,20.);
#4497=VECTOR('',#16177,20.);
#4498=VECTOR('',#16194,23.);
#4499=VECTOR('',#16211,1.);
#4500=VECTOR('',#16216,1.);
#4501=VECTOR('',#16221,1.);
#4502=VECTOR('',#16226,1.);
#4503=VECTOR('',#16233,10.);
#4504=VECTOR('',#16242,1.);
#4505=VECTOR('',#16251,1.);
#4506=VECTOR('',#16260,1.);
#4507=VECTOR('',#16269,1.);
#4508=VECTOR('',#16278,8.5);
#4509=VECTOR('',#16285,1.);
#4510=VECTOR('',#16294,1.);
#4511=VECTOR('',#16303,1.);
#4512=VECTOR('',#16312,2.5);
#4513=VECTOR('',#16319,2.5);
#4514=VECTOR('',#16326,2.5);
#4515=VECTOR('',#16333,2.5);
#4516=VECTOR('',#16340,10.);
#4517=VECTOR('',#16343,10.);
#4518=VECTOR('',#16346,10.);
#4519=VECTOR('',#16349,10.);
#4520=VECTOR('',#16352,10.);
#4521=VECTOR('',#16353,10.);
#4522=VECTOR('',#16354,10.);
#4523=VECTOR('',#16355,10.);
#4524=VECTOR('',#16356,10.);
#4525=VECTOR('',#16361,10.);
#4526=VECTOR('',#16362,10.);
#4527=VECTOR('',#16363,10.);
#4528=VECTOR('',#16364,10.);
#4529=VECTOR('',#16365,10.);
#4530=VECTOR('',#16368,10.);
#4531=VECTOR('',#16371,10.);
#4532=VECTOR('',#16372,10.);
#4533=VECTOR('',#16377,10.);
#4534=VECTOR('',#16382,10.);
#4535=VECTOR('',#16383,10.);
#4536=VECTOR('',#16386,10.);
#4537=VECTOR('',#16387,10.);
#4538=VECTOR('',#16388,10.);
#4539=VECTOR('',#16393,10.);
#4540=VECTOR('',#16396,10.);
#4541=VECTOR('',#16399,10.);
#4542=VECTOR('',#16402,10.);
#4543=VECTOR('',#16405,10.);
#4544=VECTOR('',#16406,10.);
#4545=VECTOR('',#16411,10.);
#4546=VECTOR('',#16414,10.);
#4547=VECTOR('',#16417,10.);
#4548=VECTOR('',#16418,10.);
#4549=VECTOR('',#16421,10.);
#4550=VECTOR('',#16424,10.);
#4551=VECTOR('',#16429,10.);
#4552=VECTOR('',#16432,10.);
#4553=VECTOR('',#16443,10.);
#4554=VECTOR('',#16454,10.);
#4555=VECTOR('',#16457,10.5);
#4556=VECTOR('',#16458,10.5);
#4557=VECTOR('',#16467,20.);
#4558=VECTOR('',#16476,23.);
#4559=VECTOR('',#16487,1.);
#4560=VECTOR('',#16494,1.);
#4561=VECTOR('',#16501,1.);
#4562=VECTOR('',#16518,13.5);
#4563=VECTOR('',#16525,5.5);
#4564=VECTOR('',#16544,4.5);
#4565=VECTOR('',#16553,4.5);
#4566=VECTOR('',#16558,4.75208333333333);
#4567=VECTOR('',#16577,6.24166666666667);
#4568=VECTOR('',#16580,6.24166666666667);
#4569=VECTOR('',#16607,6.46166666666667);
#4570=VECTOR('',#16620,8.9);
#4571=VECTOR('',#16627,8.9);
#4572=VECTOR('',#16638,8.9);
#4573=VECTOR('',#16645,6.46166666666667);
#4574=VECTOR('',#16656,8.79);
#4575=VECTOR('',#16667,9.01847925309041);
#4576=VECTOR('',#16672,9.16847925309041);
#4577=VECTOR('',#16679,10.);
#4578=VECTOR('',#16686,10.);
#4579=VECTOR('',#16691,9.82679491924311);
#4580=VECTOR('',#16698,9.0184792530904);
#4581=VECTOR('',#16705,8.9);
#4582=VECTOR('',#16710,8.9);
#4583=VECTOR('',#16721,8.9);
#4584=VECTOR('',#16762,6.24166666666667);
#4585=VECTOR('',#16773,6.40666666666667);
#4586=VECTOR('',#16788,6.46166666666667);
#4587=VECTOR('',#16793,6.46166666666667);
#4588=VECTOR('',#16822,15.4);
#4589=VECTOR('',#16827,20.);
#4590=VECTOR('',#16838,12.7058184384753);
#4591=VECTOR('',#16849,16.6071946160828);
#4592=VECTOR('',#16870,13.3064408708579);
#4593=VECTOR('',#16873,12.4591576910941);
#4594=VECTOR('',#16876,13.0685506725942);
#4595=VECTOR('',#16881,13.0685506725942);
#4596=VECTOR('',#16928,17.5762965073726);
#4597=VECTOR('',#16933,17.5762965073726);
#4598=VECTOR('',#17176,10.6410293263727);
#4599=VECTOR('',#17185,12.6998790237181);
#4600=VECTOR('',#17190,14.0317131491268);
#4601=VECTOR('',#17195,14.0317131491268);
#4602=VECTOR('',#17200,8.5);
#4603=VECTOR('',#17205,11.9728634517814);
#4604=VECTOR('',#17214,2.62159462638384);
#4605=VECTOR('',#17225,2.62159462638384);
#4606=VECTOR('',#17236,2.62159462638384);
#4607=VECTOR('',#17247,2.62159462638384);
#4608=VECTOR('',#17258,2.62159462638384);
#4609=VECTOR('',#17269,2.62159462638384);
#4610=VECTOR('',#17280,2.62159462638384);
#4611=VECTOR('',#17291,2.62159462638384);
#4612=VECTOR('',#17302,2.62159462638384);
#4613=VECTOR('',#17313,2.62159462638384);
#4614=VECTOR('',#17324,2.62159462638384);
#4615=VERTEX_POINT('',#17356);
#4616=VERTEX_POINT('',#17357);
#4617=VERTEX_POINT('',#17359);
#4618=VERTEX_POINT('',#17368);
#4619=VERTEX_POINT('',#17380);
#4620=VERTEX_POINT('',#17381);
#4621=VERTEX_POINT('',#17383);
#4622=VERTEX_POINT('',#17567);
#4623=VERTEX_POINT('',#17750);
#4624=VERTEX_POINT('',#17751);
#4625=VERTEX_POINT('',#17753);
#4626=VERTEX_POINT('',#17860);
#4627=VERTEX_POINT('',#18128);
#4628=VERTEX_POINT('',#18129);
#4629=VERTEX_POINT('',#18131);
#4630=VERTEX_POINT('',#18313);
#4631=VERTEX_POINT('',#18584);
#4632=VERTEX_POINT('',#18585);
#4633=VERTEX_POINT('',#18587);
#4634=VERTEX_POINT('',#18857);
#4635=VERTEX_POINT('',#18968);
#4636=VERTEX_POINT('',#18969);
#4637=VERTEX_POINT('',#18971);
#4638=VERTEX_POINT('',#19238);
#4639=VERTEX_POINT('',#19420);
#4640=VERTEX_POINT('',#19421);
#4641=VERTEX_POINT('',#19423);
#4642=VERTEX_POINT('',#19533);
#4643=VERTEX_POINT('',#19804);
#4644=VERTEX_POINT('',#19805);
#4645=VERTEX_POINT('',#19807);
#4646=VERTEX_POINT('',#19991);
#4647=VERTEX_POINT('',#20102);
#4648=VERTEX_POINT('',#20103);
#4649=VERTEX_POINT('',#20105);
#4650=VERTEX_POINT('',#20212);
#4651=VERTEX_POINT('',#20394);
#4652=VERTEX_POINT('',#20395);
#4653=VERTEX_POINT('',#20397);
#4654=VERTEX_POINT('',#20579);
#4655=VERTEX_POINT('',#20690);
#4656=VERTEX_POINT('',#20691);
#4657=VERTEX_POINT('',#20693);
#4658=VERTEX_POINT('',#20801);
#4659=VERTEX_POINT('',#20987);
#4660=VERTEX_POINT('',#20988);
#4661=VERTEX_POINT('',#20990);
#4662=VERTEX_POINT('',#21000);
#4663=VERTEX_POINT('',#21007);
#4664=VERTEX_POINT('',#21009);
#4665=VERTEX_POINT('',#21184);
#4666=VERTEX_POINT('',#21185);
#4667=VERTEX_POINT('',#21187);
#4668=VERTEX_POINT('',#21196);
#4669=VERTEX_POINT('',#21287);
#4670=VERTEX_POINT('',#21288);
#4671=VERTEX_POINT('',#21444);
#4672=VERTEX_POINT('',#21479);
#4673=VERTEX_POINT('',#21480);
#4674=VERTEX_POINT('',#21482);
#4675=VERTEX_POINT('',#21511);
#4676=VERTEX_POINT('',#21771);
#4677=VERTEX_POINT('',#21772);
#4678=VERTEX_POINT('',#21774);
#4679=VERTEX_POINT('',#22032);
#4680=VERTEX_POINT('',#22066);
#4681=VERTEX_POINT('',#22067);
#4682=VERTEX_POINT('',#22069);
#4683=VERTEX_POINT('',#22102);
#4684=VERTEX_POINT('',#22361);
#4685=VERTEX_POINT('',#22362);
#4686=VERTEX_POINT('',#22364);
#4687=VERTEX_POINT('',#22623);
#4688=VERTEX_POINT('',#22657);
#4689=VERTEX_POINT('',#22658);
#4690=VERTEX_POINT('',#22660);
#4691=VERTEX_POINT('',#22813);
#4692=VERTEX_POINT('',#23073);
#4693=VERTEX_POINT('',#23074);
#4694=VERTEX_POINT('',#23228);
#4695=VERTEX_POINT('',#23262);
#4696=VERTEX_POINT('',#23263);
#4697=VERTEX_POINT('',#23265);
#4698=VERTEX_POINT('',#23531);
#4699=VERTEX_POINT('',#23676);
#4700=VERTEX_POINT('',#23677);
#4701=VERTEX_POINT('',#23679);
#4702=VERTEX_POINT('',#23977);
#4703=VERTEX_POINT('',#23978);
#4704=VERTEX_POINT('',#24128);
#4705=VERTEX_POINT('',#24391);
#4706=VERTEX_POINT('',#24392);
#4707=VERTEX_POINT('',#24394);
#4708=VERTEX_POINT('',#24400);
#4709=VERTEX_POINT('',#24561);
#4710=VERTEX_POINT('',#24702);
#4711=VERTEX_POINT('',#24847);
#4712=VERTEX_POINT('',#24881);
#4713=VERTEX_POINT('',#25062);
#4714=VERTEX_POINT('',#26774);
#4715=VERTEX_POINT('',#26895);
#4716=VERTEX_POINT('',#26896);
#4717=VERTEX_POINT('',#26898);
#4718=VERTEX_POINT('',#26900);
#4719=VERTEX_POINT('',#26902);
#4720=VERTEX_POINT('',#26904);
#4721=VERTEX_POINT('',#26906);
#4722=VERTEX_POINT('',#26908);
#4723=VERTEX_POINT('',#26910);
#4724=VERTEX_POINT('',#26912);
#4725=VERTEX_POINT('',#26914);
#4726=VERTEX_POINT('',#26916);
#4727=VERTEX_POINT('',#26918);
#4728=VERTEX_POINT('',#26920);
#4729=VERTEX_POINT('',#26922);
#4730=VERTEX_POINT('',#26924);
#4731=VERTEX_POINT('',#26926);
#4732=VERTEX_POINT('',#26928);
#4733=VERTEX_POINT('',#26930);
#4734=VERTEX_POINT('',#26932);
#4735=VERTEX_POINT('',#26934);
#4736=VERTEX_POINT('',#26936);
#4737=VERTEX_POINT('',#26938);
#4738=VERTEX_POINT('',#26940);
#4739=VERTEX_POINT('',#26942);
#4740=VERTEX_POINT('',#26944);
#4741=VERTEX_POINT('',#26946);
#4742=VERTEX_POINT('',#26948);
#4743=VERTEX_POINT('',#26950);
#4744=VERTEX_POINT('',#26952);
#4745=VERTEX_POINT('',#26954);
#4746=VERTEX_POINT('',#26956);
#4747=VERTEX_POINT('',#26958);
#4748=VERTEX_POINT('',#26960);
#4749=VERTEX_POINT('',#26962);
#4750=VERTEX_POINT('',#26964);
#4751=VERTEX_POINT('',#26966);
#4752=VERTEX_POINT('',#26968);
#4753=VERTEX_POINT('',#26970);
#4754=VERTEX_POINT('',#26972);
#4755=VERTEX_POINT('',#26974);
#4756=VERTEX_POINT('',#26976);
#4757=VERTEX_POINT('',#26978);
#4758=VERTEX_POINT('',#26980);
#4759=VERTEX_POINT('',#26982);
#4760=VERTEX_POINT('',#26984);
#4761=VERTEX_POINT('',#26986);
#4762=VERTEX_POINT('',#26988);
#4763=VERTEX_POINT('',#26990);
#4764=VERTEX_POINT('',#26992);
#4765=VERTEX_POINT('',#26994);
#4766=VERTEX_POINT('',#26996);
#4767=VERTEX_POINT('',#26998);
#4768=VERTEX_POINT('',#27000);
#4769=VERTEX_POINT('',#27002);
#4770=VERTEX_POINT('',#27004);
#4771=VERTEX_POINT('',#27006);
#4772=VERTEX_POINT('',#27008);
#4773=VERTEX_POINT('',#27010);
#4774=VERTEX_POINT('',#27012);
#4775=VERTEX_POINT('',#27014);
#4776=VERTEX_POINT('',#27016);
#4777=VERTEX_POINT('',#27018);
#4778=VERTEX_POINT('',#27020);
#4779=VERTEX_POINT('',#27022);
#4780=VERTEX_POINT('',#27024);
#4781=VERTEX_POINT('',#27026);
#4782=VERTEX_POINT('',#27028);
#4783=VERTEX_POINT('',#27030);
#4784=VERTEX_POINT('',#27032);
#4785=VERTEX_POINT('',#27034);
#4786=VERTEX_POINT('',#27036);
#4787=VERTEX_POINT('',#27040);
#4788=VERTEX_POINT('',#27041);
#4789=VERTEX_POINT('',#27043);
#4790=VERTEX_POINT('',#27045);
#4791=VERTEX_POINT('',#27049);
#4792=VERTEX_POINT('',#27050);
#4793=VERTEX_POINT('',#27052);
#4794=VERTEX_POINT('',#27054);
#4795=VERTEX_POINT('',#27058);
#4796=VERTEX_POINT('',#27059);
#4797=VERTEX_POINT('',#27061);
#4798=VERTEX_POINT('',#27063);
#4799=VERTEX_POINT('',#27067);
#4800=VERTEX_POINT('',#27068);
#4801=VERTEX_POINT('',#27070);
#4802=VERTEX_POINT('',#27072);
#4803=VERTEX_POINT('',#27076);
#4804=VERTEX_POINT('',#27077);
#4805=VERTEX_POINT('',#27079);
#4806=VERTEX_POINT('',#27081);
#4807=VERTEX_POINT('',#27085);
#4808=VERTEX_POINT('',#27086);
#4809=VERTEX_POINT('',#27088);
#4810=VERTEX_POINT('',#27090);
#4811=VERTEX_POINT('',#27094);
#4812=VERTEX_POINT('',#27095);
#4813=VERTEX_POINT('',#27097);
#4814=VERTEX_POINT('',#27099);
#4815=VERTEX_POINT('',#27103);
#4816=VERTEX_POINT('',#27104);
#4817=VERTEX_POINT('',#27106);
#4818=VERTEX_POINT('',#27108);
#4819=VERTEX_POINT('',#27112);
#4820=VERTEX_POINT('',#27113);
#4821=VERTEX_POINT('',#27115);
#4822=VERTEX_POINT('',#27117);
#4823=VERTEX_POINT('',#27121);
#4824=VERTEX_POINT('',#27122);
#4825=VERTEX_POINT('',#27124);
#4826=VERTEX_POINT('',#27126);
#4827=VERTEX_POINT('',#27130);
#4828=VERTEX_POINT('',#27131);
#4829=VERTEX_POINT('',#27133);
#4830=VERTEX_POINT('',#27135);
#4831=VERTEX_POINT('',#27139);
#4832=VERTEX_POINT('',#27140);
#4833=VERTEX_POINT('',#27142);
#4834=VERTEX_POINT('',#27144);
#4835=VERTEX_POINT('',#27148);
#4836=VERTEX_POINT('',#27149);
#4837=VERTEX_POINT('',#27151);
#4838=VERTEX_POINT('',#27153);
#4839=VERTEX_POINT('',#27157);
#4840=VERTEX_POINT('',#27158);
#4841=VERTEX_POINT('',#27160);
#4842=VERTEX_POINT('',#27162);
#4843=VERTEX_POINT('',#27166);
#4844=VERTEX_POINT('',#27167);
#4845=VERTEX_POINT('',#27169);
#4846=VERTEX_POINT('',#27171);
#4847=VERTEX_POINT('',#27175);
#4848=VERTEX_POINT('',#27176);
#4849=VERTEX_POINT('',#27178);
#4850=VERTEX_POINT('',#27180);
#4851=VERTEX_POINT('',#27184);
#4852=VERTEX_POINT('',#27185);
#4853=VERTEX_POINT('',#27187);
#4854=VERTEX_POINT('',#27189);
#4855=VERTEX_POINT('',#27193);
#4856=VERTEX_POINT('',#27194);
#4857=VERTEX_POINT('',#27196);
#4858=VERTEX_POINT('',#27198);
#4859=VERTEX_POINT('',#27202);
#4860=VERTEX_POINT('',#27204);
#4861=VERTEX_POINT('',#27206);
#4862=VERTEX_POINT('',#27216);
#4863=VERTEX_POINT('',#27229);
#4864=VERTEX_POINT('',#27231);
#4865=VERTEX_POINT('',#27233);
#4866=VERTEX_POINT('',#27243);
#4867=VERTEX_POINT('',#27256);
#4868=VERTEX_POINT('',#27258);
#4869=VERTEX_POINT('',#27260);
#4870=VERTEX_POINT('',#27270);
#4871=VERTEX_POINT('',#27281);
#4872=VERTEX_POINT('',#27283);
#4873=VERTEX_POINT('',#27285);
#4874=VERTEX_POINT('',#27295);
#4875=VERTEX_POINT('',#27308);
#4876=VERTEX_POINT('',#27310);
#4877=VERTEX_POINT('',#27312);
#4878=VERTEX_POINT('',#27322);
#4879=VERTEX_POINT('',#27335);
#4880=VERTEX_POINT('',#27337);
#4881=VERTEX_POINT('',#27339);
#4882=VERTEX_POINT('',#27349);
#4883=VERTEX_POINT('',#27362);
#4884=VERTEX_POINT('',#27364);
#4885=VERTEX_POINT('',#27366);
#4886=VERTEX_POINT('',#27376);
#4887=VERTEX_POINT('',#27387);
#4888=VERTEX_POINT('',#27389);
#4889=VERTEX_POINT('',#27391);
#4890=VERTEX_POINT('',#27401);
#4891=VERTEX_POINT('',#27414);
#4892=VERTEX_POINT('',#27416);
#4893=VERTEX_POINT('',#27418);
#4894=VERTEX_POINT('',#27428);
#4895=VERTEX_POINT('',#27441);
#4896=VERTEX_POINT('',#27443);
#4897=VERTEX_POINT('',#27445);
#4898=VERTEX_POINT('',#27455);
#4899=VERTEX_POINT('',#27468);
#4900=VERTEX_POINT('',#27470);
#4901=VERTEX_POINT('',#27472);
#4902=VERTEX_POINT('',#27482);
#4903=VERTEX_POINT('',#27493);
#4904=VERTEX_POINT('',#27495);
#4905=VERTEX_POINT('',#27497);
#4906=VERTEX_POINT('',#27507);
#4907=VERTEX_POINT('',#27520);
#4908=VERTEX_POINT('',#27522);
#4909=VERTEX_POINT('',#27524);
#4910=VERTEX_POINT('',#27534);
#4911=VERTEX_POINT('',#27547);
#4912=VERTEX_POINT('',#27549);
#4913=VERTEX_POINT('',#27551);
#4914=VERTEX_POINT('',#27561);
#4915=VERTEX_POINT('',#27574);
#4916=VERTEX_POINT('',#27576);
#4917=VERTEX_POINT('',#27578);
#4918=VERTEX_POINT('',#27588);
#4919=VERTEX_POINT('',#27601);
#4920=VERTEX_POINT('',#27603);
#4921=VERTEX_POINT('',#27605);
#4922=VERTEX_POINT('',#27615);
#4923=VERTEX_POINT('',#27628);
#4924=VERTEX_POINT('',#27630);
#4925=VERTEX_POINT('',#27632);
#4926=VERTEX_POINT('',#27642);
#4927=VERTEX_POINT('',#27655);
#4928=VERTEX_POINT('',#27657);
#4929=VERTEX_POINT('',#27659);
#4930=VERTEX_POINT('',#27669);
#4931=VERTEX_POINT('',#27682);
#4932=VERTEX_POINT('',#27683);
#4933=VERTEX_POINT('',#27685);
#4934=VERTEX_POINT('',#27687);
#4935=VERTEX_POINT('',#27689);
#4936=VERTEX_POINT('',#27691);
#4937=VERTEX_POINT('',#27700);
#4938=VERTEX_POINT('',#27702);
#4939=VERTEX_POINT('',#27715);
#4940=VERTEX_POINT('',#27716);
#4941=VERTEX_POINT('',#27718);
#4942=VERTEX_POINT('',#27720);
#4943=VERTEX_POINT('',#27722);
#4944=VERTEX_POINT('',#27724);
#4945=VERTEX_POINT('',#27735);
#4946=VERTEX_POINT('',#27737);
#4947=VERTEX_POINT('',#27748);
#4948=VERTEX_POINT('',#27749);
#4949=VERTEX_POINT('',#27751);
#4950=VERTEX_POINT('',#27753);
#4951=VERTEX_POINT('',#27755);
#4952=VERTEX_POINT('',#27757);
#4953=VERTEX_POINT('',#27768);
#4954=VERTEX_POINT('',#27770);
#4955=VERTEX_POINT('',#27783);
#4956=VERTEX_POINT('',#27784);
#4957=VERTEX_POINT('',#27786);
#4958=VERTEX_POINT('',#27788);
#4959=VERTEX_POINT('',#27790);
#4960=VERTEX_POINT('',#27792);
#4961=VERTEX_POINT('',#27801);
#4962=VERTEX_POINT('',#27803);
#4963=VERTEX_POINT('',#27814);
#4964=VERTEX_POINT('',#27815);
#4965=VERTEX_POINT('',#27817);
#4966=VERTEX_POINT('',#27819);
#4967=VERTEX_POINT('',#27821);
#4968=VERTEX_POINT('',#27823);
#4969=VERTEX_POINT('',#27834);
#4970=VERTEX_POINT('',#27836);
#4971=VERTEX_POINT('',#27849);
#4972=VERTEX_POINT('',#27850);
#4973=VERTEX_POINT('',#27852);
#4974=VERTEX_POINT('',#27854);
#4975=VERTEX_POINT('',#27856);
#4976=VERTEX_POINT('',#27858);
#4977=VERTEX_POINT('',#27869);
#4978=VERTEX_POINT('',#27871);
#4979=VERTEX_POINT('',#27884);
#4980=VERTEX_POINT('',#27885);
#4981=VERTEX_POINT('',#27887);
#4982=VERTEX_POINT('',#27889);
#4983=VERTEX_POINT('',#27891);
#4984=VERTEX_POINT('',#27893);
#4985=VERTEX_POINT('',#27904);
#4986=VERTEX_POINT('',#27906);
#4987=VERTEX_POINT('',#27917);
#4988=VERTEX_POINT('',#27918);
#4989=VERTEX_POINT('',#27920);
#4990=VERTEX_POINT('',#27922);
#4991=VERTEX_POINT('',#27924);
#4992=VERTEX_POINT('',#27926);
#4993=VERTEX_POINT('',#27935);
#4994=VERTEX_POINT('',#27937);
#4995=VERTEX_POINT('',#27950);
#4996=VERTEX_POINT('',#27951);
#4997=VERTEX_POINT('',#27953);
#4998=VERTEX_POINT('',#27955);
#4999=VERTEX_POINT('',#27957);
#5000=VERTEX_POINT('',#27959);
#5001=VERTEX_POINT('',#27970);
#5002=VERTEX_POINT('',#27972);
#5003=VERTEX_POINT('',#27985);
#5004=VERTEX_POINT('',#27986);
#5005=VERTEX_POINT('',#27988);
#5006=VERTEX_POINT('',#27990);
#5007=VERTEX_POINT('',#27992);
#5008=VERTEX_POINT('',#27994);
#5009=VERTEX_POINT('',#28005);
#5010=VERTEX_POINT('',#28007);
#5011=VERTEX_POINT('',#28020);
#5012=VERTEX_POINT('',#28021);
#5013=VERTEX_POINT('',#28023);
#5014=VERTEX_POINT('',#28025);
#5015=VERTEX_POINT('',#28027);
#5016=VERTEX_POINT('',#28029);
#5017=VERTEX_POINT('',#28040);
#5018=VERTEX_POINT('',#28042);
#5019=VERTEX_POINT('',#28053);
#5020=VERTEX_POINT('',#28054);
#5021=VERTEX_POINT('',#28056);
#5022=VERTEX_POINT('',#28058);
#5023=VERTEX_POINT('',#28060);
#5024=VERTEX_POINT('',#28062);
#5025=VERTEX_POINT('',#28071);
#5026=VERTEX_POINT('',#28073);
#5027=VERTEX_POINT('',#28086);
#5028=VERTEX_POINT('',#28087);
#5029=VERTEX_POINT('',#28089);
#5030=VERTEX_POINT('',#28091);
#5031=VERTEX_POINT('',#28093);
#5032=VERTEX_POINT('',#28095);
#5033=VERTEX_POINT('',#28106);
#5034=VERTEX_POINT('',#28108);
#5035=VERTEX_POINT('',#28119);
#5036=VERTEX_POINT('',#28120);
#5037=VERTEX_POINT('',#28122);
#5038=VERTEX_POINT('',#28124);
#5039=VERTEX_POINT('',#28126);
#5040=VERTEX_POINT('',#28128);
#5041=VERTEX_POINT('',#28139);
#5042=VERTEX_POINT('',#28141);
#5043=VERTEX_POINT('',#28154);
#5044=VERTEX_POINT('',#28155);
#5045=VERTEX_POINT('',#28157);
#5046=VERTEX_POINT('',#28159);
#5047=VERTEX_POINT('',#28161);
#5048=VERTEX_POINT('',#28163);
#5049=VERTEX_POINT('',#28174);
#5050=VERTEX_POINT('',#28176);
#5051=VERTEX_POINT('',#28189);
#5052=VERTEX_POINT('',#28190);
#5053=VERTEX_POINT('',#28192);
#5054=VERTEX_POINT('',#28194);
#5055=VERTEX_POINT('',#28196);
#5056=VERTEX_POINT('',#28198);
#5057=VERTEX_POINT('',#28209);
#5058=VERTEX_POINT('',#28211);
#5059=VERTEX_POINT('',#28222);
#5060=VERTEX_POINT('',#28223);
#5061=VERTEX_POINT('',#28225);
#5062=VERTEX_POINT('',#28227);
#5063=VERTEX_POINT('',#28229);
#5064=VERTEX_POINT('',#28231);
#5065=VERTEX_POINT('',#28240);
#5066=VERTEX_POINT('',#28242);
#5067=VERTEX_POINT('',#28255);
#5068=VERTEX_POINT('',#28256);
#5069=VERTEX_POINT('',#28258);
#5070=VERTEX_POINT('',#28260);
#5071=VERTEX_POINT('',#28262);
#5072=VERTEX_POINT('',#28264);
#5073=VERTEX_POINT('',#28273);
#5074=VERTEX_POINT('',#28275);
#5075=VERTEX_POINT('',#28286);
#5076=VERTEX_POINT('',#28288);
#5077=VERTEX_POINT('',#28292);
#5078=VERTEX_POINT('',#28294);
#5079=VERTEX_POINT('',#28298);
#5080=VERTEX_POINT('',#28300);
#5081=VERTEX_POINT('',#28304);
#5082=VERTEX_POINT('',#28306);
#5083=VERTEX_POINT('',#28310);
#5084=VERTEX_POINT('',#28312);
#5085=VERTEX_POINT('',#28316);
#5086=VERTEX_POINT('',#28318);
#5087=VERTEX_POINT('',#28322);
#5088=VERTEX_POINT('',#28324);
#5089=VERTEX_POINT('',#28328);
#5090=VERTEX_POINT('',#28330);
#5091=VERTEX_POINT('',#28334);
#5092=VERTEX_POINT('',#28336);
#5093=VERTEX_POINT('',#28340);
#5094=VERTEX_POINT('',#28342);
#5095=VERTEX_POINT('',#28346);
#5096=VERTEX_POINT('',#28348);
#5097=VERTEX_POINT('',#28352);
#5098=VERTEX_POINT('',#28354);
#5099=VERTEX_POINT('',#28358);
#5100=VERTEX_POINT('',#28360);
#5101=VERTEX_POINT('',#28364);
#5102=VERTEX_POINT('',#28366);
#5103=VERTEX_POINT('',#28370);
#5104=VERTEX_POINT('',#28372);
#5105=VERTEX_POINT('',#28376);
#5106=VERTEX_POINT('',#28378);
#5107=VERTEX_POINT('',#28382);
#5108=VERTEX_POINT('',#28384);
#5109=VERTEX_POINT('',#28388);
#5110=VERTEX_POINT('',#28390);
#5111=VERTEX_POINT('',#28394);
#5112=VERTEX_POINT('',#28395);
#5113=VERTEX_POINT('',#28397);
#5114=VERTEX_POINT('',#28399);
#5115=VERTEX_POINT('',#28408);
#5116=VERTEX_POINT('',#28409);
#5117=VERTEX_POINT('',#28411);
#5118=VERTEX_POINT('',#28413);
#5119=VERTEX_POINT('',#28417);
#5120=VERTEX_POINT('',#28418);
#5121=VERTEX_POINT('',#28420);
#5122=VERTEX_POINT('',#28422);
#5123=VERTEX_POINT('',#28426);
#5124=VERTEX_POINT('',#28427);
#5125=VERTEX_POINT('',#28429);
#5126=VERTEX_POINT('',#28431);
#5127=VERTEX_POINT('',#28440);
#5128=VERTEX_POINT('',#28441);
#5129=VERTEX_POINT('',#28443);
#5130=VERTEX_POINT('',#28445);
#5131=VERTEX_POINT('',#28449);
#5132=VERTEX_POINT('',#28450);
#5133=VERTEX_POINT('',#28452);
#5134=VERTEX_POINT('',#28454);
#5135=VERTEX_POINT('',#28458);
#5136=VERTEX_POINT('',#28459);
#5137=VERTEX_POINT('',#28461);
#5138=VERTEX_POINT('',#28463);
#5139=VERTEX_POINT('',#28467);
#5140=VERTEX_POINT('',#28468);
#5141=VERTEX_POINT('',#28470);
#5142=VERTEX_POINT('',#28472);
#5143=VERTEX_POINT('',#28481);
#5144=VERTEX_POINT('',#28482);
#5145=VERTEX_POINT('',#28484);
#5146=VERTEX_POINT('',#28486);
#5147=VERTEX_POINT('',#28490);
#5148=VERTEX_POINT('',#28491);
#5149=VERTEX_POINT('',#28493);
#5150=VERTEX_POINT('',#28495);
#5151=VERTEX_POINT('',#28499);
#5152=VERTEX_POINT('',#28500);
#5153=VERTEX_POINT('',#28502);
#5154=VERTEX_POINT('',#28504);
#5155=VERTEX_POINT('',#28508);
#5156=VERTEX_POINT('',#28509);
#5157=VERTEX_POINT('',#28511);
#5158=VERTEX_POINT('',#28513);
#5159=VERTEX_POINT('',#28522);
#5160=VERTEX_POINT('',#28523);
#5161=VERTEX_POINT('',#28525);
#5162=VERTEX_POINT('',#28527);
#5163=VERTEX_POINT('',#28531);
#5164=VERTEX_POINT('',#28532);
#5165=VERTEX_POINT('',#28534);
#5166=VERTEX_POINT('',#28536);
#5167=VERTEX_POINT('',#28540);
#5168=VERTEX_POINT('',#28541);
#5169=VERTEX_POINT('',#28543);
#5170=VERTEX_POINT('',#28545);
#5171=VERTEX_POINT('',#28549);
#5172=VERTEX_POINT('',#28550);
#5173=VERTEX_POINT('',#28552);
#5174=VERTEX_POINT('',#28554);
#5175=VERTEX_POINT('',#28558);
#5176=VERTEX_POINT('',#28559);
#5177=VERTEX_POINT('',#28561);
#5178=VERTEX_POINT('',#28563);
#5179=VERTEX_POINT('',#28572);
#5180=VERTEX_POINT('',#28573);
#5181=VERTEX_POINT('',#28575);
#5182=VERTEX_POINT('',#28577);
#5183=VERTEX_POINT('',#28586);
#5184=VERTEX_POINT('',#28587);
#5185=VERTEX_POINT('',#28594);
#5186=VERTEX_POINT('',#28596);
#5187=VERTEX_POINT('',#28600);
#5188=VERTEX_POINT('',#28601);
#5189=VERTEX_POINT('',#28608);
#5190=VERTEX_POINT('',#28610);
#5191=VERTEX_POINT('',#28614);
#5192=VERTEX_POINT('',#28615);
#5193=VERTEX_POINT('',#28622);
#5194=VERTEX_POINT('',#28624);
#5195=VERTEX_POINT('',#28628);
#5196=VERTEX_POINT('',#28629);
#5197=VERTEX_POINT('',#28636);
#5198=VERTEX_POINT('',#28638);
#5199=VERTEX_POINT('',#28642);
#5200=VERTEX_POINT('',#28643);
#5201=VERTEX_POINT('',#28650);
#5202=VERTEX_POINT('',#28652);
#5203=VERTEX_POINT('',#28656);
#5204=VERTEX_POINT('',#28657);
#5205=VERTEX_POINT('',#28664);
#5206=VERTEX_POINT('',#28666);
#5207=VERTEX_POINT('',#28670);
#5208=VERTEX_POINT('',#28671);
#5209=VERTEX_POINT('',#28678);
#5210=VERTEX_POINT('',#28680);
#5211=VERTEX_POINT('',#28684);
#5212=VERTEX_POINT('',#28685);
#5213=VERTEX_POINT('',#28692);
#5214=VERTEX_POINT('',#28694);
#5215=VERTEX_POINT('',#28698);
#5216=VERTEX_POINT('',#28699);
#5217=VERTEX_POINT('',#28706);
#5218=VERTEX_POINT('',#28708);
#5219=VERTEX_POINT('',#28712);
#5220=VERTEX_POINT('',#28713);
#5221=VERTEX_POINT('',#28720);
#5222=VERTEX_POINT('',#28722);
#5223=VERTEX_POINT('',#28726);
#5224=VERTEX_POINT('',#28727);
#5225=VERTEX_POINT('',#28734);
#5226=VERTEX_POINT('',#28736);
#5227=VERTEX_POINT('',#28740);
#5228=VERTEX_POINT('',#28741);
#5229=VERTEX_POINT('',#28748);
#5230=VERTEX_POINT('',#28750);
#5231=VERTEX_POINT('',#28754);
#5232=VERTEX_POINT('',#28755);
#5233=VERTEX_POINT('',#28762);
#5234=VERTEX_POINT('',#28764);
#5235=VERTEX_POINT('',#28768);
#5236=VERTEX_POINT('',#28769);
#5237=VERTEX_POINT('',#28776);
#5238=VERTEX_POINT('',#28778);
#5239=VERTEX_POINT('',#28782);
#5240=VERTEX_POINT('',#28783);
#5241=VERTEX_POINT('',#28790);
#5242=VERTEX_POINT('',#28792);
#5243=VERTEX_POINT('',#28796);
#5244=VERTEX_POINT('',#28797);
#5245=VERTEX_POINT('',#28804);
#5246=VERTEX_POINT('',#28806);
#5247=VERTEX_POINT('',#28810);
#5248=VERTEX_POINT('',#28811);
#5249=VERTEX_POINT('',#28818);
#5250=VERTEX_POINT('',#28820);
#5251=VERTEX_POINT('',#28824);
#5252=VERTEX_POINT('',#28825);
#5253=VERTEX_POINT('',#28832);
#5254=VERTEX_POINT('',#28834);
#5255=VERTEX_POINT('',#31479);
#5256=VERTEX_POINT('',#31530);
#5257=VERTEX_POINT('',#31546);
#5258=VERTEX_POINT('',#31562);
#5259=VERTEX_POINT('',#31593);
#5260=VERTEX_POINT('',#31661);
#5261=VERTEX_POINT('',#31692);
#5262=VERTEX_POINT('',#31729);
#5263=VERTEX_POINT('',#31732);
#5264=VERTEX_POINT('',#31734);
#5265=VERTEX_POINT('',#31737);
#5266=VERTEX_POINT('',#31739);
#5267=VERTEX_POINT('',#31742);
#5268=VERTEX_POINT('',#31744);
#5269=VERTEX_POINT('',#31747);
#5270=VERTEX_POINT('',#31749);
#5271=VERTEX_POINT('',#31752);
#5272=VERTEX_POINT('',#31754);
#5273=VERTEX_POINT('',#31757);
#5274=VERTEX_POINT('',#31759);
#5275=VERTEX_POINT('',#31762);
#5276=VERTEX_POINT('',#31764);
#5277=VERTEX_POINT('',#31767);
#5278=VERTEX_POINT('',#31769);
#5279=VERTEX_POINT('',#31772);
#5280=VERTEX_POINT('',#31774);
#5281=VERTEX_POINT('',#31777);
#5282=VERTEX_POINT('',#31779);
#5283=VERTEX_POINT('',#31782);
#5284=VERTEX_POINT('',#31784);
#5285=VERTEX_POINT('',#31787);
#5286=VERTEX_POINT('',#31789);
#5287=VERTEX_POINT('',#31792);
#5288=VERTEX_POINT('',#31794);
#5289=VERTEX_POINT('',#31797);
#5290=VERTEX_POINT('',#31799);
#5291=VERTEX_POINT('',#32978);
#5292=VERTEX_POINT('',#32980);
#5293=VERTEX_POINT('',#32984);
#5294=VERTEX_POINT('',#32986);
#5295=VERTEX_POINT('',#32990);
#5296=VERTEX_POINT('',#32992);
#5297=VERTEX_POINT('',#32996);
#5298=VERTEX_POINT('',#32998);
#5299=VERTEX_POINT('',#33000);
#5300=VERTEX_POINT('',#33004);
#5301=VERTEX_POINT('',#33008);
#5302=VERTEX_POINT('',#33011);
#5303=VERTEX_POINT('',#33017);
#5304=VERTEX_POINT('',#33018);
#5305=VERTEX_POINT('',#33020);
#5306=VERTEX_POINT('',#33154);
#5307=VERTEX_POINT('',#33239);
#5308=VERTEX_POINT('',#33240);
#5309=VERTEX_POINT('',#33242);
#5310=VERTEX_POINT('',#33482);
#5311=VERTEX_POINT('',#33738);
#5312=VERTEX_POINT('',#33739);
#5313=VERTEX_POINT('',#33741);
#5314=VERTEX_POINT('',#33987);
#5315=VERTEX_POINT('',#34234);
#5316=VERTEX_POINT('',#34235);
#5317=VERTEX_POINT('',#34237);
#5318=VERTEX_POINT('',#34492);
#5319=VERTEX_POINT('',#34742);
#5320=VERTEX_POINT('',#34743);
#5321=VERTEX_POINT('',#34745);
#5322=VERTEX_POINT('',#34997);
#5323=VERTEX_POINT('',#35250);
#5324=VERTEX_POINT('',#35251);
#5325=VERTEX_POINT('',#35253);
#5326=VERTEX_POINT('',#35505);
#5327=VERTEX_POINT('',#35746);
#5328=VERTEX_POINT('',#35747);
#5329=VERTEX_POINT('',#35749);
#5330=VERTEX_POINT('',#36004);
#5331=VERTEX_POINT('',#36248);
#5332=VERTEX_POINT('',#36249);
#5333=VERTEX_POINT('',#36251);
#5334=VERTEX_POINT('',#36503);
#5335=VERTEX_POINT('',#36744);
#5336=VERTEX_POINT('',#36745);
#5337=VERTEX_POINT('',#36747);
#5338=VERTEX_POINT('',#36996);
#5339=VERTEX_POINT('',#37231);
#5340=VERTEX_POINT('',#37232);
#5341=VERTEX_POINT('',#37234);
#5342=VERTEX_POINT('',#37483);
#5343=VERTEX_POINT('',#37730);
#5344=VERTEX_POINT('',#37731);
#5345=VERTEX_POINT('',#37733);
#5346=VERTEX_POINT('',#37988);
#5347=VERTEX_POINT('',#38238);
#5348=VERTEX_POINT('',#38239);
#5349=VERTEX_POINT('',#38241);
#5350=VERTEX_POINT('',#38478);
#5351=VERTEX_POINT('',#38731);
#5352=VERTEX_POINT('',#38732);
#5353=VERTEX_POINT('',#38734);
#5354=VERTEX_POINT('',#38980);
#5355=VERTEX_POINT('',#39227);
#5356=VERTEX_POINT('',#39228);
#5357=VERTEX_POINT('',#39230);
#5358=VERTEX_POINT('',#39485);
#5359=VERTEX_POINT('',#39735);
#5360=VERTEX_POINT('',#39736);
#5361=VERTEX_POINT('',#39738);
#5362=VERTEX_POINT('',#39990);
#5363=VERTEX_POINT('',#40243);
#5364=VERTEX_POINT('',#40244);
#5365=VERTEX_POINT('',#40246);
#5366=VERTEX_POINT('',#40498);
#5367=VERTEX_POINT('',#40742);
#5368=VERTEX_POINT('',#40743);
#5369=VERTEX_POINT('',#40745);
#5370=VERTEX_POINT('',#40994);
#5371=VERTEX_POINT('',#41238);
#5372=VERTEX_POINT('',#41239);
#5373=VERTEX_POINT('',#41241);
#5374=VERTEX_POINT('',#41490);
#5375=VERTEX_POINT('',#41731);
#5376=VERTEX_POINT('',#41732);
#5377=VERTEX_POINT('',#41734);
#5378=VERTEX_POINT('',#41983);
#5379=VERTEX_POINT('',#42218);
#5380=VERTEX_POINT('',#42219);
#5381=VERTEX_POINT('',#42221);
#5382=VERTEX_POINT('',#42473);
#5383=VERTEX_POINT('',#42720);
#5384=VERTEX_POINT('',#42721);
#5385=VERTEX_POINT('',#42723);
#5386=VERTEX_POINT('',#42975);
#5387=VERTEX_POINT('',#43228);
#5388=VERTEX_POINT('',#43229);
#5389=VERTEX_POINT('',#43231);
#5390=VERTEX_POINT('',#43468);
#5391=VERTEX_POINT('',#43721);
#5392=VERTEX_POINT('',#43722);
#5393=VERTEX_POINT('',#43724);
#5394=VERTEX_POINT('',#43970);
#5395=VERTEX_POINT('',#44223);
#5396=VERTEX_POINT('',#44224);
#5397=VERTEX_POINT('',#44226);
#5398=VERTEX_POINT('',#44481);
#5399=VERTEX_POINT('',#44731);
#5400=VERTEX_POINT('',#44732);
#5401=VERTEX_POINT('',#44734);
#5402=VERTEX_POINT('',#44983);
#5403=VERTEX_POINT('',#45236);
#5404=VERTEX_POINT('',#45237);
#5405=VERTEX_POINT('',#45239);
#5406=VERTEX_POINT('',#45488);
#5407=VERTEX_POINT('',#45732);
#5408=VERTEX_POINT('',#45733);
#5409=VERTEX_POINT('',#45735);
#5410=VERTEX_POINT('',#45984);
#5411=VERTEX_POINT('',#46228);
#5412=VERTEX_POINT('',#46229);
#5413=VERTEX_POINT('',#46231);
#5414=VERTEX_POINT('',#46480);
#5415=VERTEX_POINT('',#46721);
#5416=VERTEX_POINT('',#46722);
#5417=VERTEX_POINT('',#46724);
#5418=VERTEX_POINT('',#46970);
#5419=VERTEX_POINT('',#47205);
#5420=VERTEX_POINT('',#47206);
#5421=VERTEX_POINT('',#47208);
#5422=VERTEX_POINT('',#47460);
#5423=VERTEX_POINT('',#47707);
#5424=VERTEX_POINT('',#47708);
#5425=VERTEX_POINT('',#47710);
#5426=VERTEX_POINT('',#47962);
#5427=VERTEX_POINT('',#48215);
#5428=VERTEX_POINT('',#48216);
#5429=VERTEX_POINT('',#48218);
#5430=VERTEX_POINT('',#48470);
#5431=VERTEX_POINT('',#48720);
#5432=VERTEX_POINT('',#48721);
#5433=VERTEX_POINT('',#48723);
#5434=VERTEX_POINT('',#48972);
#5435=VERTEX_POINT('',#49213);
#5436=VERTEX_POINT('',#49214);
#5437=VERTEX_POINT('',#49216);
#5438=VERTEX_POINT('',#49468);
#5439=VERTEX_POINT('',#49712);
#5440=VERTEX_POINT('',#49713);
#5441=VERTEX_POINT('',#49715);
#5442=VERTEX_POINT('',#49955);
#5443=VERTEX_POINT('',#50196);
#5444=VERTEX_POINT('',#50197);
#5445=VERTEX_POINT('',#50199);
#5446=VERTEX_POINT('',#50442);
#5447=VERTEX_POINT('',#50677);
#5448=VERTEX_POINT('',#50678);
#5449=VERTEX_POINT('',#50680);
#5450=VERTEX_POINT('',#50932);
#5451=VERTEX_POINT('',#51179);
#5452=VERTEX_POINT('',#51180);
#5453=VERTEX_POINT('',#51182);
#5454=VERTEX_POINT('',#51428);
#5455=VERTEX_POINT('',#51681);
#5456=VERTEX_POINT('',#51682);
#5457=VERTEX_POINT('',#51684);
#5458=VERTEX_POINT('',#51939);
#5459=VERTEX_POINT('',#52186);
#5460=VERTEX_POINT('',#52187);
#5461=VERTEX_POINT('',#52189);
#5462=VERTEX_POINT('',#52429);
#5463=VERTEX_POINT('',#52673);
#5464=VERTEX_POINT('',#52674);
#5465=VERTEX_POINT('',#52676);
#5466=VERTEX_POINT('',#52922);
#5467=VERTEX_POINT('',#53166);
#5468=VERTEX_POINT('',#53167);
#5469=VERTEX_POINT('',#53169);
#5470=VERTEX_POINT('',#53421);
#5471=VERTEX_POINT('',#53677);
#5472=VERTEX_POINT('',#53678);
#5473=VERTEX_POINT('',#53680);
#5474=VERTEX_POINT('',#53929);
#5475=VERTEX_POINT('',#54170);
#5476=VERTEX_POINT('',#54171);
#5477=VERTEX_POINT('',#54173);
#5478=VERTEX_POINT('',#54425);
#5479=VERTEX_POINT('',#54669);
#5480=VERTEX_POINT('',#54670);
#5481=VERTEX_POINT('',#54672);
#5482=VERTEX_POINT('',#54912);
#5483=VERTEX_POINT('',#55153);
#5484=VERTEX_POINT('',#55154);
#5485=VERTEX_POINT('',#55156);
#5486=VERTEX_POINT('',#55399);
#5487=VERTEX_POINT('',#55634);
#5488=VERTEX_POINT('',#55635);
#5489=VERTEX_POINT('',#55637);
#5490=VERTEX_POINT('',#55889);
#5491=VERTEX_POINT('',#56133);
#5492=VERTEX_POINT('',#56134);
#5493=VERTEX_POINT('',#56136);
#5494=VERTEX_POINT('',#56385);
#5495=VERTEX_POINT('',#56638);
#5496=VERTEX_POINT('',#56639);
#5497=VERTEX_POINT('',#56641);
#5498=VERTEX_POINT('',#56884);
#5499=VERTEX_POINT('',#57134);
#5500=VERTEX_POINT('',#57135);
#5501=VERTEX_POINT('',#57137);
#5502=VERTEX_POINT('',#57383);
#5503=VERTEX_POINT('',#57627);
#5504=VERTEX_POINT('',#57628);
#5505=VERTEX_POINT('',#57630);
#5506=VERTEX_POINT('',#57879);
#5507=VERTEX_POINT('',#58123);
#5508=VERTEX_POINT('',#58124);
#5509=VERTEX_POINT('',#58126);
#5510=VERTEX_POINT('',#58375);
#5511=VERTEX_POINT('',#58631);
#5512=VERTEX_POINT('',#58632);
#5513=VERTEX_POINT('',#58634);
#5514=VERTEX_POINT('',#58880);
#5515=VERTEX_POINT('',#59118);
#5516=VERTEX_POINT('',#59119);
#5517=VERTEX_POINT('',#59121);
#5518=VERTEX_POINT('',#59376);
#5519=VERTEX_POINT('',#59623);
#5520=VERTEX_POINT('',#59624);
#5521=VERTEX_POINT('',#59626);
#5522=VERTEX_POINT('',#59866);
#5523=VERTEX_POINT('',#60107);
#5524=VERTEX_POINT('',#60108);
#5525=VERTEX_POINT('',#60110);
#5526=VERTEX_POINT('',#60350);
#5527=VERTEX_POINT('',#60585);
#5528=VERTEX_POINT('',#60586);
#5529=VERTEX_POINT('',#60588);
#5530=VERTEX_POINT('',#60840);
#5531=VERTEX_POINT('',#61084);
#5532=VERTEX_POINT('',#61085);
#5533=VERTEX_POINT('',#61087);
#5534=VERTEX_POINT('',#61339);
#5535=VERTEX_POINT('',#61589);
#5536=VERTEX_POINT('',#61590);
#5537=VERTEX_POINT('',#61592);
#5538=VERTEX_POINT('',#61835);
#5539=VERTEX_POINT('',#62085);
#5540=VERTEX_POINT('',#62086);
#5541=VERTEX_POINT('',#62088);
#5542=VERTEX_POINT('',#62322);
#5543=VERTEX_POINT('',#62566);
#5544=VERTEX_POINT('',#62567);
#5545=VERTEX_POINT('',#62576);
#5546=VERTEX_POINT('',#62578);
#5547=VERTEX_POINT('',#62905);
#5548=VERTEX_POINT('',#63458);
#5549=VERTEX_POINT('',#63973);
#5550=VERTEX_POINT('',#63987);
#5551=VERTEX_POINT('',#64492);
#5552=VERTEX_POINT('',#64995);
#5553=VERTEX_POINT('',#65258);
#5554=VERTEX_POINT('',#65781);
#5555=VERTEX_POINT('',#66322);
#5556=VERTEX_POINT('',#66811);
#5557=VERTEX_POINT('',#67071);
#5558=VERTEX_POINT('',#67564);
#5559=VERTEX_POINT('',#67827);
#5560=VERTEX_POINT('',#67846);
#5561=VERTEX_POINT('',#67859);
#5562=VERTEX_POINT('',#68122);
#5563=VERTEX_POINT('',#68136);
#5564=VERTEX_POINT('',#68633);
#5565=VERTEX_POINT('',#68896);
#5566=VERTEX_POINT('',#68910);
#5567=VERTEX_POINT('',#69437);
#5568=VERTEX_POINT('',#69928);
#5569=VERTEX_POINT('',#69945);
#5570=VERTEX_POINT('',#69964);
#5571=VERTEX_POINT('',#70477);
#5572=VERTEX_POINT('',#70490);
#5573=VERTEX_POINT('',#71021);
#5574=VERTEX_POINT('',#71526);
#5575=VERTEX_POINT('',#72057);
#5576=VERTEX_POINT('',#72076);
#5577=VERTEX_POINT('',#72603);
#5578=VERTEX_POINT('',#72616);
#5579=VERTEX_POINT('',#73181);
#5580=VERTEX_POINT('',#73194);
#5581=VERTEX_POINT('',#73454);
#5582=VERTEX_POINT('',#73951);
#5583=VERTEX_POINT('',#73970);
#5584=VERTEX_POINT('',#74487);
#5585=VERTEX_POINT('',#74500);
#5586=VERTEX_POINT('',#74519);
#5587=VERTEX_POINT('',#74536);
#5588=VERTEX_POINT('',#74538);
#5589=VERTEX_POINT('',#74711);
#5590=VERTEX_POINT('',#74730);
#5591=VERTEX_POINT('',#74744);
#5592=VERTEX_POINT('',#74759);
#5593=VERTEX_POINT('',#74772);
#5594=VERTEX_POINT('',#74791);
#5595=VERTEX_POINT('',#74810);
#5596=VERTEX_POINT('',#74829);
#5597=VERTEX_POINT('',#74848);
#5598=VERTEX_POINT('',#74861);
#5599=VERTEX_POINT('',#74877);
#5600=VERTEX_POINT('',#74896);
#5601=VERTEX_POINT('',#74910);
#5602=VERTEX_POINT('',#74925);
#5603=VERTEX_POINT('',#74938);
#5604=VERTEX_POINT('',#74957);
#5605=VERTEX_POINT('',#74976);
#5606=VERTEX_POINT('',#74995);
#5607=VERTEX_POINT('',#75014);
#5608=VERTEX_POINT('',#75027);
#5609=VERTEX_POINT('',#75043);
#5610=VERTEX_POINT('',#75062);
#5611=VERTEX_POINT('',#75076);
#5612=VERTEX_POINT('',#75091);
#5613=VERTEX_POINT('',#75104);
#5614=VERTEX_POINT('',#75123);
#5615=VERTEX_POINT('',#75142);
#5616=VERTEX_POINT('',#75161);
#5617=VERTEX_POINT('',#75180);
#5618=VERTEX_POINT('',#75193);
#5619=VERTEX_POINT('',#75208);
#5620=VERTEX_POINT('',#75222);
#5621=VERTEX_POINT('',#75241);
#5622=VERTEX_POINT('',#75260);
#5623=VERTEX_POINT('',#75279);
#5624=VERTEX_POINT('',#75503);
#5625=VERTEX_POINT('',#75517);
#5626=VERTEX_POINT('',#75774);
#5627=VERTEX_POINT('',#75788);
#5628=VERTEX_POINT('',#75802);
#5629=VERTEX_POINT('',#75818);
#5630=VERTEX_POINT('',#75832);
#5631=VERTEX_POINT('',#75851);
#5632=VERTEX_POINT('',#75870);
#5633=VERTEX_POINT('',#75889);
#5634=VERTEX_POINT('',#76116);
#5635=VERTEX_POINT('',#76130);
#5636=VERTEX_POINT('',#76387);
#5637=VERTEX_POINT('',#76401);
#5638=VERTEX_POINT('',#76415);
#5639=VERTEX_POINT('',#76430);
#5640=VERTEX_POINT('',#76444);
#5641=VERTEX_POINT('',#76463);
#5642=VERTEX_POINT('',#76482);
#5643=VERTEX_POINT('',#76501);
#5644=VERTEX_POINT('',#76520);
#5645=VERTEX_POINT('',#76534);
#5646=VERTEX_POINT('',#76548);
#5647=VERTEX_POINT('',#76819);
#5648=VERTEX_POINT('',#76896);
#5649=VERTEX_POINT('',#76985);
#5650=VERTEX_POINT('',#76987);
#5651=VERTEX_POINT('',#81915);
#5652=VERTEX_POINT('',#81917);
#5653=VERTEX_POINT('',#81921);
#5654=VERTEX_POINT('',#81923);
#5655=VERTEX_POINT('',#81927);
#5656=VERTEX_POINT('',#81929);
#5657=VERTEX_POINT('',#81933);
#5658=VERTEX_POINT('',#81935);
#5659=VERTEX_POINT('',#81939);
#5660=VERTEX_POINT('',#81940);
#5661=VERTEX_POINT('',#81942);
#5662=VERTEX_POINT('',#81947);
#5663=VERTEX_POINT('',#81948);
#5664=VERTEX_POINT('',#81954);
#5665=VERTEX_POINT('',#81961);
#5666=VERTEX_POINT('',#81962);
#5667=VERTEX_POINT('',#81964);
#5668=VERTEX_POINT('',#82029);
#5669=VERTEX_POINT('',#82133);
#5670=VERTEX_POINT('',#82135);
#5671=VERTEX_POINT('',#82207);
#5672=VERTEX_POINT('',#82208);
#5673=VERTEX_POINT('',#82210);
#5674=VERTEX_POINT('',#82275);
#5675=VERTEX_POINT('',#82467);
#5676=VERTEX_POINT('',#82532);
#5677=VERTEX_POINT('',#82725);
#5678=VERTEX_POINT('',#82726);
#5679=VERTEX_POINT('',#82728);
#5680=VERTEX_POINT('',#82793);
#5681=VERTEX_POINT('',#82985);
#5682=VERTEX_POINT('',#83050);
#5683=VERTEX_POINT('',#83243);
#5684=VERTEX_POINT('',#83244);
#5685=VERTEX_POINT('',#83246);
#5686=VERTEX_POINT('',#83311);
#5687=VERTEX_POINT('',#83503);
#5688=VERTEX_POINT('',#83568);
#5689=VERTEX_POINT('',#83761);
#5690=VERTEX_POINT('',#83762);
#5691=VERTEX_POINT('',#83764);
#5692=VERTEX_POINT('',#83829);
#5693=VERTEX_POINT('',#84021);
#5694=VERTEX_POINT('',#84086);
#5695=VERTEX_POINT('',#84279);
#5696=VERTEX_POINT('',#84280);
#5697=VERTEX_POINT('',#84282);
#5698=VERTEX_POINT('',#84284);
#5699=VERTEX_POINT('',#84291);
#5700=VERTEX_POINT('',#84483);
#5701=VERTEX_POINT('',#84548);
#5702=VERTEX_POINT('',#84741);
#5703=VERTEX_POINT('',#84784);
#5704=VERTEX_POINT('',#84785);
#5705=VERTEX_POINT('',#84823);
#5706=VERTEX_POINT('',#84942);
#5707=VERTEX_POINT('',#85027);
#5708=VERTEX_POINT('',#85086);
#5709=VERTEX_POINT('',#85128);
#5710=VERTEX_POINT('',#85150);
#5711=VERTEX_POINT('',#85188);
#5712=VERTEX_POINT('',#85223);
#5713=VERTEX_POINT('',#85342);
#5714=VERTEX_POINT('',#85393);
#5715=VERTEX_POINT('',#85431);
#5716=VERTEX_POINT('',#85454);
#5717=VERTEX_POINT('',#85522);
#5718=VERTEX_POINT('',#85535);
#5719=VERTEX_POINT('',#85539);
#5720=VERTEX_POINT('',#85601);
#5721=VERTEX_POINT('',#85694);
#5722=VERTEX_POINT('',#85696);
#5723=VERTEX_POINT('',#85748);
#5724=VERTEX_POINT('',#85750);
#5725=VERTEX_POINT('',#85844);
#5726=VERTEX_POINT('',#85846);
#5727=VERTEX_POINT('',#85898);
#5728=VERTEX_POINT('',#85900);
#5729=VERTEX_POINT('',#86002);
#5730=VERTEX_POINT('',#86004);
#5731=VERTEX_POINT('',#86068);
#5732=VERTEX_POINT('',#86070);
#5733=VERTEX_POINT('',#86164);
#5734=VERTEX_POINT('',#86166);
#5735=VERTEX_POINT('',#86230);
#5736=VERTEX_POINT('',#86232);
#5737=VERTEX_POINT('',#87086);
#5738=VERTEX_POINT('',#87088);
#5739=VERTEX_POINT('',#87090);
#5740=VERTEX_POINT('',#87094);
#5741=VERTEX_POINT('',#87098);
#5742=VERTEX_POINT('',#87100);
#5743=VERTEX_POINT('',#87102);
#5744=VERTEX_POINT('',#87104);
#5745=VERTEX_POINT('',#87106);
#5746=VERTEX_POINT('',#87109);
#5747=VERTEX_POINT('',#87113);
#5748=VERTEX_POINT('',#87117);
#5749=VERTEX_POINT('',#87121);
#5750=VERTEX_POINT('',#87125);
#5751=VERTEX_POINT('',#87131);
#5752=VERTEX_POINT('',#87133);
#5753=VERTEX_POINT('',#87138);
#5754=VERTEX_POINT('',#87140);
#5755=VERTEX_POINT('',#87145);
#5756=VERTEX_POINT('',#87147);
#5757=VERTEX_POINT('',#87152);
#5758=VERTEX_POINT('',#87154);
#5759=VERTEX_POINT('',#87159);
#5760=VERTEX_POINT('',#87161);
#5761=VERTEX_POINT('',#87165);
#5762=VERTEX_POINT('',#87167);
#5763=VERTEX_POINT('',#87172);
#5764=VERTEX_POINT('',#87174);
#5765=VERTEX_POINT('',#87179);
#5766=VERTEX_POINT('',#87181);
#5767=VERTEX_POINT('',#87186);
#5768=VERTEX_POINT('',#87188);
#5769=VERTEX_POINT('',#87192);
#5770=VERTEX_POINT('',#87194);
#5771=VERTEX_POINT('',#87198);
#5772=VERTEX_POINT('',#87200);
#5773=VERTEX_POINT('',#87204);
#5774=VERTEX_POINT('',#87206);
#5775=VERTEX_POINT('',#87210);
#5776=VERTEX_POINT('',#87211);
#5777=VERTEX_POINT('',#87213);
#5778=VERTEX_POINT('',#87215);
#5779=VERTEX_POINT('',#87219);
#5780=VERTEX_POINT('',#87221);
#5781=VERTEX_POINT('',#87223);
#5782=VERTEX_POINT('',#87225);
#5783=VERTEX_POINT('',#87227);
#5784=VERTEX_POINT('',#87229);
#5785=VERTEX_POINT('',#87231);
#5786=VERTEX_POINT('',#87233);
#5787=VERTEX_POINT('',#87235);
#5788=VERTEX_POINT('',#87237);
#5789=VERTEX_POINT('',#87239);
#5790=VERTEX_POINT('',#87241);
#5791=VERTEX_POINT('',#87243);
#5792=VERTEX_POINT('',#87245);
#5793=VERTEX_POINT('',#87247);
#5794=VERTEX_POINT('',#87249);
#5795=VERTEX_POINT('',#87251);
#5796=VERTEX_POINT('',#87255);
#5797=VERTEX_POINT('',#87259);
#5798=VERTEX_POINT('',#87263);
#5799=VERTEX_POINT('',#87264);
#5800=VERTEX_POINT('',#87270);
#5801=VERTEX_POINT('',#87274);
#5802=VERTEX_POINT('',#87280);
#5803=VERTEX_POINT('',#87282);
#5804=VERTEX_POINT('',#87286);
#5805=VERTEX_POINT('',#87290);
#5806=VERTEX_POINT('',#87294);
#5807=VERTEX_POINT('',#87296);
#5808=VERTEX_POINT('',#87298);
#5809=VERTEX_POINT('',#87300);
#5810=VERTEX_POINT('',#87360);
#5811=VERTEX_POINT('',#87362);
#5812=VERTEX_POINT('',#87374);
#5813=VERTEX_POINT('',#87382);
#5814=VERTEX_POINT('',#87387);
#5815=VERTEX_POINT('',#87389);
#5816=VERTEX_POINT('',#87404);
#5817=VERTEX_POINT('',#87419);
#5818=VERTEX_POINT('',#87450);
#5819=VERTEX_POINT('',#87453);
#5820=VERTEX_POINT('',#87457);
#5821=VERTEX_POINT('',#87465);
#5822=VERTEX_POINT('',#87467);
#5823=VERTEX_POINT('',#87471);
#5824=VERTEX_POINT('',#87473);
#5825=VERTEX_POINT('',#87477);
#5826=VERTEX_POINT('',#87479);
#5827=VERTEX_POINT('',#87483);
#5828=VERTEX_POINT('',#87485);
#5829=VERTEX_POINT('',#87487);
#5830=VERTEX_POINT('',#87491);
#5831=VERTEX_POINT('',#87495);
#5832=VERTEX_POINT('',#87498);
#5833=VERTEX_POINT('',#87504);
#5834=VERTEX_POINT('',#87506);
#5835=VERTEX_POINT('',#87510);
#5836=VERTEX_POINT('',#87511);
#5837=VERTEX_POINT('',#87513);
#5838=VERTEX_POINT('',#87515);
#5839=VERTEX_POINT('',#87520);
#5840=VERTEX_POINT('',#87524);
#5841=VERTEX_POINT('',#87528);
#5842=VERTEX_POINT('',#87532);
#5843=VERTEX_POINT('',#87534);
#5844=VERTEX_POINT('',#87540);
#5845=VERTEX_POINT('',#87544);
#5846=VERTEX_POINT('',#87548);
#5847=VERTEX_POINT('',#87554);
#5848=VERTEX_POINT('',#87555);
#5849=VERTEX_POINT('',#87558);
#5850=VERTEX_POINT('',#87560);
#5851=VERTEX_POINT('',#87564);
#5852=VERTEX_POINT('',#87568);
#5853=VERTEX_POINT('',#87569);
#5854=VERTEX_POINT('',#87571);
#5855=VERTEX_POINT('',#87576);
#5856=VERTEX_POINT('',#87582);
#5857=VERTEX_POINT('',#87584);
#5858=VERTEX_POINT('',#87588);
#5859=VERTEX_POINT('',#87590);
#5860=VERTEX_POINT('',#87594);
#5861=VERTEX_POINT('',#87598);
#5862=VERTEX_POINT('',#87604);
#5863=VERTEX_POINT('',#87606);
#5864=VERTEX_POINT('',#87610);
#5865=VERTEX_POINT('',#87614);
#5866=VERTEX_POINT('',#87615);
#5867=VERTEX_POINT('',#87617);
#5868=VERTEX_POINT('',#87622);
#5869=VERTEX_POINT('',#87626);
#5870=VERTEX_POINT('',#87630);
#5871=VERTEX_POINT('',#87632);
#5872=VERTEX_POINT('',#87636);
#5873=VERTEX_POINT('',#87637);
#5874=VERTEX_POINT('',#87642);
#5875=VERTEX_POINT('',#87646);
#5876=VERTEX_POINT('',#87654);
#5877=VERTEX_POINT('',#87655);
#5878=VERTEX_POINT('',#87658);
#5879=VERTEX_POINT('',#87659);
#5880=VERTEX_POINT('',#87662);
#5881=VERTEX_POINT('',#87663);
#5882=VERTEX_POINT('',#87666);
#5883=VERTEX_POINT('',#87667);
#5884=VERTEX_POINT('',#87670);
#5885=VERTEX_POINT('',#87671);
#5886=VERTEX_POINT('',#87674);
#5887=VERTEX_POINT('',#87675);
#5888=VERTEX_POINT('',#87678);
#5889=VERTEX_POINT('',#87679);
#5890=VERTEX_POINT('',#87682);
#5891=VERTEX_POINT('',#87683);
#5892=VERTEX_POINT('',#87686);
#5893=VERTEX_POINT('',#87688);
#5894=VERTEX_POINT('',#87692);
#5895=VERTEX_POINT('',#87696);
#5896=VERTEX_POINT('',#87700);
#5897=VERTEX_POINT('',#87702);
#5898=VERTEX_POINT('',#87706);
#5899=VERTEX_POINT('',#87707);
#5900=VERTEX_POINT('',#87712);
#5901=VERTEX_POINT('',#87718);
#5902=VERTEX_POINT('',#87719);
#5903=VERTEX_POINT('',#87722);
#5904=VERTEX_POINT('',#87726);
#5905=VERTEX_POINT('',#87728);
#5906=VERTEX_POINT('',#87732);
#5907=VERTEX_POINT('',#87734);
#5908=VERTEX_POINT('',#87742);
#5909=VERTEX_POINT('',#87743);
#5910=VERTEX_POINT('',#87746);
#5911=VERTEX_POINT('',#87748);
#5912=VERTEX_POINT('',#87752);
#5913=VERTEX_POINT('',#87753);
#5914=VERTEX_POINT('',#87756);
#5915=VERTEX_POINT('',#87758);
#5916=VERTEX_POINT('',#87762);
#5917=VERTEX_POINT('',#87764);
#5918=VERTEX_POINT('',#87766);
#5919=VERTEX_POINT('',#87770);
#5920=VERTEX_POINT('',#87771);
#5921=VERTEX_POINT('',#87778);
#5922=VERTEX_POINT('',#87780);
#5923=VERTEX_POINT('',#87782);
#5924=VERTEX_POINT('',#87790);
#5925=VERTEX_POINT('',#87793);
#5926=VERTEX_POINT('',#87795);
#5927=VERTEX_POINT('',#87804);
#5928=VERTEX_POINT('',#87805);
#5929=VERTEX_POINT('',#87807);
#5930=VERTEX_POINT('',#87815);
#5931=VERTEX_POINT('',#87824);
#5932=VERTEX_POINT('',#87825);
#5933=VERTEX_POINT('',#87827);
#5934=VERTEX_POINT('',#87835);
#5935=VERTEX_POINT('',#87844);
#5936=VERTEX_POINT('',#87845);
#5937=VERTEX_POINT('',#87847);
#5938=VERTEX_POINT('',#87855);
#5939=VERTEX_POINT('',#87864);
#5940=VERTEX_POINT('',#87865);
#5941=VERTEX_POINT('',#87867);
#5942=VERTEX_POINT('',#87875);
#5943=VERTEX_POINT('',#87884);
#5944=VERTEX_POINT('',#87885);
#5945=VERTEX_POINT('',#87887);
#5946=VERTEX_POINT('',#87895);
#5947=VERTEX_POINT('',#87904);
#5948=VERTEX_POINT('',#87905);
#5949=VERTEX_POINT('',#87907);
#5950=VERTEX_POINT('',#87915);
#5951=VERTEX_POINT('',#87924);
#5952=VERTEX_POINT('',#87925);
#5953=VERTEX_POINT('',#87927);
#5954=VERTEX_POINT('',#87935);
#5955=VERTEX_POINT('',#87944);
#5956=VERTEX_POINT('',#87945);
#5957=VERTEX_POINT('',#87947);
#5958=VERTEX_POINT('',#87955);
#5959=VERTEX_POINT('',#87964);
#5960=VERTEX_POINT('',#87965);
#5961=VERTEX_POINT('',#87967);
#5962=VERTEX_POINT('',#87975);
#5963=VERTEX_POINT('',#87984);
#5964=VERTEX_POINT('',#87985);
#5965=VERTEX_POINT('',#87987);
#5966=VERTEX_POINT('',#87995);
#5967=VERTEX_POINT('',#88005);
#5968=VERTEX_POINT('',#88007);
#5969=VERTEX_POINT('',#88009);
#5970=VERTEX_POINT('',#88017);
#5971=VERTEX_POINT('',#88020);
#5972=VERTEX_POINT('',#88022);
#5973=VERTEX_POINT('',#88031);
#5974=VERTEX_POINT('',#88032);
#5975=VERTEX_POINT('',#88034);
#5976=VERTEX_POINT('',#88042);
#5977=VERTEX_POINT('',#88051);
#5978=VERTEX_POINT('',#88052);
#5979=VERTEX_POINT('',#88054);
#5980=VERTEX_POINT('',#88062);
#5981=VERTEX_POINT('',#88071);
#5982=VERTEX_POINT('',#88072);
#5983=VERTEX_POINT('',#88074);
#5984=VERTEX_POINT('',#88082);
#5985=VERTEX_POINT('',#88091);
#5986=VERTEX_POINT('',#88092);
#5987=VERTEX_POINT('',#88094);
#5988=VERTEX_POINT('',#88102);
#5989=VERTEX_POINT('',#88111);
#5990=VERTEX_POINT('',#88112);
#5991=VERTEX_POINT('',#88114);
#5992=VERTEX_POINT('',#88122);
#5993=VERTEX_POINT('',#88131);
#5994=VERTEX_POINT('',#88132);
#5995=VERTEX_POINT('',#88134);
#5996=VERTEX_POINT('',#88142);
#5997=VERTEX_POINT('',#88151);
#5998=VERTEX_POINT('',#88152);
#5999=VERTEX_POINT('',#88154);
#6000=VERTEX_POINT('',#88162);
#6001=VERTEX_POINT('',#88171);
#6002=VERTEX_POINT('',#88172);
#6003=VERTEX_POINT('',#88174);
#6004=VERTEX_POINT('',#88182);
#6005=VERTEX_POINT('',#88191);
#6006=VERTEX_POINT('',#88192);
#6007=VERTEX_POINT('',#88194);
#6008=VERTEX_POINT('',#88202);
#6009=VERTEX_POINT('',#88211);
#6010=VERTEX_POINT('',#88212);
#6011=VERTEX_POINT('',#88214);
#6012=VERTEX_POINT('',#88222);
#6013=VERTEX_POINT('',#88320);
#6014=VERTEX_POINT('',#88322);
#6015=VERTEX_POINT('',#88324);
#6016=VERTEX_POINT('',#88328);
#6017=VERTEX_POINT('',#88330);
#6018=VERTEX_POINT('',#88334);
#6019=VERTEX_POINT('',#88336);
#6020=VERTEX_POINT('',#88338);
#6021=VERTEX_POINT('',#88342);
#6022=VERTEX_POINT('',#88343);
#6023=VERTEX_POINT('',#88348);
#6024=VERTEX_POINT('',#88352);
#6025=VERTEX_POINT('',#88358);
#6026=VERTEX_POINT('',#88364);
#6027=VERTEX_POINT('',#88366);
#6028=VERTEX_POINT('',#88372);
#6029=VERTEX_POINT('',#88374);
#6030=VERTEX_POINT('',#88380);
#6031=VERTEX_POINT('',#88382);
#6032=VERTEX_POINT('',#88388);
#6033=VERTEX_POINT('',#88390);
#6034=VERTEX_POINT('',#88396);
#6035=VERTEX_POINT('',#88398);
#6036=VERTEX_POINT('',#88404);
#6037=VERTEX_POINT('',#88406);
#6038=VERTEX_POINT('',#88412);
#6039=VERTEX_POINT('',#88414);
#6040=VERTEX_POINT('',#88420);
#6041=VERTEX_POINT('',#88422);
#6042=VERTEX_POINT('',#88428);
#6043=VERTEX_POINT('',#88430);
#6044=VERTEX_POINT('',#88436);
#6045=VERTEX_POINT('',#88438);
#6046=VERTEX_POINT('',#88444);
#6047=VERTEX_POINT('',#88446);
#6048=EDGE_CURVE('',#4615,#4616,#3675,.T.);
#6049=EDGE_CURVE('',#4616,#4617,#2872,.T.);
#6050=EDGE_CURVE('',#4618,#4617,#2221,.T.);
#6051=EDGE_CURVE('',#4615,#4618,#2873,.T.);
#6052=EDGE_CURVE('',#4619,#4620,#3676,.T.);
#6053=EDGE_CURVE('',#4620,#4621,#2874,.T.);
#6054=EDGE_CURVE('',#4621,#4616,#2875,.T.);
#6055=EDGE_CURVE('',#4622,#4615,#2876,.T.);
#6056=EDGE_CURVE('',#4619,#4622,#2877,.T.);
#6057=EDGE_CURVE('',#4623,#4624,#3677,.T.);
#6058=EDGE_CURVE('',#4624,#4625,#2878,.T.);
#6059=EDGE_CURVE('',#4625,#4620,#2879,.T.);
#6060=EDGE_CURVE('',#4626,#4619,#2880,.T.);
#6061=EDGE_CURVE('',#4623,#4626,#2881,.T.);
#6062=EDGE_CURVE('',#4627,#4628,#3678,.T.);
#6063=EDGE_CURVE('',#4628,#4629,#2882,.T.);
#6064=EDGE_CURVE('',#4629,#4624,#2883,.T.);
#6065=EDGE_CURVE('',#4630,#4623,#2884,.T.);
#6066=EDGE_CURVE('',#4627,#4630,#2885,.T.);
#6067=EDGE_CURVE('',#4631,#4632,#3679,.T.);
#6068=EDGE_CURVE('',#4632,#4633,#2886,.T.);
#6069=EDGE_CURVE('',#4633,#4628,#2887,.T.);
#6070=EDGE_CURVE('',#4634,#4627,#2888,.T.);
#6071=EDGE_CURVE('',#4631,#4634,#2889,.T.);
#6072=EDGE_CURVE('',#4635,#4636,#3680,.T.);
#6073=EDGE_CURVE('',#4636,#4637,#2890,.T.);
#6074=EDGE_CURVE('',#4637,#4632,#2891,.T.);
#6075=EDGE_CURVE('',#4638,#4631,#2892,.T.);
#6076=EDGE_CURVE('',#4635,#4638,#2893,.T.);
#6077=EDGE_CURVE('',#4639,#4640,#3681,.T.);
#6078=EDGE_CURVE('',#4640,#4641,#2894,.T.);
#6079=EDGE_CURVE('',#4641,#4636,#2895,.T.);
#6080=EDGE_CURVE('',#4642,#4635,#2896,.T.);
#6081=EDGE_CURVE('',#4639,#4642,#2897,.T.);
#6082=EDGE_CURVE('',#4643,#4644,#3682,.T.);
#6083=EDGE_CURVE('',#4644,#4645,#2898,.T.);
#6084=EDGE_CURVE('',#4645,#4640,#2899,.T.);
#6085=EDGE_CURVE('',#4646,#4639,#2900,.T.);
#6086=EDGE_CURVE('',#4643,#4646,#2901,.T.);
#6087=EDGE_CURVE('',#4647,#4648,#3683,.T.);
#6088=EDGE_CURVE('',#4648,#4649,#2902,.T.);
#6089=EDGE_CURVE('',#4649,#4644,#2903,.T.);
#6090=EDGE_CURVE('',#4650,#4643,#2904,.T.);
#6091=EDGE_CURVE('',#4647,#4650,#2905,.T.);
#6092=EDGE_CURVE('',#4651,#4652,#3684,.T.);
#6093=EDGE_CURVE('',#4652,#4653,#2906,.T.);
#6094=EDGE_CURVE('',#4653,#4648,#2907,.T.);
#6095=EDGE_CURVE('',#4654,#4647,#2908,.T.);
#6096=EDGE_CURVE('',#4651,#4654,#2909,.T.);
#6097=EDGE_CURVE('',#4655,#4656,#3685,.T.);
#6098=EDGE_CURVE('',#4656,#4657,#2910,.T.);
#6099=EDGE_CURVE('',#4657,#4652,#2911,.T.);
#6100=EDGE_CURVE('',#4658,#4651,#2912,.T.);
#6101=EDGE_CURVE('',#4655,#4658,#2913,.T.);
#6102=EDGE_CURVE('',#4659,#4660,#3686,.T.);
#6103=EDGE_CURVE('',#4661,#4659,#2914,.T.);
#6104=EDGE_CURVE('',#4662,#4661,#2915,.T.);
#6105=EDGE_CURVE('',#4663,#4662,#2222,.T.);
#6106=EDGE_CURVE('',#4663,#4664,#2916,.T.);
#6107=EDGE_CURVE('',#4664,#4660,#2917,.T.);
#6108=EDGE_CURVE('',#4665,#4666,#3687,.T.);
#6109=EDGE_CURVE('',#4666,#4667,#2918,.T.);
#6110=EDGE_CURVE('',#4668,#4667,#2223,.T.);
#6111=EDGE_CURVE('',#4668,#4665,#2919,.T.);
#6112=EDGE_CURVE('',#4669,#4670,#3688,.T.);
#6113=EDGE_CURVE('',#4670,#4666,#2920,.T.);
#6114=EDGE_CURVE('',#4665,#4671,#2921,.T.);
#6115=EDGE_CURVE('',#4671,#4669,#2922,.T.);
#6116=EDGE_CURVE('',#4672,#4673,#3689,.T.);
#6117=EDGE_CURVE('',#4673,#4674,#2923,.T.);
#6118=EDGE_CURVE('',#4674,#4670,#2924,.T.);
#6119=EDGE_CURVE('',#4669,#4675,#2925,.T.);
#6120=EDGE_CURVE('',#4675,#4672,#2926,.T.);
#6121=EDGE_CURVE('',#4676,#4677,#3690,.T.);
#6122=EDGE_CURVE('',#4677,#4678,#2927,.T.);
#6123=EDGE_CURVE('',#4678,#4673,#2928,.T.);
#6124=EDGE_CURVE('',#4672,#4679,#2929,.T.);
#6125=EDGE_CURVE('',#4679,#4676,#2930,.T.);
#6126=EDGE_CURVE('',#4680,#4681,#3691,.T.);
#6127=EDGE_CURVE('',#4681,#4682,#2931,.T.);
#6128=EDGE_CURVE('',#4682,#4677,#2932,.T.);
#6129=EDGE_CURVE('',#4676,#4683,#2933,.T.);
#6130=EDGE_CURVE('',#4683,#4680,#2934,.T.);
#6131=EDGE_CURVE('',#4684,#4685,#3692,.T.);
#6132=EDGE_CURVE('',#4685,#4686,#2935,.T.);
#6133=EDGE_CURVE('',#4686,#4681,#2936,.T.);
#6134=EDGE_CURVE('',#4680,#4687,#2937,.T.);
#6135=EDGE_CURVE('',#4687,#4684,#2938,.T.);
#6136=EDGE_CURVE('',#4688,#4689,#3693,.T.);
#6137=EDGE_CURVE('',#4689,#4690,#2939,.T.);
#6138=EDGE_CURVE('',#4690,#4685,#2940,.T.);
#6139=EDGE_CURVE('',#4684,#4691,#2941,.T.);
#6140=EDGE_CURVE('',#4691,#4688,#2942,.T.);
#6141=EDGE_CURVE('',#4692,#4693,#3694,.T.);
#6142=EDGE_CURVE('',#4693,#4689,#2943,.T.);
#6143=EDGE_CURVE('',#4688,#4694,#2944,.T.);
#6144=EDGE_CURVE('',#4694,#4692,#2945,.T.);
#6145=EDGE_CURVE('',#4695,#4696,#3695,.T.);
#6146=EDGE_CURVE('',#4696,#4697,#2946,.T.);
#6147=EDGE_CURVE('',#4697,#4693,#2947,.T.);
#6148=EDGE_CURVE('',#4692,#4698,#2948,.T.);
#6149=EDGE_CURVE('',#4698,#4695,#2949,.T.);
#6150=EDGE_CURVE('',#4699,#4700,#3696,.T.);
#6151=EDGE_CURVE('',#4700,#4701,#2950,.T.);
#6152=EDGE_CURVE('',#4701,#4696,#2951,.T.);
#6153=EDGE_CURVE('',#4695,#4699,#2952,.T.);
#6154=EDGE_CURVE('',#4702,#4703,#3697,.T.);
#6155=EDGE_CURVE('',#4703,#4700,#2953,.T.);
#6156=EDGE_CURVE('',#4699,#4704,#2954,.T.);
#6157=EDGE_CURVE('',#4704,#4702,#2955,.T.);
#6158=EDGE_CURVE('',#4705,#4706,#3698,.T.);
#6159=EDGE_CURVE('',#4705,#4707,#2956,.T.);
#6160=EDGE_CURVE('',#4707,#4708,#2957,.T.);
#6161=EDGE_CURVE('',#4709,#4708,#2224,.F.);
#6162=EDGE_CURVE('',#4709,#4706,#2958,.T.);
#6163=EDGE_CURVE('',#4706,#4710,#2959,.T.);
#6164=EDGE_CURVE('',#4710,#4703,#2960,.T.);
#6165=EDGE_CURVE('',#4702,#4711,#2961,.T.);
#6166=EDGE_CURVE('',#4711,#4705,#2962,.T.);
#6167=EDGE_CURVE('',#4660,#4712,#2963,.T.);
#6168=EDGE_CURVE('',#4712,#4656,#2964,.T.);
#6169=EDGE_CURVE('',#4713,#4655,#2965,.T.);
#6170=EDGE_CURVE('',#4659,#4713,#2966,.T.);
#6171=EDGE_CURVE('',#4617,#4668,#2967,.T.);
#6172=EDGE_CURVE('',#4708,#4663,#2968,.T.);
#6173=EDGE_CURVE('',#4667,#4618,#2969,.T.);
#6174=EDGE_CURVE('',#4714,#4709,#2970,.T.);
#6175=EDGE_CURVE('',#4662,#4714,#2971,.T.);
#6176=EDGE_CURVE('',#4715,#4716,#2225,.T.);
#6177=EDGE_CURVE('',#4716,#4717,#3699,.T.);
#6178=EDGE_CURVE('',#4717,#4718,#2226,.T.);
#6179=EDGE_CURVE('',#4718,#4719,#3700,.T.);
#6180=EDGE_CURVE('',#4719,#4720,#2227,.T.);
#6181=EDGE_CURVE('',#4720,#4721,#3701,.T.);
#6182=EDGE_CURVE('',#4721,#4722,#2228,.T.);
#6183=EDGE_CURVE('',#4722,#4723,#3702,.T.);
#6184=EDGE_CURVE('',#4723,#4724,#2229,.T.);
#6185=EDGE_CURVE('',#4724,#4725,#3703,.T.);
#6186=EDGE_CURVE('',#4725,#4726,#2230,.T.);
#6187=EDGE_CURVE('',#4726,#4727,#3704,.T.);
#6188=EDGE_CURVE('',#4727,#4728,#2231,.T.);
#6189=EDGE_CURVE('',#4728,#4729,#3705,.T.);
#6190=EDGE_CURVE('',#4729,#4730,#2232,.T.);
#6191=EDGE_CURVE('',#4730,#4731,#3706,.T.);
#6192=EDGE_CURVE('',#4731,#4732,#2233,.T.);
#6193=EDGE_CURVE('',#4732,#4733,#3707,.T.);
#6194=EDGE_CURVE('',#4733,#4734,#2234,.T.);
#6195=EDGE_CURVE('',#4734,#4735,#3708,.T.);
#6196=EDGE_CURVE('',#4735,#4736,#2235,.T.);
#6197=EDGE_CURVE('',#4736,#4737,#3709,.T.);
#6198=EDGE_CURVE('',#4737,#4738,#2236,.T.);
#6199=EDGE_CURVE('',#4738,#4739,#3710,.T.);
#6200=EDGE_CURVE('',#4739,#4740,#2237,.T.);
#6201=EDGE_CURVE('',#4740,#4741,#3711,.T.);
#6202=EDGE_CURVE('',#4741,#4742,#2238,.T.);
#6203=EDGE_CURVE('',#4742,#4743,#3712,.T.);
#6204=EDGE_CURVE('',#4743,#4744,#2239,.T.);
#6205=EDGE_CURVE('',#4744,#4745,#3713,.T.);
#6206=EDGE_CURVE('',#4745,#4746,#2240,.T.);
#6207=EDGE_CURVE('',#4746,#4747,#3714,.T.);
#6208=EDGE_CURVE('',#4747,#4748,#2241,.T.);
#6209=EDGE_CURVE('',#4748,#4749,#3715,.T.);
#6210=EDGE_CURVE('',#4749,#4750,#2242,.T.);
#6211=EDGE_CURVE('',#4750,#4751,#3716,.T.);
#6212=EDGE_CURVE('',#4751,#4752,#2243,.T.);
#6213=EDGE_CURVE('',#4752,#4753,#3717,.T.);
#6214=EDGE_CURVE('',#4753,#4754,#2244,.T.);
#6215=EDGE_CURVE('',#4754,#4755,#3718,.T.);
#6216=EDGE_CURVE('',#4755,#4756,#2245,.T.);
#6217=EDGE_CURVE('',#4756,#4757,#3719,.T.);
#6218=EDGE_CURVE('',#4757,#4758,#2246,.T.);
#6219=EDGE_CURVE('',#4758,#4759,#3720,.T.);
#6220=EDGE_CURVE('',#4759,#4760,#2247,.T.);
#6221=EDGE_CURVE('',#4760,#4761,#3721,.T.);
#6222=EDGE_CURVE('',#4761,#4762,#2248,.T.);
#6223=EDGE_CURVE('',#4762,#4763,#3722,.T.);
#6224=EDGE_CURVE('',#4763,#4764,#2249,.T.);
#6225=EDGE_CURVE('',#4764,#4765,#3723,.T.);
#6226=EDGE_CURVE('',#4765,#4766,#2250,.T.);
#6227=EDGE_CURVE('',#4766,#4767,#3724,.T.);
#6228=EDGE_CURVE('',#4767,#4768,#2251,.T.);
#6229=EDGE_CURVE('',#4768,#4769,#3725,.T.);
#6230=EDGE_CURVE('',#4769,#4770,#2252,.T.);
#6231=EDGE_CURVE('',#4770,#4771,#3726,.T.);
#6232=EDGE_CURVE('',#4771,#4772,#2253,.T.);
#6233=EDGE_CURVE('',#4772,#4773,#3727,.T.);
#6234=EDGE_CURVE('',#4773,#4774,#2254,.T.);
#6235=EDGE_CURVE('',#4774,#4775,#3728,.T.);
#6236=EDGE_CURVE('',#4775,#4776,#2255,.T.);
#6237=EDGE_CURVE('',#4776,#4777,#3729,.T.);
#6238=EDGE_CURVE('',#4777,#4778,#2256,.T.);
#6239=EDGE_CURVE('',#4778,#4779,#3730,.T.);
#6240=EDGE_CURVE('',#4779,#4780,#2257,.T.);
#6241=EDGE_CURVE('',#4780,#4781,#3731,.T.);
#6242=EDGE_CURVE('',#4781,#4782,#2258,.T.);
#6243=EDGE_CURVE('',#4782,#4783,#3732,.T.);
#6244=EDGE_CURVE('',#4783,#4784,#2259,.T.);
#6245=EDGE_CURVE('',#4784,#4785,#3733,.T.);
#6246=EDGE_CURVE('',#4785,#4786,#2260,.T.);
#6247=EDGE_CURVE('',#4786,#4715,#3734,.T.);
#6248=EDGE_CURVE('',#4787,#4788,#3735,.T.);
#6249=EDGE_CURVE('',#4789,#4787,#2261,.T.);
#6250=EDGE_CURVE('',#4790,#4789,#3736,.T.);
#6251=EDGE_CURVE('',#4788,#4790,#2262,.T.);
#6252=EDGE_CURVE('',#4791,#4792,#3737,.T.);
#6253=EDGE_CURVE('',#4793,#4791,#2263,.T.);
#6254=EDGE_CURVE('',#4794,#4793,#3738,.T.);
#6255=EDGE_CURVE('',#4792,#4794,#2264,.T.);
#6256=EDGE_CURVE('',#4795,#4796,#3739,.T.);
#6257=EDGE_CURVE('',#4797,#4795,#2265,.T.);
#6258=EDGE_CURVE('',#4798,#4797,#3740,.T.);
#6259=EDGE_CURVE('',#4796,#4798,#2266,.T.);
#6260=EDGE_CURVE('',#4799,#4800,#3741,.T.);
#6261=EDGE_CURVE('',#4801,#4799,#2267,.T.);
#6262=EDGE_CURVE('',#4802,#4801,#3742,.T.);
#6263=EDGE_CURVE('',#4800,#4802,#2268,.T.);
#6264=EDGE_CURVE('',#4803,#4804,#3743,.T.);
#6265=EDGE_CURVE('',#4805,#4803,#2269,.T.);
#6266=EDGE_CURVE('',#4806,#4805,#3744,.T.);
#6267=EDGE_CURVE('',#4804,#4806,#2270,.T.);
#6268=EDGE_CURVE('',#4807,#4808,#3745,.T.);
#6269=EDGE_CURVE('',#4809,#4807,#2271,.T.);
#6270=EDGE_CURVE('',#4810,#4809,#3746,.T.);
#6271=EDGE_CURVE('',#4808,#4810,#2272,.T.);
#6272=EDGE_CURVE('',#4811,#4812,#3747,.T.);
#6273=EDGE_CURVE('',#4813,#4811,#2273,.T.);
#6274=EDGE_CURVE('',#4814,#4813,#3748,.T.);
#6275=EDGE_CURVE('',#4812,#4814,#2274,.T.);
#6276=EDGE_CURVE('',#4815,#4816,#3749,.T.);
#6277=EDGE_CURVE('',#4817,#4815,#2275,.T.);
#6278=EDGE_CURVE('',#4818,#4817,#3750,.T.);
#6279=EDGE_CURVE('',#4816,#4818,#2276,.T.);
#6280=EDGE_CURVE('',#4819,#4820,#3751,.T.);
#6281=EDGE_CURVE('',#4821,#4819,#2277,.T.);
#6282=EDGE_CURVE('',#4822,#4821,#3752,.T.);
#6283=EDGE_CURVE('',#4820,#4822,#2278,.T.);
#6284=EDGE_CURVE('',#4823,#4824,#3753,.T.);
#6285=EDGE_CURVE('',#4825,#4823,#2279,.T.);
#6286=EDGE_CURVE('',#4826,#4825,#3754,.T.);
#6287=EDGE_CURVE('',#4824,#4826,#2280,.T.);
#6288=EDGE_CURVE('',#4827,#4828,#3755,.T.);
#6289=EDGE_CURVE('',#4829,#4827,#2281,.T.);
#6290=EDGE_CURVE('',#4830,#4829,#3756,.T.);
#6291=EDGE_CURVE('',#4828,#4830,#2282,.T.);
#6292=EDGE_CURVE('',#4831,#4832,#3757,.T.);
#6293=EDGE_CURVE('',#4833,#4831,#2283,.T.);
#6294=EDGE_CURVE('',#4834,#4833,#3758,.T.);
#6295=EDGE_CURVE('',#4832,#4834,#2284,.T.);
#6296=EDGE_CURVE('',#4835,#4836,#3759,.T.);
#6297=EDGE_CURVE('',#4837,#4835,#2285,.T.);
#6298=EDGE_CURVE('',#4838,#4837,#3760,.T.);
#6299=EDGE_CURVE('',#4836,#4838,#2286,.T.);
#6300=EDGE_CURVE('',#4839,#4840,#3761,.T.);
#6301=EDGE_CURVE('',#4841,#4839,#2287,.T.);
#6302=EDGE_CURVE('',#4842,#4841,#3762,.T.);
#6303=EDGE_CURVE('',#4840,#4842,#2288,.T.);
#6304=EDGE_CURVE('',#4843,#4844,#3763,.T.);
#6305=EDGE_CURVE('',#4845,#4843,#2289,.T.);
#6306=EDGE_CURVE('',#4846,#4845,#3764,.T.);
#6307=EDGE_CURVE('',#4844,#4846,#2290,.T.);
#6308=EDGE_CURVE('',#4847,#4848,#3765,.T.);
#6309=EDGE_CURVE('',#4849,#4847,#2291,.T.);
#6310=EDGE_CURVE('',#4850,#4849,#3766,.T.);
#6311=EDGE_CURVE('',#4848,#4850,#2292,.T.);
#6312=EDGE_CURVE('',#4851,#4852,#3767,.T.);
#6313=EDGE_CURVE('',#4853,#4851,#2293,.T.);
#6314=EDGE_CURVE('',#4854,#4853,#3768,.T.);
#6315=EDGE_CURVE('',#4852,#4854,#2294,.T.);
#6316=EDGE_CURVE('',#4855,#4856,#3769,.T.);
#6317=EDGE_CURVE('',#4857,#4855,#2295,.T.);
#6318=EDGE_CURVE('',#4858,#4857,#3770,.T.);
#6319=EDGE_CURVE('',#4856,#4858,#2296,.T.);
#6320=EDGE_CURVE('',#4724,#4859,#2297,.T.);
#6321=EDGE_CURVE('',#4860,#4723,#2298,.T.);
#6322=EDGE_CURVE('',#4861,#4860,#3771,.T.);
#6323=EDGE_CURVE('',#4849,#4861,#2972,.T.);
#6324=EDGE_CURVE('',#4862,#4847,#2973,.T.);
#6325=EDGE_CURVE('',#4859,#4862,#3772,.T.);
#6326=EDGE_CURVE('',#4728,#4863,#2299,.T.);
#6327=EDGE_CURVE('',#4864,#4727,#2300,.T.);
#6328=EDGE_CURVE('',#4865,#4864,#3773,.T.);
#6329=EDGE_CURVE('',#4845,#4865,#2974,.T.);
#6330=EDGE_CURVE('',#4866,#4843,#2975,.T.);
#6331=EDGE_CURVE('',#4863,#4866,#3774,.T.);
#6332=EDGE_CURVE('',#4732,#4867,#2301,.T.);
#6333=EDGE_CURVE('',#4868,#4731,#2302,.T.);
#6334=EDGE_CURVE('',#4869,#4868,#3775,.T.);
#6335=EDGE_CURVE('',#4841,#4869,#2976,.T.);
#6336=EDGE_CURVE('',#4870,#4839,#2977,.T.);
#6337=EDGE_CURVE('',#4867,#4870,#3776,.T.);
#6338=EDGE_CURVE('',#4736,#4871,#2303,.T.);
#6339=EDGE_CURVE('',#4872,#4735,#2304,.T.);
#6340=EDGE_CURVE('',#4873,#4872,#3777,.T.);
#6341=EDGE_CURVE('',#4837,#4873,#2978,.T.);
#6342=EDGE_CURVE('',#4874,#4835,#2979,.T.);
#6343=EDGE_CURVE('',#4871,#4874,#3778,.T.);
#6344=EDGE_CURVE('',#4740,#4875,#2305,.T.);
#6345=EDGE_CURVE('',#4876,#4739,#2306,.T.);
#6346=EDGE_CURVE('',#4877,#4876,#3779,.T.);
#6347=EDGE_CURVE('',#4833,#4877,#2980,.T.);
#6348=EDGE_CURVE('',#4878,#4831,#2981,.T.);
#6349=EDGE_CURVE('',#4875,#4878,#3780,.T.);
#6350=EDGE_CURVE('',#4744,#4879,#2307,.T.);
#6351=EDGE_CURVE('',#4880,#4743,#2308,.T.);
#6352=EDGE_CURVE('',#4881,#4880,#3781,.T.);
#6353=EDGE_CURVE('',#4829,#4881,#2982,.T.);
#6354=EDGE_CURVE('',#4882,#4827,#2983,.T.);
#6355=EDGE_CURVE('',#4879,#4882,#3782,.T.);
#6356=EDGE_CURVE('',#4748,#4883,#2309,.T.);
#6357=EDGE_CURVE('',#4884,#4747,#2310,.T.);
#6358=EDGE_CURVE('',#4885,#4884,#3783,.T.);
#6359=EDGE_CURVE('',#4825,#4885,#2984,.T.);
#6360=EDGE_CURVE('',#4886,#4823,#2985,.T.);
#6361=EDGE_CURVE('',#4883,#4886,#3784,.T.);
#6362=EDGE_CURVE('',#4752,#4887,#2311,.T.);
#6363=EDGE_CURVE('',#4888,#4751,#2312,.T.);
#6364=EDGE_CURVE('',#4889,#4888,#3785,.T.);
#6365=EDGE_CURVE('',#4821,#4889,#2986,.T.);
#6366=EDGE_CURVE('',#4890,#4819,#2987,.T.);
#6367=EDGE_CURVE('',#4887,#4890,#3786,.T.);
#6368=EDGE_CURVE('',#4756,#4891,#2313,.T.);
#6369=EDGE_CURVE('',#4892,#4755,#2314,.T.);
#6370=EDGE_CURVE('',#4893,#4892,#3787,.T.);
#6371=EDGE_CURVE('',#4817,#4893,#2988,.T.);
#6372=EDGE_CURVE('',#4894,#4815,#2989,.T.);
#6373=EDGE_CURVE('',#4891,#4894,#3788,.T.);
#6374=EDGE_CURVE('',#4760,#4895,#2315,.T.);
#6375=EDGE_CURVE('',#4896,#4759,#2316,.T.);
#6376=EDGE_CURVE('',#4897,#4896,#3789,.T.);
#6377=EDGE_CURVE('',#4813,#4897,#2990,.T.);
#6378=EDGE_CURVE('',#4898,#4811,#2991,.T.);
#6379=EDGE_CURVE('',#4895,#4898,#3790,.T.);
#6380=EDGE_CURVE('',#4764,#4899,#2317,.T.);
#6381=EDGE_CURVE('',#4900,#4763,#2318,.T.);
#6382=EDGE_CURVE('',#4901,#4900,#3791,.T.);
#6383=EDGE_CURVE('',#4809,#4901,#2992,.T.);
#6384=EDGE_CURVE('',#4902,#4807,#2993,.T.);
#6385=EDGE_CURVE('',#4899,#4902,#3792,.T.);
#6386=EDGE_CURVE('',#4768,#4903,#2319,.T.);
#6387=EDGE_CURVE('',#4904,#4767,#2320,.T.);
#6388=EDGE_CURVE('',#4905,#4904,#3793,.T.);
#6389=EDGE_CURVE('',#4805,#4905,#2994,.T.);
#6390=EDGE_CURVE('',#4906,#4803,#2995,.T.);
#6391=EDGE_CURVE('',#4903,#4906,#3794,.T.);
#6392=EDGE_CURVE('',#4772,#4907,#2321,.T.);
#6393=EDGE_CURVE('',#4908,#4771,#2322,.T.);
#6394=EDGE_CURVE('',#4909,#4908,#3795,.T.);
#6395=EDGE_CURVE('',#4801,#4909,#2996,.T.);
#6396=EDGE_CURVE('',#4910,#4799,#2997,.T.);
#6397=EDGE_CURVE('',#4907,#4910,#3796,.T.);
#6398=EDGE_CURVE('',#4776,#4911,#2323,.T.);
#6399=EDGE_CURVE('',#4912,#4775,#2324,.T.);
#6400=EDGE_CURVE('',#4913,#4912,#3797,.T.);
#6401=EDGE_CURVE('',#4797,#4913,#2998,.T.);
#6402=EDGE_CURVE('',#4914,#4795,#2999,.T.);
#6403=EDGE_CURVE('',#4911,#4914,#3798,.T.);
#6404=EDGE_CURVE('',#4780,#4915,#2325,.T.);
#6405=EDGE_CURVE('',#4916,#4779,#2326,.T.);
#6406=EDGE_CURVE('',#4917,#4916,#3799,.T.);
#6407=EDGE_CURVE('',#4793,#4917,#3000,.T.);
#6408=EDGE_CURVE('',#4918,#4791,#3001,.T.);
#6409=EDGE_CURVE('',#4915,#4918,#3800,.T.);
#6410=EDGE_CURVE('',#4784,#4919,#2327,.T.);
#6411=EDGE_CURVE('',#4920,#4783,#2328,.T.);
#6412=EDGE_CURVE('',#4921,#4920,#3801,.T.);
#6413=EDGE_CURVE('',#4789,#4921,#3002,.T.);
#6414=EDGE_CURVE('',#4922,#4787,#3003,.T.);
#6415=EDGE_CURVE('',#4919,#4922,#3802,.T.);
#6416=EDGE_CURVE('',#4720,#4923,#2329,.T.);
#6417=EDGE_CURVE('',#4924,#4719,#2330,.T.);
#6418=EDGE_CURVE('',#4925,#4924,#3803,.T.);
#6419=EDGE_CURVE('',#4853,#4925,#3004,.T.);
#6420=EDGE_CURVE('',#4926,#4851,#3005,.T.);
#6421=EDGE_CURVE('',#4923,#4926,#3804,.T.);
#6422=EDGE_CURVE('',#4716,#4927,#2331,.T.);
#6423=EDGE_CURVE('',#4928,#4715,#2332,.T.);
#6424=EDGE_CURVE('',#4929,#4928,#3805,.T.);
#6425=EDGE_CURVE('',#4857,#4929,#3006,.T.);
#6426=EDGE_CURVE('',#4930,#4855,#3007,.T.);
#6427=EDGE_CURVE('',#4927,#4930,#3806,.T.);
#6428=EDGE_CURVE('',#4931,#4932,#2333,.T.);
#6429=EDGE_CURVE('',#4933,#4931,#2334,.T.);
#6430=EDGE_CURVE('',#4934,#4933,#2335,.T.);
#6431=EDGE_CURVE('',#4935,#4934,#3807,.T.);
#6432=EDGE_CURVE('',#4936,#4935,#3008,.T.);
#6433=EDGE_CURVE('',#4937,#4936,#2336,.T.);
#6434=EDGE_CURVE('',#4938,#4937,#3009,.T.);
#6435=EDGE_CURVE('',#4932,#4938,#3808,.T.);
#6436=EDGE_CURVE('',#4939,#4940,#2337,.T.);
#6437=EDGE_CURVE('',#4941,#4939,#2338,.T.);
#6438=EDGE_CURVE('',#4942,#4941,#2339,.T.);
#6439=EDGE_CURVE('',#4943,#4942,#3809,.T.);
#6440=EDGE_CURVE('',#4944,#4943,#3010,.T.);
#6441=EDGE_CURVE('',#4945,#4944,#2340,.T.);
#6442=EDGE_CURVE('',#4946,#4945,#3011,.T.);
#6443=EDGE_CURVE('',#4940,#4946,#3810,.T.);
#6444=EDGE_CURVE('',#4947,#4948,#2341,.T.);
#6445=EDGE_CURVE('',#4949,#4947,#2342,.T.);
#6446=EDGE_CURVE('',#4950,#4949,#2343,.T.);
#6447=EDGE_CURVE('',#4951,#4950,#3811,.T.);
#6448=EDGE_CURVE('',#4952,#4951,#3012,.T.);
#6449=EDGE_CURVE('',#4953,#4952,#2344,.T.);
#6450=EDGE_CURVE('',#4954,#4953,#3013,.T.);
#6451=EDGE_CURVE('',#4948,#4954,#3812,.T.);
#6452=EDGE_CURVE('',#4955,#4956,#2345,.T.);
#6453=EDGE_CURVE('',#4957,#4955,#2346,.T.);
#6454=EDGE_CURVE('',#4958,#4957,#2347,.T.);
#6455=EDGE_CURVE('',#4959,#4958,#3813,.T.);
#6456=EDGE_CURVE('',#4960,#4959,#3014,.T.);
#6457=EDGE_CURVE('',#4961,#4960,#2348,.T.);
#6458=EDGE_CURVE('',#4962,#4961,#3015,.T.);
#6459=EDGE_CURVE('',#4956,#4962,#3814,.T.);
#6460=EDGE_CURVE('',#4963,#4964,#2349,.T.);
#6461=EDGE_CURVE('',#4965,#4963,#2350,.T.);
#6462=EDGE_CURVE('',#4966,#4965,#2351,.T.);
#6463=EDGE_CURVE('',#4967,#4966,#3815,.T.);
#6464=EDGE_CURVE('',#4968,#4967,#3016,.T.);
#6465=EDGE_CURVE('',#4969,#4968,#2352,.T.);
#6466=EDGE_CURVE('',#4970,#4969,#3017,.T.);
#6467=EDGE_CURVE('',#4964,#4970,#3816,.T.);
#6468=EDGE_CURVE('',#4971,#4972,#2353,.T.);
#6469=EDGE_CURVE('',#4973,#4971,#2354,.T.);
#6470=EDGE_CURVE('',#4974,#4973,#2355,.T.);
#6471=EDGE_CURVE('',#4975,#4974,#3817,.T.);
#6472=EDGE_CURVE('',#4976,#4975,#3018,.T.);
#6473=EDGE_CURVE('',#4977,#4976,#2356,.T.);
#6474=EDGE_CURVE('',#4978,#4977,#3019,.T.);
#6475=EDGE_CURVE('',#4972,#4978,#3818,.T.);
#6476=EDGE_CURVE('',#4979,#4980,#2357,.T.);
#6477=EDGE_CURVE('',#4981,#4979,#2358,.T.);
#6478=EDGE_CURVE('',#4982,#4981,#2359,.T.);
#6479=EDGE_CURVE('',#4983,#4982,#3819,.T.);
#6480=EDGE_CURVE('',#4984,#4983,#3020,.T.);
#6481=EDGE_CURVE('',#4985,#4984,#2360,.T.);
#6482=EDGE_CURVE('',#4986,#4985,#3021,.T.);
#6483=EDGE_CURVE('',#4980,#4986,#3820,.T.);
#6484=EDGE_CURVE('',#4987,#4988,#2361,.T.);
#6485=EDGE_CURVE('',#4989,#4987,#2362,.T.);
#6486=EDGE_CURVE('',#4990,#4989,#2363,.T.);
#6487=EDGE_CURVE('',#4991,#4990,#3821,.T.);
#6488=EDGE_CURVE('',#4992,#4991,#3022,.T.);
#6489=EDGE_CURVE('',#4993,#4992,#2364,.T.);
#6490=EDGE_CURVE('',#4994,#4993,#3023,.T.);
#6491=EDGE_CURVE('',#4988,#4994,#3822,.T.);
#6492=EDGE_CURVE('',#4995,#4996,#2365,.T.);
#6493=EDGE_CURVE('',#4997,#4995,#2366,.T.);
#6494=EDGE_CURVE('',#4998,#4997,#2367,.T.);
#6495=EDGE_CURVE('',#4999,#4998,#3823,.T.);
#6496=EDGE_CURVE('',#5000,#4999,#3024,.T.);
#6497=EDGE_CURVE('',#5001,#5000,#2368,.T.);
#6498=EDGE_CURVE('',#5002,#5001,#3025,.T.);
#6499=EDGE_CURVE('',#4996,#5002,#3824,.T.);
#6500=EDGE_CURVE('',#5003,#5004,#2369,.T.);
#6501=EDGE_CURVE('',#5005,#5003,#2370,.T.);
#6502=EDGE_CURVE('',#5006,#5005,#2371,.T.);
#6503=EDGE_CURVE('',#5007,#5006,#3825,.T.);
#6504=EDGE_CURVE('',#5008,#5007,#3026,.T.);
#6505=EDGE_CURVE('',#5009,#5008,#2372,.T.);
#6506=EDGE_CURVE('',#5010,#5009,#3027,.T.);
#6507=EDGE_CURVE('',#5004,#5010,#3826,.T.);
#6508=EDGE_CURVE('',#5011,#5012,#2373,.T.);
#6509=EDGE_CURVE('',#5013,#5011,#2374,.T.);
#6510=EDGE_CURVE('',#5014,#5013,#2375,.T.);
#6511=EDGE_CURVE('',#5015,#5014,#3827,.T.);
#6512=EDGE_CURVE('',#5016,#5015,#3028,.T.);
#6513=EDGE_CURVE('',#5017,#5016,#2376,.T.);
#6514=EDGE_CURVE('',#5018,#5017,#3029,.T.);
#6515=EDGE_CURVE('',#5012,#5018,#3828,.T.);
#6516=EDGE_CURVE('',#5019,#5020,#2377,.T.);
#6517=EDGE_CURVE('',#5021,#5019,#2378,.T.);
#6518=EDGE_CURVE('',#5022,#5021,#2379,.T.);
#6519=EDGE_CURVE('',#5023,#5022,#3829,.T.);
#6520=EDGE_CURVE('',#5024,#5023,#3030,.T.);
#6521=EDGE_CURVE('',#5025,#5024,#2380,.T.);
#6522=EDGE_CURVE('',#5026,#5025,#3031,.T.);
#6523=EDGE_CURVE('',#5020,#5026,#3830,.T.);
#6524=EDGE_CURVE('',#5027,#5028,#2381,.T.);
#6525=EDGE_CURVE('',#5029,#5027,#2382,.T.);
#6526=EDGE_CURVE('',#5030,#5029,#2383,.T.);
#6527=EDGE_CURVE('',#5031,#5030,#3831,.T.);
#6528=EDGE_CURVE('',#5032,#5031,#3032,.T.);
#6529=EDGE_CURVE('',#5033,#5032,#2384,.T.);
#6530=EDGE_CURVE('',#5034,#5033,#3033,.T.);
#6531=EDGE_CURVE('',#5028,#5034,#3832,.T.);
#6532=EDGE_CURVE('',#5035,#5036,#2385,.T.);
#6533=EDGE_CURVE('',#5037,#5035,#2386,.T.);
#6534=EDGE_CURVE('',#5038,#5037,#2387,.T.);
#6535=EDGE_CURVE('',#5039,#5038,#3833,.T.);
#6536=EDGE_CURVE('',#5040,#5039,#3034,.T.);
#6537=EDGE_CURVE('',#5041,#5040,#2388,.T.);
#6538=EDGE_CURVE('',#5042,#5041,#3035,.T.);
#6539=EDGE_CURVE('',#5036,#5042,#3834,.T.);
#6540=EDGE_CURVE('',#5043,#5044,#2389,.T.);
#6541=EDGE_CURVE('',#5045,#5043,#2390,.T.);
#6542=EDGE_CURVE('',#5046,#5045,#2391,.T.);
#6543=EDGE_CURVE('',#5047,#5046,#3835,.T.);
#6544=EDGE_CURVE('',#5048,#5047,#3036,.T.);
#6545=EDGE_CURVE('',#5049,#5048,#2392,.T.);
#6546=EDGE_CURVE('',#5050,#5049,#3037,.T.);
#6547=EDGE_CURVE('',#5044,#5050,#3836,.T.);
#6548=EDGE_CURVE('',#5051,#5052,#2393,.T.);
#6549=EDGE_CURVE('',#5053,#5051,#2394,.T.);
#6550=EDGE_CURVE('',#5054,#5053,#2395,.T.);
#6551=EDGE_CURVE('',#5055,#5054,#3837,.T.);
#6552=EDGE_CURVE('',#5056,#5055,#3038,.T.);
#6553=EDGE_CURVE('',#5057,#5056,#2396,.T.);
#6554=EDGE_CURVE('',#5058,#5057,#3039,.T.);
#6555=EDGE_CURVE('',#5052,#5058,#3838,.T.);
#6556=EDGE_CURVE('',#5059,#5060,#2397,.T.);
#6557=EDGE_CURVE('',#5061,#5059,#2398,.T.);
#6558=EDGE_CURVE('',#5062,#5061,#2399,.T.);
#6559=EDGE_CURVE('',#5063,#5062,#3839,.T.);
#6560=EDGE_CURVE('',#5064,#5063,#3040,.T.);
#6561=EDGE_CURVE('',#5065,#5064,#2400,.T.);
#6562=EDGE_CURVE('',#5066,#5065,#3041,.T.);
#6563=EDGE_CURVE('',#5060,#5066,#3840,.T.);
#6564=EDGE_CURVE('',#5067,#5068,#2401,.T.);
#6565=EDGE_CURVE('',#5069,#5067,#2402,.T.);
#6566=EDGE_CURVE('',#5070,#5069,#2403,.T.);
#6567=EDGE_CURVE('',#5071,#5070,#3841,.T.);
#6568=EDGE_CURVE('',#5072,#5071,#3042,.T.);
#6569=EDGE_CURVE('',#5073,#5072,#2404,.T.);
#6570=EDGE_CURVE('',#5074,#5073,#3043,.T.);
#6571=EDGE_CURVE('',#5068,#5074,#3842,.T.);
#6572=EDGE_CURVE('',#4937,#5075,#3843,.T.);
#6573=EDGE_CURVE('',#5076,#4936,#3844,.T.);
#6574=EDGE_CURVE('',#5075,#5076,#2405,.T.);
#6575=EDGE_CURVE('',#4945,#5077,#3845,.T.);
#6576=EDGE_CURVE('',#5078,#4944,#3846,.T.);
#6577=EDGE_CURVE('',#5077,#5078,#2406,.T.);
#6578=EDGE_CURVE('',#4953,#5079,#3847,.T.);
#6579=EDGE_CURVE('',#5080,#4952,#3848,.T.);
#6580=EDGE_CURVE('',#5079,#5080,#2407,.T.);
#6581=EDGE_CURVE('',#4961,#5081,#3849,.T.);
#6582=EDGE_CURVE('',#5082,#4960,#3850,.T.);
#6583=EDGE_CURVE('',#5081,#5082,#2408,.T.);
#6584=EDGE_CURVE('',#4969,#5083,#3851,.T.);
#6585=EDGE_CURVE('',#5084,#4968,#3852,.T.);
#6586=EDGE_CURVE('',#5083,#5084,#2409,.T.);
#6587=EDGE_CURVE('',#4977,#5085,#3853,.T.);
#6588=EDGE_CURVE('',#5086,#4976,#3854,.T.);
#6589=EDGE_CURVE('',#5085,#5086,#2410,.T.);
#6590=EDGE_CURVE('',#4985,#5087,#3855,.T.);
#6591=EDGE_CURVE('',#5088,#4984,#3856,.T.);
#6592=EDGE_CURVE('',#5087,#5088,#2411,.T.);
#6593=EDGE_CURVE('',#4993,#5089,#3857,.T.);
#6594=EDGE_CURVE('',#5090,#4992,#3858,.T.);
#6595=EDGE_CURVE('',#5089,#5090,#2412,.T.);
#6596=EDGE_CURVE('',#5001,#5091,#3859,.T.);
#6597=EDGE_CURVE('',#5092,#5000,#3860,.T.);
#6598=EDGE_CURVE('',#5091,#5092,#2413,.T.);
#6599=EDGE_CURVE('',#5009,#5093,#3861,.T.);
#6600=EDGE_CURVE('',#5094,#5008,#3862,.T.);
#6601=EDGE_CURVE('',#5093,#5094,#2414,.T.);
#6602=EDGE_CURVE('',#5017,#5095,#3863,.T.);
#6603=EDGE_CURVE('',#5096,#5016,#3864,.T.);
#6604=EDGE_CURVE('',#5095,#5096,#2415,.T.);
#6605=EDGE_CURVE('',#5025,#5097,#3865,.T.);
#6606=EDGE_CURVE('',#5098,#5024,#3866,.T.);
#6607=EDGE_CURVE('',#5097,#5098,#2416,.T.);
#6608=EDGE_CURVE('',#5033,#5099,#3867,.T.);
#6609=EDGE_CURVE('',#5100,#5032,#3868,.T.);
#6610=EDGE_CURVE('',#5099,#5100,#2417,.T.);
#6611=EDGE_CURVE('',#5041,#5101,#3869,.T.);
#6612=EDGE_CURVE('',#5102,#5040,#3870,.T.);
#6613=EDGE_CURVE('',#5101,#5102,#2418,.T.);
#6614=EDGE_CURVE('',#5049,#5103,#3871,.T.);
#6615=EDGE_CURVE('',#5104,#5048,#3872,.T.);
#6616=EDGE_CURVE('',#5103,#5104,#2419,.T.);
#6617=EDGE_CURVE('',#5057,#5105,#3873,.T.);
#6618=EDGE_CURVE('',#5106,#5056,#3874,.T.);
#6619=EDGE_CURVE('',#5105,#5106,#2420,.T.);
#6620=EDGE_CURVE('',#5065,#5107,#3875,.T.);
#6621=EDGE_CURVE('',#5108,#5064,#3876,.T.);
#6622=EDGE_CURVE('',#5107,#5108,#2421,.T.);
#6623=EDGE_CURVE('',#5073,#5109,#3877,.T.);
#6624=EDGE_CURVE('',#5110,#5072,#3878,.T.);
#6625=EDGE_CURVE('',#5109,#5110,#2422,.T.);
#6626=EDGE_CURVE('',#5111,#5112,#190,.T.);
#6627=EDGE_CURVE('',#5113,#5111,#2423,.T.);
#6628=EDGE_CURVE('',#5114,#5113,#3044,.T.);
#6629=EDGE_CURVE('',#5112,#5114,#2424,.T.);
#6630=EDGE_CURVE('',#5115,#5116,#191,.T.);
#6631=EDGE_CURVE('',#5117,#5115,#2425,.T.);
#6632=EDGE_CURVE('',#5118,#5117,#192,.T.);
#6633=EDGE_CURVE('',#5116,#5118,#2426,.T.);
#6634=EDGE_CURVE('',#5119,#5120,#193,.T.);
#6635=EDGE_CURVE('',#5121,#5119,#2427,.T.);
#6636=EDGE_CURVE('',#5122,#5121,#194,.T.);
#6637=EDGE_CURVE('',#5120,#5122,#2428,.T.);
#6638=EDGE_CURVE('',#5123,#5124,#195,.T.);
#6639=EDGE_CURVE('',#5125,#5123,#2429,.T.);
#6640=EDGE_CURVE('',#5126,#5125,#3045,.T.);
#6641=EDGE_CURVE('',#5124,#5126,#2430,.T.);
#6642=EDGE_CURVE('',#5127,#5128,#196,.T.);
#6643=EDGE_CURVE('',#5129,#5127,#2431,.T.);
#6644=EDGE_CURVE('',#5130,#5129,#197,.T.);
#6645=EDGE_CURVE('',#5128,#5130,#2432,.T.);
#6646=EDGE_CURVE('',#5131,#5132,#198,.T.);
#6647=EDGE_CURVE('',#5133,#5131,#2433,.T.);
#6648=EDGE_CURVE('',#5134,#5133,#199,.T.);
#6649=EDGE_CURVE('',#5132,#5134,#2434,.T.);
#6650=EDGE_CURVE('',#5135,#5136,#200,.T.);
#6651=EDGE_CURVE('',#5137,#5135,#2435,.T.);
#6652=EDGE_CURVE('',#5138,#5137,#201,.T.);
#6653=EDGE_CURVE('',#5136,#5138,#2436,.T.);
#6654=EDGE_CURVE('',#5139,#5140,#202,.T.);
#6655=EDGE_CURVE('',#5141,#5139,#2437,.T.);
#6656=EDGE_CURVE('',#5142,#5141,#3046,.T.);
#6657=EDGE_CURVE('',#5140,#5142,#2438,.T.);
#6658=EDGE_CURVE('',#5143,#5144,#203,.T.);
#6659=EDGE_CURVE('',#5145,#5143,#2439,.T.);
#6660=EDGE_CURVE('',#5146,#5145,#204,.T.);
#6661=EDGE_CURVE('',#5144,#5146,#2440,.T.);
#6662=EDGE_CURVE('',#5147,#5148,#205,.T.);
#6663=EDGE_CURVE('',#5149,#5147,#2441,.T.);
#6664=EDGE_CURVE('',#5150,#5149,#206,.T.);
#6665=EDGE_CURVE('',#5148,#5150,#2442,.T.);
#6666=EDGE_CURVE('',#5151,#5152,#207,.T.);
#6667=EDGE_CURVE('',#5153,#5151,#2443,.T.);
#6668=EDGE_CURVE('',#5154,#5153,#208,.T.);
#6669=EDGE_CURVE('',#5152,#5154,#2444,.T.);
#6670=EDGE_CURVE('',#5155,#5156,#209,.T.);
#6671=EDGE_CURVE('',#5157,#5155,#2445,.T.);
#6672=EDGE_CURVE('',#5158,#5157,#3047,.T.);
#6673=EDGE_CURVE('',#5156,#5158,#2446,.T.);
#6674=EDGE_CURVE('',#5159,#5160,#210,.T.);
#6675=EDGE_CURVE('',#5161,#5159,#2447,.T.);
#6676=EDGE_CURVE('',#5162,#5161,#211,.T.);
#6677=EDGE_CURVE('',#5160,#5162,#2448,.T.);
#6678=EDGE_CURVE('',#5163,#5164,#212,.T.);
#6679=EDGE_CURVE('',#5165,#5163,#2449,.T.);
#6680=EDGE_CURVE('',#5166,#5165,#213,.T.);
#6681=EDGE_CURVE('',#5164,#5166,#2450,.T.);
#6682=EDGE_CURVE('',#5167,#5168,#214,.T.);
#6683=EDGE_CURVE('',#5169,#5167,#2451,.T.);
#6684=EDGE_CURVE('',#5170,#5169,#215,.T.);
#6685=EDGE_CURVE('',#5168,#5170,#2452,.T.);
#6686=EDGE_CURVE('',#5171,#5172,#216,.T.);
#6687=EDGE_CURVE('',#5173,#5171,#2453,.T.);
#6688=EDGE_CURVE('',#5174,#5173,#217,.T.);
#6689=EDGE_CURVE('',#5172,#5174,#2454,.T.);
#6690=EDGE_CURVE('',#5175,#5176,#218,.T.);
#6691=EDGE_CURVE('',#5177,#5175,#2455,.T.);
#6692=EDGE_CURVE('',#5178,#5177,#3048,.T.);
#6693=EDGE_CURVE('',#5176,#5178,#2456,.T.);
#6694=EDGE_CURVE('',#5179,#5180,#219,.T.);
#6695=EDGE_CURVE('',#5181,#5179,#2457,.T.);
#6696=EDGE_CURVE('',#5182,#5181,#3049,.T.);
#6697=EDGE_CURVE('',#5180,#5182,#2458,.T.);
#6698=EDGE_CURVE('',#5183,#5184,#3050,.T.);
#6699=EDGE_CURVE('',#5183,#5185,#2459,.T.);
#6700=EDGE_CURVE('',#5186,#5185,#220,.T.);
#6701=EDGE_CURVE('',#5184,#5186,#2460,.T.);
#6702=EDGE_CURVE('',#5187,#5188,#3051,.T.);
#6703=EDGE_CURVE('',#5187,#5189,#2461,.T.);
#6704=EDGE_CURVE('',#5190,#5189,#221,.T.);
#6705=EDGE_CURVE('',#5188,#5190,#2462,.T.);
#6706=EDGE_CURVE('',#5191,#5192,#3052,.T.);
#6707=EDGE_CURVE('',#5191,#5193,#2463,.T.);
#6708=EDGE_CURVE('',#5194,#5193,#222,.T.);
#6709=EDGE_CURVE('',#5192,#5194,#2464,.T.);
#6710=EDGE_CURVE('',#5195,#5196,#3053,.T.);
#6711=EDGE_CURVE('',#5195,#5197,#2465,.T.);
#6712=EDGE_CURVE('',#5198,#5197,#223,.T.);
#6713=EDGE_CURVE('',#5196,#5198,#2466,.T.);
#6714=EDGE_CURVE('',#5199,#5200,#3054,.T.);
#6715=EDGE_CURVE('',#5199,#5201,#2467,.T.);
#6716=EDGE_CURVE('',#5202,#5201,#224,.T.);
#6717=EDGE_CURVE('',#5200,#5202,#2468,.T.);
#6718=EDGE_CURVE('',#5203,#5204,#3055,.T.);
#6719=EDGE_CURVE('',#5203,#5205,#2469,.T.);
#6720=EDGE_CURVE('',#5206,#5205,#225,.T.);
#6721=EDGE_CURVE('',#5204,#5206,#2470,.T.);
#6722=EDGE_CURVE('',#5207,#5208,#3056,.T.);
#6723=EDGE_CURVE('',#5207,#5209,#2471,.T.);
#6724=EDGE_CURVE('',#5210,#5209,#226,.T.);
#6725=EDGE_CURVE('',#5208,#5210,#2472,.T.);
#6726=EDGE_CURVE('',#5211,#5212,#3057,.T.);
#6727=EDGE_CURVE('',#5211,#5213,#2473,.T.);
#6728=EDGE_CURVE('',#5214,#5213,#227,.T.);
#6729=EDGE_CURVE('',#5212,#5214,#2474,.T.);
#6730=EDGE_CURVE('',#5215,#5216,#3058,.T.);
#6731=EDGE_CURVE('',#5215,#5217,#2475,.T.);
#6732=EDGE_CURVE('',#5218,#5217,#228,.T.);
#6733=EDGE_CURVE('',#5216,#5218,#2476,.T.);
#6734=EDGE_CURVE('',#5219,#5220,#3059,.T.);
#6735=EDGE_CURVE('',#5219,#5221,#2477,.T.);
#6736=EDGE_CURVE('',#5222,#5221,#229,.T.);
#6737=EDGE_CURVE('',#5220,#5222,#2478,.T.);
#6738=EDGE_CURVE('',#5223,#5224,#3060,.T.);
#6739=EDGE_CURVE('',#5223,#5225,#2479,.T.);
#6740=EDGE_CURVE('',#5226,#5225,#230,.T.);
#6741=EDGE_CURVE('',#5224,#5226,#2480,.T.);
#6742=EDGE_CURVE('',#5227,#5228,#3061,.T.);
#6743=EDGE_CURVE('',#5227,#5229,#2481,.T.);
#6744=EDGE_CURVE('',#5230,#5229,#231,.T.);
#6745=EDGE_CURVE('',#5228,#5230,#2482,.T.);
#6746=EDGE_CURVE('',#5231,#5232,#3062,.T.);
#6747=EDGE_CURVE('',#5231,#5233,#2483,.T.);
#6748=EDGE_CURVE('',#5234,#5233,#232,.T.);
#6749=EDGE_CURVE('',#5232,#5234,#2484,.T.);
#6750=EDGE_CURVE('',#5235,#5236,#3063,.T.);
#6751=EDGE_CURVE('',#5235,#5237,#2485,.T.);
#6752=EDGE_CURVE('',#5238,#5237,#233,.T.);
#6753=EDGE_CURVE('',#5236,#5238,#2486,.T.);
#6754=EDGE_CURVE('',#5239,#5240,#3064,.T.);
#6755=EDGE_CURVE('',#5239,#5241,#2487,.T.);
#6756=EDGE_CURVE('',#5242,#5241,#234,.T.);
#6757=EDGE_CURVE('',#5240,#5242,#2488,.T.);
#6758=EDGE_CURVE('',#5243,#5244,#3065,.T.);
#6759=EDGE_CURVE('',#5243,#5245,#2489,.T.);
#6760=EDGE_CURVE('',#5246,#5245,#235,.T.);
#6761=EDGE_CURVE('',#5244,#5246,#2490,.T.);
#6762=EDGE_CURVE('',#5247,#5248,#3066,.T.);
#6763=EDGE_CURVE('',#5247,#5249,#2491,.T.);
#6764=EDGE_CURVE('',#5250,#5249,#236,.T.);
#6765=EDGE_CURVE('',#5248,#5250,#2492,.T.);
#6766=EDGE_CURVE('',#5251,#5252,#3067,.T.);
#6767=EDGE_CURVE('',#5251,#5253,#2493,.T.);
#6768=EDGE_CURVE('',#5254,#5253,#237,.T.);
#6769=EDGE_CURVE('',#5252,#5254,#2494,.T.);
#6770=EDGE_CURVE('',#5112,#5183,#3068,.T.);
#6771=EDGE_CURVE('',#5185,#5114,#3069,.T.);
#6772=EDGE_CURVE('',#5116,#5187,#3070,.T.);
#6773=EDGE_CURVE('',#5189,#5118,#3071,.T.);
#6774=EDGE_CURVE('',#5120,#5191,#3072,.T.);
#6775=EDGE_CURVE('',#5193,#5122,#3073,.T.);
#6776=EDGE_CURVE('',#5124,#5195,#3074,.T.);
#6777=EDGE_CURVE('',#5197,#5126,#3075,.T.);
#6778=EDGE_CURVE('',#5128,#5199,#3076,.T.);
#6779=EDGE_CURVE('',#5201,#5130,#3077,.T.);
#6780=EDGE_CURVE('',#5132,#5203,#3078,.T.);
#6781=EDGE_CURVE('',#5205,#5134,#3079,.T.);
#6782=EDGE_CURVE('',#5136,#5207,#3080,.T.);
#6783=EDGE_CURVE('',#5209,#5138,#3081,.T.);
#6784=EDGE_CURVE('',#5140,#5211,#3082,.T.);
#6785=EDGE_CURVE('',#5213,#5142,#3083,.T.);
#6786=EDGE_CURVE('',#5144,#5215,#3084,.T.);
#6787=EDGE_CURVE('',#5217,#5146,#3085,.T.);
#6788=EDGE_CURVE('',#5148,#5219,#3086,.T.);
#6789=EDGE_CURVE('',#5221,#5150,#3087,.T.);
#6790=EDGE_CURVE('',#5152,#5223,#3088,.T.);
#6791=EDGE_CURVE('',#5225,#5154,#3089,.T.);
#6792=EDGE_CURVE('',#5156,#5227,#3090,.T.);
#6793=EDGE_CURVE('',#5229,#5158,#3091,.T.);
#6794=EDGE_CURVE('',#5160,#5231,#3092,.T.);
#6795=EDGE_CURVE('',#5233,#5162,#3093,.T.);
#6796=EDGE_CURVE('',#5164,#5235,#3094,.T.);
#6797=EDGE_CURVE('',#5237,#5166,#3095,.T.);
#6798=EDGE_CURVE('',#5168,#5239,#3096,.T.);
#6799=EDGE_CURVE('',#5241,#5170,#3097,.T.);
#6800=EDGE_CURVE('',#5172,#5243,#3098,.T.);
#6801=EDGE_CURVE('',#5245,#5174,#3099,.T.);
#6802=EDGE_CURVE('',#5176,#5247,#3100,.T.);
#6803=EDGE_CURVE('',#5249,#5178,#3101,.T.);
#6804=EDGE_CURVE('',#5180,#5251,#3102,.T.);
#6805=EDGE_CURVE('',#5253,#5182,#3103,.T.);
#6806=EDGE_CURVE('',#5071,#4930,#3104,.T.);
#6807=EDGE_CURVE('',#5070,#4927,#3105,.T.);
#6808=EDGE_CURVE('',#5063,#4922,#3106,.T.);
#6809=EDGE_CURVE('',#5062,#4919,#3107,.T.);
#6810=EDGE_CURVE('',#5055,#4918,#3108,.T.);
#6811=EDGE_CURVE('',#5054,#4915,#3109,.T.);
#6812=EDGE_CURVE('',#5047,#4914,#3110,.T.);
#6813=EDGE_CURVE('',#5046,#4911,#3111,.T.);
#6814=EDGE_CURVE('',#5039,#4910,#3112,.T.);
#6815=EDGE_CURVE('',#5038,#4907,#3113,.T.);
#6816=EDGE_CURVE('',#5031,#4906,#3114,.T.);
#6817=EDGE_CURVE('',#5030,#4903,#3115,.T.);
#6818=EDGE_CURVE('',#5023,#4902,#3116,.T.);
#6819=EDGE_CURVE('',#5022,#4899,#3117,.T.);
#6820=EDGE_CURVE('',#5015,#4898,#3118,.T.);
#6821=EDGE_CURVE('',#5014,#4895,#3119,.T.);
#6822=EDGE_CURVE('',#5007,#4894,#3120,.T.);
#6823=EDGE_CURVE('',#5006,#4891,#3121,.T.);
#6824=EDGE_CURVE('',#4999,#4890,#3122,.T.);
#6825=EDGE_CURVE('',#4998,#4887,#3123,.T.);
#6826=EDGE_CURVE('',#4991,#4886,#3124,.T.);
#6827=EDGE_CURVE('',#4990,#4883,#3125,.T.);
#6828=EDGE_CURVE('',#4983,#4882,#3126,.T.);
#6829=EDGE_CURVE('',#4982,#4879,#3127,.T.);
#6830=EDGE_CURVE('',#4975,#4878,#3128,.T.);
#6831=EDGE_CURVE('',#4974,#4875,#3129,.T.);
#6832=EDGE_CURVE('',#4967,#4874,#3130,.T.);
#6833=EDGE_CURVE('',#4966,#4871,#3131,.T.);
#6834=EDGE_CURVE('',#4959,#4870,#3132,.T.);
#6835=EDGE_CURVE('',#4958,#4867,#3133,.T.);
#6836=EDGE_CURVE('',#4951,#4866,#3134,.T.);
#6837=EDGE_CURVE('',#4950,#4863,#3135,.T.);
#6838=EDGE_CURVE('',#4943,#4862,#3136,.T.);
#6839=EDGE_CURVE('',#4942,#4859,#3137,.T.);
#6840=EDGE_CURVE('',#4935,#4926,#3138,.T.);
#6841=EDGE_CURVE('',#4934,#4923,#3139,.T.);
#6842=EDGE_CURVE('',#5074,#4929,#3140,.T.);
#6843=EDGE_CURVE('',#5109,#5179,#2495,.T.);
#6844=EDGE_CURVE('',#5252,#4858,#2496,.T.);
#6845=EDGE_CURVE('',#5254,#4856,#2497,.T.);
#6846=EDGE_CURVE('',#5110,#5181,#2498,.T.);
#6847=EDGE_CURVE('',#5066,#4921,#3141,.T.);
#6848=EDGE_CURVE('',#5107,#5175,#2499,.T.);
#6849=EDGE_CURVE('',#5248,#4790,#2500,.T.);
#6850=EDGE_CURVE('',#5250,#4788,#2501,.T.);
#6851=EDGE_CURVE('',#5108,#5177,#2502,.T.);
#6852=EDGE_CURVE('',#5058,#4917,#3142,.T.);
#6853=EDGE_CURVE('',#5105,#5171,#2503,.T.);
#6854=EDGE_CURVE('',#5244,#4794,#2504,.T.);
#6855=EDGE_CURVE('',#5246,#4792,#2505,.T.);
#6856=EDGE_CURVE('',#5106,#5173,#2506,.T.);
#6857=EDGE_CURVE('',#5050,#4913,#3143,.T.);
#6858=EDGE_CURVE('',#5103,#5167,#2507,.T.);
#6859=EDGE_CURVE('',#5240,#4798,#2508,.T.);
#6860=EDGE_CURVE('',#5242,#4796,#2509,.T.);
#6861=EDGE_CURVE('',#5104,#5169,#2510,.T.);
#6862=EDGE_CURVE('',#5042,#4909,#3144,.T.);
#6863=EDGE_CURVE('',#5101,#5163,#2511,.T.);
#6864=EDGE_CURVE('',#5236,#4802,#2512,.T.);
#6865=EDGE_CURVE('',#5238,#4800,#2513,.T.);
#6866=EDGE_CURVE('',#5102,#5165,#2514,.T.);
#6867=EDGE_CURVE('',#5034,#4905,#3145,.T.);
#6868=EDGE_CURVE('',#5099,#5159,#2515,.T.);
#6869=EDGE_CURVE('',#5232,#4806,#2516,.T.);
#6870=EDGE_CURVE('',#5234,#4804,#2517,.T.);
#6871=EDGE_CURVE('',#5100,#5161,#2518,.T.);
#6872=EDGE_CURVE('',#5026,#4901,#3146,.T.);
#6873=EDGE_CURVE('',#5097,#5155,#2519,.T.);
#6874=EDGE_CURVE('',#5228,#4810,#2520,.T.);
#6875=EDGE_CURVE('',#5230,#4808,#2521,.T.);
#6876=EDGE_CURVE('',#5098,#5157,#2522,.T.);
#6877=EDGE_CURVE('',#5018,#4897,#3147,.T.);
#6878=EDGE_CURVE('',#5095,#5151,#2523,.T.);
#6879=EDGE_CURVE('',#5224,#4814,#2524,.T.);
#6880=EDGE_CURVE('',#5226,#4812,#2525,.T.);
#6881=EDGE_CURVE('',#5096,#5153,#2526,.T.);
#6882=EDGE_CURVE('',#5010,#4893,#3148,.T.);
#6883=EDGE_CURVE('',#5093,#5147,#2527,.T.);
#6884=EDGE_CURVE('',#5220,#4818,#2528,.T.);
#6885=EDGE_CURVE('',#5222,#4816,#2529,.T.);
#6886=EDGE_CURVE('',#5094,#5149,#2530,.T.);
#6887=EDGE_CURVE('',#5002,#4889,#3149,.T.);
#6888=EDGE_CURVE('',#5091,#5143,#2531,.T.);
#6889=EDGE_CURVE('',#5216,#4822,#2532,.T.);
#6890=EDGE_CURVE('',#5218,#4820,#2533,.T.);
#6891=EDGE_CURVE('',#5092,#5145,#2534,.T.);
#6892=EDGE_CURVE('',#4994,#4885,#3150,.T.);
#6893=EDGE_CURVE('',#5089,#5139,#2535,.T.);
#6894=EDGE_CURVE('',#5212,#4826,#2536,.T.);
#6895=EDGE_CURVE('',#5214,#4824,#2537,.T.);
#6896=EDGE_CURVE('',#5090,#5141,#2538,.T.);
#6897=EDGE_CURVE('',#4986,#4881,#3151,.T.);
#6898=EDGE_CURVE('',#5087,#5135,#2539,.T.);
#6899=EDGE_CURVE('',#5208,#4830,#2540,.T.);
#6900=EDGE_CURVE('',#5210,#4828,#2541,.T.);
#6901=EDGE_CURVE('',#5088,#5137,#2542,.T.);
#6902=EDGE_CURVE('',#4978,#4877,#3152,.T.);
#6903=EDGE_CURVE('',#5085,#5131,#2543,.T.);
#6904=EDGE_CURVE('',#5204,#4834,#2544,.T.);
#6905=EDGE_CURVE('',#5206,#4832,#2545,.T.);
#6906=EDGE_CURVE('',#5086,#5133,#2546,.T.);
#6907=EDGE_CURVE('',#4970,#4873,#3153,.T.);
#6908=EDGE_CURVE('',#5083,#5127,#2547,.T.);
#6909=EDGE_CURVE('',#5200,#4838,#2548,.T.);
#6910=EDGE_CURVE('',#5202,#4836,#2549,.T.);
#6911=EDGE_CURVE('',#5084,#5129,#2550,.T.);
#6912=EDGE_CURVE('',#4962,#4869,#3154,.T.);
#6913=EDGE_CURVE('',#5081,#5123,#2551,.T.);
#6914=EDGE_CURVE('',#5196,#4842,#2552,.T.);
#6915=EDGE_CURVE('',#5198,#4840,#2553,.T.);
#6916=EDGE_CURVE('',#5082,#5125,#2554,.T.);
#6917=EDGE_CURVE('',#4954,#4865,#3155,.T.);
#6918=EDGE_CURVE('',#5079,#5119,#2555,.T.);
#6919=EDGE_CURVE('',#5192,#4846,#2556,.T.);
#6920=EDGE_CURVE('',#5194,#4844,#2557,.T.);
#6921=EDGE_CURVE('',#5080,#5121,#2558,.T.);
#6922=EDGE_CURVE('',#4946,#4861,#3156,.T.);
#6923=EDGE_CURVE('',#5077,#5115,#2559,.T.);
#6924=EDGE_CURVE('',#5188,#4850,#2560,.T.);
#6925=EDGE_CURVE('',#5190,#4848,#2561,.T.);
#6926=EDGE_CURVE('',#5078,#5117,#2562,.T.);
#6927=EDGE_CURVE('',#4938,#4925,#3157,.T.);
#6928=EDGE_CURVE('',#5075,#5111,#2563,.T.);
#6929=EDGE_CURVE('',#5184,#4854,#2564,.T.);
#6930=EDGE_CURVE('',#5186,#4852,#2565,.T.);
#6931=EDGE_CURVE('',#5076,#5113,#2566,.T.);
#6932=EDGE_CURVE('',#5255,#5069,#3879,.F.);
#6933=EDGE_CURVE('',#4717,#5255,#3158,.T.);
#6934=EDGE_CURVE('',#5068,#4928,#3159,.T.);
#6935=EDGE_CURVE('',#5256,#4786,#3160,.T.);
#6936=EDGE_CURVE('',#5256,#5067,#3880,.T.);
#6937=EDGE_CURVE('',#5255,#5257,#2567,.T.);
#6938=EDGE_CURVE('',#5257,#4718,#3161,.T.);
#6939=EDGE_CURVE('',#4785,#5258,#3162,.T.);
#6940=EDGE_CURVE('',#5258,#5256,#2568,.T.);
#6941=EDGE_CURVE('',#5259,#4782,#3163,.T.);
#6942=EDGE_CURVE('',#5259,#5059,#3881,.T.);
#6943=EDGE_CURVE('',#5060,#4920,#3164,.T.);
#6944=EDGE_CURVE('',#5258,#5061,#3882,.F.);
#6945=EDGE_CURVE('',#5260,#5053,#3883,.F.);
#6946=EDGE_CURVE('',#4781,#5260,#3165,.T.);
#6947=EDGE_CURVE('',#5261,#4778,#3166,.T.);
#6948=EDGE_CURVE('',#5261,#5051,#3884,.T.);
#6949=EDGE_CURVE('',#5052,#4916,#3167,.T.);
#6950=EDGE_CURVE('',#5260,#5259,#2569,.T.);
#6951=EDGE_CURVE('',#5262,#5261,#2570,.T.);
#6952=EDGE_CURVE('',#5262,#5045,#3885,.F.);
#6953=EDGE_CURVE('',#5263,#5043,#3886,.T.);
#6954=EDGE_CURVE('',#5264,#5263,#2571,.T.);
#6955=EDGE_CURVE('',#5264,#5037,#3887,.F.);
#6956=EDGE_CURVE('',#5265,#5035,#3888,.T.);
#6957=EDGE_CURVE('',#5266,#5265,#2572,.T.);
#6958=EDGE_CURVE('',#5266,#5029,#3889,.F.);
#6959=EDGE_CURVE('',#5267,#5027,#3890,.T.);
#6960=EDGE_CURVE('',#5268,#5267,#2573,.T.);
#6961=EDGE_CURVE('',#5268,#5021,#3891,.F.);
#6962=EDGE_CURVE('',#5269,#5019,#3892,.T.);
#6963=EDGE_CURVE('',#5270,#5269,#2574,.T.);
#6964=EDGE_CURVE('',#5270,#5013,#3893,.F.);
#6965=EDGE_CURVE('',#5271,#5011,#3894,.T.);
#6966=EDGE_CURVE('',#5272,#5271,#2575,.T.);
#6967=EDGE_CURVE('',#5272,#5005,#3895,.F.);
#6968=EDGE_CURVE('',#5273,#5003,#3896,.T.);
#6969=EDGE_CURVE('',#5274,#5273,#2576,.T.);
#6970=EDGE_CURVE('',#5274,#4997,#3897,.F.);
#6971=EDGE_CURVE('',#5275,#4995,#3898,.T.);
#6972=EDGE_CURVE('',#5276,#5275,#2577,.T.);
#6973=EDGE_CURVE('',#5276,#4989,#3899,.F.);
#6974=EDGE_CURVE('',#5277,#4987,#3900,.T.);
#6975=EDGE_CURVE('',#5278,#5277,#2578,.T.);
#6976=EDGE_CURVE('',#5278,#4981,#3901,.F.);
#6977=EDGE_CURVE('',#5279,#4979,#3902,.T.);
#6978=EDGE_CURVE('',#5280,#5279,#2579,.T.);
#6979=EDGE_CURVE('',#5280,#4973,#3903,.F.);
#6980=EDGE_CURVE('',#5281,#4971,#3904,.T.);
#6981=EDGE_CURVE('',#5282,#5281,#2580,.T.);
#6982=EDGE_CURVE('',#5282,#4965,#3905,.F.);
#6983=EDGE_CURVE('',#5283,#4963,#3906,.T.);
#6984=EDGE_CURVE('',#5284,#5283,#2581,.T.);
#6985=EDGE_CURVE('',#5284,#4957,#3907,.F.);
#6986=EDGE_CURVE('',#5285,#4955,#3908,.T.);
#6987=EDGE_CURVE('',#5286,#5285,#2582,.T.);
#6988=EDGE_CURVE('',#5286,#4949,#3909,.F.);
#6989=EDGE_CURVE('',#5287,#4947,#3910,.T.);
#6990=EDGE_CURVE('',#5288,#5287,#2583,.T.);
#6991=EDGE_CURVE('',#5288,#4941,#3911,.F.);
#6992=EDGE_CURVE('',#5289,#4939,#3912,.T.);
#6993=EDGE_CURVE('',#5290,#5289,#2584,.T.);
#6994=EDGE_CURVE('',#5290,#4933,#3913,.F.);
#6995=EDGE_CURVE('',#5257,#4931,#3914,.T.);
#6996=EDGE_CURVE('',#4777,#5262,#3168,.T.);
#6997=EDGE_CURVE('',#5044,#4912,#3169,.T.);
#6998=EDGE_CURVE('',#5263,#4774,#3170,.T.);
#6999=EDGE_CURVE('',#4773,#5264,#3171,.T.);
#7000=EDGE_CURVE('',#5265,#4770,#3172,.T.);
#7001=EDGE_CURVE('',#5036,#4908,#3173,.T.);
#7002=EDGE_CURVE('',#4769,#5266,#3174,.T.);
#7003=EDGE_CURVE('',#5267,#4766,#3175,.T.);
#7004=EDGE_CURVE('',#5028,#4904,#3176,.T.);
#7005=EDGE_CURVE('',#4765,#5268,#3177,.T.);
#7006=EDGE_CURVE('',#5020,#4900,#3178,.T.);
#7007=EDGE_CURVE('',#5269,#4762,#3179,.T.);
#7008=EDGE_CURVE('',#4761,#5270,#3180,.T.);
#7009=EDGE_CURVE('',#5271,#4758,#3181,.T.);
#7010=EDGE_CURVE('',#5012,#4896,#3182,.T.);
#7011=EDGE_CURVE('',#4757,#5272,#3183,.T.);
#7012=EDGE_CURVE('',#5273,#4754,#3184,.T.);
#7013=EDGE_CURVE('',#5004,#4892,#3185,.T.);
#7014=EDGE_CURVE('',#4753,#5274,#3186,.T.);
#7015=EDGE_CURVE('',#4996,#4888,#3187,.T.);
#7016=EDGE_CURVE('',#5275,#4750,#3188,.T.);
#7017=EDGE_CURVE('',#4749,#5276,#3189,.T.);
#7018=EDGE_CURVE('',#5277,#4746,#3190,.T.);
#7019=EDGE_CURVE('',#4988,#4884,#3191,.T.);
#7020=EDGE_CURVE('',#4745,#5278,#3192,.T.);
#7021=EDGE_CURVE('',#5279,#4742,#3193,.T.);
#7022=EDGE_CURVE('',#4980,#4880,#3194,.T.);
#7023=EDGE_CURVE('',#4741,#5280,#3195,.T.);
#7024=EDGE_CURVE('',#4972,#4876,#3196,.T.);
#7025=EDGE_CURVE('',#5281,#4738,#3197,.T.);
#7026=EDGE_CURVE('',#4737,#5282,#3198,.T.);
#7027=EDGE_CURVE('',#5283,#4734,#3199,.T.);
#7028=EDGE_CURVE('',#4964,#4872,#3200,.T.);
#7029=EDGE_CURVE('',#4733,#5284,#3201,.T.);
#7030=EDGE_CURVE('',#5285,#4730,#3202,.T.);
#7031=EDGE_CURVE('',#4956,#4868,#3203,.T.);
#7032=EDGE_CURVE('',#4729,#5286,#3204,.T.);
#7033=EDGE_CURVE('',#4948,#4864,#3205,.T.);
#7034=EDGE_CURVE('',#5287,#4726,#3206,.T.);
#7035=EDGE_CURVE('',#4725,#5288,#3207,.T.);
#7036=EDGE_CURVE('',#5289,#4722,#3208,.T.);
#7037=EDGE_CURVE('',#4940,#4860,#3209,.T.);
#7038=EDGE_CURVE('',#4721,#5290,#3210,.T.);
#7039=EDGE_CURVE('',#4932,#4924,#3211,.T.);
#7040=EDGE_CURVE('',#5291,#5291,#2585,.T.);
#7041=EDGE_CURVE('',#5291,#5292,#3915,.T.);
#7042=EDGE_CURVE('',#5292,#5292,#2586,.T.);
#7043=EDGE_CURVE('',#5293,#5293,#2587,.T.);
#7044=EDGE_CURVE('',#5293,#5294,#3916,.T.);
#7045=EDGE_CURVE('',#5294,#5294,#2588,.T.);
#7046=EDGE_CURVE('',#5295,#5295,#2589,.T.);
#7047=EDGE_CURVE('',#5295,#5296,#3917,.T.);
#7048=EDGE_CURVE('',#5296,#5296,#2590,.T.);
#7049=EDGE_CURVE('',#5297,#5297,#2591,.T.);
#7050=EDGE_CURVE('',#5297,#5298,#2592,.T.);
#7051=EDGE_CURVE('',#5298,#5299,#2593,.T.);
#7052=EDGE_CURVE('',#5299,#5298,#2594,.T.);
#7053=EDGE_CURVE('',#5299,#5300,#3918,.T.);
#7054=EDGE_CURVE('',#5300,#5300,#2595,.T.);
#7055=EDGE_CURVE('',#5301,#5301,#2596,.T.);
#7056=EDGE_CURVE('',#5302,#5302,#2597,.T.);
#7057=EDGE_CURVE('',#5302,#5301,#3919,.T.);
#7058=EDGE_CURVE('',#5303,#5304,#3920,.T.);
#7059=EDGE_CURVE('',#5305,#5303,#3212,.T.);
#7060=EDGE_CURVE('',#5306,#5305,#2598,.T.);
#7061=EDGE_CURVE('',#5306,#5304,#3213,.T.);
#7062=EDGE_CURVE('',#5307,#5308,#3921,.T.);
#7063=EDGE_CURVE('',#5309,#5307,#3214,.T.);
#7064=EDGE_CURVE('',#5303,#5309,#3215,.T.);
#7065=EDGE_CURVE('',#5304,#5310,#3216,.T.);
#7066=EDGE_CURVE('',#5310,#5308,#3217,.T.);
#7067=EDGE_CURVE('',#5311,#5312,#3922,.T.);
#7068=EDGE_CURVE('',#5313,#5311,#3218,.T.);
#7069=EDGE_CURVE('',#5307,#5313,#3219,.T.);
#7070=EDGE_CURVE('',#5308,#5314,#3220,.T.);
#7071=EDGE_CURVE('',#5314,#5312,#3221,.T.);
#7072=EDGE_CURVE('',#5315,#5316,#3923,.T.);
#7073=EDGE_CURVE('',#5317,#5315,#3222,.T.);
#7074=EDGE_CURVE('',#5311,#5317,#3223,.T.);
#7075=EDGE_CURVE('',#5312,#5318,#3224,.T.);
#7076=EDGE_CURVE('',#5318,#5316,#3225,.T.);
#7077=EDGE_CURVE('',#5319,#5320,#3924,.T.);
#7078=EDGE_CURVE('',#5321,#5319,#3226,.T.);
#7079=EDGE_CURVE('',#5315,#5321,#3227,.T.);
#7080=EDGE_CURVE('',#5316,#5322,#3228,.T.);
#7081=EDGE_CURVE('',#5322,#5320,#3229,.T.);
#7082=EDGE_CURVE('',#5323,#5324,#3925,.T.);
#7083=EDGE_CURVE('',#5325,#5323,#3230,.T.);
#7084=EDGE_CURVE('',#5319,#5325,#3231,.T.);
#7085=EDGE_CURVE('',#5320,#5326,#3232,.T.);
#7086=EDGE_CURVE('',#5326,#5324,#3233,.T.);
#7087=EDGE_CURVE('',#5327,#5328,#3926,.T.);
#7088=EDGE_CURVE('',#5329,#5327,#3234,.T.);
#7089=EDGE_CURVE('',#5323,#5329,#3235,.T.);
#7090=EDGE_CURVE('',#5324,#5330,#3236,.T.);
#7091=EDGE_CURVE('',#5330,#5328,#3237,.T.);
#7092=EDGE_CURVE('',#5331,#5332,#3927,.T.);
#7093=EDGE_CURVE('',#5333,#5331,#3238,.T.);
#7094=EDGE_CURVE('',#5327,#5333,#3239,.T.);
#7095=EDGE_CURVE('',#5328,#5334,#3240,.T.);
#7096=EDGE_CURVE('',#5334,#5332,#3241,.T.);
#7097=EDGE_CURVE('',#5335,#5336,#3928,.T.);
#7098=EDGE_CURVE('',#5337,#5335,#3242,.T.);
#7099=EDGE_CURVE('',#5331,#5337,#3243,.T.);
#7100=EDGE_CURVE('',#5332,#5338,#3244,.T.);
#7101=EDGE_CURVE('',#5338,#5336,#3245,.T.);
#7102=EDGE_CURVE('',#5339,#5340,#3929,.T.);
#7103=EDGE_CURVE('',#5341,#5339,#3246,.T.);
#7104=EDGE_CURVE('',#5335,#5341,#3247,.T.);
#7105=EDGE_CURVE('',#5336,#5342,#3248,.T.);
#7106=EDGE_CURVE('',#5342,#5340,#3249,.T.);
#7107=EDGE_CURVE('',#5343,#5344,#3930,.T.);
#7108=EDGE_CURVE('',#5345,#5343,#3250,.T.);
#7109=EDGE_CURVE('',#5339,#5345,#3251,.T.);
#7110=EDGE_CURVE('',#5340,#5346,#3252,.T.);
#7111=EDGE_CURVE('',#5346,#5344,#3253,.T.);
#7112=EDGE_CURVE('',#5347,#5348,#3931,.T.);
#7113=EDGE_CURVE('',#5349,#5347,#3254,.T.);
#7114=EDGE_CURVE('',#5343,#5349,#3255,.T.);
#7115=EDGE_CURVE('',#5344,#5350,#3256,.T.);
#7116=EDGE_CURVE('',#5350,#5348,#3257,.T.);
#7117=EDGE_CURVE('',#5351,#5352,#3932,.T.);
#7118=EDGE_CURVE('',#5353,#5351,#3258,.T.);
#7119=EDGE_CURVE('',#5347,#5353,#3259,.T.);
#7120=EDGE_CURVE('',#5348,#5354,#3260,.T.);
#7121=EDGE_CURVE('',#5354,#5352,#3261,.T.);
#7122=EDGE_CURVE('',#5355,#5356,#3933,.T.);
#7123=EDGE_CURVE('',#5357,#5355,#3262,.T.);
#7124=EDGE_CURVE('',#5351,#5357,#3263,.T.);
#7125=EDGE_CURVE('',#5352,#5358,#3264,.T.);
#7126=EDGE_CURVE('',#5358,#5356,#3265,.T.);
#7127=EDGE_CURVE('',#5359,#5360,#3934,.T.);
#7128=EDGE_CURVE('',#5361,#5359,#3266,.T.);
#7129=EDGE_CURVE('',#5355,#5361,#3267,.T.);
#7130=EDGE_CURVE('',#5356,#5362,#3268,.T.);
#7131=EDGE_CURVE('',#5362,#5360,#3269,.T.);
#7132=EDGE_CURVE('',#5363,#5364,#3935,.T.);
#7133=EDGE_CURVE('',#5365,#5363,#3270,.T.);
#7134=EDGE_CURVE('',#5359,#5365,#3271,.T.);
#7135=EDGE_CURVE('',#5360,#5366,#3272,.T.);
#7136=EDGE_CURVE('',#5366,#5364,#3273,.T.);
#7137=EDGE_CURVE('',#5367,#5368,#3936,.T.);
#7138=EDGE_CURVE('',#5369,#5367,#3274,.T.);
#7139=EDGE_CURVE('',#5363,#5369,#3275,.T.);
#7140=EDGE_CURVE('',#5364,#5370,#3276,.T.);
#7141=EDGE_CURVE('',#5370,#5368,#3277,.T.);
#7142=EDGE_CURVE('',#5371,#5372,#3937,.T.);
#7143=EDGE_CURVE('',#5373,#5371,#3278,.T.);
#7144=EDGE_CURVE('',#5367,#5373,#3279,.T.);
#7145=EDGE_CURVE('',#5368,#5374,#3280,.T.);
#7146=EDGE_CURVE('',#5374,#5372,#3281,.T.);
#7147=EDGE_CURVE('',#5375,#5376,#3938,.T.);
#7148=EDGE_CURVE('',#5377,#5375,#3282,.T.);
#7149=EDGE_CURVE('',#5371,#5377,#3283,.T.);
#7150=EDGE_CURVE('',#5372,#5378,#3284,.T.);
#7151=EDGE_CURVE('',#5378,#5376,#3285,.T.);
#7152=EDGE_CURVE('',#5379,#5380,#3939,.T.);
#7153=EDGE_CURVE('',#5381,#5379,#3286,.T.);
#7154=EDGE_CURVE('',#5375,#5381,#3287,.T.);
#7155=EDGE_CURVE('',#5376,#5382,#3288,.T.);
#7156=EDGE_CURVE('',#5382,#5380,#3289,.T.);
#7157=EDGE_CURVE('',#5383,#5384,#3940,.T.);
#7158=EDGE_CURVE('',#5385,#5383,#3290,.T.);
#7159=EDGE_CURVE('',#5379,#5385,#3291,.T.);
#7160=EDGE_CURVE('',#5380,#5386,#3292,.T.);
#7161=EDGE_CURVE('',#5386,#5384,#3293,.T.);
#7162=EDGE_CURVE('',#5387,#5388,#3941,.T.);
#7163=EDGE_CURVE('',#5389,#5387,#3294,.T.);
#7164=EDGE_CURVE('',#5383,#5389,#3295,.T.);
#7165=EDGE_CURVE('',#5384,#5390,#3296,.T.);
#7166=EDGE_CURVE('',#5390,#5388,#3297,.T.);
#7167=EDGE_CURVE('',#5391,#5392,#3942,.T.);
#7168=EDGE_CURVE('',#5393,#5391,#3298,.T.);
#7169=EDGE_CURVE('',#5387,#5393,#3299,.T.);
#7170=EDGE_CURVE('',#5388,#5394,#3300,.T.);
#7171=EDGE_CURVE('',#5394,#5392,#3301,.T.);
#7172=EDGE_CURVE('',#5395,#5396,#3943,.T.);
#7173=EDGE_CURVE('',#5397,#5395,#3302,.T.);
#7174=EDGE_CURVE('',#5391,#5397,#3303,.T.);
#7175=EDGE_CURVE('',#5392,#5398,#3304,.T.);
#7176=EDGE_CURVE('',#5398,#5396,#3305,.T.);
#7177=EDGE_CURVE('',#5399,#5400,#3944,.T.);
#7178=EDGE_CURVE('',#5401,#5399,#3306,.T.);
#7179=EDGE_CURVE('',#5395,#5401,#3307,.T.);
#7180=EDGE_CURVE('',#5396,#5402,#3308,.T.);
#7181=EDGE_CURVE('',#5402,#5400,#3309,.T.);
#7182=EDGE_CURVE('',#5403,#5404,#3945,.T.);
#7183=EDGE_CURVE('',#5405,#5403,#3310,.T.);
#7184=EDGE_CURVE('',#5399,#5405,#3311,.T.);
#7185=EDGE_CURVE('',#5400,#5406,#3312,.T.);
#7186=EDGE_CURVE('',#5406,#5404,#3313,.T.);
#7187=EDGE_CURVE('',#5407,#5408,#3946,.T.);
#7188=EDGE_CURVE('',#5409,#5407,#3314,.T.);
#7189=EDGE_CURVE('',#5403,#5409,#3315,.T.);
#7190=EDGE_CURVE('',#5404,#5410,#3316,.T.);
#7191=EDGE_CURVE('',#5410,#5408,#3317,.T.);
#7192=EDGE_CURVE('',#5411,#5412,#3947,.T.);
#7193=EDGE_CURVE('',#5413,#5411,#3318,.T.);
#7194=EDGE_CURVE('',#5407,#5413,#3319,.T.);
#7195=EDGE_CURVE('',#5408,#5414,#3320,.T.);
#7196=EDGE_CURVE('',#5414,#5412,#3321,.T.);
#7197=EDGE_CURVE('',#5415,#5416,#3948,.T.);
#7198=EDGE_CURVE('',#5417,#5415,#3322,.T.);
#7199=EDGE_CURVE('',#5411,#5417,#3323,.T.);
#7200=EDGE_CURVE('',#5412,#5418,#3324,.T.);
#7201=EDGE_CURVE('',#5418,#5416,#3325,.T.);
#7202=EDGE_CURVE('',#5419,#5420,#3949,.T.);
#7203=EDGE_CURVE('',#5421,#5419,#3326,.T.);
#7204=EDGE_CURVE('',#5415,#5421,#3327,.T.);
#7205=EDGE_CURVE('',#5416,#5422,#3328,.T.);
#7206=EDGE_CURVE('',#5422,#5420,#3329,.T.);
#7207=EDGE_CURVE('',#5423,#5424,#3950,.T.);
#7208=EDGE_CURVE('',#5425,#5423,#3330,.T.);
#7209=EDGE_CURVE('',#5419,#5425,#3331,.T.);
#7210=EDGE_CURVE('',#5420,#5426,#3332,.T.);
#7211=EDGE_CURVE('',#5426,#5424,#3333,.T.);
#7212=EDGE_CURVE('',#5427,#5428,#3951,.T.);
#7213=EDGE_CURVE('',#5429,#5427,#3334,.T.);
#7214=EDGE_CURVE('',#5423,#5429,#3335,.T.);
#7215=EDGE_CURVE('',#5424,#5430,#3336,.T.);
#7216=EDGE_CURVE('',#5430,#5428,#3337,.T.);
#7217=EDGE_CURVE('',#5431,#5432,#3952,.T.);
#7218=EDGE_CURVE('',#5433,#5431,#3338,.T.);
#7219=EDGE_CURVE('',#5427,#5433,#3339,.T.);
#7220=EDGE_CURVE('',#5428,#5434,#3340,.T.);
#7221=EDGE_CURVE('',#5434,#5432,#3341,.T.);
#7222=EDGE_CURVE('',#5435,#5436,#3953,.T.);
#7223=EDGE_CURVE('',#5437,#5435,#3342,.T.);
#7224=EDGE_CURVE('',#5431,#5437,#3343,.T.);
#7225=EDGE_CURVE('',#5432,#5438,#3344,.T.);
#7226=EDGE_CURVE('',#5438,#5436,#3345,.T.);
#7227=EDGE_CURVE('',#5439,#5440,#3954,.T.);
#7228=EDGE_CURVE('',#5441,#5439,#3346,.T.);
#7229=EDGE_CURVE('',#5435,#5441,#3347,.T.);
#7230=EDGE_CURVE('',#5436,#5442,#3348,.T.);
#7231=EDGE_CURVE('',#5442,#5440,#3349,.T.);
#7232=EDGE_CURVE('',#5443,#5444,#3955,.T.);
#7233=EDGE_CURVE('',#5445,#5443,#3350,.T.);
#7234=EDGE_CURVE('',#5439,#5445,#3351,.T.);
#7235=EDGE_CURVE('',#5440,#5446,#3352,.T.);
#7236=EDGE_CURVE('',#5446,#5444,#3353,.T.);
#7237=EDGE_CURVE('',#5447,#5448,#3956,.T.);
#7238=EDGE_CURVE('',#5449,#5447,#3354,.T.);
#7239=EDGE_CURVE('',#5443,#5449,#3355,.T.);
#7240=EDGE_CURVE('',#5444,#5450,#3356,.T.);
#7241=EDGE_CURVE('',#5450,#5448,#3357,.T.);
#7242=EDGE_CURVE('',#5451,#5452,#3957,.T.);
#7243=EDGE_CURVE('',#5453,#5451,#3358,.T.);
#7244=EDGE_CURVE('',#5447,#5453,#3359,.T.);
#7245=EDGE_CURVE('',#5448,#5454,#3360,.T.);
#7246=EDGE_CURVE('',#5454,#5452,#3361,.T.);
#7247=EDGE_CURVE('',#5455,#5456,#3958,.T.);
#7248=EDGE_CURVE('',#5457,#5455,#3362,.T.);
#7249=EDGE_CURVE('',#5451,#5457,#3363,.T.);
#7250=EDGE_CURVE('',#5452,#5458,#3364,.T.);
#7251=EDGE_CURVE('',#5458,#5456,#3365,.T.);
#7252=EDGE_CURVE('',#5459,#5460,#3959,.T.);
#7253=EDGE_CURVE('',#5461,#5459,#3366,.T.);
#7254=EDGE_CURVE('',#5455,#5461,#3367,.T.);
#7255=EDGE_CURVE('',#5456,#5462,#3368,.T.);
#7256=EDGE_CURVE('',#5462,#5460,#3369,.T.);
#7257=EDGE_CURVE('',#5463,#5464,#3960,.T.);
#7258=EDGE_CURVE('',#5465,#5463,#3370,.T.);
#7259=EDGE_CURVE('',#5459,#5465,#3371,.T.);
#7260=EDGE_CURVE('',#5460,#5466,#3372,.T.);
#7261=EDGE_CURVE('',#5466,#5464,#3373,.T.);
#7262=EDGE_CURVE('',#5467,#5468,#3961,.T.);
#7263=EDGE_CURVE('',#5469,#5467,#3374,.T.);
#7264=EDGE_CURVE('',#5463,#5469,#3375,.T.);
#7265=EDGE_CURVE('',#5464,#5470,#3376,.T.);
#7266=EDGE_CURVE('',#5470,#5468,#3377,.T.);
#7267=EDGE_CURVE('',#5471,#5472,#3962,.T.);
#7268=EDGE_CURVE('',#5473,#5471,#3378,.T.);
#7269=EDGE_CURVE('',#5467,#5473,#3379,.T.);
#7270=EDGE_CURVE('',#5468,#5474,#3380,.T.);
#7271=EDGE_CURVE('',#5474,#5472,#3381,.T.);
#7272=EDGE_CURVE('',#5475,#5476,#3963,.T.);
#7273=EDGE_CURVE('',#5477,#5475,#3382,.T.);
#7274=EDGE_CURVE('',#5471,#5477,#3383,.T.);
#7275=EDGE_CURVE('',#5472,#5478,#3384,.T.);
#7276=EDGE_CURVE('',#5478,#5476,#3385,.T.);
#7277=EDGE_CURVE('',#5479,#5480,#3964,.T.);
#7278=EDGE_CURVE('',#5481,#5479,#3386,.T.);
#7279=EDGE_CURVE('',#5475,#5481,#3387,.T.);
#7280=EDGE_CURVE('',#5476,#5482,#3388,.T.);
#7281=EDGE_CURVE('',#5482,#5480,#3389,.T.);
#7282=EDGE_CURVE('',#5483,#5484,#3965,.T.);
#7283=EDGE_CURVE('',#5485,#5483,#3390,.T.);
#7284=EDGE_CURVE('',#5479,#5485,#3391,.T.);
#7285=EDGE_CURVE('',#5480,#5486,#3392,.T.);
#7286=EDGE_CURVE('',#5486,#5484,#3393,.T.);
#7287=EDGE_CURVE('',#5487,#5488,#3966,.T.);
#7288=EDGE_CURVE('',#5489,#5487,#3394,.T.);
#7289=EDGE_CURVE('',#5483,#5489,#3395,.T.);
#7290=EDGE_CURVE('',#5484,#5490,#3396,.T.);
#7291=EDGE_CURVE('',#5490,#5488,#3397,.T.);
#7292=EDGE_CURVE('',#5491,#5492,#3967,.T.);
#7293=EDGE_CURVE('',#5493,#5491,#3398,.T.);
#7294=EDGE_CURVE('',#5487,#5493,#3399,.T.);
#7295=EDGE_CURVE('',#5488,#5494,#3400,.T.);
#7296=EDGE_CURVE('',#5494,#5492,#3401,.T.);
#7297=EDGE_CURVE('',#5495,#5496,#3968,.T.);
#7298=EDGE_CURVE('',#5497,#5495,#3402,.T.);
#7299=EDGE_CURVE('',#5491,#5497,#3403,.T.);
#7300=EDGE_CURVE('',#5492,#5498,#3404,.T.);
#7301=EDGE_CURVE('',#5498,#5496,#3405,.T.);
#7302=EDGE_CURVE('',#5499,#5500,#3969,.T.);
#7303=EDGE_CURVE('',#5501,#5499,#3406,.T.);
#7304=EDGE_CURVE('',#5495,#5501,#3407,.T.);
#7305=EDGE_CURVE('',#5496,#5502,#3408,.T.);
#7306=EDGE_CURVE('',#5502,#5500,#3409,.T.);
#7307=EDGE_CURVE('',#5503,#5504,#3970,.T.);
#7308=EDGE_CURVE('',#5505,#5503,#3410,.T.);
#7309=EDGE_CURVE('',#5499,#5505,#3411,.T.);
#7310=EDGE_CURVE('',#5500,#5506,#3412,.T.);
#7311=EDGE_CURVE('',#5506,#5504,#3413,.T.);
#7312=EDGE_CURVE('',#5507,#5508,#3971,.T.);
#7313=EDGE_CURVE('',#5509,#5507,#3414,.T.);
#7314=EDGE_CURVE('',#5503,#5509,#3415,.T.);
#7315=EDGE_CURVE('',#5504,#5510,#3416,.T.);
#7316=EDGE_CURVE('',#5510,#5508,#3417,.T.);
#7317=EDGE_CURVE('',#5511,#5512,#3972,.T.);
#7318=EDGE_CURVE('',#5513,#5511,#3418,.T.);
#7319=EDGE_CURVE('',#5507,#5513,#3419,.T.);
#7320=EDGE_CURVE('',#5508,#5514,#3420,.T.);
#7321=EDGE_CURVE('',#5514,#5512,#3421,.T.);
#7322=EDGE_CURVE('',#5515,#5516,#3973,.T.);
#7323=EDGE_CURVE('',#5517,#5515,#3422,.T.);
#7324=EDGE_CURVE('',#5511,#5517,#3423,.T.);
#7325=EDGE_CURVE('',#5512,#5518,#3424,.T.);
#7326=EDGE_CURVE('',#5518,#5516,#3425,.T.);
#7327=EDGE_CURVE('',#5519,#5520,#3974,.T.);
#7328=EDGE_CURVE('',#5521,#5519,#3426,.T.);
#7329=EDGE_CURVE('',#5515,#5521,#3427,.T.);
#7330=EDGE_CURVE('',#5516,#5522,#3428,.T.);
#7331=EDGE_CURVE('',#5522,#5520,#3429,.T.);
#7332=EDGE_CURVE('',#5523,#5524,#3975,.T.);
#7333=EDGE_CURVE('',#5525,#5523,#3430,.T.);
#7334=EDGE_CURVE('',#5519,#5525,#3431,.T.);
#7335=EDGE_CURVE('',#5520,#5526,#3432,.T.);
#7336=EDGE_CURVE('',#5526,#5524,#3433,.T.);
#7337=EDGE_CURVE('',#5527,#5528,#3976,.T.);
#7338=EDGE_CURVE('',#5529,#5527,#3434,.T.);
#7339=EDGE_CURVE('',#5523,#5529,#3435,.T.);
#7340=EDGE_CURVE('',#5524,#5530,#3436,.T.);
#7341=EDGE_CURVE('',#5530,#5528,#3437,.T.);
#7342=EDGE_CURVE('',#5531,#5532,#3977,.T.);
#7343=EDGE_CURVE('',#5533,#5531,#3438,.T.);
#7344=EDGE_CURVE('',#5527,#5533,#3439,.T.);
#7345=EDGE_CURVE('',#5528,#5534,#3440,.T.);
#7346=EDGE_CURVE('',#5534,#5532,#3441,.T.);
#7347=EDGE_CURVE('',#5535,#5536,#3978,.T.);
#7348=EDGE_CURVE('',#5537,#5535,#3442,.T.);
#7349=EDGE_CURVE('',#5531,#5537,#3443,.T.);
#7350=EDGE_CURVE('',#5532,#5538,#3444,.T.);
#7351=EDGE_CURVE('',#5538,#5536,#3445,.T.);
#7352=EDGE_CURVE('',#5539,#5540,#3979,.T.);
#7353=EDGE_CURVE('',#5541,#5539,#3446,.T.);
#7354=EDGE_CURVE('',#5535,#5541,#3447,.T.);
#7355=EDGE_CURVE('',#5536,#5542,#3448,.T.);
#7356=EDGE_CURVE('',#5542,#5540,#3449,.T.);
#7357=EDGE_CURVE('',#5543,#5544,#3450,.T.);
#7358=EDGE_CURVE('',#5545,#5544,#2599,.T.);
#7359=EDGE_CURVE('',#5545,#5546,#3451,.T.);
#7360=EDGE_CURVE('',#5546,#5547,#3452,.T.);
#7361=EDGE_CURVE('',#5547,#5548,#3453,.T.);
#7362=EDGE_CURVE('',#5548,#5549,#3454,.T.);
#7363=EDGE_CURVE('',#5549,#5550,#3455,.T.);
#7364=EDGE_CURVE('',#5550,#5551,#3456,.T.);
#7365=EDGE_CURVE('',#5551,#5552,#3457,.T.);
#7366=EDGE_CURVE('',#5552,#5553,#3458,.T.);
#7367=EDGE_CURVE('',#5553,#5554,#3459,.T.);
#7368=EDGE_CURVE('',#5554,#5555,#3460,.T.);
#7369=EDGE_CURVE('',#5555,#5556,#3461,.T.);
#7370=EDGE_CURVE('',#5556,#5557,#3462,.T.);
#7371=EDGE_CURVE('',#5557,#5558,#3463,.T.);
#7372=EDGE_CURVE('',#5558,#5559,#3464,.T.);
#7373=EDGE_CURVE('',#5559,#5560,#3465,.T.);
#7374=EDGE_CURVE('',#5560,#5561,#3466,.T.);
#7375=EDGE_CURVE('',#5561,#5562,#3467,.T.);
#7376=EDGE_CURVE('',#5562,#5563,#3468,.T.);
#7377=EDGE_CURVE('',#5563,#5564,#3469,.T.);
#7378=EDGE_CURVE('',#5564,#5565,#3470,.T.);
#7379=EDGE_CURVE('',#5565,#5566,#3471,.T.);
#7380=EDGE_CURVE('',#5566,#5567,#3472,.T.);
#7381=EDGE_CURVE('',#5567,#5568,#3473,.T.);
#7382=EDGE_CURVE('',#5568,#5569,#3474,.T.);
#7383=EDGE_CURVE('',#5569,#5570,#3475,.T.);
#7384=EDGE_CURVE('',#5570,#5571,#3476,.T.);
#7385=EDGE_CURVE('',#5571,#5572,#3477,.T.);
#7386=EDGE_CURVE('',#5572,#5573,#3478,.T.);
#7387=EDGE_CURVE('',#5573,#5574,#3479,.T.);
#7388=EDGE_CURVE('',#5574,#5575,#3480,.T.);
#7389=EDGE_CURVE('',#5575,#5576,#3481,.T.);
#7390=EDGE_CURVE('',#5576,#5577,#3482,.T.);
#7391=EDGE_CURVE('',#5577,#5578,#3483,.T.);
#7392=EDGE_CURVE('',#5578,#5579,#3484,.T.);
#7393=EDGE_CURVE('',#5579,#5580,#3485,.T.);
#7394=EDGE_CURVE('',#5580,#5581,#3486,.T.);
#7395=EDGE_CURVE('',#5581,#5582,#3487,.T.);
#7396=EDGE_CURVE('',#5582,#5583,#3488,.T.);
#7397=EDGE_CURVE('',#5583,#5584,#3489,.T.);
#7398=EDGE_CURVE('',#5584,#5585,#3490,.T.);
#7399=EDGE_CURVE('',#5585,#5586,#3491,.T.);
#7400=EDGE_CURVE('',#5587,#5586,#2600,.F.);
#7401=EDGE_CURVE('',#5587,#5588,#3492,.T.);
#7402=EDGE_CURVE('',#5588,#5589,#3493,.T.);
#7403=EDGE_CURVE('',#5589,#5590,#3494,.T.);
#7404=EDGE_CURVE('',#5590,#5591,#3495,.T.);
#7405=EDGE_CURVE('',#5591,#5592,#3496,.T.);
#7406=EDGE_CURVE('',#5592,#5593,#3497,.T.);
#7407=EDGE_CURVE('',#5593,#5594,#3498,.T.);
#7408=EDGE_CURVE('',#5594,#5595,#3499,.T.);
#7409=EDGE_CURVE('',#5595,#5596,#3500,.T.);
#7410=EDGE_CURVE('',#5596,#5597,#3501,.T.);
#7411=EDGE_CURVE('',#5597,#5598,#3502,.T.);
#7412=EDGE_CURVE('',#5598,#5599,#3503,.T.);
#7413=EDGE_CURVE('',#5599,#5600,#3504,.T.);
#7414=EDGE_CURVE('',#5600,#5601,#3505,.T.);
#7415=EDGE_CURVE('',#5601,#5602,#3506,.T.);
#7416=EDGE_CURVE('',#5602,#5603,#3507,.T.);
#7417=EDGE_CURVE('',#5603,#5604,#3508,.T.);
#7418=EDGE_CURVE('',#5604,#5605,#3509,.T.);
#7419=EDGE_CURVE('',#5605,#5606,#3510,.T.);
#7420=EDGE_CURVE('',#5606,#5607,#3511,.T.);
#7421=EDGE_CURVE('',#5607,#5608,#3512,.T.);
#7422=EDGE_CURVE('',#5608,#5609,#3513,.T.);
#7423=EDGE_CURVE('',#5609,#5610,#3514,.T.);
#7424=EDGE_CURVE('',#5610,#5611,#3515,.T.);
#7425=EDGE_CURVE('',#5611,#5612,#3516,.T.);
#7426=EDGE_CURVE('',#5612,#5613,#3517,.T.);
#7427=EDGE_CURVE('',#5613,#5614,#3518,.T.);
#7428=EDGE_CURVE('',#5614,#5615,#3519,.T.);
#7429=EDGE_CURVE('',#5615,#5616,#3520,.T.);
#7430=EDGE_CURVE('',#5616,#5617,#3521,.T.);
#7431=EDGE_CURVE('',#5617,#5618,#3522,.T.);
#7432=EDGE_CURVE('',#5618,#5619,#3523,.T.);
#7433=EDGE_CURVE('',#5619,#5620,#3524,.T.);
#7434=EDGE_CURVE('',#5620,#5621,#3525,.T.);
#7435=EDGE_CURVE('',#5621,#5622,#3526,.T.);
#7436=EDGE_CURVE('',#5622,#5623,#3527,.T.);
#7437=EDGE_CURVE('',#5623,#5624,#3528,.T.);
#7438=EDGE_CURVE('',#5624,#5625,#3529,.T.);
#7439=EDGE_CURVE('',#5625,#5626,#3530,.T.);
#7440=EDGE_CURVE('',#5626,#5627,#3531,.T.);
#7441=EDGE_CURVE('',#5627,#5628,#3532,.T.);
#7442=EDGE_CURVE('',#5628,#5629,#3533,.T.);
#7443=EDGE_CURVE('',#5629,#5630,#3534,.T.);
#7444=EDGE_CURVE('',#5630,#5631,#3535,.T.);
#7445=EDGE_CURVE('',#5631,#5632,#3536,.T.);
#7446=EDGE_CURVE('',#5632,#5633,#3537,.T.);
#7447=EDGE_CURVE('',#5633,#5634,#3538,.T.);
#7448=EDGE_CURVE('',#5634,#5635,#3539,.T.);
#7449=EDGE_CURVE('',#5635,#5636,#3540,.T.);
#7450=EDGE_CURVE('',#5636,#5637,#3541,.T.);
#7451=EDGE_CURVE('',#5637,#5638,#3542,.T.);
#7452=EDGE_CURVE('',#5638,#5639,#3543,.T.);
#7453=EDGE_CURVE('',#5639,#5640,#3544,.T.);
#7454=EDGE_CURVE('',#5640,#5641,#3545,.T.);
#7455=EDGE_CURVE('',#5641,#5642,#3546,.T.);
#7456=EDGE_CURVE('',#5642,#5643,#3547,.T.);
#7457=EDGE_CURVE('',#5643,#5644,#3548,.T.);
#7458=EDGE_CURVE('',#5644,#5645,#3549,.T.);
#7459=EDGE_CURVE('',#5645,#5646,#3550,.T.);
#7460=EDGE_CURVE('',#5646,#5543,#3551,.T.);
#7461=EDGE_CURVE('',#5540,#5647,#3552,.T.);
#7462=EDGE_CURVE('',#5647,#5648,#3553,.T.);
#7463=EDGE_CURVE('',#5649,#5648,#2601,.T.);
#7464=EDGE_CURVE('',#5650,#5649,#3554,.T.);
#7465=EDGE_CURVE('',#5539,#5650,#3555,.T.);
#7466=EDGE_CURVE('',#5586,#5649,#3556,.T.);
#7467=EDGE_CURVE('',#5305,#5545,#3557,.T.);
#7468=EDGE_CURVE('',#5648,#5587,#3558,.T.);
#7469=EDGE_CURVE('',#5544,#5306,#3559,.T.);
#7470=EDGE_CURVE('',#5651,#5651,#2602,.T.);
#7471=EDGE_CURVE('',#5651,#5652,#3980,.T.);
#7472=EDGE_CURVE('',#5652,#5652,#2603,.T.);
#7473=EDGE_CURVE('',#5653,#5653,#2604,.T.);
#7474=EDGE_CURVE('',#5653,#5654,#3981,.T.);
#7475=EDGE_CURVE('',#5654,#5654,#2605,.T.);
#7476=EDGE_CURVE('',#5655,#5655,#2606,.T.);
#7477=EDGE_CURVE('',#5655,#5656,#3982,.T.);
#7478=EDGE_CURVE('',#5656,#5656,#2607,.T.);
#7479=EDGE_CURVE('',#5657,#5657,#2608,.T.);
#7480=EDGE_CURVE('',#5657,#5658,#3983,.T.);
#7481=EDGE_CURVE('',#5658,#5658,#2609,.T.);
#7482=EDGE_CURVE('',#5659,#5660,#2610,.T.);
#7483=EDGE_CURVE('',#5660,#5661,#2611,.T.);
#7484=EDGE_CURVE('',#5661,#5661,#2612,.T.);
#7485=EDGE_CURVE('',#5660,#5659,#2613,.T.);
#7486=EDGE_CURVE('',#5662,#5663,#2614,.T.);
#7487=EDGE_CURVE('',#5663,#5662,#2615,.T.);
#7488=EDGE_CURVE('',#5663,#5659,#3984,.T.);
#7489=EDGE_CURVE('',#5664,#5664,#2616,.T.);
#7490=EDGE_CURVE('',#5664,#5662,#2617,.T.);
#7491=EDGE_CURVE('',#5665,#5666,#3985,.T.);
#7492=EDGE_CURVE('',#5665,#5667,#3560,.T.);
#7493=EDGE_CURVE('',#5667,#5668,#3561,.T.);
#7494=EDGE_CURVE('',#5668,#5669,#2618,.T.);
#7495=EDGE_CURVE('',#5669,#5670,#3562,.T.);
#7496=EDGE_CURVE('',#5670,#5666,#3563,.T.);
#7497=EDGE_CURVE('',#5671,#5672,#3986,.T.);
#7498=EDGE_CURVE('',#5671,#5673,#3564,.T.);
#7499=EDGE_CURVE('',#5673,#5674,#3565,.T.);
#7500=EDGE_CURVE('',#5674,#5665,#3566,.T.);
#7501=EDGE_CURVE('',#5666,#5675,#3567,.T.);
#7502=EDGE_CURVE('',#5675,#5676,#3568,.T.);
#7503=EDGE_CURVE('',#5676,#5672,#3569,.T.);
#7504=EDGE_CURVE('',#5677,#5678,#3987,.T.);
#7505=EDGE_CURVE('',#5677,#5679,#3570,.T.);
#7506=EDGE_CURVE('',#5679,#5680,#3571,.T.);
#7507=EDGE_CURVE('',#5680,#5671,#3572,.T.);
#7508=EDGE_CURVE('',#5672,#5681,#3573,.T.);
#7509=EDGE_CURVE('',#5681,#5682,#3574,.T.);
#7510=EDGE_CURVE('',#5682,#5678,#3575,.T.);
#7511=EDGE_CURVE('',#5683,#5684,#3988,.T.);
#7512=EDGE_CURVE('',#5683,#5685,#3576,.T.);
#7513=EDGE_CURVE('',#5685,#5686,#3577,.T.);
#7514=EDGE_CURVE('',#5686,#5677,#3578,.T.);
#7515=EDGE_CURVE('',#5678,#5687,#3579,.T.);
#7516=EDGE_CURVE('',#5687,#5688,#3580,.T.);
#7517=EDGE_CURVE('',#5688,#5684,#3581,.T.);
#7518=EDGE_CURVE('',#5689,#5690,#3989,.T.);
#7519=EDGE_CURVE('',#5689,#5691,#3582,.T.);
#7520=EDGE_CURVE('',#5691,#5692,#3583,.T.);
#7521=EDGE_CURVE('',#5692,#5683,#3584,.T.);
#7522=EDGE_CURVE('',#5684,#5693,#3585,.T.);
#7523=EDGE_CURVE('',#5693,#5694,#3586,.T.);
#7524=EDGE_CURVE('',#5694,#5690,#3587,.T.);
#7525=EDGE_CURVE('',#5695,#5696,#3990,.T.);
#7526=EDGE_CURVE('',#5695,#5697,#2619,.T.);
#7527=EDGE_CURVE('',#5697,#5698,#3588,.T.);
#7528=EDGE_CURVE('',#5698,#5699,#3589,.T.);
#7529=EDGE_CURVE('',#5699,#5689,#3590,.T.);
#7530=EDGE_CURVE('',#5690,#5700,#3591,.T.);
#7531=EDGE_CURVE('',#5700,#5701,#3592,.T.);
#7532=EDGE_CURVE('',#5701,#5696,#3593,.T.);
#7533=EDGE_CURVE('',#5696,#5702,#3594,.T.);
#7534=EDGE_CURVE('',#5702,#5695,#2620,.T.);
#7535=EDGE_CURVE('',#5703,#5704,#3595,.T.);
#7536=EDGE_CURVE('',#5705,#5703,#3596,.T.);
#7537=EDGE_CURVE('',#5706,#5705,#238,.T.);
#7538=EDGE_CURVE('',#5669,#5706,#3597,.T.);
#7539=EDGE_CURVE('',#5704,#5668,#3598,.T.);
#7540=EDGE_CURVE('',#5707,#5707,#2621,.T.);
#7541=EDGE_CURVE('',#5670,#5706,#3991,.T.);
#7542=EDGE_CURVE('',#5705,#5708,#3599,.T.);
#7543=EDGE_CURVE('',#5675,#5708,#3992,.T.);
#7544=EDGE_CURVE('',#5703,#5709,#3600,.T.);
#7545=EDGE_CURVE('',#5708,#5709,#3993,.T.);
#7546=EDGE_CURVE('',#5710,#5702,#3601,.T.);
#7547=EDGE_CURVE('',#5711,#5710,#3602,.T.);
#7548=EDGE_CURVE('',#5712,#5711,#3603,.T.);
#7549=EDGE_CURVE('',#5713,#5712,#239,.T.);
#7550=EDGE_CURVE('',#5697,#5713,#3604,.T.);
#7551=EDGE_CURVE('',#5714,#5714,#2622,.T.);
#7552=EDGE_CURVE('',#5715,#5711,#3605,.T.);
#7553=EDGE_CURVE('',#5715,#5716,#3994,.T.);
#7554=EDGE_CURVE('',#5716,#5712,#3606,.T.);
#7555=EDGE_CURVE('',#5710,#5715,#3995,.T.);
#7556=EDGE_CURVE('',#5701,#5717,#3996,.T.);
#7557=EDGE_CURVE('',#5717,#5715,#3607,.T.);
#7558=EDGE_CURVE('',#5718,#5718,#2623,.T.);
#7559=EDGE_CURVE('',#5718,#5707,#3997,.T.);
#7560=EDGE_CURVE('',#5714,#5719,#3998,.T.);
#7561=EDGE_CURVE('',#5719,#5719,#2624,.T.);
#7562=EDGE_CURVE('',#5713,#5698,#3999,.T.);
#7563=EDGE_CURVE('',#5716,#5699,#4000,.T.);
#7564=EDGE_CURVE('',#5720,#5716,#3608,.T.);
#7565=EDGE_CURVE('',#5720,#5691,#4001,.T.);
#7566=EDGE_CURVE('',#5717,#5720,#4002,.T.);
#7567=EDGE_CURVE('',#5694,#5721,#4003,.T.);
#7568=EDGE_CURVE('',#5721,#5722,#3609,.T.);
#7569=EDGE_CURVE('',#5700,#5722,#4004,.T.);
#7570=EDGE_CURVE('',#5723,#5692,#4005,.T.);
#7571=EDGE_CURVE('',#5724,#5723,#3610,.T.);
#7572=EDGE_CURVE('',#5724,#5685,#4006,.T.);
#7573=EDGE_CURVE('',#5721,#5724,#4007,.T.);
#7574=EDGE_CURVE('',#5722,#5723,#4008,.T.);
#7575=EDGE_CURVE('',#5688,#5725,#4009,.T.);
#7576=EDGE_CURVE('',#5725,#5726,#3611,.T.);
#7577=EDGE_CURVE('',#5693,#5726,#4010,.T.);
#7578=EDGE_CURVE('',#5727,#5686,#4011,.T.);
#7579=EDGE_CURVE('',#5728,#5727,#3612,.T.);
#7580=EDGE_CURVE('',#5728,#5679,#4012,.T.);
#7581=EDGE_CURVE('',#5725,#5728,#4013,.T.);
#7582=EDGE_CURVE('',#5726,#5727,#4014,.T.);
#7583=EDGE_CURVE('',#5682,#5729,#4015,.T.);
#7584=EDGE_CURVE('',#5729,#5730,#3613,.T.);
#7585=EDGE_CURVE('',#5687,#5730,#4016,.T.);
#7586=EDGE_CURVE('',#5731,#5680,#4017,.T.);
#7587=EDGE_CURVE('',#5732,#5731,#3614,.T.);
#7588=EDGE_CURVE('',#5732,#5673,#4018,.T.);
#7589=EDGE_CURVE('',#5729,#5732,#4019,.T.);
#7590=EDGE_CURVE('',#5730,#5731,#4020,.T.);
#7591=EDGE_CURVE('',#5676,#5733,#4021,.T.);
#7592=EDGE_CURVE('',#5733,#5734,#3615,.T.);
#7593=EDGE_CURVE('',#5681,#5734,#4022,.T.);
#7594=EDGE_CURVE('',#5735,#5674,#4023,.T.);
#7595=EDGE_CURVE('',#5736,#5735,#3616,.T.);
#7596=EDGE_CURVE('',#5736,#5667,#4024,.T.);
#7597=EDGE_CURVE('',#5733,#5736,#4025,.T.);
#7598=EDGE_CURVE('',#5734,#5735,#4026,.T.);
#7599=EDGE_CURVE('',#5709,#5704,#4027,.T.);
#7600=EDGE_CURVE('',#5722,#5717,#3617,.T.);
#7601=EDGE_CURVE('',#5723,#5720,#3618,.T.);
#7602=EDGE_CURVE('',#5726,#5721,#3619,.T.);
#7603=EDGE_CURVE('',#5727,#5724,#3620,.T.);
#7604=EDGE_CURVE('',#5730,#5725,#3621,.T.);
#7605=EDGE_CURVE('',#5731,#5728,#3622,.T.);
#7606=EDGE_CURVE('',#5734,#5729,#3623,.T.);
#7607=EDGE_CURVE('',#5735,#5732,#3624,.T.);
#7608=EDGE_CURVE('',#5708,#5733,#3625,.T.);
#7609=EDGE_CURVE('',#5709,#5736,#3626,.T.);
#7610=EDGE_CURVE('',#5737,#5737,#2625,.T.);
#7611=EDGE_CURVE('',#5737,#5738,#2626,.T.);
#7612=EDGE_CURVE('',#5738,#5739,#2627,.T.);
#7613=EDGE_CURVE('',#5739,#5738,#2628,.T.);
#7614=EDGE_CURVE('',#5739,#5740,#4028,.T.);
#7615=EDGE_CURVE('',#5740,#5740,#2629,.T.);
#7616=EDGE_CURVE('',#5741,#5741,#2630,.T.);
#7617=EDGE_CURVE('',#5742,#5742,#2631,.T.);
#7618=EDGE_CURVE('',#5743,#5743,#2632,.T.);
#7619=EDGE_CURVE('',#5744,#5744,#2633,.T.);
#7620=EDGE_CURVE('',#5745,#5745,#2634,.T.);
#7621=EDGE_CURVE('',#5741,#5746,#4029,.T.);
#7622=EDGE_CURVE('',#5746,#5746,#2635,.T.);
#7623=EDGE_CURVE('',#5742,#5747,#4030,.T.);
#7624=EDGE_CURVE('',#5747,#5747,#2636,.T.);
#7625=EDGE_CURVE('',#5743,#5748,#4031,.T.);
#7626=EDGE_CURVE('',#5748,#5748,#2637,.T.);
#7627=EDGE_CURVE('',#5744,#5749,#4032,.T.);
#7628=EDGE_CURVE('',#5749,#5749,#2638,.T.);
#7629=EDGE_CURVE('',#5750,#5750,#2639,.T.);
#7630=EDGE_CURVE('',#5750,#5745,#4033,.T.);
#7631=EDGE_CURVE('',#5751,#5751,#2640,.T.);
#7632=EDGE_CURVE('',#5751,#5752,#4034,.T.);
#7633=EDGE_CURVE('',#5752,#5752,#2641,.T.);
#7634=EDGE_CURVE('',#5753,#5753,#2642,.T.);
#7635=EDGE_CURVE('',#5753,#5754,#4035,.T.);
#7636=EDGE_CURVE('',#5754,#5754,#2643,.T.);
#7637=EDGE_CURVE('',#5755,#5755,#2644,.T.);
#7638=EDGE_CURVE('',#5755,#5756,#4036,.T.);
#7639=EDGE_CURVE('',#5756,#5756,#2645,.T.);
#7640=EDGE_CURVE('',#5757,#5757,#2646,.T.);
#7641=EDGE_CURVE('',#5757,#5758,#4037,.T.);
#7642=EDGE_CURVE('',#5758,#5758,#2647,.T.);
#7643=EDGE_CURVE('',#5759,#5759,#2648,.T.);
#7644=EDGE_CURVE('',#5759,#5760,#4038,.T.);
#7645=EDGE_CURVE('',#5760,#5760,#2649,.T.);
#7646=EDGE_CURVE('',#5761,#5761,#2650,.T.);
#7647=EDGE_CURVE('',#5761,#5762,#4039,.T.);
#7648=EDGE_CURVE('',#5762,#5762,#2651,.T.);
#7649=EDGE_CURVE('',#5763,#5763,#2652,.T.);
#7650=EDGE_CURVE('',#5763,#5764,#4040,.T.);
#7651=EDGE_CURVE('',#5764,#5764,#2653,.T.);
#7652=EDGE_CURVE('',#5765,#5765,#2654,.T.);
#7653=EDGE_CURVE('',#5765,#5766,#4041,.T.);
#7654=EDGE_CURVE('',#5766,#5766,#2655,.T.);
#7655=EDGE_CURVE('',#5767,#5767,#2656,.T.);
#7656=EDGE_CURVE('',#5767,#5768,#4042,.T.);
#7657=EDGE_CURVE('',#5768,#5768,#2657,.T.);
#7658=EDGE_CURVE('',#5769,#5769,#2658,.T.);
#7659=EDGE_CURVE('',#5769,#5770,#4043,.T.);
#7660=EDGE_CURVE('',#5770,#5770,#2659,.T.);
#7661=EDGE_CURVE('',#5771,#5771,#2660,.T.);
#7662=EDGE_CURVE('',#5771,#5772,#4044,.T.);
#7663=EDGE_CURVE('',#5772,#5772,#2661,.T.);
#7664=EDGE_CURVE('',#5773,#5773,#2662,.T.);
#7665=EDGE_CURVE('',#5773,#5774,#4045,.T.);
#7666=EDGE_CURVE('',#5774,#5774,#2663,.T.);
#7667=EDGE_CURVE('',#5775,#5776,#2664,.T.);
#7668=EDGE_CURVE('',#5776,#5777,#4046,.T.);
#7669=EDGE_CURVE('',#5777,#5778,#2665,.T.);
#7670=EDGE_CURVE('',#5778,#5775,#4047,.T.);
#7671=EDGE_CURVE('',#5777,#5779,#4048,.T.);
#7672=EDGE_CURVE('',#5780,#5779,#2666,.T.);
#7673=EDGE_CURVE('',#5780,#5781,#4049,.T.);
#7674=EDGE_CURVE('',#5782,#5781,#2667,.T.);
#7675=EDGE_CURVE('',#5782,#5783,#4050,.T.);
#7676=EDGE_CURVE('',#5783,#5784,#4051,.T.);
#7677=EDGE_CURVE('',#5784,#5785,#4052,.T.);
#7678=EDGE_CURVE('',#5785,#5786,#4053,.T.);
#7679=EDGE_CURVE('',#5786,#5787,#4054,.T.);
#7680=EDGE_CURVE('',#5787,#5788,#2668,.T.);
#7681=EDGE_CURVE('',#5788,#5789,#2669,.T.);
#7682=EDGE_CURVE('',#5789,#5790,#4055,.T.);
#7683=EDGE_CURVE('',#5790,#5791,#4056,.T.);
#7684=EDGE_CURVE('',#5791,#5792,#4057,.T.);
#7685=EDGE_CURVE('',#5792,#5793,#4058,.T.);
#7686=EDGE_CURVE('',#5793,#5794,#4059,.T.);
#7687=EDGE_CURVE('',#5795,#5794,#2670,.T.);
#7688=EDGE_CURVE('',#5778,#5795,#4060,.T.);
#7689=EDGE_CURVE('',#5796,#5776,#4061,.T.);
#7690=EDGE_CURVE('',#5779,#5796,#4062,.T.);
#7691=EDGE_CURVE('',#5796,#5797,#2671,.T.);
#7692=EDGE_CURVE('',#5797,#5780,#4063,.T.);
#7693=EDGE_CURVE('',#5798,#5799,#2672,.T.);
#7694=EDGE_CURVE('',#5799,#5795,#4064,.T.);
#7695=EDGE_CURVE('',#5794,#5798,#4065,.T.);
#7696=EDGE_CURVE('',#5783,#5793,#4066,.T.);
#7697=EDGE_CURVE('',#5800,#5782,#4067,.T.);
#7698=EDGE_CURVE('',#5798,#5800,#4068,.T.);
#7699=EDGE_CURVE('',#5801,#5800,#2673,.T.);
#7700=EDGE_CURVE('',#5781,#5801,#4069,.T.);
#7701=EDGE_CURVE('',#5801,#5797,#4070,.T.);
#7702=EDGE_CURVE('',#5802,#5792,#4071,.T.);
#7703=EDGE_CURVE('',#5803,#5802,#2674,.T.);
#7704=EDGE_CURVE('',#5803,#5793,#4072,.T.);
#7705=EDGE_CURVE('',#5804,#5803,#4073,.T.);
#7706=EDGE_CURVE('',#5783,#5804,#4074,.T.);
#7707=EDGE_CURVE('',#5805,#5804,#2675,.T.);
#7708=EDGE_CURVE('',#5784,#5805,#4075,.T.);
#7709=EDGE_CURVE('',#5802,#5806,#4076,.T.);
#7710=EDGE_CURVE('',#5807,#5806,#2676,.T.);
#7711=EDGE_CURVE('',#5807,#5808,#4077,.T.);
#7712=EDGE_CURVE('',#5809,#5808,#3627,.F.);
#7713=EDGE_CURVE('',#5809,#5810,#4078,.T.);
#7714=EDGE_CURVE('',#5810,#5811,#2677,.T.);
#7715=EDGE_CURVE('',#5811,#5805,#4079,.T.);
#7716=EDGE_CURVE('',#5806,#5791,#4080,.T.);
#7717=EDGE_CURVE('',#5787,#5809,#240,.F.);
#7718=EDGE_CURVE('',#5810,#5786,#4081,.T.);
#7719=EDGE_CURVE('',#5790,#5807,#4082,.T.);
#7720=EDGE_CURVE('',#5808,#5789,#241,.F.);
#7721=EDGE_CURVE('',#5812,#5806,#2678,.T.);
#7722=EDGE_CURVE('',#5812,#5807,#2679,.T.);
#7723=EDGE_CURVE('',#5785,#5811,#4083,.T.);
#7724=EDGE_CURVE('',#5811,#5810,#2680,.T.);
#7725=EDGE_CURVE('',#5813,#5813,#2681,.T.);
#7726=EDGE_CURVE('',#5799,#5775,#4084,.T.);
#7727=EDGE_CURVE('',#5813,#5814,#4085,.T.);
#7728=EDGE_CURVE('',#5815,#5814,#3628,.F.);
#7729=EDGE_CURVE('',#5816,#5815,#3629,.F.);
#7730=EDGE_CURVE('',#5816,#5817,#4086,.T.);
#7731=EDGE_CURVE('',#5817,#5817,#2682,.T.);
#7732=EDGE_CURVE('',#5814,#5816,#3630,.F.);
#7733=EDGE_CURVE('',#5818,#5818,#2683,.F.);
#7734=EDGE_CURVE('',#5818,#5819,#4087,.T.);
#7735=EDGE_CURVE('',#5819,#5819,#2684,.T.);
#7736=EDGE_CURVE('',#5820,#5820,#2685,.T.);
#7737=EDGE_CURVE('',#5820,#5788,#4088,.T.);
#7738=EDGE_CURVE('',#5821,#5821,#2686,.T.);
#7739=EDGE_CURVE('',#5821,#5822,#4089,.T.);
#7740=EDGE_CURVE('',#5822,#5822,#2687,.T.);
#7741=EDGE_CURVE('',#5823,#5823,#2688,.T.);
#7742=EDGE_CURVE('',#5823,#5824,#4090,.T.);
#7743=EDGE_CURVE('',#5824,#5824,#2689,.T.);
#7744=EDGE_CURVE('',#5825,#5825,#2690,.T.);
#7745=EDGE_CURVE('',#5825,#5826,#4091,.T.);
#7746=EDGE_CURVE('',#5826,#5826,#2691,.T.);
#7747=EDGE_CURVE('',#5827,#5827,#2692,.T.);
#7748=EDGE_CURVE('',#5827,#5828,#2693,.T.);
#7749=EDGE_CURVE('',#5829,#5828,#2694,.T.);
#7750=EDGE_CURVE('',#5828,#5829,#2695,.T.);
#7751=EDGE_CURVE('',#5830,#5830,#2696,.T.);
#7752=EDGE_CURVE('',#5830,#5829,#4092,.T.);
#7753=EDGE_CURVE('',#5831,#5831,#2697,.T.);
#7754=EDGE_CURVE('',#5831,#5832,#4093,.T.);
#7755=EDGE_CURVE('',#5832,#5832,#2698,.T.);
#7756=EDGE_CURVE('',#5833,#5833,#2699,.T.);
#7757=EDGE_CURVE('',#5833,#5834,#2700,.T.);
#7758=EDGE_CURVE('',#5834,#5834,#2701,.T.);
#7759=EDGE_CURVE('',#5835,#5836,#2702,.T.);
#7760=EDGE_CURVE('',#5836,#5837,#4094,.T.);
#7761=EDGE_CURVE('',#5838,#5837,#2703,.T.);
#7762=EDGE_CURVE('',#5837,#5838,#2704,.T.);
#7763=EDGE_CURVE('',#5836,#5835,#2705,.T.);
#7764=EDGE_CURVE('',#5835,#5839,#4095,.T.);
#7765=EDGE_CURVE('',#5839,#5839,#2706,.T.);
#7766=EDGE_CURVE('',#5839,#5840,#4096,.T.);
#7767=EDGE_CURVE('',#5840,#5840,#2707,.T.);
#7768=EDGE_CURVE('',#5840,#5841,#2708,.T.);
#7769=EDGE_CURVE('',#5841,#5841,#2709,.T.);
#7770=EDGE_CURVE('',#5842,#5842,#2710,.T.);
#7771=EDGE_CURVE('',#5842,#5843,#2711,.T.);
#7772=EDGE_CURVE('',#5843,#5843,#2712,.T.);
#7773=EDGE_CURVE('',#5843,#5833,#4097,.T.);
#7774=EDGE_CURVE('',#5834,#5844,#4098,.T.);
#7775=EDGE_CURVE('',#5844,#5844,#2713,.T.);
#7776=EDGE_CURVE('',#5844,#5845,#2714,.T.);
#7777=EDGE_CURVE('',#5845,#5845,#2715,.T.);
#7778=EDGE_CURVE('',#5846,#5846,#2716,.T.);
#7779=EDGE_CURVE('',#5846,#5838,#2717,.T.);
#7780=EDGE_CURVE('',#5847,#5848,#2718,.T.);
#7781=EDGE_CURVE('',#5849,#5849,#2719,.T.);
#7782=EDGE_CURVE('',#5849,#5850,#4099,.T.);
#7783=EDGE_CURVE('',#5850,#5850,#2720,.T.);
#7784=EDGE_CURVE('',#5850,#5851,#2721,.T.);
#7785=EDGE_CURVE('',#5851,#5851,#2722,.T.);
#7786=EDGE_CURVE('',#5852,#5853,#2723,.T.);
#7787=EDGE_CURVE('',#5853,#5854,#4100,.T.);
#7788=EDGE_CURVE('',#5854,#5854,#2724,.T.);
#7789=EDGE_CURVE('',#5853,#5852,#2725,.T.);
#7790=EDGE_CURVE('',#5852,#5855,#4101,.T.);
#7791=EDGE_CURVE('',#5855,#5855,#2726,.T.);
#7792=EDGE_CURVE('',#5856,#5856,#2727,.T.);
#7793=EDGE_CURVE('',#5856,#5857,#4102,.T.);
#7794=EDGE_CURVE('',#5857,#5857,#2728,.T.);
#7795=EDGE_CURVE('',#5858,#5858,#2729,.T.);
#7796=EDGE_CURVE('',#5858,#5859,#4103,.T.);
#7797=EDGE_CURVE('',#5859,#5859,#2730,.T.);
#7798=EDGE_CURVE('',#5860,#5860,#2731,.T.);
#7799=EDGE_CURVE('',#5860,#5858,#2732,.T.);
#7800=EDGE_CURVE('',#5857,#5861,#4104,.T.);
#7801=EDGE_CURVE('',#5861,#5861,#2733,.T.);
#7802=EDGE_CURVE('',#5862,#5862,#2734,.T.);
#7803=EDGE_CURVE('',#5862,#5863,#4105,.T.);
#7804=EDGE_CURVE('',#5863,#5863,#2735,.T.);
#7805=EDGE_CURVE('',#5863,#5864,#4106,.T.);
#7806=EDGE_CURVE('',#5864,#5864,#2736,.T.);
#7807=EDGE_CURVE('',#5865,#5866,#2737,.T.);
#7808=EDGE_CURVE('',#5866,#5867,#4107,.T.);
#7809=EDGE_CURVE('',#5867,#5867,#2738,.T.);
#7810=EDGE_CURVE('',#5866,#5865,#2739,.T.);
#7811=EDGE_CURVE('',#5865,#5868,#4108,.T.);
#7812=EDGE_CURVE('',#5868,#5868,#2740,.T.);
#7813=EDGE_CURVE('',#5868,#5869,#4109,.T.);
#7814=EDGE_CURVE('',#5869,#5869,#2741,.T.);
#7815=EDGE_CURVE('',#5870,#5870,#2742,.T.);
#7816=EDGE_CURVE('',#5870,#5871,#4110,.T.);
#7817=EDGE_CURVE('',#5871,#5871,#2743,.T.);
#7818=EDGE_CURVE('',#5872,#5873,#2744,.T.);
#7819=EDGE_CURVE('',#5873,#5870,#4111,.T.);
#7820=EDGE_CURVE('',#5873,#5872,#2745,.T.);
#7821=EDGE_CURVE('',#5872,#5874,#4112,.T.);
#7822=EDGE_CURVE('',#5874,#5874,#2746,.T.);
#7823=EDGE_CURVE('',#5874,#5875,#2747,.T.);
#7824=EDGE_CURVE('',#5875,#5875,#2748,.T.);
#7825=EDGE_CURVE('',#5875,#5862,#4113,.T.);
#7826=EDGE_CURVE('',#5876,#5877,#2749,.T.);
#7827=EDGE_CURVE('',#5878,#5879,#2750,.T.);
#7828=EDGE_CURVE('',#5880,#5881,#2751,.T.);
#7829=EDGE_CURVE('',#5882,#5883,#2752,.T.);
#7830=EDGE_CURVE('',#5884,#5885,#2753,.T.);
#7831=EDGE_CURVE('',#5886,#5887,#2754,.T.);
#7832=EDGE_CURVE('',#5888,#5889,#2755,.T.);
#7833=EDGE_CURVE('',#5890,#5891,#2756,.T.);
#7834=EDGE_CURVE('',#5892,#5892,#2757,.T.);
#7835=EDGE_CURVE('',#5892,#5893,#4114,.T.);
#7836=EDGE_CURVE('',#5893,#5893,#2758,.T.);
#7837=EDGE_CURVE('',#5893,#5894,#2759,.T.);
#7838=EDGE_CURVE('',#5894,#5894,#2760,.T.);
#7839=EDGE_CURVE('',#5894,#5895,#4115,.T.);
#7840=EDGE_CURVE('',#5895,#5895,#2761,.T.);
#7841=EDGE_CURVE('',#5895,#5896,#2762,.T.);
#7842=EDGE_CURVE('',#5896,#5897,#2763,.T.);
#7843=EDGE_CURVE('',#5897,#5896,#2764,.T.);
#7844=EDGE_CURVE('',#5898,#5899,#2765,.T.);
#7845=EDGE_CURVE('',#5899,#5897,#4116,.T.);
#7846=EDGE_CURVE('',#5899,#5898,#2766,.T.);
#7847=EDGE_CURVE('',#5898,#5900,#4117,.T.);
#7848=EDGE_CURVE('',#5900,#5900,#2767,.T.);
#7849=EDGE_CURVE('',#5901,#5902,#2768,.T.);
#7850=EDGE_CURVE('',#5902,#5901,#2769,.T.);
#7851=EDGE_CURVE('',#5902,#5903,#2770,.T.);
#7852=EDGE_CURVE('',#5903,#5903,#2771,.T.);
#7853=EDGE_CURVE('',#5904,#5904,#2772,.T.);
#7854=EDGE_CURVE('',#5904,#5905,#2773,.T.);
#7855=EDGE_CURVE('',#5905,#5905,#2774,.T.);
#7856=EDGE_CURVE('',#5906,#5906,#2775,.T.);
#7857=EDGE_CURVE('',#5906,#5907,#4118,.T.);
#7858=EDGE_CURVE('',#5907,#5907,#2776,.T.);
#7859=EDGE_CURVE('',#5901,#5904,#4119,.T.);
#7860=EDGE_CURVE('',#5908,#5909,#2777,.T.);
#7861=EDGE_CURVE('',#5909,#5908,#2778,.T.);
#7862=EDGE_CURVE('',#5909,#5910,#4120,.T.);
#7863=EDGE_CURVE('',#5910,#5911,#2779,.T.);
#7864=EDGE_CURVE('',#5911,#5910,#2780,.T.);
#7865=EDGE_CURVE('',#5912,#5913,#2781,.T.);
#7866=EDGE_CURVE('',#5913,#5912,#2782,.T.);
#7867=EDGE_CURVE('',#5913,#5914,#4121,.T.);
#7868=EDGE_CURVE('',#5914,#5915,#2783,.T.);
#7869=EDGE_CURVE('',#5915,#5914,#2784,.T.);
#7870=EDGE_CURVE('',#5916,#5916,#2785,.T.);
#7871=EDGE_CURVE('',#5916,#5917,#2786,.T.);
#7872=EDGE_CURVE('',#5917,#5918,#2787,.T.);
#7873=EDGE_CURVE('',#5918,#5917,#2788,.T.);
#7874=EDGE_CURVE('',#5919,#5920,#2789,.T.);
#7875=EDGE_CURVE('',#5920,#5919,#2790,.T.);
#7876=EDGE_CURVE('',#5920,#5916,#4122,.T.);
#7877=EDGE_CURVE('',#5919,#5911,#4123,.T.);
#7878=EDGE_CURVE('',#5908,#5921,#4124,.T.);
#7879=EDGE_CURVE('',#5921,#5922,#242,.T.);
#7880=EDGE_CURVE('',#5922,#5923,#3631,.T.);
#7881=EDGE_CURVE('',#5924,#5923,#243,.T.);
#7882=EDGE_CURVE('',#5924,#5915,#4125,.T.);
#7883=EDGE_CURVE('',#5925,#5924,#244,.T.);
#7884=EDGE_CURVE('',#5925,#5926,#3632,.T.);
#7885=EDGE_CURVE('',#5926,#5921,#245,.T.);
#7886=EDGE_CURVE('',#5927,#5928,#246,.F.);
#7887=EDGE_CURVE('',#5928,#5929,#3633,.T.);
#7888=EDGE_CURVE('',#5930,#5929,#247,.F.);
#7889=EDGE_CURVE('',#5930,#5927,#3634,.T.);
#7890=EDGE_CURVE('',#5931,#5932,#248,.T.);
#7891=EDGE_CURVE('',#5931,#5933,#3635,.T.);
#7892=EDGE_CURVE('',#5933,#5934,#249,.T.);
#7893=EDGE_CURVE('',#5934,#5932,#3636,.T.);
#7894=EDGE_CURVE('',#5935,#5936,#250,.T.);
#7895=EDGE_CURVE('',#5935,#5937,#3637,.T.);
#7896=EDGE_CURVE('',#5937,#5938,#251,.T.);
#7897=EDGE_CURVE('',#5938,#5936,#3638,.T.);
#7898=EDGE_CURVE('',#5939,#5940,#252,.T.);
#7899=EDGE_CURVE('',#5939,#5941,#3639,.T.);
#7900=EDGE_CURVE('',#5941,#5942,#253,.T.);
#7901=EDGE_CURVE('',#5942,#5940,#3640,.T.);
#7902=EDGE_CURVE('',#5943,#5944,#254,.T.);
#7903=EDGE_CURVE('',#5943,#5945,#3641,.T.);
#7904=EDGE_CURVE('',#5945,#5946,#255,.T.);
#7905=EDGE_CURVE('',#5946,#5944,#3642,.T.);
#7906=EDGE_CURVE('',#5947,#5948,#256,.T.);
#7907=EDGE_CURVE('',#5947,#5949,#3643,.T.);
#7908=EDGE_CURVE('',#5949,#5950,#257,.T.);
#7909=EDGE_CURVE('',#5950,#5948,#3644,.T.);
#7910=EDGE_CURVE('',#5951,#5952,#258,.T.);
#7911=EDGE_CURVE('',#5951,#5953,#3645,.T.);
#7912=EDGE_CURVE('',#5953,#5954,#259,.T.);
#7913=EDGE_CURVE('',#5954,#5952,#3646,.T.);
#7914=EDGE_CURVE('',#5955,#5956,#260,.T.);
#7915=EDGE_CURVE('',#5955,#5957,#3647,.T.);
#7916=EDGE_CURVE('',#5957,#5958,#261,.T.);
#7917=EDGE_CURVE('',#5958,#5956,#3648,.T.);
#7918=EDGE_CURVE('',#5959,#5960,#262,.T.);
#7919=EDGE_CURVE('',#5959,#5961,#3649,.T.);
#7920=EDGE_CURVE('',#5961,#5962,#263,.T.);
#7921=EDGE_CURVE('',#5962,#5960,#3650,.T.);
#7922=EDGE_CURVE('',#5963,#5964,#264,.T.);
#7923=EDGE_CURVE('',#5963,#5965,#3651,.T.);
#7924=EDGE_CURVE('',#5965,#5966,#265,.T.);
#7925=EDGE_CURVE('',#5966,#5964,#3652,.T.);
#7926=EDGE_CURVE('',#5912,#5967,#4126,.T.);
#7927=EDGE_CURVE('',#5968,#5967,#266,.T.);
#7928=EDGE_CURVE('',#5968,#5969,#3653,.T.);
#7929=EDGE_CURVE('',#5969,#5970,#267,.T.);
#7930=EDGE_CURVE('',#5970,#5918,#4127,.T.);
#7931=EDGE_CURVE('',#5970,#5971,#268,.T.);
#7932=EDGE_CURVE('',#5971,#5972,#3654,.T.);
#7933=EDGE_CURVE('',#5967,#5972,#269,.T.);
#7934=EDGE_CURVE('',#5973,#5974,#270,.F.);
#7935=EDGE_CURVE('',#5974,#5975,#3655,.T.);
#7936=EDGE_CURVE('',#5976,#5975,#271,.F.);
#7937=EDGE_CURVE('',#5976,#5973,#3656,.T.);
#7938=EDGE_CURVE('',#5977,#5978,#272,.T.);
#7939=EDGE_CURVE('',#5977,#5979,#3657,.T.);
#7940=EDGE_CURVE('',#5979,#5980,#273,.T.);
#7941=EDGE_CURVE('',#5980,#5978,#3658,.T.);
#7942=EDGE_CURVE('',#5981,#5982,#274,.T.);
#7943=EDGE_CURVE('',#5981,#5983,#3659,.T.);
#7944=EDGE_CURVE('',#5983,#5984,#275,.T.);
#7945=EDGE_CURVE('',#5984,#5982,#3660,.T.);
#7946=EDGE_CURVE('',#5985,#5986,#276,.T.);
#7947=EDGE_CURVE('',#5985,#5987,#3661,.T.);
#7948=EDGE_CURVE('',#5987,#5988,#277,.T.);
#7949=EDGE_CURVE('',#5988,#5986,#3662,.T.);
#7950=EDGE_CURVE('',#5989,#5990,#278,.T.);
#7951=EDGE_CURVE('',#5989,#5991,#3663,.T.);
#7952=EDGE_CURVE('',#5991,#5992,#279,.T.);
#7953=EDGE_CURVE('',#5992,#5990,#3664,.T.);
#7954=EDGE_CURVE('',#5993,#5994,#280,.T.);
#7955=EDGE_CURVE('',#5993,#5995,#3665,.T.);
#7956=EDGE_CURVE('',#5995,#5996,#281,.T.);
#7957=EDGE_CURVE('',#5996,#5994,#3666,.T.);
#7958=EDGE_CURVE('',#5997,#5998,#282,.T.);
#7959=EDGE_CURVE('',#5997,#5999,#3667,.T.);
#7960=EDGE_CURVE('',#5999,#6000,#283,.T.);
#7961=EDGE_CURVE('',#6000,#5998,#3668,.T.);
#7962=EDGE_CURVE('',#6001,#6002,#284,.T.);
#7963=EDGE_CURVE('',#6001,#6003,#3669,.T.);
#7964=EDGE_CURVE('',#6003,#6004,#285,.T.);
#7965=EDGE_CURVE('',#6004,#6002,#3670,.T.);
#7966=EDGE_CURVE('',#6005,#6006,#286,.T.);
#7967=EDGE_CURVE('',#6005,#6007,#3671,.T.);
#7968=EDGE_CURVE('',#6007,#6008,#287,.T.);
#7969=EDGE_CURVE('',#6008,#6006,#3672,.T.);
#7970=EDGE_CURVE('',#6009,#6010,#288,.T.);
#7971=EDGE_CURVE('',#6009,#6011,#3673,.T.);
#7972=EDGE_CURVE('',#6011,#6012,#289,.T.);
#7973=EDGE_CURVE('',#6012,#6010,#3674,.T.);
#7974=EDGE_CURVE('',#6004,#5941,#2791,.T.);
#7975=EDGE_CURVE('',#6002,#5939,#2792,.T.);
#7976=EDGE_CURVE('',#5940,#6001,#2793,.T.);
#7977=EDGE_CURVE('',#5942,#6003,#2794,.T.);
#7978=EDGE_CURVE('',#6008,#5945,#2795,.T.);
#7979=EDGE_CURVE('',#6006,#5943,#2796,.T.);
#7980=EDGE_CURVE('',#5944,#6005,#2797,.T.);
#7981=EDGE_CURVE('',#5946,#6007,#2798,.T.);
#7982=EDGE_CURVE('',#6000,#5937,#2799,.T.);
#7983=EDGE_CURVE('',#5998,#5935,#2800,.T.);
#7984=EDGE_CURVE('',#5936,#5997,#2801,.T.);
#7985=EDGE_CURVE('',#5938,#5999,#2802,.T.);
#7986=EDGE_CURVE('',#6012,#5949,#2803,.T.);
#7987=EDGE_CURVE('',#6010,#5947,#2804,.T.);
#7988=EDGE_CURVE('',#5948,#6009,#2805,.T.);
#7989=EDGE_CURVE('',#5950,#6011,#2806,.T.);
#7990=EDGE_CURVE('',#5974,#5927,#2807,.T.);
#7991=EDGE_CURVE('',#5975,#5930,#2808,.T.);
#7992=EDGE_CURVE('',#5929,#5976,#2809,.T.);
#7993=EDGE_CURVE('',#5928,#5973,#2810,.T.);
#7994=EDGE_CURVE('',#5988,#5961,#2811,.T.);
#7995=EDGE_CURVE('',#5986,#5959,#2812,.T.);
#7996=EDGE_CURVE('',#5960,#5985,#2813,.T.);
#7997=EDGE_CURVE('',#5962,#5987,#2814,.T.);
#7998=EDGE_CURVE('',#5984,#5957,#2815,.T.);
#7999=EDGE_CURVE('',#5982,#5955,#2816,.T.);
#8000=EDGE_CURVE('',#5956,#5981,#2817,.T.);
#8001=EDGE_CURVE('',#5958,#5983,#2818,.T.);
#8002=EDGE_CURVE('',#5992,#5965,#2819,.T.);
#8003=EDGE_CURVE('',#5990,#5963,#2820,.T.);
#8004=EDGE_CURVE('',#5964,#5989,#2821,.T.);
#8005=EDGE_CURVE('',#5966,#5991,#2822,.T.);
#8006=EDGE_CURVE('',#5980,#5953,#2823,.T.);
#8007=EDGE_CURVE('',#5978,#5951,#2824,.T.);
#8008=EDGE_CURVE('',#5952,#5977,#2825,.T.);
#8009=EDGE_CURVE('',#5954,#5979,#2826,.T.);
#8010=EDGE_CURVE('',#5971,#5926,#2827,.T.);
#8011=EDGE_CURVE('',#5972,#5925,#2828,.T.);
#8012=EDGE_CURVE('',#5923,#5968,#2829,.T.);
#8013=EDGE_CURVE('',#5922,#5969,#2830,.T.);
#8014=EDGE_CURVE('',#5996,#5933,#2831,.T.);
#8015=EDGE_CURVE('',#5994,#5931,#2832,.T.);
#8016=EDGE_CURVE('',#5932,#5993,#2833,.T.);
#8017=EDGE_CURVE('',#5934,#5995,#2834,.T.);
#8018=EDGE_CURVE('',#6013,#6013,#2835,.T.);
#8019=EDGE_CURVE('',#6013,#6014,#2836,.T.);
#8020=EDGE_CURVE('',#6015,#6014,#2837,.T.);
#8021=EDGE_CURVE('',#6014,#6015,#2838,.T.);
#8022=EDGE_CURVE('',#6016,#6016,#2839,.T.);
#8023=EDGE_CURVE('',#6016,#6017,#2840,.T.);
#8024=EDGE_CURVE('',#6017,#6017,#2841,.T.);
#8025=EDGE_CURVE('',#6018,#6018,#2842,.T.);
#8026=EDGE_CURVE('',#6018,#6019,#4128,.T.);
#8027=EDGE_CURVE('',#6019,#6020,#2843,.T.);
#8028=EDGE_CURVE('',#6020,#6019,#2844,.T.);
#8029=EDGE_CURVE('',#6021,#6022,#2845,.T.);
#8030=EDGE_CURVE('',#6022,#6020,#4129,.T.);
#8031=EDGE_CURVE('',#6022,#6021,#2846,.T.);
#8032=EDGE_CURVE('',#6021,#6023,#4130,.T.);
#8033=EDGE_CURVE('',#6023,#6023,#2847,.T.);
#8034=EDGE_CURVE('',#6023,#6024,#4131,.T.);
#8035=EDGE_CURVE('',#6024,#6024,#2848,.T.);
#8036=EDGE_CURVE('',#6017,#6015,#4132,.T.);
#8037=EDGE_CURVE('',#6025,#6025,#2849,.T.);
#8038=EDGE_CURVE('',#6025,#6018,#4133,.T.);
#8039=EDGE_CURVE('',#6026,#6026,#2850,.T.);
#8040=EDGE_CURVE('',#6026,#6027,#4134,.T.);
#8041=EDGE_CURVE('',#6027,#6027,#2851,.T.);
#8042=EDGE_CURVE('',#6028,#6028,#2852,.T.);
#8043=EDGE_CURVE('',#6028,#6029,#4135,.T.);
#8044=EDGE_CURVE('',#6029,#6029,#2853,.T.);
#8045=EDGE_CURVE('',#6030,#6030,#2854,.T.);
#8046=EDGE_CURVE('',#6030,#6031,#4136,.T.);
#8047=EDGE_CURVE('',#6031,#6031,#2855,.T.);
#8048=EDGE_CURVE('',#6032,#6032,#2856,.T.);
#8049=EDGE_CURVE('',#6032,#6033,#4137,.T.);
#8050=EDGE_CURVE('',#6033,#6033,#2857,.T.);
#8051=EDGE_CURVE('',#6034,#6034,#2858,.T.);
#8052=EDGE_CURVE('',#6034,#6035,#4138,.T.);
#8053=EDGE_CURVE('',#6035,#6035,#2859,.T.);
#8054=EDGE_CURVE('',#6036,#6036,#2860,.T.);
#8055=EDGE_CURVE('',#6036,#6037,#4139,.T.);
#8056=EDGE_CURVE('',#6037,#6037,#2861,.T.);
#8057=EDGE_CURVE('',#6038,#6038,#2862,.T.);
#8058=EDGE_CURVE('',#6038,#6039,#4140,.T.);
#8059=EDGE_CURVE('',#6039,#6039,#2863,.T.);
#8060=EDGE_CURVE('',#6040,#6040,#2864,.T.);
#8061=EDGE_CURVE('',#6040,#6041,#4141,.T.);
#8062=EDGE_CURVE('',#6041,#6041,#2865,.T.);
#8063=EDGE_CURVE('',#6042,#6042,#2866,.T.);
#8064=EDGE_CURVE('',#6042,#6043,#4142,.T.);
#8065=EDGE_CURVE('',#6043,#6043,#2867,.T.);
#8066=EDGE_CURVE('',#6044,#6044,#2868,.T.);
#8067=EDGE_CURVE('',#6044,#6045,#4143,.T.);
#8068=EDGE_CURVE('',#6045,#6045,#2869,.T.);
#8069=EDGE_CURVE('',#6046,#6046,#2870,.T.);
#8070=EDGE_CURVE('',#6046,#6047,#4144,.T.);
#8071=EDGE_CURVE('',#6047,#6047,#2871,.T.);
#8072=ORIENTED_EDGE('',*,*,#6048,.T.);
#8073=ORIENTED_EDGE('',*,*,#6049,.T.);
#8074=ORIENTED_EDGE('',*,*,#6050,.F.);
#8075=ORIENTED_EDGE('',*,*,#6051,.F.);
#8076=ORIENTED_EDGE('',*,*,#6052,.T.);
#8077=ORIENTED_EDGE('',*,*,#6053,.T.);
#8078=ORIENTED_EDGE('',*,*,#6054,.T.);
#8079=ORIENTED_EDGE('',*,*,#6048,.F.);
#8080=ORIENTED_EDGE('',*,*,#6055,.F.);
#8081=ORIENTED_EDGE('',*,*,#6056,.F.);
#8082=ORIENTED_EDGE('',*,*,#6057,.T.);
#8083=ORIENTED_EDGE('',*,*,#6058,.T.);
#8084=ORIENTED_EDGE('',*,*,#6059,.T.);
#8085=ORIENTED_EDGE('',*,*,#6052,.F.);
#8086=ORIENTED_EDGE('',*,*,#6060,.F.);
#8087=ORIENTED_EDGE('',*,*,#6061,.F.);
#8088=ORIENTED_EDGE('',*,*,#6062,.T.);
#8089=ORIENTED_EDGE('',*,*,#6063,.T.);
#8090=ORIENTED_EDGE('',*,*,#6064,.T.);
#8091=ORIENTED_EDGE('',*,*,#6057,.F.);
#8092=ORIENTED_EDGE('',*,*,#6065,.F.);
#8093=ORIENTED_EDGE('',*,*,#6066,.F.);
#8094=ORIENTED_EDGE('',*,*,#6067,.T.);
#8095=ORIENTED_EDGE('',*,*,#6068,.T.);
#8096=ORIENTED_EDGE('',*,*,#6069,.T.);
#8097=ORIENTED_EDGE('',*,*,#6062,.F.);
#8098=ORIENTED_EDGE('',*,*,#6070,.F.);
#8099=ORIENTED_EDGE('',*,*,#6071,.F.);
#8100=ORIENTED_EDGE('',*,*,#6072,.T.);
#8101=ORIENTED_EDGE('',*,*,#6073,.T.);
#8102=ORIENTED_EDGE('',*,*,#6074,.T.);
#8103=ORIENTED_EDGE('',*,*,#6067,.F.);
#8104=ORIENTED_EDGE('',*,*,#6075,.F.);
#8105=ORIENTED_EDGE('',*,*,#6076,.F.);
#8106=ORIENTED_EDGE('',*,*,#6077,.T.);
#8107=ORIENTED_EDGE('',*,*,#6078,.T.);
#8108=ORIENTED_EDGE('',*,*,#6079,.T.);
#8109=ORIENTED_EDGE('',*,*,#6072,.F.);
#8110=ORIENTED_EDGE('',*,*,#6080,.F.);
#8111=ORIENTED_EDGE('',*,*,#6081,.F.);
#8112=ORIENTED_EDGE('',*,*,#6082,.T.);
#8113=ORIENTED_EDGE('',*,*,#6083,.T.);
#8114=ORIENTED_EDGE('',*,*,#6084,.T.);
#8115=ORIENTED_EDGE('',*,*,#6077,.F.);
#8116=ORIENTED_EDGE('',*,*,#6085,.F.);
#8117=ORIENTED_EDGE('',*,*,#6086,.F.);
#8118=ORIENTED_EDGE('',*,*,#6087,.T.);
#8119=ORIENTED_EDGE('',*,*,#6088,.T.);
#8120=ORIENTED_EDGE('',*,*,#6089,.T.);
#8121=ORIENTED_EDGE('',*,*,#6082,.F.);
#8122=ORIENTED_EDGE('',*,*,#6090,.F.);
#8123=ORIENTED_EDGE('',*,*,#6091,.F.);
#8124=ORIENTED_EDGE('',*,*,#6092,.T.);
#8125=ORIENTED_EDGE('',*,*,#6093,.T.);
#8126=ORIENTED_EDGE('',*,*,#6094,.T.);
#8127=ORIENTED_EDGE('',*,*,#6087,.F.);
#8128=ORIENTED_EDGE('',*,*,#6095,.F.);
#8129=ORIENTED_EDGE('',*,*,#6096,.F.);
#8130=ORIENTED_EDGE('',*,*,#6097,.T.);
#8131=ORIENTED_EDGE('',*,*,#6098,.T.);
#8132=ORIENTED_EDGE('',*,*,#6099,.T.);
#8133=ORIENTED_EDGE('',*,*,#6092,.F.);
#8134=ORIENTED_EDGE('',*,*,#6100,.F.);
#8135=ORIENTED_EDGE('',*,*,#6101,.F.);
#8136=ORIENTED_EDGE('',*,*,#6102,.F.);
#8137=ORIENTED_EDGE('',*,*,#6103,.F.);
#8138=ORIENTED_EDGE('',*,*,#6104,.F.);
#8139=ORIENTED_EDGE('',*,*,#6105,.F.);
#8140=ORIENTED_EDGE('',*,*,#6106,.T.);
#8141=ORIENTED_EDGE('',*,*,#6107,.T.);
#8142=ORIENTED_EDGE('',*,*,#6108,.T.);
#8143=ORIENTED_EDGE('',*,*,#6109,.T.);
#8144=ORIENTED_EDGE('',*,*,#6110,.F.);
#8145=ORIENTED_EDGE('',*,*,#6111,.T.);
#8146=ORIENTED_EDGE('',*,*,#6112,.T.);
#8147=ORIENTED_EDGE('',*,*,#6113,.T.);
#8148=ORIENTED_EDGE('',*,*,#6108,.F.);
#8149=ORIENTED_EDGE('',*,*,#6114,.T.);
#8150=ORIENTED_EDGE('',*,*,#6115,.T.);
#8151=ORIENTED_EDGE('',*,*,#6116,.T.);
#8152=ORIENTED_EDGE('',*,*,#6117,.T.);
#8153=ORIENTED_EDGE('',*,*,#6118,.T.);
#8154=ORIENTED_EDGE('',*,*,#6112,.F.);
#8155=ORIENTED_EDGE('',*,*,#6119,.T.);
#8156=ORIENTED_EDGE('',*,*,#6120,.T.);
#8157=ORIENTED_EDGE('',*,*,#6121,.T.);
#8158=ORIENTED_EDGE('',*,*,#6122,.T.);
#8159=ORIENTED_EDGE('',*,*,#6123,.T.);
#8160=ORIENTED_EDGE('',*,*,#6116,.F.);
#8161=ORIENTED_EDGE('',*,*,#6124,.T.);
#8162=ORIENTED_EDGE('',*,*,#6125,.T.);
#8163=ORIENTED_EDGE('',*,*,#6126,.T.);
#8164=ORIENTED_EDGE('',*,*,#6127,.T.);
#8165=ORIENTED_EDGE('',*,*,#6128,.T.);
#8166=ORIENTED_EDGE('',*,*,#6121,.F.);
#8167=ORIENTED_EDGE('',*,*,#6129,.T.);
#8168=ORIENTED_EDGE('',*,*,#6130,.T.);
#8169=ORIENTED_EDGE('',*,*,#6131,.T.);
#8170=ORIENTED_EDGE('',*,*,#6132,.T.);
#8171=ORIENTED_EDGE('',*,*,#6133,.T.);
#8172=ORIENTED_EDGE('',*,*,#6126,.F.);
#8173=ORIENTED_EDGE('',*,*,#6134,.T.);
#8174=ORIENTED_EDGE('',*,*,#6135,.T.);
#8175=ORIENTED_EDGE('',*,*,#6136,.T.);
#8176=ORIENTED_EDGE('',*,*,#6137,.T.);
#8177=ORIENTED_EDGE('',*,*,#6138,.T.);
#8178=ORIENTED_EDGE('',*,*,#6131,.F.);
#8179=ORIENTED_EDGE('',*,*,#6139,.T.);
#8180=ORIENTED_EDGE('',*,*,#6140,.T.);
#8181=ORIENTED_EDGE('',*,*,#6141,.T.);
#8182=ORIENTED_EDGE('',*,*,#6142,.T.);
#8183=ORIENTED_EDGE('',*,*,#6136,.F.);
#8184=ORIENTED_EDGE('',*,*,#6143,.T.);
#8185=ORIENTED_EDGE('',*,*,#6144,.T.);
#8186=ORIENTED_EDGE('',*,*,#6145,.T.);
#8187=ORIENTED_EDGE('',*,*,#6146,.T.);
#8188=ORIENTED_EDGE('',*,*,#6147,.T.);
#8189=ORIENTED_EDGE('',*,*,#6141,.F.);
#8190=ORIENTED_EDGE('',*,*,#6148,.T.);
#8191=ORIENTED_EDGE('',*,*,#6149,.T.);
#8192=ORIENTED_EDGE('',*,*,#6150,.T.);
#8193=ORIENTED_EDGE('',*,*,#6151,.T.);
#8194=ORIENTED_EDGE('',*,*,#6152,.T.);
#8195=ORIENTED_EDGE('',*,*,#6145,.F.);
#8196=ORIENTED_EDGE('',*,*,#6153,.T.);
#8197=ORIENTED_EDGE('',*,*,#6154,.T.);
#8198=ORIENTED_EDGE('',*,*,#6155,.T.);
#8199=ORIENTED_EDGE('',*,*,#6150,.F.);
#8200=ORIENTED_EDGE('',*,*,#6156,.T.);
#8201=ORIENTED_EDGE('',*,*,#6157,.T.);
#8202=ORIENTED_EDGE('',*,*,#6158,.F.);
#8203=ORIENTED_EDGE('',*,*,#6159,.T.);
#8204=ORIENTED_EDGE('',*,*,#6160,.T.);
#8205=ORIENTED_EDGE('',*,*,#6161,.F.);
#8206=ORIENTED_EDGE('',*,*,#6162,.T.);
#8207=ORIENTED_EDGE('',*,*,#6158,.T.);
#8208=ORIENTED_EDGE('',*,*,#6163,.T.);
#8209=ORIENTED_EDGE('',*,*,#6164,.T.);
#8210=ORIENTED_EDGE('',*,*,#6154,.F.);
#8211=ORIENTED_EDGE('',*,*,#6165,.T.);
#8212=ORIENTED_EDGE('',*,*,#6166,.T.);
#8213=ORIENTED_EDGE('',*,*,#6102,.T.);
#8214=ORIENTED_EDGE('',*,*,#6167,.T.);
#8215=ORIENTED_EDGE('',*,*,#6168,.T.);
#8216=ORIENTED_EDGE('',*,*,#6097,.F.);
#8217=ORIENTED_EDGE('',*,*,#6169,.F.);
#8218=ORIENTED_EDGE('',*,*,#6170,.F.);
#8219=ORIENTED_EDGE('',*,*,#6171,.F.);
#8220=ORIENTED_EDGE('',*,*,#6049,.F.);
#8221=ORIENTED_EDGE('',*,*,#6054,.F.);
#8222=ORIENTED_EDGE('',*,*,#6053,.F.);
#8223=ORIENTED_EDGE('',*,*,#6059,.F.);
#8224=ORIENTED_EDGE('',*,*,#6058,.F.);
#8225=ORIENTED_EDGE('',*,*,#6064,.F.);
#8226=ORIENTED_EDGE('',*,*,#6063,.F.);
#8227=ORIENTED_EDGE('',*,*,#6069,.F.);
#8228=ORIENTED_EDGE('',*,*,#6068,.F.);
#8229=ORIENTED_EDGE('',*,*,#6074,.F.);
#8230=ORIENTED_EDGE('',*,*,#6073,.F.);
#8231=ORIENTED_EDGE('',*,*,#6079,.F.);
#8232=ORIENTED_EDGE('',*,*,#6078,.F.);
#8233=ORIENTED_EDGE('',*,*,#6084,.F.);
#8234=ORIENTED_EDGE('',*,*,#6083,.F.);
#8235=ORIENTED_EDGE('',*,*,#6089,.F.);
#8236=ORIENTED_EDGE('',*,*,#6088,.F.);
#8237=ORIENTED_EDGE('',*,*,#6094,.F.);
#8238=ORIENTED_EDGE('',*,*,#6093,.F.);
#8239=ORIENTED_EDGE('',*,*,#6099,.F.);
#8240=ORIENTED_EDGE('',*,*,#6098,.F.);
#8241=ORIENTED_EDGE('',*,*,#6168,.F.);
#8242=ORIENTED_EDGE('',*,*,#6167,.F.);
#8243=ORIENTED_EDGE('',*,*,#6107,.F.);
#8244=ORIENTED_EDGE('',*,*,#6106,.F.);
#8245=ORIENTED_EDGE('',*,*,#6172,.F.);
#8246=ORIENTED_EDGE('',*,*,#6160,.F.);
#8247=ORIENTED_EDGE('',*,*,#6159,.F.);
#8248=ORIENTED_EDGE('',*,*,#6166,.F.);
#8249=ORIENTED_EDGE('',*,*,#6165,.F.);
#8250=ORIENTED_EDGE('',*,*,#6157,.F.);
#8251=ORIENTED_EDGE('',*,*,#6156,.F.);
#8252=ORIENTED_EDGE('',*,*,#6153,.F.);
#8253=ORIENTED_EDGE('',*,*,#6149,.F.);
#8254=ORIENTED_EDGE('',*,*,#6148,.F.);
#8255=ORIENTED_EDGE('',*,*,#6144,.F.);
#8256=ORIENTED_EDGE('',*,*,#6143,.F.);
#8257=ORIENTED_EDGE('',*,*,#6140,.F.);
#8258=ORIENTED_EDGE('',*,*,#6139,.F.);
#8259=ORIENTED_EDGE('',*,*,#6135,.F.);
#8260=ORIENTED_EDGE('',*,*,#6134,.F.);
#8261=ORIENTED_EDGE('',*,*,#6130,.F.);
#8262=ORIENTED_EDGE('',*,*,#6129,.F.);
#8263=ORIENTED_EDGE('',*,*,#6125,.F.);
#8264=ORIENTED_EDGE('',*,*,#6124,.F.);
#8265=ORIENTED_EDGE('',*,*,#6120,.F.);
#8266=ORIENTED_EDGE('',*,*,#6119,.F.);
#8267=ORIENTED_EDGE('',*,*,#6115,.F.);
#8268=ORIENTED_EDGE('',*,*,#6114,.F.);
#8269=ORIENTED_EDGE('',*,*,#6111,.F.);
#8270=ORIENTED_EDGE('',*,*,#6173,.F.);
#8271=ORIENTED_EDGE('',*,*,#6109,.F.);
#8272=ORIENTED_EDGE('',*,*,#6113,.F.);
#8273=ORIENTED_EDGE('',*,*,#6118,.F.);
#8274=ORIENTED_EDGE('',*,*,#6117,.F.);
#8275=ORIENTED_EDGE('',*,*,#6123,.F.);
#8276=ORIENTED_EDGE('',*,*,#6122,.F.);
#8277=ORIENTED_EDGE('',*,*,#6128,.F.);
#8278=ORIENTED_EDGE('',*,*,#6127,.F.);
#8279=ORIENTED_EDGE('',*,*,#6133,.F.);
#8280=ORIENTED_EDGE('',*,*,#6132,.F.);
#8281=ORIENTED_EDGE('',*,*,#6138,.F.);
#8282=ORIENTED_EDGE('',*,*,#6137,.F.);
#8283=ORIENTED_EDGE('',*,*,#6142,.F.);
#8284=ORIENTED_EDGE('',*,*,#6147,.F.);
#8285=ORIENTED_EDGE('',*,*,#6146,.F.);
#8286=ORIENTED_EDGE('',*,*,#6152,.F.);
#8287=ORIENTED_EDGE('',*,*,#6151,.F.);
#8288=ORIENTED_EDGE('',*,*,#6155,.F.);
#8289=ORIENTED_EDGE('',*,*,#6164,.F.);
#8290=ORIENTED_EDGE('',*,*,#6163,.F.);
#8291=ORIENTED_EDGE('',*,*,#6162,.F.);
#8292=ORIENTED_EDGE('',*,*,#6174,.F.);
#8293=ORIENTED_EDGE('',*,*,#6175,.F.);
#8294=ORIENTED_EDGE('',*,*,#6104,.T.);
#8295=ORIENTED_EDGE('',*,*,#6103,.T.);
#8296=ORIENTED_EDGE('',*,*,#6170,.T.);
#8297=ORIENTED_EDGE('',*,*,#6169,.T.);
#8298=ORIENTED_EDGE('',*,*,#6101,.T.);
#8299=ORIENTED_EDGE('',*,*,#6100,.T.);
#8300=ORIENTED_EDGE('',*,*,#6096,.T.);
#8301=ORIENTED_EDGE('',*,*,#6095,.T.);
#8302=ORIENTED_EDGE('',*,*,#6091,.T.);
#8303=ORIENTED_EDGE('',*,*,#6090,.T.);
#8304=ORIENTED_EDGE('',*,*,#6086,.T.);
#8305=ORIENTED_EDGE('',*,*,#6085,.T.);
#8306=ORIENTED_EDGE('',*,*,#6081,.T.);
#8307=ORIENTED_EDGE('',*,*,#6080,.T.);
#8308=ORIENTED_EDGE('',*,*,#6076,.T.);
#8309=ORIENTED_EDGE('',*,*,#6075,.T.);
#8310=ORIENTED_EDGE('',*,*,#6071,.T.);
#8311=ORIENTED_EDGE('',*,*,#6070,.T.);
#8312=ORIENTED_EDGE('',*,*,#6066,.T.);
#8313=ORIENTED_EDGE('',*,*,#6065,.T.);
#8314=ORIENTED_EDGE('',*,*,#6061,.T.);
#8315=ORIENTED_EDGE('',*,*,#6060,.T.);
#8316=ORIENTED_EDGE('',*,*,#6056,.T.);
#8317=ORIENTED_EDGE('',*,*,#6055,.T.);
#8318=ORIENTED_EDGE('',*,*,#6051,.T.);
#8319=ORIENTED_EDGE('',*,*,#6176,.T.);
#8320=ORIENTED_EDGE('',*,*,#6177,.T.);
#8321=ORIENTED_EDGE('',*,*,#6178,.T.);
#8322=ORIENTED_EDGE('',*,*,#6179,.T.);
#8323=ORIENTED_EDGE('',*,*,#6180,.T.);
#8324=ORIENTED_EDGE('',*,*,#6181,.T.);
#8325=ORIENTED_EDGE('',*,*,#6182,.T.);
#8326=ORIENTED_EDGE('',*,*,#6183,.T.);
#8327=ORIENTED_EDGE('',*,*,#6184,.T.);
#8328=ORIENTED_EDGE('',*,*,#6185,.T.);
#8329=ORIENTED_EDGE('',*,*,#6186,.T.);
#8330=ORIENTED_EDGE('',*,*,#6187,.T.);
#8331=ORIENTED_EDGE('',*,*,#6188,.T.);
#8332=ORIENTED_EDGE('',*,*,#6189,.T.);
#8333=ORIENTED_EDGE('',*,*,#6190,.T.);
#8334=ORIENTED_EDGE('',*,*,#6191,.T.);
#8335=ORIENTED_EDGE('',*,*,#6192,.T.);
#8336=ORIENTED_EDGE('',*,*,#6193,.T.);
#8337=ORIENTED_EDGE('',*,*,#6194,.T.);
#8338=ORIENTED_EDGE('',*,*,#6195,.T.);
#8339=ORIENTED_EDGE('',*,*,#6196,.T.);
#8340=ORIENTED_EDGE('',*,*,#6197,.T.);
#8341=ORIENTED_EDGE('',*,*,#6198,.T.);
#8342=ORIENTED_EDGE('',*,*,#6199,.T.);
#8343=ORIENTED_EDGE('',*,*,#6200,.T.);
#8344=ORIENTED_EDGE('',*,*,#6201,.T.);
#8345=ORIENTED_EDGE('',*,*,#6202,.T.);
#8346=ORIENTED_EDGE('',*,*,#6203,.T.);
#8347=ORIENTED_EDGE('',*,*,#6204,.T.);
#8348=ORIENTED_EDGE('',*,*,#6205,.T.);
#8349=ORIENTED_EDGE('',*,*,#6206,.T.);
#8350=ORIENTED_EDGE('',*,*,#6207,.T.);
#8351=ORIENTED_EDGE('',*,*,#6208,.T.);
#8352=ORIENTED_EDGE('',*,*,#6209,.T.);
#8353=ORIENTED_EDGE('',*,*,#6210,.T.);
#8354=ORIENTED_EDGE('',*,*,#6211,.T.);
#8355=ORIENTED_EDGE('',*,*,#6212,.T.);
#8356=ORIENTED_EDGE('',*,*,#6213,.T.);
#8357=ORIENTED_EDGE('',*,*,#6214,.T.);
#8358=ORIENTED_EDGE('',*,*,#6215,.T.);
#8359=ORIENTED_EDGE('',*,*,#6216,.T.);
#8360=ORIENTED_EDGE('',*,*,#6217,.T.);
#8361=ORIENTED_EDGE('',*,*,#6218,.T.);
#8362=ORIENTED_EDGE('',*,*,#6219,.T.);
#8363=ORIENTED_EDGE('',*,*,#6220,.T.);
#8364=ORIENTED_EDGE('',*,*,#6221,.T.);
#8365=ORIENTED_EDGE('',*,*,#6222,.T.);
#8366=ORIENTED_EDGE('',*,*,#6223,.T.);
#8367=ORIENTED_EDGE('',*,*,#6224,.T.);
#8368=ORIENTED_EDGE('',*,*,#6225,.T.);
#8369=ORIENTED_EDGE('',*,*,#6226,.T.);
#8370=ORIENTED_EDGE('',*,*,#6227,.T.);
#8371=ORIENTED_EDGE('',*,*,#6228,.T.);
#8372=ORIENTED_EDGE('',*,*,#6229,.T.);
#8373=ORIENTED_EDGE('',*,*,#6230,.T.);
#8374=ORIENTED_EDGE('',*,*,#6231,.T.);
#8375=ORIENTED_EDGE('',*,*,#6232,.T.);
#8376=ORIENTED_EDGE('',*,*,#6233,.T.);
#8377=ORIENTED_EDGE('',*,*,#6234,.T.);
#8378=ORIENTED_EDGE('',*,*,#6235,.T.);
#8379=ORIENTED_EDGE('',*,*,#6236,.T.);
#8380=ORIENTED_EDGE('',*,*,#6237,.T.);
#8381=ORIENTED_EDGE('',*,*,#6238,.T.);
#8382=ORIENTED_EDGE('',*,*,#6239,.T.);
#8383=ORIENTED_EDGE('',*,*,#6240,.T.);
#8384=ORIENTED_EDGE('',*,*,#6241,.T.);
#8385=ORIENTED_EDGE('',*,*,#6242,.T.);
#8386=ORIENTED_EDGE('',*,*,#6243,.T.);
#8387=ORIENTED_EDGE('',*,*,#6244,.T.);
#8388=ORIENTED_EDGE('',*,*,#6245,.T.);
#8389=ORIENTED_EDGE('',*,*,#6246,.T.);
#8390=ORIENTED_EDGE('',*,*,#6247,.T.);
#8391=ORIENTED_EDGE('',*,*,#6173,.T.);
#8392=ORIENTED_EDGE('',*,*,#6050,.T.);
#8393=ORIENTED_EDGE('',*,*,#6171,.T.);
#8394=ORIENTED_EDGE('',*,*,#6110,.T.);
#8395=ORIENTED_EDGE('',*,*,#6248,.F.);
#8396=ORIENTED_EDGE('',*,*,#6249,.F.);
#8397=ORIENTED_EDGE('',*,*,#6250,.F.);
#8398=ORIENTED_EDGE('',*,*,#6251,.F.);
#8399=ORIENTED_EDGE('',*,*,#6252,.F.);
#8400=ORIENTED_EDGE('',*,*,#6253,.F.);
#8401=ORIENTED_EDGE('',*,*,#6254,.F.);
#8402=ORIENTED_EDGE('',*,*,#6255,.F.);
#8403=ORIENTED_EDGE('',*,*,#6256,.F.);
#8404=ORIENTED_EDGE('',*,*,#6257,.F.);
#8405=ORIENTED_EDGE('',*,*,#6258,.F.);
#8406=ORIENTED_EDGE('',*,*,#6259,.F.);
#8407=ORIENTED_EDGE('',*,*,#6260,.F.);
#8408=ORIENTED_EDGE('',*,*,#6261,.F.);
#8409=ORIENTED_EDGE('',*,*,#6262,.F.);
#8410=ORIENTED_EDGE('',*,*,#6263,.F.);
#8411=ORIENTED_EDGE('',*,*,#6264,.F.);
#8412=ORIENTED_EDGE('',*,*,#6265,.F.);
#8413=ORIENTED_EDGE('',*,*,#6266,.F.);
#8414=ORIENTED_EDGE('',*,*,#6267,.F.);
#8415=ORIENTED_EDGE('',*,*,#6268,.F.);
#8416=ORIENTED_EDGE('',*,*,#6269,.F.);
#8417=ORIENTED_EDGE('',*,*,#6270,.F.);
#8418=ORIENTED_EDGE('',*,*,#6271,.F.);
#8419=ORIENTED_EDGE('',*,*,#6272,.F.);
#8420=ORIENTED_EDGE('',*,*,#6273,.F.);
#8421=ORIENTED_EDGE('',*,*,#6274,.F.);
#8422=ORIENTED_EDGE('',*,*,#6275,.F.);
#8423=ORIENTED_EDGE('',*,*,#6276,.F.);
#8424=ORIENTED_EDGE('',*,*,#6277,.F.);
#8425=ORIENTED_EDGE('',*,*,#6278,.F.);
#8426=ORIENTED_EDGE('',*,*,#6279,.F.);
#8427=ORIENTED_EDGE('',*,*,#6280,.F.);
#8428=ORIENTED_EDGE('',*,*,#6281,.F.);
#8429=ORIENTED_EDGE('',*,*,#6282,.F.);
#8430=ORIENTED_EDGE('',*,*,#6283,.F.);
#8431=ORIENTED_EDGE('',*,*,#6284,.F.);
#8432=ORIENTED_EDGE('',*,*,#6285,.F.);
#8433=ORIENTED_EDGE('',*,*,#6286,.F.);
#8434=ORIENTED_EDGE('',*,*,#6287,.F.);
#8435=ORIENTED_EDGE('',*,*,#6288,.F.);
#8436=ORIENTED_EDGE('',*,*,#6289,.F.);
#8437=ORIENTED_EDGE('',*,*,#6290,.F.);
#8438=ORIENTED_EDGE('',*,*,#6291,.F.);
#8439=ORIENTED_EDGE('',*,*,#6292,.F.);
#8440=ORIENTED_EDGE('',*,*,#6293,.F.);
#8441=ORIENTED_EDGE('',*,*,#6294,.F.);
#8442=ORIENTED_EDGE('',*,*,#6295,.F.);
#8443=ORIENTED_EDGE('',*,*,#6296,.F.);
#8444=ORIENTED_EDGE('',*,*,#6297,.F.);
#8445=ORIENTED_EDGE('',*,*,#6298,.F.);
#8446=ORIENTED_EDGE('',*,*,#6299,.F.);
#8447=ORIENTED_EDGE('',*,*,#6300,.F.);
#8448=ORIENTED_EDGE('',*,*,#6301,.F.);
#8449=ORIENTED_EDGE('',*,*,#6302,.F.);
#8450=ORIENTED_EDGE('',*,*,#6303,.F.);
#8451=ORIENTED_EDGE('',*,*,#6304,.F.);
#8452=ORIENTED_EDGE('',*,*,#6305,.F.);
#8453=ORIENTED_EDGE('',*,*,#6306,.F.);
#8454=ORIENTED_EDGE('',*,*,#6307,.F.);
#8455=ORIENTED_EDGE('',*,*,#6308,.F.);
#8456=ORIENTED_EDGE('',*,*,#6309,.F.);
#8457=ORIENTED_EDGE('',*,*,#6310,.F.);
#8458=ORIENTED_EDGE('',*,*,#6311,.F.);
#8459=ORIENTED_EDGE('',*,*,#6312,.F.);
#8460=ORIENTED_EDGE('',*,*,#6313,.F.);
#8461=ORIENTED_EDGE('',*,*,#6314,.F.);
#8462=ORIENTED_EDGE('',*,*,#6315,.F.);
#8463=ORIENTED_EDGE('',*,*,#6316,.F.);
#8464=ORIENTED_EDGE('',*,*,#6317,.F.);
#8465=ORIENTED_EDGE('',*,*,#6318,.F.);
#8466=ORIENTED_EDGE('',*,*,#6319,.F.);
#8467=ORIENTED_EDGE('',*,*,#6320,.F.);
#8468=ORIENTED_EDGE('',*,*,#6184,.F.);
#8469=ORIENTED_EDGE('',*,*,#6321,.F.);
#8470=ORIENTED_EDGE('',*,*,#6322,.F.);
#8471=ORIENTED_EDGE('',*,*,#6323,.F.);
#8472=ORIENTED_EDGE('',*,*,#6309,.T.);
#8473=ORIENTED_EDGE('',*,*,#6324,.F.);
#8474=ORIENTED_EDGE('',*,*,#6325,.F.);
#8475=ORIENTED_EDGE('',*,*,#6326,.F.);
#8476=ORIENTED_EDGE('',*,*,#6188,.F.);
#8477=ORIENTED_EDGE('',*,*,#6327,.F.);
#8478=ORIENTED_EDGE('',*,*,#6328,.F.);
#8479=ORIENTED_EDGE('',*,*,#6329,.F.);
#8480=ORIENTED_EDGE('',*,*,#6305,.T.);
#8481=ORIENTED_EDGE('',*,*,#6330,.F.);
#8482=ORIENTED_EDGE('',*,*,#6331,.F.);
#8483=ORIENTED_EDGE('',*,*,#6332,.F.);
#8484=ORIENTED_EDGE('',*,*,#6192,.F.);
#8485=ORIENTED_EDGE('',*,*,#6333,.F.);
#8486=ORIENTED_EDGE('',*,*,#6334,.F.);
#8487=ORIENTED_EDGE('',*,*,#6335,.F.);
#8488=ORIENTED_EDGE('',*,*,#6301,.T.);
#8489=ORIENTED_EDGE('',*,*,#6336,.F.);
#8490=ORIENTED_EDGE('',*,*,#6337,.F.);
#8491=ORIENTED_EDGE('',*,*,#6338,.F.);
#8492=ORIENTED_EDGE('',*,*,#6196,.F.);
#8493=ORIENTED_EDGE('',*,*,#6339,.F.);
#8494=ORIENTED_EDGE('',*,*,#6340,.F.);
#8495=ORIENTED_EDGE('',*,*,#6341,.F.);
#8496=ORIENTED_EDGE('',*,*,#6297,.T.);
#8497=ORIENTED_EDGE('',*,*,#6342,.F.);
#8498=ORIENTED_EDGE('',*,*,#6343,.F.);
#8499=ORIENTED_EDGE('',*,*,#6344,.F.);
#8500=ORIENTED_EDGE('',*,*,#6200,.F.);
#8501=ORIENTED_EDGE('',*,*,#6345,.F.);
#8502=ORIENTED_EDGE('',*,*,#6346,.F.);
#8503=ORIENTED_EDGE('',*,*,#6347,.F.);
#8504=ORIENTED_EDGE('',*,*,#6293,.T.);
#8505=ORIENTED_EDGE('',*,*,#6348,.F.);
#8506=ORIENTED_EDGE('',*,*,#6349,.F.);
#8507=ORIENTED_EDGE('',*,*,#6350,.F.);
#8508=ORIENTED_EDGE('',*,*,#6204,.F.);
#8509=ORIENTED_EDGE('',*,*,#6351,.F.);
#8510=ORIENTED_EDGE('',*,*,#6352,.F.);
#8511=ORIENTED_EDGE('',*,*,#6353,.F.);
#8512=ORIENTED_EDGE('',*,*,#6289,.T.);
#8513=ORIENTED_EDGE('',*,*,#6354,.F.);
#8514=ORIENTED_EDGE('',*,*,#6355,.F.);
#8515=ORIENTED_EDGE('',*,*,#6356,.F.);
#8516=ORIENTED_EDGE('',*,*,#6208,.F.);
#8517=ORIENTED_EDGE('',*,*,#6357,.F.);
#8518=ORIENTED_EDGE('',*,*,#6358,.F.);
#8519=ORIENTED_EDGE('',*,*,#6359,.F.);
#8520=ORIENTED_EDGE('',*,*,#6285,.T.);
#8521=ORIENTED_EDGE('',*,*,#6360,.F.);
#8522=ORIENTED_EDGE('',*,*,#6361,.F.);
#8523=ORIENTED_EDGE('',*,*,#6362,.F.);
#8524=ORIENTED_EDGE('',*,*,#6212,.F.);
#8525=ORIENTED_EDGE('',*,*,#6363,.F.);
#8526=ORIENTED_EDGE('',*,*,#6364,.F.);
#8527=ORIENTED_EDGE('',*,*,#6365,.F.);
#8528=ORIENTED_EDGE('',*,*,#6281,.T.);
#8529=ORIENTED_EDGE('',*,*,#6366,.F.);
#8530=ORIENTED_EDGE('',*,*,#6367,.F.);
#8531=ORIENTED_EDGE('',*,*,#6368,.F.);
#8532=ORIENTED_EDGE('',*,*,#6216,.F.);
#8533=ORIENTED_EDGE('',*,*,#6369,.F.);
#8534=ORIENTED_EDGE('',*,*,#6370,.F.);
#8535=ORIENTED_EDGE('',*,*,#6371,.F.);
#8536=ORIENTED_EDGE('',*,*,#6277,.T.);
#8537=ORIENTED_EDGE('',*,*,#6372,.F.);
#8538=ORIENTED_EDGE('',*,*,#6373,.F.);
#8539=ORIENTED_EDGE('',*,*,#6374,.F.);
#8540=ORIENTED_EDGE('',*,*,#6220,.F.);
#8541=ORIENTED_EDGE('',*,*,#6375,.F.);
#8542=ORIENTED_EDGE('',*,*,#6376,.F.);
#8543=ORIENTED_EDGE('',*,*,#6377,.F.);
#8544=ORIENTED_EDGE('',*,*,#6273,.T.);
#8545=ORIENTED_EDGE('',*,*,#6378,.F.);
#8546=ORIENTED_EDGE('',*,*,#6379,.F.);
#8547=ORIENTED_EDGE('',*,*,#6380,.F.);
#8548=ORIENTED_EDGE('',*,*,#6224,.F.);
#8549=ORIENTED_EDGE('',*,*,#6381,.F.);
#8550=ORIENTED_EDGE('',*,*,#6382,.F.);
#8551=ORIENTED_EDGE('',*,*,#6383,.F.);
#8552=ORIENTED_EDGE('',*,*,#6269,.T.);
#8553=ORIENTED_EDGE('',*,*,#6384,.F.);
#8554=ORIENTED_EDGE('',*,*,#6385,.F.);
#8555=ORIENTED_EDGE('',*,*,#6386,.F.);
#8556=ORIENTED_EDGE('',*,*,#6228,.F.);
#8557=ORIENTED_EDGE('',*,*,#6387,.F.);
#8558=ORIENTED_EDGE('',*,*,#6388,.F.);
#8559=ORIENTED_EDGE('',*,*,#6389,.F.);
#8560=ORIENTED_EDGE('',*,*,#6265,.T.);
#8561=ORIENTED_EDGE('',*,*,#6390,.F.);
#8562=ORIENTED_EDGE('',*,*,#6391,.F.);
#8563=ORIENTED_EDGE('',*,*,#6392,.F.);
#8564=ORIENTED_EDGE('',*,*,#6232,.F.);
#8565=ORIENTED_EDGE('',*,*,#6393,.F.);
#8566=ORIENTED_EDGE('',*,*,#6394,.F.);
#8567=ORIENTED_EDGE('',*,*,#6395,.F.);
#8568=ORIENTED_EDGE('',*,*,#6261,.T.);
#8569=ORIENTED_EDGE('',*,*,#6396,.F.);
#8570=ORIENTED_EDGE('',*,*,#6397,.F.);
#8571=ORIENTED_EDGE('',*,*,#6398,.F.);
#8572=ORIENTED_EDGE('',*,*,#6236,.F.);
#8573=ORIENTED_EDGE('',*,*,#6399,.F.);
#8574=ORIENTED_EDGE('',*,*,#6400,.F.);
#8575=ORIENTED_EDGE('',*,*,#6401,.F.);
#8576=ORIENTED_EDGE('',*,*,#6257,.T.);
#8577=ORIENTED_EDGE('',*,*,#6402,.F.);
#8578=ORIENTED_EDGE('',*,*,#6403,.F.);
#8579=ORIENTED_EDGE('',*,*,#6404,.F.);
#8580=ORIENTED_EDGE('',*,*,#6240,.F.);
#8581=ORIENTED_EDGE('',*,*,#6405,.F.);
#8582=ORIENTED_EDGE('',*,*,#6406,.F.);
#8583=ORIENTED_EDGE('',*,*,#6407,.F.);
#8584=ORIENTED_EDGE('',*,*,#6253,.T.);
#8585=ORIENTED_EDGE('',*,*,#6408,.F.);
#8586=ORIENTED_EDGE('',*,*,#6409,.F.);
#8587=ORIENTED_EDGE('',*,*,#6410,.F.);
#8588=ORIENTED_EDGE('',*,*,#6244,.F.);
#8589=ORIENTED_EDGE('',*,*,#6411,.F.);
#8590=ORIENTED_EDGE('',*,*,#6412,.F.);
#8591=ORIENTED_EDGE('',*,*,#6413,.F.);
#8592=ORIENTED_EDGE('',*,*,#6249,.T.);
#8593=ORIENTED_EDGE('',*,*,#6414,.F.);
#8594=ORIENTED_EDGE('',*,*,#6415,.F.);
#8595=ORIENTED_EDGE('',*,*,#6416,.F.);
#8596=ORIENTED_EDGE('',*,*,#6180,.F.);
#8597=ORIENTED_EDGE('',*,*,#6417,.F.);
#8598=ORIENTED_EDGE('',*,*,#6418,.F.);
#8599=ORIENTED_EDGE('',*,*,#6419,.F.);
#8600=ORIENTED_EDGE('',*,*,#6313,.T.);
#8601=ORIENTED_EDGE('',*,*,#6420,.F.);
#8602=ORIENTED_EDGE('',*,*,#6421,.F.);
#8603=ORIENTED_EDGE('',*,*,#6422,.F.);
#8604=ORIENTED_EDGE('',*,*,#6176,.F.);
#8605=ORIENTED_EDGE('',*,*,#6423,.F.);
#8606=ORIENTED_EDGE('',*,*,#6424,.F.);
#8607=ORIENTED_EDGE('',*,*,#6425,.F.);
#8608=ORIENTED_EDGE('',*,*,#6317,.T.);
#8609=ORIENTED_EDGE('',*,*,#6426,.F.);
#8610=ORIENTED_EDGE('',*,*,#6427,.F.);
#8611=ORIENTED_EDGE('',*,*,#6428,.F.);
#8612=ORIENTED_EDGE('',*,*,#6429,.F.);
#8613=ORIENTED_EDGE('',*,*,#6430,.F.);
#8614=ORIENTED_EDGE('',*,*,#6431,.F.);
#8615=ORIENTED_EDGE('',*,*,#6432,.F.);
#8616=ORIENTED_EDGE('',*,*,#6433,.F.);
#8617=ORIENTED_EDGE('',*,*,#6434,.F.);
#8618=ORIENTED_EDGE('',*,*,#6435,.F.);
#8619=ORIENTED_EDGE('',*,*,#6436,.F.);
#8620=ORIENTED_EDGE('',*,*,#6437,.F.);
#8621=ORIENTED_EDGE('',*,*,#6438,.F.);
#8622=ORIENTED_EDGE('',*,*,#6439,.F.);
#8623=ORIENTED_EDGE('',*,*,#6440,.F.);
#8624=ORIENTED_EDGE('',*,*,#6441,.F.);
#8625=ORIENTED_EDGE('',*,*,#6442,.F.);
#8626=ORIENTED_EDGE('',*,*,#6443,.F.);
#8627=ORIENTED_EDGE('',*,*,#6444,.F.);
#8628=ORIENTED_EDGE('',*,*,#6445,.F.);
#8629=ORIENTED_EDGE('',*,*,#6446,.F.);
#8630=ORIENTED_EDGE('',*,*,#6447,.F.);
#8631=ORIENTED_EDGE('',*,*,#6448,.F.);
#8632=ORIENTED_EDGE('',*,*,#6449,.F.);
#8633=ORIENTED_EDGE('',*,*,#6450,.F.);
#8634=ORIENTED_EDGE('',*,*,#6451,.F.);
#8635=ORIENTED_EDGE('',*,*,#6452,.F.);
#8636=ORIENTED_EDGE('',*,*,#6453,.F.);
#8637=ORIENTED_EDGE('',*,*,#6454,.F.);
#8638=ORIENTED_EDGE('',*,*,#6455,.F.);
#8639=ORIENTED_EDGE('',*,*,#6456,.F.);
#8640=ORIENTED_EDGE('',*,*,#6457,.F.);
#8641=ORIENTED_EDGE('',*,*,#6458,.F.);
#8642=ORIENTED_EDGE('',*,*,#6459,.F.);
#8643=ORIENTED_EDGE('',*,*,#6460,.F.);
#8644=ORIENTED_EDGE('',*,*,#6461,.F.);
#8645=ORIENTED_EDGE('',*,*,#6462,.F.);
#8646=ORIENTED_EDGE('',*,*,#6463,.F.);
#8647=ORIENTED_EDGE('',*,*,#6464,.F.);
#8648=ORIENTED_EDGE('',*,*,#6465,.F.);
#8649=ORIENTED_EDGE('',*,*,#6466,.F.);
#8650=ORIENTED_EDGE('',*,*,#6467,.F.);
#8651=ORIENTED_EDGE('',*,*,#6468,.F.);
#8652=ORIENTED_EDGE('',*,*,#6469,.F.);
#8653=ORIENTED_EDGE('',*,*,#6470,.F.);
#8654=ORIENTED_EDGE('',*,*,#6471,.F.);
#8655=ORIENTED_EDGE('',*,*,#6472,.F.);
#8656=ORIENTED_EDGE('',*,*,#6473,.F.);
#8657=ORIENTED_EDGE('',*,*,#6474,.F.);
#8658=ORIENTED_EDGE('',*,*,#6475,.F.);
#8659=ORIENTED_EDGE('',*,*,#6476,.F.);
#8660=ORIENTED_EDGE('',*,*,#6477,.F.);
#8661=ORIENTED_EDGE('',*,*,#6478,.F.);
#8662=ORIENTED_EDGE('',*,*,#6479,.F.);
#8663=ORIENTED_EDGE('',*,*,#6480,.F.);
#8664=ORIENTED_EDGE('',*,*,#6481,.F.);
#8665=ORIENTED_EDGE('',*,*,#6482,.F.);
#8666=ORIENTED_EDGE('',*,*,#6483,.F.);
#8667=ORIENTED_EDGE('',*,*,#6484,.F.);
#8668=ORIENTED_EDGE('',*,*,#6485,.F.);
#8669=ORIENTED_EDGE('',*,*,#6486,.F.);
#8670=ORIENTED_EDGE('',*,*,#6487,.F.);
#8671=ORIENTED_EDGE('',*,*,#6488,.F.);
#8672=ORIENTED_EDGE('',*,*,#6489,.F.);
#8673=ORIENTED_EDGE('',*,*,#6490,.F.);
#8674=ORIENTED_EDGE('',*,*,#6491,.F.);
#8675=ORIENTED_EDGE('',*,*,#6492,.F.);
#8676=ORIENTED_EDGE('',*,*,#6493,.F.);
#8677=ORIENTED_EDGE('',*,*,#6494,.F.);
#8678=ORIENTED_EDGE('',*,*,#6495,.F.);
#8679=ORIENTED_EDGE('',*,*,#6496,.F.);
#8680=ORIENTED_EDGE('',*,*,#6497,.F.);
#8681=ORIENTED_EDGE('',*,*,#6498,.F.);
#8682=ORIENTED_EDGE('',*,*,#6499,.F.);
#8683=ORIENTED_EDGE('',*,*,#6500,.F.);
#8684=ORIENTED_EDGE('',*,*,#6501,.F.);
#8685=ORIENTED_EDGE('',*,*,#6502,.F.);
#8686=ORIENTED_EDGE('',*,*,#6503,.F.);
#8687=ORIENTED_EDGE('',*,*,#6504,.F.);
#8688=ORIENTED_EDGE('',*,*,#6505,.F.);
#8689=ORIENTED_EDGE('',*,*,#6506,.F.);
#8690=ORIENTED_EDGE('',*,*,#6507,.F.);
#8691=ORIENTED_EDGE('',*,*,#6508,.F.);
#8692=ORIENTED_EDGE('',*,*,#6509,.F.);
#8693=ORIENTED_EDGE('',*,*,#6510,.F.);
#8694=ORIENTED_EDGE('',*,*,#6511,.F.);
#8695=ORIENTED_EDGE('',*,*,#6512,.F.);
#8696=ORIENTED_EDGE('',*,*,#6513,.F.);
#8697=ORIENTED_EDGE('',*,*,#6514,.F.);
#8698=ORIENTED_EDGE('',*,*,#6515,.F.);
#8699=ORIENTED_EDGE('',*,*,#6516,.F.);
#8700=ORIENTED_EDGE('',*,*,#6517,.F.);
#8701=ORIENTED_EDGE('',*,*,#6518,.F.);
#8702=ORIENTED_EDGE('',*,*,#6519,.F.);
#8703=ORIENTED_EDGE('',*,*,#6520,.F.);
#8704=ORIENTED_EDGE('',*,*,#6521,.F.);
#8705=ORIENTED_EDGE('',*,*,#6522,.F.);
#8706=ORIENTED_EDGE('',*,*,#6523,.F.);
#8707=ORIENTED_EDGE('',*,*,#6524,.F.);
#8708=ORIENTED_EDGE('',*,*,#6525,.F.);
#8709=ORIENTED_EDGE('',*,*,#6526,.F.);
#8710=ORIENTED_EDGE('',*,*,#6527,.F.);
#8711=ORIENTED_EDGE('',*,*,#6528,.F.);
#8712=ORIENTED_EDGE('',*,*,#6529,.F.);
#8713=ORIENTED_EDGE('',*,*,#6530,.F.);
#8714=ORIENTED_EDGE('',*,*,#6531,.F.);
#8715=ORIENTED_EDGE('',*,*,#6532,.F.);
#8716=ORIENTED_EDGE('',*,*,#6533,.F.);
#8717=ORIENTED_EDGE('',*,*,#6534,.F.);
#8718=ORIENTED_EDGE('',*,*,#6535,.F.);
#8719=ORIENTED_EDGE('',*,*,#6536,.F.);
#8720=ORIENTED_EDGE('',*,*,#6537,.F.);
#8721=ORIENTED_EDGE('',*,*,#6538,.F.);
#8722=ORIENTED_EDGE('',*,*,#6539,.F.);
#8723=ORIENTED_EDGE('',*,*,#6540,.F.);
#8724=ORIENTED_EDGE('',*,*,#6541,.F.);
#8725=ORIENTED_EDGE('',*,*,#6542,.F.);
#8726=ORIENTED_EDGE('',*,*,#6543,.F.);
#8727=ORIENTED_EDGE('',*,*,#6544,.F.);
#8728=ORIENTED_EDGE('',*,*,#6545,.F.);
#8729=ORIENTED_EDGE('',*,*,#6546,.F.);
#8730=ORIENTED_EDGE('',*,*,#6547,.F.);
#8731=ORIENTED_EDGE('',*,*,#6548,.F.);
#8732=ORIENTED_EDGE('',*,*,#6549,.F.);
#8733=ORIENTED_EDGE('',*,*,#6550,.F.);
#8734=ORIENTED_EDGE('',*,*,#6551,.F.);
#8735=ORIENTED_EDGE('',*,*,#6552,.F.);
#8736=ORIENTED_EDGE('',*,*,#6553,.F.);
#8737=ORIENTED_EDGE('',*,*,#6554,.F.);
#8738=ORIENTED_EDGE('',*,*,#6555,.F.);
#8739=ORIENTED_EDGE('',*,*,#6556,.F.);
#8740=ORIENTED_EDGE('',*,*,#6557,.F.);
#8741=ORIENTED_EDGE('',*,*,#6558,.F.);
#8742=ORIENTED_EDGE('',*,*,#6559,.F.);
#8743=ORIENTED_EDGE('',*,*,#6560,.F.);
#8744=ORIENTED_EDGE('',*,*,#6561,.F.);
#8745=ORIENTED_EDGE('',*,*,#6562,.F.);
#8746=ORIENTED_EDGE('',*,*,#6563,.F.);
#8747=ORIENTED_EDGE('',*,*,#6564,.F.);
#8748=ORIENTED_EDGE('',*,*,#6565,.F.);
#8749=ORIENTED_EDGE('',*,*,#6566,.F.);
#8750=ORIENTED_EDGE('',*,*,#6567,.F.);
#8751=ORIENTED_EDGE('',*,*,#6568,.F.);
#8752=ORIENTED_EDGE('',*,*,#6569,.F.);
#8753=ORIENTED_EDGE('',*,*,#6570,.F.);
#8754=ORIENTED_EDGE('',*,*,#6571,.F.);
#8755=ORIENTED_EDGE('',*,*,#6572,.F.);
#8756=ORIENTED_EDGE('',*,*,#6433,.T.);
#8757=ORIENTED_EDGE('',*,*,#6573,.F.);
#8758=ORIENTED_EDGE('',*,*,#6574,.F.);
#8759=ORIENTED_EDGE('',*,*,#6575,.F.);
#8760=ORIENTED_EDGE('',*,*,#6441,.T.);
#8761=ORIENTED_EDGE('',*,*,#6576,.F.);
#8762=ORIENTED_EDGE('',*,*,#6577,.F.);
#8763=ORIENTED_EDGE('',*,*,#6578,.F.);
#8764=ORIENTED_EDGE('',*,*,#6449,.T.);
#8765=ORIENTED_EDGE('',*,*,#6579,.F.);
#8766=ORIENTED_EDGE('',*,*,#6580,.F.);
#8767=ORIENTED_EDGE('',*,*,#6581,.F.);
#8768=ORIENTED_EDGE('',*,*,#6457,.T.);
#8769=ORIENTED_EDGE('',*,*,#6582,.F.);
#8770=ORIENTED_EDGE('',*,*,#6583,.F.);
#8771=ORIENTED_EDGE('',*,*,#6584,.F.);
#8772=ORIENTED_EDGE('',*,*,#6465,.T.);
#8773=ORIENTED_EDGE('',*,*,#6585,.F.);
#8774=ORIENTED_EDGE('',*,*,#6586,.F.);
#8775=ORIENTED_EDGE('',*,*,#6587,.F.);
#8776=ORIENTED_EDGE('',*,*,#6473,.T.);
#8777=ORIENTED_EDGE('',*,*,#6588,.F.);
#8778=ORIENTED_EDGE('',*,*,#6589,.F.);
#8779=ORIENTED_EDGE('',*,*,#6590,.F.);
#8780=ORIENTED_EDGE('',*,*,#6481,.T.);
#8781=ORIENTED_EDGE('',*,*,#6591,.F.);
#8782=ORIENTED_EDGE('',*,*,#6592,.F.);
#8783=ORIENTED_EDGE('',*,*,#6593,.F.);
#8784=ORIENTED_EDGE('',*,*,#6489,.T.);
#8785=ORIENTED_EDGE('',*,*,#6594,.F.);
#8786=ORIENTED_EDGE('',*,*,#6595,.F.);
#8787=ORIENTED_EDGE('',*,*,#6596,.F.);
#8788=ORIENTED_EDGE('',*,*,#6497,.T.);
#8789=ORIENTED_EDGE('',*,*,#6597,.F.);
#8790=ORIENTED_EDGE('',*,*,#6598,.F.);
#8791=ORIENTED_EDGE('',*,*,#6599,.F.);
#8792=ORIENTED_EDGE('',*,*,#6505,.T.);
#8793=ORIENTED_EDGE('',*,*,#6600,.F.);
#8794=ORIENTED_EDGE('',*,*,#6601,.F.);
#8795=ORIENTED_EDGE('',*,*,#6602,.F.);
#8796=ORIENTED_EDGE('',*,*,#6513,.T.);
#8797=ORIENTED_EDGE('',*,*,#6603,.F.);
#8798=ORIENTED_EDGE('',*,*,#6604,.F.);
#8799=ORIENTED_EDGE('',*,*,#6605,.F.);
#8800=ORIENTED_EDGE('',*,*,#6521,.T.);
#8801=ORIENTED_EDGE('',*,*,#6606,.F.);
#8802=ORIENTED_EDGE('',*,*,#6607,.F.);
#8803=ORIENTED_EDGE('',*,*,#6608,.F.);
#8804=ORIENTED_EDGE('',*,*,#6529,.T.);
#8805=ORIENTED_EDGE('',*,*,#6609,.F.);
#8806=ORIENTED_EDGE('',*,*,#6610,.F.);
#8807=ORIENTED_EDGE('',*,*,#6611,.F.);
#8808=ORIENTED_EDGE('',*,*,#6537,.T.);
#8809=ORIENTED_EDGE('',*,*,#6612,.F.);
#8810=ORIENTED_EDGE('',*,*,#6613,.F.);
#8811=ORIENTED_EDGE('',*,*,#6614,.F.);
#8812=ORIENTED_EDGE('',*,*,#6545,.T.);
#8813=ORIENTED_EDGE('',*,*,#6615,.F.);
#8814=ORIENTED_EDGE('',*,*,#6616,.F.);
#8815=ORIENTED_EDGE('',*,*,#6617,.F.);
#8816=ORIENTED_EDGE('',*,*,#6553,.T.);
#8817=ORIENTED_EDGE('',*,*,#6618,.F.);
#8818=ORIENTED_EDGE('',*,*,#6619,.F.);
#8819=ORIENTED_EDGE('',*,*,#6620,.F.);
#8820=ORIENTED_EDGE('',*,*,#6561,.T.);
#8821=ORIENTED_EDGE('',*,*,#6621,.F.);
#8822=ORIENTED_EDGE('',*,*,#6622,.F.);
#8823=ORIENTED_EDGE('',*,*,#6623,.F.);
#8824=ORIENTED_EDGE('',*,*,#6569,.T.);
#8825=ORIENTED_EDGE('',*,*,#6624,.F.);
#8826=ORIENTED_EDGE('',*,*,#6625,.F.);
#8827=ORIENTED_EDGE('',*,*,#6626,.F.);
#8828=ORIENTED_EDGE('',*,*,#6627,.F.);
#8829=ORIENTED_EDGE('',*,*,#6628,.F.);
#8830=ORIENTED_EDGE('',*,*,#6629,.F.);
#8831=ORIENTED_EDGE('',*,*,#6630,.F.);
#8832=ORIENTED_EDGE('',*,*,#6631,.F.);
#8833=ORIENTED_EDGE('',*,*,#6632,.F.);
#8834=ORIENTED_EDGE('',*,*,#6633,.F.);
#8835=ORIENTED_EDGE('',*,*,#6634,.F.);
#8836=ORIENTED_EDGE('',*,*,#6635,.F.);
#8837=ORIENTED_EDGE('',*,*,#6636,.F.);
#8838=ORIENTED_EDGE('',*,*,#6637,.F.);
#8839=ORIENTED_EDGE('',*,*,#6638,.F.);
#8840=ORIENTED_EDGE('',*,*,#6639,.F.);
#8841=ORIENTED_EDGE('',*,*,#6640,.F.);
#8842=ORIENTED_EDGE('',*,*,#6641,.F.);
#8843=ORIENTED_EDGE('',*,*,#6642,.F.);
#8844=ORIENTED_EDGE('',*,*,#6643,.F.);
#8845=ORIENTED_EDGE('',*,*,#6644,.F.);
#8846=ORIENTED_EDGE('',*,*,#6645,.F.);
#8847=ORIENTED_EDGE('',*,*,#6646,.F.);
#8848=ORIENTED_EDGE('',*,*,#6647,.F.);
#8849=ORIENTED_EDGE('',*,*,#6648,.F.);
#8850=ORIENTED_EDGE('',*,*,#6649,.F.);
#8851=ORIENTED_EDGE('',*,*,#6650,.F.);
#8852=ORIENTED_EDGE('',*,*,#6651,.F.);
#8853=ORIENTED_EDGE('',*,*,#6652,.F.);
#8854=ORIENTED_EDGE('',*,*,#6653,.F.);
#8855=ORIENTED_EDGE('',*,*,#6654,.F.);
#8856=ORIENTED_EDGE('',*,*,#6655,.F.);
#8857=ORIENTED_EDGE('',*,*,#6656,.F.);
#8858=ORIENTED_EDGE('',*,*,#6657,.F.);
#8859=ORIENTED_EDGE('',*,*,#6658,.F.);
#8860=ORIENTED_EDGE('',*,*,#6659,.F.);
#8861=ORIENTED_EDGE('',*,*,#6660,.F.);
#8862=ORIENTED_EDGE('',*,*,#6661,.F.);
#8863=ORIENTED_EDGE('',*,*,#6662,.F.);
#8864=ORIENTED_EDGE('',*,*,#6663,.F.);
#8865=ORIENTED_EDGE('',*,*,#6664,.F.);
#8866=ORIENTED_EDGE('',*,*,#6665,.F.);
#8867=ORIENTED_EDGE('',*,*,#6666,.F.);
#8868=ORIENTED_EDGE('',*,*,#6667,.F.);
#8869=ORIENTED_EDGE('',*,*,#6668,.F.);
#8870=ORIENTED_EDGE('',*,*,#6669,.F.);
#8871=ORIENTED_EDGE('',*,*,#6670,.F.);
#8872=ORIENTED_EDGE('',*,*,#6671,.F.);
#8873=ORIENTED_EDGE('',*,*,#6672,.F.);
#8874=ORIENTED_EDGE('',*,*,#6673,.F.);
#8875=ORIENTED_EDGE('',*,*,#6674,.F.);
#8876=ORIENTED_EDGE('',*,*,#6675,.F.);
#8877=ORIENTED_EDGE('',*,*,#6676,.F.);
#8878=ORIENTED_EDGE('',*,*,#6677,.F.);
#8879=ORIENTED_EDGE('',*,*,#6678,.F.);
#8880=ORIENTED_EDGE('',*,*,#6679,.F.);
#8881=ORIENTED_EDGE('',*,*,#6680,.F.);
#8882=ORIENTED_EDGE('',*,*,#6681,.F.);
#8883=ORIENTED_EDGE('',*,*,#6682,.F.);
#8884=ORIENTED_EDGE('',*,*,#6683,.F.);
#8885=ORIENTED_EDGE('',*,*,#6684,.F.);
#8886=ORIENTED_EDGE('',*,*,#6685,.F.);
#8887=ORIENTED_EDGE('',*,*,#6686,.F.);
#8888=ORIENTED_EDGE('',*,*,#6687,.F.);
#8889=ORIENTED_EDGE('',*,*,#6688,.F.);
#8890=ORIENTED_EDGE('',*,*,#6689,.F.);
#8891=ORIENTED_EDGE('',*,*,#6690,.F.);
#8892=ORIENTED_EDGE('',*,*,#6691,.F.);
#8893=ORIENTED_EDGE('',*,*,#6692,.F.);
#8894=ORIENTED_EDGE('',*,*,#6693,.F.);
#8895=ORIENTED_EDGE('',*,*,#6694,.F.);
#8896=ORIENTED_EDGE('',*,*,#6695,.F.);
#8897=ORIENTED_EDGE('',*,*,#6696,.F.);
#8898=ORIENTED_EDGE('',*,*,#6697,.F.);
#8899=ORIENTED_EDGE('',*,*,#6698,.F.);
#8900=ORIENTED_EDGE('',*,*,#6699,.T.);
#8901=ORIENTED_EDGE('',*,*,#6700,.F.);
#8902=ORIENTED_EDGE('',*,*,#6701,.F.);
#8903=ORIENTED_EDGE('',*,*,#6702,.F.);
#8904=ORIENTED_EDGE('',*,*,#6703,.T.);
#8905=ORIENTED_EDGE('',*,*,#6704,.F.);
#8906=ORIENTED_EDGE('',*,*,#6705,.F.);
#8907=ORIENTED_EDGE('',*,*,#6706,.F.);
#8908=ORIENTED_EDGE('',*,*,#6707,.T.);
#8909=ORIENTED_EDGE('',*,*,#6708,.F.);
#8910=ORIENTED_EDGE('',*,*,#6709,.F.);
#8911=ORIENTED_EDGE('',*,*,#6710,.F.);
#8912=ORIENTED_EDGE('',*,*,#6711,.T.);
#8913=ORIENTED_EDGE('',*,*,#6712,.F.);
#8914=ORIENTED_EDGE('',*,*,#6713,.F.);
#8915=ORIENTED_EDGE('',*,*,#6714,.F.);
#8916=ORIENTED_EDGE('',*,*,#6715,.T.);
#8917=ORIENTED_EDGE('',*,*,#6716,.F.);
#8918=ORIENTED_EDGE('',*,*,#6717,.F.);
#8919=ORIENTED_EDGE('',*,*,#6718,.F.);
#8920=ORIENTED_EDGE('',*,*,#6719,.T.);
#8921=ORIENTED_EDGE('',*,*,#6720,.F.);
#8922=ORIENTED_EDGE('',*,*,#6721,.F.);
#8923=ORIENTED_EDGE('',*,*,#6722,.F.);
#8924=ORIENTED_EDGE('',*,*,#6723,.T.);
#8925=ORIENTED_EDGE('',*,*,#6724,.F.);
#8926=ORIENTED_EDGE('',*,*,#6725,.F.);
#8927=ORIENTED_EDGE('',*,*,#6726,.F.);
#8928=ORIENTED_EDGE('',*,*,#6727,.T.);
#8929=ORIENTED_EDGE('',*,*,#6728,.F.);
#8930=ORIENTED_EDGE('',*,*,#6729,.F.);
#8931=ORIENTED_EDGE('',*,*,#6730,.F.);
#8932=ORIENTED_EDGE('',*,*,#6731,.T.);
#8933=ORIENTED_EDGE('',*,*,#6732,.F.);
#8934=ORIENTED_EDGE('',*,*,#6733,.F.);
#8935=ORIENTED_EDGE('',*,*,#6734,.F.);
#8936=ORIENTED_EDGE('',*,*,#6735,.T.);
#8937=ORIENTED_EDGE('',*,*,#6736,.F.);
#8938=ORIENTED_EDGE('',*,*,#6737,.F.);
#8939=ORIENTED_EDGE('',*,*,#6738,.F.);
#8940=ORIENTED_EDGE('',*,*,#6739,.T.);
#8941=ORIENTED_EDGE('',*,*,#6740,.F.);
#8942=ORIENTED_EDGE('',*,*,#6741,.F.);
#8943=ORIENTED_EDGE('',*,*,#6742,.F.);
#8944=ORIENTED_EDGE('',*,*,#6743,.T.);
#8945=ORIENTED_EDGE('',*,*,#6744,.F.);
#8946=ORIENTED_EDGE('',*,*,#6745,.F.);
#8947=ORIENTED_EDGE('',*,*,#6746,.F.);
#8948=ORIENTED_EDGE('',*,*,#6747,.T.);
#8949=ORIENTED_EDGE('',*,*,#6748,.F.);
#8950=ORIENTED_EDGE('',*,*,#6749,.F.);
#8951=ORIENTED_EDGE('',*,*,#6750,.F.);
#8952=ORIENTED_EDGE('',*,*,#6751,.T.);
#8953=ORIENTED_EDGE('',*,*,#6752,.F.);
#8954=ORIENTED_EDGE('',*,*,#6753,.F.);
#8955=ORIENTED_EDGE('',*,*,#6754,.F.);
#8956=ORIENTED_EDGE('',*,*,#6755,.T.);
#8957=ORIENTED_EDGE('',*,*,#6756,.F.);
#8958=ORIENTED_EDGE('',*,*,#6757,.F.);
#8959=ORIENTED_EDGE('',*,*,#6758,.F.);
#8960=ORIENTED_EDGE('',*,*,#6759,.T.);
#8961=ORIENTED_EDGE('',*,*,#6760,.F.);
#8962=ORIENTED_EDGE('',*,*,#6761,.F.);
#8963=ORIENTED_EDGE('',*,*,#6762,.F.);
#8964=ORIENTED_EDGE('',*,*,#6763,.T.);
#8965=ORIENTED_EDGE('',*,*,#6764,.F.);
#8966=ORIENTED_EDGE('',*,*,#6765,.F.);
#8967=ORIENTED_EDGE('',*,*,#6766,.F.);
#8968=ORIENTED_EDGE('',*,*,#6767,.T.);
#8969=ORIENTED_EDGE('',*,*,#6768,.F.);
#8970=ORIENTED_EDGE('',*,*,#6769,.F.);
#8971=ORIENTED_EDGE('',*,*,#6770,.F.);
#8972=ORIENTED_EDGE('',*,*,#6629,.T.);
#8973=ORIENTED_EDGE('',*,*,#6771,.F.);
#8974=ORIENTED_EDGE('',*,*,#6699,.F.);
#8975=ORIENTED_EDGE('',*,*,#6772,.F.);
#8976=ORIENTED_EDGE('',*,*,#6633,.T.);
#8977=ORIENTED_EDGE('',*,*,#6773,.F.);
#8978=ORIENTED_EDGE('',*,*,#6703,.F.);
#8979=ORIENTED_EDGE('',*,*,#6774,.F.);
#8980=ORIENTED_EDGE('',*,*,#6637,.T.);
#8981=ORIENTED_EDGE('',*,*,#6775,.F.);
#8982=ORIENTED_EDGE('',*,*,#6707,.F.);
#8983=ORIENTED_EDGE('',*,*,#6776,.F.);
#8984=ORIENTED_EDGE('',*,*,#6641,.T.);
#8985=ORIENTED_EDGE('',*,*,#6777,.F.);
#8986=ORIENTED_EDGE('',*,*,#6711,.F.);
#8987=ORIENTED_EDGE('',*,*,#6778,.F.);
#8988=ORIENTED_EDGE('',*,*,#6645,.T.);
#8989=ORIENTED_EDGE('',*,*,#6779,.F.);
#8990=ORIENTED_EDGE('',*,*,#6715,.F.);
#8991=ORIENTED_EDGE('',*,*,#6780,.F.);
#8992=ORIENTED_EDGE('',*,*,#6649,.T.);
#8993=ORIENTED_EDGE('',*,*,#6781,.F.);
#8994=ORIENTED_EDGE('',*,*,#6719,.F.);
#8995=ORIENTED_EDGE('',*,*,#6782,.F.);
#8996=ORIENTED_EDGE('',*,*,#6653,.T.);
#8997=ORIENTED_EDGE('',*,*,#6783,.F.);
#8998=ORIENTED_EDGE('',*,*,#6723,.F.);
#8999=ORIENTED_EDGE('',*,*,#6784,.F.);
#9000=ORIENTED_EDGE('',*,*,#6657,.T.);
#9001=ORIENTED_EDGE('',*,*,#6785,.F.);
#9002=ORIENTED_EDGE('',*,*,#6727,.F.);
#9003=ORIENTED_EDGE('',*,*,#6786,.F.);
#9004=ORIENTED_EDGE('',*,*,#6661,.T.);
#9005=ORIENTED_EDGE('',*,*,#6787,.F.);
#9006=ORIENTED_EDGE('',*,*,#6731,.F.);
#9007=ORIENTED_EDGE('',*,*,#6788,.F.);
#9008=ORIENTED_EDGE('',*,*,#6665,.T.);
#9009=ORIENTED_EDGE('',*,*,#6789,.F.);
#9010=ORIENTED_EDGE('',*,*,#6735,.F.);
#9011=ORIENTED_EDGE('',*,*,#6790,.F.);
#9012=ORIENTED_EDGE('',*,*,#6669,.T.);
#9013=ORIENTED_EDGE('',*,*,#6791,.F.);
#9014=ORIENTED_EDGE('',*,*,#6739,.F.);
#9015=ORIENTED_EDGE('',*,*,#6792,.F.);
#9016=ORIENTED_EDGE('',*,*,#6673,.T.);
#9017=ORIENTED_EDGE('',*,*,#6793,.F.);
#9018=ORIENTED_EDGE('',*,*,#6743,.F.);
#9019=ORIENTED_EDGE('',*,*,#6794,.F.);
#9020=ORIENTED_EDGE('',*,*,#6677,.T.);
#9021=ORIENTED_EDGE('',*,*,#6795,.F.);
#9022=ORIENTED_EDGE('',*,*,#6747,.F.);
#9023=ORIENTED_EDGE('',*,*,#6796,.F.);
#9024=ORIENTED_EDGE('',*,*,#6681,.T.);
#9025=ORIENTED_EDGE('',*,*,#6797,.F.);
#9026=ORIENTED_EDGE('',*,*,#6751,.F.);
#9027=ORIENTED_EDGE('',*,*,#6798,.F.);
#9028=ORIENTED_EDGE('',*,*,#6685,.T.);
#9029=ORIENTED_EDGE('',*,*,#6799,.F.);
#9030=ORIENTED_EDGE('',*,*,#6755,.F.);
#9031=ORIENTED_EDGE('',*,*,#6800,.F.);
#9032=ORIENTED_EDGE('',*,*,#6689,.T.);
#9033=ORIENTED_EDGE('',*,*,#6801,.F.);
#9034=ORIENTED_EDGE('',*,*,#6759,.F.);
#9035=ORIENTED_EDGE('',*,*,#6802,.F.);
#9036=ORIENTED_EDGE('',*,*,#6693,.T.);
#9037=ORIENTED_EDGE('',*,*,#6803,.F.);
#9038=ORIENTED_EDGE('',*,*,#6763,.F.);
#9039=ORIENTED_EDGE('',*,*,#6804,.F.);
#9040=ORIENTED_EDGE('',*,*,#6697,.T.);
#9041=ORIENTED_EDGE('',*,*,#6805,.F.);
#9042=ORIENTED_EDGE('',*,*,#6767,.F.);
#9043=ORIENTED_EDGE('',*,*,#6427,.T.);
#9044=ORIENTED_EDGE('',*,*,#6806,.F.);
#9045=ORIENTED_EDGE('',*,*,#6567,.T.);
#9046=ORIENTED_EDGE('',*,*,#6807,.T.);
#9047=ORIENTED_EDGE('',*,*,#6415,.T.);
#9048=ORIENTED_EDGE('',*,*,#6808,.F.);
#9049=ORIENTED_EDGE('',*,*,#6559,.T.);
#9050=ORIENTED_EDGE('',*,*,#6809,.T.);
#9051=ORIENTED_EDGE('',*,*,#6409,.T.);
#9052=ORIENTED_EDGE('',*,*,#6810,.F.);
#9053=ORIENTED_EDGE('',*,*,#6551,.T.);
#9054=ORIENTED_EDGE('',*,*,#6811,.T.);
#9055=ORIENTED_EDGE('',*,*,#6403,.T.);
#9056=ORIENTED_EDGE('',*,*,#6812,.F.);
#9057=ORIENTED_EDGE('',*,*,#6543,.T.);
#9058=ORIENTED_EDGE('',*,*,#6813,.T.);
#9059=ORIENTED_EDGE('',*,*,#6397,.T.);
#9060=ORIENTED_EDGE('',*,*,#6814,.F.);
#9061=ORIENTED_EDGE('',*,*,#6535,.T.);
#9062=ORIENTED_EDGE('',*,*,#6815,.T.);
#9063=ORIENTED_EDGE('',*,*,#6391,.T.);
#9064=ORIENTED_EDGE('',*,*,#6816,.F.);
#9065=ORIENTED_EDGE('',*,*,#6527,.T.);
#9066=ORIENTED_EDGE('',*,*,#6817,.T.);
#9067=ORIENTED_EDGE('',*,*,#6385,.T.);
#9068=ORIENTED_EDGE('',*,*,#6818,.F.);
#9069=ORIENTED_EDGE('',*,*,#6519,.T.);
#9070=ORIENTED_EDGE('',*,*,#6819,.T.);
#9071=ORIENTED_EDGE('',*,*,#6379,.T.);
#9072=ORIENTED_EDGE('',*,*,#6820,.F.);
#9073=ORIENTED_EDGE('',*,*,#6511,.T.);
#9074=ORIENTED_EDGE('',*,*,#6821,.T.);
#9075=ORIENTED_EDGE('',*,*,#6373,.T.);
#9076=ORIENTED_EDGE('',*,*,#6822,.F.);
#9077=ORIENTED_EDGE('',*,*,#6503,.T.);
#9078=ORIENTED_EDGE('',*,*,#6823,.T.);
#9079=ORIENTED_EDGE('',*,*,#6367,.T.);
#9080=ORIENTED_EDGE('',*,*,#6824,.F.);
#9081=ORIENTED_EDGE('',*,*,#6495,.T.);
#9082=ORIENTED_EDGE('',*,*,#6825,.T.);
#9083=ORIENTED_EDGE('',*,*,#6361,.T.);
#9084=ORIENTED_EDGE('',*,*,#6826,.F.);
#9085=ORIENTED_EDGE('',*,*,#6487,.T.);
#9086=ORIENTED_EDGE('',*,*,#6827,.T.);
#9087=ORIENTED_EDGE('',*,*,#6355,.T.);
#9088=ORIENTED_EDGE('',*,*,#6828,.F.);
#9089=ORIENTED_EDGE('',*,*,#6479,.T.);
#9090=ORIENTED_EDGE('',*,*,#6829,.T.);
#9091=ORIENTED_EDGE('',*,*,#6349,.T.);
#9092=ORIENTED_EDGE('',*,*,#6830,.F.);
#9093=ORIENTED_EDGE('',*,*,#6471,.T.);
#9094=ORIENTED_EDGE('',*,*,#6831,.T.);
#9095=ORIENTED_EDGE('',*,*,#6343,.T.);
#9096=ORIENTED_EDGE('',*,*,#6832,.F.);
#9097=ORIENTED_EDGE('',*,*,#6463,.T.);
#9098=ORIENTED_EDGE('',*,*,#6833,.T.);
#9099=ORIENTED_EDGE('',*,*,#6337,.T.);
#9100=ORIENTED_EDGE('',*,*,#6834,.F.);
#9101=ORIENTED_EDGE('',*,*,#6455,.T.);
#9102=ORIENTED_EDGE('',*,*,#6835,.T.);
#9103=ORIENTED_EDGE('',*,*,#6331,.T.);
#9104=ORIENTED_EDGE('',*,*,#6836,.F.);
#9105=ORIENTED_EDGE('',*,*,#6447,.T.);
#9106=ORIENTED_EDGE('',*,*,#6837,.T.);
#9107=ORIENTED_EDGE('',*,*,#6325,.T.);
#9108=ORIENTED_EDGE('',*,*,#6838,.F.);
#9109=ORIENTED_EDGE('',*,*,#6439,.T.);
#9110=ORIENTED_EDGE('',*,*,#6839,.T.);
#9111=ORIENTED_EDGE('',*,*,#6421,.T.);
#9112=ORIENTED_EDGE('',*,*,#6840,.F.);
#9113=ORIENTED_EDGE('',*,*,#6431,.T.);
#9114=ORIENTED_EDGE('',*,*,#6841,.T.);
#9115=ORIENTED_EDGE('',*,*,#6318,.T.);
#9116=ORIENTED_EDGE('',*,*,#6425,.T.);
#9117=ORIENTED_EDGE('',*,*,#6842,.F.);
#9118=ORIENTED_EDGE('',*,*,#6570,.T.);
#9119=ORIENTED_EDGE('',*,*,#6623,.T.);
#9120=ORIENTED_EDGE('',*,*,#6843,.T.);
#9121=ORIENTED_EDGE('',*,*,#6694,.T.);
#9122=ORIENTED_EDGE('',*,*,#6804,.T.);
#9123=ORIENTED_EDGE('',*,*,#6766,.T.);
#9124=ORIENTED_EDGE('',*,*,#6844,.T.);
#9125=ORIENTED_EDGE('',*,*,#6426,.T.);
#9126=ORIENTED_EDGE('',*,*,#6316,.T.);
#9127=ORIENTED_EDGE('',*,*,#6845,.F.);
#9128=ORIENTED_EDGE('',*,*,#6768,.T.);
#9129=ORIENTED_EDGE('',*,*,#6805,.T.);
#9130=ORIENTED_EDGE('',*,*,#6696,.T.);
#9131=ORIENTED_EDGE('',*,*,#6846,.F.);
#9132=ORIENTED_EDGE('',*,*,#6624,.T.);
#9133=ORIENTED_EDGE('',*,*,#6568,.T.);
#9134=ORIENTED_EDGE('',*,*,#6806,.T.);
#9135=ORIENTED_EDGE('',*,*,#6625,.T.);
#9136=ORIENTED_EDGE('',*,*,#6846,.T.);
#9137=ORIENTED_EDGE('',*,*,#6695,.T.);
#9138=ORIENTED_EDGE('',*,*,#6843,.F.);
#9139=ORIENTED_EDGE('',*,*,#6319,.T.);
#9140=ORIENTED_EDGE('',*,*,#6844,.F.);
#9141=ORIENTED_EDGE('',*,*,#6769,.T.);
#9142=ORIENTED_EDGE('',*,*,#6845,.T.);
#9143=ORIENTED_EDGE('',*,*,#6250,.T.);
#9144=ORIENTED_EDGE('',*,*,#6413,.T.);
#9145=ORIENTED_EDGE('',*,*,#6847,.F.);
#9146=ORIENTED_EDGE('',*,*,#6562,.T.);
#9147=ORIENTED_EDGE('',*,*,#6620,.T.);
#9148=ORIENTED_EDGE('',*,*,#6848,.T.);
#9149=ORIENTED_EDGE('',*,*,#6690,.T.);
#9150=ORIENTED_EDGE('',*,*,#6802,.T.);
#9151=ORIENTED_EDGE('',*,*,#6762,.T.);
#9152=ORIENTED_EDGE('',*,*,#6849,.T.);
#9153=ORIENTED_EDGE('',*,*,#6414,.T.);
#9154=ORIENTED_EDGE('',*,*,#6248,.T.);
#9155=ORIENTED_EDGE('',*,*,#6850,.F.);
#9156=ORIENTED_EDGE('',*,*,#6764,.T.);
#9157=ORIENTED_EDGE('',*,*,#6803,.T.);
#9158=ORIENTED_EDGE('',*,*,#6692,.T.);
#9159=ORIENTED_EDGE('',*,*,#6851,.F.);
#9160=ORIENTED_EDGE('',*,*,#6621,.T.);
#9161=ORIENTED_EDGE('',*,*,#6560,.T.);
#9162=ORIENTED_EDGE('',*,*,#6808,.T.);
#9163=ORIENTED_EDGE('',*,*,#6622,.T.);
#9164=ORIENTED_EDGE('',*,*,#6851,.T.);
#9165=ORIENTED_EDGE('',*,*,#6691,.T.);
#9166=ORIENTED_EDGE('',*,*,#6848,.F.);
#9167=ORIENTED_EDGE('',*,*,#6251,.T.);
#9168=ORIENTED_EDGE('',*,*,#6849,.F.);
#9169=ORIENTED_EDGE('',*,*,#6765,.T.);
#9170=ORIENTED_EDGE('',*,*,#6850,.T.);
#9171=ORIENTED_EDGE('',*,*,#6254,.T.);
#9172=ORIENTED_EDGE('',*,*,#6407,.T.);
#9173=ORIENTED_EDGE('',*,*,#6852,.F.);
#9174=ORIENTED_EDGE('',*,*,#6554,.T.);
#9175=ORIENTED_EDGE('',*,*,#6617,.T.);
#9176=ORIENTED_EDGE('',*,*,#6853,.T.);
#9177=ORIENTED_EDGE('',*,*,#6686,.T.);
#9178=ORIENTED_EDGE('',*,*,#6800,.T.);
#9179=ORIENTED_EDGE('',*,*,#6758,.T.);
#9180=ORIENTED_EDGE('',*,*,#6854,.T.);
#9181=ORIENTED_EDGE('',*,*,#6408,.T.);
#9182=ORIENTED_EDGE('',*,*,#6252,.T.);
#9183=ORIENTED_EDGE('',*,*,#6855,.F.);
#9184=ORIENTED_EDGE('',*,*,#6760,.T.);
#9185=ORIENTED_EDGE('',*,*,#6801,.T.);
#9186=ORIENTED_EDGE('',*,*,#6688,.T.);
#9187=ORIENTED_EDGE('',*,*,#6856,.F.);
#9188=ORIENTED_EDGE('',*,*,#6618,.T.);
#9189=ORIENTED_EDGE('',*,*,#6552,.T.);
#9190=ORIENTED_EDGE('',*,*,#6810,.T.);
#9191=ORIENTED_EDGE('',*,*,#6619,.T.);
#9192=ORIENTED_EDGE('',*,*,#6856,.T.);
#9193=ORIENTED_EDGE('',*,*,#6687,.T.);
#9194=ORIENTED_EDGE('',*,*,#6853,.F.);
#9195=ORIENTED_EDGE('',*,*,#6255,.T.);
#9196=ORIENTED_EDGE('',*,*,#6854,.F.);
#9197=ORIENTED_EDGE('',*,*,#6761,.T.);
#9198=ORIENTED_EDGE('',*,*,#6855,.T.);
#9199=ORIENTED_EDGE('',*,*,#6258,.T.);
#9200=ORIENTED_EDGE('',*,*,#6401,.T.);
#9201=ORIENTED_EDGE('',*,*,#6857,.F.);
#9202=ORIENTED_EDGE('',*,*,#6546,.T.);
#9203=ORIENTED_EDGE('',*,*,#6614,.T.);
#9204=ORIENTED_EDGE('',*,*,#6858,.T.);
#9205=ORIENTED_EDGE('',*,*,#6682,.T.);
#9206=ORIENTED_EDGE('',*,*,#6798,.T.);
#9207=ORIENTED_EDGE('',*,*,#6754,.T.);
#9208=ORIENTED_EDGE('',*,*,#6859,.T.);
#9209=ORIENTED_EDGE('',*,*,#6402,.T.);
#9210=ORIENTED_EDGE('',*,*,#6256,.T.);
#9211=ORIENTED_EDGE('',*,*,#6860,.F.);
#9212=ORIENTED_EDGE('',*,*,#6756,.T.);
#9213=ORIENTED_EDGE('',*,*,#6799,.T.);
#9214=ORIENTED_EDGE('',*,*,#6684,.T.);
#9215=ORIENTED_EDGE('',*,*,#6861,.F.);
#9216=ORIENTED_EDGE('',*,*,#6615,.T.);
#9217=ORIENTED_EDGE('',*,*,#6544,.T.);
#9218=ORIENTED_EDGE('',*,*,#6812,.T.);
#9219=ORIENTED_EDGE('',*,*,#6616,.T.);
#9220=ORIENTED_EDGE('',*,*,#6861,.T.);
#9221=ORIENTED_EDGE('',*,*,#6683,.T.);
#9222=ORIENTED_EDGE('',*,*,#6858,.F.);
#9223=ORIENTED_EDGE('',*,*,#6259,.T.);
#9224=ORIENTED_EDGE('',*,*,#6859,.F.);
#9225=ORIENTED_EDGE('',*,*,#6757,.T.);
#9226=ORIENTED_EDGE('',*,*,#6860,.T.);
#9227=ORIENTED_EDGE('',*,*,#6262,.T.);
#9228=ORIENTED_EDGE('',*,*,#6395,.T.);
#9229=ORIENTED_EDGE('',*,*,#6862,.F.);
#9230=ORIENTED_EDGE('',*,*,#6538,.T.);
#9231=ORIENTED_EDGE('',*,*,#6611,.T.);
#9232=ORIENTED_EDGE('',*,*,#6863,.T.);
#9233=ORIENTED_EDGE('',*,*,#6678,.T.);
#9234=ORIENTED_EDGE('',*,*,#6796,.T.);
#9235=ORIENTED_EDGE('',*,*,#6750,.T.);
#9236=ORIENTED_EDGE('',*,*,#6864,.T.);
#9237=ORIENTED_EDGE('',*,*,#6396,.T.);
#9238=ORIENTED_EDGE('',*,*,#6260,.T.);
#9239=ORIENTED_EDGE('',*,*,#6865,.F.);
#9240=ORIENTED_EDGE('',*,*,#6752,.T.);
#9241=ORIENTED_EDGE('',*,*,#6797,.T.);
#9242=ORIENTED_EDGE('',*,*,#6680,.T.);
#9243=ORIENTED_EDGE('',*,*,#6866,.F.);
#9244=ORIENTED_EDGE('',*,*,#6612,.T.);
#9245=ORIENTED_EDGE('',*,*,#6536,.T.);
#9246=ORIENTED_EDGE('',*,*,#6814,.T.);
#9247=ORIENTED_EDGE('',*,*,#6613,.T.);
#9248=ORIENTED_EDGE('',*,*,#6866,.T.);
#9249=ORIENTED_EDGE('',*,*,#6679,.T.);
#9250=ORIENTED_EDGE('',*,*,#6863,.F.);
#9251=ORIENTED_EDGE('',*,*,#6263,.T.);
#9252=ORIENTED_EDGE('',*,*,#6864,.F.);
#9253=ORIENTED_EDGE('',*,*,#6753,.T.);
#9254=ORIENTED_EDGE('',*,*,#6865,.T.);
#9255=ORIENTED_EDGE('',*,*,#6266,.T.);
#9256=ORIENTED_EDGE('',*,*,#6389,.T.);
#9257=ORIENTED_EDGE('',*,*,#6867,.F.);
#9258=ORIENTED_EDGE('',*,*,#6530,.T.);
#9259=ORIENTED_EDGE('',*,*,#6608,.T.);
#9260=ORIENTED_EDGE('',*,*,#6868,.T.);
#9261=ORIENTED_EDGE('',*,*,#6674,.T.);
#9262=ORIENTED_EDGE('',*,*,#6794,.T.);
#9263=ORIENTED_EDGE('',*,*,#6746,.T.);
#9264=ORIENTED_EDGE('',*,*,#6869,.T.);
#9265=ORIENTED_EDGE('',*,*,#6390,.T.);
#9266=ORIENTED_EDGE('',*,*,#6264,.T.);
#9267=ORIENTED_EDGE('',*,*,#6870,.F.);
#9268=ORIENTED_EDGE('',*,*,#6748,.T.);
#9269=ORIENTED_EDGE('',*,*,#6795,.T.);
#9270=ORIENTED_EDGE('',*,*,#6676,.T.);
#9271=ORIENTED_EDGE('',*,*,#6871,.F.);
#9272=ORIENTED_EDGE('',*,*,#6609,.T.);
#9273=ORIENTED_EDGE('',*,*,#6528,.T.);
#9274=ORIENTED_EDGE('',*,*,#6816,.T.);
#9275=ORIENTED_EDGE('',*,*,#6610,.T.);
#9276=ORIENTED_EDGE('',*,*,#6871,.T.);
#9277=ORIENTED_EDGE('',*,*,#6675,.T.);
#9278=ORIENTED_EDGE('',*,*,#6868,.F.);
#9279=ORIENTED_EDGE('',*,*,#6267,.T.);
#9280=ORIENTED_EDGE('',*,*,#6869,.F.);
#9281=ORIENTED_EDGE('',*,*,#6749,.T.);
#9282=ORIENTED_EDGE('',*,*,#6870,.T.);
#9283=ORIENTED_EDGE('',*,*,#6270,.T.);
#9284=ORIENTED_EDGE('',*,*,#6383,.T.);
#9285=ORIENTED_EDGE('',*,*,#6872,.F.);
#9286=ORIENTED_EDGE('',*,*,#6522,.T.);
#9287=ORIENTED_EDGE('',*,*,#6605,.T.);
#9288=ORIENTED_EDGE('',*,*,#6873,.T.);
#9289=ORIENTED_EDGE('',*,*,#6670,.T.);
#9290=ORIENTED_EDGE('',*,*,#6792,.T.);
#9291=ORIENTED_EDGE('',*,*,#6742,.T.);
#9292=ORIENTED_EDGE('',*,*,#6874,.T.);
#9293=ORIENTED_EDGE('',*,*,#6384,.T.);
#9294=ORIENTED_EDGE('',*,*,#6268,.T.);
#9295=ORIENTED_EDGE('',*,*,#6875,.F.);
#9296=ORIENTED_EDGE('',*,*,#6744,.T.);
#9297=ORIENTED_EDGE('',*,*,#6793,.T.);
#9298=ORIENTED_EDGE('',*,*,#6672,.T.);
#9299=ORIENTED_EDGE('',*,*,#6876,.F.);
#9300=ORIENTED_EDGE('',*,*,#6606,.T.);
#9301=ORIENTED_EDGE('',*,*,#6520,.T.);
#9302=ORIENTED_EDGE('',*,*,#6818,.T.);
#9303=ORIENTED_EDGE('',*,*,#6607,.T.);
#9304=ORIENTED_EDGE('',*,*,#6876,.T.);
#9305=ORIENTED_EDGE('',*,*,#6671,.T.);
#9306=ORIENTED_EDGE('',*,*,#6873,.F.);
#9307=ORIENTED_EDGE('',*,*,#6271,.T.);
#9308=ORIENTED_EDGE('',*,*,#6874,.F.);
#9309=ORIENTED_EDGE('',*,*,#6745,.T.);
#9310=ORIENTED_EDGE('',*,*,#6875,.T.);
#9311=ORIENTED_EDGE('',*,*,#6274,.T.);
#9312=ORIENTED_EDGE('',*,*,#6377,.T.);
#9313=ORIENTED_EDGE('',*,*,#6877,.F.);
#9314=ORIENTED_EDGE('',*,*,#6514,.T.);
#9315=ORIENTED_EDGE('',*,*,#6602,.T.);
#9316=ORIENTED_EDGE('',*,*,#6878,.T.);
#9317=ORIENTED_EDGE('',*,*,#6666,.T.);
#9318=ORIENTED_EDGE('',*,*,#6790,.T.);
#9319=ORIENTED_EDGE('',*,*,#6738,.T.);
#9320=ORIENTED_EDGE('',*,*,#6879,.T.);
#9321=ORIENTED_EDGE('',*,*,#6378,.T.);
#9322=ORIENTED_EDGE('',*,*,#6272,.T.);
#9323=ORIENTED_EDGE('',*,*,#6880,.F.);
#9324=ORIENTED_EDGE('',*,*,#6740,.T.);
#9325=ORIENTED_EDGE('',*,*,#6791,.T.);
#9326=ORIENTED_EDGE('',*,*,#6668,.T.);
#9327=ORIENTED_EDGE('',*,*,#6881,.F.);
#9328=ORIENTED_EDGE('',*,*,#6603,.T.);
#9329=ORIENTED_EDGE('',*,*,#6512,.T.);
#9330=ORIENTED_EDGE('',*,*,#6820,.T.);
#9331=ORIENTED_EDGE('',*,*,#6604,.T.);
#9332=ORIENTED_EDGE('',*,*,#6881,.T.);
#9333=ORIENTED_EDGE('',*,*,#6667,.T.);
#9334=ORIENTED_EDGE('',*,*,#6878,.F.);
#9335=ORIENTED_EDGE('',*,*,#6275,.T.);
#9336=ORIENTED_EDGE('',*,*,#6879,.F.);
#9337=ORIENTED_EDGE('',*,*,#6741,.T.);
#9338=ORIENTED_EDGE('',*,*,#6880,.T.);
#9339=ORIENTED_EDGE('',*,*,#6278,.T.);
#9340=ORIENTED_EDGE('',*,*,#6371,.T.);
#9341=ORIENTED_EDGE('',*,*,#6882,.F.);
#9342=ORIENTED_EDGE('',*,*,#6506,.T.);
#9343=ORIENTED_EDGE('',*,*,#6599,.T.);
#9344=ORIENTED_EDGE('',*,*,#6883,.T.);
#9345=ORIENTED_EDGE('',*,*,#6662,.T.);
#9346=ORIENTED_EDGE('',*,*,#6788,.T.);
#9347=ORIENTED_EDGE('',*,*,#6734,.T.);
#9348=ORIENTED_EDGE('',*,*,#6884,.T.);
#9349=ORIENTED_EDGE('',*,*,#6372,.T.);
#9350=ORIENTED_EDGE('',*,*,#6276,.T.);
#9351=ORIENTED_EDGE('',*,*,#6885,.F.);
#9352=ORIENTED_EDGE('',*,*,#6736,.T.);
#9353=ORIENTED_EDGE('',*,*,#6789,.T.);
#9354=ORIENTED_EDGE('',*,*,#6664,.T.);
#9355=ORIENTED_EDGE('',*,*,#6886,.F.);
#9356=ORIENTED_EDGE('',*,*,#6600,.T.);
#9357=ORIENTED_EDGE('',*,*,#6504,.T.);
#9358=ORIENTED_EDGE('',*,*,#6822,.T.);
#9359=ORIENTED_EDGE('',*,*,#6601,.T.);
#9360=ORIENTED_EDGE('',*,*,#6886,.T.);
#9361=ORIENTED_EDGE('',*,*,#6663,.T.);
#9362=ORIENTED_EDGE('',*,*,#6883,.F.);
#9363=ORIENTED_EDGE('',*,*,#6279,.T.);
#9364=ORIENTED_EDGE('',*,*,#6884,.F.);
#9365=ORIENTED_EDGE('',*,*,#6737,.T.);
#9366=ORIENTED_EDGE('',*,*,#6885,.T.);
#9367=ORIENTED_EDGE('',*,*,#6282,.T.);
#9368=ORIENTED_EDGE('',*,*,#6365,.T.);
#9369=ORIENTED_EDGE('',*,*,#6887,.F.);
#9370=ORIENTED_EDGE('',*,*,#6498,.T.);
#9371=ORIENTED_EDGE('',*,*,#6596,.T.);
#9372=ORIENTED_EDGE('',*,*,#6888,.T.);
#9373=ORIENTED_EDGE('',*,*,#6658,.T.);
#9374=ORIENTED_EDGE('',*,*,#6786,.T.);
#9375=ORIENTED_EDGE('',*,*,#6730,.T.);
#9376=ORIENTED_EDGE('',*,*,#6889,.T.);
#9377=ORIENTED_EDGE('',*,*,#6366,.T.);
#9378=ORIENTED_EDGE('',*,*,#6280,.T.);
#9379=ORIENTED_EDGE('',*,*,#6890,.F.);
#9380=ORIENTED_EDGE('',*,*,#6732,.T.);
#9381=ORIENTED_EDGE('',*,*,#6787,.T.);
#9382=ORIENTED_EDGE('',*,*,#6660,.T.);
#9383=ORIENTED_EDGE('',*,*,#6891,.F.);
#9384=ORIENTED_EDGE('',*,*,#6597,.T.);
#9385=ORIENTED_EDGE('',*,*,#6496,.T.);
#9386=ORIENTED_EDGE('',*,*,#6824,.T.);
#9387=ORIENTED_EDGE('',*,*,#6598,.T.);
#9388=ORIENTED_EDGE('',*,*,#6891,.T.);
#9389=ORIENTED_EDGE('',*,*,#6659,.T.);
#9390=ORIENTED_EDGE('',*,*,#6888,.F.);
#9391=ORIENTED_EDGE('',*,*,#6283,.T.);
#9392=ORIENTED_EDGE('',*,*,#6889,.F.);
#9393=ORIENTED_EDGE('',*,*,#6733,.T.);
#9394=ORIENTED_EDGE('',*,*,#6890,.T.);
#9395=ORIENTED_EDGE('',*,*,#6286,.T.);
#9396=ORIENTED_EDGE('',*,*,#6359,.T.);
#9397=ORIENTED_EDGE('',*,*,#6892,.F.);
#9398=ORIENTED_EDGE('',*,*,#6490,.T.);
#9399=ORIENTED_EDGE('',*,*,#6593,.T.);
#9400=ORIENTED_EDGE('',*,*,#6893,.T.);
#9401=ORIENTED_EDGE('',*,*,#6654,.T.);
#9402=ORIENTED_EDGE('',*,*,#6784,.T.);
#9403=ORIENTED_EDGE('',*,*,#6726,.T.);
#9404=ORIENTED_EDGE('',*,*,#6894,.T.);
#9405=ORIENTED_EDGE('',*,*,#6360,.T.);
#9406=ORIENTED_EDGE('',*,*,#6284,.T.);
#9407=ORIENTED_EDGE('',*,*,#6895,.F.);
#9408=ORIENTED_EDGE('',*,*,#6728,.T.);
#9409=ORIENTED_EDGE('',*,*,#6785,.T.);
#9410=ORIENTED_EDGE('',*,*,#6656,.T.);
#9411=ORIENTED_EDGE('',*,*,#6896,.F.);
#9412=ORIENTED_EDGE('',*,*,#6594,.T.);
#9413=ORIENTED_EDGE('',*,*,#6488,.T.);
#9414=ORIENTED_EDGE('',*,*,#6826,.T.);
#9415=ORIENTED_EDGE('',*,*,#6595,.T.);
#9416=ORIENTED_EDGE('',*,*,#6896,.T.);
#9417=ORIENTED_EDGE('',*,*,#6655,.T.);
#9418=ORIENTED_EDGE('',*,*,#6893,.F.);
#9419=ORIENTED_EDGE('',*,*,#6287,.T.);
#9420=ORIENTED_EDGE('',*,*,#6894,.F.);
#9421=ORIENTED_EDGE('',*,*,#6729,.T.);
#9422=ORIENTED_EDGE('',*,*,#6895,.T.);
#9423=ORIENTED_EDGE('',*,*,#6290,.T.);
#9424=ORIENTED_EDGE('',*,*,#6353,.T.);
#9425=ORIENTED_EDGE('',*,*,#6897,.F.);
#9426=ORIENTED_EDGE('',*,*,#6482,.T.);
#9427=ORIENTED_EDGE('',*,*,#6590,.T.);
#9428=ORIENTED_EDGE('',*,*,#6898,.T.);
#9429=ORIENTED_EDGE('',*,*,#6650,.T.);
#9430=ORIENTED_EDGE('',*,*,#6782,.T.);
#9431=ORIENTED_EDGE('',*,*,#6722,.T.);
#9432=ORIENTED_EDGE('',*,*,#6899,.T.);
#9433=ORIENTED_EDGE('',*,*,#6354,.T.);
#9434=ORIENTED_EDGE('',*,*,#6288,.T.);
#9435=ORIENTED_EDGE('',*,*,#6900,.F.);
#9436=ORIENTED_EDGE('',*,*,#6724,.T.);
#9437=ORIENTED_EDGE('',*,*,#6783,.T.);
#9438=ORIENTED_EDGE('',*,*,#6652,.T.);
#9439=ORIENTED_EDGE('',*,*,#6901,.F.);
#9440=ORIENTED_EDGE('',*,*,#6591,.T.);
#9441=ORIENTED_EDGE('',*,*,#6480,.T.);
#9442=ORIENTED_EDGE('',*,*,#6828,.T.);
#9443=ORIENTED_EDGE('',*,*,#6592,.T.);
#9444=ORIENTED_EDGE('',*,*,#6901,.T.);
#9445=ORIENTED_EDGE('',*,*,#6651,.T.);
#9446=ORIENTED_EDGE('',*,*,#6898,.F.);
#9447=ORIENTED_EDGE('',*,*,#6291,.T.);
#9448=ORIENTED_EDGE('',*,*,#6899,.F.);
#9449=ORIENTED_EDGE('',*,*,#6725,.T.);
#9450=ORIENTED_EDGE('',*,*,#6900,.T.);
#9451=ORIENTED_EDGE('',*,*,#6294,.T.);
#9452=ORIENTED_EDGE('',*,*,#6347,.T.);
#9453=ORIENTED_EDGE('',*,*,#6902,.F.);
#9454=ORIENTED_EDGE('',*,*,#6474,.T.);
#9455=ORIENTED_EDGE('',*,*,#6587,.T.);
#9456=ORIENTED_EDGE('',*,*,#6903,.T.);
#9457=ORIENTED_EDGE('',*,*,#6646,.T.);
#9458=ORIENTED_EDGE('',*,*,#6780,.T.);
#9459=ORIENTED_EDGE('',*,*,#6718,.T.);
#9460=ORIENTED_EDGE('',*,*,#6904,.T.);
#9461=ORIENTED_EDGE('',*,*,#6348,.T.);
#9462=ORIENTED_EDGE('',*,*,#6292,.T.);
#9463=ORIENTED_EDGE('',*,*,#6905,.F.);
#9464=ORIENTED_EDGE('',*,*,#6720,.T.);
#9465=ORIENTED_EDGE('',*,*,#6781,.T.);
#9466=ORIENTED_EDGE('',*,*,#6648,.T.);
#9467=ORIENTED_EDGE('',*,*,#6906,.F.);
#9468=ORIENTED_EDGE('',*,*,#6588,.T.);
#9469=ORIENTED_EDGE('',*,*,#6472,.T.);
#9470=ORIENTED_EDGE('',*,*,#6830,.T.);
#9471=ORIENTED_EDGE('',*,*,#6589,.T.);
#9472=ORIENTED_EDGE('',*,*,#6906,.T.);
#9473=ORIENTED_EDGE('',*,*,#6647,.T.);
#9474=ORIENTED_EDGE('',*,*,#6903,.F.);
#9475=ORIENTED_EDGE('',*,*,#6295,.T.);
#9476=ORIENTED_EDGE('',*,*,#6904,.F.);
#9477=ORIENTED_EDGE('',*,*,#6721,.T.);
#9478=ORIENTED_EDGE('',*,*,#6905,.T.);
#9479=ORIENTED_EDGE('',*,*,#6298,.T.);
#9480=ORIENTED_EDGE('',*,*,#6341,.T.);
#9481=ORIENTED_EDGE('',*,*,#6907,.F.);
#9482=ORIENTED_EDGE('',*,*,#6466,.T.);
#9483=ORIENTED_EDGE('',*,*,#6584,.T.);
#9484=ORIENTED_EDGE('',*,*,#6908,.T.);
#9485=ORIENTED_EDGE('',*,*,#6642,.T.);
#9486=ORIENTED_EDGE('',*,*,#6778,.T.);
#9487=ORIENTED_EDGE('',*,*,#6714,.T.);
#9488=ORIENTED_EDGE('',*,*,#6909,.T.);
#9489=ORIENTED_EDGE('',*,*,#6342,.T.);
#9490=ORIENTED_EDGE('',*,*,#6296,.T.);
#9491=ORIENTED_EDGE('',*,*,#6910,.F.);
#9492=ORIENTED_EDGE('',*,*,#6716,.T.);
#9493=ORIENTED_EDGE('',*,*,#6779,.T.);
#9494=ORIENTED_EDGE('',*,*,#6644,.T.);
#9495=ORIENTED_EDGE('',*,*,#6911,.F.);
#9496=ORIENTED_EDGE('',*,*,#6585,.T.);
#9497=ORIENTED_EDGE('',*,*,#6464,.T.);
#9498=ORIENTED_EDGE('',*,*,#6832,.T.);
#9499=ORIENTED_EDGE('',*,*,#6586,.T.);
#9500=ORIENTED_EDGE('',*,*,#6911,.T.);
#9501=ORIENTED_EDGE('',*,*,#6643,.T.);
#9502=ORIENTED_EDGE('',*,*,#6908,.F.);
#9503=ORIENTED_EDGE('',*,*,#6299,.T.);
#9504=ORIENTED_EDGE('',*,*,#6909,.F.);
#9505=ORIENTED_EDGE('',*,*,#6717,.T.);
#9506=ORIENTED_EDGE('',*,*,#6910,.T.);
#9507=ORIENTED_EDGE('',*,*,#6302,.T.);
#9508=ORIENTED_EDGE('',*,*,#6335,.T.);
#9509=ORIENTED_EDGE('',*,*,#6912,.F.);
#9510=ORIENTED_EDGE('',*,*,#6458,.T.);
#9511=ORIENTED_EDGE('',*,*,#6581,.T.);
#9512=ORIENTED_EDGE('',*,*,#6913,.T.);
#9513=ORIENTED_EDGE('',*,*,#6638,.T.);
#9514=ORIENTED_EDGE('',*,*,#6776,.T.);
#9515=ORIENTED_EDGE('',*,*,#6710,.T.);
#9516=ORIENTED_EDGE('',*,*,#6914,.T.);
#9517=ORIENTED_EDGE('',*,*,#6336,.T.);
#9518=ORIENTED_EDGE('',*,*,#6300,.T.);
#9519=ORIENTED_EDGE('',*,*,#6915,.F.);
#9520=ORIENTED_EDGE('',*,*,#6712,.T.);
#9521=ORIENTED_EDGE('',*,*,#6777,.T.);
#9522=ORIENTED_EDGE('',*,*,#6640,.T.);
#9523=ORIENTED_EDGE('',*,*,#6916,.F.);
#9524=ORIENTED_EDGE('',*,*,#6582,.T.);
#9525=ORIENTED_EDGE('',*,*,#6456,.T.);
#9526=ORIENTED_EDGE('',*,*,#6834,.T.);
#9527=ORIENTED_EDGE('',*,*,#6583,.T.);
#9528=ORIENTED_EDGE('',*,*,#6916,.T.);
#9529=ORIENTED_EDGE('',*,*,#6639,.T.);
#9530=ORIENTED_EDGE('',*,*,#6913,.F.);
#9531=ORIENTED_EDGE('',*,*,#6303,.T.);
#9532=ORIENTED_EDGE('',*,*,#6914,.F.);
#9533=ORIENTED_EDGE('',*,*,#6713,.T.);
#9534=ORIENTED_EDGE('',*,*,#6915,.T.);
#9535=ORIENTED_EDGE('',*,*,#6306,.T.);
#9536=ORIENTED_EDGE('',*,*,#6329,.T.);
#9537=ORIENTED_EDGE('',*,*,#6917,.F.);
#9538=ORIENTED_EDGE('',*,*,#6450,.T.);
#9539=ORIENTED_EDGE('',*,*,#6578,.T.);
#9540=ORIENTED_EDGE('',*,*,#6918,.T.);
#9541=ORIENTED_EDGE('',*,*,#6634,.T.);
#9542=ORIENTED_EDGE('',*,*,#6774,.T.);
#9543=ORIENTED_EDGE('',*,*,#6706,.T.);
#9544=ORIENTED_EDGE('',*,*,#6919,.T.);
#9545=ORIENTED_EDGE('',*,*,#6330,.T.);
#9546=ORIENTED_EDGE('',*,*,#6304,.T.);
#9547=ORIENTED_EDGE('',*,*,#6920,.F.);
#9548=ORIENTED_EDGE('',*,*,#6708,.T.);
#9549=ORIENTED_EDGE('',*,*,#6775,.T.);
#9550=ORIENTED_EDGE('',*,*,#6636,.T.);
#9551=ORIENTED_EDGE('',*,*,#6921,.F.);
#9552=ORIENTED_EDGE('',*,*,#6579,.T.);
#9553=ORIENTED_EDGE('',*,*,#6448,.T.);
#9554=ORIENTED_EDGE('',*,*,#6836,.T.);
#9555=ORIENTED_EDGE('',*,*,#6580,.T.);
#9556=ORIENTED_EDGE('',*,*,#6921,.T.);
#9557=ORIENTED_EDGE('',*,*,#6635,.T.);
#9558=ORIENTED_EDGE('',*,*,#6918,.F.);
#9559=ORIENTED_EDGE('',*,*,#6307,.T.);
#9560=ORIENTED_EDGE('',*,*,#6919,.F.);
#9561=ORIENTED_EDGE('',*,*,#6709,.T.);
#9562=ORIENTED_EDGE('',*,*,#6920,.T.);
#9563=ORIENTED_EDGE('',*,*,#6310,.T.);
#9564=ORIENTED_EDGE('',*,*,#6323,.T.);
#9565=ORIENTED_EDGE('',*,*,#6922,.F.);
#9566=ORIENTED_EDGE('',*,*,#6442,.T.);
#9567=ORIENTED_EDGE('',*,*,#6575,.T.);
#9568=ORIENTED_EDGE('',*,*,#6923,.T.);
#9569=ORIENTED_EDGE('',*,*,#6630,.T.);
#9570=ORIENTED_EDGE('',*,*,#6772,.T.);
#9571=ORIENTED_EDGE('',*,*,#6702,.T.);
#9572=ORIENTED_EDGE('',*,*,#6924,.T.);
#9573=ORIENTED_EDGE('',*,*,#6324,.T.);
#9574=ORIENTED_EDGE('',*,*,#6308,.T.);
#9575=ORIENTED_EDGE('',*,*,#6925,.F.);
#9576=ORIENTED_EDGE('',*,*,#6704,.T.);
#9577=ORIENTED_EDGE('',*,*,#6773,.T.);
#9578=ORIENTED_EDGE('',*,*,#6632,.T.);
#9579=ORIENTED_EDGE('',*,*,#6926,.F.);
#9580=ORIENTED_EDGE('',*,*,#6576,.T.);
#9581=ORIENTED_EDGE('',*,*,#6440,.T.);
#9582=ORIENTED_EDGE('',*,*,#6838,.T.);
#9583=ORIENTED_EDGE('',*,*,#6577,.T.);
#9584=ORIENTED_EDGE('',*,*,#6926,.T.);
#9585=ORIENTED_EDGE('',*,*,#6631,.T.);
#9586=ORIENTED_EDGE('',*,*,#6923,.F.);
#9587=ORIENTED_EDGE('',*,*,#6311,.T.);
#9588=ORIENTED_EDGE('',*,*,#6924,.F.);
#9589=ORIENTED_EDGE('',*,*,#6705,.T.);
#9590=ORIENTED_EDGE('',*,*,#6925,.T.);
#9591=ORIENTED_EDGE('',*,*,#6314,.T.);
#9592=ORIENTED_EDGE('',*,*,#6419,.T.);
#9593=ORIENTED_EDGE('',*,*,#6927,.F.);
#9594=ORIENTED_EDGE('',*,*,#6434,.T.);
#9595=ORIENTED_EDGE('',*,*,#6572,.T.);
#9596=ORIENTED_EDGE('',*,*,#6928,.T.);
#9597=ORIENTED_EDGE('',*,*,#6626,.T.);
#9598=ORIENTED_EDGE('',*,*,#6770,.T.);
#9599=ORIENTED_EDGE('',*,*,#6698,.T.);
#9600=ORIENTED_EDGE('',*,*,#6929,.T.);
#9601=ORIENTED_EDGE('',*,*,#6420,.T.);
#9602=ORIENTED_EDGE('',*,*,#6312,.T.);
#9603=ORIENTED_EDGE('',*,*,#6930,.F.);
#9604=ORIENTED_EDGE('',*,*,#6700,.T.);
#9605=ORIENTED_EDGE('',*,*,#6771,.T.);
#9606=ORIENTED_EDGE('',*,*,#6628,.T.);
#9607=ORIENTED_EDGE('',*,*,#6931,.F.);
#9608=ORIENTED_EDGE('',*,*,#6573,.T.);
#9609=ORIENTED_EDGE('',*,*,#6432,.T.);
#9610=ORIENTED_EDGE('',*,*,#6840,.T.);
#9611=ORIENTED_EDGE('',*,*,#6574,.T.);
#9612=ORIENTED_EDGE('',*,*,#6931,.T.);
#9613=ORIENTED_EDGE('',*,*,#6627,.T.);
#9614=ORIENTED_EDGE('',*,*,#6928,.F.);
#9615=ORIENTED_EDGE('',*,*,#6315,.T.);
#9616=ORIENTED_EDGE('',*,*,#6929,.F.);
#9617=ORIENTED_EDGE('',*,*,#6701,.T.);
#9618=ORIENTED_EDGE('',*,*,#6930,.T.);
#9619=ORIENTED_EDGE('',*,*,#6422,.T.);
#9620=ORIENTED_EDGE('',*,*,#6807,.F.);
#9621=ORIENTED_EDGE('',*,*,#6566,.T.);
#9622=ORIENTED_EDGE('',*,*,#6932,.F.);
#9623=ORIENTED_EDGE('',*,*,#6933,.F.);
#9624=ORIENTED_EDGE('',*,*,#6177,.F.);
#9625=ORIENTED_EDGE('',*,*,#6424,.T.);
#9626=ORIENTED_EDGE('',*,*,#6934,.F.);
#9627=ORIENTED_EDGE('',*,*,#6571,.T.);
#9628=ORIENTED_EDGE('',*,*,#6842,.T.);
#9629=ORIENTED_EDGE('',*,*,#6423,.T.);
#9630=ORIENTED_EDGE('',*,*,#6247,.F.);
#9631=ORIENTED_EDGE('',*,*,#6935,.F.);
#9632=ORIENTED_EDGE('',*,*,#6936,.T.);
#9633=ORIENTED_EDGE('',*,*,#6564,.T.);
#9634=ORIENTED_EDGE('',*,*,#6934,.T.);
#9635=ORIENTED_EDGE('',*,*,#6933,.T.);
#9636=ORIENTED_EDGE('',*,*,#6937,.T.);
#9637=ORIENTED_EDGE('',*,*,#6938,.T.);
#9638=ORIENTED_EDGE('',*,*,#6178,.F.);
#9639=ORIENTED_EDGE('',*,*,#6935,.T.);
#9640=ORIENTED_EDGE('',*,*,#6246,.F.);
#9641=ORIENTED_EDGE('',*,*,#6939,.T.);
#9642=ORIENTED_EDGE('',*,*,#6940,.T.);
#9643=ORIENTED_EDGE('',*,*,#6411,.T.);
#9644=ORIENTED_EDGE('',*,*,#6243,.F.);
#9645=ORIENTED_EDGE('',*,*,#6941,.F.);
#9646=ORIENTED_EDGE('',*,*,#6942,.T.);
#9647=ORIENTED_EDGE('',*,*,#6556,.T.);
#9648=ORIENTED_EDGE('',*,*,#6943,.T.);
#9649=ORIENTED_EDGE('',*,*,#6410,.T.);
#9650=ORIENTED_EDGE('',*,*,#6809,.F.);
#9651=ORIENTED_EDGE('',*,*,#6558,.T.);
#9652=ORIENTED_EDGE('',*,*,#6944,.F.);
#9653=ORIENTED_EDGE('',*,*,#6939,.F.);
#9654=ORIENTED_EDGE('',*,*,#6245,.F.);
#9655=ORIENTED_EDGE('',*,*,#6412,.T.);
#9656=ORIENTED_EDGE('',*,*,#6943,.F.);
#9657=ORIENTED_EDGE('',*,*,#6563,.T.);
#9658=ORIENTED_EDGE('',*,*,#6847,.T.);
#9659=ORIENTED_EDGE('',*,*,#6404,.T.);
#9660=ORIENTED_EDGE('',*,*,#6811,.F.);
#9661=ORIENTED_EDGE('',*,*,#6550,.T.);
#9662=ORIENTED_EDGE('',*,*,#6945,.F.);
#9663=ORIENTED_EDGE('',*,*,#6946,.F.);
#9664=ORIENTED_EDGE('',*,*,#6241,.F.);
#9665=ORIENTED_EDGE('',*,*,#6405,.T.);
#9666=ORIENTED_EDGE('',*,*,#6239,.F.);
#9667=ORIENTED_EDGE('',*,*,#6947,.F.);
#9668=ORIENTED_EDGE('',*,*,#6948,.T.);
#9669=ORIENTED_EDGE('',*,*,#6548,.T.);
#9670=ORIENTED_EDGE('',*,*,#6949,.T.);
#9671=ORIENTED_EDGE('',*,*,#6406,.T.);
#9672=ORIENTED_EDGE('',*,*,#6949,.F.);
#9673=ORIENTED_EDGE('',*,*,#6555,.T.);
#9674=ORIENTED_EDGE('',*,*,#6852,.T.);
#9675=ORIENTED_EDGE('',*,*,#6565,.T.);
#9676=ORIENTED_EDGE('',*,*,#6936,.F.);
#9677=ORIENTED_EDGE('',*,*,#6940,.F.);
#9678=ORIENTED_EDGE('',*,*,#6944,.T.);
#9679=ORIENTED_EDGE('',*,*,#6557,.T.);
#9680=ORIENTED_EDGE('',*,*,#6942,.F.);
#9681=ORIENTED_EDGE('',*,*,#6950,.F.);
#9682=ORIENTED_EDGE('',*,*,#6945,.T.);
#9683=ORIENTED_EDGE('',*,*,#6549,.T.);
#9684=ORIENTED_EDGE('',*,*,#6948,.F.);
#9685=ORIENTED_EDGE('',*,*,#6951,.F.);
#9686=ORIENTED_EDGE('',*,*,#6952,.T.);
#9687=ORIENTED_EDGE('',*,*,#6541,.T.);
#9688=ORIENTED_EDGE('',*,*,#6953,.F.);
#9689=ORIENTED_EDGE('',*,*,#6954,.F.);
#9690=ORIENTED_EDGE('',*,*,#6955,.T.);
#9691=ORIENTED_EDGE('',*,*,#6533,.T.);
#9692=ORIENTED_EDGE('',*,*,#6956,.F.);
#9693=ORIENTED_EDGE('',*,*,#6957,.F.);
#9694=ORIENTED_EDGE('',*,*,#6958,.T.);
#9695=ORIENTED_EDGE('',*,*,#6525,.T.);
#9696=ORIENTED_EDGE('',*,*,#6959,.F.);
#9697=ORIENTED_EDGE('',*,*,#6960,.F.);
#9698=ORIENTED_EDGE('',*,*,#6961,.T.);
#9699=ORIENTED_EDGE('',*,*,#6517,.T.);
#9700=ORIENTED_EDGE('',*,*,#6962,.F.);
#9701=ORIENTED_EDGE('',*,*,#6963,.F.);
#9702=ORIENTED_EDGE('',*,*,#6964,.T.);
#9703=ORIENTED_EDGE('',*,*,#6509,.T.);
#9704=ORIENTED_EDGE('',*,*,#6965,.F.);
#9705=ORIENTED_EDGE('',*,*,#6966,.F.);
#9706=ORIENTED_EDGE('',*,*,#6967,.T.);
#9707=ORIENTED_EDGE('',*,*,#6501,.T.);
#9708=ORIENTED_EDGE('',*,*,#6968,.F.);
#9709=ORIENTED_EDGE('',*,*,#6969,.F.);
#9710=ORIENTED_EDGE('',*,*,#6970,.T.);
#9711=ORIENTED_EDGE('',*,*,#6493,.T.);
#9712=ORIENTED_EDGE('',*,*,#6971,.F.);
#9713=ORIENTED_EDGE('',*,*,#6972,.F.);
#9714=ORIENTED_EDGE('',*,*,#6973,.T.);
#9715=ORIENTED_EDGE('',*,*,#6485,.T.);
#9716=ORIENTED_EDGE('',*,*,#6974,.F.);
#9717=ORIENTED_EDGE('',*,*,#6975,.F.);
#9718=ORIENTED_EDGE('',*,*,#6976,.T.);
#9719=ORIENTED_EDGE('',*,*,#6477,.T.);
#9720=ORIENTED_EDGE('',*,*,#6977,.F.);
#9721=ORIENTED_EDGE('',*,*,#6978,.F.);
#9722=ORIENTED_EDGE('',*,*,#6979,.T.);
#9723=ORIENTED_EDGE('',*,*,#6469,.T.);
#9724=ORIENTED_EDGE('',*,*,#6980,.F.);
#9725=ORIENTED_EDGE('',*,*,#6981,.F.);
#9726=ORIENTED_EDGE('',*,*,#6982,.T.);
#9727=ORIENTED_EDGE('',*,*,#6461,.T.);
#9728=ORIENTED_EDGE('',*,*,#6983,.F.);
#9729=ORIENTED_EDGE('',*,*,#6984,.F.);
#9730=ORIENTED_EDGE('',*,*,#6985,.T.);
#9731=ORIENTED_EDGE('',*,*,#6453,.T.);
#9732=ORIENTED_EDGE('',*,*,#6986,.F.);
#9733=ORIENTED_EDGE('',*,*,#6987,.F.);
#9734=ORIENTED_EDGE('',*,*,#6988,.T.);
#9735=ORIENTED_EDGE('',*,*,#6445,.T.);
#9736=ORIENTED_EDGE('',*,*,#6989,.F.);
#9737=ORIENTED_EDGE('',*,*,#6990,.F.);
#9738=ORIENTED_EDGE('',*,*,#6991,.T.);
#9739=ORIENTED_EDGE('',*,*,#6437,.T.);
#9740=ORIENTED_EDGE('',*,*,#6992,.F.);
#9741=ORIENTED_EDGE('',*,*,#6993,.F.);
#9742=ORIENTED_EDGE('',*,*,#6994,.T.);
#9743=ORIENTED_EDGE('',*,*,#6429,.T.);
#9744=ORIENTED_EDGE('',*,*,#6995,.F.);
#9745=ORIENTED_EDGE('',*,*,#6937,.F.);
#9746=ORIENTED_EDGE('',*,*,#6932,.T.);
#9747=ORIENTED_EDGE('',*,*,#6175,.T.);
#9748=ORIENTED_EDGE('',*,*,#6174,.T.);
#9749=ORIENTED_EDGE('',*,*,#6161,.T.);
#9750=ORIENTED_EDGE('',*,*,#6172,.T.);
#9751=ORIENTED_EDGE('',*,*,#6105,.T.);
#9752=ORIENTED_EDGE('',*,*,#6947,.T.);
#9753=ORIENTED_EDGE('',*,*,#6238,.F.);
#9754=ORIENTED_EDGE('',*,*,#6996,.T.);
#9755=ORIENTED_EDGE('',*,*,#6951,.T.);
#9756=ORIENTED_EDGE('',*,*,#6398,.T.);
#9757=ORIENTED_EDGE('',*,*,#6813,.F.);
#9758=ORIENTED_EDGE('',*,*,#6542,.T.);
#9759=ORIENTED_EDGE('',*,*,#6952,.F.);
#9760=ORIENTED_EDGE('',*,*,#6996,.F.);
#9761=ORIENTED_EDGE('',*,*,#6237,.F.);
#9762=ORIENTED_EDGE('',*,*,#6400,.T.);
#9763=ORIENTED_EDGE('',*,*,#6997,.F.);
#9764=ORIENTED_EDGE('',*,*,#6547,.T.);
#9765=ORIENTED_EDGE('',*,*,#6857,.T.);
#9766=ORIENTED_EDGE('',*,*,#6399,.T.);
#9767=ORIENTED_EDGE('',*,*,#6235,.F.);
#9768=ORIENTED_EDGE('',*,*,#6998,.F.);
#9769=ORIENTED_EDGE('',*,*,#6953,.T.);
#9770=ORIENTED_EDGE('',*,*,#6540,.T.);
#9771=ORIENTED_EDGE('',*,*,#6997,.T.);
#9772=ORIENTED_EDGE('',*,*,#6941,.T.);
#9773=ORIENTED_EDGE('',*,*,#6242,.F.);
#9774=ORIENTED_EDGE('',*,*,#6946,.T.);
#9775=ORIENTED_EDGE('',*,*,#6950,.T.);
#9776=ORIENTED_EDGE('',*,*,#6998,.T.);
#9777=ORIENTED_EDGE('',*,*,#6234,.F.);
#9778=ORIENTED_EDGE('',*,*,#6999,.T.);
#9779=ORIENTED_EDGE('',*,*,#6954,.T.);
#9780=ORIENTED_EDGE('',*,*,#6393,.T.);
#9781=ORIENTED_EDGE('',*,*,#6231,.F.);
#9782=ORIENTED_EDGE('',*,*,#7000,.F.);
#9783=ORIENTED_EDGE('',*,*,#6956,.T.);
#9784=ORIENTED_EDGE('',*,*,#6532,.T.);
#9785=ORIENTED_EDGE('',*,*,#7001,.T.);
#9786=ORIENTED_EDGE('',*,*,#6392,.T.);
#9787=ORIENTED_EDGE('',*,*,#6815,.F.);
#9788=ORIENTED_EDGE('',*,*,#6534,.T.);
#9789=ORIENTED_EDGE('',*,*,#6955,.F.);
#9790=ORIENTED_EDGE('',*,*,#6999,.F.);
#9791=ORIENTED_EDGE('',*,*,#6233,.F.);
#9792=ORIENTED_EDGE('',*,*,#6394,.T.);
#9793=ORIENTED_EDGE('',*,*,#7001,.F.);
#9794=ORIENTED_EDGE('',*,*,#6539,.T.);
#9795=ORIENTED_EDGE('',*,*,#6862,.T.);
#9796=ORIENTED_EDGE('',*,*,#6386,.T.);
#9797=ORIENTED_EDGE('',*,*,#6817,.F.);
#9798=ORIENTED_EDGE('',*,*,#6526,.T.);
#9799=ORIENTED_EDGE('',*,*,#6958,.F.);
#9800=ORIENTED_EDGE('',*,*,#7002,.F.);
#9801=ORIENTED_EDGE('',*,*,#6229,.F.);
#9802=ORIENTED_EDGE('',*,*,#6387,.T.);
#9803=ORIENTED_EDGE('',*,*,#6227,.F.);
#9804=ORIENTED_EDGE('',*,*,#7003,.F.);
#9805=ORIENTED_EDGE('',*,*,#6959,.T.);
#9806=ORIENTED_EDGE('',*,*,#6524,.T.);
#9807=ORIENTED_EDGE('',*,*,#7004,.T.);
#9808=ORIENTED_EDGE('',*,*,#6388,.T.);
#9809=ORIENTED_EDGE('',*,*,#7004,.F.);
#9810=ORIENTED_EDGE('',*,*,#6531,.T.);
#9811=ORIENTED_EDGE('',*,*,#6867,.T.);
#9812=ORIENTED_EDGE('',*,*,#7003,.T.);
#9813=ORIENTED_EDGE('',*,*,#6226,.F.);
#9814=ORIENTED_EDGE('',*,*,#7005,.T.);
#9815=ORIENTED_EDGE('',*,*,#6960,.T.);
#9816=ORIENTED_EDGE('',*,*,#6380,.T.);
#9817=ORIENTED_EDGE('',*,*,#6819,.F.);
#9818=ORIENTED_EDGE('',*,*,#6518,.T.);
#9819=ORIENTED_EDGE('',*,*,#6961,.F.);
#9820=ORIENTED_EDGE('',*,*,#7005,.F.);
#9821=ORIENTED_EDGE('',*,*,#6225,.F.);
#9822=ORIENTED_EDGE('',*,*,#6382,.T.);
#9823=ORIENTED_EDGE('',*,*,#7006,.F.);
#9824=ORIENTED_EDGE('',*,*,#6523,.T.);
#9825=ORIENTED_EDGE('',*,*,#6872,.T.);
#9826=ORIENTED_EDGE('',*,*,#6381,.T.);
#9827=ORIENTED_EDGE('',*,*,#6223,.F.);
#9828=ORIENTED_EDGE('',*,*,#7007,.F.);
#9829=ORIENTED_EDGE('',*,*,#6962,.T.);
#9830=ORIENTED_EDGE('',*,*,#6516,.T.);
#9831=ORIENTED_EDGE('',*,*,#7006,.T.);
#9832=ORIENTED_EDGE('',*,*,#7000,.T.);
#9833=ORIENTED_EDGE('',*,*,#6230,.F.);
#9834=ORIENTED_EDGE('',*,*,#7002,.T.);
#9835=ORIENTED_EDGE('',*,*,#6957,.T.);
#9836=ORIENTED_EDGE('',*,*,#7007,.T.);
#9837=ORIENTED_EDGE('',*,*,#6222,.F.);
#9838=ORIENTED_EDGE('',*,*,#7008,.T.);
#9839=ORIENTED_EDGE('',*,*,#6963,.T.);
#9840=ORIENTED_EDGE('',*,*,#6375,.T.);
#9841=ORIENTED_EDGE('',*,*,#6219,.F.);
#9842=ORIENTED_EDGE('',*,*,#7009,.F.);
#9843=ORIENTED_EDGE('',*,*,#6965,.T.);
#9844=ORIENTED_EDGE('',*,*,#6508,.T.);
#9845=ORIENTED_EDGE('',*,*,#7010,.T.);
#9846=ORIENTED_EDGE('',*,*,#6374,.T.);
#9847=ORIENTED_EDGE('',*,*,#6821,.F.);
#9848=ORIENTED_EDGE('',*,*,#6510,.T.);
#9849=ORIENTED_EDGE('',*,*,#6964,.F.);
#9850=ORIENTED_EDGE('',*,*,#7008,.F.);
#9851=ORIENTED_EDGE('',*,*,#6221,.F.);
#9852=ORIENTED_EDGE('',*,*,#6376,.T.);
#9853=ORIENTED_EDGE('',*,*,#7010,.F.);
#9854=ORIENTED_EDGE('',*,*,#6515,.T.);
#9855=ORIENTED_EDGE('',*,*,#6877,.T.);
#9856=ORIENTED_EDGE('',*,*,#6368,.T.);
#9857=ORIENTED_EDGE('',*,*,#6823,.F.);
#9858=ORIENTED_EDGE('',*,*,#6502,.T.);
#9859=ORIENTED_EDGE('',*,*,#6967,.F.);
#9860=ORIENTED_EDGE('',*,*,#7011,.F.);
#9861=ORIENTED_EDGE('',*,*,#6217,.F.);
#9862=ORIENTED_EDGE('',*,*,#6369,.T.);
#9863=ORIENTED_EDGE('',*,*,#6215,.F.);
#9864=ORIENTED_EDGE('',*,*,#7012,.F.);
#9865=ORIENTED_EDGE('',*,*,#6968,.T.);
#9866=ORIENTED_EDGE('',*,*,#6500,.T.);
#9867=ORIENTED_EDGE('',*,*,#7013,.T.);
#9868=ORIENTED_EDGE('',*,*,#6370,.T.);
#9869=ORIENTED_EDGE('',*,*,#7013,.F.);
#9870=ORIENTED_EDGE('',*,*,#6507,.T.);
#9871=ORIENTED_EDGE('',*,*,#6882,.T.);
#9872=ORIENTED_EDGE('',*,*,#7012,.T.);
#9873=ORIENTED_EDGE('',*,*,#6214,.F.);
#9874=ORIENTED_EDGE('',*,*,#7014,.T.);
#9875=ORIENTED_EDGE('',*,*,#6969,.T.);
#9876=ORIENTED_EDGE('',*,*,#6362,.T.);
#9877=ORIENTED_EDGE('',*,*,#6825,.F.);
#9878=ORIENTED_EDGE('',*,*,#6494,.T.);
#9879=ORIENTED_EDGE('',*,*,#6970,.F.);
#9880=ORIENTED_EDGE('',*,*,#7014,.F.);
#9881=ORIENTED_EDGE('',*,*,#6213,.F.);
#9882=ORIENTED_EDGE('',*,*,#6364,.T.);
#9883=ORIENTED_EDGE('',*,*,#7015,.F.);
#9884=ORIENTED_EDGE('',*,*,#6499,.T.);
#9885=ORIENTED_EDGE('',*,*,#6887,.T.);
#9886=ORIENTED_EDGE('',*,*,#6363,.T.);
#9887=ORIENTED_EDGE('',*,*,#6211,.F.);
#9888=ORIENTED_EDGE('',*,*,#7016,.F.);
#9889=ORIENTED_EDGE('',*,*,#6971,.T.);
#9890=ORIENTED_EDGE('',*,*,#6492,.T.);
#9891=ORIENTED_EDGE('',*,*,#7015,.T.);
#9892=ORIENTED_EDGE('',*,*,#7009,.T.);
#9893=ORIENTED_EDGE('',*,*,#6218,.F.);
#9894=ORIENTED_EDGE('',*,*,#7011,.T.);
#9895=ORIENTED_EDGE('',*,*,#6966,.T.);
#9896=ORIENTED_EDGE('',*,*,#7016,.T.);
#9897=ORIENTED_EDGE('',*,*,#6210,.F.);
#9898=ORIENTED_EDGE('',*,*,#7017,.T.);
#9899=ORIENTED_EDGE('',*,*,#6972,.T.);
#9900=ORIENTED_EDGE('',*,*,#6357,.T.);
#9901=ORIENTED_EDGE('',*,*,#6207,.F.);
#9902=ORIENTED_EDGE('',*,*,#7018,.F.);
#9903=ORIENTED_EDGE('',*,*,#6974,.T.);
#9904=ORIENTED_EDGE('',*,*,#6484,.T.);
#9905=ORIENTED_EDGE('',*,*,#7019,.T.);
#9906=ORIENTED_EDGE('',*,*,#6356,.T.);
#9907=ORIENTED_EDGE('',*,*,#6827,.F.);
#9908=ORIENTED_EDGE('',*,*,#6486,.T.);
#9909=ORIENTED_EDGE('',*,*,#6973,.F.);
#9910=ORIENTED_EDGE('',*,*,#7017,.F.);
#9911=ORIENTED_EDGE('',*,*,#6209,.F.);
#9912=ORIENTED_EDGE('',*,*,#6358,.T.);
#9913=ORIENTED_EDGE('',*,*,#7019,.F.);
#9914=ORIENTED_EDGE('',*,*,#6491,.T.);
#9915=ORIENTED_EDGE('',*,*,#6892,.T.);
#9916=ORIENTED_EDGE('',*,*,#6350,.T.);
#9917=ORIENTED_EDGE('',*,*,#6829,.F.);
#9918=ORIENTED_EDGE('',*,*,#6478,.T.);
#9919=ORIENTED_EDGE('',*,*,#6976,.F.);
#9920=ORIENTED_EDGE('',*,*,#7020,.F.);
#9921=ORIENTED_EDGE('',*,*,#6205,.F.);
#9922=ORIENTED_EDGE('',*,*,#6351,.T.);
#9923=ORIENTED_EDGE('',*,*,#6203,.F.);
#9924=ORIENTED_EDGE('',*,*,#7021,.F.);
#9925=ORIENTED_EDGE('',*,*,#6977,.T.);
#9926=ORIENTED_EDGE('',*,*,#6476,.T.);
#9927=ORIENTED_EDGE('',*,*,#7022,.T.);
#9928=ORIENTED_EDGE('',*,*,#6352,.T.);
#9929=ORIENTED_EDGE('',*,*,#7022,.F.);
#9930=ORIENTED_EDGE('',*,*,#6483,.T.);
#9931=ORIENTED_EDGE('',*,*,#6897,.T.);
#9932=ORIENTED_EDGE('',*,*,#7021,.T.);
#9933=ORIENTED_EDGE('',*,*,#6202,.F.);
#9934=ORIENTED_EDGE('',*,*,#7023,.T.);
#9935=ORIENTED_EDGE('',*,*,#6978,.T.);
#9936=ORIENTED_EDGE('',*,*,#6344,.T.);
#9937=ORIENTED_EDGE('',*,*,#6831,.F.);
#9938=ORIENTED_EDGE('',*,*,#6470,.T.);
#9939=ORIENTED_EDGE('',*,*,#6979,.F.);
#9940=ORIENTED_EDGE('',*,*,#7023,.F.);
#9941=ORIENTED_EDGE('',*,*,#6201,.F.);
#9942=ORIENTED_EDGE('',*,*,#6346,.T.);
#9943=ORIENTED_EDGE('',*,*,#7024,.F.);
#9944=ORIENTED_EDGE('',*,*,#6475,.T.);
#9945=ORIENTED_EDGE('',*,*,#6902,.T.);
#9946=ORIENTED_EDGE('',*,*,#6345,.T.);
#9947=ORIENTED_EDGE('',*,*,#6199,.F.);
#9948=ORIENTED_EDGE('',*,*,#7025,.F.);
#9949=ORIENTED_EDGE('',*,*,#6980,.T.);
#9950=ORIENTED_EDGE('',*,*,#6468,.T.);
#9951=ORIENTED_EDGE('',*,*,#7024,.T.);
#9952=ORIENTED_EDGE('',*,*,#7018,.T.);
#9953=ORIENTED_EDGE('',*,*,#6206,.F.);
#9954=ORIENTED_EDGE('',*,*,#7020,.T.);
#9955=ORIENTED_EDGE('',*,*,#6975,.T.);
#9956=ORIENTED_EDGE('',*,*,#7025,.T.);
#9957=ORIENTED_EDGE('',*,*,#6198,.F.);
#9958=ORIENTED_EDGE('',*,*,#7026,.T.);
#9959=ORIENTED_EDGE('',*,*,#6981,.T.);
#9960=ORIENTED_EDGE('',*,*,#6339,.T.);
#9961=ORIENTED_EDGE('',*,*,#6195,.F.);
#9962=ORIENTED_EDGE('',*,*,#7027,.F.);
#9963=ORIENTED_EDGE('',*,*,#6983,.T.);
#9964=ORIENTED_EDGE('',*,*,#6460,.T.);
#9965=ORIENTED_EDGE('',*,*,#7028,.T.);
#9966=ORIENTED_EDGE('',*,*,#6338,.T.);
#9967=ORIENTED_EDGE('',*,*,#6833,.F.);
#9968=ORIENTED_EDGE('',*,*,#6462,.T.);
#9969=ORIENTED_EDGE('',*,*,#6982,.F.);
#9970=ORIENTED_EDGE('',*,*,#7026,.F.);
#9971=ORIENTED_EDGE('',*,*,#6197,.F.);
#9972=ORIENTED_EDGE('',*,*,#6340,.T.);
#9973=ORIENTED_EDGE('',*,*,#7028,.F.);
#9974=ORIENTED_EDGE('',*,*,#6467,.T.);
#9975=ORIENTED_EDGE('',*,*,#6907,.T.);
#9976=ORIENTED_EDGE('',*,*,#6332,.T.);
#9977=ORIENTED_EDGE('',*,*,#6835,.F.);
#9978=ORIENTED_EDGE('',*,*,#6454,.T.);
#9979=ORIENTED_EDGE('',*,*,#6985,.F.);
#9980=ORIENTED_EDGE('',*,*,#7029,.F.);
#9981=ORIENTED_EDGE('',*,*,#6193,.F.);
#9982=ORIENTED_EDGE('',*,*,#6333,.T.);
#9983=ORIENTED_EDGE('',*,*,#6191,.F.);
#9984=ORIENTED_EDGE('',*,*,#7030,.F.);
#9985=ORIENTED_EDGE('',*,*,#6986,.T.);
#9986=ORIENTED_EDGE('',*,*,#6452,.T.);
#9987=ORIENTED_EDGE('',*,*,#7031,.T.);
#9988=ORIENTED_EDGE('',*,*,#6334,.T.);
#9989=ORIENTED_EDGE('',*,*,#7031,.F.);
#9990=ORIENTED_EDGE('',*,*,#6459,.T.);
#9991=ORIENTED_EDGE('',*,*,#6912,.T.);
#9992=ORIENTED_EDGE('',*,*,#7030,.T.);
#9993=ORIENTED_EDGE('',*,*,#6190,.F.);
#9994=ORIENTED_EDGE('',*,*,#7032,.T.);
#9995=ORIENTED_EDGE('',*,*,#6987,.T.);
#9996=ORIENTED_EDGE('',*,*,#6326,.T.);
#9997=ORIENTED_EDGE('',*,*,#6837,.F.);
#9998=ORIENTED_EDGE('',*,*,#6446,.T.);
#9999=ORIENTED_EDGE('',*,*,#6988,.F.);
#10000=ORIENTED_EDGE('',*,*,#7032,.F.);
#10001=ORIENTED_EDGE('',*,*,#6189,.F.);
#10002=ORIENTED_EDGE('',*,*,#6328,.T.);
#10003=ORIENTED_EDGE('',*,*,#7033,.F.);
#10004=ORIENTED_EDGE('',*,*,#6451,.T.);
#10005=ORIENTED_EDGE('',*,*,#6917,.T.);
#10006=ORIENTED_EDGE('',*,*,#6327,.T.);
#10007=ORIENTED_EDGE('',*,*,#6187,.F.);
#10008=ORIENTED_EDGE('',*,*,#7034,.F.);
#10009=ORIENTED_EDGE('',*,*,#6989,.T.);
#10010=ORIENTED_EDGE('',*,*,#6444,.T.);
#10011=ORIENTED_EDGE('',*,*,#7033,.T.);
#10012=ORIENTED_EDGE('',*,*,#7027,.T.);
#10013=ORIENTED_EDGE('',*,*,#6194,.F.);
#10014=ORIENTED_EDGE('',*,*,#7029,.T.);
#10015=ORIENTED_EDGE('',*,*,#6984,.T.);
#10016=ORIENTED_EDGE('',*,*,#7034,.T.);
#10017=ORIENTED_EDGE('',*,*,#6186,.F.);
#10018=ORIENTED_EDGE('',*,*,#7035,.T.);
#10019=ORIENTED_EDGE('',*,*,#6990,.T.);
#10020=ORIENTED_EDGE('',*,*,#6321,.T.);
#10021=ORIENTED_EDGE('',*,*,#6183,.F.);
#10022=ORIENTED_EDGE('',*,*,#7036,.F.);
#10023=ORIENTED_EDGE('',*,*,#6992,.T.);
#10024=ORIENTED_EDGE('',*,*,#6436,.T.);
#10025=ORIENTED_EDGE('',*,*,#7037,.T.);
#10026=ORIENTED_EDGE('',*,*,#6320,.T.);
#10027=ORIENTED_EDGE('',*,*,#6839,.F.);
#10028=ORIENTED_EDGE('',*,*,#6438,.T.);
#10029=ORIENTED_EDGE('',*,*,#6991,.F.);
#10030=ORIENTED_EDGE('',*,*,#7035,.F.);
#10031=ORIENTED_EDGE('',*,*,#6185,.F.);
#10032=ORIENTED_EDGE('',*,*,#6322,.T.);
#10033=ORIENTED_EDGE('',*,*,#7037,.F.);
#10034=ORIENTED_EDGE('',*,*,#6443,.T.);
#10035=ORIENTED_EDGE('',*,*,#6922,.T.);
#10036=ORIENTED_EDGE('',*,*,#6416,.T.);
#10037=ORIENTED_EDGE('',*,*,#6841,.F.);
#10038=ORIENTED_EDGE('',*,*,#6430,.T.);
#10039=ORIENTED_EDGE('',*,*,#6994,.F.);
#10040=ORIENTED_EDGE('',*,*,#7038,.F.);
#10041=ORIENTED_EDGE('',*,*,#6181,.F.);
#10042=ORIENTED_EDGE('',*,*,#6417,.T.);
#10043=ORIENTED_EDGE('',*,*,#6179,.F.);
#10044=ORIENTED_EDGE('',*,*,#6938,.F.);
#10045=ORIENTED_EDGE('',*,*,#6995,.T.);
#10046=ORIENTED_EDGE('',*,*,#6428,.T.);
#10047=ORIENTED_EDGE('',*,*,#7039,.T.);
#10048=ORIENTED_EDGE('',*,*,#6418,.T.);
#10049=ORIENTED_EDGE('',*,*,#7039,.F.);
#10050=ORIENTED_EDGE('',*,*,#6435,.T.);
#10051=ORIENTED_EDGE('',*,*,#6927,.T.);
#10052=ORIENTED_EDGE('',*,*,#7036,.T.);
#10053=ORIENTED_EDGE('',*,*,#6182,.F.);
#10054=ORIENTED_EDGE('',*,*,#7038,.T.);
#10055=ORIENTED_EDGE('',*,*,#6993,.T.);
#10056=ORIENTED_EDGE('',*,*,#7040,.F.);
#10057=ORIENTED_EDGE('',*,*,#7041,.T.);
#10058=ORIENTED_EDGE('',*,*,#7042,.F.);
#10059=ORIENTED_EDGE('',*,*,#7041,.F.);
#10060=ORIENTED_EDGE('',*,*,#7043,.F.);
#10061=ORIENTED_EDGE('',*,*,#7044,.T.);
#10062=ORIENTED_EDGE('',*,*,#7045,.F.);
#10063=ORIENTED_EDGE('',*,*,#7044,.F.);
#10064=ORIENTED_EDGE('',*,*,#7046,.F.);
#10065=ORIENTED_EDGE('',*,*,#7047,.T.);
#10066=ORIENTED_EDGE('',*,*,#7048,.F.);
#10067=ORIENTED_EDGE('',*,*,#7047,.F.);
#10068=ORIENTED_EDGE('',*,*,#7049,.T.);
#10069=ORIENTED_EDGE('',*,*,#7050,.T.);
#10070=ORIENTED_EDGE('',*,*,#7051,.T.);
#10071=ORIENTED_EDGE('',*,*,#7052,.T.);
#10072=ORIENTED_EDGE('',*,*,#7050,.F.);
#10073=ORIENTED_EDGE('',*,*,#7052,.F.);
#10074=ORIENTED_EDGE('',*,*,#7053,.T.);
#10075=ORIENTED_EDGE('',*,*,#7054,.T.);
#10076=ORIENTED_EDGE('',*,*,#7053,.F.);
#10077=ORIENTED_EDGE('',*,*,#7051,.F.);
#10078=ORIENTED_EDGE('',*,*,#7049,.F.);
#10079=ORIENTED_EDGE('',*,*,#7040,.T.);
#10080=ORIENTED_EDGE('',*,*,#7043,.T.);
#10081=ORIENTED_EDGE('',*,*,#7046,.T.);
#10082=ORIENTED_EDGE('',*,*,#7055,.T.);
#10083=ORIENTED_EDGE('',*,*,#7056,.T.);
#10084=ORIENTED_EDGE('',*,*,#7057,.T.);
#10085=ORIENTED_EDGE('',*,*,#7055,.F.);
#10086=ORIENTED_EDGE('',*,*,#7057,.F.);
#10087=ORIENTED_EDGE('',*,*,#7054,.F.);
#10088=ORIENTED_EDGE('',*,*,#7042,.T.);
#10089=ORIENTED_EDGE('',*,*,#7045,.T.);
#10090=ORIENTED_EDGE('',*,*,#7048,.T.);
#10091=ORIENTED_EDGE('',*,*,#7056,.F.);
#10092=ORIENTED_EDGE('',*,*,#7058,.F.);
#10093=ORIENTED_EDGE('',*,*,#7059,.F.);
#10094=ORIENTED_EDGE('',*,*,#7060,.F.);
#10095=ORIENTED_EDGE('',*,*,#7061,.T.);
#10096=ORIENTED_EDGE('',*,*,#7062,.F.);
#10097=ORIENTED_EDGE('',*,*,#7063,.F.);
#10098=ORIENTED_EDGE('',*,*,#7064,.F.);
#10099=ORIENTED_EDGE('',*,*,#7058,.T.);
#10100=ORIENTED_EDGE('',*,*,#7065,.T.);
#10101=ORIENTED_EDGE('',*,*,#7066,.T.);
#10102=ORIENTED_EDGE('',*,*,#7067,.F.);
#10103=ORIENTED_EDGE('',*,*,#7068,.F.);
#10104=ORIENTED_EDGE('',*,*,#7069,.F.);
#10105=ORIENTED_EDGE('',*,*,#7062,.T.);
#10106=ORIENTED_EDGE('',*,*,#7070,.T.);
#10107=ORIENTED_EDGE('',*,*,#7071,.T.);
#10108=ORIENTED_EDGE('',*,*,#7072,.F.);
#10109=ORIENTED_EDGE('',*,*,#7073,.F.);
#10110=ORIENTED_EDGE('',*,*,#7074,.F.);
#10111=ORIENTED_EDGE('',*,*,#7067,.T.);
#10112=ORIENTED_EDGE('',*,*,#7075,.T.);
#10113=ORIENTED_EDGE('',*,*,#7076,.T.);
#10114=ORIENTED_EDGE('',*,*,#7077,.F.);
#10115=ORIENTED_EDGE('',*,*,#7078,.F.);
#10116=ORIENTED_EDGE('',*,*,#7079,.F.);
#10117=ORIENTED_EDGE('',*,*,#7072,.T.);
#10118=ORIENTED_EDGE('',*,*,#7080,.T.);
#10119=ORIENTED_EDGE('',*,*,#7081,.T.);
#10120=ORIENTED_EDGE('',*,*,#7082,.F.);
#10121=ORIENTED_EDGE('',*,*,#7083,.F.);
#10122=ORIENTED_EDGE('',*,*,#7084,.F.);
#10123=ORIENTED_EDGE('',*,*,#7077,.T.);
#10124=ORIENTED_EDGE('',*,*,#7085,.T.);
#10125=ORIENTED_EDGE('',*,*,#7086,.T.);
#10126=ORIENTED_EDGE('',*,*,#7087,.F.);
#10127=ORIENTED_EDGE('',*,*,#7088,.F.);
#10128=ORIENTED_EDGE('',*,*,#7089,.F.);
#10129=ORIENTED_EDGE('',*,*,#7082,.T.);
#10130=ORIENTED_EDGE('',*,*,#7090,.T.);
#10131=ORIENTED_EDGE('',*,*,#7091,.T.);
#10132=ORIENTED_EDGE('',*,*,#7092,.F.);
#10133=ORIENTED_EDGE('',*,*,#7093,.F.);
#10134=ORIENTED_EDGE('',*,*,#7094,.F.);
#10135=ORIENTED_EDGE('',*,*,#7087,.T.);
#10136=ORIENTED_EDGE('',*,*,#7095,.T.);
#10137=ORIENTED_EDGE('',*,*,#7096,.T.);
#10138=ORIENTED_EDGE('',*,*,#7097,.F.);
#10139=ORIENTED_EDGE('',*,*,#7098,.F.);
#10140=ORIENTED_EDGE('',*,*,#7099,.F.);
#10141=ORIENTED_EDGE('',*,*,#7092,.T.);
#10142=ORIENTED_EDGE('',*,*,#7100,.T.);
#10143=ORIENTED_EDGE('',*,*,#7101,.T.);
#10144=ORIENTED_EDGE('',*,*,#7102,.F.);
#10145=ORIENTED_EDGE('',*,*,#7103,.F.);
#10146=ORIENTED_EDGE('',*,*,#7104,.F.);
#10147=ORIENTED_EDGE('',*,*,#7097,.T.);
#10148=ORIENTED_EDGE('',*,*,#7105,.T.);
#10149=ORIENTED_EDGE('',*,*,#7106,.T.);
#10150=ORIENTED_EDGE('',*,*,#7107,.F.);
#10151=ORIENTED_EDGE('',*,*,#7108,.F.);
#10152=ORIENTED_EDGE('',*,*,#7109,.F.);
#10153=ORIENTED_EDGE('',*,*,#7102,.T.);
#10154=ORIENTED_EDGE('',*,*,#7110,.T.);
#10155=ORIENTED_EDGE('',*,*,#7111,.T.);
#10156=ORIENTED_EDGE('',*,*,#7112,.F.);
#10157=ORIENTED_EDGE('',*,*,#7113,.F.);
#10158=ORIENTED_EDGE('',*,*,#7114,.F.);
#10159=ORIENTED_EDGE('',*,*,#7107,.T.);
#10160=ORIENTED_EDGE('',*,*,#7115,.T.);
#10161=ORIENTED_EDGE('',*,*,#7116,.T.);
#10162=ORIENTED_EDGE('',*,*,#7117,.F.);
#10163=ORIENTED_EDGE('',*,*,#7118,.F.);
#10164=ORIENTED_EDGE('',*,*,#7119,.F.);
#10165=ORIENTED_EDGE('',*,*,#7112,.T.);
#10166=ORIENTED_EDGE('',*,*,#7120,.T.);
#10167=ORIENTED_EDGE('',*,*,#7121,.T.);
#10168=ORIENTED_EDGE('',*,*,#7122,.F.);
#10169=ORIENTED_EDGE('',*,*,#7123,.F.);
#10170=ORIENTED_EDGE('',*,*,#7124,.F.);
#10171=ORIENTED_EDGE('',*,*,#7117,.T.);
#10172=ORIENTED_EDGE('',*,*,#7125,.T.);
#10173=ORIENTED_EDGE('',*,*,#7126,.T.);
#10174=ORIENTED_EDGE('',*,*,#7127,.F.);
#10175=ORIENTED_EDGE('',*,*,#7128,.F.);
#10176=ORIENTED_EDGE('',*,*,#7129,.F.);
#10177=ORIENTED_EDGE('',*,*,#7122,.T.);
#10178=ORIENTED_EDGE('',*,*,#7130,.T.);
#10179=ORIENTED_EDGE('',*,*,#7131,.T.);
#10180=ORIENTED_EDGE('',*,*,#7132,.F.);
#10181=ORIENTED_EDGE('',*,*,#7133,.F.);
#10182=ORIENTED_EDGE('',*,*,#7134,.F.);
#10183=ORIENTED_EDGE('',*,*,#7127,.T.);
#10184=ORIENTED_EDGE('',*,*,#7135,.T.);
#10185=ORIENTED_EDGE('',*,*,#7136,.T.);
#10186=ORIENTED_EDGE('',*,*,#7137,.F.);
#10187=ORIENTED_EDGE('',*,*,#7138,.F.);
#10188=ORIENTED_EDGE('',*,*,#7139,.F.);
#10189=ORIENTED_EDGE('',*,*,#7132,.T.);
#10190=ORIENTED_EDGE('',*,*,#7140,.T.);
#10191=ORIENTED_EDGE('',*,*,#7141,.T.);
#10192=ORIENTED_EDGE('',*,*,#7142,.F.);
#10193=ORIENTED_EDGE('',*,*,#7143,.F.);
#10194=ORIENTED_EDGE('',*,*,#7144,.F.);
#10195=ORIENTED_EDGE('',*,*,#7137,.T.);
#10196=ORIENTED_EDGE('',*,*,#7145,.T.);
#10197=ORIENTED_EDGE('',*,*,#7146,.T.);
#10198=ORIENTED_EDGE('',*,*,#7147,.F.);
#10199=ORIENTED_EDGE('',*,*,#7148,.F.);
#10200=ORIENTED_EDGE('',*,*,#7149,.F.);
#10201=ORIENTED_EDGE('',*,*,#7142,.T.);
#10202=ORIENTED_EDGE('',*,*,#7150,.T.);
#10203=ORIENTED_EDGE('',*,*,#7151,.T.);
#10204=ORIENTED_EDGE('',*,*,#7152,.F.);
#10205=ORIENTED_EDGE('',*,*,#7153,.F.);
#10206=ORIENTED_EDGE('',*,*,#7154,.F.);
#10207=ORIENTED_EDGE('',*,*,#7147,.T.);
#10208=ORIENTED_EDGE('',*,*,#7155,.T.);
#10209=ORIENTED_EDGE('',*,*,#7156,.T.);
#10210=ORIENTED_EDGE('',*,*,#7157,.F.);
#10211=ORIENTED_EDGE('',*,*,#7158,.F.);
#10212=ORIENTED_EDGE('',*,*,#7159,.F.);
#10213=ORIENTED_EDGE('',*,*,#7152,.T.);
#10214=ORIENTED_EDGE('',*,*,#7160,.T.);
#10215=ORIENTED_EDGE('',*,*,#7161,.T.);
#10216=ORIENTED_EDGE('',*,*,#7162,.F.);
#10217=ORIENTED_EDGE('',*,*,#7163,.F.);
#10218=ORIENTED_EDGE('',*,*,#7164,.F.);
#10219=ORIENTED_EDGE('',*,*,#7157,.T.);
#10220=ORIENTED_EDGE('',*,*,#7165,.T.);
#10221=ORIENTED_EDGE('',*,*,#7166,.T.);
#10222=ORIENTED_EDGE('',*,*,#7167,.F.);
#10223=ORIENTED_EDGE('',*,*,#7168,.F.);
#10224=ORIENTED_EDGE('',*,*,#7169,.F.);
#10225=ORIENTED_EDGE('',*,*,#7162,.T.);
#10226=ORIENTED_EDGE('',*,*,#7170,.T.);
#10227=ORIENTED_EDGE('',*,*,#7171,.T.);
#10228=ORIENTED_EDGE('',*,*,#7172,.F.);
#10229=ORIENTED_EDGE('',*,*,#7173,.F.);
#10230=ORIENTED_EDGE('',*,*,#7174,.F.);
#10231=ORIENTED_EDGE('',*,*,#7167,.T.);
#10232=ORIENTED_EDGE('',*,*,#7175,.T.);
#10233=ORIENTED_EDGE('',*,*,#7176,.T.);
#10234=ORIENTED_EDGE('',*,*,#7177,.F.);
#10235=ORIENTED_EDGE('',*,*,#7178,.F.);
#10236=ORIENTED_EDGE('',*,*,#7179,.F.);
#10237=ORIENTED_EDGE('',*,*,#7172,.T.);
#10238=ORIENTED_EDGE('',*,*,#7180,.T.);
#10239=ORIENTED_EDGE('',*,*,#7181,.T.);
#10240=ORIENTED_EDGE('',*,*,#7182,.F.);
#10241=ORIENTED_EDGE('',*,*,#7183,.F.);
#10242=ORIENTED_EDGE('',*,*,#7184,.F.);
#10243=ORIENTED_EDGE('',*,*,#7177,.T.);
#10244=ORIENTED_EDGE('',*,*,#7185,.T.);
#10245=ORIENTED_EDGE('',*,*,#7186,.T.);
#10246=ORIENTED_EDGE('',*,*,#7187,.F.);
#10247=ORIENTED_EDGE('',*,*,#7188,.F.);
#10248=ORIENTED_EDGE('',*,*,#7189,.F.);
#10249=ORIENTED_EDGE('',*,*,#7182,.T.);
#10250=ORIENTED_EDGE('',*,*,#7190,.T.);
#10251=ORIENTED_EDGE('',*,*,#7191,.T.);
#10252=ORIENTED_EDGE('',*,*,#7192,.F.);
#10253=ORIENTED_EDGE('',*,*,#7193,.F.);
#10254=ORIENTED_EDGE('',*,*,#7194,.F.);
#10255=ORIENTED_EDGE('',*,*,#7187,.T.);
#10256=ORIENTED_EDGE('',*,*,#7195,.T.);
#10257=ORIENTED_EDGE('',*,*,#7196,.T.);
#10258=ORIENTED_EDGE('',*,*,#7197,.F.);
#10259=ORIENTED_EDGE('',*,*,#7198,.F.);
#10260=ORIENTED_EDGE('',*,*,#7199,.F.);
#10261=ORIENTED_EDGE('',*,*,#7192,.T.);
#10262=ORIENTED_EDGE('',*,*,#7200,.T.);
#10263=ORIENTED_EDGE('',*,*,#7201,.T.);
#10264=ORIENTED_EDGE('',*,*,#7202,.F.);
#10265=ORIENTED_EDGE('',*,*,#7203,.F.);
#10266=ORIENTED_EDGE('',*,*,#7204,.F.);
#10267=ORIENTED_EDGE('',*,*,#7197,.T.);
#10268=ORIENTED_EDGE('',*,*,#7205,.T.);
#10269=ORIENTED_EDGE('',*,*,#7206,.T.);
#10270=ORIENTED_EDGE('',*,*,#7207,.F.);
#10271=ORIENTED_EDGE('',*,*,#7208,.F.);
#10272=ORIENTED_EDGE('',*,*,#7209,.F.);
#10273=ORIENTED_EDGE('',*,*,#7202,.T.);
#10274=ORIENTED_EDGE('',*,*,#7210,.T.);
#10275=ORIENTED_EDGE('',*,*,#7211,.T.);
#10276=ORIENTED_EDGE('',*,*,#7212,.F.);
#10277=ORIENTED_EDGE('',*,*,#7213,.F.);
#10278=ORIENTED_EDGE('',*,*,#7214,.F.);
#10279=ORIENTED_EDGE('',*,*,#7207,.T.);
#10280=ORIENTED_EDGE('',*,*,#7215,.T.);
#10281=ORIENTED_EDGE('',*,*,#7216,.T.);
#10282=ORIENTED_EDGE('',*,*,#7217,.F.);
#10283=ORIENTED_EDGE('',*,*,#7218,.F.);
#10284=ORIENTED_EDGE('',*,*,#7219,.F.);
#10285=ORIENTED_EDGE('',*,*,#7212,.T.);
#10286=ORIENTED_EDGE('',*,*,#7220,.T.);
#10287=ORIENTED_EDGE('',*,*,#7221,.T.);
#10288=ORIENTED_EDGE('',*,*,#7222,.F.);
#10289=ORIENTED_EDGE('',*,*,#7223,.F.);
#10290=ORIENTED_EDGE('',*,*,#7224,.F.);
#10291=ORIENTED_EDGE('',*,*,#7217,.T.);
#10292=ORIENTED_EDGE('',*,*,#7225,.T.);
#10293=ORIENTED_EDGE('',*,*,#7226,.T.);
#10294=ORIENTED_EDGE('',*,*,#7227,.F.);
#10295=ORIENTED_EDGE('',*,*,#7228,.F.);
#10296=ORIENTED_EDGE('',*,*,#7229,.F.);
#10297=ORIENTED_EDGE('',*,*,#7222,.T.);
#10298=ORIENTED_EDGE('',*,*,#7230,.T.);
#10299=ORIENTED_EDGE('',*,*,#7231,.T.);
#10300=ORIENTED_EDGE('',*,*,#7232,.F.);
#10301=ORIENTED_EDGE('',*,*,#7233,.F.);
#10302=ORIENTED_EDGE('',*,*,#7234,.F.);
#10303=ORIENTED_EDGE('',*,*,#7227,.T.);
#10304=ORIENTED_EDGE('',*,*,#7235,.T.);
#10305=ORIENTED_EDGE('',*,*,#7236,.T.);
#10306=ORIENTED_EDGE('',*,*,#7237,.F.);
#10307=ORIENTED_EDGE('',*,*,#7238,.F.);
#10308=ORIENTED_EDGE('',*,*,#7239,.F.);
#10309=ORIENTED_EDGE('',*,*,#7232,.T.);
#10310=ORIENTED_EDGE('',*,*,#7240,.T.);
#10311=ORIENTED_EDGE('',*,*,#7241,.T.);
#10312=ORIENTED_EDGE('',*,*,#7242,.F.);
#10313=ORIENTED_EDGE('',*,*,#7243,.F.);
#10314=ORIENTED_EDGE('',*,*,#7244,.F.);
#10315=ORIENTED_EDGE('',*,*,#7237,.T.);
#10316=ORIENTED_EDGE('',*,*,#7245,.T.);
#10317=ORIENTED_EDGE('',*,*,#7246,.T.);
#10318=ORIENTED_EDGE('',*,*,#7247,.F.);
#10319=ORIENTED_EDGE('',*,*,#7248,.F.);
#10320=ORIENTED_EDGE('',*,*,#7249,.F.);
#10321=ORIENTED_EDGE('',*,*,#7242,.T.);
#10322=ORIENTED_EDGE('',*,*,#7250,.T.);
#10323=ORIENTED_EDGE('',*,*,#7251,.T.);
#10324=ORIENTED_EDGE('',*,*,#7252,.F.);
#10325=ORIENTED_EDGE('',*,*,#7253,.F.);
#10326=ORIENTED_EDGE('',*,*,#7254,.F.);
#10327=ORIENTED_EDGE('',*,*,#7247,.T.);
#10328=ORIENTED_EDGE('',*,*,#7255,.T.);
#10329=ORIENTED_EDGE('',*,*,#7256,.T.);
#10330=ORIENTED_EDGE('',*,*,#7257,.F.);
#10331=ORIENTED_EDGE('',*,*,#7258,.F.);
#10332=ORIENTED_EDGE('',*,*,#7259,.F.);
#10333=ORIENTED_EDGE('',*,*,#7252,.T.);
#10334=ORIENTED_EDGE('',*,*,#7260,.T.);
#10335=ORIENTED_EDGE('',*,*,#7261,.T.);
#10336=ORIENTED_EDGE('',*,*,#7262,.F.);
#10337=ORIENTED_EDGE('',*,*,#7263,.F.);
#10338=ORIENTED_EDGE('',*,*,#7264,.F.);
#10339=ORIENTED_EDGE('',*,*,#7257,.T.);
#10340=ORIENTED_EDGE('',*,*,#7265,.T.);
#10341=ORIENTED_EDGE('',*,*,#7266,.T.);
#10342=ORIENTED_EDGE('',*,*,#7267,.F.);
#10343=ORIENTED_EDGE('',*,*,#7268,.F.);
#10344=ORIENTED_EDGE('',*,*,#7269,.F.);
#10345=ORIENTED_EDGE('',*,*,#7262,.T.);
#10346=ORIENTED_EDGE('',*,*,#7270,.T.);
#10347=ORIENTED_EDGE('',*,*,#7271,.T.);
#10348=ORIENTED_EDGE('',*,*,#7272,.F.);
#10349=ORIENTED_EDGE('',*,*,#7273,.F.);
#10350=ORIENTED_EDGE('',*,*,#7274,.F.);
#10351=ORIENTED_EDGE('',*,*,#7267,.T.);
#10352=ORIENTED_EDGE('',*,*,#7275,.T.);
#10353=ORIENTED_EDGE('',*,*,#7276,.T.);
#10354=ORIENTED_EDGE('',*,*,#7277,.F.);
#10355=ORIENTED_EDGE('',*,*,#7278,.F.);
#10356=ORIENTED_EDGE('',*,*,#7279,.F.);
#10357=ORIENTED_EDGE('',*,*,#7272,.T.);
#10358=ORIENTED_EDGE('',*,*,#7280,.T.);
#10359=ORIENTED_EDGE('',*,*,#7281,.T.);
#10360=ORIENTED_EDGE('',*,*,#7282,.F.);
#10361=ORIENTED_EDGE('',*,*,#7283,.F.);
#10362=ORIENTED_EDGE('',*,*,#7284,.F.);
#10363=ORIENTED_EDGE('',*,*,#7277,.T.);
#10364=ORIENTED_EDGE('',*,*,#7285,.T.);
#10365=ORIENTED_EDGE('',*,*,#7286,.T.);
#10366=ORIENTED_EDGE('',*,*,#7287,.F.);
#10367=ORIENTED_EDGE('',*,*,#7288,.F.);
#10368=ORIENTED_EDGE('',*,*,#7289,.F.);
#10369=ORIENTED_EDGE('',*,*,#7282,.T.);
#10370=ORIENTED_EDGE('',*,*,#7290,.T.);
#10371=ORIENTED_EDGE('',*,*,#7291,.T.);
#10372=ORIENTED_EDGE('',*,*,#7292,.F.);
#10373=ORIENTED_EDGE('',*,*,#7293,.F.);
#10374=ORIENTED_EDGE('',*,*,#7294,.F.);
#10375=ORIENTED_EDGE('',*,*,#7287,.T.);
#10376=ORIENTED_EDGE('',*,*,#7295,.T.);
#10377=ORIENTED_EDGE('',*,*,#7296,.T.);
#10378=ORIENTED_EDGE('',*,*,#7297,.F.);
#10379=ORIENTED_EDGE('',*,*,#7298,.F.);
#10380=ORIENTED_EDGE('',*,*,#7299,.F.);
#10381=ORIENTED_EDGE('',*,*,#7292,.T.);
#10382=ORIENTED_EDGE('',*,*,#7300,.T.);
#10383=ORIENTED_EDGE('',*,*,#7301,.T.);
#10384=ORIENTED_EDGE('',*,*,#7302,.F.);
#10385=ORIENTED_EDGE('',*,*,#7303,.F.);
#10386=ORIENTED_EDGE('',*,*,#7304,.F.);
#10387=ORIENTED_EDGE('',*,*,#7297,.T.);
#10388=ORIENTED_EDGE('',*,*,#7305,.T.);
#10389=ORIENTED_EDGE('',*,*,#7306,.T.);
#10390=ORIENTED_EDGE('',*,*,#7307,.F.);
#10391=ORIENTED_EDGE('',*,*,#7308,.F.);
#10392=ORIENTED_EDGE('',*,*,#7309,.F.);
#10393=ORIENTED_EDGE('',*,*,#7302,.T.);
#10394=ORIENTED_EDGE('',*,*,#7310,.T.);
#10395=ORIENTED_EDGE('',*,*,#7311,.T.);
#10396=ORIENTED_EDGE('',*,*,#7312,.F.);
#10397=ORIENTED_EDGE('',*,*,#7313,.F.);
#10398=ORIENTED_EDGE('',*,*,#7314,.F.);
#10399=ORIENTED_EDGE('',*,*,#7307,.T.);
#10400=ORIENTED_EDGE('',*,*,#7315,.T.);
#10401=ORIENTED_EDGE('',*,*,#7316,.T.);
#10402=ORIENTED_EDGE('',*,*,#7317,.F.);
#10403=ORIENTED_EDGE('',*,*,#7318,.F.);
#10404=ORIENTED_EDGE('',*,*,#7319,.F.);
#10405=ORIENTED_EDGE('',*,*,#7312,.T.);
#10406=ORIENTED_EDGE('',*,*,#7320,.T.);
#10407=ORIENTED_EDGE('',*,*,#7321,.T.);
#10408=ORIENTED_EDGE('',*,*,#7322,.F.);
#10409=ORIENTED_EDGE('',*,*,#7323,.F.);
#10410=ORIENTED_EDGE('',*,*,#7324,.F.);
#10411=ORIENTED_EDGE('',*,*,#7317,.T.);
#10412=ORIENTED_EDGE('',*,*,#7325,.T.);
#10413=ORIENTED_EDGE('',*,*,#7326,.T.);
#10414=ORIENTED_EDGE('',*,*,#7327,.F.);
#10415=ORIENTED_EDGE('',*,*,#7328,.F.);
#10416=ORIENTED_EDGE('',*,*,#7329,.F.);
#10417=ORIENTED_EDGE('',*,*,#7322,.T.);
#10418=ORIENTED_EDGE('',*,*,#7330,.T.);
#10419=ORIENTED_EDGE('',*,*,#7331,.T.);
#10420=ORIENTED_EDGE('',*,*,#7332,.F.);
#10421=ORIENTED_EDGE('',*,*,#7333,.F.);
#10422=ORIENTED_EDGE('',*,*,#7334,.F.);
#10423=ORIENTED_EDGE('',*,*,#7327,.T.);
#10424=ORIENTED_EDGE('',*,*,#7335,.T.);
#10425=ORIENTED_EDGE('',*,*,#7336,.T.);
#10426=ORIENTED_EDGE('',*,*,#7337,.F.);
#10427=ORIENTED_EDGE('',*,*,#7338,.F.);
#10428=ORIENTED_EDGE('',*,*,#7339,.F.);
#10429=ORIENTED_EDGE('',*,*,#7332,.T.);
#10430=ORIENTED_EDGE('',*,*,#7340,.T.);
#10431=ORIENTED_EDGE('',*,*,#7341,.T.);
#10432=ORIENTED_EDGE('',*,*,#7342,.F.);
#10433=ORIENTED_EDGE('',*,*,#7343,.F.);
#10434=ORIENTED_EDGE('',*,*,#7344,.F.);
#10435=ORIENTED_EDGE('',*,*,#7337,.T.);
#10436=ORIENTED_EDGE('',*,*,#7345,.T.);
#10437=ORIENTED_EDGE('',*,*,#7346,.T.);
#10438=ORIENTED_EDGE('',*,*,#7347,.F.);
#10439=ORIENTED_EDGE('',*,*,#7348,.F.);
#10440=ORIENTED_EDGE('',*,*,#7349,.F.);
#10441=ORIENTED_EDGE('',*,*,#7342,.T.);
#10442=ORIENTED_EDGE('',*,*,#7350,.T.);
#10443=ORIENTED_EDGE('',*,*,#7351,.T.);
#10444=ORIENTED_EDGE('',*,*,#7352,.F.);
#10445=ORIENTED_EDGE('',*,*,#7353,.F.);
#10446=ORIENTED_EDGE('',*,*,#7354,.F.);
#10447=ORIENTED_EDGE('',*,*,#7347,.T.);
#10448=ORIENTED_EDGE('',*,*,#7355,.T.);
#10449=ORIENTED_EDGE('',*,*,#7356,.T.);
#10450=ORIENTED_EDGE('',*,*,#7357,.T.);
#10451=ORIENTED_EDGE('',*,*,#7358,.F.);
#10452=ORIENTED_EDGE('',*,*,#7359,.T.);
#10453=ORIENTED_EDGE('',*,*,#7360,.T.);
#10454=ORIENTED_EDGE('',*,*,#7361,.T.);
#10455=ORIENTED_EDGE('',*,*,#7362,.T.);
#10456=ORIENTED_EDGE('',*,*,#7363,.T.);
#10457=ORIENTED_EDGE('',*,*,#7364,.T.);
#10458=ORIENTED_EDGE('',*,*,#7365,.T.);
#10459=ORIENTED_EDGE('',*,*,#7366,.T.);
#10460=ORIENTED_EDGE('',*,*,#7367,.T.);
#10461=ORIENTED_EDGE('',*,*,#7368,.T.);
#10462=ORIENTED_EDGE('',*,*,#7369,.T.);
#10463=ORIENTED_EDGE('',*,*,#7370,.T.);
#10464=ORIENTED_EDGE('',*,*,#7371,.T.);
#10465=ORIENTED_EDGE('',*,*,#7372,.T.);
#10466=ORIENTED_EDGE('',*,*,#7373,.T.);
#10467=ORIENTED_EDGE('',*,*,#7374,.T.);
#10468=ORIENTED_EDGE('',*,*,#7375,.T.);
#10469=ORIENTED_EDGE('',*,*,#7376,.T.);
#10470=ORIENTED_EDGE('',*,*,#7377,.T.);
#10471=ORIENTED_EDGE('',*,*,#7378,.T.);
#10472=ORIENTED_EDGE('',*,*,#7379,.T.);
#10473=ORIENTED_EDGE('',*,*,#7380,.T.);
#10474=ORIENTED_EDGE('',*,*,#7381,.T.);
#10475=ORIENTED_EDGE('',*,*,#7382,.T.);
#10476=ORIENTED_EDGE('',*,*,#7383,.T.);
#10477=ORIENTED_EDGE('',*,*,#7384,.T.);
#10478=ORIENTED_EDGE('',*,*,#7385,.T.);
#10479=ORIENTED_EDGE('',*,*,#7386,.T.);
#10480=ORIENTED_EDGE('',*,*,#7387,.T.);
#10481=ORIENTED_EDGE('',*,*,#7388,.T.);
#10482=ORIENTED_EDGE('',*,*,#7389,.T.);
#10483=ORIENTED_EDGE('',*,*,#7390,.T.);
#10484=ORIENTED_EDGE('',*,*,#7391,.T.);
#10485=ORIENTED_EDGE('',*,*,#7392,.T.);
#10486=ORIENTED_EDGE('',*,*,#7393,.T.);
#10487=ORIENTED_EDGE('',*,*,#7394,.T.);
#10488=ORIENTED_EDGE('',*,*,#7395,.T.);
#10489=ORIENTED_EDGE('',*,*,#7396,.T.);
#10490=ORIENTED_EDGE('',*,*,#7397,.T.);
#10491=ORIENTED_EDGE('',*,*,#7398,.T.);
#10492=ORIENTED_EDGE('',*,*,#7399,.T.);
#10493=ORIENTED_EDGE('',*,*,#7400,.F.);
#10494=ORIENTED_EDGE('',*,*,#7401,.T.);
#10495=ORIENTED_EDGE('',*,*,#7402,.T.);
#10496=ORIENTED_EDGE('',*,*,#7403,.T.);
#10497=ORIENTED_EDGE('',*,*,#7404,.T.);
#10498=ORIENTED_EDGE('',*,*,#7405,.T.);
#10499=ORIENTED_EDGE('',*,*,#7406,.T.);
#10500=ORIENTED_EDGE('',*,*,#7407,.T.);
#10501=ORIENTED_EDGE('',*,*,#7408,.T.);
#10502=ORIENTED_EDGE('',*,*,#7409,.T.);
#10503=ORIENTED_EDGE('',*,*,#7410,.T.);
#10504=ORIENTED_EDGE('',*,*,#7411,.T.);
#10505=ORIENTED_EDGE('',*,*,#7412,.T.);
#10506=ORIENTED_EDGE('',*,*,#7413,.T.);
#10507=ORIENTED_EDGE('',*,*,#7414,.T.);
#10508=ORIENTED_EDGE('',*,*,#7415,.T.);
#10509=ORIENTED_EDGE('',*,*,#7416,.T.);
#10510=ORIENTED_EDGE('',*,*,#7417,.T.);
#10511=ORIENTED_EDGE('',*,*,#7418,.T.);
#10512=ORIENTED_EDGE('',*,*,#7419,.T.);
#10513=ORIENTED_EDGE('',*,*,#7420,.T.);
#10514=ORIENTED_EDGE('',*,*,#7421,.T.);
#10515=ORIENTED_EDGE('',*,*,#7422,.T.);
#10516=ORIENTED_EDGE('',*,*,#7423,.T.);
#10517=ORIENTED_EDGE('',*,*,#7424,.T.);
#10518=ORIENTED_EDGE('',*,*,#7425,.T.);
#10519=ORIENTED_EDGE('',*,*,#7426,.T.);
#10520=ORIENTED_EDGE('',*,*,#7427,.T.);
#10521=ORIENTED_EDGE('',*,*,#7428,.T.);
#10522=ORIENTED_EDGE('',*,*,#7429,.T.);
#10523=ORIENTED_EDGE('',*,*,#7430,.T.);
#10524=ORIENTED_EDGE('',*,*,#7431,.T.);
#10525=ORIENTED_EDGE('',*,*,#7432,.T.);
#10526=ORIENTED_EDGE('',*,*,#7433,.T.);
#10527=ORIENTED_EDGE('',*,*,#7434,.T.);
#10528=ORIENTED_EDGE('',*,*,#7435,.T.);
#10529=ORIENTED_EDGE('',*,*,#7436,.T.);
#10530=ORIENTED_EDGE('',*,*,#7437,.T.);
#10531=ORIENTED_EDGE('',*,*,#7438,.T.);
#10532=ORIENTED_EDGE('',*,*,#7439,.T.);
#10533=ORIENTED_EDGE('',*,*,#7440,.T.);
#10534=ORIENTED_EDGE('',*,*,#7441,.T.);
#10535=ORIENTED_EDGE('',*,*,#7442,.T.);
#10536=ORIENTED_EDGE('',*,*,#7443,.T.);
#10537=ORIENTED_EDGE('',*,*,#7444,.T.);
#10538=ORIENTED_EDGE('',*,*,#7445,.T.);
#10539=ORIENTED_EDGE('',*,*,#7446,.T.);
#10540=ORIENTED_EDGE('',*,*,#7447,.T.);
#10541=ORIENTED_EDGE('',*,*,#7448,.T.);
#10542=ORIENTED_EDGE('',*,*,#7449,.T.);
#10543=ORIENTED_EDGE('',*,*,#7450,.T.);
#10544=ORIENTED_EDGE('',*,*,#7451,.T.);
#10545=ORIENTED_EDGE('',*,*,#7452,.T.);
#10546=ORIENTED_EDGE('',*,*,#7453,.T.);
#10547=ORIENTED_EDGE('',*,*,#7454,.T.);
#10548=ORIENTED_EDGE('',*,*,#7455,.T.);
#10549=ORIENTED_EDGE('',*,*,#7456,.T.);
#10550=ORIENTED_EDGE('',*,*,#7457,.T.);
#10551=ORIENTED_EDGE('',*,*,#7458,.T.);
#10552=ORIENTED_EDGE('',*,*,#7459,.T.);
#10553=ORIENTED_EDGE('',*,*,#7460,.T.);
#10554=ORIENTED_EDGE('',*,*,#7352,.T.);
#10555=ORIENTED_EDGE('',*,*,#7461,.T.);
#10556=ORIENTED_EDGE('',*,*,#7462,.T.);
#10557=ORIENTED_EDGE('',*,*,#7463,.F.);
#10558=ORIENTED_EDGE('',*,*,#7464,.F.);
#10559=ORIENTED_EDGE('',*,*,#7465,.F.);
#10560=ORIENTED_EDGE('',*,*,#7466,.F.);
#10561=ORIENTED_EDGE('',*,*,#7399,.F.);
#10562=ORIENTED_EDGE('',*,*,#7398,.F.);
#10563=ORIENTED_EDGE('',*,*,#7397,.F.);
#10564=ORIENTED_EDGE('',*,*,#7396,.F.);
#10565=ORIENTED_EDGE('',*,*,#7395,.F.);
#10566=ORIENTED_EDGE('',*,*,#7394,.F.);
#10567=ORIENTED_EDGE('',*,*,#7393,.F.);
#10568=ORIENTED_EDGE('',*,*,#7392,.F.);
#10569=ORIENTED_EDGE('',*,*,#7391,.F.);
#10570=ORIENTED_EDGE('',*,*,#7390,.F.);
#10571=ORIENTED_EDGE('',*,*,#7389,.F.);
#10572=ORIENTED_EDGE('',*,*,#7388,.F.);
#10573=ORIENTED_EDGE('',*,*,#7387,.F.);
#10574=ORIENTED_EDGE('',*,*,#7386,.F.);
#10575=ORIENTED_EDGE('',*,*,#7385,.F.);
#10576=ORIENTED_EDGE('',*,*,#7384,.F.);
#10577=ORIENTED_EDGE('',*,*,#7383,.F.);
#10578=ORIENTED_EDGE('',*,*,#7382,.F.);
#10579=ORIENTED_EDGE('',*,*,#7381,.F.);
#10580=ORIENTED_EDGE('',*,*,#7380,.F.);
#10581=ORIENTED_EDGE('',*,*,#7379,.F.);
#10582=ORIENTED_EDGE('',*,*,#7378,.F.);
#10583=ORIENTED_EDGE('',*,*,#7377,.F.);
#10584=ORIENTED_EDGE('',*,*,#7376,.F.);
#10585=ORIENTED_EDGE('',*,*,#7375,.F.);
#10586=ORIENTED_EDGE('',*,*,#7374,.F.);
#10587=ORIENTED_EDGE('',*,*,#7373,.F.);
#10588=ORIENTED_EDGE('',*,*,#7372,.F.);
#10589=ORIENTED_EDGE('',*,*,#7371,.F.);
#10590=ORIENTED_EDGE('',*,*,#7370,.F.);
#10591=ORIENTED_EDGE('',*,*,#7369,.F.);
#10592=ORIENTED_EDGE('',*,*,#7368,.F.);
#10593=ORIENTED_EDGE('',*,*,#7367,.F.);
#10594=ORIENTED_EDGE('',*,*,#7366,.F.);
#10595=ORIENTED_EDGE('',*,*,#7365,.F.);
#10596=ORIENTED_EDGE('',*,*,#7364,.F.);
#10597=ORIENTED_EDGE('',*,*,#7363,.F.);
#10598=ORIENTED_EDGE('',*,*,#7362,.F.);
#10599=ORIENTED_EDGE('',*,*,#7361,.F.);
#10600=ORIENTED_EDGE('',*,*,#7360,.F.);
#10601=ORIENTED_EDGE('',*,*,#7359,.F.);
#10602=ORIENTED_EDGE('',*,*,#7467,.F.);
#10603=ORIENTED_EDGE('',*,*,#7059,.T.);
#10604=ORIENTED_EDGE('',*,*,#7064,.T.);
#10605=ORIENTED_EDGE('',*,*,#7063,.T.);
#10606=ORIENTED_EDGE('',*,*,#7069,.T.);
#10607=ORIENTED_EDGE('',*,*,#7068,.T.);
#10608=ORIENTED_EDGE('',*,*,#7074,.T.);
#10609=ORIENTED_EDGE('',*,*,#7073,.T.);
#10610=ORIENTED_EDGE('',*,*,#7079,.T.);
#10611=ORIENTED_EDGE('',*,*,#7078,.T.);
#10612=ORIENTED_EDGE('',*,*,#7084,.T.);
#10613=ORIENTED_EDGE('',*,*,#7083,.T.);
#10614=ORIENTED_EDGE('',*,*,#7089,.T.);
#10615=ORIENTED_EDGE('',*,*,#7088,.T.);
#10616=ORIENTED_EDGE('',*,*,#7094,.T.);
#10617=ORIENTED_EDGE('',*,*,#7093,.T.);
#10618=ORIENTED_EDGE('',*,*,#7099,.T.);
#10619=ORIENTED_EDGE('',*,*,#7098,.T.);
#10620=ORIENTED_EDGE('',*,*,#7104,.T.);
#10621=ORIENTED_EDGE('',*,*,#7103,.T.);
#10622=ORIENTED_EDGE('',*,*,#7109,.T.);
#10623=ORIENTED_EDGE('',*,*,#7108,.T.);
#10624=ORIENTED_EDGE('',*,*,#7114,.T.);
#10625=ORIENTED_EDGE('',*,*,#7113,.T.);
#10626=ORIENTED_EDGE('',*,*,#7119,.T.);
#10627=ORIENTED_EDGE('',*,*,#7118,.T.);
#10628=ORIENTED_EDGE('',*,*,#7124,.T.);
#10629=ORIENTED_EDGE('',*,*,#7123,.T.);
#10630=ORIENTED_EDGE('',*,*,#7129,.T.);
#10631=ORIENTED_EDGE('',*,*,#7128,.T.);
#10632=ORIENTED_EDGE('',*,*,#7134,.T.);
#10633=ORIENTED_EDGE('',*,*,#7133,.T.);
#10634=ORIENTED_EDGE('',*,*,#7139,.T.);
#10635=ORIENTED_EDGE('',*,*,#7138,.T.);
#10636=ORIENTED_EDGE('',*,*,#7144,.T.);
#10637=ORIENTED_EDGE('',*,*,#7143,.T.);
#10638=ORIENTED_EDGE('',*,*,#7149,.T.);
#10639=ORIENTED_EDGE('',*,*,#7148,.T.);
#10640=ORIENTED_EDGE('',*,*,#7154,.T.);
#10641=ORIENTED_EDGE('',*,*,#7153,.T.);
#10642=ORIENTED_EDGE('',*,*,#7159,.T.);
#10643=ORIENTED_EDGE('',*,*,#7158,.T.);
#10644=ORIENTED_EDGE('',*,*,#7164,.T.);
#10645=ORIENTED_EDGE('',*,*,#7163,.T.);
#10646=ORIENTED_EDGE('',*,*,#7169,.T.);
#10647=ORIENTED_EDGE('',*,*,#7168,.T.);
#10648=ORIENTED_EDGE('',*,*,#7174,.T.);
#10649=ORIENTED_EDGE('',*,*,#7173,.T.);
#10650=ORIENTED_EDGE('',*,*,#7179,.T.);
#10651=ORIENTED_EDGE('',*,*,#7178,.T.);
#10652=ORIENTED_EDGE('',*,*,#7184,.T.);
#10653=ORIENTED_EDGE('',*,*,#7183,.T.);
#10654=ORIENTED_EDGE('',*,*,#7189,.T.);
#10655=ORIENTED_EDGE('',*,*,#7188,.T.);
#10656=ORIENTED_EDGE('',*,*,#7194,.T.);
#10657=ORIENTED_EDGE('',*,*,#7193,.T.);
#10658=ORIENTED_EDGE('',*,*,#7199,.T.);
#10659=ORIENTED_EDGE('',*,*,#7198,.T.);
#10660=ORIENTED_EDGE('',*,*,#7204,.T.);
#10661=ORIENTED_EDGE('',*,*,#7203,.T.);
#10662=ORIENTED_EDGE('',*,*,#7209,.T.);
#10663=ORIENTED_EDGE('',*,*,#7208,.T.);
#10664=ORIENTED_EDGE('',*,*,#7214,.T.);
#10665=ORIENTED_EDGE('',*,*,#7213,.T.);
#10666=ORIENTED_EDGE('',*,*,#7219,.T.);
#10667=ORIENTED_EDGE('',*,*,#7218,.T.);
#10668=ORIENTED_EDGE('',*,*,#7224,.T.);
#10669=ORIENTED_EDGE('',*,*,#7223,.T.);
#10670=ORIENTED_EDGE('',*,*,#7229,.T.);
#10671=ORIENTED_EDGE('',*,*,#7228,.T.);
#10672=ORIENTED_EDGE('',*,*,#7234,.T.);
#10673=ORIENTED_EDGE('',*,*,#7233,.T.);
#10674=ORIENTED_EDGE('',*,*,#7239,.T.);
#10675=ORIENTED_EDGE('',*,*,#7238,.T.);
#10676=ORIENTED_EDGE('',*,*,#7244,.T.);
#10677=ORIENTED_EDGE('',*,*,#7243,.T.);
#10678=ORIENTED_EDGE('',*,*,#7249,.T.);
#10679=ORIENTED_EDGE('',*,*,#7248,.T.);
#10680=ORIENTED_EDGE('',*,*,#7254,.T.);
#10681=ORIENTED_EDGE('',*,*,#7253,.T.);
#10682=ORIENTED_EDGE('',*,*,#7259,.T.);
#10683=ORIENTED_EDGE('',*,*,#7258,.T.);
#10684=ORIENTED_EDGE('',*,*,#7264,.T.);
#10685=ORIENTED_EDGE('',*,*,#7263,.T.);
#10686=ORIENTED_EDGE('',*,*,#7269,.T.);
#10687=ORIENTED_EDGE('',*,*,#7268,.T.);
#10688=ORIENTED_EDGE('',*,*,#7274,.T.);
#10689=ORIENTED_EDGE('',*,*,#7273,.T.);
#10690=ORIENTED_EDGE('',*,*,#7279,.T.);
#10691=ORIENTED_EDGE('',*,*,#7278,.T.);
#10692=ORIENTED_EDGE('',*,*,#7284,.T.);
#10693=ORIENTED_EDGE('',*,*,#7283,.T.);
#10694=ORIENTED_EDGE('',*,*,#7289,.T.);
#10695=ORIENTED_EDGE('',*,*,#7288,.T.);
#10696=ORIENTED_EDGE('',*,*,#7294,.T.);
#10697=ORIENTED_EDGE('',*,*,#7293,.T.);
#10698=ORIENTED_EDGE('',*,*,#7299,.T.);
#10699=ORIENTED_EDGE('',*,*,#7298,.T.);
#10700=ORIENTED_EDGE('',*,*,#7304,.T.);
#10701=ORIENTED_EDGE('',*,*,#7303,.T.);
#10702=ORIENTED_EDGE('',*,*,#7309,.T.);
#10703=ORIENTED_EDGE('',*,*,#7308,.T.);
#10704=ORIENTED_EDGE('',*,*,#7314,.T.);
#10705=ORIENTED_EDGE('',*,*,#7313,.T.);
#10706=ORIENTED_EDGE('',*,*,#7319,.T.);
#10707=ORIENTED_EDGE('',*,*,#7318,.T.);
#10708=ORIENTED_EDGE('',*,*,#7324,.T.);
#10709=ORIENTED_EDGE('',*,*,#7323,.T.);
#10710=ORIENTED_EDGE('',*,*,#7329,.T.);
#10711=ORIENTED_EDGE('',*,*,#7328,.T.);
#10712=ORIENTED_EDGE('',*,*,#7334,.T.);
#10713=ORIENTED_EDGE('',*,*,#7333,.T.);
#10714=ORIENTED_EDGE('',*,*,#7339,.T.);
#10715=ORIENTED_EDGE('',*,*,#7338,.T.);
#10716=ORIENTED_EDGE('',*,*,#7344,.T.);
#10717=ORIENTED_EDGE('',*,*,#7343,.T.);
#10718=ORIENTED_EDGE('',*,*,#7349,.T.);
#10719=ORIENTED_EDGE('',*,*,#7348,.T.);
#10720=ORIENTED_EDGE('',*,*,#7354,.T.);
#10721=ORIENTED_EDGE('',*,*,#7353,.T.);
#10722=ORIENTED_EDGE('',*,*,#7465,.T.);
#10723=ORIENTED_EDGE('',*,*,#7464,.T.);
#10724=ORIENTED_EDGE('',*,*,#7468,.F.);
#10725=ORIENTED_EDGE('',*,*,#7462,.F.);
#10726=ORIENTED_EDGE('',*,*,#7461,.F.);
#10727=ORIENTED_EDGE('',*,*,#7356,.F.);
#10728=ORIENTED_EDGE('',*,*,#7355,.F.);
#10729=ORIENTED_EDGE('',*,*,#7351,.F.);
#10730=ORIENTED_EDGE('',*,*,#7350,.F.);
#10731=ORIENTED_EDGE('',*,*,#7346,.F.);
#10732=ORIENTED_EDGE('',*,*,#7345,.F.);
#10733=ORIENTED_EDGE('',*,*,#7341,.F.);
#10734=ORIENTED_EDGE('',*,*,#7340,.F.);
#10735=ORIENTED_EDGE('',*,*,#7336,.F.);
#10736=ORIENTED_EDGE('',*,*,#7335,.F.);
#10737=ORIENTED_EDGE('',*,*,#7331,.F.);
#10738=ORIENTED_EDGE('',*,*,#7330,.F.);
#10739=ORIENTED_EDGE('',*,*,#7326,.F.);
#10740=ORIENTED_EDGE('',*,*,#7325,.F.);
#10741=ORIENTED_EDGE('',*,*,#7321,.F.);
#10742=ORIENTED_EDGE('',*,*,#7320,.F.);
#10743=ORIENTED_EDGE('',*,*,#7316,.F.);
#10744=ORIENTED_EDGE('',*,*,#7315,.F.);
#10745=ORIENTED_EDGE('',*,*,#7311,.F.);
#10746=ORIENTED_EDGE('',*,*,#7310,.F.);
#10747=ORIENTED_EDGE('',*,*,#7306,.F.);
#10748=ORIENTED_EDGE('',*,*,#7305,.F.);
#10749=ORIENTED_EDGE('',*,*,#7301,.F.);
#10750=ORIENTED_EDGE('',*,*,#7300,.F.);
#10751=ORIENTED_EDGE('',*,*,#7296,.F.);
#10752=ORIENTED_EDGE('',*,*,#7295,.F.);
#10753=ORIENTED_EDGE('',*,*,#7291,.F.);
#10754=ORIENTED_EDGE('',*,*,#7290,.F.);
#10755=ORIENTED_EDGE('',*,*,#7286,.F.);
#10756=ORIENTED_EDGE('',*,*,#7285,.F.);
#10757=ORIENTED_EDGE('',*,*,#7281,.F.);
#10758=ORIENTED_EDGE('',*,*,#7280,.F.);
#10759=ORIENTED_EDGE('',*,*,#7276,.F.);
#10760=ORIENTED_EDGE('',*,*,#7275,.F.);
#10761=ORIENTED_EDGE('',*,*,#7271,.F.);
#10762=ORIENTED_EDGE('',*,*,#7270,.F.);
#10763=ORIENTED_EDGE('',*,*,#7266,.F.);
#10764=ORIENTED_EDGE('',*,*,#7265,.F.);
#10765=ORIENTED_EDGE('',*,*,#7261,.F.);
#10766=ORIENTED_EDGE('',*,*,#7260,.F.);
#10767=ORIENTED_EDGE('',*,*,#7256,.F.);
#10768=ORIENTED_EDGE('',*,*,#7255,.F.);
#10769=ORIENTED_EDGE('',*,*,#7251,.F.);
#10770=ORIENTED_EDGE('',*,*,#7250,.F.);
#10771=ORIENTED_EDGE('',*,*,#7246,.F.);
#10772=ORIENTED_EDGE('',*,*,#7245,.F.);
#10773=ORIENTED_EDGE('',*,*,#7241,.F.);
#10774=ORIENTED_EDGE('',*,*,#7240,.F.);
#10775=ORIENTED_EDGE('',*,*,#7236,.F.);
#10776=ORIENTED_EDGE('',*,*,#7235,.F.);
#10777=ORIENTED_EDGE('',*,*,#7231,.F.);
#10778=ORIENTED_EDGE('',*,*,#7230,.F.);
#10779=ORIENTED_EDGE('',*,*,#7226,.F.);
#10780=ORIENTED_EDGE('',*,*,#7225,.F.);
#10781=ORIENTED_EDGE('',*,*,#7221,.F.);
#10782=ORIENTED_EDGE('',*,*,#7220,.F.);
#10783=ORIENTED_EDGE('',*,*,#7216,.F.);
#10784=ORIENTED_EDGE('',*,*,#7215,.F.);
#10785=ORIENTED_EDGE('',*,*,#7211,.F.);
#10786=ORIENTED_EDGE('',*,*,#7210,.F.);
#10787=ORIENTED_EDGE('',*,*,#7206,.F.);
#10788=ORIENTED_EDGE('',*,*,#7205,.F.);
#10789=ORIENTED_EDGE('',*,*,#7201,.F.);
#10790=ORIENTED_EDGE('',*,*,#7200,.F.);
#10791=ORIENTED_EDGE('',*,*,#7196,.F.);
#10792=ORIENTED_EDGE('',*,*,#7195,.F.);
#10793=ORIENTED_EDGE('',*,*,#7191,.F.);
#10794=ORIENTED_EDGE('',*,*,#7190,.F.);
#10795=ORIENTED_EDGE('',*,*,#7186,.F.);
#10796=ORIENTED_EDGE('',*,*,#7185,.F.);
#10797=ORIENTED_EDGE('',*,*,#7181,.F.);
#10798=ORIENTED_EDGE('',*,*,#7180,.F.);
#10799=ORIENTED_EDGE('',*,*,#7176,.F.);
#10800=ORIENTED_EDGE('',*,*,#7175,.F.);
#10801=ORIENTED_EDGE('',*,*,#7171,.F.);
#10802=ORIENTED_EDGE('',*,*,#7170,.F.);
#10803=ORIENTED_EDGE('',*,*,#7166,.F.);
#10804=ORIENTED_EDGE('',*,*,#7165,.F.);
#10805=ORIENTED_EDGE('',*,*,#7161,.F.);
#10806=ORIENTED_EDGE('',*,*,#7160,.F.);
#10807=ORIENTED_EDGE('',*,*,#7156,.F.);
#10808=ORIENTED_EDGE('',*,*,#7155,.F.);
#10809=ORIENTED_EDGE('',*,*,#7151,.F.);
#10810=ORIENTED_EDGE('',*,*,#7150,.F.);
#10811=ORIENTED_EDGE('',*,*,#7146,.F.);
#10812=ORIENTED_EDGE('',*,*,#7145,.F.);
#10813=ORIENTED_EDGE('',*,*,#7141,.F.);
#10814=ORIENTED_EDGE('',*,*,#7140,.F.);
#10815=ORIENTED_EDGE('',*,*,#7136,.F.);
#10816=ORIENTED_EDGE('',*,*,#7135,.F.);
#10817=ORIENTED_EDGE('',*,*,#7131,.F.);
#10818=ORIENTED_EDGE('',*,*,#7130,.F.);
#10819=ORIENTED_EDGE('',*,*,#7126,.F.);
#10820=ORIENTED_EDGE('',*,*,#7125,.F.);
#10821=ORIENTED_EDGE('',*,*,#7121,.F.);
#10822=ORIENTED_EDGE('',*,*,#7120,.F.);
#10823=ORIENTED_EDGE('',*,*,#7116,.F.);
#10824=ORIENTED_EDGE('',*,*,#7115,.F.);
#10825=ORIENTED_EDGE('',*,*,#7111,.F.);
#10826=ORIENTED_EDGE('',*,*,#7110,.F.);
#10827=ORIENTED_EDGE('',*,*,#7106,.F.);
#10828=ORIENTED_EDGE('',*,*,#7105,.F.);
#10829=ORIENTED_EDGE('',*,*,#7101,.F.);
#10830=ORIENTED_EDGE('',*,*,#7100,.F.);
#10831=ORIENTED_EDGE('',*,*,#7096,.F.);
#10832=ORIENTED_EDGE('',*,*,#7095,.F.);
#10833=ORIENTED_EDGE('',*,*,#7091,.F.);
#10834=ORIENTED_EDGE('',*,*,#7090,.F.);
#10835=ORIENTED_EDGE('',*,*,#7086,.F.);
#10836=ORIENTED_EDGE('',*,*,#7085,.F.);
#10837=ORIENTED_EDGE('',*,*,#7081,.F.);
#10838=ORIENTED_EDGE('',*,*,#7080,.F.);
#10839=ORIENTED_EDGE('',*,*,#7076,.F.);
#10840=ORIENTED_EDGE('',*,*,#7075,.F.);
#10841=ORIENTED_EDGE('',*,*,#7071,.F.);
#10842=ORIENTED_EDGE('',*,*,#7070,.F.);
#10843=ORIENTED_EDGE('',*,*,#7066,.F.);
#10844=ORIENTED_EDGE('',*,*,#7065,.F.);
#10845=ORIENTED_EDGE('',*,*,#7061,.F.);
#10846=ORIENTED_EDGE('',*,*,#7469,.F.);
#10847=ORIENTED_EDGE('',*,*,#7357,.F.);
#10848=ORIENTED_EDGE('',*,*,#7460,.F.);
#10849=ORIENTED_EDGE('',*,*,#7459,.F.);
#10850=ORIENTED_EDGE('',*,*,#7458,.F.);
#10851=ORIENTED_EDGE('',*,*,#7457,.F.);
#10852=ORIENTED_EDGE('',*,*,#7456,.F.);
#10853=ORIENTED_EDGE('',*,*,#7455,.F.);
#10854=ORIENTED_EDGE('',*,*,#7454,.F.);
#10855=ORIENTED_EDGE('',*,*,#7453,.F.);
#10856=ORIENTED_EDGE('',*,*,#7452,.F.);
#10857=ORIENTED_EDGE('',*,*,#7451,.F.);
#10858=ORIENTED_EDGE('',*,*,#7450,.F.);
#10859=ORIENTED_EDGE('',*,*,#7449,.F.);
#10860=ORIENTED_EDGE('',*,*,#7448,.F.);
#10861=ORIENTED_EDGE('',*,*,#7447,.F.);
#10862=ORIENTED_EDGE('',*,*,#7446,.F.);
#10863=ORIENTED_EDGE('',*,*,#7445,.F.);
#10864=ORIENTED_EDGE('',*,*,#7444,.F.);
#10865=ORIENTED_EDGE('',*,*,#7443,.F.);
#10866=ORIENTED_EDGE('',*,*,#7442,.F.);
#10867=ORIENTED_EDGE('',*,*,#7441,.F.);
#10868=ORIENTED_EDGE('',*,*,#7440,.F.);
#10869=ORIENTED_EDGE('',*,*,#7439,.F.);
#10870=ORIENTED_EDGE('',*,*,#7438,.F.);
#10871=ORIENTED_EDGE('',*,*,#7437,.F.);
#10872=ORIENTED_EDGE('',*,*,#7436,.F.);
#10873=ORIENTED_EDGE('',*,*,#7435,.F.);
#10874=ORIENTED_EDGE('',*,*,#7434,.F.);
#10875=ORIENTED_EDGE('',*,*,#7433,.F.);
#10876=ORIENTED_EDGE('',*,*,#7432,.F.);
#10877=ORIENTED_EDGE('',*,*,#7431,.F.);
#10878=ORIENTED_EDGE('',*,*,#7430,.F.);
#10879=ORIENTED_EDGE('',*,*,#7429,.F.);
#10880=ORIENTED_EDGE('',*,*,#7428,.F.);
#10881=ORIENTED_EDGE('',*,*,#7427,.F.);
#10882=ORIENTED_EDGE('',*,*,#7426,.F.);
#10883=ORIENTED_EDGE('',*,*,#7425,.F.);
#10884=ORIENTED_EDGE('',*,*,#7424,.F.);
#10885=ORIENTED_EDGE('',*,*,#7423,.F.);
#10886=ORIENTED_EDGE('',*,*,#7422,.F.);
#10887=ORIENTED_EDGE('',*,*,#7421,.F.);
#10888=ORIENTED_EDGE('',*,*,#7420,.F.);
#10889=ORIENTED_EDGE('',*,*,#7419,.F.);
#10890=ORIENTED_EDGE('',*,*,#7418,.F.);
#10891=ORIENTED_EDGE('',*,*,#7417,.F.);
#10892=ORIENTED_EDGE('',*,*,#7416,.F.);
#10893=ORIENTED_EDGE('',*,*,#7415,.F.);
#10894=ORIENTED_EDGE('',*,*,#7414,.F.);
#10895=ORIENTED_EDGE('',*,*,#7413,.F.);
#10896=ORIENTED_EDGE('',*,*,#7412,.F.);
#10897=ORIENTED_EDGE('',*,*,#7411,.F.);
#10898=ORIENTED_EDGE('',*,*,#7410,.F.);
#10899=ORIENTED_EDGE('',*,*,#7409,.F.);
#10900=ORIENTED_EDGE('',*,*,#7408,.F.);
#10901=ORIENTED_EDGE('',*,*,#7407,.F.);
#10902=ORIENTED_EDGE('',*,*,#7406,.F.);
#10903=ORIENTED_EDGE('',*,*,#7405,.F.);
#10904=ORIENTED_EDGE('',*,*,#7404,.F.);
#10905=ORIENTED_EDGE('',*,*,#7403,.F.);
#10906=ORIENTED_EDGE('',*,*,#7402,.F.);
#10907=ORIENTED_EDGE('',*,*,#7401,.F.);
#10908=ORIENTED_EDGE('',*,*,#7470,.F.);
#10909=ORIENTED_EDGE('',*,*,#7471,.T.);
#10910=ORIENTED_EDGE('',*,*,#7472,.F.);
#10911=ORIENTED_EDGE('',*,*,#7471,.F.);
#10912=ORIENTED_EDGE('',*,*,#7473,.F.);
#10913=ORIENTED_EDGE('',*,*,#7474,.T.);
#10914=ORIENTED_EDGE('',*,*,#7475,.F.);
#10915=ORIENTED_EDGE('',*,*,#7474,.F.);
#10916=ORIENTED_EDGE('',*,*,#7476,.F.);
#10917=ORIENTED_EDGE('',*,*,#7477,.T.);
#10918=ORIENTED_EDGE('',*,*,#7478,.F.);
#10919=ORIENTED_EDGE('',*,*,#7477,.F.);
#10920=ORIENTED_EDGE('',*,*,#7479,.F.);
#10921=ORIENTED_EDGE('',*,*,#7480,.T.);
#10922=ORIENTED_EDGE('',*,*,#7481,.F.);
#10923=ORIENTED_EDGE('',*,*,#7480,.F.);
#10924=ORIENTED_EDGE('',*,*,#7482,.T.);
#10925=ORIENTED_EDGE('',*,*,#7483,.T.);
#10926=ORIENTED_EDGE('',*,*,#7484,.T.);
#10927=ORIENTED_EDGE('',*,*,#7483,.F.);
#10928=ORIENTED_EDGE('',*,*,#7485,.T.);
#10929=ORIENTED_EDGE('',*,*,#7486,.F.);
#10930=ORIENTED_EDGE('',*,*,#7487,.F.);
#10931=ORIENTED_EDGE('',*,*,#7488,.T.);
#10932=ORIENTED_EDGE('',*,*,#7485,.F.);
#10933=ORIENTED_EDGE('',*,*,#7482,.F.);
#10934=ORIENTED_EDGE('',*,*,#7488,.F.);
#10935=ORIENTED_EDGE('',*,*,#7484,.F.);
#10936=ORIENTED_EDGE('',*,*,#7400,.T.);
#10937=ORIENTED_EDGE('',*,*,#7466,.T.);
#10938=ORIENTED_EDGE('',*,*,#7463,.T.);
#10939=ORIENTED_EDGE('',*,*,#7468,.T.);
#10940=ORIENTED_EDGE('',*,*,#7481,.T.);
#10941=ORIENTED_EDGE('',*,*,#7478,.T.);
#10942=ORIENTED_EDGE('',*,*,#7475,.T.);
#10943=ORIENTED_EDGE('',*,*,#7472,.T.);
#10944=ORIENTED_EDGE('',*,*,#7489,.T.);
#10945=ORIENTED_EDGE('',*,*,#7490,.T.);
#10946=ORIENTED_EDGE('',*,*,#7486,.T.);
#10947=ORIENTED_EDGE('',*,*,#7487,.T.);
#10948=ORIENTED_EDGE('',*,*,#7490,.F.);
#10949=ORIENTED_EDGE('',*,*,#7489,.F.);
#10950=ORIENTED_EDGE('',*,*,#7470,.T.);
#10951=ORIENTED_EDGE('',*,*,#7473,.T.);
#10952=ORIENTED_EDGE('',*,*,#7476,.T.);
#10953=ORIENTED_EDGE('',*,*,#7479,.T.);
#10954=ORIENTED_EDGE('',*,*,#7467,.T.);
#10955=ORIENTED_EDGE('',*,*,#7358,.T.);
#10956=ORIENTED_EDGE('',*,*,#7469,.T.);
#10957=ORIENTED_EDGE('',*,*,#7060,.T.);
#10958=ORIENTED_EDGE('',*,*,#7491,.F.);
#10959=ORIENTED_EDGE('',*,*,#7492,.T.);
#10960=ORIENTED_EDGE('',*,*,#7493,.T.);
#10961=ORIENTED_EDGE('',*,*,#7494,.T.);
#10962=ORIENTED_EDGE('',*,*,#7495,.T.);
#10963=ORIENTED_EDGE('',*,*,#7496,.T.);
#10964=ORIENTED_EDGE('',*,*,#7497,.F.);
#10965=ORIENTED_EDGE('',*,*,#7498,.T.);
#10966=ORIENTED_EDGE('',*,*,#7499,.T.);
#10967=ORIENTED_EDGE('',*,*,#7500,.T.);
#10968=ORIENTED_EDGE('',*,*,#7491,.T.);
#10969=ORIENTED_EDGE('',*,*,#7501,.T.);
#10970=ORIENTED_EDGE('',*,*,#7502,.T.);
#10971=ORIENTED_EDGE('',*,*,#7503,.T.);
#10972=ORIENTED_EDGE('',*,*,#7504,.F.);
#10973=ORIENTED_EDGE('',*,*,#7505,.T.);
#10974=ORIENTED_EDGE('',*,*,#7506,.T.);
#10975=ORIENTED_EDGE('',*,*,#7507,.T.);
#10976=ORIENTED_EDGE('',*,*,#7497,.T.);
#10977=ORIENTED_EDGE('',*,*,#7508,.T.);
#10978=ORIENTED_EDGE('',*,*,#7509,.T.);
#10979=ORIENTED_EDGE('',*,*,#7510,.T.);
#10980=ORIENTED_EDGE('',*,*,#7511,.F.);
#10981=ORIENTED_EDGE('',*,*,#7512,.T.);
#10982=ORIENTED_EDGE('',*,*,#7513,.T.);
#10983=ORIENTED_EDGE('',*,*,#7514,.T.);
#10984=ORIENTED_EDGE('',*,*,#7504,.T.);
#10985=ORIENTED_EDGE('',*,*,#7515,.T.);
#10986=ORIENTED_EDGE('',*,*,#7516,.T.);
#10987=ORIENTED_EDGE('',*,*,#7517,.T.);
#10988=ORIENTED_EDGE('',*,*,#7518,.F.);
#10989=ORIENTED_EDGE('',*,*,#7519,.T.);
#10990=ORIENTED_EDGE('',*,*,#7520,.T.);
#10991=ORIENTED_EDGE('',*,*,#7521,.T.);
#10992=ORIENTED_EDGE('',*,*,#7511,.T.);
#10993=ORIENTED_EDGE('',*,*,#7522,.T.);
#10994=ORIENTED_EDGE('',*,*,#7523,.T.);
#10995=ORIENTED_EDGE('',*,*,#7524,.T.);
#10996=ORIENTED_EDGE('',*,*,#7525,.F.);
#10997=ORIENTED_EDGE('',*,*,#7526,.T.);
#10998=ORIENTED_EDGE('',*,*,#7527,.T.);
#10999=ORIENTED_EDGE('',*,*,#7528,.T.);
#11000=ORIENTED_EDGE('',*,*,#7529,.T.);
#11001=ORIENTED_EDGE('',*,*,#7518,.T.);
#11002=ORIENTED_EDGE('',*,*,#7530,.T.);
#11003=ORIENTED_EDGE('',*,*,#7531,.T.);
#11004=ORIENTED_EDGE('',*,*,#7532,.T.);
#11005=ORIENTED_EDGE('',*,*,#7525,.T.);
#11006=ORIENTED_EDGE('',*,*,#7533,.T.);
#11007=ORIENTED_EDGE('',*,*,#7534,.T.);
#11008=ORIENTED_EDGE('',*,*,#7535,.F.);
#11009=ORIENTED_EDGE('',*,*,#7536,.F.);
#11010=ORIENTED_EDGE('',*,*,#7537,.F.);
#11011=ORIENTED_EDGE('',*,*,#7538,.F.);
#11012=ORIENTED_EDGE('',*,*,#7494,.F.);
#11013=ORIENTED_EDGE('',*,*,#7539,.F.);
#11014=ORIENTED_EDGE('',*,*,#7540,.F.);
#11015=ORIENTED_EDGE('',*,*,#7538,.T.);
#11016=ORIENTED_EDGE('',*,*,#7541,.F.);
#11017=ORIENTED_EDGE('',*,*,#7495,.F.);
#11018=ORIENTED_EDGE('',*,*,#7537,.T.);
#11019=ORIENTED_EDGE('',*,*,#7542,.T.);
#11020=ORIENTED_EDGE('',*,*,#7543,.F.);
#11021=ORIENTED_EDGE('',*,*,#7501,.F.);
#11022=ORIENTED_EDGE('',*,*,#7496,.F.);
#11023=ORIENTED_EDGE('',*,*,#7541,.T.);
#11024=ORIENTED_EDGE('',*,*,#7536,.T.);
#11025=ORIENTED_EDGE('',*,*,#7544,.T.);
#11026=ORIENTED_EDGE('',*,*,#7545,.F.);
#11027=ORIENTED_EDGE('',*,*,#7542,.F.);
#11028=ORIENTED_EDGE('',*,*,#7534,.F.);
#11029=ORIENTED_EDGE('',*,*,#7546,.F.);
#11030=ORIENTED_EDGE('',*,*,#7547,.F.);
#11031=ORIENTED_EDGE('',*,*,#7548,.F.);
#11032=ORIENTED_EDGE('',*,*,#7549,.F.);
#11033=ORIENTED_EDGE('',*,*,#7550,.F.);
#11034=ORIENTED_EDGE('',*,*,#7526,.F.);
#11035=ORIENTED_EDGE('',*,*,#7551,.T.);
#11036=ORIENTED_EDGE('',*,*,#7548,.T.);
#11037=ORIENTED_EDGE('',*,*,#7552,.F.);
#11038=ORIENTED_EDGE('',*,*,#7553,.T.);
#11039=ORIENTED_EDGE('',*,*,#7554,.T.);
#11040=ORIENTED_EDGE('',*,*,#7547,.T.);
#11041=ORIENTED_EDGE('',*,*,#7555,.T.);
#11042=ORIENTED_EDGE('',*,*,#7552,.T.);
#11043=ORIENTED_EDGE('',*,*,#7546,.T.);
#11044=ORIENTED_EDGE('',*,*,#7533,.F.);
#11045=ORIENTED_EDGE('',*,*,#7532,.F.);
#11046=ORIENTED_EDGE('',*,*,#7556,.T.);
#11047=ORIENTED_EDGE('',*,*,#7557,.T.);
#11048=ORIENTED_EDGE('',*,*,#7555,.F.);
#11049=ORIENTED_EDGE('',*,*,#7558,.F.);
#11050=ORIENTED_EDGE('',*,*,#7559,.T.);
#11051=ORIENTED_EDGE('',*,*,#7540,.T.);
#11052=ORIENTED_EDGE('',*,*,#7559,.F.);
#11053=ORIENTED_EDGE('',*,*,#7551,.F.);
#11054=ORIENTED_EDGE('',*,*,#7560,.T.);
#11055=ORIENTED_EDGE('',*,*,#7561,.F.);
#11056=ORIENTED_EDGE('',*,*,#7560,.F.);
#11057=ORIENTED_EDGE('',*,*,#7561,.T.);
#11058=ORIENTED_EDGE('',*,*,#7550,.T.);
#11059=ORIENTED_EDGE('',*,*,#7562,.T.);
#11060=ORIENTED_EDGE('',*,*,#7527,.F.);
#11061=ORIENTED_EDGE('',*,*,#7529,.F.);
#11062=ORIENTED_EDGE('',*,*,#7563,.F.);
#11063=ORIENTED_EDGE('',*,*,#7564,.F.);
#11064=ORIENTED_EDGE('',*,*,#7565,.T.);
#11065=ORIENTED_EDGE('',*,*,#7519,.F.);
#11066=ORIENTED_EDGE('',*,*,#7566,.T.);
#11067=ORIENTED_EDGE('',*,*,#7564,.T.);
#11068=ORIENTED_EDGE('',*,*,#7553,.F.);
#11069=ORIENTED_EDGE('',*,*,#7557,.F.);
#11070=ORIENTED_EDGE('',*,*,#7524,.F.);
#11071=ORIENTED_EDGE('',*,*,#7567,.T.);
#11072=ORIENTED_EDGE('',*,*,#7568,.T.);
#11073=ORIENTED_EDGE('',*,*,#7569,.F.);
#11074=ORIENTED_EDGE('',*,*,#7530,.F.);
#11075=ORIENTED_EDGE('',*,*,#7521,.F.);
#11076=ORIENTED_EDGE('',*,*,#7570,.F.);
#11077=ORIENTED_EDGE('',*,*,#7571,.F.);
#11078=ORIENTED_EDGE('',*,*,#7572,.T.);
#11079=ORIENTED_EDGE('',*,*,#7512,.F.);
#11080=ORIENTED_EDGE('',*,*,#7573,.T.);
#11081=ORIENTED_EDGE('',*,*,#7571,.T.);
#11082=ORIENTED_EDGE('',*,*,#7574,.F.);
#11083=ORIENTED_EDGE('',*,*,#7568,.F.);
#11084=ORIENTED_EDGE('',*,*,#7517,.F.);
#11085=ORIENTED_EDGE('',*,*,#7575,.T.);
#11086=ORIENTED_EDGE('',*,*,#7576,.T.);
#11087=ORIENTED_EDGE('',*,*,#7577,.F.);
#11088=ORIENTED_EDGE('',*,*,#7522,.F.);
#11089=ORIENTED_EDGE('',*,*,#7514,.F.);
#11090=ORIENTED_EDGE('',*,*,#7578,.F.);
#11091=ORIENTED_EDGE('',*,*,#7579,.F.);
#11092=ORIENTED_EDGE('',*,*,#7580,.T.);
#11093=ORIENTED_EDGE('',*,*,#7505,.F.);
#11094=ORIENTED_EDGE('',*,*,#7581,.T.);
#11095=ORIENTED_EDGE('',*,*,#7579,.T.);
#11096=ORIENTED_EDGE('',*,*,#7582,.F.);
#11097=ORIENTED_EDGE('',*,*,#7576,.F.);
#11098=ORIENTED_EDGE('',*,*,#7510,.F.);
#11099=ORIENTED_EDGE('',*,*,#7583,.T.);
#11100=ORIENTED_EDGE('',*,*,#7584,.T.);
#11101=ORIENTED_EDGE('',*,*,#7585,.F.);
#11102=ORIENTED_EDGE('',*,*,#7515,.F.);
#11103=ORIENTED_EDGE('',*,*,#7507,.F.);
#11104=ORIENTED_EDGE('',*,*,#7586,.F.);
#11105=ORIENTED_EDGE('',*,*,#7587,.F.);
#11106=ORIENTED_EDGE('',*,*,#7588,.T.);
#11107=ORIENTED_EDGE('',*,*,#7498,.F.);
#11108=ORIENTED_EDGE('',*,*,#7589,.T.);
#11109=ORIENTED_EDGE('',*,*,#7587,.T.);
#11110=ORIENTED_EDGE('',*,*,#7590,.F.);
#11111=ORIENTED_EDGE('',*,*,#7584,.F.);
#11112=ORIENTED_EDGE('',*,*,#7503,.F.);
#11113=ORIENTED_EDGE('',*,*,#7591,.T.);
#11114=ORIENTED_EDGE('',*,*,#7592,.T.);
#11115=ORIENTED_EDGE('',*,*,#7593,.F.);
#11116=ORIENTED_EDGE('',*,*,#7508,.F.);
#11117=ORIENTED_EDGE('',*,*,#7500,.F.);
#11118=ORIENTED_EDGE('',*,*,#7594,.F.);
#11119=ORIENTED_EDGE('',*,*,#7595,.F.);
#11120=ORIENTED_EDGE('',*,*,#7596,.T.);
#11121=ORIENTED_EDGE('',*,*,#7492,.F.);
#11122=ORIENTED_EDGE('',*,*,#7597,.T.);
#11123=ORIENTED_EDGE('',*,*,#7595,.T.);
#11124=ORIENTED_EDGE('',*,*,#7598,.F.);
#11125=ORIENTED_EDGE('',*,*,#7592,.F.);
#11126=ORIENTED_EDGE('',*,*,#7535,.T.);
#11127=ORIENTED_EDGE('',*,*,#7599,.F.);
#11128=ORIENTED_EDGE('',*,*,#7544,.F.);
#11129=ORIENTED_EDGE('',*,*,#7549,.T.);
#11130=ORIENTED_EDGE('',*,*,#7554,.F.);
#11131=ORIENTED_EDGE('',*,*,#7563,.T.);
#11132=ORIENTED_EDGE('',*,*,#7528,.F.);
#11133=ORIENTED_EDGE('',*,*,#7562,.F.);
#11134=ORIENTED_EDGE('',*,*,#7531,.F.);
#11135=ORIENTED_EDGE('',*,*,#7569,.T.);
#11136=ORIENTED_EDGE('',*,*,#7600,.T.);
#11137=ORIENTED_EDGE('',*,*,#7556,.F.);
#11138=ORIENTED_EDGE('',*,*,#7520,.F.);
#11139=ORIENTED_EDGE('',*,*,#7565,.F.);
#11140=ORIENTED_EDGE('',*,*,#7601,.F.);
#11141=ORIENTED_EDGE('',*,*,#7570,.T.);
#11142=ORIENTED_EDGE('',*,*,#7574,.T.);
#11143=ORIENTED_EDGE('',*,*,#7601,.T.);
#11144=ORIENTED_EDGE('',*,*,#7566,.F.);
#11145=ORIENTED_EDGE('',*,*,#7600,.F.);
#11146=ORIENTED_EDGE('',*,*,#7523,.F.);
#11147=ORIENTED_EDGE('',*,*,#7577,.T.);
#11148=ORIENTED_EDGE('',*,*,#7602,.T.);
#11149=ORIENTED_EDGE('',*,*,#7567,.F.);
#11150=ORIENTED_EDGE('',*,*,#7513,.F.);
#11151=ORIENTED_EDGE('',*,*,#7572,.F.);
#11152=ORIENTED_EDGE('',*,*,#7603,.F.);
#11153=ORIENTED_EDGE('',*,*,#7578,.T.);
#11154=ORIENTED_EDGE('',*,*,#7582,.T.);
#11155=ORIENTED_EDGE('',*,*,#7603,.T.);
#11156=ORIENTED_EDGE('',*,*,#7573,.F.);
#11157=ORIENTED_EDGE('',*,*,#7602,.F.);
#11158=ORIENTED_EDGE('',*,*,#7516,.F.);
#11159=ORIENTED_EDGE('',*,*,#7585,.T.);
#11160=ORIENTED_EDGE('',*,*,#7604,.T.);
#11161=ORIENTED_EDGE('',*,*,#7575,.F.);
#11162=ORIENTED_EDGE('',*,*,#7506,.F.);
#11163=ORIENTED_EDGE('',*,*,#7580,.F.);
#11164=ORIENTED_EDGE('',*,*,#7605,.F.);
#11165=ORIENTED_EDGE('',*,*,#7586,.T.);
#11166=ORIENTED_EDGE('',*,*,#7590,.T.);
#11167=ORIENTED_EDGE('',*,*,#7605,.T.);
#11168=ORIENTED_EDGE('',*,*,#7581,.F.);
#11169=ORIENTED_EDGE('',*,*,#7604,.F.);
#11170=ORIENTED_EDGE('',*,*,#7509,.F.);
#11171=ORIENTED_EDGE('',*,*,#7593,.T.);
#11172=ORIENTED_EDGE('',*,*,#7606,.T.);
#11173=ORIENTED_EDGE('',*,*,#7583,.F.);
#11174=ORIENTED_EDGE('',*,*,#7499,.F.);
#11175=ORIENTED_EDGE('',*,*,#7588,.F.);
#11176=ORIENTED_EDGE('',*,*,#7607,.F.);
#11177=ORIENTED_EDGE('',*,*,#7594,.T.);
#11178=ORIENTED_EDGE('',*,*,#7598,.T.);
#11179=ORIENTED_EDGE('',*,*,#7607,.T.);
#11180=ORIENTED_EDGE('',*,*,#7589,.F.);
#11181=ORIENTED_EDGE('',*,*,#7606,.F.);
#11182=ORIENTED_EDGE('',*,*,#7502,.F.);
#11183=ORIENTED_EDGE('',*,*,#7543,.T.);
#11184=ORIENTED_EDGE('',*,*,#7608,.T.);
#11185=ORIENTED_EDGE('',*,*,#7591,.F.);
#11186=ORIENTED_EDGE('',*,*,#7539,.T.);
#11187=ORIENTED_EDGE('',*,*,#7493,.F.);
#11188=ORIENTED_EDGE('',*,*,#7596,.F.);
#11189=ORIENTED_EDGE('',*,*,#7609,.F.);
#11190=ORIENTED_EDGE('',*,*,#7599,.T.);
#11191=ORIENTED_EDGE('',*,*,#7545,.T.);
#11192=ORIENTED_EDGE('',*,*,#7609,.T.);
#11193=ORIENTED_EDGE('',*,*,#7597,.F.);
#11194=ORIENTED_EDGE('',*,*,#7608,.F.);
#11195=ORIENTED_EDGE('',*,*,#7558,.T.);
#11196=ORIENTED_EDGE('',*,*,#7610,.T.);
#11197=ORIENTED_EDGE('',*,*,#7611,.T.);
#11198=ORIENTED_EDGE('',*,*,#7612,.T.);
#11199=ORIENTED_EDGE('',*,*,#7613,.T.);
#11200=ORIENTED_EDGE('',*,*,#7611,.F.);
#11201=ORIENTED_EDGE('',*,*,#7613,.F.);
#11202=ORIENTED_EDGE('',*,*,#7614,.T.);
#11203=ORIENTED_EDGE('',*,*,#7615,.T.);
#11204=ORIENTED_EDGE('',*,*,#7614,.F.);
#11205=ORIENTED_EDGE('',*,*,#7612,.F.);
#11206=ORIENTED_EDGE('',*,*,#7610,.F.);
#11207=ORIENTED_EDGE('',*,*,#7616,.T.);
#11208=ORIENTED_EDGE('',*,*,#7617,.T.);
#11209=ORIENTED_EDGE('',*,*,#7618,.T.);
#11210=ORIENTED_EDGE('',*,*,#7619,.T.);
#11211=ORIENTED_EDGE('',*,*,#7620,.T.);
#11212=ORIENTED_EDGE('',*,*,#7616,.F.);
#11213=ORIENTED_EDGE('',*,*,#7621,.T.);
#11214=ORIENTED_EDGE('',*,*,#7622,.F.);
#11215=ORIENTED_EDGE('',*,*,#7621,.F.);
#11216=ORIENTED_EDGE('',*,*,#7617,.F.);
#11217=ORIENTED_EDGE('',*,*,#7623,.T.);
#11218=ORIENTED_EDGE('',*,*,#7624,.F.);
#11219=ORIENTED_EDGE('',*,*,#7623,.F.);
#11220=ORIENTED_EDGE('',*,*,#7618,.F.);
#11221=ORIENTED_EDGE('',*,*,#7625,.T.);
#11222=ORIENTED_EDGE('',*,*,#7626,.F.);
#11223=ORIENTED_EDGE('',*,*,#7625,.F.);
#11224=ORIENTED_EDGE('',*,*,#7619,.F.);
#11225=ORIENTED_EDGE('',*,*,#7627,.T.);
#11226=ORIENTED_EDGE('',*,*,#7628,.F.);
#11227=ORIENTED_EDGE('',*,*,#7627,.F.);
#11228=ORIENTED_EDGE('',*,*,#7629,.T.);
#11229=ORIENTED_EDGE('',*,*,#7630,.T.);
#11230=ORIENTED_EDGE('',*,*,#7620,.F.);
#11231=ORIENTED_EDGE('',*,*,#7630,.F.);
#11232=ORIENTED_EDGE('',*,*,#7615,.F.);
#11233=ORIENTED_EDGE('',*,*,#7629,.F.);
#11234=ORIENTED_EDGE('',*,*,#7628,.T.);
#11235=ORIENTED_EDGE('',*,*,#7626,.T.);
#11236=ORIENTED_EDGE('',*,*,#7624,.T.);
#11237=ORIENTED_EDGE('',*,*,#7622,.T.);
#11238=ORIENTED_EDGE('',*,*,#7631,.F.);
#11239=ORIENTED_EDGE('',*,*,#7632,.T.);
#11240=ORIENTED_EDGE('',*,*,#7633,.T.);
#11241=ORIENTED_EDGE('',*,*,#7632,.F.);
#11242=ORIENTED_EDGE('',*,*,#7633,.F.);
#11243=ORIENTED_EDGE('',*,*,#7634,.F.);
#11244=ORIENTED_EDGE('',*,*,#7635,.T.);
#11245=ORIENTED_EDGE('',*,*,#7636,.T.);
#11246=ORIENTED_EDGE('',*,*,#7635,.F.);
#11247=ORIENTED_EDGE('',*,*,#7636,.F.);
#11248=ORIENTED_EDGE('',*,*,#7637,.F.);
#11249=ORIENTED_EDGE('',*,*,#7638,.T.);
#11250=ORIENTED_EDGE('',*,*,#7639,.T.);
#11251=ORIENTED_EDGE('',*,*,#7638,.F.);
#11252=ORIENTED_EDGE('',*,*,#7639,.F.);
#11253=ORIENTED_EDGE('',*,*,#7640,.F.);
#11254=ORIENTED_EDGE('',*,*,#7641,.T.);
#11255=ORIENTED_EDGE('',*,*,#7642,.T.);
#11256=ORIENTED_EDGE('',*,*,#7641,.F.);
#11257=ORIENTED_EDGE('',*,*,#7642,.F.);
#11258=ORIENTED_EDGE('',*,*,#7643,.F.);
#11259=ORIENTED_EDGE('',*,*,#7644,.T.);
#11260=ORIENTED_EDGE('',*,*,#7645,.F.);
#11261=ORIENTED_EDGE('',*,*,#7644,.F.);
#11262=ORIENTED_EDGE('',*,*,#7646,.F.);
#11263=ORIENTED_EDGE('',*,*,#7647,.T.);
#11264=ORIENTED_EDGE('',*,*,#7648,.T.);
#11265=ORIENTED_EDGE('',*,*,#7647,.F.);
#11266=ORIENTED_EDGE('',*,*,#7648,.F.);
#11267=ORIENTED_EDGE('',*,*,#7649,.F.);
#11268=ORIENTED_EDGE('',*,*,#7650,.T.);
#11269=ORIENTED_EDGE('',*,*,#7651,.T.);
#11270=ORIENTED_EDGE('',*,*,#7650,.F.);
#11271=ORIENTED_EDGE('',*,*,#7651,.F.);
#11272=ORIENTED_EDGE('',*,*,#7652,.F.);
#11273=ORIENTED_EDGE('',*,*,#7653,.T.);
#11274=ORIENTED_EDGE('',*,*,#7654,.T.);
#11275=ORIENTED_EDGE('',*,*,#7653,.F.);
#11276=ORIENTED_EDGE('',*,*,#7654,.F.);
#11277=ORIENTED_EDGE('',*,*,#7655,.F.);
#11278=ORIENTED_EDGE('',*,*,#7656,.T.);
#11279=ORIENTED_EDGE('',*,*,#7657,.F.);
#11280=ORIENTED_EDGE('',*,*,#7656,.F.);
#11281=ORIENTED_EDGE('',*,*,#7658,.F.);
#11282=ORIENTED_EDGE('',*,*,#7659,.T.);
#11283=ORIENTED_EDGE('',*,*,#7660,.F.);
#11284=ORIENTED_EDGE('',*,*,#7659,.F.);
#11285=ORIENTED_EDGE('',*,*,#7661,.F.);
#11286=ORIENTED_EDGE('',*,*,#7662,.T.);
#11287=ORIENTED_EDGE('',*,*,#7663,.F.);
#11288=ORIENTED_EDGE('',*,*,#7662,.F.);
#11289=ORIENTED_EDGE('',*,*,#7664,.F.);
#11290=ORIENTED_EDGE('',*,*,#7665,.T.);
#11291=ORIENTED_EDGE('',*,*,#7666,.F.);
#11292=ORIENTED_EDGE('',*,*,#7665,.F.);
#11293=ORIENTED_EDGE('',*,*,#7667,.T.);
#11294=ORIENTED_EDGE('',*,*,#7668,.T.);
#11295=ORIENTED_EDGE('',*,*,#7669,.T.);
#11296=ORIENTED_EDGE('',*,*,#7670,.T.);
#11297=ORIENTED_EDGE('',*,*,#7669,.F.);
#11298=ORIENTED_EDGE('',*,*,#7671,.T.);
#11299=ORIENTED_EDGE('',*,*,#7672,.F.);
#11300=ORIENTED_EDGE('',*,*,#7673,.T.);
#11301=ORIENTED_EDGE('',*,*,#7674,.F.);
#11302=ORIENTED_EDGE('',*,*,#7675,.T.);
#11303=ORIENTED_EDGE('',*,*,#7676,.T.);
#11304=ORIENTED_EDGE('',*,*,#7677,.T.);
#11305=ORIENTED_EDGE('',*,*,#7678,.T.);
#11306=ORIENTED_EDGE('',*,*,#7679,.T.);
#11307=ORIENTED_EDGE('',*,*,#7680,.T.);
#11308=ORIENTED_EDGE('',*,*,#7681,.T.);
#11309=ORIENTED_EDGE('',*,*,#7682,.T.);
#11310=ORIENTED_EDGE('',*,*,#7683,.T.);
#11311=ORIENTED_EDGE('',*,*,#7684,.T.);
#11312=ORIENTED_EDGE('',*,*,#7685,.T.);
#11313=ORIENTED_EDGE('',*,*,#7686,.T.);
#11314=ORIENTED_EDGE('',*,*,#7687,.F.);
#11315=ORIENTED_EDGE('',*,*,#7688,.F.);
#11316=ORIENTED_EDGE('',*,*,#7655,.T.);
#11317=ORIENTED_EDGE('',*,*,#7658,.T.);
#11318=ORIENTED_EDGE('',*,*,#7661,.T.);
#11319=ORIENTED_EDGE('',*,*,#7664,.T.);
#11320=ORIENTED_EDGE('',*,*,#7668,.F.);
#11321=ORIENTED_EDGE('',*,*,#7689,.F.);
#11322=ORIENTED_EDGE('',*,*,#7690,.F.);
#11323=ORIENTED_EDGE('',*,*,#7671,.F.);
#11324=ORIENTED_EDGE('',*,*,#7691,.T.);
#11325=ORIENTED_EDGE('',*,*,#7692,.T.);
#11326=ORIENTED_EDGE('',*,*,#7672,.T.);
#11327=ORIENTED_EDGE('',*,*,#7690,.T.);
#11328=ORIENTED_EDGE('',*,*,#7693,.T.);
#11329=ORIENTED_EDGE('',*,*,#7694,.T.);
#11330=ORIENTED_EDGE('',*,*,#7687,.T.);
#11331=ORIENTED_EDGE('',*,*,#7695,.T.);
#11332=ORIENTED_EDGE('',*,*,#7695,.F.);
#11333=ORIENTED_EDGE('',*,*,#7686,.F.);
#11334=ORIENTED_EDGE('',*,*,#7696,.F.);
#11335=ORIENTED_EDGE('',*,*,#7675,.F.);
#11336=ORIENTED_EDGE('',*,*,#7697,.F.);
#11337=ORIENTED_EDGE('',*,*,#7698,.F.);
#11338=ORIENTED_EDGE('',*,*,#7699,.T.);
#11339=ORIENTED_EDGE('',*,*,#7697,.T.);
#11340=ORIENTED_EDGE('',*,*,#7674,.T.);
#11341=ORIENTED_EDGE('',*,*,#7700,.T.);
#11342=ORIENTED_EDGE('',*,*,#7692,.F.);
#11343=ORIENTED_EDGE('',*,*,#7701,.F.);
#11344=ORIENTED_EDGE('',*,*,#7700,.F.);
#11345=ORIENTED_EDGE('',*,*,#7673,.F.);
#11346=ORIENTED_EDGE('',*,*,#7685,.F.);
#11347=ORIENTED_EDGE('',*,*,#7702,.F.);
#11348=ORIENTED_EDGE('',*,*,#7703,.F.);
#11349=ORIENTED_EDGE('',*,*,#7704,.T.);
#11350=ORIENTED_EDGE('',*,*,#7705,.F.);
#11351=ORIENTED_EDGE('',*,*,#7706,.F.);
#11352=ORIENTED_EDGE('',*,*,#7696,.T.);
#11353=ORIENTED_EDGE('',*,*,#7704,.F.);
#11354=ORIENTED_EDGE('',*,*,#7676,.F.);
#11355=ORIENTED_EDGE('',*,*,#7706,.T.);
#11356=ORIENTED_EDGE('',*,*,#7707,.F.);
#11357=ORIENTED_EDGE('',*,*,#7708,.F.);
#11358=ORIENTED_EDGE('',*,*,#7707,.T.);
#11359=ORIENTED_EDGE('',*,*,#7705,.T.);
#11360=ORIENTED_EDGE('',*,*,#7703,.T.);
#11361=ORIENTED_EDGE('',*,*,#7709,.T.);
#11362=ORIENTED_EDGE('',*,*,#7710,.F.);
#11363=ORIENTED_EDGE('',*,*,#7711,.T.);
#11364=ORIENTED_EDGE('',*,*,#7712,.F.);
#11365=ORIENTED_EDGE('',*,*,#7713,.T.);
#11366=ORIENTED_EDGE('',*,*,#7714,.T.);
#11367=ORIENTED_EDGE('',*,*,#7715,.T.);
#11368=ORIENTED_EDGE('',*,*,#7709,.F.);
#11369=ORIENTED_EDGE('',*,*,#7702,.T.);
#11370=ORIENTED_EDGE('',*,*,#7684,.F.);
#11371=ORIENTED_EDGE('',*,*,#7716,.F.);
#11372=ORIENTED_EDGE('',*,*,#7713,.F.);
#11373=ORIENTED_EDGE('',*,*,#7717,.F.);
#11374=ORIENTED_EDGE('',*,*,#7679,.F.);
#11375=ORIENTED_EDGE('',*,*,#7718,.F.);
#11376=ORIENTED_EDGE('',*,*,#7719,.F.);
#11377=ORIENTED_EDGE('',*,*,#7682,.F.);
#11378=ORIENTED_EDGE('',*,*,#7720,.F.);
#11379=ORIENTED_EDGE('',*,*,#7711,.F.);
#11380=ORIENTED_EDGE('',*,*,#7721,.T.);
#11381=ORIENTED_EDGE('',*,*,#7716,.T.);
#11382=ORIENTED_EDGE('',*,*,#7683,.F.);
#11383=ORIENTED_EDGE('',*,*,#7719,.T.);
#11384=ORIENTED_EDGE('',*,*,#7722,.F.);
#11385=ORIENTED_EDGE('',*,*,#7723,.F.);
#11386=ORIENTED_EDGE('',*,*,#7677,.F.);
#11387=ORIENTED_EDGE('',*,*,#7708,.T.);
#11388=ORIENTED_EDGE('',*,*,#7715,.F.);
#11389=ORIENTED_EDGE('',*,*,#7724,.T.);
#11390=ORIENTED_EDGE('',*,*,#7718,.T.);
#11391=ORIENTED_EDGE('',*,*,#7678,.F.);
#11392=ORIENTED_EDGE('',*,*,#7723,.T.);
#11393=ORIENTED_EDGE('',*,*,#7710,.T.);
#11394=ORIENTED_EDGE('',*,*,#7721,.F.);
#11395=ORIENTED_EDGE('',*,*,#7722,.T.);
#11396=ORIENTED_EDGE('',*,*,#7725,.T.);
#11397=ORIENTED_EDGE('',*,*,#7670,.F.);
#11398=ORIENTED_EDGE('',*,*,#7688,.T.);
#11399=ORIENTED_EDGE('',*,*,#7694,.F.);
#11400=ORIENTED_EDGE('',*,*,#7726,.T.);
#11401=ORIENTED_EDGE('',*,*,#7725,.F.);
#11402=ORIENTED_EDGE('',*,*,#7727,.T.);
#11403=ORIENTED_EDGE('',*,*,#7728,.F.);
#11404=ORIENTED_EDGE('',*,*,#7729,.F.);
#11405=ORIENTED_EDGE('',*,*,#7730,.T.);
#11406=ORIENTED_EDGE('',*,*,#7731,.T.);
#11407=ORIENTED_EDGE('',*,*,#7730,.F.);
#11408=ORIENTED_EDGE('',*,*,#7732,.F.);
#11409=ORIENTED_EDGE('',*,*,#7727,.F.);
#11410=ORIENTED_EDGE('',*,*,#7733,.F.);
#11411=ORIENTED_EDGE('',*,*,#7643,.T.);
#11412=ORIENTED_EDGE('',*,*,#7733,.T.);
#11413=ORIENTED_EDGE('',*,*,#7734,.T.);
#11414=ORIENTED_EDGE('',*,*,#7735,.F.);
#11415=ORIENTED_EDGE('',*,*,#7734,.F.);
#11416=ORIENTED_EDGE('',*,*,#7728,.T.);
#11417=ORIENTED_EDGE('',*,*,#7732,.T.);
#11418=ORIENTED_EDGE('',*,*,#7729,.T.);
#11419=ORIENTED_EDGE('',*,*,#7736,.F.);
#11420=ORIENTED_EDGE('',*,*,#7735,.T.);
#11421=ORIENTED_EDGE('',*,*,#7640,.T.);
#11422=ORIENTED_EDGE('',*,*,#7637,.T.);
#11423=ORIENTED_EDGE('',*,*,#7634,.T.);
#11424=ORIENTED_EDGE('',*,*,#7631,.T.);
#11425=ORIENTED_EDGE('',*,*,#7736,.T.);
#11426=ORIENTED_EDGE('',*,*,#7737,.T.);
#11427=ORIENTED_EDGE('',*,*,#7680,.F.);
#11428=ORIENTED_EDGE('',*,*,#7717,.T.);
#11429=ORIENTED_EDGE('',*,*,#7712,.T.);
#11430=ORIENTED_EDGE('',*,*,#7720,.T.);
#11431=ORIENTED_EDGE('',*,*,#7681,.F.);
#11432=ORIENTED_EDGE('',*,*,#7737,.F.);
#11433=ORIENTED_EDGE('',*,*,#7714,.F.);
#11434=ORIENTED_EDGE('',*,*,#7724,.F.);
#11435=ORIENTED_EDGE('',*,*,#7646,.T.);
#11436=ORIENTED_EDGE('',*,*,#7649,.T.);
#11437=ORIENTED_EDGE('',*,*,#7652,.T.);
#11438=ORIENTED_EDGE('',*,*,#7731,.F.);
#11439=ORIENTED_EDGE('',*,*,#7667,.F.);
#11440=ORIENTED_EDGE('',*,*,#7726,.F.);
#11441=ORIENTED_EDGE('',*,*,#7693,.F.);
#11442=ORIENTED_EDGE('',*,*,#7698,.T.);
#11443=ORIENTED_EDGE('',*,*,#7699,.F.);
#11444=ORIENTED_EDGE('',*,*,#7701,.T.);
#11445=ORIENTED_EDGE('',*,*,#7691,.F.);
#11446=ORIENTED_EDGE('',*,*,#7689,.T.);
#11447=ORIENTED_EDGE('',*,*,#7645,.T.);
#11448=ORIENTED_EDGE('',*,*,#7657,.T.);
#11449=ORIENTED_EDGE('',*,*,#7660,.T.);
#11450=ORIENTED_EDGE('',*,*,#7663,.T.);
#11451=ORIENTED_EDGE('',*,*,#7666,.T.);
#11452=ORIENTED_EDGE('',*,*,#7738,.T.);
#11453=ORIENTED_EDGE('',*,*,#7739,.T.);
#11454=ORIENTED_EDGE('',*,*,#7740,.T.);
#11455=ORIENTED_EDGE('',*,*,#7739,.F.);
#11456=ORIENTED_EDGE('',*,*,#7741,.T.);
#11457=ORIENTED_EDGE('',*,*,#7742,.T.);
#11458=ORIENTED_EDGE('',*,*,#7743,.T.);
#11459=ORIENTED_EDGE('',*,*,#7742,.F.);
#11460=ORIENTED_EDGE('',*,*,#7744,.T.);
#11461=ORIENTED_EDGE('',*,*,#7745,.T.);
#11462=ORIENTED_EDGE('',*,*,#7746,.T.);
#11463=ORIENTED_EDGE('',*,*,#7745,.F.);
#11464=ORIENTED_EDGE('',*,*,#7747,.F.);
#11465=ORIENTED_EDGE('',*,*,#7748,.T.);
#11466=ORIENTED_EDGE('',*,*,#7749,.F.);
#11467=ORIENTED_EDGE('',*,*,#7750,.F.);
#11468=ORIENTED_EDGE('',*,*,#7748,.F.);
#11469=ORIENTED_EDGE('',*,*,#7751,.F.);
#11470=ORIENTED_EDGE('',*,*,#7752,.T.);
#11471=ORIENTED_EDGE('',*,*,#7749,.T.);
#11472=ORIENTED_EDGE('',*,*,#7750,.T.);
#11473=ORIENTED_EDGE('',*,*,#7752,.F.);
#11474=ORIENTED_EDGE('',*,*,#7747,.T.);
#11475=ORIENTED_EDGE('',*,*,#7740,.F.);
#11476=ORIENTED_EDGE('',*,*,#7743,.F.);
#11477=ORIENTED_EDGE('',*,*,#7746,.F.);
#11478=ORIENTED_EDGE('',*,*,#7753,.F.);
#11479=ORIENTED_EDGE('',*,*,#7753,.T.);
#11480=ORIENTED_EDGE('',*,*,#7754,.T.);
#11481=ORIENTED_EDGE('',*,*,#7755,.F.);
#11482=ORIENTED_EDGE('',*,*,#7754,.F.);
#11483=ORIENTED_EDGE('',*,*,#7751,.T.);
#11484=ORIENTED_EDGE('',*,*,#7738,.F.);
#11485=ORIENTED_EDGE('',*,*,#7741,.F.);
#11486=ORIENTED_EDGE('',*,*,#7744,.F.);
#11487=ORIENTED_EDGE('',*,*,#7755,.T.);
#11488=ORIENTED_EDGE('',*,*,#7756,.F.);
#11489=ORIENTED_EDGE('',*,*,#7757,.T.);
#11490=ORIENTED_EDGE('',*,*,#7758,.T.);
#11491=ORIENTED_EDGE('',*,*,#7757,.F.);
#11492=ORIENTED_EDGE('',*,*,#7759,.T.);
#11493=ORIENTED_EDGE('',*,*,#7760,.T.);
#11494=ORIENTED_EDGE('',*,*,#7761,.F.);
#11495=ORIENTED_EDGE('',*,*,#7762,.F.);
#11496=ORIENTED_EDGE('',*,*,#7760,.F.);
#11497=ORIENTED_EDGE('',*,*,#7763,.T.);
#11498=ORIENTED_EDGE('',*,*,#7759,.F.);
#11499=ORIENTED_EDGE('',*,*,#7764,.T.);
#11500=ORIENTED_EDGE('',*,*,#7765,.T.);
#11501=ORIENTED_EDGE('',*,*,#7764,.F.);
#11502=ORIENTED_EDGE('',*,*,#7763,.F.);
#11503=ORIENTED_EDGE('',*,*,#7765,.F.);
#11504=ORIENTED_EDGE('',*,*,#7766,.T.);
#11505=ORIENTED_EDGE('',*,*,#7767,.T.);
#11506=ORIENTED_EDGE('',*,*,#7766,.F.);
#11507=ORIENTED_EDGE('',*,*,#7767,.F.);
#11508=ORIENTED_EDGE('',*,*,#7768,.T.);
#11509=ORIENTED_EDGE('',*,*,#7769,.T.);
#11510=ORIENTED_EDGE('',*,*,#7768,.F.);
#11511=ORIENTED_EDGE('',*,*,#7770,.F.);
#11512=ORIENTED_EDGE('',*,*,#7771,.T.);
#11513=ORIENTED_EDGE('',*,*,#7772,.T.);
#11514=ORIENTED_EDGE('',*,*,#7771,.F.);
#11515=ORIENTED_EDGE('',*,*,#7772,.F.);
#11516=ORIENTED_EDGE('',*,*,#7773,.T.);
#11517=ORIENTED_EDGE('',*,*,#7756,.T.);
#11518=ORIENTED_EDGE('',*,*,#7773,.F.);
#11519=ORIENTED_EDGE('',*,*,#7758,.F.);
#11520=ORIENTED_EDGE('',*,*,#7774,.T.);
#11521=ORIENTED_EDGE('',*,*,#7775,.T.);
#11522=ORIENTED_EDGE('',*,*,#7774,.F.);
#11523=ORIENTED_EDGE('',*,*,#7775,.F.);
#11524=ORIENTED_EDGE('',*,*,#7776,.T.);
#11525=ORIENTED_EDGE('',*,*,#7777,.T.);
#11526=ORIENTED_EDGE('',*,*,#7776,.F.);
#11527=ORIENTED_EDGE('',*,*,#7778,.F.);
#11528=ORIENTED_EDGE('',*,*,#7779,.T.);
#11529=ORIENTED_EDGE('',*,*,#7761,.T.);
#11530=ORIENTED_EDGE('',*,*,#7762,.T.);
#11531=ORIENTED_EDGE('',*,*,#7779,.F.);
#11532=ORIENTED_EDGE('',*,*,#7777,.F.);
#11533=ORIENTED_EDGE('',*,*,#7778,.T.);
#11534=ORIENTED_EDGE('',*,*,#7770,.T.);
#11535=ORIENTED_EDGE('',*,*,#7769,.F.);
#11536=ORIENTED_EDGE('',*,*,#7780,.T.);
#11537=ORIENTED_EDGE('',*,*,#7780,.F.);
#11538=ORIENTED_EDGE('',*,*,#7781,.F.);
#11539=ORIENTED_EDGE('',*,*,#7782,.T.);
#11540=ORIENTED_EDGE('',*,*,#7783,.T.);
#11541=ORIENTED_EDGE('',*,*,#7782,.F.);
#11542=ORIENTED_EDGE('',*,*,#7783,.F.);
#11543=ORIENTED_EDGE('',*,*,#7784,.T.);
#11544=ORIENTED_EDGE('',*,*,#7785,.T.);
#11545=ORIENTED_EDGE('',*,*,#7784,.F.);
#11546=ORIENTED_EDGE('',*,*,#7786,.T.);
#11547=ORIENTED_EDGE('',*,*,#7787,.T.);
#11548=ORIENTED_EDGE('',*,*,#7788,.F.);
#11549=ORIENTED_EDGE('',*,*,#7787,.F.);
#11550=ORIENTED_EDGE('',*,*,#7789,.T.);
#11551=ORIENTED_EDGE('',*,*,#7786,.F.);
#11552=ORIENTED_EDGE('',*,*,#7790,.T.);
#11553=ORIENTED_EDGE('',*,*,#7791,.T.);
#11554=ORIENTED_EDGE('',*,*,#7790,.F.);
#11555=ORIENTED_EDGE('',*,*,#7789,.F.);
#11556=ORIENTED_EDGE('',*,*,#7791,.F.);
#11557=ORIENTED_EDGE('',*,*,#7781,.T.);
#11558=ORIENTED_EDGE('',*,*,#7788,.T.);
#11559=ORIENTED_EDGE('',*,*,#7785,.F.);
#11560=ORIENTED_EDGE('',*,*,#7792,.F.);
#11561=ORIENTED_EDGE('',*,*,#7793,.T.);
#11562=ORIENTED_EDGE('',*,*,#7794,.T.);
#11563=ORIENTED_EDGE('',*,*,#7793,.F.);
#11564=ORIENTED_EDGE('',*,*,#7795,.F.);
#11565=ORIENTED_EDGE('',*,*,#7796,.T.);
#11566=ORIENTED_EDGE('',*,*,#7797,.T.);
#11567=ORIENTED_EDGE('',*,*,#7796,.F.);
#11568=ORIENTED_EDGE('',*,*,#7798,.F.);
#11569=ORIENTED_EDGE('',*,*,#7799,.T.);
#11570=ORIENTED_EDGE('',*,*,#7795,.T.);
#11571=ORIENTED_EDGE('',*,*,#7799,.F.);
#11572=ORIENTED_EDGE('',*,*,#7794,.F.);
#11573=ORIENTED_EDGE('',*,*,#7800,.T.);
#11574=ORIENTED_EDGE('',*,*,#7801,.T.);
#11575=ORIENTED_EDGE('',*,*,#7800,.F.);
#11576=ORIENTED_EDGE('',*,*,#7801,.F.);
#11577=ORIENTED_EDGE('',*,*,#7798,.T.);
#11578=ORIENTED_EDGE('',*,*,#7792,.T.);
#11579=ORIENTED_EDGE('',*,*,#7797,.F.);
#11580=ORIENTED_EDGE('',*,*,#7802,.F.);
#11581=ORIENTED_EDGE('',*,*,#7803,.T.);
#11582=ORIENTED_EDGE('',*,*,#7804,.T.);
#11583=ORIENTED_EDGE('',*,*,#7803,.F.);
#11584=ORIENTED_EDGE('',*,*,#7804,.F.);
#11585=ORIENTED_EDGE('',*,*,#7805,.T.);
#11586=ORIENTED_EDGE('',*,*,#7806,.T.);
#11587=ORIENTED_EDGE('',*,*,#7805,.F.);
#11588=ORIENTED_EDGE('',*,*,#7807,.T.);
#11589=ORIENTED_EDGE('',*,*,#7808,.T.);
#11590=ORIENTED_EDGE('',*,*,#7809,.F.);
#11591=ORIENTED_EDGE('',*,*,#7808,.F.);
#11592=ORIENTED_EDGE('',*,*,#7810,.T.);
#11593=ORIENTED_EDGE('',*,*,#7807,.F.);
#11594=ORIENTED_EDGE('',*,*,#7811,.T.);
#11595=ORIENTED_EDGE('',*,*,#7812,.T.);
#11596=ORIENTED_EDGE('',*,*,#7811,.F.);
#11597=ORIENTED_EDGE('',*,*,#7810,.F.);
#11598=ORIENTED_EDGE('',*,*,#7812,.F.);
#11599=ORIENTED_EDGE('',*,*,#7813,.T.);
#11600=ORIENTED_EDGE('',*,*,#7814,.T.);
#11601=ORIENTED_EDGE('',*,*,#7813,.F.);
#11602=ORIENTED_EDGE('',*,*,#7815,.T.);
#11603=ORIENTED_EDGE('',*,*,#7816,.T.);
#11604=ORIENTED_EDGE('',*,*,#7817,.F.);
#11605=ORIENTED_EDGE('',*,*,#7816,.F.);
#11606=ORIENTED_EDGE('',*,*,#7818,.T.);
#11607=ORIENTED_EDGE('',*,*,#7819,.T.);
#11608=ORIENTED_EDGE('',*,*,#7815,.F.);
#11609=ORIENTED_EDGE('',*,*,#7819,.F.);
#11610=ORIENTED_EDGE('',*,*,#7820,.T.);
#11611=ORIENTED_EDGE('',*,*,#7818,.F.);
#11612=ORIENTED_EDGE('',*,*,#7821,.T.);
#11613=ORIENTED_EDGE('',*,*,#7822,.T.);
#11614=ORIENTED_EDGE('',*,*,#7821,.F.);
#11615=ORIENTED_EDGE('',*,*,#7820,.F.);
#11616=ORIENTED_EDGE('',*,*,#7822,.F.);
#11617=ORIENTED_EDGE('',*,*,#7823,.T.);
#11618=ORIENTED_EDGE('',*,*,#7824,.T.);
#11619=ORIENTED_EDGE('',*,*,#7823,.F.);
#11620=ORIENTED_EDGE('',*,*,#7824,.F.);
#11621=ORIENTED_EDGE('',*,*,#7825,.T.);
#11622=ORIENTED_EDGE('',*,*,#7802,.T.);
#11623=ORIENTED_EDGE('',*,*,#7825,.F.);
#11624=ORIENTED_EDGE('',*,*,#7814,.F.);
#11625=ORIENTED_EDGE('',*,*,#7817,.T.);
#11626=ORIENTED_EDGE('',*,*,#7809,.T.);
#11627=ORIENTED_EDGE('',*,*,#7806,.F.);
#11628=ORIENTED_EDGE('',*,*,#7826,.T.);
#11629=ORIENTED_EDGE('',*,*,#7826,.F.);
#11630=ORIENTED_EDGE('',*,*,#7827,.T.);
#11631=ORIENTED_EDGE('',*,*,#7827,.F.);
#11632=ORIENTED_EDGE('',*,*,#7828,.T.);
#11633=ORIENTED_EDGE('',*,*,#7828,.F.);
#11634=ORIENTED_EDGE('',*,*,#7829,.T.);
#11635=ORIENTED_EDGE('',*,*,#7829,.F.);
#11636=ORIENTED_EDGE('',*,*,#7830,.T.);
#11637=ORIENTED_EDGE('',*,*,#7830,.F.);
#11638=ORIENTED_EDGE('',*,*,#7831,.T.);
#11639=ORIENTED_EDGE('',*,*,#7831,.F.);
#11640=ORIENTED_EDGE('',*,*,#7832,.T.);
#11641=ORIENTED_EDGE('',*,*,#7832,.F.);
#11642=ORIENTED_EDGE('',*,*,#7833,.T.);
#11643=ORIENTED_EDGE('',*,*,#7833,.F.);
#11644=ORIENTED_EDGE('',*,*,#7834,.F.);
#11645=ORIENTED_EDGE('',*,*,#7835,.T.);
#11646=ORIENTED_EDGE('',*,*,#7836,.T.);
#11647=ORIENTED_EDGE('',*,*,#7835,.F.);
#11648=ORIENTED_EDGE('',*,*,#7836,.F.);
#11649=ORIENTED_EDGE('',*,*,#7837,.T.);
#11650=ORIENTED_EDGE('',*,*,#7838,.T.);
#11651=ORIENTED_EDGE('',*,*,#7837,.F.);
#11652=ORIENTED_EDGE('',*,*,#7838,.F.);
#11653=ORIENTED_EDGE('',*,*,#7839,.T.);
#11654=ORIENTED_EDGE('',*,*,#7840,.T.);
#11655=ORIENTED_EDGE('',*,*,#7839,.F.);
#11656=ORIENTED_EDGE('',*,*,#7840,.F.);
#11657=ORIENTED_EDGE('',*,*,#7841,.T.);
#11658=ORIENTED_EDGE('',*,*,#7842,.T.);
#11659=ORIENTED_EDGE('',*,*,#7843,.T.);
#11660=ORIENTED_EDGE('',*,*,#7841,.F.);
#11661=ORIENTED_EDGE('',*,*,#7844,.T.);
#11662=ORIENTED_EDGE('',*,*,#7845,.T.);
#11663=ORIENTED_EDGE('',*,*,#7842,.F.);
#11664=ORIENTED_EDGE('',*,*,#7843,.F.);
#11665=ORIENTED_EDGE('',*,*,#7845,.F.);
#11666=ORIENTED_EDGE('',*,*,#7846,.T.);
#11667=ORIENTED_EDGE('',*,*,#7844,.F.);
#11668=ORIENTED_EDGE('',*,*,#7847,.T.);
#11669=ORIENTED_EDGE('',*,*,#7848,.T.);
#11670=ORIENTED_EDGE('',*,*,#7847,.F.);
#11671=ORIENTED_EDGE('',*,*,#7846,.F.);
#11672=ORIENTED_EDGE('',*,*,#7848,.F.);
#11673=ORIENTED_EDGE('',*,*,#7834,.T.);
#11674=ORIENTED_EDGE('',*,*,#7849,.F.);
#11675=ORIENTED_EDGE('',*,*,#7850,.F.);
#11676=ORIENTED_EDGE('',*,*,#7851,.T.);
#11677=ORIENTED_EDGE('',*,*,#7852,.F.);
#11678=ORIENTED_EDGE('',*,*,#7851,.F.);
#11679=ORIENTED_EDGE('',*,*,#7853,.F.);
#11680=ORIENTED_EDGE('',*,*,#7854,.T.);
#11681=ORIENTED_EDGE('',*,*,#7855,.F.);
#11682=ORIENTED_EDGE('',*,*,#7854,.F.);
#11683=ORIENTED_EDGE('',*,*,#7856,.T.);
#11684=ORIENTED_EDGE('',*,*,#7857,.T.);
#11685=ORIENTED_EDGE('',*,*,#7858,.F.);
#11686=ORIENTED_EDGE('',*,*,#7857,.F.);
#11687=ORIENTED_EDGE('',*,*,#7849,.T.);
#11688=ORIENTED_EDGE('',*,*,#7850,.T.);
#11689=ORIENTED_EDGE('',*,*,#7859,.T.);
#11690=ORIENTED_EDGE('',*,*,#7853,.T.);
#11691=ORIENTED_EDGE('',*,*,#7859,.F.);
#11692=ORIENTED_EDGE('',*,*,#7852,.T.);
#11693=ORIENTED_EDGE('',*,*,#7856,.F.);
#11694=ORIENTED_EDGE('',*,*,#7855,.T.);
#11695=ORIENTED_EDGE('',*,*,#7858,.T.);
#11696=ORIENTED_EDGE('',*,*,#7860,.F.);
#11697=ORIENTED_EDGE('',*,*,#7861,.F.);
#11698=ORIENTED_EDGE('',*,*,#7862,.T.);
#11699=ORIENTED_EDGE('',*,*,#7863,.T.);
#11700=ORIENTED_EDGE('',*,*,#7864,.T.);
#11701=ORIENTED_EDGE('',*,*,#7862,.F.);
#11702=ORIENTED_EDGE('',*,*,#7865,.F.);
#11703=ORIENTED_EDGE('',*,*,#7866,.F.);
#11704=ORIENTED_EDGE('',*,*,#7867,.T.);
#11705=ORIENTED_EDGE('',*,*,#7868,.T.);
#11706=ORIENTED_EDGE('',*,*,#7869,.T.);
#11707=ORIENTED_EDGE('',*,*,#7867,.F.);
#11708=ORIENTED_EDGE('',*,*,#7870,.F.);
#11709=ORIENTED_EDGE('',*,*,#7871,.T.);
#11710=ORIENTED_EDGE('',*,*,#7872,.T.);
#11711=ORIENTED_EDGE('',*,*,#7873,.T.);
#11712=ORIENTED_EDGE('',*,*,#7871,.F.);
#11713=ORIENTED_EDGE('',*,*,#7874,.F.);
#11714=ORIENTED_EDGE('',*,*,#7875,.F.);
#11715=ORIENTED_EDGE('',*,*,#7876,.T.);
#11716=ORIENTED_EDGE('',*,*,#7870,.T.);
#11717=ORIENTED_EDGE('',*,*,#7876,.F.);
#11718=ORIENTED_EDGE('',*,*,#7874,.T.);
#11719=ORIENTED_EDGE('',*,*,#7875,.T.);
#11720=ORIENTED_EDGE('',*,*,#7877,.T.);
#11721=ORIENTED_EDGE('',*,*,#7863,.F.);
#11722=ORIENTED_EDGE('',*,*,#7864,.F.);
#11723=ORIENTED_EDGE('',*,*,#7877,.F.);
#11724=ORIENTED_EDGE('',*,*,#7860,.T.);
#11725=ORIENTED_EDGE('',*,*,#7861,.T.);
#11726=ORIENTED_EDGE('',*,*,#7878,.T.);
#11727=ORIENTED_EDGE('',*,*,#7879,.T.);
#11728=ORIENTED_EDGE('',*,*,#7880,.T.);
#11729=ORIENTED_EDGE('',*,*,#7881,.F.);
#11730=ORIENTED_EDGE('',*,*,#7882,.T.);
#11731=ORIENTED_EDGE('',*,*,#7868,.F.);
#11732=ORIENTED_EDGE('',*,*,#7869,.F.);
#11733=ORIENTED_EDGE('',*,*,#7882,.F.);
#11734=ORIENTED_EDGE('',*,*,#7883,.F.);
#11735=ORIENTED_EDGE('',*,*,#7884,.T.);
#11736=ORIENTED_EDGE('',*,*,#7885,.T.);
#11737=ORIENTED_EDGE('',*,*,#7878,.F.);
#11738=ORIENTED_EDGE('',*,*,#7886,.T.);
#11739=ORIENTED_EDGE('',*,*,#7887,.T.);
#11740=ORIENTED_EDGE('',*,*,#7888,.F.);
#11741=ORIENTED_EDGE('',*,*,#7889,.T.);
#11742=ORIENTED_EDGE('',*,*,#7890,.F.);
#11743=ORIENTED_EDGE('',*,*,#7891,.T.);
#11744=ORIENTED_EDGE('',*,*,#7892,.T.);
#11745=ORIENTED_EDGE('',*,*,#7893,.T.);
#11746=ORIENTED_EDGE('',*,*,#7894,.F.);
#11747=ORIENTED_EDGE('',*,*,#7895,.T.);
#11748=ORIENTED_EDGE('',*,*,#7896,.T.);
#11749=ORIENTED_EDGE('',*,*,#7897,.T.);
#11750=ORIENTED_EDGE('',*,*,#7898,.F.);
#11751=ORIENTED_EDGE('',*,*,#7899,.T.);
#11752=ORIENTED_EDGE('',*,*,#7900,.T.);
#11753=ORIENTED_EDGE('',*,*,#7901,.T.);
#11754=ORIENTED_EDGE('',*,*,#7902,.F.);
#11755=ORIENTED_EDGE('',*,*,#7903,.T.);
#11756=ORIENTED_EDGE('',*,*,#7904,.T.);
#11757=ORIENTED_EDGE('',*,*,#7905,.T.);
#11758=ORIENTED_EDGE('',*,*,#7906,.F.);
#11759=ORIENTED_EDGE('',*,*,#7907,.T.);
#11760=ORIENTED_EDGE('',*,*,#7908,.T.);
#11761=ORIENTED_EDGE('',*,*,#7909,.T.);
#11762=ORIENTED_EDGE('',*,*,#7910,.F.);
#11763=ORIENTED_EDGE('',*,*,#7911,.T.);
#11764=ORIENTED_EDGE('',*,*,#7912,.T.);
#11765=ORIENTED_EDGE('',*,*,#7913,.T.);
#11766=ORIENTED_EDGE('',*,*,#7914,.F.);
#11767=ORIENTED_EDGE('',*,*,#7915,.T.);
#11768=ORIENTED_EDGE('',*,*,#7916,.T.);
#11769=ORIENTED_EDGE('',*,*,#7917,.T.);
#11770=ORIENTED_EDGE('',*,*,#7918,.F.);
#11771=ORIENTED_EDGE('',*,*,#7919,.T.);
#11772=ORIENTED_EDGE('',*,*,#7920,.T.);
#11773=ORIENTED_EDGE('',*,*,#7921,.T.);
#11774=ORIENTED_EDGE('',*,*,#7922,.F.);
#11775=ORIENTED_EDGE('',*,*,#7923,.T.);
#11776=ORIENTED_EDGE('',*,*,#7924,.T.);
#11777=ORIENTED_EDGE('',*,*,#7925,.T.);
#11778=ORIENTED_EDGE('',*,*,#7865,.T.);
#11779=ORIENTED_EDGE('',*,*,#7866,.T.);
#11780=ORIENTED_EDGE('',*,*,#7926,.T.);
#11781=ORIENTED_EDGE('',*,*,#7927,.F.);
#11782=ORIENTED_EDGE('',*,*,#7928,.T.);
#11783=ORIENTED_EDGE('',*,*,#7929,.T.);
#11784=ORIENTED_EDGE('',*,*,#7930,.T.);
#11785=ORIENTED_EDGE('',*,*,#7872,.F.);
#11786=ORIENTED_EDGE('',*,*,#7873,.F.);
#11787=ORIENTED_EDGE('',*,*,#7930,.F.);
#11788=ORIENTED_EDGE('',*,*,#7931,.T.);
#11789=ORIENTED_EDGE('',*,*,#7932,.T.);
#11790=ORIENTED_EDGE('',*,*,#7933,.F.);
#11791=ORIENTED_EDGE('',*,*,#7926,.F.);
#11792=ORIENTED_EDGE('',*,*,#7934,.T.);
#11793=ORIENTED_EDGE('',*,*,#7935,.T.);
#11794=ORIENTED_EDGE('',*,*,#7936,.F.);
#11795=ORIENTED_EDGE('',*,*,#7937,.T.);
#11796=ORIENTED_EDGE('',*,*,#7938,.F.);
#11797=ORIENTED_EDGE('',*,*,#7939,.T.);
#11798=ORIENTED_EDGE('',*,*,#7940,.T.);
#11799=ORIENTED_EDGE('',*,*,#7941,.T.);
#11800=ORIENTED_EDGE('',*,*,#7942,.F.);
#11801=ORIENTED_EDGE('',*,*,#7943,.T.);
#11802=ORIENTED_EDGE('',*,*,#7944,.T.);
#11803=ORIENTED_EDGE('',*,*,#7945,.T.);
#11804=ORIENTED_EDGE('',*,*,#7946,.F.);
#11805=ORIENTED_EDGE('',*,*,#7947,.T.);
#11806=ORIENTED_EDGE('',*,*,#7948,.T.);
#11807=ORIENTED_EDGE('',*,*,#7949,.T.);
#11808=ORIENTED_EDGE('',*,*,#7950,.F.);
#11809=ORIENTED_EDGE('',*,*,#7951,.T.);
#11810=ORIENTED_EDGE('',*,*,#7952,.T.);
#11811=ORIENTED_EDGE('',*,*,#7953,.T.);
#11812=ORIENTED_EDGE('',*,*,#7954,.F.);
#11813=ORIENTED_EDGE('',*,*,#7955,.T.);
#11814=ORIENTED_EDGE('',*,*,#7956,.T.);
#11815=ORIENTED_EDGE('',*,*,#7957,.T.);
#11816=ORIENTED_EDGE('',*,*,#7958,.F.);
#11817=ORIENTED_EDGE('',*,*,#7959,.T.);
#11818=ORIENTED_EDGE('',*,*,#7960,.T.);
#11819=ORIENTED_EDGE('',*,*,#7961,.T.);
#11820=ORIENTED_EDGE('',*,*,#7962,.F.);
#11821=ORIENTED_EDGE('',*,*,#7963,.T.);
#11822=ORIENTED_EDGE('',*,*,#7964,.T.);
#11823=ORIENTED_EDGE('',*,*,#7965,.T.);
#11824=ORIENTED_EDGE('',*,*,#7966,.F.);
#11825=ORIENTED_EDGE('',*,*,#7967,.T.);
#11826=ORIENTED_EDGE('',*,*,#7968,.T.);
#11827=ORIENTED_EDGE('',*,*,#7969,.T.);
#11828=ORIENTED_EDGE('',*,*,#7970,.F.);
#11829=ORIENTED_EDGE('',*,*,#7971,.T.);
#11830=ORIENTED_EDGE('',*,*,#7972,.T.);
#11831=ORIENTED_EDGE('',*,*,#7973,.T.);
#11832=ORIENTED_EDGE('',*,*,#7974,.T.);
#11833=ORIENTED_EDGE('',*,*,#7899,.F.);
#11834=ORIENTED_EDGE('',*,*,#7975,.F.);
#11835=ORIENTED_EDGE('',*,*,#7965,.F.);
#11836=ORIENTED_EDGE('',*,*,#7976,.F.);
#11837=ORIENTED_EDGE('',*,*,#7901,.F.);
#11838=ORIENTED_EDGE('',*,*,#7977,.T.);
#11839=ORIENTED_EDGE('',*,*,#7963,.F.);
#11840=ORIENTED_EDGE('',*,*,#7962,.T.);
#11841=ORIENTED_EDGE('',*,*,#7975,.T.);
#11842=ORIENTED_EDGE('',*,*,#7898,.T.);
#11843=ORIENTED_EDGE('',*,*,#7976,.T.);
#11844=ORIENTED_EDGE('',*,*,#7977,.F.);
#11845=ORIENTED_EDGE('',*,*,#7900,.F.);
#11846=ORIENTED_EDGE('',*,*,#7974,.F.);
#11847=ORIENTED_EDGE('',*,*,#7964,.F.);
#11848=ORIENTED_EDGE('',*,*,#7978,.T.);
#11849=ORIENTED_EDGE('',*,*,#7903,.F.);
#11850=ORIENTED_EDGE('',*,*,#7979,.F.);
#11851=ORIENTED_EDGE('',*,*,#7969,.F.);
#11852=ORIENTED_EDGE('',*,*,#7980,.F.);
#11853=ORIENTED_EDGE('',*,*,#7905,.F.);
#11854=ORIENTED_EDGE('',*,*,#7981,.T.);
#11855=ORIENTED_EDGE('',*,*,#7967,.F.);
#11856=ORIENTED_EDGE('',*,*,#7966,.T.);
#11857=ORIENTED_EDGE('',*,*,#7979,.T.);
#11858=ORIENTED_EDGE('',*,*,#7902,.T.);
#11859=ORIENTED_EDGE('',*,*,#7980,.T.);
#11860=ORIENTED_EDGE('',*,*,#7981,.F.);
#11861=ORIENTED_EDGE('',*,*,#7904,.F.);
#11862=ORIENTED_EDGE('',*,*,#7978,.F.);
#11863=ORIENTED_EDGE('',*,*,#7968,.F.);
#11864=ORIENTED_EDGE('',*,*,#7982,.T.);
#11865=ORIENTED_EDGE('',*,*,#7895,.F.);
#11866=ORIENTED_EDGE('',*,*,#7983,.F.);
#11867=ORIENTED_EDGE('',*,*,#7961,.F.);
#11868=ORIENTED_EDGE('',*,*,#7984,.F.);
#11869=ORIENTED_EDGE('',*,*,#7897,.F.);
#11870=ORIENTED_EDGE('',*,*,#7985,.T.);
#11871=ORIENTED_EDGE('',*,*,#7959,.F.);
#11872=ORIENTED_EDGE('',*,*,#7958,.T.);
#11873=ORIENTED_EDGE('',*,*,#7983,.T.);
#11874=ORIENTED_EDGE('',*,*,#7894,.T.);
#11875=ORIENTED_EDGE('',*,*,#7984,.T.);
#11876=ORIENTED_EDGE('',*,*,#7985,.F.);
#11877=ORIENTED_EDGE('',*,*,#7896,.F.);
#11878=ORIENTED_EDGE('',*,*,#7982,.F.);
#11879=ORIENTED_EDGE('',*,*,#7960,.F.);
#11880=ORIENTED_EDGE('',*,*,#7986,.T.);
#11881=ORIENTED_EDGE('',*,*,#7907,.F.);
#11882=ORIENTED_EDGE('',*,*,#7987,.F.);
#11883=ORIENTED_EDGE('',*,*,#7973,.F.);
#11884=ORIENTED_EDGE('',*,*,#7988,.F.);
#11885=ORIENTED_EDGE('',*,*,#7909,.F.);
#11886=ORIENTED_EDGE('',*,*,#7989,.T.);
#11887=ORIENTED_EDGE('',*,*,#7971,.F.);
#11888=ORIENTED_EDGE('',*,*,#7970,.T.);
#11889=ORIENTED_EDGE('',*,*,#7987,.T.);
#11890=ORIENTED_EDGE('',*,*,#7906,.T.);
#11891=ORIENTED_EDGE('',*,*,#7988,.T.);
#11892=ORIENTED_EDGE('',*,*,#7989,.F.);
#11893=ORIENTED_EDGE('',*,*,#7908,.F.);
#11894=ORIENTED_EDGE('',*,*,#7986,.F.);
#11895=ORIENTED_EDGE('',*,*,#7972,.F.);
#11896=ORIENTED_EDGE('',*,*,#7990,.T.);
#11897=ORIENTED_EDGE('',*,*,#7889,.F.);
#11898=ORIENTED_EDGE('',*,*,#7991,.F.);
#11899=ORIENTED_EDGE('',*,*,#7935,.F.);
#11900=ORIENTED_EDGE('',*,*,#7992,.F.);
#11901=ORIENTED_EDGE('',*,*,#7887,.F.);
#11902=ORIENTED_EDGE('',*,*,#7993,.T.);
#11903=ORIENTED_EDGE('',*,*,#7937,.F.);
#11904=ORIENTED_EDGE('',*,*,#7936,.T.);
#11905=ORIENTED_EDGE('',*,*,#7991,.T.);
#11906=ORIENTED_EDGE('',*,*,#7888,.T.);
#11907=ORIENTED_EDGE('',*,*,#7992,.T.);
#11908=ORIENTED_EDGE('',*,*,#7993,.F.);
#11909=ORIENTED_EDGE('',*,*,#7886,.F.);
#11910=ORIENTED_EDGE('',*,*,#7990,.F.);
#11911=ORIENTED_EDGE('',*,*,#7934,.F.);
#11912=ORIENTED_EDGE('',*,*,#7994,.T.);
#11913=ORIENTED_EDGE('',*,*,#7919,.F.);
#11914=ORIENTED_EDGE('',*,*,#7995,.F.);
#11915=ORIENTED_EDGE('',*,*,#7949,.F.);
#11916=ORIENTED_EDGE('',*,*,#7996,.F.);
#11917=ORIENTED_EDGE('',*,*,#7921,.F.);
#11918=ORIENTED_EDGE('',*,*,#7997,.T.);
#11919=ORIENTED_EDGE('',*,*,#7947,.F.);
#11920=ORIENTED_EDGE('',*,*,#7946,.T.);
#11921=ORIENTED_EDGE('',*,*,#7995,.T.);
#11922=ORIENTED_EDGE('',*,*,#7918,.T.);
#11923=ORIENTED_EDGE('',*,*,#7996,.T.);
#11924=ORIENTED_EDGE('',*,*,#7997,.F.);
#11925=ORIENTED_EDGE('',*,*,#7920,.F.);
#11926=ORIENTED_EDGE('',*,*,#7994,.F.);
#11927=ORIENTED_EDGE('',*,*,#7948,.F.);
#11928=ORIENTED_EDGE('',*,*,#7998,.T.);
#11929=ORIENTED_EDGE('',*,*,#7915,.F.);
#11930=ORIENTED_EDGE('',*,*,#7999,.F.);
#11931=ORIENTED_EDGE('',*,*,#7945,.F.);
#11932=ORIENTED_EDGE('',*,*,#8000,.F.);
#11933=ORIENTED_EDGE('',*,*,#7917,.F.);
#11934=ORIENTED_EDGE('',*,*,#8001,.T.);
#11935=ORIENTED_EDGE('',*,*,#7943,.F.);
#11936=ORIENTED_EDGE('',*,*,#7942,.T.);
#11937=ORIENTED_EDGE('',*,*,#7999,.T.);
#11938=ORIENTED_EDGE('',*,*,#7914,.T.);
#11939=ORIENTED_EDGE('',*,*,#8000,.T.);
#11940=ORIENTED_EDGE('',*,*,#8001,.F.);
#11941=ORIENTED_EDGE('',*,*,#7916,.F.);
#11942=ORIENTED_EDGE('',*,*,#7998,.F.);
#11943=ORIENTED_EDGE('',*,*,#7944,.F.);
#11944=ORIENTED_EDGE('',*,*,#8002,.T.);
#11945=ORIENTED_EDGE('',*,*,#7923,.F.);
#11946=ORIENTED_EDGE('',*,*,#8003,.F.);
#11947=ORIENTED_EDGE('',*,*,#7953,.F.);
#11948=ORIENTED_EDGE('',*,*,#8004,.F.);
#11949=ORIENTED_EDGE('',*,*,#7925,.F.);
#11950=ORIENTED_EDGE('',*,*,#8005,.T.);
#11951=ORIENTED_EDGE('',*,*,#7951,.F.);
#11952=ORIENTED_EDGE('',*,*,#7950,.T.);
#11953=ORIENTED_EDGE('',*,*,#8003,.T.);
#11954=ORIENTED_EDGE('',*,*,#7922,.T.);
#11955=ORIENTED_EDGE('',*,*,#8004,.T.);
#11956=ORIENTED_EDGE('',*,*,#8005,.F.);
#11957=ORIENTED_EDGE('',*,*,#7924,.F.);
#11958=ORIENTED_EDGE('',*,*,#8002,.F.);
#11959=ORIENTED_EDGE('',*,*,#7952,.F.);
#11960=ORIENTED_EDGE('',*,*,#8006,.T.);
#11961=ORIENTED_EDGE('',*,*,#7911,.F.);
#11962=ORIENTED_EDGE('',*,*,#8007,.F.);
#11963=ORIENTED_EDGE('',*,*,#7941,.F.);
#11964=ORIENTED_EDGE('',*,*,#8008,.F.);
#11965=ORIENTED_EDGE('',*,*,#7913,.F.);
#11966=ORIENTED_EDGE('',*,*,#8009,.T.);
#11967=ORIENTED_EDGE('',*,*,#7939,.F.);
#11968=ORIENTED_EDGE('',*,*,#7938,.T.);
#11969=ORIENTED_EDGE('',*,*,#8007,.T.);
#11970=ORIENTED_EDGE('',*,*,#7910,.T.);
#11971=ORIENTED_EDGE('',*,*,#8008,.T.);
#11972=ORIENTED_EDGE('',*,*,#8009,.F.);
#11973=ORIENTED_EDGE('',*,*,#7912,.F.);
#11974=ORIENTED_EDGE('',*,*,#8006,.F.);
#11975=ORIENTED_EDGE('',*,*,#7940,.F.);
#11976=ORIENTED_EDGE('',*,*,#8010,.T.);
#11977=ORIENTED_EDGE('',*,*,#7884,.F.);
#11978=ORIENTED_EDGE('',*,*,#8011,.F.);
#11979=ORIENTED_EDGE('',*,*,#7932,.F.);
#11980=ORIENTED_EDGE('',*,*,#8012,.F.);
#11981=ORIENTED_EDGE('',*,*,#7880,.F.);
#11982=ORIENTED_EDGE('',*,*,#8013,.T.);
#11983=ORIENTED_EDGE('',*,*,#7928,.F.);
#11984=ORIENTED_EDGE('',*,*,#7927,.T.);
#11985=ORIENTED_EDGE('',*,*,#7933,.T.);
#11986=ORIENTED_EDGE('',*,*,#8011,.T.);
#11987=ORIENTED_EDGE('',*,*,#7883,.T.);
#11988=ORIENTED_EDGE('',*,*,#7881,.T.);
#11989=ORIENTED_EDGE('',*,*,#8012,.T.);
#11990=ORIENTED_EDGE('',*,*,#8013,.F.);
#11991=ORIENTED_EDGE('',*,*,#7879,.F.);
#11992=ORIENTED_EDGE('',*,*,#7885,.F.);
#11993=ORIENTED_EDGE('',*,*,#8010,.F.);
#11994=ORIENTED_EDGE('',*,*,#7931,.F.);
#11995=ORIENTED_EDGE('',*,*,#7929,.F.);
#11996=ORIENTED_EDGE('',*,*,#8014,.T.);
#11997=ORIENTED_EDGE('',*,*,#7891,.F.);
#11998=ORIENTED_EDGE('',*,*,#8015,.F.);
#11999=ORIENTED_EDGE('',*,*,#7957,.F.);
#12000=ORIENTED_EDGE('',*,*,#8016,.F.);
#12001=ORIENTED_EDGE('',*,*,#7893,.F.);
#12002=ORIENTED_EDGE('',*,*,#8017,.T.);
#12003=ORIENTED_EDGE('',*,*,#7955,.F.);
#12004=ORIENTED_EDGE('',*,*,#7954,.T.);
#12005=ORIENTED_EDGE('',*,*,#8015,.T.);
#12006=ORIENTED_EDGE('',*,*,#7890,.T.);
#12007=ORIENTED_EDGE('',*,*,#8016,.T.);
#12008=ORIENTED_EDGE('',*,*,#8017,.F.);
#12009=ORIENTED_EDGE('',*,*,#7892,.F.);
#12010=ORIENTED_EDGE('',*,*,#8014,.F.);
#12011=ORIENTED_EDGE('',*,*,#7956,.F.);
#12012=ORIENTED_EDGE('',*,*,#8018,.F.);
#12013=ORIENTED_EDGE('',*,*,#8019,.T.);
#12014=ORIENTED_EDGE('',*,*,#8020,.F.);
#12015=ORIENTED_EDGE('',*,*,#8021,.F.);
#12016=ORIENTED_EDGE('',*,*,#8019,.F.);
#12017=ORIENTED_EDGE('',*,*,#8022,.F.);
#12018=ORIENTED_EDGE('',*,*,#8023,.T.);
#12019=ORIENTED_EDGE('',*,*,#8024,.F.);
#12020=ORIENTED_EDGE('',*,*,#8023,.F.);
#12021=ORIENTED_EDGE('',*,*,#8025,.F.);
#12022=ORIENTED_EDGE('',*,*,#8026,.T.);
#12023=ORIENTED_EDGE('',*,*,#8027,.T.);
#12024=ORIENTED_EDGE('',*,*,#8028,.T.);
#12025=ORIENTED_EDGE('',*,*,#8026,.F.);
#12026=ORIENTED_EDGE('',*,*,#8029,.T.);
#12027=ORIENTED_EDGE('',*,*,#8030,.T.);
#12028=ORIENTED_EDGE('',*,*,#8027,.F.);
#12029=ORIENTED_EDGE('',*,*,#8028,.F.);
#12030=ORIENTED_EDGE('',*,*,#8030,.F.);
#12031=ORIENTED_EDGE('',*,*,#8031,.T.);
#12032=ORIENTED_EDGE('',*,*,#8029,.F.);
#12033=ORIENTED_EDGE('',*,*,#8032,.T.);
#12034=ORIENTED_EDGE('',*,*,#8033,.T.);
#12035=ORIENTED_EDGE('',*,*,#8032,.F.);
#12036=ORIENTED_EDGE('',*,*,#8031,.F.);
#12037=ORIENTED_EDGE('',*,*,#8033,.F.);
#12038=ORIENTED_EDGE('',*,*,#8034,.T.);
#12039=ORIENTED_EDGE('',*,*,#8035,.T.);
#12040=ORIENTED_EDGE('',*,*,#8034,.F.);
#12041=ORIENTED_EDGE('',*,*,#8024,.T.);
#12042=ORIENTED_EDGE('',*,*,#8036,.T.);
#12043=ORIENTED_EDGE('',*,*,#8020,.T.);
#12044=ORIENTED_EDGE('',*,*,#8021,.T.);
#12045=ORIENTED_EDGE('',*,*,#8036,.F.);
#12046=ORIENTED_EDGE('',*,*,#8037,.F.);
#12047=ORIENTED_EDGE('',*,*,#8038,.T.);
#12048=ORIENTED_EDGE('',*,*,#8025,.T.);
#12049=ORIENTED_EDGE('',*,*,#8038,.F.);
#12050=ORIENTED_EDGE('',*,*,#8037,.T.);
#12051=ORIENTED_EDGE('',*,*,#8018,.T.);
#12052=ORIENTED_EDGE('',*,*,#8035,.F.);
#12053=ORIENTED_EDGE('',*,*,#8022,.T.);
#12054=ORIENTED_EDGE('',*,*,#8039,.F.);
#12055=ORIENTED_EDGE('',*,*,#8040,.T.);
#12056=ORIENTED_EDGE('',*,*,#8041,.T.);
#12057=ORIENTED_EDGE('',*,*,#8040,.F.);
#12058=ORIENTED_EDGE('',*,*,#8041,.F.);
#12059=ORIENTED_EDGE('',*,*,#8039,.T.);
#12060=ORIENTED_EDGE('',*,*,#8042,.F.);
#12061=ORIENTED_EDGE('',*,*,#8043,.T.);
#12062=ORIENTED_EDGE('',*,*,#8044,.T.);
#12063=ORIENTED_EDGE('',*,*,#8043,.F.);
#12064=ORIENTED_EDGE('',*,*,#8044,.F.);
#12065=ORIENTED_EDGE('',*,*,#8042,.T.);
#12066=ORIENTED_EDGE('',*,*,#8045,.F.);
#12067=ORIENTED_EDGE('',*,*,#8046,.T.);
#12068=ORIENTED_EDGE('',*,*,#8047,.T.);
#12069=ORIENTED_EDGE('',*,*,#8046,.F.);
#12070=ORIENTED_EDGE('',*,*,#8047,.F.);
#12071=ORIENTED_EDGE('',*,*,#8045,.T.);
#12072=ORIENTED_EDGE('',*,*,#8048,.F.);
#12073=ORIENTED_EDGE('',*,*,#8049,.T.);
#12074=ORIENTED_EDGE('',*,*,#8050,.T.);
#12075=ORIENTED_EDGE('',*,*,#8049,.F.);
#12076=ORIENTED_EDGE('',*,*,#8050,.F.);
#12077=ORIENTED_EDGE('',*,*,#8048,.T.);
#12078=ORIENTED_EDGE('',*,*,#8051,.F.);
#12079=ORIENTED_EDGE('',*,*,#8052,.T.);
#12080=ORIENTED_EDGE('',*,*,#8053,.T.);
#12081=ORIENTED_EDGE('',*,*,#8052,.F.);
#12082=ORIENTED_EDGE('',*,*,#8053,.F.);
#12083=ORIENTED_EDGE('',*,*,#8051,.T.);
#12084=ORIENTED_EDGE('',*,*,#8054,.F.);
#12085=ORIENTED_EDGE('',*,*,#8055,.T.);
#12086=ORIENTED_EDGE('',*,*,#8056,.T.);
#12087=ORIENTED_EDGE('',*,*,#8055,.F.);
#12088=ORIENTED_EDGE('',*,*,#8056,.F.);
#12089=ORIENTED_EDGE('',*,*,#8054,.T.);
#12090=ORIENTED_EDGE('',*,*,#8057,.F.);
#12091=ORIENTED_EDGE('',*,*,#8058,.T.);
#12092=ORIENTED_EDGE('',*,*,#8059,.T.);
#12093=ORIENTED_EDGE('',*,*,#8058,.F.);
#12094=ORIENTED_EDGE('',*,*,#8059,.F.);
#12095=ORIENTED_EDGE('',*,*,#8057,.T.);
#12096=ORIENTED_EDGE('',*,*,#8060,.F.);
#12097=ORIENTED_EDGE('',*,*,#8061,.T.);
#12098=ORIENTED_EDGE('',*,*,#8062,.T.);
#12099=ORIENTED_EDGE('',*,*,#8061,.F.);
#12100=ORIENTED_EDGE('',*,*,#8062,.F.);
#12101=ORIENTED_EDGE('',*,*,#8060,.T.);
#12102=ORIENTED_EDGE('',*,*,#8063,.F.);
#12103=ORIENTED_EDGE('',*,*,#8064,.T.);
#12104=ORIENTED_EDGE('',*,*,#8065,.T.);
#12105=ORIENTED_EDGE('',*,*,#8064,.F.);
#12106=ORIENTED_EDGE('',*,*,#8065,.F.);
#12107=ORIENTED_EDGE('',*,*,#8063,.T.);
#12108=ORIENTED_EDGE('',*,*,#8066,.F.);
#12109=ORIENTED_EDGE('',*,*,#8067,.T.);
#12110=ORIENTED_EDGE('',*,*,#8068,.T.);
#12111=ORIENTED_EDGE('',*,*,#8067,.F.);
#12112=ORIENTED_EDGE('',*,*,#8068,.F.);
#12113=ORIENTED_EDGE('',*,*,#8066,.T.);
#12114=ORIENTED_EDGE('',*,*,#8069,.F.);
#12115=ORIENTED_EDGE('',*,*,#8070,.T.);
#12116=ORIENTED_EDGE('',*,*,#8071,.T.);
#12117=ORIENTED_EDGE('',*,*,#8070,.F.);
#12118=ORIENTED_EDGE('',*,*,#8071,.F.);
#12119=ORIENTED_EDGE('',*,*,#8069,.T.);
#12120=CYLINDRICAL_SURFACE('',#13129,8.12525);
#12121=CYLINDRICAL_SURFACE('',#13131,8.12525);
#12122=CYLINDRICAL_SURFACE('',#13132,8.12525);
#12123=CYLINDRICAL_SURFACE('',#13133,8.12525);
#12124=CYLINDRICAL_SURFACE('',#13134,8.12525);
#12125=CYLINDRICAL_SURFACE('',#13135,8.12525);
#12126=CYLINDRICAL_SURFACE('',#13136,8.12525);
#12127=CYLINDRICAL_SURFACE('',#13137,8.12525);
#12128=CYLINDRICAL_SURFACE('',#13138,8.12525);
#12129=CYLINDRICAL_SURFACE('',#13139,8.12525);
#12130=CYLINDRICAL_SURFACE('',#13140,8.12525);
#12131=CYLINDRICAL_SURFACE('',#13141,8.12525);
#12132=CYLINDRICAL_SURFACE('',#13143,7.01125);
#12133=CYLINDRICAL_SURFACE('',#13145,7.01125);
#12134=CYLINDRICAL_SURFACE('',#13146,7.01125);
#12135=CYLINDRICAL_SURFACE('',#13147,7.01125);
#12136=CYLINDRICAL_SURFACE('',#13148,7.01125);
#12137=CYLINDRICAL_SURFACE('',#13149,7.01125);
#12138=CYLINDRICAL_SURFACE('',#13150,7.01125);
#12139=CYLINDRICAL_SURFACE('',#13151,7.01125);
#12140=CYLINDRICAL_SURFACE('',#13152,7.01125);
#12141=CYLINDRICAL_SURFACE('',#13153,7.01125);
#12142=CYLINDRICAL_SURFACE('',#13154,7.01125);
#12143=CYLINDRICAL_SURFACE('',#13155,7.01125);
#12144=CYLINDRICAL_SURFACE('',#13157,7.01125);
#12145=CYLINDRICAL_SURFACE('',#13158,8.12525);
#12146=CYLINDRICAL_SURFACE('',#13676,15.5);
#12147=CYLINDRICAL_SURFACE('',#13678,15.5);
#12148=CYLINDRICAL_SURFACE('',#13697,15.5);
#12149=CYLINDRICAL_SURFACE('',#13698,15.5);
#12150=CYLINDRICAL_SURFACE('',#13699,15.5);
#12151=CYLINDRICAL_SURFACE('',#13700,15.5);
#12152=CYLINDRICAL_SURFACE('',#13701,15.5);
#12153=CYLINDRICAL_SURFACE('',#13702,15.5);
#12154=CYLINDRICAL_SURFACE('',#13703,15.5);
#12155=CYLINDRICAL_SURFACE('',#13704,15.5);
#12156=CYLINDRICAL_SURFACE('',#13705,15.5);
#12157=CYLINDRICAL_SURFACE('',#13706,15.5);
#12158=CYLINDRICAL_SURFACE('',#13707,15.5);
#12159=CYLINDRICAL_SURFACE('',#13708,15.5);
#12160=CYLINDRICAL_SURFACE('',#13709,15.5);
#12161=CYLINDRICAL_SURFACE('',#13710,15.5);
#12162=CYLINDRICAL_SURFACE('',#13711,15.5);
#12163=CYLINDRICAL_SURFACE('',#13712,15.5);
#12164=CYLINDRICAL_SURFACE('',#13714,1.);
#12165=CYLINDRICAL_SURFACE('',#13717,1.);
#12166=CYLINDRICAL_SURFACE('',#13720,1.);
#12167=CYLINDRICAL_SURFACE('',#13728,13.5);
#12168=CYLINDRICAL_SURFACE('',#13732,5.5);
#12169=CYLINDRICAL_SURFACE('',#13736,6.767);
#12170=CYLINDRICAL_SURFACE('',#13738,6.767);
#12171=CYLINDRICAL_SURFACE('',#13739,6.767);
#12172=CYLINDRICAL_SURFACE('',#13740,6.767);
#12173=CYLINDRICAL_SURFACE('',#13741,6.767);
#12174=CYLINDRICAL_SURFACE('',#13742,6.767);
#12175=CYLINDRICAL_SURFACE('',#13743,6.767);
#12176=CYLINDRICAL_SURFACE('',#13744,6.767);
#12177=CYLINDRICAL_SURFACE('',#13745,6.767);
#12178=CYLINDRICAL_SURFACE('',#13746,6.767);
#12179=CYLINDRICAL_SURFACE('',#13747,6.767);
#12180=CYLINDRICAL_SURFACE('',#13748,6.767);
#12181=CYLINDRICAL_SURFACE('',#13749,6.767);
#12182=CYLINDRICAL_SURFACE('',#13750,6.767);
#12183=CYLINDRICAL_SURFACE('',#13751,6.767);
#12184=CYLINDRICAL_SURFACE('',#13752,6.767);
#12185=CYLINDRICAL_SURFACE('',#13753,6.767);
#12186=CYLINDRICAL_SURFACE('',#13754,6.767);
#12187=CYLINDRICAL_SURFACE('',#13755,6.767);
#12188=CYLINDRICAL_SURFACE('',#13756,6.767);
#12189=CYLINDRICAL_SURFACE('',#13757,6.767);
#12190=CYLINDRICAL_SURFACE('',#13758,6.767);
#12191=CYLINDRICAL_SURFACE('',#13759,6.767);
#12192=CYLINDRICAL_SURFACE('',#13760,6.767);
#12193=CYLINDRICAL_SURFACE('',#13761,6.767);
#12194=CYLINDRICAL_SURFACE('',#13762,6.767);
#12195=CYLINDRICAL_SURFACE('',#13763,6.767);
#12196=CYLINDRICAL_SURFACE('',#13764,6.767);
#12197=CYLINDRICAL_SURFACE('',#13765,6.767);
#12198=CYLINDRICAL_SURFACE('',#13766,6.767);
#12199=CYLINDRICAL_SURFACE('',#13767,6.767);
#12200=CYLINDRICAL_SURFACE('',#13768,6.767);
#12201=CYLINDRICAL_SURFACE('',#13769,6.767);
#12202=CYLINDRICAL_SURFACE('',#13770,6.767);
#12203=CYLINDRICAL_SURFACE('',#13771,6.767);
#12204=CYLINDRICAL_SURFACE('',#13772,6.767);
#12205=CYLINDRICAL_SURFACE('',#13773,6.767);
#12206=CYLINDRICAL_SURFACE('',#13774,6.767);
#12207=CYLINDRICAL_SURFACE('',#13775,6.767);
#12208=CYLINDRICAL_SURFACE('',#13776,6.767);
#12209=CYLINDRICAL_SURFACE('',#13777,6.767);
#12210=CYLINDRICAL_SURFACE('',#13778,6.767);
#12211=CYLINDRICAL_SURFACE('',#13779,6.767);
#12212=CYLINDRICAL_SURFACE('',#13780,6.767);
#12213=CYLINDRICAL_SURFACE('',#13781,6.767);
#12214=CYLINDRICAL_SURFACE('',#13782,6.767);
#12215=CYLINDRICAL_SURFACE('',#13783,6.767);
#12216=CYLINDRICAL_SURFACE('',#13784,6.767);
#12217=CYLINDRICAL_SURFACE('',#13785,6.767);
#12218=CYLINDRICAL_SURFACE('',#13786,6.767);
#12219=CYLINDRICAL_SURFACE('',#13787,6.767);
#12220=CYLINDRICAL_SURFACE('',#13788,6.767);
#12221=CYLINDRICAL_SURFACE('',#13789,6.767);
#12222=CYLINDRICAL_SURFACE('',#13790,6.767);
#12223=CYLINDRICAL_SURFACE('',#13791,6.767);
#12224=CYLINDRICAL_SURFACE('',#13792,6.767);
#12225=CYLINDRICAL_SURFACE('',#13793,6.767);
#12226=CYLINDRICAL_SURFACE('',#13794,6.767);
#12227=CYLINDRICAL_SURFACE('',#13795,6.767);
#12228=CYLINDRICAL_SURFACE('',#13796,6.767);
#12229=CYLINDRICAL_SURFACE('',#13797,7.911);
#12230=CYLINDRICAL_SURFACE('',#13800,6.767);
#12231=CYLINDRICAL_SURFACE('',#13802,2.);
#12232=CYLINDRICAL_SURFACE('',#13805,2.);
#12233=CYLINDRICAL_SURFACE('',#13808,2.);
#12234=CYLINDRICAL_SURFACE('',#13811,2.);
#12235=CYLINDRICAL_SURFACE('',#13819,20.);
#12236=CYLINDRICAL_SURFACE('',#13829,6.);
#12237=CYLINDRICAL_SURFACE('',#13831,6.);
#12238=CYLINDRICAL_SURFACE('',#13832,6.);
#12239=CYLINDRICAL_SURFACE('',#13833,6.);
#12240=CYLINDRICAL_SURFACE('',#13834,6.);
#12241=CYLINDRICAL_SURFACE('',#13835,6.);
#12242=CYLINDRICAL_SURFACE('',#13837,6.);
#12243=CYLINDRICAL_SURFACE('',#13845,4.5);
#12244=CYLINDRICAL_SURFACE('',#13847,4.5);
#12245=CYLINDRICAL_SURFACE('',#13857,23.);
#12246=CYLINDRICAL_SURFACE('',#13865,1.);
#12247=CYLINDRICAL_SURFACE('',#13867,1.);
#12248=CYLINDRICAL_SURFACE('',#13869,1.);
#12249=CYLINDRICAL_SURFACE('',#13871,1.);
#12250=CYLINDRICAL_SURFACE('',#13873,10.);
#12251=CYLINDRICAL_SURFACE('',#13877,1.);
#12252=CYLINDRICAL_SURFACE('',#13881,1.);
#12253=CYLINDRICAL_SURFACE('',#13885,1.);
#12254=CYLINDRICAL_SURFACE('',#13889,1.);
#12255=CYLINDRICAL_SURFACE('',#13893,8.5);
#12256=CYLINDRICAL_SURFACE('',#13896,1.);
#12257=CYLINDRICAL_SURFACE('',#13900,1.);
#12258=CYLINDRICAL_SURFACE('',#13904,1.);
#12259=CYLINDRICAL_SURFACE('',#13908,2.5);
#12260=CYLINDRICAL_SURFACE('',#13911,2.5);
#12261=CYLINDRICAL_SURFACE('',#13914,2.5);
#12262=CYLINDRICAL_SURFACE('',#13917,2.5);
#12263=CYLINDRICAL_SURFACE('',#13920,5.);
#12264=CYLINDRICAL_SURFACE('',#13930,5.);
#12265=CYLINDRICAL_SURFACE('',#13932,5.);
#12266=CYLINDRICAL_SURFACE('',#13935,5.);
#12267=CYLINDRICAL_SURFACE('',#13943,13.5);
#12268=CYLINDRICAL_SURFACE('',#13960,10.5);
#12269=CYLINDRICAL_SURFACE('',#13964,20.);
#12270=CYLINDRICAL_SURFACE('',#13968,23.);
#12271=CYLINDRICAL_SURFACE('',#13972,1.);
#12272=CYLINDRICAL_SURFACE('',#13975,1.);
#12273=CYLINDRICAL_SURFACE('',#13978,1.);
#12274=CYLINDRICAL_SURFACE('',#13986,13.5);
#12275=CYLINDRICAL_SURFACE('',#13990,5.5);
#12276=CYLINDRICAL_SURFACE('',#14003,4.5);
#12277=CYLINDRICAL_SURFACE('',#14014,6.24166666666667);
#12278=CYLINDRICAL_SURFACE('',#14015,6.24166666666667);
#12279=CYLINDRICAL_SURFACE('',#14027,6.46166666666667);
#12280=CYLINDRICAL_SURFACE('',#14037,8.9);
#12281=CYLINDRICAL_SURFACE('',#14041,8.9);
#12282=CYLINDRICAL_SURFACE('',#14044,6.46166666666667);
#12283=CYLINDRICAL_SURFACE('',#14063,10.);
#12284=CYLINDRICAL_SURFACE('',#14073,8.9);
#12285=CYLINDRICAL_SURFACE('',#14078,8.9);
#12286=CYLINDRICAL_SURFACE('',#14097,6.24166666666667);
#12287=CYLINDRICAL_SURFACE('',#14103,6.40666666666667);
#12288=CYLINDRICAL_SURFACE('',#14112,6.46166666666667);
#12289=CYLINDRICAL_SURFACE('',#14128,20.);
#12290=CYLINDRICAL_SURFACE('',#14200,2.74859462638384);
#12291=CYLINDRICAL_SURFACE('',#14203,2.74859462638384);
#12292=CYLINDRICAL_SURFACE('',#14208,2.74859462638384);
#12293=CYLINDRICAL_SURFACE('',#14211,2.74859462638384);
#12294=CYLINDRICAL_SURFACE('',#14216,2.74859462638384);
#12295=CYLINDRICAL_SURFACE('',#14219,2.74859462638384);
#12296=CYLINDRICAL_SURFACE('',#14224,2.74859462638384);
#12297=CYLINDRICAL_SURFACE('',#14227,2.74859462638384);
#12298=CYLINDRICAL_SURFACE('',#14232,2.74859462638384);
#12299=CYLINDRICAL_SURFACE('',#14235,2.74859462638384);
#12300=CYLINDRICAL_SURFACE('',#14240,2.74859462638384);
#12301=CYLINDRICAL_SURFACE('',#14243,2.74859462638384);
#12302=CYLINDRICAL_SURFACE('',#14248,2.74859462638384);
#12303=CYLINDRICAL_SURFACE('',#14251,2.74859462638384);
#12304=CYLINDRICAL_SURFACE('',#14256,2.74859462638384);
#12305=CYLINDRICAL_SURFACE('',#14259,2.74859462638384);
#12306=CYLINDRICAL_SURFACE('',#14264,2.74859462638384);
#12307=CYLINDRICAL_SURFACE('',#14267,2.74859462638384);
#12308=CYLINDRICAL_SURFACE('',#14272,2.74859462638384);
#12309=CYLINDRICAL_SURFACE('',#14275,2.74859462638384);
#12310=CYLINDRICAL_SURFACE('',#14280,2.74859462638384);
#12311=CYLINDRICAL_SURFACE('',#14283,2.74859462638384);
#12312=CYLINDRICAL_SURFACE('',#14306,14.0317131491268);
#12313=CYLINDRICAL_SURFACE('',#14308,8.5);
#12314=CYLINDRICAL_SURFACE('',#14309,11.9728634517814);
#12315=CYLINDRICAL_SURFACE('',#14313,2.62159462638384);
#12316=CYLINDRICAL_SURFACE('',#14318,2.62159462638384);
#12317=CYLINDRICAL_SURFACE('',#14323,2.62159462638384);
#12318=CYLINDRICAL_SURFACE('',#14328,2.62159462638384);
#12319=CYLINDRICAL_SURFACE('',#14333,2.62159462638384);
#12320=CYLINDRICAL_SURFACE('',#14338,2.62159462638384);
#12321=CYLINDRICAL_SURFACE('',#14343,2.62159462638384);
#12322=CYLINDRICAL_SURFACE('',#14348,2.62159462638384);
#12323=CYLINDRICAL_SURFACE('',#14353,2.62159462638384);
#12324=CYLINDRICAL_SURFACE('',#14358,2.62159462638384);
#12325=CYLINDRICAL_SURFACE('',#14363,2.62159462638384);
#12326=ADVANCED_FACE('',(#796),#12120,.F.);
#12327=ADVANCED_FACE('',(#797),#12121,.F.);
#12328=ADVANCED_FACE('',(#798),#12122,.F.);
#12329=ADVANCED_FACE('',(#799),#12123,.F.);
#12330=ADVANCED_FACE('',(#800),#12124,.F.);
#12331=ADVANCED_FACE('',(#801),#12125,.F.);
#12332=ADVANCED_FACE('',(#802),#12126,.F.);
#12333=ADVANCED_FACE('',(#803),#12127,.F.);
#12334=ADVANCED_FACE('',(#804),#12128,.F.);
#12335=ADVANCED_FACE('',(#805),#12129,.F.);
#12336=ADVANCED_FACE('',(#806),#12130,.F.);
#12337=ADVANCED_FACE('',(#807),#12131,.F.);
#12338=ADVANCED_FACE('',(#808),#12132,.F.);
#12339=ADVANCED_FACE('',(#809),#12133,.F.);
#12340=ADVANCED_FACE('',(#810),#12134,.F.);
#12341=ADVANCED_FACE('',(#811),#12135,.F.);
#12342=ADVANCED_FACE('',(#812),#12136,.F.);
#12343=ADVANCED_FACE('',(#813),#12137,.F.);
#12344=ADVANCED_FACE('',(#814),#12138,.F.);
#12345=ADVANCED_FACE('',(#815),#12139,.F.);
#12346=ADVANCED_FACE('',(#816),#12140,.F.);
#12347=ADVANCED_FACE('',(#817),#12141,.F.);
#12348=ADVANCED_FACE('',(#818),#12142,.F.);
#12349=ADVANCED_FACE('',(#819),#12143,.F.);
#12350=ADVANCED_FACE('',(#820),#12144,.F.);
#12351=ADVANCED_FACE('',(#821),#12145,.F.);
#12352=ADVANCED_FACE('',(#822),#610,.F.);
#12353=ADVANCED_FACE('',(#823),#611,.F.);
#12354=ADVANCED_FACE('',(#824,#347),#440,.T.);
#12355=ADVANCED_FACE('',(#825),#441,.F.);
#12356=ADVANCED_FACE('',(#826),#442,.F.);
#12357=ADVANCED_FACE('',(#827),#443,.F.);
#12358=ADVANCED_FACE('',(#828),#444,.F.);
#12359=ADVANCED_FACE('',(#829),#445,.F.);
#12360=ADVANCED_FACE('',(#830),#446,.F.);
#12361=ADVANCED_FACE('',(#831),#447,.F.);
#12362=ADVANCED_FACE('',(#832),#448,.F.);
#12363=ADVANCED_FACE('',(#833),#449,.F.);
#12364=ADVANCED_FACE('',(#834),#450,.F.);
#12365=ADVANCED_FACE('',(#835),#451,.F.);
#12366=ADVANCED_FACE('',(#836),#452,.F.);
#12367=ADVANCED_FACE('',(#837),#453,.F.);
#12368=ADVANCED_FACE('',(#838),#454,.F.);
#12369=ADVANCED_FACE('',(#839),#455,.F.);
#12370=ADVANCED_FACE('',(#840),#456,.F.);
#12371=ADVANCED_FACE('',(#841),#457,.F.);
#12372=ADVANCED_FACE('',(#842),#458,.F.);
#12373=ADVANCED_FACE('',(#843),#290,.T.);
#12374=ADVANCED_FACE('',(#844),#291,.T.);
#12375=ADVANCED_FACE('',(#845),#292,.T.);
#12376=ADVANCED_FACE('',(#846),#293,.T.);
#12377=ADVANCED_FACE('',(#847),#294,.T.);
#12378=ADVANCED_FACE('',(#848),#295,.T.);
#12379=ADVANCED_FACE('',(#849),#296,.T.);
#12380=ADVANCED_FACE('',(#850),#297,.T.);
#12381=ADVANCED_FACE('',(#851),#298,.T.);
#12382=ADVANCED_FACE('',(#852),#299,.T.);
#12383=ADVANCED_FACE('',(#853),#300,.T.);
#12384=ADVANCED_FACE('',(#854),#301,.T.);
#12385=ADVANCED_FACE('',(#855),#302,.T.);
#12386=ADVANCED_FACE('',(#856),#303,.T.);
#12387=ADVANCED_FACE('',(#857),#304,.T.);
#12388=ADVANCED_FACE('',(#858),#305,.T.);
#12389=ADVANCED_FACE('',(#859),#306,.T.);
#12390=ADVANCED_FACE('',(#860),#307,.T.);
#12391=ADVANCED_FACE('',(#861),#308,.T.);
#12392=ADVANCED_FACE('',(#862),#309,.T.);
#12393=ADVANCED_FACE('',(#863),#310,.T.);
#12394=ADVANCED_FACE('',(#864),#311,.T.);
#12395=ADVANCED_FACE('',(#865),#312,.T.);
#12396=ADVANCED_FACE('',(#866),#313,.T.);
#12397=ADVANCED_FACE('',(#867),#314,.T.);
#12398=ADVANCED_FACE('',(#868),#315,.T.);
#12399=ADVANCED_FACE('',(#869),#316,.T.);
#12400=ADVANCED_FACE('',(#870),#317,.T.);
#12401=ADVANCED_FACE('',(#871),#318,.T.);
#12402=ADVANCED_FACE('',(#872),#319,.T.);
#12403=ADVANCED_FACE('',(#873),#320,.T.);
#12404=ADVANCED_FACE('',(#874),#321,.T.);
#12405=ADVANCED_FACE('',(#875),#322,.T.);
#12406=ADVANCED_FACE('',(#876),#323,.T.);
#12407=ADVANCED_FACE('',(#877),#324,.T.);
#12408=ADVANCED_FACE('',(#878),#325,.T.);
#12409=ADVANCED_FACE('',(#879),#459,.F.);
#12410=ADVANCED_FACE('',(#880),#460,.F.);
#12411=ADVANCED_FACE('',(#881),#461,.F.);
#12412=ADVANCED_FACE('',(#882),#462,.F.);
#12413=ADVANCED_FACE('',(#883),#463,.F.);
#12414=ADVANCED_FACE('',(#884),#464,.F.);
#12415=ADVANCED_FACE('',(#885),#465,.F.);
#12416=ADVANCED_FACE('',(#886),#466,.F.);
#12417=ADVANCED_FACE('',(#887),#467,.F.);
#12418=ADVANCED_FACE('',(#888),#468,.F.);
#12419=ADVANCED_FACE('',(#889),#469,.F.);
#12420=ADVANCED_FACE('',(#890),#470,.F.);
#12421=ADVANCED_FACE('',(#891),#471,.F.);
#12422=ADVANCED_FACE('',(#892),#472,.F.);
#12423=ADVANCED_FACE('',(#893),#473,.F.);
#12424=ADVANCED_FACE('',(#894),#474,.F.);
#12425=ADVANCED_FACE('',(#895),#475,.F.);
#12426=ADVANCED_FACE('',(#896),#476,.F.);
#12427=ADVANCED_FACE('',(#897),#477,.F.);
#12428=ADVANCED_FACE('',(#898),#478,.F.);
#12429=ADVANCED_FACE('',(#899),#479,.F.);
#12430=ADVANCED_FACE('',(#900),#480,.F.);
#12431=ADVANCED_FACE('',(#901),#481,.F.);
#12432=ADVANCED_FACE('',(#902),#482,.F.);
#12433=ADVANCED_FACE('',(#903),#483,.F.);
#12434=ADVANCED_FACE('',(#904),#484,.F.);
#12435=ADVANCED_FACE('',(#905),#485,.F.);
#12436=ADVANCED_FACE('',(#906),#486,.F.);
#12437=ADVANCED_FACE('',(#907),#487,.F.);
#12438=ADVANCED_FACE('',(#908),#488,.F.);
#12439=ADVANCED_FACE('',(#909),#489,.F.);
#12440=ADVANCED_FACE('',(#910),#490,.F.);
#12441=ADVANCED_FACE('',(#911),#491,.F.);
#12442=ADVANCED_FACE('',(#912),#492,.F.);
#12443=ADVANCED_FACE('',(#913),#493,.F.);
#12444=ADVANCED_FACE('',(#914),#494,.F.);
#12445=ADVANCED_FACE('',(#915),#495,.F.);
#12446=ADVANCED_FACE('',(#916),#496,.F.);
#12447=ADVANCED_FACE('',(#917),#497,.F.);
#12448=ADVANCED_FACE('',(#918),#498,.F.);
#12449=ADVANCED_FACE('',(#919),#499,.F.);
#12450=ADVANCED_FACE('',(#920),#500,.F.);
#12451=ADVANCED_FACE('',(#921),#501,.F.);
#12452=ADVANCED_FACE('',(#922),#502,.F.);
#12453=ADVANCED_FACE('',(#923),#503,.F.);
#12454=ADVANCED_FACE('',(#924),#504,.F.);
#12455=ADVANCED_FACE('',(#925),#505,.F.);
#12456=ADVANCED_FACE('',(#926),#506,.F.);
#12457=ADVANCED_FACE('',(#927),#507,.F.);
#12458=ADVANCED_FACE('',(#928),#508,.F.);
#12459=ADVANCED_FACE('',(#929),#509,.F.);
#12460=ADVANCED_FACE('',(#930),#510,.F.);
#12461=ADVANCED_FACE('',(#931),#511,.F.);
#12462=ADVANCED_FACE('',(#932),#512,.F.);
#12463=ADVANCED_FACE('',(#933),#152,.F.);
#12464=ADVANCED_FACE('',(#934),#153,.F.);
#12465=ADVANCED_FACE('',(#935),#154,.F.);
#12466=ADVANCED_FACE('',(#936),#155,.F.);
#12467=ADVANCED_FACE('',(#937),#156,.F.);
#12468=ADVANCED_FACE('',(#938),#157,.F.);
#12469=ADVANCED_FACE('',(#939),#158,.F.);
#12470=ADVANCED_FACE('',(#940),#159,.F.);
#12471=ADVANCED_FACE('',(#941),#160,.F.);
#12472=ADVANCED_FACE('',(#942),#161,.F.);
#12473=ADVANCED_FACE('',(#943),#162,.F.);
#12474=ADVANCED_FACE('',(#944),#163,.F.);
#12475=ADVANCED_FACE('',(#945),#164,.F.);
#12476=ADVANCED_FACE('',(#946),#165,.F.);
#12477=ADVANCED_FACE('',(#947),#166,.F.);
#12478=ADVANCED_FACE('',(#948),#167,.F.);
#12479=ADVANCED_FACE('',(#949),#168,.F.);
#12480=ADVANCED_FACE('',(#950),#169,.F.);
#12481=ADVANCED_FACE('',(#951),#612,.T.);
#12482=ADVANCED_FACE('',(#952),#613,.T.);
#12483=ADVANCED_FACE('',(#953),#614,.T.);
#12484=ADVANCED_FACE('',(#954),#615,.T.);
#12485=ADVANCED_FACE('',(#955),#616,.T.);
#12486=ADVANCED_FACE('',(#956),#617,.T.);
#12487=ADVANCED_FACE('',(#957),#618,.T.);
#12488=ADVANCED_FACE('',(#958),#619,.T.);
#12489=ADVANCED_FACE('',(#959),#620,.T.);
#12490=ADVANCED_FACE('',(#960),#621,.T.);
#12491=ADVANCED_FACE('',(#961),#622,.T.);
#12492=ADVANCED_FACE('',(#962),#623,.T.);
#12493=ADVANCED_FACE('',(#963),#624,.T.);
#12494=ADVANCED_FACE('',(#964),#625,.T.);
#12495=ADVANCED_FACE('',(#965),#626,.T.);
#12496=ADVANCED_FACE('',(#966),#627,.T.);
#12497=ADVANCED_FACE('',(#967),#628,.T.);
#12498=ADVANCED_FACE('',(#968),#629,.T.);
#12499=ADVANCED_FACE('',(#969),#630,.T.);
#12500=ADVANCED_FACE('',(#970),#631,.T.);
#12501=ADVANCED_FACE('',(#971),#632,.T.);
#12502=ADVANCED_FACE('',(#972),#633,.T.);
#12503=ADVANCED_FACE('',(#973),#634,.T.);
#12504=ADVANCED_FACE('',(#974),#635,.T.);
#12505=ADVANCED_FACE('',(#975),#636,.T.);
#12506=ADVANCED_FACE('',(#976),#637,.T.);
#12507=ADVANCED_FACE('',(#977),#638,.T.);
#12508=ADVANCED_FACE('',(#978),#639,.T.);
#12509=ADVANCED_FACE('',(#979),#640,.T.);
#12510=ADVANCED_FACE('',(#980),#641,.T.);
#12511=ADVANCED_FACE('',(#981),#642,.T.);
#12512=ADVANCED_FACE('',(#982),#643,.T.);
#12513=ADVANCED_FACE('',(#983),#644,.T.);
#12514=ADVANCED_FACE('',(#984),#645,.T.);
#12515=ADVANCED_FACE('',(#985),#646,.T.);
#12516=ADVANCED_FACE('',(#986),#647,.T.);
#12517=ADVANCED_FACE('',(#987),#648,.T.);
#12518=ADVANCED_FACE('',(#988),#649,.T.);
#12519=ADVANCED_FACE('',(#989),#650,.T.);
#12520=ADVANCED_FACE('',(#990),#651,.T.);
#12521=ADVANCED_FACE('',(#991),#652,.T.);
#12522=ADVANCED_FACE('',(#992),#653,.T.);
#12523=ADVANCED_FACE('',(#993),#654,.T.);
#12524=ADVANCED_FACE('',(#994),#655,.T.);
#12525=ADVANCED_FACE('',(#995),#656,.T.);
#12526=ADVANCED_FACE('',(#996),#657,.T.);
#12527=ADVANCED_FACE('',(#997),#658,.T.);
#12528=ADVANCED_FACE('',(#998),#659,.T.);
#12529=ADVANCED_FACE('',(#999),#660,.T.);
#12530=ADVANCED_FACE('',(#1000),#661,.T.);
#12531=ADVANCED_FACE('',(#1001),#662,.T.);
#12532=ADVANCED_FACE('',(#1002),#663,.T.);
#12533=ADVANCED_FACE('',(#1003),#664,.T.);
#12534=ADVANCED_FACE('',(#1004),#665,.T.);
#12535=ADVANCED_FACE('',(#1005),#666,.T.);
#12536=ADVANCED_FACE('',(#1006),#667,.T.);
#12537=ADVANCED_FACE('',(#1007),#668,.T.);
#12538=ADVANCED_FACE('',(#1008),#669,.T.);
#12539=ADVANCED_FACE('',(#1009),#670,.T.);
#12540=ADVANCED_FACE('',(#1010),#671,.T.);
#12541=ADVANCED_FACE('',(#1011),#672,.T.);
#12542=ADVANCED_FACE('',(#1012),#673,.T.);
#12543=ADVANCED_FACE('',(#1013),#674,.T.);
#12544=ADVANCED_FACE('',(#1014),#675,.T.);
#12545=ADVANCED_FACE('',(#1015),#676,.T.);
#12546=ADVANCED_FACE('',(#1016),#677,.T.);
#12547=ADVANCED_FACE('',(#1017),#678,.T.);
#12548=ADVANCED_FACE('',(#1018),#679,.T.);
#12549=ADVANCED_FACE('',(#1019),#680,.T.);
#12550=ADVANCED_FACE('',(#1020),#681,.T.);
#12551=ADVANCED_FACE('',(#1021),#682,.T.);
#12552=ADVANCED_FACE('',(#1022),#683,.T.);
#12553=ADVANCED_FACE('',(#1023),#684,.T.);
#12554=ADVANCED_FACE('',(#1024),#685,.T.);
#12555=ADVANCED_FACE('',(#1025),#686,.T.);
#12556=ADVANCED_FACE('',(#1026),#687,.T.);
#12557=ADVANCED_FACE('',(#1027),#688,.T.);
#12558=ADVANCED_FACE('',(#1028),#689,.T.);
#12559=ADVANCED_FACE('',(#1029),#690,.T.);
#12560=ADVANCED_FACE('',(#1030),#691,.T.);
#12561=ADVANCED_FACE('',(#1031),#692,.T.);
#12562=ADVANCED_FACE('',(#1032),#693,.T.);
#12563=ADVANCED_FACE('',(#1033),#694,.T.);
#12564=ADVANCED_FACE('',(#1034),#695,.T.);
#12565=ADVANCED_FACE('',(#1035),#696,.T.);
#12566=ADVANCED_FACE('',(#1036),#697,.T.);
#12567=ADVANCED_FACE('',(#1037),#698,.T.);
#12568=ADVANCED_FACE('',(#1038),#699,.T.);
#12569=ADVANCED_FACE('',(#1039),#700,.T.);
#12570=ADVANCED_FACE('',(#1040),#701,.T.);
#12571=ADVANCED_FACE('',(#1041),#702,.T.);
#12572=ADVANCED_FACE('',(#1042),#703,.T.);
#12573=ADVANCED_FACE('',(#1043),#704,.T.);
#12574=ADVANCED_FACE('',(#1044),#12146,.T.);
#12575=ADVANCED_FACE('',(#1045),#12147,.T.);
#12576=ADVANCED_FACE('',(#1046),#705,.T.);
#12577=ADVANCED_FACE('',(#1047),#706,.T.);
#12578=ADVANCED_FACE('',(#1048),#707,.T.);
#12579=ADVANCED_FACE('',(#1049),#708,.T.);
#12580=ADVANCED_FACE('',(#1050),#709,.T.);
#12581=ADVANCED_FACE('',(#1051),#710,.T.);
#12582=ADVANCED_FACE('',(#1052,#348),#513,.F.);
#12583=ADVANCED_FACE('',(#1053),#12148,.T.);
#12584=ADVANCED_FACE('',(#1054),#711,.T.);
#12585=ADVANCED_FACE('',(#1055),#712,.T.);
#12586=ADVANCED_FACE('',(#1056),#713,.T.);
#12587=ADVANCED_FACE('',(#1057),#12149,.T.);
#12588=ADVANCED_FACE('',(#1058),#12150,.T.);
#12589=ADVANCED_FACE('',(#1059),#714,.T.);
#12590=ADVANCED_FACE('',(#1060),#715,.T.);
#12591=ADVANCED_FACE('',(#1061),#716,.T.);
#12592=ADVANCED_FACE('',(#1062),#717,.T.);
#12593=ADVANCED_FACE('',(#1063),#718,.T.);
#12594=ADVANCED_FACE('',(#1064),#719,.T.);
#12595=ADVANCED_FACE('',(#1065),#12151,.T.);
#12596=ADVANCED_FACE('',(#1066),#720,.T.);
#12597=ADVANCED_FACE('',(#1067),#721,.T.);
#12598=ADVANCED_FACE('',(#1068),#722,.T.);
#12599=ADVANCED_FACE('',(#1069),#12152,.T.);
#12600=ADVANCED_FACE('',(#1070),#12153,.T.);
#12601=ADVANCED_FACE('',(#1071),#723,.T.);
#12602=ADVANCED_FACE('',(#1072),#724,.T.);
#12603=ADVANCED_FACE('',(#1073),#725,.T.);
#12604=ADVANCED_FACE('',(#1074),#726,.T.);
#12605=ADVANCED_FACE('',(#1075),#727,.T.);
#12606=ADVANCED_FACE('',(#1076),#728,.T.);
#12607=ADVANCED_FACE('',(#1077),#12154,.T.);
#12608=ADVANCED_FACE('',(#1078),#729,.T.);
#12609=ADVANCED_FACE('',(#1079),#730,.T.);
#12610=ADVANCED_FACE('',(#1080),#731,.T.);
#12611=ADVANCED_FACE('',(#1081),#12155,.T.);
#12612=ADVANCED_FACE('',(#1082),#12156,.T.);
#12613=ADVANCED_FACE('',(#1083),#732,.T.);
#12614=ADVANCED_FACE('',(#1084),#733,.T.);
#12615=ADVANCED_FACE('',(#1085),#734,.T.);
#12616=ADVANCED_FACE('',(#1086),#735,.T.);
#12617=ADVANCED_FACE('',(#1087),#736,.T.);
#12618=ADVANCED_FACE('',(#1088),#737,.T.);
#12619=ADVANCED_FACE('',(#1089),#12157,.T.);
#12620=ADVANCED_FACE('',(#1090),#738,.T.);
#12621=ADVANCED_FACE('',(#1091),#739,.T.);
#12622=ADVANCED_FACE('',(#1092),#740,.T.);
#12623=ADVANCED_FACE('',(#1093),#12158,.T.);
#12624=ADVANCED_FACE('',(#1094),#12159,.T.);
#12625=ADVANCED_FACE('',(#1095),#741,.T.);
#12626=ADVANCED_FACE('',(#1096),#742,.T.);
#12627=ADVANCED_FACE('',(#1097),#743,.T.);
#12628=ADVANCED_FACE('',(#1098),#744,.T.);
#12629=ADVANCED_FACE('',(#1099),#745,.T.);
#12630=ADVANCED_FACE('',(#1100),#746,.T.);
#12631=ADVANCED_FACE('',(#1101),#12160,.T.);
#12632=ADVANCED_FACE('',(#1102),#747,.T.);
#12633=ADVANCED_FACE('',(#1103),#748,.T.);
#12634=ADVANCED_FACE('',(#1104),#749,.T.);
#12635=ADVANCED_FACE('',(#1105),#12161,.T.);
#12636=ADVANCED_FACE('',(#1106),#12162,.T.);
#12637=ADVANCED_FACE('',(#1107),#750,.T.);
#12638=ADVANCED_FACE('',(#1108),#751,.T.);
#12639=ADVANCED_FACE('',(#1109),#752,.T.);
#12640=ADVANCED_FACE('',(#1110),#753,.T.);
#12641=ADVANCED_FACE('',(#1111),#754,.T.);
#12642=ADVANCED_FACE('',(#1112),#755,.T.);
#12643=ADVANCED_FACE('',(#1113),#12163,.T.);
#12644=ADVANCED_FACE('',(#1114),#12164,.F.);
#12645=ADVANCED_FACE('',(#1115),#12165,.F.);
#12646=ADVANCED_FACE('',(#1116),#12166,.F.);
#12647=ADVANCED_FACE('',(#1117),#170,.T.);
#12648=ADVANCED_FACE('',(#1118),#12167,.T.);
#12649=ADVANCED_FACE('',(#1119,#349,#350,#351,#352),#514,.T.);
#12650=ADVANCED_FACE('',(#1120),#12168,.F.);
#12651=ADVANCED_FACE('',(#1121,#353,#354,#355,#356),#515,.F.);
#12652=ADVANCED_FACE('',(#1122),#12169,.T.);
#12653=ADVANCED_FACE('',(#1123),#12170,.T.);
#12654=ADVANCED_FACE('',(#1124),#12171,.T.);
#12655=ADVANCED_FACE('',(#1125),#12172,.T.);
#12656=ADVANCED_FACE('',(#1126),#12173,.T.);
#12657=ADVANCED_FACE('',(#1127),#12174,.T.);
#12658=ADVANCED_FACE('',(#1128),#12175,.T.);
#12659=ADVANCED_FACE('',(#1129),#12176,.T.);
#12660=ADVANCED_FACE('',(#1130),#12177,.T.);
#12661=ADVANCED_FACE('',(#1131),#12178,.T.);
#12662=ADVANCED_FACE('',(#1132),#12179,.T.);
#12663=ADVANCED_FACE('',(#1133),#12180,.T.);
#12664=ADVANCED_FACE('',(#1134),#12181,.T.);
#12665=ADVANCED_FACE('',(#1135),#12182,.T.);
#12666=ADVANCED_FACE('',(#1136),#12183,.T.);
#12667=ADVANCED_FACE('',(#1137),#12184,.T.);
#12668=ADVANCED_FACE('',(#1138),#12185,.T.);
#12669=ADVANCED_FACE('',(#1139),#12186,.T.);
#12670=ADVANCED_FACE('',(#1140),#12187,.T.);
#12671=ADVANCED_FACE('',(#1141),#12188,.T.);
#12672=ADVANCED_FACE('',(#1142),#12189,.T.);
#12673=ADVANCED_FACE('',(#1143),#12190,.T.);
#12674=ADVANCED_FACE('',(#1144),#12191,.T.);
#12675=ADVANCED_FACE('',(#1145),#12192,.T.);
#12676=ADVANCED_FACE('',(#1146),#12193,.T.);
#12677=ADVANCED_FACE('',(#1147),#12194,.T.);
#12678=ADVANCED_FACE('',(#1148),#12195,.T.);
#12679=ADVANCED_FACE('',(#1149),#12196,.T.);
#12680=ADVANCED_FACE('',(#1150),#12197,.T.);
#12681=ADVANCED_FACE('',(#1151),#12198,.T.);
#12682=ADVANCED_FACE('',(#1152),#12199,.T.);
#12683=ADVANCED_FACE('',(#1153),#12200,.T.);
#12684=ADVANCED_FACE('',(#1154),#12201,.T.);
#12685=ADVANCED_FACE('',(#1155),#12202,.T.);
#12686=ADVANCED_FACE('',(#1156),#12203,.T.);
#12687=ADVANCED_FACE('',(#1157),#12204,.T.);
#12688=ADVANCED_FACE('',(#1158),#12205,.T.);
#12689=ADVANCED_FACE('',(#1159),#12206,.T.);
#12690=ADVANCED_FACE('',(#1160),#12207,.T.);
#12691=ADVANCED_FACE('',(#1161),#12208,.T.);
#12692=ADVANCED_FACE('',(#1162),#12209,.T.);
#12693=ADVANCED_FACE('',(#1163),#12210,.T.);
#12694=ADVANCED_FACE('',(#1164),#12211,.T.);
#12695=ADVANCED_FACE('',(#1165),#12212,.T.);
#12696=ADVANCED_FACE('',(#1166),#12213,.T.);
#12697=ADVANCED_FACE('',(#1167),#12214,.T.);
#12698=ADVANCED_FACE('',(#1168),#12215,.T.);
#12699=ADVANCED_FACE('',(#1169),#12216,.T.);
#12700=ADVANCED_FACE('',(#1170),#12217,.T.);
#12701=ADVANCED_FACE('',(#1171),#12218,.T.);
#12702=ADVANCED_FACE('',(#1172),#12219,.T.);
#12703=ADVANCED_FACE('',(#1173),#12220,.T.);
#12704=ADVANCED_FACE('',(#1174),#12221,.T.);
#12705=ADVANCED_FACE('',(#1175),#12222,.T.);
#12706=ADVANCED_FACE('',(#1176),#12223,.T.);
#12707=ADVANCED_FACE('',(#1177),#12224,.T.);
#12708=ADVANCED_FACE('',(#1178),#12225,.T.);
#12709=ADVANCED_FACE('',(#1179),#12226,.T.);
#12710=ADVANCED_FACE('',(#1180),#12227,.T.);
#12711=ADVANCED_FACE('',(#1181),#12228,.T.);
#12712=ADVANCED_FACE('',(#1182),#12229,.T.);
#12713=ADVANCED_FACE('',(#1183),#12230,.T.);
#12714=ADVANCED_FACE('',(#1184),#756,.F.);
#12715=ADVANCED_FACE('',(#1185),#757,.F.);
#12716=ADVANCED_FACE('',(#1186),#12231,.F.);
#12717=ADVANCED_FACE('',(#1187),#12232,.F.);
#12718=ADVANCED_FACE('',(#1188),#12233,.F.);
#12719=ADVANCED_FACE('',(#1189),#12234,.F.);
#12720=ADVANCED_FACE('',(#1190),#171,.T.);
#12721=ADVANCED_FACE('',(#1191),#12235,.T.);
#12722=ADVANCED_FACE('',(#1192,#357,#358,#359,#360,#361),#516,.F.);
#12723=ADVANCED_FACE('',(#1193),#172,.T.);
#12724=ADVANCED_FACE('',(#1194,#362,#363,#364,#365),#517,.T.);
#12725=ADVANCED_FACE('',(#1195),#518,.F.);
#12726=ADVANCED_FACE('',(#1196),#12236,.T.);
#12727=ADVANCED_FACE('',(#1197),#12237,.T.);
#12728=ADVANCED_FACE('',(#1198),#12238,.T.);
#12729=ADVANCED_FACE('',(#1199),#12239,.T.);
#12730=ADVANCED_FACE('',(#1200),#12240,.T.);
#12731=ADVANCED_FACE('',(#1201),#12241,.T.);
#12732=ADVANCED_FACE('',(#1202),#12242,.T.);
#12733=ADVANCED_FACE('',(#1203,#366),#519,.F.);
#12734=ADVANCED_FACE('',(#1204),#758,.T.);
#12735=ADVANCED_FACE('',(#1205),#759,.T.);
#12736=ADVANCED_FACE('',(#1206),#760,.T.);
#12737=ADVANCED_FACE('',(#1207,#367),#520,.T.);
#12738=ADVANCED_FACE('',(#1208),#761,.T.);
#12739=ADVANCED_FACE('',(#1209),#762,.T.);
#12740=ADVANCED_FACE('',(#1210),#763,.T.);
#12741=ADVANCED_FACE('',(#1211),#12243,.T.);
#12742=ADVANCED_FACE('',(#1212),#12244,.T.);
#12743=ADVANCED_FACE('',(#1213),#521,.T.);
#12744=ADVANCED_FACE('',(#1214),#764,.T.);
#12745=ADVANCED_FACE('',(#1215),#765,.T.);
#12746=ADVANCED_FACE('',(#1216),#766,.T.);
#12747=ADVANCED_FACE('',(#1217),#767,.T.);
#12748=ADVANCED_FACE('',(#1218),#768,.T.);
#12749=ADVANCED_FACE('',(#1219),#769,.T.);
#12750=ADVANCED_FACE('',(#1220),#770,.T.);
#12751=ADVANCED_FACE('',(#1221),#771,.T.);
#12752=ADVANCED_FACE('',(#1222),#772,.T.);
#12753=ADVANCED_FACE('',(#1223),#773,.T.);
#12754=ADVANCED_FACE('',(#1224),#774,.T.);
#12755=ADVANCED_FACE('',(#1225),#775,.T.);
#12756=ADVANCED_FACE('',(#1226),#776,.T.);
#12757=ADVANCED_FACE('',(#1227),#777,.T.);
#12758=ADVANCED_FACE('',(#1228),#778,.T.);
#12759=ADVANCED_FACE('',(#1229),#779,.T.);
#12760=ADVANCED_FACE('',(#1230),#780,.T.);
#12761=ADVANCED_FACE('',(#1231),#781,.T.);
#12762=ADVANCED_FACE('',(#1232),#782,.T.);
#12763=ADVANCED_FACE('',(#1233),#783,.T.);
#12764=ADVANCED_FACE('',(#1234),#784,.T.);
#12765=ADVANCED_FACE('',(#1235),#785,.T.);
#12766=ADVANCED_FACE('',(#1236),#786,.T.);
#12767=ADVANCED_FACE('',(#1237),#787,.T.);
#12768=ADVANCED_FACE('',(#1238),#788,.T.);
#12769=ADVANCED_FACE('',(#1239),#789,.T.);
#12770=ADVANCED_FACE('',(#1240),#790,.T.);
#12771=ADVANCED_FACE('',(#1241),#791,.T.);
#12772=ADVANCED_FACE('',(#1242),#792,.T.);
#12773=ADVANCED_FACE('',(#1243),#793,.T.);
#12774=ADVANCED_FACE('',(#1244),#794,.T.);
#12775=ADVANCED_FACE('',(#1245),#795,.T.);
#12776=ADVANCED_FACE('',(#1246),#522,.F.);
#12777=ADVANCED_FACE('',(#1247),#173,.T.);
#12778=ADVANCED_FACE('',(#1248),#12245,.T.);
#12779=ADVANCED_FACE('',(#1249,#368,#369,#370,#371,#372),#523,.T.);
#12780=ADVANCED_FACE('',(#1250),#12246,.F.);
#12781=ADVANCED_FACE('',(#1251),#12247,.F.);
#12782=ADVANCED_FACE('',(#1252),#12248,.F.);
#12783=ADVANCED_FACE('',(#1253),#12249,.F.);
#12784=ADVANCED_FACE('',(#1254),#12250,.F.);
#12785=ADVANCED_FACE('',(#1255,#373,#374,#375,#376,#377),#524,.F.);
#12786=ADVANCED_FACE('',(#1256),#12251,.F.);
#12787=ADVANCED_FACE('',(#1257),#525,.T.);
#12788=ADVANCED_FACE('',(#1258),#12252,.F.);
#12789=ADVANCED_FACE('',(#1259),#526,.T.);
#12790=ADVANCED_FACE('',(#1260),#12253,.F.);
#12791=ADVANCED_FACE('',(#1261),#527,.T.);
#12792=ADVANCED_FACE('',(#1262),#12254,.F.);
#12793=ADVANCED_FACE('',(#1263),#528,.T.);
#12794=ADVANCED_FACE('',(#1264),#12255,.F.);
#12795=ADVANCED_FACE('',(#1265),#12256,.F.);
#12796=ADVANCED_FACE('',(#1266),#529,.T.);
#12797=ADVANCED_FACE('',(#1267),#12257,.F.);
#12798=ADVANCED_FACE('',(#1268),#530,.T.);
#12799=ADVANCED_FACE('',(#1269),#12258,.F.);
#12800=ADVANCED_FACE('',(#1270),#531,.T.);
#12801=ADVANCED_FACE('',(#1271),#12259,.F.);
#12802=ADVANCED_FACE('',(#1272),#12260,.F.);
#12803=ADVANCED_FACE('',(#1273),#12261,.F.);
#12804=ADVANCED_FACE('',(#1274),#12262,.F.);
#12805=ADVANCED_FACE('',(#1275),#12263,.T.);
#12806=ADVANCED_FACE('',(#1276,#378,#379,#380,#381),#532,.T.);
#12807=ADVANCED_FACE('',(#1277),#533,.T.);
#12808=ADVANCED_FACE('',(#1278),#12264,.T.);
#12809=ADVANCED_FACE('',(#1279),#12265,.T.);
#12810=ADVANCED_FACE('',(#1280),#534,.T.);
#12811=ADVANCED_FACE('',(#1281),#12266,.T.);
#12812=ADVANCED_FACE('',(#1282),#535,.T.);
#12813=ADVANCED_FACE('',(#1283),#536,.F.);
#12814=ADVANCED_FACE('',(#1284),#537,.T.);
#12815=ADVANCED_FACE('',(#1285),#538,.T.);
#12816=ADVANCED_FACE('',(#1286),#12267,.T.);
#12817=ADVANCED_FACE('',(#1287),#539,.T.);
#12818=ADVANCED_FACE('',(#1288),#540,.T.);
#12819=ADVANCED_FACE('',(#1289),#541,.T.);
#12820=ADVANCED_FACE('',(#1290),#542,.F.);
#12821=ADVANCED_FACE('',(#1291),#543,.T.);
#12822=ADVANCED_FACE('',(#1292),#544,.T.);
#12823=ADVANCED_FACE('',(#1293,#382),#545,.F.);
#12824=ADVANCED_FACE('',(#1294),#546,.F.);
#12825=ADVANCED_FACE('',(#1295),#12268,.F.);
#12826=ADVANCED_FACE('',(#1296,#383),#547,.T.);
#12827=ADVANCED_FACE('',(#1297,#384),#12269,.F.);
#12828=ADVANCED_FACE('',(#1298,#385,#386,#387,#388,#389),#548,.T.);
#12829=ADVANCED_FACE('',(#1299),#12270,.T.);
#12830=ADVANCED_FACE('',(#1300,#390,#391,#392,#393),#549,.T.);
#12831=ADVANCED_FACE('',(#1301,#394,#395,#396,#397,#398),#550,.T.);
#12832=ADVANCED_FACE('',(#1302),#12271,.F.);
#12833=ADVANCED_FACE('',(#1303),#12272,.F.);
#12834=ADVANCED_FACE('',(#1304),#12273,.F.);
#12835=ADVANCED_FACE('',(#1305),#174,.T.);
#12836=ADVANCED_FACE('',(#1306),#12274,.T.);
#12837=ADVANCED_FACE('',(#1307,#399,#400,#401,#402),#551,.F.);
#12838=ADVANCED_FACE('',(#1308),#12275,.F.);
#12839=ADVANCED_FACE('',(#1309,#403,#404,#405,#406),#552,.T.);
#12840=ADVANCED_FACE('',(#1310),#175,.F.);
#12841=ADVANCED_FACE('',(#1311),#326,.F.);
#12842=ADVANCED_FACE('',(#1312),#12276,.F.);
#12843=ADVANCED_FACE('',(#1313),#327,.F.);
#12844=ADVANCED_FACE('',(#1314),#176,.T.);
#12845=ADVANCED_FACE('',(#1315),#177,.T.);
#12846=ADVANCED_FACE('',(#1316),#12277,.T.);
#12847=ADVANCED_FACE('',(#1317),#12278,.T.);
#12848=ADVANCED_FACE('',(#1318),#178,.T.);
#12849=ADVANCED_FACE('',(#1319),#179,.T.);
#12850=ADVANCED_FACE('',(#1320,#407),#553,.F.);
#12851=ADVANCED_FACE('',(#1321,#408),#554,.F.);
#12852=ADVANCED_FACE('',(#1322),#55,.T.);
#12853=ADVANCED_FACE('',(#1323),#12279,.F.);
#12854=ADVANCED_FACE('',(#1324),#180,.T.);
#12855=ADVANCED_FACE('',(#1325),#328,.T.);
#12856=ADVANCED_FACE('',(#1326),#12280,.T.);
#12857=ADVANCED_FACE('',(#1327,#409),#555,.F.);
#12858=ADVANCED_FACE('',(#1328,#410),#556,.F.);
#12859=ADVANCED_FACE('',(#1329),#12281,.T.);
#12860=ADVANCED_FACE('',(#1330),#12282,.F.);
#12861=ADVANCED_FACE('',(#1331),#181,.T.);
#12862=ADVANCED_FACE('',(#1332),#329,.T.);
#12863=ADVANCED_FACE('',(#1333,#411),#557,.F.);
#12864=ADVANCED_FACE('',(#1334,#412),#558,.F.);
#12865=ADVANCED_FACE('',(#1335),#330,.F.);
#12866=ADVANCED_FACE('',(#1336),#331,.F.);
#12867=ADVANCED_FACE('',(#1337),#332,.T.);
#12868=ADVANCED_FACE('',(#1338),#12283,.T.);
#12869=ADVANCED_FACE('',(#1339),#333,.T.);
#12870=ADVANCED_FACE('',(#1340),#334,.F.);
#12871=ADVANCED_FACE('',(#1341),#335,.F.);
#12872=ADVANCED_FACE('',(#1342),#12284,.F.);
#12873=ADVANCED_FACE('',(#1343),#182,.F.);
#12874=ADVANCED_FACE('',(#1344),#12285,.F.);
#12875=ADVANCED_FACE('',(#1345,#413),#559,.F.);
#12876=ADVANCED_FACE('',(#1346,#414),#560,.F.);
#12877=ADVANCED_FACE('',(#1347),#56,.T.);
#12878=ADVANCED_FACE('',(#1348),#57,.T.);
#12879=ADVANCED_FACE('',(#1349),#58,.T.);
#12880=ADVANCED_FACE('',(#1350),#59,.T.);
#12881=ADVANCED_FACE('',(#1351),#60,.T.);
#12882=ADVANCED_FACE('',(#1352),#61,.T.);
#12883=ADVANCED_FACE('',(#1353),#62,.T.);
#12884=ADVANCED_FACE('',(#1354),#63,.T.);
#12885=ADVANCED_FACE('',(#1355),#12286,.F.);
#12886=ADVANCED_FACE('',(#1356),#183,.T.);
#12887=ADVANCED_FACE('',(#1357),#12287,.T.);
#12888=ADVANCED_FACE('',(#1358),#184,.T.);
#12889=ADVANCED_FACE('',(#1359),#336,.T.);
#12890=ADVANCED_FACE('',(#1360),#12288,.T.);
#12891=ADVANCED_FACE('',(#1361,#415),#561,.F.);
#12892=ADVANCED_FACE('',(#1362),#185,.T.);
#12893=ADVANCED_FACE('',(#1363),#186,.T.);
#12894=ADVANCED_FACE('',(#1364),#337,.F.);
#12895=ADVANCED_FACE('',(#1365),#12289,.T.);
#12896=ADVANCED_FACE('',(#1366,#416),#562,.F.);
#12897=ADVANCED_FACE('',(#1367,#417),#563,.F.);
#12898=ADVANCED_FACE('',(#1368),#338,.T.);
#12899=ADVANCED_FACE('',(#1369),#339,.T.);
#12900=ADVANCED_FACE('',(#1370),#187,.T.);
#12901=ADVANCED_FACE('',(#1371),#340,.F.);
#12902=ADVANCED_FACE('',(#1372),#341,.F.);
#12903=ADVANCED_FACE('',(#1373,#418,#419,#420,#421,#422,#423,#424,#425,
#426,#427),#342,.F.);
#12904=ADVANCED_FACE('',(#1374,#428,#429,#430,#431,#432,#433,#434,#435,
#436,#437),#343,.T.);
#12905=ADVANCED_FACE('',(#1375),#12290,.F.);
#12906=ADVANCED_FACE('',(#1376),#12291,.F.);
#12907=ADVANCED_FACE('',(#1377),#564,.T.);
#12908=ADVANCED_FACE('',(#1378),#565,.F.);
#12909=ADVANCED_FACE('',(#1379),#12292,.F.);
#12910=ADVANCED_FACE('',(#1380),#12293,.F.);
#12911=ADVANCED_FACE('',(#1381),#566,.T.);
#12912=ADVANCED_FACE('',(#1382),#567,.F.);
#12913=ADVANCED_FACE('',(#1383),#12294,.F.);
#12914=ADVANCED_FACE('',(#1384),#12295,.F.);
#12915=ADVANCED_FACE('',(#1385),#568,.T.);
#12916=ADVANCED_FACE('',(#1386),#569,.F.);
#12917=ADVANCED_FACE('',(#1387),#12296,.F.);
#12918=ADVANCED_FACE('',(#1388),#12297,.F.);
#12919=ADVANCED_FACE('',(#1389),#570,.T.);
#12920=ADVANCED_FACE('',(#1390),#571,.F.);
#12921=ADVANCED_FACE('',(#1391),#12298,.F.);
#12922=ADVANCED_FACE('',(#1392),#12299,.F.);
#12923=ADVANCED_FACE('',(#1393),#572,.T.);
#12924=ADVANCED_FACE('',(#1394),#573,.F.);
#12925=ADVANCED_FACE('',(#1395),#12300,.F.);
#12926=ADVANCED_FACE('',(#1396),#12301,.F.);
#12927=ADVANCED_FACE('',(#1397),#574,.T.);
#12928=ADVANCED_FACE('',(#1398),#575,.F.);
#12929=ADVANCED_FACE('',(#1399),#12302,.F.);
#12930=ADVANCED_FACE('',(#1400),#12303,.F.);
#12931=ADVANCED_FACE('',(#1401),#576,.T.);
#12932=ADVANCED_FACE('',(#1402),#577,.F.);
#12933=ADVANCED_FACE('',(#1403),#12304,.F.);
#12934=ADVANCED_FACE('',(#1404),#12305,.F.);
#12935=ADVANCED_FACE('',(#1405),#578,.T.);
#12936=ADVANCED_FACE('',(#1406),#579,.F.);
#12937=ADVANCED_FACE('',(#1407),#12306,.F.);
#12938=ADVANCED_FACE('',(#1408),#12307,.F.);
#12939=ADVANCED_FACE('',(#1409),#580,.T.);
#12940=ADVANCED_FACE('',(#1410),#581,.F.);
#12941=ADVANCED_FACE('',(#1411),#12308,.F.);
#12942=ADVANCED_FACE('',(#1412),#12309,.F.);
#12943=ADVANCED_FACE('',(#1413),#582,.T.);
#12944=ADVANCED_FACE('',(#1414),#583,.F.);
#12945=ADVANCED_FACE('',(#1415),#12310,.F.);
#12946=ADVANCED_FACE('',(#1416),#12311,.F.);
#12947=ADVANCED_FACE('',(#1417),#584,.T.);
#12948=ADVANCED_FACE('',(#1418),#585,.F.);
#12949=ADVANCED_FACE('',(#1419),#188,.T.);
#12950=ADVANCED_FACE('',(#1420),#189,.T.);
#12951=ADVANCED_FACE('',(#1421),#344,.T.);
#12952=ADVANCED_FACE('',(#1422),#345,.T.);
#12953=ADVANCED_FACE('',(#1423),#346,.F.);
#12954=ADVANCED_FACE('',(#1424),#12312,.T.);
#12955=ADVANCED_FACE('',(#1425),#12313,.F.);
#12956=ADVANCED_FACE('',(#1426),#12314,.T.);
#12957=ADVANCED_FACE('',(#1427,#438),#586,.F.);
#12958=ADVANCED_FACE('',(#1428,#439),#587,.F.);
#12959=ADVANCED_FACE('',(#1429),#12315,.T.);
#12960=ADVANCED_FACE('',(#1430),#588,.F.);
#12961=ADVANCED_FACE('',(#1431),#589,.T.);
#12962=ADVANCED_FACE('',(#1432),#12316,.T.);
#12963=ADVANCED_FACE('',(#1433),#590,.F.);
#12964=ADVANCED_FACE('',(#1434),#591,.T.);
#12965=ADVANCED_FACE('',(#1435),#12317,.T.);
#12966=ADVANCED_FACE('',(#1436),#592,.F.);
#12967=ADVANCED_FACE('',(#1437),#593,.T.);
#12968=ADVANCED_FACE('',(#1438),#12318,.T.);
#12969=ADVANCED_FACE('',(#1439),#594,.F.);
#12970=ADVANCED_FACE('',(#1440),#595,.T.);
#12971=ADVANCED_FACE('',(#1441),#12319,.T.);
#12972=ADVANCED_FACE('',(#1442),#596,.F.);
#12973=ADVANCED_FACE('',(#1443),#597,.T.);
#12974=ADVANCED_FACE('',(#1444),#12320,.T.);
#12975=ADVANCED_FACE('',(#1445),#598,.F.);
#12976=ADVANCED_FACE('',(#1446),#599,.T.);
#12977=ADVANCED_FACE('',(#1447),#12321,.T.);
#12978=ADVANCED_FACE('',(#1448),#600,.F.);
#12979=ADVANCED_FACE('',(#1449),#601,.T.);
#12980=ADVANCED_FACE('',(#1450),#12322,.T.);
#12981=ADVANCED_FACE('',(#1451),#602,.F.);
#12982=ADVANCED_FACE('',(#1452),#603,.T.);
#12983=ADVANCED_FACE('',(#1453),#12323,.T.);
#12984=ADVANCED_FACE('',(#1454),#604,.F.);
#12985=ADVANCED_FACE('',(#1455),#605,.T.);
#12986=ADVANCED_FACE('',(#1456),#12324,.T.);
#12987=ADVANCED_FACE('',(#1457),#606,.F.);
#12988=ADVANCED_FACE('',(#1458),#607,.T.);
#12989=ADVANCED_FACE('',(#1459),#12325,.T.);
#12990=ADVANCED_FACE('',(#1460),#608,.F.);
#12991=ADVANCED_FACE('',(#1461),#609,.T.);
#12992=CLOSED_SHELL('',(#12326,#12327,#12328,#12329,#12330,#12331,#12332,
#12333,#12334,#12335,#12336,#12337,#12338,#12339,#12340,#12341,#12342,#12343,
#12344,#12345,#12346,#12347,#12348,#12349,#12350,#12351,#12352,#12353,#12354,
#12355,#12356,#12357,#12358,#12359,#12360,#12361,#12362,#12363,#12364,#12365,
#12366,#12367,#12368,#12369,#12370,#12371,#12372,#12373,#12374,#12375,#12376,
#12377,#12378,#12379,#12380,#12381,#12382,#12383,#12384,#12385,#12386,#12387,
#12388,#12389,#12390,#12391,#12392,#12393,#12394,#12395,#12396,#12397,#12398,
#12399,#12400,#12401,#12402,#12403,#12404,#12405,#12406,#12407,#12408,#12409,
#12410,#12411,#12412,#12413,#12414,#12415,#12416,#12417,#12418,#12419,#12420,
#12421,#12422,#12423,#12424,#12425,#12426,#12427,#12428,#12429,#12430,#12431,
#12432,#12433,#12434,#12435,#12436,#12437,#12438,#12439,#12440,#12441,#12442,
#12443,#12444,#12445,#12446,#12447,#12448,#12449,#12450,#12451,#12452,#12453,
#12454,#12455,#12456,#12457,#12458,#12459,#12460,#12461,#12462,#12463,#12464,
#12465,#12466,#12467,#12468,#12469,#12470,#12471,#12472,#12473,#12474,#12475,
#12476,#12477,#12478,#12479,#12480,#12481,#12482,#12483,#12484,#12485,#12486,
#12487,#12488,#12489,#12490,#12491,#12492,#12493,#12494,#12495,#12496,#12497,
#12498,#12499,#12500,#12501,#12502,#12503,#12504,#12505,#12506,#12507,#12508,
#12509,#12510,#12511,#12512,#12513,#12514,#12515,#12516,#12517,#12518,#12519,
#12520,#12521,#12522,#12523,#12524,#12525,#12526,#12527,#12528,#12529,#12530,
#12531,#12532,#12533,#12534,#12535,#12536,#12537,#12538,#12539,#12540,#12541,
#12542,#12543,#12544,#12545,#12546,#12547,#12548,#12549,#12550,#12551,#12552,
#12553,#12554,#12555,#12556,#12557,#12558,#12559,#12560,#12561,#12562,#12563,
#12564,#12565,#12566,#12567,#12568,#12569,#12570,#12571,#12572,#12573,#12574,
#12575,#12576,#12577,#12578,#12579,#12580,#12581,#12582,#12583,#12584,#12585,
#12586,#12587,#12588,#12589,#12590,#12591,#12592,#12593,#12594,#12595,#12596,
#12597,#12598,#12599,#12600,#12601,#12602,#12603,#12604,#12605,#12606,#12607,
#12608,#12609,#12610,#12611,#12612,#12613,#12614,#12615,#12616,#12617,#12618,
#12619,#12620,#12621,#12622,#12623,#12624,#12625,#12626,#12627,#12628,#12629,
#12630,#12631,#12632,#12633,#12634,#12635,#12636,#12637,#12638,#12639,#12640,
#12641,#12642,#12643));
#12993=CLOSED_SHELL('',(#12644,#12645,#12646,#12647,#12648,#12649,#12650,
#12651));
#12994=CLOSED_SHELL('',(#12652,#12653,#12654,#12655,#12656,#12657,#12658,
#12659,#12660,#12661,#12662,#12663,#12664,#12665,#12666,#12667,#12668,#12669,
#12670,#12671,#12672,#12673,#12674,#12675,#12676,#12677,#12678,#12679,#12680,
#12681,#12682,#12683,#12684,#12685,#12686,#12687,#12688,#12689,#12690,#12691,
#12692,#12693,#12694,#12695,#12696,#12697,#12698,#12699,#12700,#12701,#12702,
#12703,#12704,#12705,#12706,#12707,#12708,#12709,#12710,#12711,#12712,#12713,
#12714,#12715,#12716,#12717,#12718,#12719,#12720,#12721,#12722,#12723,#12724,
#12725));
#12995=CLOSED_SHELL('',(#12726,#12727,#12728,#12729,#12730,#12731,#12732,
#12733,#12734,#12735,#12736,#12737,#12738,#12739,#12740,#12741,#12742,#12743,
#12744,#12745,#12746,#12747,#12748,#12749,#12750,#12751,#12752,#12753,#12754,
#12755,#12756,#12757,#12758,#12759,#12760,#12761,#12762,#12763,#12764,#12765,
#12766,#12767,#12768,#12769,#12770,#12771,#12772,#12773,#12774,#12775,#12776));
#12996=CLOSED_SHELL('',(#12777,#12778,#12779,#12780,#12781,#12782,#12783,
#12784,#12785));
#12997=CLOSED_SHELL('',(#12786,#12787,#12788,#12789,#12790,#12791,#12792,
#12793,#12794,#12795,#12796,#12797,#12798,#12799,#12800,#12801,#12802,#12803,
#12804,#12805,#12806,#12807,#12808,#12809,#12810,#12811,#12812,#12813,#12814,
#12815,#12816,#12817,#12818,#12819,#12820,#12821,#12822,#12823,#12824,#12825,
#12826,#12827,#12828,#12829,#12830,#12831));
#12998=CLOSED_SHELL('',(#12832,#12833,#12834,#12835,#12836,#12837,#12838,
#12839));
#12999=CLOSED_SHELL('',(#12840,#12841,#12842,#12843,#12844,#12845,#12846,
#12847,#12848,#12849,#12850,#12851));
#13000=CLOSED_SHELL('',(#12852));
#13001=CLOSED_SHELL('',(#12853,#12854,#12855,#12856,#12857,#12858));
#13002=CLOSED_SHELL('',(#12859,#12860,#12861,#12862,#12863,#12864));
#13003=CLOSED_SHELL('',(#12865,#12866,#12867,#12868,#12869,#12870,#12871,
#12872,#12873,#12874,#12875,#12876));
#13004=CLOSED_SHELL('',(#12877));
#13005=CLOSED_SHELL('',(#12878));
#13006=CLOSED_SHELL('',(#12879));
#13007=CLOSED_SHELL('',(#12880));
#13008=CLOSED_SHELL('',(#12881));
#13009=CLOSED_SHELL('',(#12882));
#13010=CLOSED_SHELL('',(#12883));
#13011=CLOSED_SHELL('',(#12884));
#13012=CLOSED_SHELL('',(#12885,#12886,#12887,#12888,#12889,#12890,#12891));
#13013=CLOSED_SHELL('',(#12892,#12893,#12894,#12895,#12896,#12897));
#13014=CLOSED_SHELL('',(#12898,#12899,#12900,#12901,#12902,#12903,#12904,
#12905,#12906,#12907,#12908,#12909,#12910,#12911,#12912,#12913,#12914,#12915,
#12916,#12917,#12918,#12919,#12920,#12921,#12922,#12923,#12924,#12925,#12926,
#12927,#12928,#12929,#12930,#12931,#12932,#12933,#12934,#12935,#12936,#12937,
#12938,#12939,#12940,#12941,#12942,#12943,#12944,#12945,#12946,#12947,#12948));
#13015=CLOSED_SHELL('',(#12949,#12950,#12951,#12952,#12953,#12954,#12955,
#12956,#12957,#12958));
#13016=CLOSED_SHELL('',(#12959,#12960,#12961));
#13017=CLOSED_SHELL('',(#12962,#12963,#12964));
#13018=CLOSED_SHELL('',(#12965,#12966,#12967));
#13019=CLOSED_SHELL('',(#12968,#12969,#12970));
#13020=CLOSED_SHELL('',(#12971,#12972,#12973));
#13021=CLOSED_SHELL('',(#12974,#12975,#12976));
#13022=CLOSED_SHELL('',(#12977,#12978,#12979));
#13023=CLOSED_SHELL('',(#12980,#12981,#12982));
#13024=CLOSED_SHELL('',(#12983,#12984,#12985));
#13025=CLOSED_SHELL('',(#12986,#12987,#12988));
#13026=CLOSED_SHELL('',(#12989,#12990,#12991));
#13027=DERIVED_UNIT_ELEMENT(#13045,1.);
#13028=DERIVED_UNIT_ELEMENT(#88485,-3.);
#13029=DERIVED_UNIT_ELEMENT(#13045,1.);
#13030=DERIVED_UNIT_ELEMENT(#88485,-3.);
#13031=DERIVED_UNIT_ELEMENT(#13045,1.);
#13032=DERIVED_UNIT_ELEMENT(#88485,-3.);
#13033=DERIVED_UNIT_ELEMENT(#13045,1.);
#13034=DERIVED_UNIT_ELEMENT(#88485,-3.);
#13035=DERIVED_UNIT_ELEMENT(#13045,1.);
#13036=DERIVED_UNIT_ELEMENT(#88485,-3.);
#13037=DERIVED_UNIT_ELEMENT(#13045,1.);
#13038=DERIVED_UNIT_ELEMENT(#88485,-3.);
#13039=DERIVED_UNIT_ELEMENT(#13045,1.);
#13040=DERIVED_UNIT_ELEMENT(#88485,-3.);
#13041=DERIVED_UNIT_ELEMENT(#13045,1.);
#13042=DERIVED_UNIT_ELEMENT(#88485,-3.);
#13043=DERIVED_UNIT_ELEMENT(#13045,1.);
#13044=DERIVED_UNIT_ELEMENT(#88485,-3.);
#13045=(
MASS_UNIT()
NAMED_UNIT(*)
SI_UNIT(.KILO.,.GRAM.)
);
#13046=DERIVED_UNIT((#13027,#13028));
#13047=DERIVED_UNIT((#13029,#13030));
#13048=DERIVED_UNIT((#13031,#13032));
#13049=DERIVED_UNIT((#13033,#13034));
#13050=DERIVED_UNIT((#13035,#13036));
#13051=DERIVED_UNIT((#13037,#13038));
#13052=DERIVED_UNIT((#13039,#13040));
#13053=DERIVED_UNIT((#13041,#13042));
#13054=DERIVED_UNIT((#13043,#13044));
#13055=MEASURE_REPRESENTATION_ITEM('density measure',
POSITIVE_RATIO_MEASURE(7850.),#13046);
#13056=MEASURE_REPRESENTATION_ITEM('density measure',
POSITIVE_RATIO_MEASURE(7850.),#13047);
#13057=MEASURE_REPRESENTATION_ITEM('density measure',
POSITIVE_RATIO_MEASURE(7850.),#13048);
#13058=MEASURE_REPRESENTATION_ITEM('density measure',
POSITIVE_RATIO_MEASURE(7850.),#13049);
#13059=MEASURE_REPRESENTATION_ITEM('density measure',
POSITIVE_RATIO_MEASURE(7850.),#13050);
#13060=MEASURE_REPRESENTATION_ITEM('density measure',
POSITIVE_RATIO_MEASURE(7850.),#13051);
#13061=MEASURE_REPRESENTATION_ITEM('density measure',
POSITIVE_RATIO_MEASURE(7850.),#13052);
#13062=MEASURE_REPRESENTATION_ITEM('density measure',
POSITIVE_RATIO_MEASURE(7850.),#13053);
#13063=MEASURE_REPRESENTATION_ITEM('density measure',
POSITIVE_RATIO_MEASURE(7850.),#13054);
#13064=PROPERTY_DEFINITION_REPRESENTATION(#13109,#13082);
#13065=PROPERTY_DEFINITION_REPRESENTATION(#13110,#13083);
#13066=PROPERTY_DEFINITION_REPRESENTATION(#13111,#13084);
#13067=PROPERTY_DEFINITION_REPRESENTATION(#13112,#13085);
#13068=PROPERTY_DEFINITION_REPRESENTATION(#13113,#13086);
#13069=PROPERTY_DEFINITION_REPRESENTATION(#13114,#13087);
#13070=PROPERTY_DEFINITION_REPRESENTATION(#13115,#13088);
#13071=PROPERTY_DEFINITION_REPRESENTATION(#13116,#13089);
#13072=PROPERTY_DEFINITION_REPRESENTATION(#13117,#13090);
#13073=PROPERTY_DEFINITION_REPRESENTATION(#13118,#13091);
#13074=PROPERTY_DEFINITION_REPRESENTATION(#13119,#13092);
#13075=PROPERTY_DEFINITION_REPRESENTATION(#13120,#13093);
#13076=PROPERTY_DEFINITION_REPRESENTATION(#13121,#13094);
#13077=PROPERTY_DEFINITION_REPRESENTATION(#13122,#13095);
#13078=PROPERTY_DEFINITION_REPRESENTATION(#13123,#13096);
#13079=PROPERTY_DEFINITION_REPRESENTATION(#13124,#13097);
#13080=PROPERTY_DEFINITION_REPRESENTATION(#13125,#13098);
#13081=PROPERTY_DEFINITION_REPRESENTATION(#13126,#13099);
#13082=REPRESENTATION('material name',(#13100),#88474);
#13083=REPRESENTATION('density',(#13055),#88474);
#13084=REPRESENTATION('material name',(#13101),#88475);
#13085=REPRESENTATION('density',(#13056),#88475);
#13086=REPRESENTATION('material name',(#13102),#88476);
#13087=REPRESENTATION('density',(#13057),#88476);
#13088=REPRESENTATION('material name',(#13103),#88477);
#13089=REPRESENTATION('density',(#13058),#88477);
#13090=REPRESENTATION('material name',(#13104),#88478);
#13091=REPRESENTATION('density',(#13059),#88478);
#13092=REPRESENTATION('material name',(#13105),#88479);
#13093=REPRESENTATION('density',(#13060),#88479);
#13094=REPRESENTATION('material name',(#13106),#88480);
#13095=REPRESENTATION('density',(#13061),#88480);
#13096=REPRESENTATION('material name',(#13107),#88481);
#13097=REPRESENTATION('density',(#13062),#88481);
#13098=REPRESENTATION('material name',(#13108),#88482);
#13099=REPRESENTATION('density',(#13063),#88482);
#13100=DESCRIPTIVE_REPRESENTATION_ITEM('Steel','Steel');
#13101=DESCRIPTIVE_REPRESENTATION_ITEM('Steel','Steel');
#13102=DESCRIPTIVE_REPRESENTATION_ITEM('Steel','Steel');
#13103=DESCRIPTIVE_REPRESENTATION_ITEM('Steel','Steel');
#13104=DESCRIPTIVE_REPRESENTATION_ITEM('Steel','Steel');
#13105=DESCRIPTIVE_REPRESENTATION_ITEM('Steel','Steel');
#13106=DESCRIPTIVE_REPRESENTATION_ITEM('Steel','Steel');
#13107=DESCRIPTIVE_REPRESENTATION_ITEM('Steel','Steel');
#13108=DESCRIPTIVE_REPRESENTATION_ITEM('Steel','Steel');
#13109=PROPERTY_DEFINITION('material property','material name',#88531);
#13110=PROPERTY_DEFINITION('material property','density of part',#88531);
#13111=PROPERTY_DEFINITION('material property','material name',#88532);
#13112=PROPERTY_DEFINITION('material property','density of part',#88532);
#13113=PROPERTY_DEFINITION('material property','material name',#88533);
#13114=PROPERTY_DEFINITION('material property','density of part',#88533);
#13115=PROPERTY_DEFINITION('material property','material name',#88534);
#13116=PROPERTY_DEFINITION('material property','density of part',#88534);
#13117=PROPERTY_DEFINITION('material property','material name',#88535);
#13118=PROPERTY_DEFINITION('material property','density of part',#88535);
#13119=PROPERTY_DEFINITION('material property','material name',#88536);
#13120=PROPERTY_DEFINITION('material property','density of part',#88536);
#13121=PROPERTY_DEFINITION('material property','material name',#88537);
#13122=PROPERTY_DEFINITION('material property','density of part',#88537);
#13123=PROPERTY_DEFINITION('material property','material name',#88538);
#13124=PROPERTY_DEFINITION('material property','density of part',#88538);
#13125=PROPERTY_DEFINITION('material property','material name',#88539);
#13126=PROPERTY_DEFINITION('material property','density of part',#88539);
#13127=AXIS2_PLACEMENT_3D('',#17353,#14379,#14380);
#13128=AXIS2_PLACEMENT_3D('',#17354,#14381,#14382);
#13129=AXIS2_PLACEMENT_3D('',#17355,#14383,#14384);
#13130=AXIS2_PLACEMENT_3D('',#17369,#14386,#14387);
#13131=AXIS2_PLACEMENT_3D('',#17379,#14388,#14389);
#13132=AXIS2_PLACEMENT_3D('',#17749,#14391,#14392);
#13133=AXIS2_PLACEMENT_3D('',#18127,#14394,#14395);
#13134=AXIS2_PLACEMENT_3D('',#18583,#14397,#14398);
#13135=AXIS2_PLACEMENT_3D('',#18967,#14400,#14401);
#13136=AXIS2_PLACEMENT_3D('',#19419,#14403,#14404);
#13137=AXIS2_PLACEMENT_3D('',#19803,#14406,#14407);
#13138=AXIS2_PLACEMENT_3D('',#20101,#14409,#14410);
#13139=AXIS2_PLACEMENT_3D('',#20393,#14412,#14413);
#13140=AXIS2_PLACEMENT_3D('',#20689,#14415,#14416);
#13141=AXIS2_PLACEMENT_3D('',#20986,#14418,#14419);
#13142=AXIS2_PLACEMENT_3D('',#21008,#14421,#14422);
#13143=AXIS2_PLACEMENT_3D('',#21183,#14423,#14424);
#13144=AXIS2_PLACEMENT_3D('',#21197,#14426,#14427);
#13145=AXIS2_PLACEMENT_3D('',#21286,#14428,#14429);
#13146=AXIS2_PLACEMENT_3D('',#21478,#14431,#14432);
#13147=AXIS2_PLACEMENT_3D('',#21770,#14434,#14435);
#13148=AXIS2_PLACEMENT_3D('',#22065,#14437,#14438);
#13149=AXIS2_PLACEMENT_3D('',#22360,#14440,#14441);
#13150=AXIS2_PLACEMENT_3D('',#22656,#14443,#14444);
#13151=AXIS2_PLACEMENT_3D('',#23072,#14446,#14447);
#13152=AXIS2_PLACEMENT_3D('',#23261,#14449,#14450);
#13153=AXIS2_PLACEMENT_3D('',#23675,#14452,#14453);
#13154=AXIS2_PLACEMENT_3D('',#23976,#14455,#14456);
#13155=AXIS2_PLACEMENT_3D('',#24390,#14458,#14459);
#13156=AXIS2_PLACEMENT_3D('',#24562,#14461,#14462);
#13157=AXIS2_PLACEMENT_3D('',#24701,#14463,#14464);
#13158=AXIS2_PLACEMENT_3D('',#24880,#14465,#14466);
#13159=AXIS2_PLACEMENT_3D('',#26894,#14467,#14468);
#13160=AXIS2_PLACEMENT_3D('',#26897,#14469,#14470);
#13161=AXIS2_PLACEMENT_3D('',#26901,#14472,#14473);
#13162=AXIS2_PLACEMENT_3D('',#26905,#14475,#14476);
#13163=AXIS2_PLACEMENT_3D('',#26909,#14478,#14479);
#13164=AXIS2_PLACEMENT_3D('',#26913,#14481,#14482);
#13165=AXIS2_PLACEMENT_3D('',#26917,#14484,#14485);
#13166=AXIS2_PLACEMENT_3D('',#26921,#14487,#14488);
#13167=AXIS2_PLACEMENT_3D('',#26925,#14490,#14491);
#13168=AXIS2_PLACEMENT_3D('',#26929,#14493,#14494);
#13169=AXIS2_PLACEMENT_3D('',#26933,#14496,#14497);
#13170=AXIS2_PLACEMENT_3D('',#26937,#14499,#14500);
#13171=AXIS2_PLACEMENT_3D('',#26941,#14502,#14503);
#13172=AXIS2_PLACEMENT_3D('',#26945,#14505,#14506);
#13173=AXIS2_PLACEMENT_3D('',#26949,#14508,#14509);
#13174=AXIS2_PLACEMENT_3D('',#26953,#14511,#14512);
#13175=AXIS2_PLACEMENT_3D('',#26957,#14514,#14515);
#13176=AXIS2_PLACEMENT_3D('',#26961,#14517,#14518);
#13177=AXIS2_PLACEMENT_3D('',#26965,#14520,#14521);
#13178=AXIS2_PLACEMENT_3D('',#26969,#14523,#14524);
#13179=AXIS2_PLACEMENT_3D('',#26973,#14526,#14527);
#13180=AXIS2_PLACEMENT_3D('',#26977,#14529,#14530);
#13181=AXIS2_PLACEMENT_3D('',#26981,#14532,#14533);
#13182=AXIS2_PLACEMENT_3D('',#26985,#14535,#14536);
#13183=AXIS2_PLACEMENT_3D('',#26989,#14538,#14539);
#13184=AXIS2_PLACEMENT_3D('',#26993,#14541,#14542);
#13185=AXIS2_PLACEMENT_3D('',#26997,#14544,#14545);
#13186=AXIS2_PLACEMENT_3D('',#27001,#14547,#14548);
#13187=AXIS2_PLACEMENT_3D('',#27005,#14550,#14551);
#13188=AXIS2_PLACEMENT_3D('',#27009,#14553,#14554);
#13189=AXIS2_PLACEMENT_3D('',#27013,#14556,#14557);
#13190=AXIS2_PLACEMENT_3D('',#27017,#14559,#14560);
#13191=AXIS2_PLACEMENT_3D('',#27021,#14562,#14563);
#13192=AXIS2_PLACEMENT_3D('',#27025,#14565,#14566);
#13193=AXIS2_PLACEMENT_3D('',#27029,#14568,#14569);
#13194=AXIS2_PLACEMENT_3D('',#27033,#14571,#14572);
#13195=AXIS2_PLACEMENT_3D('',#27037,#14574,#14575);
#13196=AXIS2_PLACEMENT_3D('',#27039,#14577,#14578);
#13197=AXIS2_PLACEMENT_3D('',#27044,#14580,#14581);
#13198=AXIS2_PLACEMENT_3D('',#27047,#14583,#14584);
#13199=AXIS2_PLACEMENT_3D('',#27048,#14585,#14586);
#13200=AXIS2_PLACEMENT_3D('',#27053,#14588,#14589);
#13201=AXIS2_PLACEMENT_3D('',#27056,#14591,#14592);
#13202=AXIS2_PLACEMENT_3D('',#27057,#14593,#14594);
#13203=AXIS2_PLACEMENT_3D('',#27062,#14596,#14597);
#13204=AXIS2_PLACEMENT_3D('',#27065,#14599,#14600);
#13205=AXIS2_PLACEMENT_3D('',#27066,#14601,#14602);
#13206=AXIS2_PLACEMENT_3D('',#27071,#14604,#14605);
#13207=AXIS2_PLACEMENT_3D('',#27074,#14607,#14608);
#13208=AXIS2_PLACEMENT_3D('',#27075,#14609,#14610);
#13209=AXIS2_PLACEMENT_3D('',#27080,#14612,#14613);
#13210=AXIS2_PLACEMENT_3D('',#27083,#14615,#14616);
#13211=AXIS2_PLACEMENT_3D('',#27084,#14617,#14618);
#13212=AXIS2_PLACEMENT_3D('',#27089,#14620,#14621);
#13213=AXIS2_PLACEMENT_3D('',#27092,#14623,#14624);
#13214=AXIS2_PLACEMENT_3D('',#27093,#14625,#14626);
#13215=AXIS2_PLACEMENT_3D('',#27098,#14628,#14629);
#13216=AXIS2_PLACEMENT_3D('',#27101,#14631,#14632);
#13217=AXIS2_PLACEMENT_3D('',#27102,#14633,#14634);
#13218=AXIS2_PLACEMENT_3D('',#27107,#14636,#14637);
#13219=AXIS2_PLACEMENT_3D('',#27110,#14639,#14640);
#13220=AXIS2_PLACEMENT_3D('',#27111,#14641,#14642);
#13221=AXIS2_PLACEMENT_3D('',#27116,#14644,#14645);
#13222=AXIS2_PLACEMENT_3D('',#27119,#14647,#14648);
#13223=AXIS2_PLACEMENT_3D('',#27120,#14649,#14650);
#13224=AXIS2_PLACEMENT_3D('',#27125,#14652,#14653);
#13225=AXIS2_PLACEMENT_3D('',#27128,#14655,#14656);
#13226=AXIS2_PLACEMENT_3D('',#27129,#14657,#14658);
#13227=AXIS2_PLACEMENT_3D('',#27134,#14660,#14661);
#13228=AXIS2_PLACEMENT_3D('',#27137,#14663,#14664);
#13229=AXIS2_PLACEMENT_3D('',#27138,#14665,#14666);
#13230=AXIS2_PLACEMENT_3D('',#27143,#14668,#14669);
#13231=AXIS2_PLACEMENT_3D('',#27146,#14671,#14672);
#13232=AXIS2_PLACEMENT_3D('',#27147,#14673,#14674);
#13233=AXIS2_PLACEMENT_3D('',#27152,#14676,#14677);
#13234=AXIS2_PLACEMENT_3D('',#27155,#14679,#14680);
#13235=AXIS2_PLACEMENT_3D('',#27156,#14681,#14682);
#13236=AXIS2_PLACEMENT_3D('',#27161,#14684,#14685);
#13237=AXIS2_PLACEMENT_3D('',#27164,#14687,#14688);
#13238=AXIS2_PLACEMENT_3D('',#27165,#14689,#14690);
#13239=AXIS2_PLACEMENT_3D('',#27170,#14692,#14693);
#13240=AXIS2_PLACEMENT_3D('',#27173,#14695,#14696);
#13241=AXIS2_PLACEMENT_3D('',#27174,#14697,#14698);
#13242=AXIS2_PLACEMENT_3D('',#27179,#14700,#14701);
#13243=AXIS2_PLACEMENT_3D('',#27182,#14703,#14704);
#13244=AXIS2_PLACEMENT_3D('',#27183,#14705,#14706);
#13245=AXIS2_PLACEMENT_3D('',#27188,#14708,#14709);
#13246=AXIS2_PLACEMENT_3D('',#27191,#14711,#14712);
#13247=AXIS2_PLACEMENT_3D('',#27192,#14713,#14714);
#13248=AXIS2_PLACEMENT_3D('',#27197,#14716,#14717);
#13249=AXIS2_PLACEMENT_3D('',#27200,#14719,#14720);
#13250=AXIS2_PLACEMENT_3D('',#27201,#14721,#14722);
#13251=AXIS2_PLACEMENT_3D('',#27203,#14723,#14724);
#13252=AXIS2_PLACEMENT_3D('',#27205,#14725,#14726);
#13253=AXIS2_PLACEMENT_3D('',#27228,#14729,#14730);
#13254=AXIS2_PLACEMENT_3D('',#27230,#14731,#14732);
#13255=AXIS2_PLACEMENT_3D('',#27232,#14733,#14734);
#13256=AXIS2_PLACEMENT_3D('',#27255,#14737,#14738);
#13257=AXIS2_PLACEMENT_3D('',#27257,#14739,#14740);
#13258=AXIS2_PLACEMENT_3D('',#27259,#14741,#14742);
#13259=AXIS2_PLACEMENT_3D('',#27280,#14745,#14746);
#13260=AXIS2_PLACEMENT_3D('',#27282,#14747,#14748);
#13261=AXIS2_PLACEMENT_3D('',#27284,#14749,#14750);
#13262=AXIS2_PLACEMENT_3D('',#27307,#14753,#14754);
#13263=AXIS2_PLACEMENT_3D('',#27309,#14755,#14756);
#13264=AXIS2_PLACEMENT_3D('',#27311,#14757,#14758);
#13265=AXIS2_PLACEMENT_3D('',#27334,#14761,#14762);
#13266=AXIS2_PLACEMENT_3D('',#27336,#14763,#14764);
#13267=AXIS2_PLACEMENT_3D('',#27338,#14765,#14766);
#13268=AXIS2_PLACEMENT_3D('',#27361,#14769,#14770);
#13269=AXIS2_PLACEMENT_3D('',#27363,#14771,#14772);
#13270=AXIS2_PLACEMENT_3D('',#27365,#14773,#14774);
#13271=AXIS2_PLACEMENT_3D('',#27386,#14777,#14778);
#13272=AXIS2_PLACEMENT_3D('',#27388,#14779,#14780);
#13273=AXIS2_PLACEMENT_3D('',#27390,#14781,#14782);
#13274=AXIS2_PLACEMENT_3D('',#27413,#14785,#14786);
#13275=AXIS2_PLACEMENT_3D('',#27415,#14787,#14788);
#13276=AXIS2_PLACEMENT_3D('',#27417,#14789,#14790);
#13277=AXIS2_PLACEMENT_3D('',#27440,#14793,#14794);
#13278=AXIS2_PLACEMENT_3D('',#27442,#14795,#14796);
#13279=AXIS2_PLACEMENT_3D('',#27444,#14797,#14798);
#13280=AXIS2_PLACEMENT_3D('',#27467,#14801,#14802);
#13281=AXIS2_PLACEMENT_3D('',#27469,#14803,#14804);
#13282=AXIS2_PLACEMENT_3D('',#27471,#14805,#14806);
#13283=AXIS2_PLACEMENT_3D('',#27492,#14809,#14810);
#13284=AXIS2_PLACEMENT_3D('',#27494,#14811,#14812);
#13285=AXIS2_PLACEMENT_3D('',#27496,#14813,#14814);
#13286=AXIS2_PLACEMENT_3D('',#27519,#14817,#14818);
#13287=AXIS2_PLACEMENT_3D('',#27521,#14819,#14820);
#13288=AXIS2_PLACEMENT_3D('',#27523,#14821,#14822);
#13289=AXIS2_PLACEMENT_3D('',#27546,#14825,#14826);
#13290=AXIS2_PLACEMENT_3D('',#27548,#14827,#14828);
#13291=AXIS2_PLACEMENT_3D('',#27550,#14829,#14830);
#13292=AXIS2_PLACEMENT_3D('',#27573,#14833,#14834);
#13293=AXIS2_PLACEMENT_3D('',#27575,#14835,#14836);
#13294=AXIS2_PLACEMENT_3D('',#27577,#14837,#14838);
#13295=AXIS2_PLACEMENT_3D('',#27600,#14841,#14842);
#13296=AXIS2_PLACEMENT_3D('',#27602,#14843,#14844);
#13297=AXIS2_PLACEMENT_3D('',#27604,#14845,#14846);
#13298=AXIS2_PLACEMENT_3D('',#27627,#14849,#14850);
#13299=AXIS2_PLACEMENT_3D('',#27629,#14851,#14852);
#13300=AXIS2_PLACEMENT_3D('',#27631,#14853,#14854);
#13301=AXIS2_PLACEMENT_3D('',#27654,#14857,#14858);
#13302=AXIS2_PLACEMENT_3D('',#27656,#14859,#14860);
#13303=AXIS2_PLACEMENT_3D('',#27658,#14861,#14862);
#13304=AXIS2_PLACEMENT_3D('',#27681,#14865,#14866);
#13305=AXIS2_PLACEMENT_3D('',#27684,#14867,#14868);
#13306=AXIS2_PLACEMENT_3D('',#27686,#14869,#14870);
#13307=AXIS2_PLACEMENT_3D('',#27688,#14871,#14872);
#13308=AXIS2_PLACEMENT_3D('',#27701,#14874,#14875);
#13309=AXIS2_PLACEMENT_3D('',#27714,#14877,#14878);
#13310=AXIS2_PLACEMENT_3D('',#27717,#14879,#14880);
#13311=AXIS2_PLACEMENT_3D('',#27719,#14881,#14882);
#13312=AXIS2_PLACEMENT_3D('',#27721,#14883,#14884);
#13313=AXIS2_PLACEMENT_3D('',#27736,#14886,#14887);
#13314=AXIS2_PLACEMENT_3D('',#27747,#14889,#14890);
#13315=AXIS2_PLACEMENT_3D('',#27750,#14891,#14892);
#13316=AXIS2_PLACEMENT_3D('',#27752,#14893,#14894);
#13317=AXIS2_PLACEMENT_3D('',#27754,#14895,#14896);
#13318=AXIS2_PLACEMENT_3D('',#27769,#14898,#14899);
#13319=AXIS2_PLACEMENT_3D('',#27782,#14901,#14902);
#13320=AXIS2_PLACEMENT_3D('',#27785,#14903,#14904);
#13321=AXIS2_PLACEMENT_3D('',#27787,#14905,#14906);
#13322=AXIS2_PLACEMENT_3D('',#27789,#14907,#14908);
#13323=AXIS2_PLACEMENT_3D('',#27802,#14910,#14911);
#13324=AXIS2_PLACEMENT_3D('',#27813,#14913,#14914);
#13325=AXIS2_PLACEMENT_3D('',#27816,#14915,#14916);
#13326=AXIS2_PLACEMENT_3D('',#27818,#14917,#14918);
#13327=AXIS2_PLACEMENT_3D('',#27820,#14919,#14920);
#13328=AXIS2_PLACEMENT_3D('',#27835,#14922,#14923);
#13329=AXIS2_PLACEMENT_3D('',#27848,#14925,#14926);
#13330=AXIS2_PLACEMENT_3D('',#27851,#14927,#14928);
#13331=AXIS2_PLACEMENT_3D('',#27853,#14929,#14930);
#13332=AXIS2_PLACEMENT_3D('',#27855,#14931,#14932);
#13333=AXIS2_PLACEMENT_3D('',#27870,#14934,#14935);
#13334=AXIS2_PLACEMENT_3D('',#27883,#14937,#14938);
#13335=AXIS2_PLACEMENT_3D('',#27886,#14939,#14940);
#13336=AXIS2_PLACEMENT_3D('',#27888,#14941,#14942);
#13337=AXIS2_PLACEMENT_3D('',#27890,#14943,#14944);
#13338=AXIS2_PLACEMENT_3D('',#27905,#14946,#14947);
#13339=AXIS2_PLACEMENT_3D('',#27916,#14949,#14950);
#13340=AXIS2_PLACEMENT_3D('',#27919,#14951,#14952);
#13341=AXIS2_PLACEMENT_3D('',#27921,#14953,#14954);
#13342=AXIS2_PLACEMENT_3D('',#27923,#14955,#14956);
#13343=AXIS2_PLACEMENT_3D('',#27936,#14958,#14959);
#13344=AXIS2_PLACEMENT_3D('',#27949,#14961,#14962);
#13345=AXIS2_PLACEMENT_3D('',#27952,#14963,#14964);
#13346=AXIS2_PLACEMENT_3D('',#27954,#14965,#14966);
#13347=AXIS2_PLACEMENT_3D('',#27956,#14967,#14968);
#13348=AXIS2_PLACEMENT_3D('',#27971,#14970,#14971);
#13349=AXIS2_PLACEMENT_3D('',#27984,#14973,#14974);
#13350=AXIS2_PLACEMENT_3D('',#27987,#14975,#14976);
#13351=AXIS2_PLACEMENT_3D('',#27989,#14977,#14978);
#13352=AXIS2_PLACEMENT_3D('',#27991,#14979,#14980);
#13353=AXIS2_PLACEMENT_3D('',#28006,#14982,#14983);
#13354=AXIS2_PLACEMENT_3D('',#28019,#14985,#14986);
#13355=AXIS2_PLACEMENT_3D('',#28022,#14987,#14988);
#13356=AXIS2_PLACEMENT_3D('',#28024,#14989,#14990);
#13357=AXIS2_PLACEMENT_3D('',#28026,#14991,#14992);
#13358=AXIS2_PLACEMENT_3D('',#28041,#14994,#14995);
#13359=AXIS2_PLACEMENT_3D('',#28052,#14997,#14998);
#13360=AXIS2_PLACEMENT_3D('',#28055,#14999,#15000);
#13361=AXIS2_PLACEMENT_3D('',#28057,#15001,#15002);
#13362=AXIS2_PLACEMENT_3D('',#28059,#15003,#15004);
#13363=AXIS2_PLACEMENT_3D('',#28072,#15006,#15007);
#13364=AXIS2_PLACEMENT_3D('',#28085,#15009,#15010);
#13365=AXIS2_PLACEMENT_3D('',#28088,#15011,#15012);
#13366=AXIS2_PLACEMENT_3D('',#28090,#15013,#15014);
#13367=AXIS2_PLACEMENT_3D('',#28092,#15015,#15016);
#13368=AXIS2_PLACEMENT_3D('',#28107,#15018,#15019);
#13369=AXIS2_PLACEMENT_3D('',#28118,#15021,#15022);
#13370=AXIS2_PLACEMENT_3D('',#28121,#15023,#15024);
#13371=AXIS2_PLACEMENT_3D('',#28123,#15025,#15026);
#13372=AXIS2_PLACEMENT_3D('',#28125,#15027,#15028);
#13373=AXIS2_PLACEMENT_3D('',#28140,#15030,#15031);
#13374=AXIS2_PLACEMENT_3D('',#28153,#15033,#15034);
#13375=AXIS2_PLACEMENT_3D('',#28156,#15035,#15036);
#13376=AXIS2_PLACEMENT_3D('',#28158,#15037,#15038);
#13377=AXIS2_PLACEMENT_3D('',#28160,#15039,#15040);
#13378=AXIS2_PLACEMENT_3D('',#28175,#15042,#15043);
#13379=AXIS2_PLACEMENT_3D('',#28188,#15045,#15046);
#13380=AXIS2_PLACEMENT_3D('',#28191,#15047,#15048);
#13381=AXIS2_PLACEMENT_3D('',#28193,#15049,#15050);
#13382=AXIS2_PLACEMENT_3D('',#28195,#15051,#15052);
#13383=AXIS2_PLACEMENT_3D('',#28210,#15054,#15055);
#13384=AXIS2_PLACEMENT_3D('',#28221,#15057,#15058);
#13385=AXIS2_PLACEMENT_3D('',#28224,#15059,#15060);
#13386=AXIS2_PLACEMENT_3D('',#28226,#15061,#15062);
#13387=AXIS2_PLACEMENT_3D('',#28228,#15063,#15064);
#13388=AXIS2_PLACEMENT_3D('',#28241,#15066,#15067);
#13389=AXIS2_PLACEMENT_3D('',#28254,#15069,#15070);
#13390=AXIS2_PLACEMENT_3D('',#28257,#15071,#15072);
#13391=AXIS2_PLACEMENT_3D('',#28259,#15073,#15074);
#13392=AXIS2_PLACEMENT_3D('',#28261,#15075,#15076);
#13393=AXIS2_PLACEMENT_3D('',#28274,#15078,#15079);
#13394=AXIS2_PLACEMENT_3D('',#28285,#15081,#15082);
#13395=AXIS2_PLACEMENT_3D('',#28290,#15085,#15086);
#13396=AXIS2_PLACEMENT_3D('',#28291,#15087,#15088);
#13397=AXIS2_PLACEMENT_3D('',#28296,#15091,#15092);
#13398=AXIS2_PLACEMENT_3D('',#28297,#15093,#15094);
#13399=AXIS2_PLACEMENT_3D('',#28302,#15097,#15098);
#13400=AXIS2_PLACEMENT_3D('',#28303,#15099,#15100);
#13401=AXIS2_PLACEMENT_3D('',#28308,#15103,#15104);
#13402=AXIS2_PLACEMENT_3D('',#28309,#15105,#15106);
#13403=AXIS2_PLACEMENT_3D('',#28314,#15109,#15110);
#13404=AXIS2_PLACEMENT_3D('',#28315,#15111,#15112);
#13405=AXIS2_PLACEMENT_3D('',#28320,#15115,#15116);
#13406=AXIS2_PLACEMENT_3D('',#28321,#15117,#15118);
#13407=AXIS2_PLACEMENT_3D('',#28326,#15121,#15122);
#13408=AXIS2_PLACEMENT_3D('',#28327,#15123,#15124);
#13409=AXIS2_PLACEMENT_3D('',#28332,#15127,#15128);
#13410=AXIS2_PLACEMENT_3D('',#28333,#15129,#15130);
#13411=AXIS2_PLACEMENT_3D('',#28338,#15133,#15134);
#13412=AXIS2_PLACEMENT_3D('',#28339,#15135,#15136);
#13413=AXIS2_PLACEMENT_3D('',#28344,#15139,#15140);
#13414=AXIS2_PLACEMENT_3D('',#28345,#15141,#15142);
#13415=AXIS2_PLACEMENT_3D('',#28350,#15145,#15146);
#13416=AXIS2_PLACEMENT_3D('',#28351,#15147,#15148);
#13417=AXIS2_PLACEMENT_3D('',#28356,#15151,#15152);
#13418=AXIS2_PLACEMENT_3D('',#28357,#15153,#15154);
#13419=AXIS2_PLACEMENT_3D('',#28362,#15157,#15158);
#13420=AXIS2_PLACEMENT_3D('',#28363,#15159,#15160);
#13421=AXIS2_PLACEMENT_3D('',#28368,#15163,#15164);
#13422=AXIS2_PLACEMENT_3D('',#28369,#15165,#15166);
#13423=AXIS2_PLACEMENT_3D('',#28374,#15169,#15170);
#13424=AXIS2_PLACEMENT_3D('',#28375,#15171,#15172);
#13425=AXIS2_PLACEMENT_3D('',#28380,#15175,#15176);
#13426=AXIS2_PLACEMENT_3D('',#28381,#15177,#15178);
#13427=AXIS2_PLACEMENT_3D('',#28386,#15181,#15182);
#13428=AXIS2_PLACEMENT_3D('',#28387,#15183,#15184);
#13429=AXIS2_PLACEMENT_3D('',#28392,#15187,#15188);
#13430=AXIS2_PLACEMENT_3D('',#28393,#15189,#15190);
#13431=AXIS2_PLACEMENT_3D('',#28396,#15191,#15192);
#13432=AXIS2_PLACEMENT_3D('',#28398,#15193,#15194);
#13433=AXIS2_PLACEMENT_3D('',#28406,#15195,#15196);
#13434=AXIS2_PLACEMENT_3D('',#28407,#15197,#15198);
#13435=AXIS2_PLACEMENT_3D('',#28410,#15199,#15200);
#13436=AXIS2_PLACEMENT_3D('',#28412,#15201,#15202);
#13437=AXIS2_PLACEMENT_3D('',#28414,#15203,#15204);
#13438=AXIS2_PLACEMENT_3D('',#28415,#15205,#15206);
#13439=AXIS2_PLACEMENT_3D('',#28416,#15207,#15208);
#13440=AXIS2_PLACEMENT_3D('',#28419,#15209,#15210);
#13441=AXIS2_PLACEMENT_3D('',#28421,#15211,#15212);
#13442=AXIS2_PLACEMENT_3D('',#28423,#15213,#15214);
#13443=AXIS2_PLACEMENT_3D('',#28424,#15215,#15216);
#13444=AXIS2_PLACEMENT_3D('',#28425,#15217,#15218);
#13445=AXIS2_PLACEMENT_3D('',#28428,#15219,#15220);
#13446=AXIS2_PLACEMENT_3D('',#28430,#15221,#15222);
#13447=AXIS2_PLACEMENT_3D('',#28438,#15223,#15224);
#13448=AXIS2_PLACEMENT_3D('',#28439,#15225,#15226);
#13449=AXIS2_PLACEMENT_3D('',#28442,#15227,#15228);
#13450=AXIS2_PLACEMENT_3D('',#28444,#15229,#15230);
#13451=AXIS2_PLACEMENT_3D('',#28446,#15231,#15232);
#13452=AXIS2_PLACEMENT_3D('',#28447,#15233,#15234);
#13453=AXIS2_PLACEMENT_3D('',#28448,#15235,#15236);
#13454=AXIS2_PLACEMENT_3D('',#28451,#15237,#15238);
#13455=AXIS2_PLACEMENT_3D('',#28453,#15239,#15240);
#13456=AXIS2_PLACEMENT_3D('',#28455,#15241,#15242);
#13457=AXIS2_PLACEMENT_3D('',#28456,#15243,#15244);
#13458=AXIS2_PLACEMENT_3D('',#28457,#15245,#15246);
#13459=AXIS2_PLACEMENT_3D('',#28460,#15247,#15248);
#13460=AXIS2_PLACEMENT_3D('',#28462,#15249,#15250);
#13461=AXIS2_PLACEMENT_3D('',#28464,#15251,#15252);
#13462=AXIS2_PLACEMENT_3D('',#28465,#15253,#15254);
#13463=AXIS2_PLACEMENT_3D('',#28466,#15255,#15256);
#13464=AXIS2_PLACEMENT_3D('',#28469,#15257,#15258);
#13465=AXIS2_PLACEMENT_3D('',#28471,#15259,#15260);
#13466=AXIS2_PLACEMENT_3D('',#28479,#15261,#15262);
#13467=AXIS2_PLACEMENT_3D('',#28480,#15263,#15264);
#13468=AXIS2_PLACEMENT_3D('',#28483,#15265,#15266);
#13469=AXIS2_PLACEMENT_3D('',#28485,#15267,#15268);
#13470=AXIS2_PLACEMENT_3D('',#28487,#15269,#15270);
#13471=AXIS2_PLACEMENT_3D('',#28488,#15271,#15272);
#13472=AXIS2_PLACEMENT_3D('',#28489,#15273,#15274);
#13473=AXIS2_PLACEMENT_3D('',#28492,#15275,#15276);
#13474=AXIS2_PLACEMENT_3D('',#28494,#15277,#15278);
#13475=AXIS2_PLACEMENT_3D('',#28496,#15279,#15280);
#13476=AXIS2_PLACEMENT_3D('',#28497,#15281,#15282);
#13477=AXIS2_PLACEMENT_3D('',#28498,#15283,#15284);
#13478=AXIS2_PLACEMENT_3D('',#28501,#15285,#15286);
#13479=AXIS2_PLACEMENT_3D('',#28503,#15287,#15288);
#13480=AXIS2_PLACEMENT_3D('',#28505,#15289,#15290);
#13481=AXIS2_PLACEMENT_3D('',#28506,#15291,#15292);
#13482=AXIS2_PLACEMENT_3D('',#28507,#15293,#15294);
#13483=AXIS2_PLACEMENT_3D('',#28510,#15295,#15296);
#13484=AXIS2_PLACEMENT_3D('',#28512,#15297,#15298);
#13485=AXIS2_PLACEMENT_3D('',#28520,#15299,#15300);
#13486=AXIS2_PLACEMENT_3D('',#28521,#15301,#15302);
#13487=AXIS2_PLACEMENT_3D('',#28524,#15303,#15304);
#13488=AXIS2_PLACEMENT_3D('',#28526,#15305,#15306);
#13489=AXIS2_PLACEMENT_3D('',#28528,#15307,#15308);
#13490=AXIS2_PLACEMENT_3D('',#28529,#15309,#15310);
#13491=AXIS2_PLACEMENT_3D('',#28530,#15311,#15312);
#13492=AXIS2_PLACEMENT_3D('',#28533,#15313,#15314);
#13493=AXIS2_PLACEMENT_3D('',#28535,#15315,#15316);
#13494=AXIS2_PLACEMENT_3D('',#28537,#15317,#15318);
#13495=AXIS2_PLACEMENT_3D('',#28538,#15319,#15320);
#13496=AXIS2_PLACEMENT_3D('',#28539,#15321,#15322);
#13497=AXIS2_PLACEMENT_3D('',#28542,#15323,#15324);
#13498=AXIS2_PLACEMENT_3D('',#28544,#15325,#15326);
#13499=AXIS2_PLACEMENT_3D('',#28546,#15327,#15328);
#13500=AXIS2_PLACEMENT_3D('',#28547,#15329,#15330);
#13501=AXIS2_PLACEMENT_3D('',#28548,#15331,#15332);
#13502=AXIS2_PLACEMENT_3D('',#28551,#15333,#15334);
#13503=AXIS2_PLACEMENT_3D('',#28553,#15335,#15336);
#13504=AXIS2_PLACEMENT_3D('',#28555,#15337,#15338);
#13505=AXIS2_PLACEMENT_3D('',#28556,#15339,#15340);
#13506=AXIS2_PLACEMENT_3D('',#28557,#15341,#15342);
#13507=AXIS2_PLACEMENT_3D('',#28560,#15343,#15344);
#13508=AXIS2_PLACEMENT_3D('',#28562,#15345,#15346);
#13509=AXIS2_PLACEMENT_3D('',#28570,#15347,#15348);
#13510=AXIS2_PLACEMENT_3D('',#28571,#15349,#15350);
#13511=AXIS2_PLACEMENT_3D('',#28574,#15351,#15352);
#13512=AXIS2_PLACEMENT_3D('',#28576,#15353,#15354);
#13513=AXIS2_PLACEMENT_3D('',#28584,#15355,#15356);
#13514=AXIS2_PLACEMENT_3D('',#28585,#15357,#15358);
#13515=AXIS2_PLACEMENT_3D('',#28595,#15359,#15360);
#13516=AXIS2_PLACEMENT_3D('',#28597,#15361,#15362);
#13517=AXIS2_PLACEMENT_3D('',#28598,#15363,#15364);
#13518=AXIS2_PLACEMENT_3D('',#28599,#15365,#15366);
#13519=AXIS2_PLACEMENT_3D('',#28609,#15367,#15368);
#13520=AXIS2_PLACEMENT_3D('',#28611,#15369,#15370);
#13521=AXIS2_PLACEMENT_3D('',#28612,#15371,#15372);
#13522=AXIS2_PLACEMENT_3D('',#28613,#15373,#15374);
#13523=AXIS2_PLACEMENT_3D('',#28623,#15375,#15376);
#13524=AXIS2_PLACEMENT_3D('',#28625,#15377,#15378);
#13525=AXIS2_PLACEMENT_3D('',#28626,#15379,#15380);
#13526=AXIS2_PLACEMENT_3D('',#28627,#15381,#15382);
#13527=AXIS2_PLACEMENT_3D('',#28637,#15383,#15384);
#13528=AXIS2_PLACEMENT_3D('',#28639,#15385,#15386);
#13529=AXIS2_PLACEMENT_3D('',#28640,#15387,#15388);
#13530=AXIS2_PLACEMENT_3D('',#28641,#15389,#15390);
#13531=AXIS2_PLACEMENT_3D('',#28651,#15391,#15392);
#13532=AXIS2_PLACEMENT_3D('',#28653,#15393,#15394);
#13533=AXIS2_PLACEMENT_3D('',#28654,#15395,#15396);
#13534=AXIS2_PLACEMENT_3D('',#28655,#15397,#15398);
#13535=AXIS2_PLACEMENT_3D('',#28665,#15399,#15400);
#13536=AXIS2_PLACEMENT_3D('',#28667,#15401,#15402);
#13537=AXIS2_PLACEMENT_3D('',#28668,#15403,#15404);
#13538=AXIS2_PLACEMENT_3D('',#28669,#15405,#15406);
#13539=AXIS2_PLACEMENT_3D('',#28679,#15407,#15408);
#13540=AXIS2_PLACEMENT_3D('',#28681,#15409,#15410);
#13541=AXIS2_PLACEMENT_3D('',#28682,#15411,#15412);
#13542=AXIS2_PLACEMENT_3D('',#28683,#15413,#15414);
#13543=AXIS2_PLACEMENT_3D('',#28693,#15415,#15416);
#13544=AXIS2_PLACEMENT_3D('',#28695,#15417,#15418);
#13545=AXIS2_PLACEMENT_3D('',#28696,#15419,#15420);
#13546=AXIS2_PLACEMENT_3D('',#28697,#15421,#15422);
#13547=AXIS2_PLACEMENT_3D('',#28707,#15423,#15424);
#13548=AXIS2_PLACEMENT_3D('',#28709,#15425,#15426);
#13549=AXIS2_PLACEMENT_3D('',#28710,#15427,#15428);
#13550=AXIS2_PLACEMENT_3D('',#28711,#15429,#15430);
#13551=AXIS2_PLACEMENT_3D('',#28721,#15431,#15432);
#13552=AXIS2_PLACEMENT_3D('',#28723,#15433,#15434);
#13553=AXIS2_PLACEMENT_3D('',#28724,#15435,#15436);
#13554=AXIS2_PLACEMENT_3D('',#28725,#15437,#15438);
#13555=AXIS2_PLACEMENT_3D('',#28735,#15439,#15440);
#13556=AXIS2_PLACEMENT_3D('',#28737,#15441,#15442);
#13557=AXIS2_PLACEMENT_3D('',#28738,#15443,#15444);
#13558=AXIS2_PLACEMENT_3D('',#28739,#15445,#15446);
#13559=AXIS2_PLACEMENT_3D('',#28749,#15447,#15448);
#13560=AXIS2_PLACEMENT_3D('',#28751,#15449,#15450);
#13561=AXIS2_PLACEMENT_3D('',#28752,#15451,#15452);
#13562=AXIS2_PLACEMENT_3D('',#28753,#15453,#15454);
#13563=AXIS2_PLACEMENT_3D('',#28763,#15455,#15456);
#13564=AXIS2_PLACEMENT_3D('',#28765,#15457,#15458);
#13565=AXIS2_PLACEMENT_3D('',#28766,#15459,#15460);
#13566=AXIS2_PLACEMENT_3D('',#28767,#15461,#15462);
#13567=AXIS2_PLACEMENT_3D('',#28777,#15463,#15464);
#13568=AXIS2_PLACEMENT_3D('',#28779,#15465,#15466);
#13569=AXIS2_PLACEMENT_3D('',#28780,#15467,#15468);
#13570=AXIS2_PLACEMENT_3D('',#28781,#15469,#15470);
#13571=AXIS2_PLACEMENT_3D('',#28791,#15471,#15472);
#13572=AXIS2_PLACEMENT_3D('',#28793,#15473,#15474);
#13573=AXIS2_PLACEMENT_3D('',#28794,#15475,#15476);
#13574=AXIS2_PLACEMENT_3D('',#28795,#15477,#15478);
#13575=AXIS2_PLACEMENT_3D('',#28805,#15479,#15480);
#13576=AXIS2_PLACEMENT_3D('',#28807,#15481,#15482);
#13577=AXIS2_PLACEMENT_3D('',#28808,#15483,#15484);
#13578=AXIS2_PLACEMENT_3D('',#28809,#15485,#15486);
#13579=AXIS2_PLACEMENT_3D('',#28819,#15487,#15488);
#13580=AXIS2_PLACEMENT_3D('',#28821,#15489,#15490);
#13581=AXIS2_PLACEMENT_3D('',#28822,#15491,#15492);
#13582=AXIS2_PLACEMENT_3D('',#28823,#15493,#15494);
#13583=AXIS2_PLACEMENT_3D('',#28833,#15495,#15496);
#13584=AXIS2_PLACEMENT_3D('',#28835,#15497,#15498);
#13585=AXIS2_PLACEMENT_3D('',#28836,#15499,#15500);
#13586=AXIS2_PLACEMENT_3D('',#28837,#15501,#15502);
#13587=AXIS2_PLACEMENT_3D('',#28866,#15503,#15504);
#13588=AXIS2_PLACEMENT_3D('',#28895,#15505,#15506);
#13589=AXIS2_PLACEMENT_3D('',#28924,#15507,#15508);
#13590=AXIS2_PLACEMENT_3D('',#28953,#15509,#15510);
#13591=AXIS2_PLACEMENT_3D('',#28982,#15511,#15512);
#13592=AXIS2_PLACEMENT_3D('',#29011,#15513,#15514);
#13593=AXIS2_PLACEMENT_3D('',#29040,#15515,#15516);
#13594=AXIS2_PLACEMENT_3D('',#29069,#15517,#15518);
#13595=AXIS2_PLACEMENT_3D('',#29098,#15519,#15520);
#13596=AXIS2_PLACEMENT_3D('',#29127,#15521,#15522);
#13597=AXIS2_PLACEMENT_3D('',#29156,#15523,#15524);
#13598=AXIS2_PLACEMENT_3D('',#29185,#15525,#15526);
#13599=AXIS2_PLACEMENT_3D('',#29214,#15527,#15528);
#13600=AXIS2_PLACEMENT_3D('',#29243,#15529,#15530);
#13601=AXIS2_PLACEMENT_3D('',#29272,#15531,#15532);
#13602=AXIS2_PLACEMENT_3D('',#29301,#15533,#15534);
#13603=AXIS2_PLACEMENT_3D('',#29330,#15535,#15536);
#13604=AXIS2_PLACEMENT_3D('',#29823,#15537,#15538);
#13605=AXIS2_PLACEMENT_3D('',#29824,#15539,#15540);
#13606=AXIS2_PLACEMENT_3D('',#29849,#15541,#15542);
#13607=AXIS2_PLACEMENT_3D('',#29850,#15543,#15544);
#13608=AXIS2_PLACEMENT_3D('',#29911,#15545,#15546);
#13609=AXIS2_PLACEMENT_3D('',#29912,#15547,#15548);
#13610=AXIS2_PLACEMENT_3D('',#29937,#15549,#15550);
#13611=AXIS2_PLACEMENT_3D('',#29938,#15551,#15552);
#13612=AXIS2_PLACEMENT_3D('',#30003,#15553,#15554);
#13613=AXIS2_PLACEMENT_3D('',#30004,#15555,#15556);
#13614=AXIS2_PLACEMENT_3D('',#30033,#15557,#15558);
#13615=AXIS2_PLACEMENT_3D('',#30034,#15559,#15560);
#13616=AXIS2_PLACEMENT_3D('',#30095,#15561,#15562);
#13617=AXIS2_PLACEMENT_3D('',#30096,#15563,#15564);
#13618=AXIS2_PLACEMENT_3D('',#30125,#15565,#15566);
#13619=AXIS2_PLACEMENT_3D('',#30126,#15567,#15568);
#13620=AXIS2_PLACEMENT_3D('',#30187,#15569,#15570);
#13621=AXIS2_PLACEMENT_3D('',#30188,#15571,#15572);
#13622=AXIS2_PLACEMENT_3D('',#30217,#15573,#15574);
#13623=AXIS2_PLACEMENT_3D('',#30218,#15575,#15576);
#13624=AXIS2_PLACEMENT_3D('',#30283,#15577,#15578);
#13625=AXIS2_PLACEMENT_3D('',#30284,#15579,#15580);
#13626=AXIS2_PLACEMENT_3D('',#30313,#15581,#15582);
#13627=AXIS2_PLACEMENT_3D('',#30314,#15583,#15584);
#13628=AXIS2_PLACEMENT_3D('',#30375,#15585,#15586);
#13629=AXIS2_PLACEMENT_3D('',#30376,#15587,#15588);
#13630=AXIS2_PLACEMENT_3D('',#30405,#15589,#15590);
#13631=AXIS2_PLACEMENT_3D('',#30406,#15591,#15592);
#13632=AXIS2_PLACEMENT_3D('',#30471,#15593,#15594);
#13633=AXIS2_PLACEMENT_3D('',#30472,#15595,#15596);
#13634=AXIS2_PLACEMENT_3D('',#30501,#15597,#15598);
#13635=AXIS2_PLACEMENT_3D('',#30502,#15599,#15600);
#13636=AXIS2_PLACEMENT_3D('',#30563,#15601,#15602);
#13637=AXIS2_PLACEMENT_3D('',#30564,#15603,#15604);
#13638=AXIS2_PLACEMENT_3D('',#30593,#15605,#15606);
#13639=AXIS2_PLACEMENT_3D('',#30594,#15607,#15608);
#13640=AXIS2_PLACEMENT_3D('',#30655,#15609,#15610);
#13641=AXIS2_PLACEMENT_3D('',#30656,#15611,#15612);
#13642=AXIS2_PLACEMENT_3D('',#30685,#15613,#15614);
#13643=AXIS2_PLACEMENT_3D('',#30686,#15615,#15616);
#13644=AXIS2_PLACEMENT_3D('',#30747,#15617,#15618);
#13645=AXIS2_PLACEMENT_3D('',#30748,#15619,#15620);
#13646=AXIS2_PLACEMENT_3D('',#30777,#15621,#15622);
#13647=AXIS2_PLACEMENT_3D('',#30778,#15623,#15624);
#13648=AXIS2_PLACEMENT_3D('',#30843,#15625,#15626);
#13649=AXIS2_PLACEMENT_3D('',#30844,#15627,#15628);
#13650=AXIS2_PLACEMENT_3D('',#30873,#15629,#15630);
#13651=AXIS2_PLACEMENT_3D('',#30874,#15631,#15632);
#13652=AXIS2_PLACEMENT_3D('',#30935,#15633,#15634);
#13653=AXIS2_PLACEMENT_3D('',#30936,#15635,#15636);
#13654=AXIS2_PLACEMENT_3D('',#30965,#15637,#15638);
#13655=AXIS2_PLACEMENT_3D('',#30966,#15639,#15640);
#13656=AXIS2_PLACEMENT_3D('',#31027,#15641,#15642);
#13657=AXIS2_PLACEMENT_3D('',#31028,#15643,#15644);
#13658=AXIS2_PLACEMENT_3D('',#31057,#15645,#15646);
#13659=AXIS2_PLACEMENT_3D('',#31058,#15647,#15648);
#13660=AXIS2_PLACEMENT_3D('',#31123,#15649,#15650);
#13661=AXIS2_PLACEMENT_3D('',#31124,#15651,#15652);
#13662=AXIS2_PLACEMENT_3D('',#31153,#15653,#15654);
#13663=AXIS2_PLACEMENT_3D('',#31154,#15655,#15656);
#13664=AXIS2_PLACEMENT_3D('',#31215,#15657,#15658);
#13665=AXIS2_PLACEMENT_3D('',#31216,#15659,#15660);
#13666=AXIS2_PLACEMENT_3D('',#31245,#15661,#15662);
#13667=AXIS2_PLACEMENT_3D('',#31246,#15663,#15664);
#13668=AXIS2_PLACEMENT_3D('',#31311,#15665,#15666);
#13669=AXIS2_PLACEMENT_3D('',#31312,#15667,#15668);
#13670=AXIS2_PLACEMENT_3D('',#31341,#15669,#15670);
#13671=AXIS2_PLACEMENT_3D('',#31342,#15671,#15672);
#13672=AXIS2_PLACEMENT_3D('',#31403,#15673,#15674);
#13673=AXIS2_PLACEMENT_3D('',#31404,#15675,#15676);
#13674=AXIS2_PLACEMENT_3D('',#31429,#15677,#15678);
#13675=AXIS2_PLACEMENT_3D('',#31430,#15679,#15680);
#13676=AXIS2_PLACEMENT_3D('',#31545,#15683,#15684);
#13677=AXIS2_PLACEMENT_3D('',#31547,#15685,#15686);
#13678=AXIS2_PLACEMENT_3D('',#31561,#15687,#15688);
#13679=AXIS2_PLACEMENT_3D('',#31576,#15689,#15690);
#13680=AXIS2_PLACEMENT_3D('',#31727,#15695,#15696);
#13681=AXIS2_PLACEMENT_3D('',#31728,#15697,#15698);
#13682=AXIS2_PLACEMENT_3D('',#31730,#15699,#15700);
#13683=AXIS2_PLACEMENT_3D('',#31735,#15703,#15704);
#13684=AXIS2_PLACEMENT_3D('',#31740,#15707,#15708);
#13685=AXIS2_PLACEMENT_3D('',#31745,#15711,#15712);
#13686=AXIS2_PLACEMENT_3D('',#31750,#15715,#15716);
#13687=AXIS2_PLACEMENT_3D('',#31755,#15719,#15720);
#13688=AXIS2_PLACEMENT_3D('',#31760,#15723,#15724);
#13689=AXIS2_PLACEMENT_3D('',#31765,#15727,#15728);
#13690=AXIS2_PLACEMENT_3D('',#31770,#15731,#15732);
#13691=AXIS2_PLACEMENT_3D('',#31775,#15735,#15736);
#13692=AXIS2_PLACEMENT_3D('',#31780,#15739,#15740);
#13693=AXIS2_PLACEMENT_3D('',#31785,#15743,#15744);
#13694=AXIS2_PLACEMENT_3D('',#31790,#15747,#15748);
#13695=AXIS2_PLACEMENT_3D('',#31795,#15751,#15752);
#13696=AXIS2_PLACEMENT_3D('',#31800,#15755,#15756);
#13697=AXIS2_PLACEMENT_3D('',#31803,#15759,#15760);
#13698=AXIS2_PLACEMENT_3D('',#31882,#15761,#15762);
#13699=AXIS2_PLACEMENT_3D('',#31883,#15763,#15764);
#13700=AXIS2_PLACEMENT_3D('',#32040,#15765,#15766);
#13701=AXIS2_PLACEMENT_3D('',#32119,#15767,#15768);
#13702=AXIS2_PLACEMENT_3D('',#32120,#15769,#15770);
#13703=AXIS2_PLACEMENT_3D('',#32277,#15771,#15772);
#13704=AXIS2_PLACEMENT_3D('',#32356,#15773,#15774);
#13705=AXIS2_PLACEMENT_3D('',#32357,#15775,#15776);
#13706=AXIS2_PLACEMENT_3D('',#32514,#15777,#15778);
#13707=AXIS2_PLACEMENT_3D('',#32593,#15779,#15780);
#13708=AXIS2_PLACEMENT_3D('',#32594,#15781,#15782);
#13709=AXIS2_PLACEMENT_3D('',#32751,#15783,#15784);
#13710=AXIS2_PLACEMENT_3D('',#32830,#15785,#15786);
#13711=AXIS2_PLACEMENT_3D('',#32831,#15787,#15788);
#13712=AXIS2_PLACEMENT_3D('',#32975,#15789,#15790);
#13713=AXIS2_PLACEMENT_3D('',#32976,#15791,#15792);
#13714=AXIS2_PLACEMENT_3D('',#32977,#15793,#15794);
#13715=AXIS2_PLACEMENT_3D('',#32979,#15795,#15796);
#13716=AXIS2_PLACEMENT_3D('',#32982,#15798,#15799);
#13717=AXIS2_PLACEMENT_3D('',#32983,#15800,#15801);
#13718=AXIS2_PLACEMENT_3D('',#32985,#15802,#15803);
#13719=AXIS2_PLACEMENT_3D('',#32988,#15805,#15806);
#13720=AXIS2_PLACEMENT_3D('',#32989,#15807,#15808);
#13721=AXIS2_PLACEMENT_3D('',#32991,#15809,#15810);
#13722=AXIS2_PLACEMENT_3D('',#32994,#15812,#15813);
#13723=AXIS2_PLACEMENT_3D('',#32995,#15814,#15815);
#13724=AXIS2_PLACEMENT_3D('',#32997,#15816,#15817);
#13725=AXIS2_PLACEMENT_3D('',#32999,#15818,#15819);
#13726=AXIS2_PLACEMENT_3D('',#33001,#15820,#15821);
#13727=AXIS2_PLACEMENT_3D('',#33002,#15822,#15823);
#13728=AXIS2_PLACEMENT_3D('',#33003,#15824,#15825);
#13729=AXIS2_PLACEMENT_3D('',#33006,#15827,#15828);
#13730=AXIS2_PLACEMENT_3D('',#33007,#15829,#15830);
#13731=AXIS2_PLACEMENT_3D('',#33009,#15831,#15832);
#13732=AXIS2_PLACEMENT_3D('',#33010,#15833,#15834);
#13733=AXIS2_PLACEMENT_3D('',#33012,#15835,#15836);
#13734=AXIS2_PLACEMENT_3D('',#33014,#15838,#15839);
#13735=AXIS2_PLACEMENT_3D('',#33015,#15840,#15841);
#13736=AXIS2_PLACEMENT_3D('',#33016,#15842,#15843);
#13737=AXIS2_PLACEMENT_3D('',#33155,#15845,#15846);
#13738=AXIS2_PLACEMENT_3D('',#33238,#15847,#15848);
#13739=AXIS2_PLACEMENT_3D('',#33737,#15850,#15851);
#13740=AXIS2_PLACEMENT_3D('',#34233,#15853,#15854);
#13741=AXIS2_PLACEMENT_3D('',#34741,#15856,#15857);
#13742=AXIS2_PLACEMENT_3D('',#35249,#15859,#15860);
#13743=AXIS2_PLACEMENT_3D('',#35745,#15862,#15863);
#13744=AXIS2_PLACEMENT_3D('',#36247,#15865,#15866);
#13745=AXIS2_PLACEMENT_3D('',#36743,#15868,#15869);
#13746=AXIS2_PLACEMENT_3D('',#37230,#15871,#15872);
#13747=AXIS2_PLACEMENT_3D('',#37729,#15874,#15875);
#13748=AXIS2_PLACEMENT_3D('',#38237,#15877,#15878);
#13749=AXIS2_PLACEMENT_3D('',#38730,#15880,#15881);
#13750=AXIS2_PLACEMENT_3D('',#39226,#15883,#15884);
#13751=AXIS2_PLACEMENT_3D('',#39734,#15886,#15887);
#13752=AXIS2_PLACEMENT_3D('',#40242,#15889,#15890);
#13753=AXIS2_PLACEMENT_3D('',#40741,#15892,#15893);
#13754=AXIS2_PLACEMENT_3D('',#41237,#15895,#15896);
#13755=AXIS2_PLACEMENT_3D('',#41730,#15898,#15899);
#13756=AXIS2_PLACEMENT_3D('',#42217,#15901,#15902);
#13757=AXIS2_PLACEMENT_3D('',#42719,#15904,#15905);
#13758=AXIS2_PLACEMENT_3D('',#43227,#15907,#15908);
#13759=AXIS2_PLACEMENT_3D('',#43720,#15910,#15911);
#13760=AXIS2_PLACEMENT_3D('',#44222,#15913,#15914);
#13761=AXIS2_PLACEMENT_3D('',#44730,#15916,#15917);
#13762=AXIS2_PLACEMENT_3D('',#45235,#15919,#15920);
#13763=AXIS2_PLACEMENT_3D('',#45731,#15922,#15923);
#13764=AXIS2_PLACEMENT_3D('',#46227,#15925,#15926);
#13765=AXIS2_PLACEMENT_3D('',#46720,#15928,#15929);
#13766=AXIS2_PLACEMENT_3D('',#47204,#15931,#15932);
#13767=AXIS2_PLACEMENT_3D('',#47706,#15934,#15935);
#13768=AXIS2_PLACEMENT_3D('',#48214,#15937,#15938);
#13769=AXIS2_PLACEMENT_3D('',#48719,#15940,#15941);
#13770=AXIS2_PLACEMENT_3D('',#49212,#15943,#15944);
#13771=AXIS2_PLACEMENT_3D('',#49711,#15946,#15947);
#13772=AXIS2_PLACEMENT_3D('',#50195,#15949,#15950);
#13773=AXIS2_PLACEMENT_3D('',#50676,#15952,#15953);
#13774=AXIS2_PLACEMENT_3D('',#51178,#15955,#15956);
#13775=AXIS2_PLACEMENT_3D('',#51680,#15958,#15959);
#13776=AXIS2_PLACEMENT_3D('',#52185,#15961,#15962);
#13777=AXIS2_PLACEMENT_3D('',#52672,#15964,#15965);
#13778=AXIS2_PLACEMENT_3D('',#53165,#15967,#15968);
#13779=AXIS2_PLACEMENT_3D('',#53676,#15970,#15971);
#13780=AXIS2_PLACEMENT_3D('',#54169,#15973,#15974);
#13781=AXIS2_PLACEMENT_3D('',#54668,#15976,#15977);
#13782=AXIS2_PLACEMENT_3D('',#55152,#15979,#15980);
#13783=AXIS2_PLACEMENT_3D('',#55633,#15982,#15983);
#13784=AXIS2_PLACEMENT_3D('',#56132,#15985,#15986);
#13785=AXIS2_PLACEMENT_3D('',#56637,#15988,#15989);
#13786=AXIS2_PLACEMENT_3D('',#57133,#15991,#15992);
#13787=AXIS2_PLACEMENT_3D('',#57626,#15994,#15995);
#13788=AXIS2_PLACEMENT_3D('',#58122,#15997,#15998);
#13789=AXIS2_PLACEMENT_3D('',#58630,#16000,#16001);
#13790=AXIS2_PLACEMENT_3D('',#59117,#16003,#16004);
#13791=AXIS2_PLACEMENT_3D('',#59622,#16006,#16007);
#13792=AXIS2_PLACEMENT_3D('',#60106,#16009,#16010);
#13793=AXIS2_PLACEMENT_3D('',#60584,#16012,#16013);
#13794=AXIS2_PLACEMENT_3D('',#61083,#16015,#16016);
#13795=AXIS2_PLACEMENT_3D('',#61588,#16018,#16019);
#13796=AXIS2_PLACEMENT_3D('',#62084,#16021,#16022);
#13797=AXIS2_PLACEMENT_3D('',#62565,#16024,#16025);
#13798=AXIS2_PLACEMENT_3D('',#62577,#16026,#16027);
#13799=AXIS2_PLACEMENT_3D('',#74537,#16028,#16029);
#13800=AXIS2_PLACEMENT_3D('',#76818,#16030,#16031);
#13801=AXIS2_PLACEMENT_3D('',#76986,#16032,#16033);
#13802=AXIS2_PLACEMENT_3D('',#81914,#16034,#16035);
#13803=AXIS2_PLACEMENT_3D('',#81916,#16036,#16037);
#13804=AXIS2_PLACEMENT_3D('',#81919,#16039,#16040);
#13805=AXIS2_PLACEMENT_3D('',#81920,#16041,#16042);
#13806=AXIS2_PLACEMENT_3D('',#81922,#16043,#16044);
#13807=AXIS2_PLACEMENT_3D('',#81925,#16046,#16047);
#13808=AXIS2_PLACEMENT_3D('',#81926,#16048,#16049);
#13809=AXIS2_PLACEMENT_3D('',#81928,#16050,#16051);
#13810=AXIS2_PLACEMENT_3D('',#81931,#16053,#16054);
#13811=AXIS2_PLACEMENT_3D('',#81932,#16055,#16056);
#13812=AXIS2_PLACEMENT_3D('',#81934,#16057,#16058);
#13813=AXIS2_PLACEMENT_3D('',#81937,#16060,#16061);
#13814=AXIS2_PLACEMENT_3D('',#81938,#16062,#16063);
#13815=AXIS2_PLACEMENT_3D('',#81941,#16064,#16065);
#13816=AXIS2_PLACEMENT_3D('',#81943,#16066,#16067);
#13817=AXIS2_PLACEMENT_3D('',#81944,#16068,#16069);
#13818=AXIS2_PLACEMENT_3D('',#81945,#16070,#16071);
#13819=AXIS2_PLACEMENT_3D('',#81946,#16072,#16073);
#13820=AXIS2_PLACEMENT_3D('',#81949,#16074,#16075);
#13821=AXIS2_PLACEMENT_3D('',#81950,#16076,#16077);
#13822=AXIS2_PLACEMENT_3D('',#81952,#16079,#16080);
#13823=AXIS2_PLACEMENT_3D('',#81953,#16081,#16082);
#13824=AXIS2_PLACEMENT_3D('',#81955,#16083,#16084);
#13825=AXIS2_PLACEMENT_3D('',#81956,#16085,#16086);
#13826=AXIS2_PLACEMENT_3D('',#81957,#16087,#16088);
#13827=AXIS2_PLACEMENT_3D('',#81958,#16089,#16090);
#13828=AXIS2_PLACEMENT_3D('',#81959,#16091,#16092);
#13829=AXIS2_PLACEMENT_3D('',#81960,#16093,#16094);
#13830=AXIS2_PLACEMENT_3D('',#82134,#16096,#16097);
#13831=AXIS2_PLACEMENT_3D('',#82206,#16098,#16099);
#13832=AXIS2_PLACEMENT_3D('',#82724,#16101,#16102);
#13833=AXIS2_PLACEMENT_3D('',#83242,#16104,#16105);
#13834=AXIS2_PLACEMENT_3D('',#83760,#16107,#16108);
#13835=AXIS2_PLACEMENT_3D('',#84278,#16110,#16111);
#13836=AXIS2_PLACEMENT_3D('',#84283,#16113,#16114);
#13837=AXIS2_PLACEMENT_3D('',#84740,#16115,#16116);
#13838=AXIS2_PLACEMENT_3D('',#84782,#16117,#16118);
#13839=AXIS2_PLACEMENT_3D('',#84783,#16119,#16120);
#13840=AXIS2_PLACEMENT_3D('',#84943,#16121,#16122);
#13841=AXIS2_PLACEMENT_3D('',#85028,#16123,#16124);
#13842=AXIS2_PLACEMENT_3D('',#85149,#16128,#16129);
#13843=AXIS2_PLACEMENT_3D('',#85343,#16130,#16131);
#13844=AXIS2_PLACEMENT_3D('',#85394,#16132,#16133);
#13845=AXIS2_PLACEMENT_3D('',#85534,#16137,#16138);
#13846=AXIS2_PLACEMENT_3D('',#85536,#16139,#16140);
#13847=AXIS2_PLACEMENT_3D('',#85538,#16142,#16143);
#13848=AXIS2_PLACEMENT_3D('',#85541,#16145,#16146);
#13849=AXIS2_PLACEMENT_3D('',#85542,#16147,#16148);
#13850=AXIS2_PLACEMENT_3D('',#87083,#16178,#16179);
#13851=AXIS2_PLACEMENT_3D('',#87084,#16180,#16181);
#13852=AXIS2_PLACEMENT_3D('',#87085,#16182,#16183);
#13853=AXIS2_PLACEMENT_3D('',#87087,#16184,#16185);
#13854=AXIS2_PLACEMENT_3D('',#87089,#16186,#16187);
#13855=AXIS2_PLACEMENT_3D('',#87091,#16188,#16189);
#13856=AXIS2_PLACEMENT_3D('',#87092,#16190,#16191);
#13857=AXIS2_PLACEMENT_3D('',#87093,#16192,#16193);
#13858=AXIS2_PLACEMENT_3D('',#87096,#16195,#16196);
#13859=AXIS2_PLACEMENT_3D('',#87097,#16197,#16198);
#13860=AXIS2_PLACEMENT_3D('',#87099,#16199,#16200);
#13861=AXIS2_PLACEMENT_3D('',#87101,#16201,#16202);
#13862=AXIS2_PLACEMENT_3D('',#87103,#16203,#16204);
#13863=AXIS2_PLACEMENT_3D('',#87105,#16205,#16206);
#13864=AXIS2_PLACEMENT_3D('',#87107,#16207,#16208);
#13865=AXIS2_PLACEMENT_3D('',#87108,#16209,#16210);
#13866=AXIS2_PLACEMENT_3D('',#87111,#16212,#16213);
#13867=AXIS2_PLACEMENT_3D('',#87112,#16214,#16215);
#13868=AXIS2_PLACEMENT_3D('',#87115,#16217,#16218);
#13869=AXIS2_PLACEMENT_3D('',#87116,#16219,#16220);
#13870=AXIS2_PLACEMENT_3D('',#87119,#16222,#16223);
#13871=AXIS2_PLACEMENT_3D('',#87120,#16224,#16225);
#13872=AXIS2_PLACEMENT_3D('',#87123,#16227,#16228);
#13873=AXIS2_PLACEMENT_3D('',#87124,#16229,#16230);
#13874=AXIS2_PLACEMENT_3D('',#87126,#16231,#16232);
#13875=AXIS2_PLACEMENT_3D('',#87128,#16234,#16235);
#13876=AXIS2_PLACEMENT_3D('',#87129,#16236,#16237);
#13877=AXIS2_PLACEMENT_3D('',#87130,#16238,#16239);
#13878=AXIS2_PLACEMENT_3D('',#87132,#16240,#16241);
#13879=AXIS2_PLACEMENT_3D('',#87135,#16243,#16244);
#13880=AXIS2_PLACEMENT_3D('',#87136,#16245,#16246);
#13881=AXIS2_PLACEMENT_3D('',#87137,#16247,#16248);
#13882=AXIS2_PLACEMENT_3D('',#87139,#16249,#16250);
#13883=AXIS2_PLACEMENT_3D('',#87142,#16252,#16253);
#13884=AXIS2_PLACEMENT_3D('',#87143,#16254,#16255);
#13885=AXIS2_PLACEMENT_3D('',#87144,#16256,#16257);
#13886=AXIS2_PLACEMENT_3D('',#87146,#16258,#16259);
#13887=AXIS2_PLACEMENT_3D('',#87149,#16261,#16262);
#13888=AXIS2_PLACEMENT_3D('',#87150,#16263,#16264);
#13889=AXIS2_PLACEMENT_3D('',#87151,#16265,#16266);
#13890=AXIS2_PLACEMENT_3D('',#87153,#16267,#16268);
#13891=AXIS2_PLACEMENT_3D('',#87156,#16270,#16271);
#13892=AXIS2_PLACEMENT_3D('',#87157,#16272,#16273);
#13893=AXIS2_PLACEMENT_3D('',#87158,#16274,#16275);
#13894=AXIS2_PLACEMENT_3D('',#87160,#16276,#16277);
#13895=AXIS2_PLACEMENT_3D('',#87163,#16279,#16280);
#13896=AXIS2_PLACEMENT_3D('',#87164,#16281,#16282);
#13897=AXIS2_PLACEMENT_3D('',#87166,#16283,#16284);
#13898=AXIS2_PLACEMENT_3D('',#87169,#16286,#16287);
#13899=AXIS2_PLACEMENT_3D('',#87170,#16288,#16289);
#13900=AXIS2_PLACEMENT_3D('',#87171,#16290,#16291);
#13901=AXIS2_PLACEMENT_3D('',#87173,#16292,#16293);
#13902=AXIS2_PLACEMENT_3D('',#87176,#16295,#16296);
#13903=AXIS2_PLACEMENT_3D('',#87177,#16297,#16298);
#13904=AXIS2_PLACEMENT_3D('',#87178,#16299,#16300);
#13905=AXIS2_PLACEMENT_3D('',#87180,#16301,#16302);
#13906=AXIS2_PLACEMENT_3D('',#87183,#16304,#16305);
#13907=AXIS2_PLACEMENT_3D('',#87184,#16306,#16307);
#13908=AXIS2_PLACEMENT_3D('',#87185,#16308,#16309);
#13909=AXIS2_PLACEMENT_3D('',#87187,#16310,#16311);
#13910=AXIS2_PLACEMENT_3D('',#87190,#16313,#16314);
#13911=AXIS2_PLACEMENT_3D('',#87191,#16315,#16316);
#13912=AXIS2_PLACEMENT_3D('',#87193,#16317,#16318);
#13913=AXIS2_PLACEMENT_3D('',#87196,#16320,#16321);
#13914=AXIS2_PLACEMENT_3D('',#87197,#16322,#16323);
#13915=AXIS2_PLACEMENT_3D('',#87199,#16324,#16325);
#13916=AXIS2_PLACEMENT_3D('',#87202,#16327,#16328);
#13917=AXIS2_PLACEMENT_3D('',#87203,#16329,#16330);
#13918=AXIS2_PLACEMENT_3D('',#87205,#16331,#16332);
#13919=AXIS2_PLACEMENT_3D('',#87208,#16334,#16335);
#13920=AXIS2_PLACEMENT_3D('',#87209,#16336,#16337);
#13921=AXIS2_PLACEMENT_3D('',#87212,#16338,#16339);
#13922=AXIS2_PLACEMENT_3D('',#87216,#16341,#16342);
#13923=AXIS2_PLACEMENT_3D('',#87218,#16344,#16345);
#13924=AXIS2_PLACEMENT_3D('',#87222,#16347,#16348);
#13925=AXIS2_PLACEMENT_3D('',#87226,#16350,#16351);
#13926=AXIS2_PLACEMENT_3D('',#87238,#16357,#16358);
#13927=AXIS2_PLACEMENT_3D('',#87240,#16359,#16360);
#13928=AXIS2_PLACEMENT_3D('',#87252,#16366,#16367);
#13929=AXIS2_PLACEMENT_3D('',#87254,#16369,#16370);
#13930=AXIS2_PLACEMENT_3D('',#87258,#16373,#16374);
#13931=AXIS2_PLACEMENT_3D('',#87260,#16375,#16376);
#13932=AXIS2_PLACEMENT_3D('',#87262,#16378,#16379);
#13933=AXIS2_PLACEMENT_3D('',#87265,#16380,#16381);
#13934=AXIS2_PLACEMENT_3D('',#87268,#16384,#16385);
#13935=AXIS2_PLACEMENT_3D('',#87273,#16389,#16390);
#13936=AXIS2_PLACEMENT_3D('',#87275,#16391,#16392);
#13937=AXIS2_PLACEMENT_3D('',#87277,#16394,#16395);
#13938=AXIS2_PLACEMENT_3D('',#87279,#16397,#16398);
#13939=AXIS2_PLACEMENT_3D('',#87283,#16400,#16401);
#13940=AXIS2_PLACEMENT_3D('',#87285,#16403,#16404);
#13941=AXIS2_PLACEMENT_3D('',#87289,#16407,#16408);
#13942=AXIS2_PLACEMENT_3D('',#87291,#16409,#16410);
#13943=AXIS2_PLACEMENT_3D('',#87293,#16412,#16413);
#13944=AXIS2_PLACEMENT_3D('',#87297,#16415,#16416);
#13945=AXIS2_PLACEMENT_3D('',#87363,#16419,#16420);
#13946=AXIS2_PLACEMENT_3D('',#87365,#16422,#16423);
#13947=AXIS2_PLACEMENT_3D('',#87367,#16425,#16426);
#13948=AXIS2_PLACEMENT_3D('',#87368,#16427,#16428);
#13949=AXIS2_PLACEMENT_3D('',#87370,#16430,#16431);
#13950=AXIS2_PLACEMENT_3D('',#87372,#16433,#16434);
#13951=AXIS2_PLACEMENT_3D('',#87373,#16435,#16436);
#13952=AXIS2_PLACEMENT_3D('',#87375,#16437,#16438);
#13953=AXIS2_PLACEMENT_3D('',#87376,#16439,#16440);
#13954=AXIS2_PLACEMENT_3D('',#87377,#16441,#16442);
#13955=AXIS2_PLACEMENT_3D('',#87379,#16444,#16445);
#13956=AXIS2_PLACEMENT_3D('',#87380,#16446,#16447);
#13957=AXIS2_PLACEMENT_3D('',#87381,#16448,#16449);
#13958=AXIS2_PLACEMENT_3D('',#87383,#16450,#16451);
#13959=AXIS2_PLACEMENT_3D('',#87384,#16452,#16453);
#13960=AXIS2_PLACEMENT_3D('',#87386,#16455,#16456);
#13961=AXIS2_PLACEMENT_3D('',#87421,#16459,#16460);
#13962=AXIS2_PLACEMENT_3D('',#87449,#16461,#16462);
#13963=AXIS2_PLACEMENT_3D('',#87451,#16463,#16464);
#13964=AXIS2_PLACEMENT_3D('',#87452,#16465,#16466);
#13965=AXIS2_PLACEMENT_3D('',#87455,#16468,#16469);
#13966=AXIS2_PLACEMENT_3D('',#87456,#16470,#16471);
#13967=AXIS2_PLACEMENT_3D('',#87458,#16472,#16473);
#13968=AXIS2_PLACEMENT_3D('',#87459,#16474,#16475);
#13969=AXIS2_PLACEMENT_3D('',#87461,#16477,#16478);
#13970=AXIS2_PLACEMENT_3D('',#87462,#16479,#16480);
#13971=AXIS2_PLACEMENT_3D('',#87463,#16481,#16482);
#13972=AXIS2_PLACEMENT_3D('',#87464,#16483,#16484);
#13973=AXIS2_PLACEMENT_3D('',#87466,#16485,#16486);
#13974=AXIS2_PLACEMENT_3D('',#87469,#16488,#16489);
#13975=AXIS2_PLACEMENT_3D('',#87470,#16490,#16491);
#13976=AXIS2_PLACEMENT_3D('',#87472,#16492,#16493);
#13977=AXIS2_PLACEMENT_3D('',#87475,#16495,#16496);
#13978=AXIS2_PLACEMENT_3D('',#87476,#16497,#16498);
#13979=AXIS2_PLACEMENT_3D('',#87478,#16499,#16500);
#13980=AXIS2_PLACEMENT_3D('',#87481,#16502,#16503);
#13981=AXIS2_PLACEMENT_3D('',#87482,#16504,#16505);
#13982=AXIS2_PLACEMENT_3D('',#87484,#16506,#16507);
#13983=AXIS2_PLACEMENT_3D('',#87486,#16508,#16509);
#13984=AXIS2_PLACEMENT_3D('',#87488,#16510,#16511);
#13985=AXIS2_PLACEMENT_3D('',#87489,#16512,#16513);
#13986=AXIS2_PLACEMENT_3D('',#87490,#16514,#16515);
#13987=AXIS2_PLACEMENT_3D('',#87492,#16516,#16517);
#13988=AXIS2_PLACEMENT_3D('',#87494,#16519,#16520);
#13989=AXIS2_PLACEMENT_3D('',#87496,#16521,#16522);
#13990=AXIS2_PLACEMENT_3D('',#87497,#16523,#16524);
#13991=AXIS2_PLACEMENT_3D('',#87500,#16526,#16527);
#13992=AXIS2_PLACEMENT_3D('',#87501,#16528,#16529);
#13993=AXIS2_PLACEMENT_3D('',#87502,#16530,#16531);
#13994=AXIS2_PLACEMENT_3D('',#87503,#16532,#16533);
#13995=AXIS2_PLACEMENT_3D('',#87505,#16534,#16535);
#13996=AXIS2_PLACEMENT_3D('',#87507,#16536,#16537);
#13997=AXIS2_PLACEMENT_3D('',#87508,#16538,#16539);
#13998=AXIS2_PLACEMENT_3D('',#87509,#16540,#16541);
#13999=AXIS2_PLACEMENT_3D('',#87512,#16542,#16543);
#14000=AXIS2_PLACEMENT_3D('',#87516,#16545,#16546);
#14001=AXIS2_PLACEMENT_3D('',#87517,#16547,#16548);
#14002=AXIS2_PLACEMENT_3D('',#87518,#16549,#16550);
#14003=AXIS2_PLACEMENT_3D('',#87519,#16551,#16552);
#14004=AXIS2_PLACEMENT_3D('',#87522,#16554,#16555);
#14005=AXIS2_PLACEMENT_3D('',#87523,#16556,#16557);
#14006=AXIS2_PLACEMENT_3D('',#87526,#16559,#16560);
#14007=AXIS2_PLACEMENT_3D('',#87527,#16561,#16562);
#14008=AXIS2_PLACEMENT_3D('',#87529,#16563,#16564);
#14009=AXIS2_PLACEMENT_3D('',#87530,#16565,#16566);
#14010=AXIS2_PLACEMENT_3D('',#87531,#16567,#16568);
#14011=AXIS2_PLACEMENT_3D('',#87533,#16569,#16570);
#14012=AXIS2_PLACEMENT_3D('',#87535,#16571,#16572);
#14013=AXIS2_PLACEMENT_3D('',#87536,#16573,#16574);
#14014=AXIS2_PLACEMENT_3D('',#87537,#16575,#16576);
#14015=AXIS2_PLACEMENT_3D('',#87539,#16578,#16579);
#14016=AXIS2_PLACEMENT_3D('',#87542,#16581,#16582);
#14017=AXIS2_PLACEMENT_3D('',#87543,#16583,#16584);
#14018=AXIS2_PLACEMENT_3D('',#87545,#16585,#16586);
#14019=AXIS2_PLACEMENT_3D('',#87546,#16587,#16588);
#14020=AXIS2_PLACEMENT_3D('',#87547,#16589,#16590);
#14021=AXIS2_PLACEMENT_3D('',#87549,#16591,#16592);
#14022=AXIS2_PLACEMENT_3D('',#87550,#16593,#16594);
#14023=AXIS2_PLACEMENT_3D('',#87551,#16595,#16596);
#14024=AXIS2_PLACEMENT_3D('',#87552,#16597,#16598);
#14025=AXIS2_PLACEMENT_3D('',#87553,#16599,#16600);
#14026=AXIS2_PLACEMENT_3D('',#87556,#16601,#16602);
#14027=AXIS2_PLACEMENT_3D('',#87557,#16603,#16604);
#14028=AXIS2_PLACEMENT_3D('',#87559,#16605,#16606);
#14029=AXIS2_PLACEMENT_3D('',#87562,#16608,#16609);
#14030=AXIS2_PLACEMENT_3D('',#87563,#16610,#16611);
#14031=AXIS2_PLACEMENT_3D('',#87565,#16612,#16613);
#14032=AXIS2_PLACEMENT_3D('',#87566,#16614,#16615);
#14033=AXIS2_PLACEMENT_3D('',#87567,#16616,#16617);
#14034=AXIS2_PLACEMENT_3D('',#87570,#16618,#16619);
#14035=AXIS2_PLACEMENT_3D('',#87573,#16621,#16622);
#14036=AXIS2_PLACEMENT_3D('',#87574,#16623,#16624);
#14037=AXIS2_PLACEMENT_3D('',#87575,#16625,#16626);
#14038=AXIS2_PLACEMENT_3D('',#87578,#16628,#16629);
#14039=AXIS2_PLACEMENT_3D('',#87579,#16630,#16631);
#14040=AXIS2_PLACEMENT_3D('',#87580,#16632,#16633);
#14041=AXIS2_PLACEMENT_3D('',#87581,#16634,#16635);
#14042=AXIS2_PLACEMENT_3D('',#87583,#16636,#16637);
#14043=AXIS2_PLACEMENT_3D('',#87586,#16639,#16640);
#14044=AXIS2_PLACEMENT_3D('',#87587,#16641,#16642);
#14045=AXIS2_PLACEMENT_3D('',#87589,#16643,#16644);
#14046=AXIS2_PLACEMENT_3D('',#87592,#16646,#16647);
#14047=AXIS2_PLACEMENT_3D('',#87593,#16648,#16649);
#14048=AXIS2_PLACEMENT_3D('',#87595,#16650,#16651);
#14049=AXIS2_PLACEMENT_3D('',#87596,#16652,#16653);
#14050=AXIS2_PLACEMENT_3D('',#87597,#16654,#16655);
#14051=AXIS2_PLACEMENT_3D('',#87600,#16657,#16658);
#14052=AXIS2_PLACEMENT_3D('',#87601,#16659,#16660);
#14053=AXIS2_PLACEMENT_3D('',#87602,#16661,#16662);
#14054=AXIS2_PLACEMENT_3D('',#87603,#16663,#16664);
#14055=AXIS2_PLACEMENT_3D('',#87605,#16665,#16666);
#14056=AXIS2_PLACEMENT_3D('',#87608,#16668,#16669);
#14057=AXIS2_PLACEMENT_3D('',#87609,#16670,#16671);
#14058=AXIS2_PLACEMENT_3D('',#87612,#16673,#16674);
#14059=AXIS2_PLACEMENT_3D('',#87613,#16675,#16676);
#14060=AXIS2_PLACEMENT_3D('',#87616,#16677,#16678);
#14061=AXIS2_PLACEMENT_3D('',#87619,#16680,#16681);
#14062=AXIS2_PLACEMENT_3D('',#87620,#16682,#16683);
#14063=AXIS2_PLACEMENT_3D('',#87621,#16684,#16685);
#14064=AXIS2_PLACEMENT_3D('',#87624,#16687,#16688);
#14065=AXIS2_PLACEMENT_3D('',#87625,#16689,#16690);
#14066=AXIS2_PLACEMENT_3D('',#87628,#16692,#16693);
#14067=AXIS2_PLACEMENT_3D('',#87629,#16694,#16695);
#14068=AXIS2_PLACEMENT_3D('',#87631,#16696,#16697);
#14069=AXIS2_PLACEMENT_3D('',#87634,#16699,#16700);
#14070=AXIS2_PLACEMENT_3D('',#87635,#16701,#16702);
#14071=AXIS2_PLACEMENT_3D('',#87638,#16703,#16704);
#14072=AXIS2_PLACEMENT_3D('',#87640,#16706,#16707);
#14073=AXIS2_PLACEMENT_3D('',#87641,#16708,#16709);
#14074=AXIS2_PLACEMENT_3D('',#87644,#16711,#16712);
#14075=AXIS2_PLACEMENT_3D('',#87645,#16713,#16714);
#14076=AXIS2_PLACEMENT_3D('',#87647,#16715,#16716);
#14077=AXIS2_PLACEMENT_3D('',#87648,#16717,#16718);
#14078=AXIS2_PLACEMENT_3D('',#87649,#16719,#16720);
#14079=AXIS2_PLACEMENT_3D('',#87651,#16722,#16723);
#14080=AXIS2_PLACEMENT_3D('',#87652,#16724,#16725);
#14081=AXIS2_PLACEMENT_3D('',#87653,#16726,#16727);
#14082=AXIS2_PLACEMENT_3D('',#87656,#16728,#16729);
#14083=AXIS2_PLACEMENT_3D('',#87657,#16730,#16731);
#14084=AXIS2_PLACEMENT_3D('',#87660,#16732,#16733);
#14085=AXIS2_PLACEMENT_3D('',#87661,#16734,#16735);
#14086=AXIS2_PLACEMENT_3D('',#87664,#16736,#16737);
#14087=AXIS2_PLACEMENT_3D('',#87665,#16738,#16739);
#14088=AXIS2_PLACEMENT_3D('',#87668,#16740,#16741);
#14089=AXIS2_PLACEMENT_3D('',#87669,#16742,#16743);
#14090=AXIS2_PLACEMENT_3D('',#87672,#16744,#16745);
#14091=AXIS2_PLACEMENT_3D('',#87673,#16746,#16747);
#14092=AXIS2_PLACEMENT_3D('',#87676,#16748,#16749);
#14093=AXIS2_PLACEMENT_3D('',#87677,#16750,#16751);
#14094=AXIS2_PLACEMENT_3D('',#87680,#16752,#16753);
#14095=AXIS2_PLACEMENT_3D('',#87681,#16754,#16755);
#14096=AXIS2_PLACEMENT_3D('',#87684,#16756,#16757);
#14097=AXIS2_PLACEMENT_3D('',#87685,#16758,#16759);
#14098=AXIS2_PLACEMENT_3D('',#87687,#16760,#16761);
#14099=AXIS2_PLACEMENT_3D('',#87690,#16763,#16764);
#14100=AXIS2_PLACEMENT_3D('',#87691,#16765,#16766);
#14101=AXIS2_PLACEMENT_3D('',#87693,#16767,#16768);
#14102=AXIS2_PLACEMENT_3D('',#87694,#16769,#16770);
#14103=AXIS2_PLACEMENT_3D('',#87695,#16771,#16772);
#14104=AXIS2_PLACEMENT_3D('',#87698,#16774,#16775);
#14105=AXIS2_PLACEMENT_3D('',#87699,#16776,#16777);
#14106=AXIS2_PLACEMENT_3D('',#87701,#16778,#16779);
#14107=AXIS2_PLACEMENT_3D('',#87703,#16780,#16781);
#14108=AXIS2_PLACEMENT_3D('',#87704,#16782,#16783);
#14109=AXIS2_PLACEMENT_3D('',#87705,#16784,#16785);
#14110=AXIS2_PLACEMENT_3D('',#87708,#16786,#16787);
#14111=AXIS2_PLACEMENT_3D('',#87710,#16789,#16790);
#14112=AXIS2_PLACEMENT_3D('',#87711,#16791,#16792);
#14113=AXIS2_PLACEMENT_3D('',#87714,#16794,#16795);
#14114=AXIS2_PLACEMENT_3D('',#87715,#16796,#16797);
#14115=AXIS2_PLACEMENT_3D('',#87716,#16798,#16799);
#14116=AXIS2_PLACEMENT_3D('',#87717,#16800,#16801);
#14117=AXIS2_PLACEMENT_3D('',#87720,#16802,#16803);
#14118=AXIS2_PLACEMENT_3D('',#87721,#16804,#16805);
#14119=AXIS2_PLACEMENT_3D('',#87723,#16806,#16807);
#14120=AXIS2_PLACEMENT_3D('',#87724,#16808,#16809);
#14121=AXIS2_PLACEMENT_3D('',#87725,#16810,#16811);
#14122=AXIS2_PLACEMENT_3D('',#87727,#16812,#16813);
#14123=AXIS2_PLACEMENT_3D('',#87729,#16814,#16815);
#14124=AXIS2_PLACEMENT_3D('',#87730,#16816,#16817);
#14125=AXIS2_PLACEMENT_3D('',#87731,#16818,#16819);
#14126=AXIS2_PLACEMENT_3D('',#87733,#16820,#16821);
#14127=AXIS2_PLACEMENT_3D('',#87736,#16823,#16824);
#14128=AXIS2_PLACEMENT_3D('',#87737,#16825,#16826);
#14129=AXIS2_PLACEMENT_3D('',#87739,#16828,#16829);
#14130=AXIS2_PLACEMENT_3D('',#87740,#16830,#16831);
#14131=AXIS2_PLACEMENT_3D('',#87741,#16832,#16833);
#14132=AXIS2_PLACEMENT_3D('',#87744,#16834,#16835);
#14133=AXIS2_PLACEMENT_3D('',#87745,#16836,#16837);
#14134=AXIS2_PLACEMENT_3D('',#87749,#16839,#16840);
#14135=AXIS2_PLACEMENT_3D('',#87750,#16841,#16842);
#14136=AXIS2_PLACEMENT_3D('',#87751,#16843,#16844);
#14137=AXIS2_PLACEMENT_3D('',#87754,#16845,#16846);
#14138=AXIS2_PLACEMENT_3D('',#87755,#16847,#16848);
#14139=AXIS2_PLACEMENT_3D('',#87759,#16850,#16851);
#14140=AXIS2_PLACEMENT_3D('',#87760,#16852,#16853);
#14141=AXIS2_PLACEMENT_3D('',#87761,#16854,#16855);
#14142=AXIS2_PLACEMENT_3D('',#87763,#16856,#16857);
#14143=AXIS2_PLACEMENT_3D('',#87765,#16858,#16859);
#14144=AXIS2_PLACEMENT_3D('',#87767,#16860,#16861);
#14145=AXIS2_PLACEMENT_3D('',#87768,#16862,#16863);
#14146=AXIS2_PLACEMENT_3D('',#87769,#16864,#16865);
#14147=AXIS2_PLACEMENT_3D('',#87772,#16866,#16867);
#14148=AXIS2_PLACEMENT_3D('',#87773,#16868,#16869);
#14149=AXIS2_PLACEMENT_3D('',#87775,#16871,#16872);
#14150=AXIS2_PLACEMENT_3D('',#87777,#16874,#16875);
#14151=AXIS2_PLACEMENT_3D('',#87781,#16877,#16878);
#14152=AXIS2_PLACEMENT_3D('',#87791,#16879,#16880);
#14153=AXIS2_PLACEMENT_3D('',#87794,#16882,#16883);
#14154=AXIS2_PLACEMENT_3D('',#87803,#16884,#16885);
#14155=AXIS2_PLACEMENT_3D('',#87806,#16886,#16887);
#14156=AXIS2_PLACEMENT_3D('',#87816,#16888,#16889);
#14157=AXIS2_PLACEMENT_3D('',#87826,#16890,#16891);
#14158=AXIS2_PLACEMENT_3D('',#87836,#16892,#16893);
#14159=AXIS2_PLACEMENT_3D('',#87846,#16894,#16895);
#14160=AXIS2_PLACEMENT_3D('',#87856,#16896,#16897);
#14161=AXIS2_PLACEMENT_3D('',#87866,#16898,#16899);
#14162=AXIS2_PLACEMENT_3D('',#87876,#16900,#16901);
#14163=AXIS2_PLACEMENT_3D('',#87886,#16902,#16903);
#14164=AXIS2_PLACEMENT_3D('',#87896,#16904,#16905);
#14165=AXIS2_PLACEMENT_3D('',#87906,#16906,#16907);
#14166=AXIS2_PLACEMENT_3D('',#87916,#16908,#16909);
#14167=AXIS2_PLACEMENT_3D('',#87926,#16910,#16911);
#14168=AXIS2_PLACEMENT_3D('',#87936,#16912,#16913);
#14169=AXIS2_PLACEMENT_3D('',#87946,#16914,#16915);
#14170=AXIS2_PLACEMENT_3D('',#87956,#16916,#16917);
#14171=AXIS2_PLACEMENT_3D('',#87966,#16918,#16919);
#14172=AXIS2_PLACEMENT_3D('',#87976,#16920,#16921);
#14173=AXIS2_PLACEMENT_3D('',#87986,#16922,#16923);
#14174=AXIS2_PLACEMENT_3D('',#87996,#16924,#16925);
#14175=AXIS2_PLACEMENT_3D('',#88004,#16926,#16927);
#14176=AXIS2_PLACEMENT_3D('',#88008,#16929,#16930);
#14177=AXIS2_PLACEMENT_3D('',#88018,#16931,#16932);
#14178=AXIS2_PLACEMENT_3D('',#88021,#16934,#16935);
#14179=AXIS2_PLACEMENT_3D('',#88030,#16936,#16937);
#14180=AXIS2_PLACEMENT_3D('',#88033,#16938,#16939);
#14181=AXIS2_PLACEMENT_3D('',#88043,#16940,#16941);
#14182=AXIS2_PLACEMENT_3D('',#88053,#16942,#16943);
#14183=AXIS2_PLACEMENT_3D('',#88063,#16944,#16945);
#14184=AXIS2_PLACEMENT_3D('',#88073,#16946,#16947);
#14185=AXIS2_PLACEMENT_3D('',#88083,#16948,#16949);
#14186=AXIS2_PLACEMENT_3D('',#88093,#16950,#16951);
#14187=AXIS2_PLACEMENT_3D('',#88103,#16952,#16953);
#14188=AXIS2_PLACEMENT_3D('',#88113,#16954,#16955);
#14189=AXIS2_PLACEMENT_3D('',#88123,#16956,#16957);
#14190=AXIS2_PLACEMENT_3D('',#88133,#16958,#16959);
#14191=AXIS2_PLACEMENT_3D('',#88143,#16960,#16961);
#14192=AXIS2_PLACEMENT_3D('',#88153,#16962,#16963);
#14193=AXIS2_PLACEMENT_3D('',#88163,#16964,#16965);
#14194=AXIS2_PLACEMENT_3D('',#88173,#16966,#16967);
#14195=AXIS2_PLACEMENT_3D('',#88183,#16968,#16969);
#14196=AXIS2_PLACEMENT_3D('',#88193,#16970,#16971);
#14197=AXIS2_PLACEMENT_3D('',#88203,#16972,#16973);
#14198=AXIS2_PLACEMENT_3D('',#88213,#16974,#16975);
#14199=AXIS2_PLACEMENT_3D('',#88223,#16976,#16977);
#14200=AXIS2_PLACEMENT_3D('',#88231,#16978,#16979);
#14201=AXIS2_PLACEMENT_3D('',#88232,#16980,#16981);
#14202=AXIS2_PLACEMENT_3D('',#88233,#16982,#16983);
#14203=AXIS2_PLACEMENT_3D('',#88234,#16984,#16985);
#14204=AXIS2_PLACEMENT_3D('',#88235,#16986,#16987);
#14205=AXIS2_PLACEMENT_3D('',#88236,#16988,#16989);
#14206=AXIS2_PLACEMENT_3D('',#88237,#16990,#16991);
#14207=AXIS2_PLACEMENT_3D('',#88238,#16992,#16993);
#14208=AXIS2_PLACEMENT_3D('',#88239,#16994,#16995);
#14209=AXIS2_PLACEMENT_3D('',#88240,#16996,#16997);
#14210=AXIS2_PLACEMENT_3D('',#88241,#16998,#16999);
#14211=AXIS2_PLACEMENT_3D('',#88242,#17000,#17001);
#14212=AXIS2_PLACEMENT_3D('',#88243,#17002,#17003);
#14213=AXIS2_PLACEMENT_3D('',#88244,#17004,#17005);
#14214=AXIS2_PLACEMENT_3D('',#88245,#17006,#17007);
#14215=AXIS2_PLACEMENT_3D('',#88246,#17008,#17009);
#14216=AXIS2_PLACEMENT_3D('',#88247,#17010,#17011);
#14217=AXIS2_PLACEMENT_3D('',#88248,#17012,#17013);
#14218=AXIS2_PLACEMENT_3D('',#88249,#17014,#17015);
#14219=AXIS2_PLACEMENT_3D('',#88250,#17016,#17017);
#14220=AXIS2_PLACEMENT_3D('',#88251,#17018,#17019);
#14221=AXIS2_PLACEMENT_3D('',#88252,#17020,#17021);
#14222=AXIS2_PLACEMENT_3D('',#88253,#17022,#17023);
#14223=AXIS2_PLACEMENT_3D('',#88254,#17024,#17025);
#14224=AXIS2_PLACEMENT_3D('',#88255,#17026,#17027);
#14225=AXIS2_PLACEMENT_3D('',#88256,#17028,#17029);
#14226=AXIS2_PLACEMENT_3D('',#88257,#17030,#17031);
#14227=AXIS2_PLACEMENT_3D('',#88258,#17032,#17033);
#14228=AXIS2_PLACEMENT_3D('',#88259,#17034,#17035);
#14229=AXIS2_PLACEMENT_3D('',#88260,#17036,#17037);
#14230=AXIS2_PLACEMENT_3D('',#88261,#17038,#17039);
#14231=AXIS2_PLACEMENT_3D('',#88262,#17040,#17041);
#14232=AXIS2_PLACEMENT_3D('',#88263,#17042,#17043);
#14233=AXIS2_PLACEMENT_3D('',#88264,#17044,#17045);
#14234=AXIS2_PLACEMENT_3D('',#88265,#17046,#17047);
#14235=AXIS2_PLACEMENT_3D('',#88266,#17048,#17049);
#14236=AXIS2_PLACEMENT_3D('',#88267,#17050,#17051);
#14237=AXIS2_PLACEMENT_3D('',#88268,#17052,#17053);
#14238=AXIS2_PLACEMENT_3D('',#88269,#17054,#17055);
#14239=AXIS2_PLACEMENT_3D('',#88270,#17056,#17057);
#14240=AXIS2_PLACEMENT_3D('',#88271,#17058,#17059);
#14241=AXIS2_PLACEMENT_3D('',#88272,#17060,#17061);
#14242=AXIS2_PLACEMENT_3D('',#88273,#17062,#17063);
#14243=AXIS2_PLACEMENT_3D('',#88274,#17064,#17065);
#14244=AXIS2_PLACEMENT_3D('',#88275,#17066,#17067);
#14245=AXIS2_PLACEMENT_3D('',#88276,#17068,#17069);
#14246=AXIS2_PLACEMENT_3D('',#88277,#17070,#17071);
#14247=AXIS2_PLACEMENT_3D('',#88278,#17072,#17073);
#14248=AXIS2_PLACEMENT_3D('',#88279,#17074,#17075);
#14249=AXIS2_PLACEMENT_3D('',#88280,#17076,#17077);
#14250=AXIS2_PLACEMENT_3D('',#88281,#17078,#17079);
#14251=AXIS2_PLACEMENT_3D('',#88282,#17080,#17081);
#14252=AXIS2_PLACEMENT_3D('',#88283,#17082,#17083);
#14253=AXIS2_PLACEMENT_3D('',#88284,#17084,#17085);
#14254=AXIS2_PLACEMENT_3D('',#88285,#17086,#17087);
#14255=AXIS2_PLACEMENT_3D('',#88286,#17088,#17089);
#14256=AXIS2_PLACEMENT_3D('',#88287,#17090,#17091);
#14257=AXIS2_PLACEMENT_3D('',#88288,#17092,#17093);
#14258=AXIS2_PLACEMENT_3D('',#88289,#17094,#17095);
#14259=AXIS2_PLACEMENT_3D('',#88290,#17096,#17097);
#14260=AXIS2_PLACEMENT_3D('',#88291,#17098,#17099);
#14261=AXIS2_PLACEMENT_3D('',#88292,#17100,#17101);
#14262=AXIS2_PLACEMENT_3D('',#88293,#17102,#17103);
#14263=AXIS2_PLACEMENT_3D('',#88294,#17104,#17105);
#14264=AXIS2_PLACEMENT_3D('',#88295,#17106,#17107);
#14265=AXIS2_PLACEMENT_3D('',#88296,#17108,#17109);
#14266=AXIS2_PLACEMENT_3D('',#88297,#17110,#17111);
#14267=AXIS2_PLACEMENT_3D('',#88298,#17112,#17113);
#14268=AXIS2_PLACEMENT_3D('',#88299,#17114,#17115);
#14269=AXIS2_PLACEMENT_3D('',#88300,#17116,#17117);
#14270=AXIS2_PLACEMENT_3D('',#88301,#17118,#17119);
#14271=AXIS2_PLACEMENT_3D('',#88302,#17120,#17121);
#14272=AXIS2_PLACEMENT_3D('',#88303,#17122,#17123);
#14273=AXIS2_PLACEMENT_3D('',#88304,#17124,#17125);
#14274=AXIS2_PLACEMENT_3D('',#88305,#17126,#17127);
#14275=AXIS2_PLACEMENT_3D('',#88306,#17128,#17129);
#14276=AXIS2_PLACEMENT_3D('',#88307,#17130,#17131);
#14277=AXIS2_PLACEMENT_3D('',#88308,#17132,#17133);
#14278=AXIS2_PLACEMENT_3D('',#88309,#17134,#17135);
#14279=AXIS2_PLACEMENT_3D('',#88310,#17136,#17137);
#14280=AXIS2_PLACEMENT_3D('',#88311,#17138,#17139);
#14281=AXIS2_PLACEMENT_3D('',#88312,#17140,#17141);
#14282=AXIS2_PLACEMENT_3D('',#88313,#17142,#17143);
#14283=AXIS2_PLACEMENT_3D('',#88314,#17144,#17145);
#14284=AXIS2_PLACEMENT_3D('',#88315,#17146,#17147);
#14285=AXIS2_PLACEMENT_3D('',#88316,#17148,#17149);
#14286=AXIS2_PLACEMENT_3D('',#88317,#17150,#17151);
#14287=AXIS2_PLACEMENT_3D('',#88318,#17152,#17153);
#14288=AXIS2_PLACEMENT_3D('',#88319,#17154,#17155);
#14289=AXIS2_PLACEMENT_3D('',#88321,#17156,#17157);
#14290=AXIS2_PLACEMENT_3D('',#88323,#17158,#17159);
#14291=AXIS2_PLACEMENT_3D('',#88325,#17160,#17161);
#14292=AXIS2_PLACEMENT_3D('',#88326,#17162,#17163);
#14293=AXIS2_PLACEMENT_3D('',#88327,#17164,#17165);
#14294=AXIS2_PLACEMENT_3D('',#88329,#17166,#17167);
#14295=AXIS2_PLACEMENT_3D('',#88331,#17168,#17169);
#14296=AXIS2_PLACEMENT_3D('',#88332,#17170,#17171);
#14297=AXIS2_PLACEMENT_3D('',#88333,#17172,#17173);
#14298=AXIS2_PLACEMENT_3D('',#88335,#17174,#17175);
#14299=AXIS2_PLACEMENT_3D('',#88339,#17177,#17178);
#14300=AXIS2_PLACEMENT_3D('',#88340,#17179,#17180);
#14301=AXIS2_PLACEMENT_3D('',#88341,#17181,#17182);
#14302=AXIS2_PLACEMENT_3D('',#88344,#17183,#17184);
#14303=AXIS2_PLACEMENT_3D('',#88346,#17186,#17187);
#14304=AXIS2_PLACEMENT_3D('',#88347,#17188,#17189);
#14305=AXIS2_PLACEMENT_3D('',#88350,#17191,#17192);
#14306=AXIS2_PLACEMENT_3D('',#88351,#17193,#17194);
#14307=AXIS2_PLACEMENT_3D('',#88354,#17196,#17197);
#14308=AXIS2_PLACEMENT_3D('',#88355,#17198,#17199);
#14309=AXIS2_PLACEMENT_3D('',#88357,#17201,#17202);
#14310=AXIS2_PLACEMENT_3D('',#88359,#17203,#17204);
#14311=AXIS2_PLACEMENT_3D('',#88361,#17206,#17207);
#14312=AXIS2_PLACEMENT_3D('',#88362,#17208,#17209);
#14313=AXIS2_PLACEMENT_3D('',#88363,#17210,#17211);
#14314=AXIS2_PLACEMENT_3D('',#88365,#17212,#17213);
#14315=AXIS2_PLACEMENT_3D('',#88368,#17215,#17216);
#14316=AXIS2_PLACEMENT_3D('',#88369,#17217,#17218);
#14317=AXIS2_PLACEMENT_3D('',#88370,#17219,#17220);
#14318=AXIS2_PLACEMENT_3D('',#88371,#17221,#17222);
#14319=AXIS2_PLACEMENT_3D('',#88373,#17223,#17224);
#14320=AXIS2_PLACEMENT_3D('',#88376,#17226,#17227);
#14321=AXIS2_PLACEMENT_3D('',#88377,#17228,#17229);
#14322=AXIS2_PLACEMENT_3D('',#88378,#17230,#17231);
#14323=AXIS2_PLACEMENT_3D('',#88379,#17232,#17233);
#14324=AXIS2_PLACEMENT_3D('',#88381,#17234,#17235);
#14325=AXIS2_PLACEMENT_3D('',#88384,#17237,#17238);
#14326=AXIS2_PLACEMENT_3D('',#88385,#17239,#17240);
#14327=AXIS2_PLACEMENT_3D('',#88386,#17241,#17242);
#14328=AXIS2_PLACEMENT_3D('',#88387,#17243,#17244);
#14329=AXIS2_PLACEMENT_3D('',#88389,#17245,#17246);
#14330=AXIS2_PLACEMENT_3D('',#88392,#17248,#17249);
#14331=AXIS2_PLACEMENT_3D('',#88393,#17250,#17251);
#14332=AXIS2_PLACEMENT_3D('',#88394,#17252,#17253);
#14333=AXIS2_PLACEMENT_3D('',#88395,#17254,#17255);
#14334=AXIS2_PLACEMENT_3D('',#88397,#17256,#17257);
#14335=AXIS2_PLACEMENT_3D('',#88400,#17259,#17260);
#14336=AXIS2_PLACEMENT_3D('',#88401,#17261,#17262);
#14337=AXIS2_PLACEMENT_3D('',#88402,#17263,#17264);
#14338=AXIS2_PLACEMENT_3D('',#88403,#17265,#17266);
#14339=AXIS2_PLACEMENT_3D('',#88405,#17267,#17268);
#14340=AXIS2_PLACEMENT_3D('',#88408,#17270,#17271);
#14341=AXIS2_PLACEMENT_3D('',#88409,#17272,#17273);
#14342=AXIS2_PLACEMENT_3D('',#88410,#17274,#17275);
#14343=AXIS2_PLACEMENT_3D('',#88411,#17276,#17277);
#14344=AXIS2_PLACEMENT_3D('',#88413,#17278,#17279);
#14345=AXIS2_PLACEMENT_3D('',#88416,#17281,#17282);
#14346=AXIS2_PLACEMENT_3D('',#88417,#17283,#17284);
#14347=AXIS2_PLACEMENT_3D('',#88418,#17285,#17286);
#14348=AXIS2_PLACEMENT_3D('',#88419,#17287,#17288);
#14349=AXIS2_PLACEMENT_3D('',#88421,#17289,#17290);
#14350=AXIS2_PLACEMENT_3D('',#88424,#17292,#17293);
#14351=AXIS2_PLACEMENT_3D('',#88425,#17294,#17295);
#14352=AXIS2_PLACEMENT_3D('',#88426,#17296,#17297);
#14353=AXIS2_PLACEMENT_3D('',#88427,#17298,#17299);
#14354=AXIS2_PLACEMENT_3D('',#88429,#17300,#17301);
#14355=AXIS2_PLACEMENT_3D('',#88432,#17303,#17304);
#14356=AXIS2_PLACEMENT_3D('',#88433,#17305,#17306);
#14357=AXIS2_PLACEMENT_3D('',#88434,#17307,#17308);
#14358=AXIS2_PLACEMENT_3D('',#88435,#17309,#17310);
#14359=AXIS2_PLACEMENT_3D('',#88437,#17311,#17312);
#14360=AXIS2_PLACEMENT_3D('',#88440,#17314,#17315);
#14361=AXIS2_PLACEMENT_3D('',#88441,#17316,#17317);
#14362=AXIS2_PLACEMENT_3D('',#88442,#17318,#17319);
#14363=AXIS2_PLACEMENT_3D('',#88443,#17320,#17321);
#14364=AXIS2_PLACEMENT_3D('',#88445,#17322,#17323);
#14365=AXIS2_PLACEMENT_3D('',#88448,#17325,#17326);
#14366=AXIS2_PLACEMENT_3D('',#88449,#17327,#17328);
#14367=AXIS2_PLACEMENT_3D('',#88450,#17329,#17330);
#14368=AXIS2_PLACEMENT_3D('',#88451,#17331,#17332);
#14369=AXIS2_PLACEMENT_3D('',#88452,#17333,#17334);
#14370=AXIS2_PLACEMENT_3D('',#88453,#17335,#17336);
#14371=AXIS2_PLACEMENT_3D('',#88454,#17337,#17338);
#14372=AXIS2_PLACEMENT_3D('',#88455,#17339,#17340);
#14373=AXIS2_PLACEMENT_3D('',#88456,#17341,#17342);
#14374=AXIS2_PLACEMENT_3D('',#88457,#17343,#17344);
#14375=AXIS2_PLACEMENT_3D('',#88458,#17345,#17346);
#14376=AXIS2_PLACEMENT_3D('',#88459,#17347,#17348);
#14377=AXIS2_PLACEMENT_3D('',#88460,#17349,#17350);
#14378=AXIS2_PLACEMENT_3D('',#88461,#17351,#17352);
#14379=DIRECTION('axis',(0.,0.,1.));
#14380=DIRECTION('refdir',(1.,0.,0.));
#14381=DIRECTION('axis',(0.,0.,1.));
#14382=DIRECTION('refdir',(1.,0.,0.));
#14383=DIRECTION('center_axis',(0.,0.,1.));
#14384=DIRECTION('ref_axis',(-0.608812046626718,0.793314497461244,0.));
#14385=DIRECTION('',(0.,0.,1.));
#14386=DIRECTION('center_axis',(0.,0.,-1.));
#14387=DIRECTION('ref_axis',(1.,6.43162402581532E-14,0.));
#14388=DIRECTION('center_axis',(0.,0.,1.));
#14389=DIRECTION('ref_axis',(-0.608812046626718,0.793314497461244,0.));
#14390=DIRECTION('',(0.,0.,1.));
#14391=DIRECTION('center_axis',(0.,0.,1.));
#14392=DIRECTION('ref_axis',(-0.608812046626718,0.793314497461244,0.));
#14393=DIRECTION('',(0.,0.,1.));
#14394=DIRECTION('center_axis',(0.,0.,1.));
#14395=DIRECTION('ref_axis',(-0.608812046626718,0.793314497461244,0.));
#14396=DIRECTION('',(0.,0.,1.));
#14397=DIRECTION('center_axis',(0.,0.,1.));
#14398=DIRECTION('ref_axis',(-0.608812046626718,0.793314497461244,0.));
#14399=DIRECTION('',(0.,0.,1.));
#14400=DIRECTION('center_axis',(0.,0.,1.));
#14401=DIRECTION('ref_axis',(-0.608812046626718,0.793314497461244,0.));
#14402=DIRECTION('',(0.,0.,1.));
#14403=DIRECTION('center_axis',(0.,0.,1.));
#14404=DIRECTION('ref_axis',(-0.608812046626718,0.793314497461244,0.));
#14405=DIRECTION('',(0.,0.,1.));
#14406=DIRECTION('center_axis',(0.,0.,1.));
#14407=DIRECTION('ref_axis',(-0.608812046626718,0.793314497461244,0.));
#14408=DIRECTION('',(0.,0.,1.));
#14409=DIRECTION('center_axis',(0.,0.,1.));
#14410=DIRECTION('ref_axis',(-0.608812046626718,0.793314497461244,0.));
#14411=DIRECTION('',(0.,0.,1.));
#14412=DIRECTION('center_axis',(0.,0.,1.));
#14413=DIRECTION('ref_axis',(-0.608812046626718,0.793314497461244,0.));
#14414=DIRECTION('',(0.,0.,1.));
#14415=DIRECTION('center_axis',(0.,0.,1.));
#14416=DIRECTION('ref_axis',(-0.608812046626718,0.793314497461244,0.));
#14417=DIRECTION('',(0.,0.,1.));
#14418=DIRECTION('center_axis',(0.,0.,1.));
#14419=DIRECTION('ref_axis',(-0.608812046626718,0.793314497461244,0.));
#14420=DIRECTION('',(0.,0.,1.));
#14421=DIRECTION('center_axis',(0.,0.,1.));
#14422=DIRECTION('ref_axis',(1.,6.43162402581532E-14,0.));
#14423=DIRECTION('center_axis',(0.,0.,1.));
#14424=DIRECTION('ref_axis',(0.93738942346349,0.348283029702549,0.));
#14425=DIRECTION('',(0.,0.,1.));
#14426=DIRECTION('center_axis',(0.,0.,-1.));
#14427=DIRECTION('ref_axis',(1.,0.,0.));
#14428=DIRECTION('center_axis',(0.,0.,1.));
#14429=DIRECTION('ref_axis',(0.93738942346349,0.348283029702549,0.));
#14430=DIRECTION('',(0.,0.,1.));
#14431=DIRECTION('center_axis',(0.,0.,1.));
#14432=DIRECTION('ref_axis',(0.93738942346349,0.348283029702549,0.));
#14433=DIRECTION('',(0.,0.,1.));
#14434=DIRECTION('center_axis',(0.,0.,1.));
#14435=DIRECTION('ref_axis',(0.93738942346349,0.348283029702549,0.));
#14436=DIRECTION('',(0.,0.,1.));
#14437=DIRECTION('center_axis',(0.,0.,1.));
#14438=DIRECTION('ref_axis',(0.93738942346349,0.348283029702549,0.));
#14439=DIRECTION('',(0.,0.,1.));
#14440=DIRECTION('center_axis',(0.,0.,1.));
#14441=DIRECTION('ref_axis',(0.93738942346349,0.348283029702549,0.));
#14442=DIRECTION('',(0.,0.,1.));
#14443=DIRECTION('center_axis',(0.,0.,1.));
#14444=DIRECTION('ref_axis',(0.93738942346349,0.348283029702549,0.));
#14445=DIRECTION('',(0.,0.,1.));
#14446=DIRECTION('center_axis',(0.,0.,1.));
#14447=DIRECTION('ref_axis',(0.93738942346349,0.348283029702549,0.));
#14448=DIRECTION('',(0.,0.,1.));
#14449=DIRECTION('center_axis',(0.,0.,1.));
#14450=DIRECTION('ref_axis',(0.93738942346349,0.348283029702549,0.));
#14451=DIRECTION('',(0.,0.,1.));
#14452=DIRECTION('center_axis',(0.,0.,1.));
#14453=DIRECTION('ref_axis',(0.93738942346349,0.348283029702549,0.));
#14454=DIRECTION('',(0.,0.,1.));
#14455=DIRECTION('center_axis',(0.,0.,1.));
#14456=DIRECTION('ref_axis',(0.93738942346349,0.348283029702549,0.));
#14457=DIRECTION('',(0.,0.,1.));
#14458=DIRECTION('center_axis',(0.,0.,1.));
#14459=DIRECTION('ref_axis',(0.93738942346349,0.348283029702549,0.));
#14460=DIRECTION('',(0.,0.,1.));
#14461=DIRECTION('center_axis',(0.,0.,-1.));
#14462=DIRECTION('ref_axis',(1.,0.,0.));
#14463=DIRECTION('center_axis',(0.,0.,1.));
#14464=DIRECTION('ref_axis',(0.93738942346349,0.348283029702549,0.));
#14465=DIRECTION('center_axis',(0.,0.,1.));
#14466=DIRECTION('ref_axis',(-0.608812046626718,0.793314497461244,0.));
#14467=DIRECTION('center_axis',(0.,0.,1.));
#14468=DIRECTION('ref_axis',(1.,0.,0.));
#14469=DIRECTION('center_axis',(0.,0.,1.));
#14470=DIRECTION('ref_axis',(0.,-1.,0.));
#14471=DIRECTION('',(-0.990431813260487,0.138002982871906,0.));
#14472=DIRECTION('center_axis',(0.,0.,1.));
#14473=DIRECTION('ref_axis',(1.,0.,0.));
#14474=DIRECTION('',(0.999687555793007,0.0249958155018767,0.));
#14475=DIRECTION('center_axis',(0.,0.,1.));
#14476=DIRECTION('ref_axis',(0.,-1.,0.));
#14477=DIRECTION('',(-0.977901266293703,-0.209067246074493,0.));
#14478=DIRECTION('center_axis',(0.,0.,1.));
#14479=DIRECTION('ref_axis',(1.,0.,0.));
#14480=DIRECTION('',(0.930849946869696,0.365401664490851,0.));
#14481=DIRECTION('center_axis',(0.,0.,1.));
#14482=DIRECTION('ref_axis',(0.,-1.,0.));
#14483=DIRECTION('',(-0.847421394326308,-0.530920879640325,0.));
#14484=DIRECTION('center_axis',(0.,0.,1.));
#14485=DIRECTION('ref_axis',(1.,0.,0.));
#14486=DIRECTION('',(0.749738096471781,0.661734679988038,0.));
#14487=DIRECTION('center_axis',(0.,0.,1.));
#14488=DIRECTION('ref_axis',(0.,-1.,0.));
#14489=DIRECTION('',(-0.614729995595327,-0.788737619563926,0.));
#14490=DIRECTION('center_axis',(0.,0.,1.));
#14491=DIRECTION('ref_axis',(1.,0.,0.));
#14492=DIRECTION('',(0.478196766683598,0.87825272691484,0.));
#14493=DIRECTION('center_axis',(0.,0.,1.));
#14494=DIRECTION('ref_axis',(0.,-1.,0.));
#14495=DIRECTION('',(-0.307893086947081,-0.951420962040567,0.));
#14496=DIRECTION('center_axis',(0.,0.,1.));
#14497=DIRECTION('ref_axis',(1.,0.,0.));
#14498=DIRECTION('',(0.148977849400632,0.98884053334598,0.));
#14499=DIRECTION('center_axis',(0.,0.,1.));
#14500=DIRECTION('ref_axis',(0.,-1.,0.));
#14501=DIRECTION('',(0.0360802720049828,-0.999348895017174,0.));
#14502=DIRECTION('center_axis',(0.,0.,1.));
#14503=DIRECTION('ref_axis',(1.,0.,0.));
#14504=DIRECTION('',(-0.198209995198882,0.980159577723576,0.));
#14505=DIRECTION('center_axis',(0.,0.,1.));
#14506=DIRECTION('ref_axis',(0.,-1.,0.));
#14507=DIRECTION('',(0.375701817665145,-0.92674060243582,0.));
#14508=DIRECTION('center_axis',(0.,0.,1.));
#14509=DIRECTION('ref_axis',(1.,0.,0.));
#14510=DIRECTION('',(-0.521490789109412,0.853256911412994,0.));
#14511=DIRECTION('center_axis',(0.,0.,1.));
#14512=DIRECTION('ref_axis',(0.,-1.,0.));
#14513=DIRECTION('',(0.670008179346718,-0.742353715965978,0.));
#14514=DIRECTION('center_axis',(0.,0.,1.));
#14515=DIRECTION('ref_axis',(1.,0.,0.));
#14516=DIRECTION('',(-0.781872097469079,0.623438868855081,0.));
#14517=DIRECTION('center_axis',(0.,0.,1.));
#14518=DIRECTION('ref_axis',(0.,-1.,0.));
#14519=DIRECTION('',(0.883501666331281,-0.468428015376802,0.));
#14520=DIRECTION('center_axis',(0.,0.,1.));
#14521=DIRECTION('ref_axis',(1.,0.,0.));
#14522=DIRECTION('',(-0.947948091670679,0.318424897735586,0.));
#14523=DIRECTION('center_axis',(0.,0.,1.));
#14524=DIRECTION('ref_axis',(0.,-1.,0.));
#14525=DIRECTION('',(0.990431813260487,-0.138002982871907,0.));
#14526=DIRECTION('center_axis',(0.,0.,1.));
#14527=DIRECTION('ref_axis',(1.,0.,0.));
#14528=DIRECTION('',(-0.999687555793007,-0.0249958155018767,0.));
#14529=DIRECTION('center_axis',(0.,0.,1.));
#14530=DIRECTION('ref_axis',(0.,-1.,0.));
#14531=DIRECTION('',(0.977901266293703,0.209067246074493,0.));
#14532=DIRECTION('center_axis',(0.,0.,1.));
#14533=DIRECTION('ref_axis',(1.,0.,0.));
#14534=DIRECTION('',(-0.930849946869696,-0.365401664490851,0.));
#14535=DIRECTION('center_axis',(0.,0.,1.));
#14536=DIRECTION('ref_axis',(0.,-1.,0.));
#14537=DIRECTION('',(0.847421394326308,0.530920879640325,0.));
#14538=DIRECTION('center_axis',(0.,0.,1.));
#14539=DIRECTION('ref_axis',(1.,0.,0.));
#14540=DIRECTION('',(-0.749738096471781,-0.661734679988038,0.));
#14541=DIRECTION('center_axis',(0.,0.,1.));
#14542=DIRECTION('ref_axis',(0.,-1.,0.));
#14543=DIRECTION('',(0.614729995595327,0.788737619563926,0.));
#14544=DIRECTION('center_axis',(0.,0.,1.));
#14545=DIRECTION('ref_axis',(1.,0.,0.));
#14546=DIRECTION('',(-0.478196766683598,-0.87825272691484,0.));
#14547=DIRECTION('center_axis',(0.,0.,1.));
#14548=DIRECTION('ref_axis',(0.,-1.,0.));
#14549=DIRECTION('',(0.307893086947081,0.951420962040567,0.));
#14550=DIRECTION('center_axis',(0.,0.,1.));
#14551=DIRECTION('ref_axis',(1.,0.,0.));
#14552=DIRECTION('',(-0.148977849400632,-0.98884053334598,0.));
#14553=DIRECTION('center_axis',(0.,0.,1.));
#14554=DIRECTION('ref_axis',(0.,-1.,0.));
#14555=DIRECTION('',(-0.0360802720049828,0.999348895017174,0.));
#14556=DIRECTION('center_axis',(0.,0.,1.));
#14557=DIRECTION('ref_axis',(1.,0.,0.));
#14558=DIRECTION('',(0.198209995198882,-0.980159577723576,0.));
#14559=DIRECTION('center_axis',(0.,0.,1.));
#14560=DIRECTION('ref_axis',(0.,-1.,0.));
#14561=DIRECTION('',(-0.375701817665128,0.926740602435827,0.));
#14562=DIRECTION('center_axis',(0.,0.,1.));
#14563=DIRECTION('ref_axis',(1.,0.,0.));
#14564=DIRECTION('',(0.521490789109416,-0.853256911412992,0.));
#14565=DIRECTION('center_axis',(0.,0.,1.));
#14566=DIRECTION('ref_axis',(0.,-1.,0.));
#14567=DIRECTION('',(-0.670008179346718,0.742353715965978,0.));
#14568=DIRECTION('center_axis',(0.,0.,1.));
#14569=DIRECTION('ref_axis',(1.,0.,0.));
#14570=DIRECTION('',(0.781872097469079,-0.623438868855081,0.));
#14571=DIRECTION('center_axis',(0.,0.,1.));
#14572=DIRECTION('ref_axis',(0.,-1.,0.));
#14573=DIRECTION('',(-0.883501666331281,0.468428015376802,0.));
#14574=DIRECTION('center_axis',(0.,0.,1.));
#14575=DIRECTION('ref_axis',(1.,0.,0.));
#14576=DIRECTION('',(0.947948091670678,-0.318424897735588,0.));
#14577=DIRECTION('center_axis',(0.,0.,-1.));
#14578=DIRECTION('ref_axis',(-1.,0.,0.));
#14579=DIRECTION('',(0.474277008002355,-0.880375669632194,0.));
#14580=DIRECTION('center_axis',(0.,0.,1.));
#14581=DIRECTION('ref_axis',(1.,0.,0.));
#14582=DIRECTION('',(-0.990722494271237,0.13590047588209,0.));
#14583=DIRECTION('center_axis',(0.,0.,-1.));
#14584=DIRECTION('ref_axis',(0.796664686286605,-0.60442152313089,0.));
#14585=DIRECTION('center_axis',(0.,0.,-1.));
#14586=DIRECTION('ref_axis',(-1.,0.,0.));
#14587=DIRECTION('',(0.144555196347935,-0.98949673835178,0.));
#14588=DIRECTION('center_axis',(0.,0.,1.));
#14589=DIRECTION('ref_axis',(1.,0.,0.));
#14590=DIRECTION('',(-0.884491140557834,0.466556987167379,0.));
#14591=DIRECTION('center_axis',(0.,0.,-1.));
#14592=DIRECTION('ref_axis',(0.541895590973931,-0.840445815316499,0.));
#14593=DIRECTION('center_axis',(0.,0.,-1.));
#14594=DIRECTION('ref_axis',(-1.,0.,0.));
#14595=DIRECTION('',(-0.202590371288481,-0.979263570986481,0.));
#14596=DIRECTION('center_axis',(0.,0.,1.));
#14597=DIRECTION('ref_axis',(1.,0.,0.));
#14598=DIRECTION('',(-0.671582337664226,0.74092993173272,0.));
#14599=DIRECTION('center_axis',(0.,0.,-1.));
#14600=DIRECTION('ref_axis',(0.221765889862626,-0.975099938515759,0.));
#14601=DIRECTION('center_axis',(0.,0.,-1.));
#14602=DIRECTION('ref_axis',(-1.,0.,0.));
#14603=DIRECTION('',(-0.525300549059025,-0.850916760416838,-1.44557603741106E-12));
#14604=DIRECTION('center_axis',(0.,0.,1.));
#14605=DIRECTION('ref_axis',(1.,0.,0.));
#14606=DIRECTION('',(-0.377668004938845,0.92594107698358,0.));
#14607=DIRECTION('center_axis',(0.,0.,-1.));
#14608=DIRECTION('ref_axis',(-0.125112050482103,-0.992142618187609,0.));
#14609=DIRECTION('center_axis',(0.,0.,-1.));
#14610=DIRECTION('ref_axis',(-1.,0.,0.));
#14611=DIRECTION('',(-0.78465171542998,-0.619936839906123,0.));
#14612=DIRECTION('center_axis',(0.,0.,1.));
#14613=DIRECTION('ref_axis',(1.,0.,0.));
#14614=DIRECTION('',(-0.0381953670132134,0.999270290731555,0.));
#14615=DIRECTION('center_axis',(0.,0.,-1.));
#14616=DIRECTION('ref_axis',(-0.456899631081401,-0.889518255640479,0.));
#14617=DIRECTION('center_axis',(0.,0.,-1.));
#14618=DIRECTION('ref_axis',(-1.,0.,0.));
#14619=DIRECTION('',(-0.949362313354307,-0.314183382728237,0.));
#14620=DIRECTION('center_axis',(0.,0.,1.));
#14621=DIRECTION('ref_axis',(1.,0.,0.));
#14622=DIRECTION('',(0.305872997935251,0.952072323478685,0.));
#14623=DIRECTION('center_axis',(0.,0.,-1.));
#14624=DIRECTION('ref_axis',(-0.733578373052014,-0.679604863571738,0.));
#14625=DIRECTION('center_axis',(0.,0.,-1.));
#14626=DIRECTION('ref_axis',(-1.,0.,0.));
#14627=DIRECTION('',(-0.999565805862472,0.0294652295173026,-1.4455760374657E-12));
#14628=DIRECTION('center_axis',(0.,0.,1.));
#14629=DIRECTION('ref_axis',(1.,0.,0.));
#14630=DIRECTION('',(0.613059210435848,0.790036964008504,0.));
#14631=DIRECTION('center_axis',(0.,0.,-1.));
#14632=DIRECTION('ref_axis',(-0.921776736768698,-0.387721095056807,0.));
#14633=DIRECTION('center_axis',(0.,0.,-1.));
#14634=DIRECTION('ref_axis',(-1.,0.,0.));
#14635=DIRECTION('',(-0.929206905711275,0.36955990905194,0.));
#14636=DIRECTION('center_axis',(0.,0.,1.));
#14637=DIRECTION('ref_axis',(1.,0.,0.));
#14638=DIRECTION('',(0.846292579865157,0.532718377067262,0.));
#14639=DIRECTION('center_axis',(0.,0.,-1.));
#14640=DIRECTION('ref_axis',(-0.998795222055377,-0.049072440323971,0.));
#14641=DIRECTION('center_axis',(0.,0.,-1.));
#14642=DIRECTION('ref_axis',(-1.,0.,0.));
#14643=DIRECTION('',(-0.746771944067323,0.66508019332552,0.));
#14644=DIRECTION('center_axis',(0.,0.,1.));
#14645=DIRECTION('ref_axis',(1.,0.,0.));
#14646=DIRECTION('',(0.977455315104272,0.211142385546837,0.));
#14647=DIRECTION('center_axis',(0.,0.,-1.));
#14648=DIRECTION('ref_axis',(-0.955344262914612,0.295495074943961,0.));
#14649=DIRECTION('center_axis',(0.,0.,-1.));
#14650=DIRECTION('ref_axis',(-1.,0.,0.));
#14651=DIRECTION('',(-0.474265266635988,0.880381994853765,0.));
#14652=DIRECTION('center_axis',(0.,0.,1.));
#14653=DIRECTION('ref_axis',(1.,0.,0.));
#14654=DIRECTION('',(0.990722494271013,-0.135900475883722,0.));
#14655=DIRECTION('center_axis',(0.,0.,-1.));
#14656=DIRECTION('ref_axis',(-0.796664686286608,0.604421523130886,0.));
#14657=DIRECTION('center_axis',(0.,0.,-1.));
#14658=DIRECTION('ref_axis',(-1.,0.,0.));
#14659=DIRECTION('',(-0.144555196349004,0.989496738351623,0.));
#14660=DIRECTION('center_axis',(0.,0.,1.));
#14661=DIRECTION('ref_axis',(1.,0.,0.));
#14662=DIRECTION('',(0.884491140558253,-0.466556987166584,0.));
#14663=DIRECTION('center_axis',(0.,0.,-1.));
#14664=DIRECTION('ref_axis',(-0.541895590973931,0.840445815316499,0.));
#14665=DIRECTION('center_axis',(0.,0.,-1.));
#14666=DIRECTION('ref_axis',(-1.,0.,0.));
#14667=DIRECTION('',(0.202590371280164,0.979263570988202,0.));
#14668=DIRECTION('center_axis',(0.,0.,1.));
#14669=DIRECTION('ref_axis',(1.,0.,0.));
#14670=DIRECTION('',(0.671582337664788,-0.740929931732211,1.44548415250913E-12));
#14671=DIRECTION('center_axis',(0.,0.,-1.));
#14672=DIRECTION('ref_axis',(-0.221765889862635,0.975099938515757,0.));
#14673=DIRECTION('center_axis',(0.,0.,-1.));
#14674=DIRECTION('ref_axis',(-1.,0.,0.));
#14675=DIRECTION('',(0.525300549057258,0.850916760417929,0.));
#14676=DIRECTION('center_axis',(0.,0.,1.));
#14677=DIRECTION('ref_axis',(1.,0.,0.));
#14678=DIRECTION('',(0.377668004939932,-0.925941076983137,0.));
#14679=DIRECTION('center_axis',(0.,0.,-1.));
#14680=DIRECTION('ref_axis',(0.125112050482093,0.99214261818761,0.));
#14681=DIRECTION('center_axis',(0.,0.,-1.));
#14682=DIRECTION('ref_axis',(-1.,0.,0.));
#14683=DIRECTION('',(0.784651716122117,0.619936839030088,1.4455738977615E-12));
#14684=DIRECTION('center_axis',(0.,0.,1.));
#14685=DIRECTION('ref_axis',(1.,0.,0.));
#14686=DIRECTION('',(0.0381953670132134,-0.999270290731555,0.));
#14687=DIRECTION('center_axis',(0.,0.,-1.));
#14688=DIRECTION('ref_axis',(0.456899631081495,0.88951825564043,0.));
#14689=DIRECTION('center_axis',(0.,0.,-1.));
#14690=DIRECTION('ref_axis',(-1.,0.,0.));
#14691=DIRECTION('',(0.949362313026162,0.314183383719787,-1.44557603741564E-12));
#14692=DIRECTION('center_axis',(0.,0.,1.));
#14693=DIRECTION('ref_axis',(1.,0.,0.));
#14694=DIRECTION('',(-0.305872997971906,-0.952072323466909,1.44548415256294E-12));
#14695=DIRECTION('center_axis',(0.,0.,-1.));
#14696=DIRECTION('ref_axis',(0.733578373052045,0.679604863571704,0.));
#14697=DIRECTION('center_axis',(0.,0.,-1.));
#14698=DIRECTION('ref_axis',(-1.,0.,0.));
#14699=DIRECTION('',(0.999565805862573,-0.0294652295138758,0.));
#14700=DIRECTION('center_axis',(0.,0.,1.));
#14701=DIRECTION('ref_axis',(1.,0.,0.));
#14702=DIRECTION('',(-0.613059210433514,-0.790036964010315,0.));
#14703=DIRECTION('center_axis',(0.,0.,-1.));
#14704=DIRECTION('ref_axis',(0.921776736768698,0.387721095056807,0.));
#14705=DIRECTION('center_axis',(0.,0.,-1.));
#14706=DIRECTION('ref_axis',(-1.,0.,0.));
#14707=DIRECTION('',(0.92921182631369,-0.36954753664282,0.));
#14708=DIRECTION('center_axis',(0.,0.,1.));
#14709=DIRECTION('ref_axis',(1.,0.,0.));
#14710=DIRECTION('',(-0.846292579863551,-0.532718377069813,0.));
#14711=DIRECTION('center_axis',(0.,0.,-1.));
#14712=DIRECTION('ref_axis',(0.998795222055378,0.0490724403239548,0.));
#14713=DIRECTION('center_axis',(0.,0.,-1.));
#14714=DIRECTION('ref_axis',(-1.,0.,0.));
#14715=DIRECTION('',(0.746780806816249,-0.665070241832298,-1.44557391839046E-12));
#14716=DIRECTION('center_axis',(0.,0.,1.));
#14717=DIRECTION('ref_axis',(1.,0.,0.));
#14718=DIRECTION('',(-0.977456573143307,-0.211136561540019,0.));
#14719=DIRECTION('center_axis',(0.,0.,-1.));
#14720=DIRECTION('ref_axis',(0.955344262914614,-0.295495074943952,0.));
#14721=DIRECTION('center_axis',(0.,0.,-1.));
#14722=DIRECTION('ref_axis',(0.,-1.,0.));
#14723=DIRECTION('center_axis',(-0.619032382875318,-0.33848017230615,-0.708681932821279));
#14724=DIRECTION('ref_axis',(-0.451228736779563,0.891841105362626,-0.0318130459071304));
#14725=DIRECTION('center_axis',(0.67086774319136,0.218417923344258,0.708681932821286));
#14726=DIRECTION('ref_axis',(-0.287922260464996,0.957389170141623,-0.0225110822543487));
#14727=DIRECTION('',(-0.685495936603333,-0.181409993675129,0.705113987306385));
#14728=DIRECTION('',(0.645329675210074,0.295341295811932,-0.70450204348986));
#14729=DIRECTION('center_axis',(0.,0.,-1.));
#14730=DIRECTION('ref_axis',(0.,-1.,0.));
#14731=DIRECTION('center_axis',(-0.465933125170307,-0.529788864512786,-0.708681932821265));
#14732=DIRECTION('ref_axis',(-0.729043936918215,0.683727188396728,-0.0318130459072231));
#14733=DIRECTION('center_axis',(0.555706138352604,0.43469599249356,0.708681932821259));
#14734=DIRECTION('ref_axis',(-0.598004804709664,0.8011763256112,-0.0225110822550398));
#14735=DIRECTION('',(-0.582109601172995,-0.404923050876555,0.7051139873035));
#14736=DIRECTION('',(0.505398861452357,0.498245784270093,-0.704502043502885));
#14737=DIRECTION('center_axis',(0.,0.,-1.));
#14738=DIRECTION('ref_axis',(0.,-1.,0.));
#14739=DIRECTION('center_axis',(-0.256635456129185,-0.657197200808165,-0.70868193282126));
#14740=DIRECTION('ref_axis',(-0.918925678721932,0.393145681771461,-0.0318130459071376));
#14741=DIRECTION('center_axis',(0.37351817187998,0.598543309517481,0.708681932821276));
#14742=DIRECTION('ref_axis',(-0.83595914389466,0.548329792109296,-0.0225110822547992));
#14743=DIRECTION('',(-0.408512256818674,-0.579596412148449,0.705113987276922));
#14744=DIRECTION('',(0.304509486091619,0.641054477849826,-0.704502043509389));
#14745=DIRECTION('center_axis',(0.,0.,-1.));
#14746=DIRECTION('ref_axis',(0.0617633245521631,0.998090823392473,0.));
#14747=DIRECTION('center_axis',(-0.0163837635432463,-0.705337855488318,
-0.708681932821276));
#14748=DIRECTION('ref_axis',(-0.997971421773015,0.0551450037126303,-0.0318130459070098));
#14749=DIRECTION('center_axis',(0.146278401337234,0.6901974698555,0.708681932821269));
#14750=DIRECTION('ref_axis',(-0.973084472883285,0.229346593192864,-0.022511082254869));
#14751=DIRECTION('',(-0.185642305292501,-0.684361892155193,0.705113987275426));
#14752=DIRECTION('',(0.0668917726419952,0.70654254045347,-0.704502043490556));
#14753=DIRECTION('center_axis',(0.,0.,-1.));
#14754=DIRECTION('ref_axis',(0.,-1.,0.));
#14755=DIRECTION('center_axis',(0.225844052724809,-0.668404355118618,-0.708681932821275));
#14756=DIRECTION('ref_axis',(-0.95664708286883,-0.289506975647697,-0.0318130459070163));
#14757=DIRECTION('center_axis',(-0.0986047032458038,0.69860362909915,0.708681932821279));
#14758=DIRECTION('ref_axis',(-0.992841453244872,-0.117299189657614,-0.0225110822546955));
#14759=DIRECTION('',(0.0596188480477669,-0.706583227868191,0.705113987276402));
#14760=DIRECTION('',(-0.1787940758072,0.686811145215674,-0.704502043477365));
#14761=DIRECTION('center_axis',(0.,0.,-1.));
#14762=DIRECTION('ref_axis',(0.,-1.,0.));
#14763=DIRECTION('center_axis',(0.440831743130997,-0.550851424923984,-0.708681932821279));
#14764=DIRECTION('ref_axis',(-0.799936987163271,-0.599240141077255,-0.0318130459066631));
#14765=DIRECTION('center_axis',(-0.331594625366901,0.622747880382156,0.708681932821288));
#14766=DIRECTION('ref_axis',(-0.892847101565944,-0.449796959083795,-0.0225110822543812));
#14767=DIRECTION('',(0.297689088430308,-0.643580198230555,0.705113987292163));
#14768=DIRECTION('',(-0.402914719960345,0.584240189604372,-0.704502043496202));
#14769=DIRECTION('center_axis',(0.,0.,-1.));
#14770=DIRECTION('ref_axis',(0.,-1.,0.));
#14771=DIRECTION('center_axis',(0.60264861933197,-0.366857683182414,-0.708681932821278));
#14772=DIRECTION('ref_axis',(-0.546742684993606,-0.836696101649882,-0.0318130459068674));
#14773=DIRECTION('center_axis',(-0.524589341853953,0.471779546510804,0.708681932821274));
#14774=DIRECTION('ref_axis',(-0.685162212418179,-0.728042576948589,-0.0225110822548518));
#14775=DIRECTION('',(0.499853631303652,-0.502951898509268,0.705113987280408));
#14776=DIRECTION('',(-0.578437902573191,0.411201244629492,-0.704502043490212));
#14777=DIRECTION('center_axis',(0.,0.,-1.));
#14778=DIRECTION('ref_axis',(0.,-1.,0.));
#14779=DIRECTION('center_axis',(0.691777177895169,-0.138615490606495,-0.708681932821288));
#14780=DIRECTION('ref_axis',(-0.227603145951143,-0.973234164044439,-0.0318130459067542));
#14781=DIRECTION('center_axis',(-0.654310841598713,0.263907636606227,0.708681932821276));
#14782=DIRECTION('ref_axis',(-0.394836648535736,-0.918475515269075,-0.0225110822546137));
#14783=DIRECTION('',(0.641728449228522,-0.301660176976957,0.705113987293535));
#14784=DIRECTION('',(-0.684192937232473,0.188565360909515,-0.704502043507516));
#14785=DIRECTION('center_axis',(0.,0.,-1.));
#14786=DIRECTION('ref_axis',(0.,-1.,0.));
#14787=DIRECTION('center_axis',(0.697467199260489,0.106345775884312,-0.708681932821271));
#14788=DIRECTION('ref_axis',(0.118988691558466,-0.992385822848809,-0.0318130459072569));
#14789=DIRECTION('center_axis',(-0.705112797247349,0.0242045708643797,0.70868193282127));
#14790=DIRECTION('ref_axis',(-0.0568879576711038,-0.998126751193317,-0.0225110822548537));
#14791=DIRECTION('',(0.706201345226432,-0.0639837860996167,0.705113987321721));
#14792=DIRECTION('',(-0.707424206095769,-0.056814288281615,-0.704502043486621));
#14793=DIRECTION('center_axis',(0.,0.,-1.));
#14794=DIRECTION('ref_axis',(0.,-1.,0.));
#14795=DIRECTION('center_axis',(0.61903238287525,0.338480172306288,-0.708681932821273));
#14796=DIRECTION('ref_axis',(0.451228736779656,-0.891841105362575,-0.0318130459072342));
#14797=DIRECTION('center_axis',(-0.670867743191319,-0.218417923344399,0.708681932821281));
#14798=DIRECTION('ref_axis',(0.287922260465025,-0.957389170141609,-0.0225110822545478));
#14799=DIRECTION('',(0.685495936588057,0.181409993663856,0.705113987324136));
#14800=DIRECTION('',(-0.645329675209038,-0.295341295816895,-0.704502043488729));
#14801=DIRECTION('center_axis',(0.,0.,-1.));
#14802=DIRECTION('ref_axis',(0.,-1.,0.));
#14803=DIRECTION('center_axis',(0.465933125169797,0.529788864513252,-0.708681932821252));
#14804=DIRECTION('ref_axis',(0.729043936918548,-0.683727188396351,-0.031813045907688));
#14805=DIRECTION('center_axis',(-0.55570613835297,-0.434695992493057,0.70868193282128));
#14806=DIRECTION('ref_axis',(0.598004804709207,-0.80117632561155,-0.0225110822547272));
#14807=DIRECTION('',(0.58210960117426,0.404923050894126,0.705113987292365));
#14808=DIRECTION('',(-0.505398861452357,-0.498245784270093,-0.704502043502885));
#14809=DIRECTION('center_axis',(0.,0.,-1.));
#14810=DIRECTION('ref_axis',(0.,-1.,0.));
#14811=DIRECTION('center_axis',(0.256635456129172,0.657197200808164,-0.708681932821267));
#14812=DIRECTION('ref_axis',(0.918925678721868,-0.393145681771596,-0.0318130459073145));
#14813=DIRECTION('center_axis',(-0.373518171879956,-0.598543309517493,0.708681932821278));
#14814=DIRECTION('ref_axis',(0.835959143894646,-0.548329792109316,-0.0225110822548671));
#14815=DIRECTION('',(0.408512256819533,0.579596412136736,0.705113987286052));
#14816=DIRECTION('',(-0.304509486097168,-0.641054477848632,-0.704502043508077));
#14817=DIRECTION('center_axis',(0.,0.,-1.));
#14818=DIRECTION('ref_axis',(0.,-1.,0.));
#14819=DIRECTION('center_axis',(0.0163837635434838,0.705337855488308,-0.708681932821281));
#14820=DIRECTION('ref_axis',(0.997971421773012,-0.0551450037127905,-0.0318130459068232));
#14821=DIRECTION('center_axis',(-0.146278401337369,-0.690197469855462,0.708681932821278));
#14822=DIRECTION('ref_axis',(0.973084472883258,-0.229346593192995,-0.0225110822547478));
#14823=DIRECTION('',(0.185642305292172,0.684361892155236,0.705113987275471));
#14824=DIRECTION('',(-0.0668917726414032,-0.706542540453498,-0.704502043490584));
#14825=DIRECTION('center_axis',(0.,0.,-1.));
#14826=DIRECTION('ref_axis',(0.,-1.,0.));
#14827=DIRECTION('center_axis',(-0.225844052724565,0.668404355118693,-0.708681932821282));
#14828=DIRECTION('ref_axis',(0.956647082868877,0.289506975647566,-0.0318130459067811));
#14829=DIRECTION('center_axis',(0.0986047032463636,-0.698603629099088,0.708681932821262));
#14830=DIRECTION('ref_axis',(0.992841453244803,0.117299189658157,-0.0225110822549345));
#14831=DIRECTION('',(-0.0596188480500861,0.706583227852509,0.70511398729192));
#14832=DIRECTION('',(0.178794075800621,-0.686811145216509,-0.704502043478221));
#14833=DIRECTION('center_axis',(0.,0.,-1.));
#14834=DIRECTION('ref_axis',(0.,-1.,0.));
#14835=DIRECTION('center_axis',(-0.440831743131266,0.550851424923786,-0.708681932821265));
#14836=DIRECTION('ref_axis',(0.799936987163221,0.599240141077298,-0.031813045907131));
#14837=DIRECTION('center_axis',(0.331594625366664,-0.622747880382285,0.708681932821286));
#14838=DIRECTION('ref_axis',(0.892847101566032,0.449796959083631,-0.0225110822541639));
#14839=DIRECTION('',(-0.297689088430928,0.643580198230424,0.70511398729202));
#14840=DIRECTION('',(0.402914719960345,-0.584240189604372,-0.704502043496202));
#14841=DIRECTION('center_axis',(0.,0.,-1.));
#14842=DIRECTION('ref_axis',(0.,-1.,0.));
#14843=DIRECTION('center_axis',(-0.602648619332025,0.366857683182321,-0.70868193282128));
#14844=DIRECTION('ref_axis',(0.546742684993566,0.836696101649904,-0.0318130459069726));
#14845=DIRECTION('center_axis',(0.524589341854173,-0.471779546510578,0.708681932821261));
#14846=DIRECTION('ref_axis',(0.685162212417927,0.728042576948822,-0.022511082254977));
#14847=DIRECTION('',(-0.499853631345304,0.502951898491402,0.705113987263625));
#14848=DIRECTION('',(0.578437902573191,-0.411201244629492,-0.704502043490212));
#14849=DIRECTION('center_axis',(0.,0.,-1.));
#14850=DIRECTION('ref_axis',(0.,-1.,0.));
#14851=DIRECTION('center_axis',(-0.697467199260449,-0.106345775884652,-0.70868193282126));
#14852=DIRECTION('ref_axis',(-0.118988691558859,0.992385822848759,-0.0318130459073474));
#14853=DIRECTION('center_axis',(0.705112797247378,-0.0242045708638981,0.708681932821257));
#14854=DIRECTION('ref_axis',(0.0568879576706311,0.998126751193339,-0.0225110822550593));
#14855=DIRECTION('',(-0.706201345257537,0.0639837861036678,0.7051139872902));
#14856=DIRECTION('',(0.707424206095769,0.056814288281615,-0.704502043486621));
#14857=DIRECTION('center_axis',(0.,0.,-1.));
#14858=DIRECTION('ref_axis',(0.,-1.,0.));
#14859=DIRECTION('center_axis',(-0.691777177895279,0.138615490606009,-0.708681932821276));
#14860=DIRECTION('ref_axis',(0.227603145950679,0.97323416404454,-0.0318130459069853));
#14861=DIRECTION('center_axis',(0.654310841598881,-0.263907636605812,0.708681932821276));
#14862=DIRECTION('ref_axis',(0.394836648535391,0.918475515269218,-0.0225110822548663));
#14863=DIRECTION('',(-0.641728449232441,0.3016601769701,0.705113987292902));
#14864=DIRECTION('',(0.684192937233218,-0.188565360903944,-0.704502043508283));
#14865=DIRECTION('center_axis',(0.,0.,1.));
#14866=DIRECTION('ref_axis',(0.,-1.,0.));
#14867=DIRECTION('center_axis',(-0.703660934063436,0.0512953015946455,0.708681932821268));
#14868=DIRECTION('ref_axis',(-0.040760194859215,-0.998662373690501,0.031813045907198));
#14869=DIRECTION('center_axis',(0.,0.,-1.));
#14870=DIRECTION('ref_axis',(0.,-1.,0.));
#14871=DIRECTION('center_axis',(0.701040101070486,0.0794524687080656,-0.70868193282126));
#14872=DIRECTION('ref_axis',(0.135024713403112,-0.990586481810706,0.0225110822551012));
#14873=DIRECTION('',(-0.699004252188757,-0.119194464416953,-0.705113987291694));
#14874=DIRECTION('center_axis',(0.,0.,1.));
#14875=DIRECTION('ref_axis',(1.,0.,0.));
#14876=DIRECTION('',(0.709701051035535,-0.00113528531252956,0.704502043493358));
#14877=DIRECTION('center_axis',(0.,0.,1.));
#14878=DIRECTION('ref_axis',(0.,-1.,0.));
#14879=DIRECTION('center_axis',(-0.678769013677884,-0.19246439713213,0.708681932821289));
#14880=DIRECTION('ref_axis',(0.303260593853006,-0.952376470901111,0.0318130459067882));
#14881=DIRECTION('center_axis',(0.,0.,-1.));
#14882=DIRECTION('ref_axis',(0.,-1.,0.));
#14883=DIRECTION('center_axis',(0.631587865115614,0.314430734393761,-0.708681932821277));
#14884=DIRECTION('ref_axis',(0.465682257294193,-0.884665635377067,0.0225110822546476));
#14885=DIRECTION('',(-0.616082229859789,-0.351079693163982,-0.705113987309055));
#14886=DIRECTION('center_axis',(0.,0.,1.));
#14887=DIRECTION('ref_axis',(1.,0.,0.));
#14888=DIRECTION('',(0.66728913109891,0.241665235964873,0.704502043462831));
#14889=DIRECTION('center_axis',(0.,0.,1.));
#14890=DIRECTION('ref_axis',(0.,-1.,0.));
#14891=DIRECTION('center_axis',(-0.572007532679314,-0.413010049091819,0.708681932821274));
#14892=DIRECTION('ref_axis',(0.610703679296142,-0.791219910141464,0.0318130459071324));
#14893=DIRECTION('center_axis',(0.,0.,-1.));
#14894=DIRECTION('ref_axis',(0.,-1.,0.));
#14895=DIRECTION('center_axis',(0.485956811383988,0.511484013007474,-0.708681932821261));
#14896=DIRECTION('ref_axis',(0.740171648217135,-0.672041057042826,0.0225110822550047));
#14897=DIRECTION('',(-0.458851598246782,-0.540619529544785,-0.705113987282304));
#14898=DIRECTION('center_axis',(0.,0.,1.));
#14899=DIRECTION('ref_axis',(1.,0.,0.));
#14900=DIRECTION('',(0.544392293801187,0.455317363180238,0.704502043457986));
#14901=DIRECTION('center_axis',(0.,0.,1.));
#14902=DIRECTION('ref_axis',(0.,-1.,0.));
#14903=DIRECTION('center_axis',(-0.396253501306999,-0.583740593752603,0.708681932821279));
#14904=DIRECTION('ref_axis',(0.844486887990209,-0.534630551056288,0.0318130459067074));
#14905=DIRECTION('center_axis',(0.,0.,-1.));
#14906=DIRECTION('ref_axis',(0.,-1.,0.));
#14907=DIRECTION('center_axis',(0.281712194240451,0.646844770952772,-0.708681932821267));
#14908=DIRECTION('ref_axis',(0.925385414595141,-0.378358408959404,0.0225110822549279));
#14909=DIRECTION('',(-0.24627669192658,-0.664952671929248,-0.705113987315423));
#14910=DIRECTION('center_axis',(0.,0.,1.));
#14911=DIRECTION('ref_axis',(1.,0.,0.));
#14912=DIRECTION('',(0.355833711437326,0.614051496670459,0.704502043461555));
#14913=DIRECTION('center_axis',(0.,0.,1.));
#14914=DIRECTION('ref_axis',(0.,-1.,0.));
#14915=DIRECTION('center_axis',(-0.172705449598815,-0.684063407712745,0.708681932821276));
#14916=DIRECTION('ref_axis',(0.976412514693378,-0.21355685720732,0.0318130459070931));
#14917=DIRECTION('center_axis',(0.,0.,-1.));
#14918=DIRECTION('ref_axis',(0.,-1.,0.));
#14919=DIRECTION('center_axis',(0.0434889288417849,0.704186503109001,-0.708681932821284));
#14920=DIRECTION('ref_axis',(0.998984042738759,-0.0390401527796353,0.0225110822545011));
#14921=DIRECTION('',(-0.0039971818986142,-0.70908270844906,-0.705113987320784));
#14922=DIRECTION('center_axis',(0.,0.,1.));
#14923=DIRECTION('ref_axis',(1.,0.,0.));
#14924=DIRECTION('',(0.124356331985472,0.698721957173194,0.704502043474098));
#14925=DIRECTION('center_axis',(0.,0.,1.));
#14926=DIRECTION('ref_axis',(0.,-1.,0.));
#14927=DIRECTION('center_axis',(0.0716734281918473,-0.701878079002291,0.708681932821264));
#14928=DIRECTION('ref_axis',(0.990568381810636,0.133274945384173,0.0318130459073441));
#14929=DIRECTION('center_axis',(0.,0.,-1.));
#14930=DIRECTION('ref_axis',(0.,-1.,0.));
#14931=DIRECTION('center_axis',(-0.199979743202182,0.676592950304318,-0.708681932821268));
#14932=DIRECTION('ref_axis',(0.952090451893775,0.304986921995709,0.022511082254978));
#14933=DIRECTION('',(0.238764447245934,-0.667686905404276,-0.705113987297802));
#14934=DIRECTION('center_axis',(0.,0.,1.));
#14935=DIRECTION('ref_axis',(1.,0.,0.));
#14936=DIRECTION('',(-0.122120256424646,0.699116237642577,0.704502043457126));
#14937=DIRECTION('center_axis',(0.,0.,1.));
#14938=DIRECTION('ref_axis',(0.,-1.,0.));
#14939=DIRECTION('center_axis',(0.307407432756173,-0.635035895346844,0.708681932821271));
#14940=DIRECTION('ref_axis',(0.885247082849198,0.464031822634076,0.0318130459070229));
#14941=DIRECTION('center_axis',(0.,0.,-1.));
#14942=DIRECTION('ref_axis',(0.,-1.,0.));
#14943=DIRECTION('center_axis',(-0.419327906830114,0.567392302244386,-0.70868193282127));
#14944=DIRECTION('ref_axis',(0.790360701191827,0.612228072851353,0.0225110822547893));
#14945=DIRECTION('',(0.452727560264035,-0.545758207516331,-0.705113987314063));
#14946=DIRECTION('center_axis',(0.,0.,1.));
#14947=DIRECTION('ref_axis',(1.,0.,0.));
#14948=DIRECTION('',(-0.35386733960517,0.615186781972065,0.704502043465889));
#14949=DIRECTION('center_axis',(0.,0.,1.));
#14950=DIRECTION('ref_axis',(0.,-1.,0.));
#14951=DIRECTION('center_axis',(0.5060635640791,-0.49159901058105,0.70868193282127));
#14952=DIRECTION('ref_axis',(0.673151920840624,0.738819613693819,0.0318130459072238));
#14953=DIRECTION('center_axis',(0.,0.,-1.));
#14954=DIRECTION('ref_axis',(0.,-1.,0.));
#14955=DIRECTION('center_axis',(-0.588098936273544,0.389755768714997,-0.708681932821282));
#14956=DIRECTION('ref_axis',(0.533301785444319,0.845625482597132,0.0225110822545249));
#14957=DIRECTION('',(0.612085047945861,-0.358003015318079,-0.705113987312885));
#14958=DIRECTION('center_axis',(0.,0.,1.));
#14959=DIRECTION('ref_axis',(1.,0.,0.));
#14960=DIRECTION('',(-0.542932799114604,0.45705672118749,0.704502043476754));
#14961=DIRECTION('center_axis',(0.,0.,1.));
#14962=DIRECTION('ref_axis',(0.,-1.,0.));
#14963=DIRECTION('center_axis',(0.643680960871656,-0.288868029909898,0.708681932821287));
#14964=DIRECTION('ref_axis',(0.379864702514146,0.924494855525966,0.0318130459067162));
#14965=DIRECTION('center_axis',(0.,0.,-1.));
#14966=DIRECTION('ref_axis',(0.,-1.,0.));
#14967=DIRECTION('center_axis',(-0.685936554586207,0.165108937296249,-0.708681932821281));
#14968=DIRECTION('ref_axis',(0.211918803676205,0.97702797903856,0.0225110822545819));
#14969=DIRECTION('',(0.697616045442606,-0.12706737586408,-0.705113987332571));
#14970=DIRECTION('center_axis',(0.,0.,1.));
#14971=DIRECTION('ref_axis',(1.,0.,0.));
#14972=DIRECTION('',(-0.666512550211308,0.243798874435375,0.70450204345684));
#14973=DIRECTION('center_axis',(0.,0.,1.));
#14974=DIRECTION('ref_axis',(0.,-1.,0.));
#14975=DIRECTION('center_axis',(0.703660934063412,-0.0512953015951689,0.708681932821253));
#14976=DIRECTION('ref_axis',(0.0407601948595917,0.998662373690474,0.031813045907557));
#14977=DIRECTION('center_axis',(0.,0.,-1.));
#14978=DIRECTION('ref_axis',(0.,-1.,0.));
#14979=DIRECTION('center_axis',(-0.701040101070454,-0.0794524687082925,
-0.708681932821266));
#14980=DIRECTION('ref_axis',(-0.135024713403322,0.99058648181068,0.0225110822549792));
#14981=DIRECTION('',(0.699004252188757,0.119194464416953,-0.705113987291694));
#14982=DIRECTION('center_axis',(0.,0.,1.));
#14983=DIRECTION('ref_axis',(1.,0.,0.));
#14984=DIRECTION('',(-0.709701051066567,0.00113528531247919,0.704502043462096));
#14985=DIRECTION('center_axis',(0.,0.,1.));
#14986=DIRECTION('ref_axis',(0.,-1.,0.));
#14987=DIRECTION('center_axis',(0.678769013677966,0.192464397131867,0.708681932821283));
#14988=DIRECTION('ref_axis',(-0.303260593852791,0.952376470901174,0.0318130459069519));
#14989=DIRECTION('center_axis',(0.,0.,-1.));
#14990=DIRECTION('ref_axis',(0.,-1.,0.));
#14991=DIRECTION('center_axis',(-0.631587865115661,-0.314430734393692,-0.708681932821265));
#14992=DIRECTION('ref_axis',(-0.465682257294258,0.884665635377028,0.0225110822548306));
#14993=DIRECTION('',(0.616082229859789,0.351079693163982,-0.705113987309055));
#14994=DIRECTION('center_axis',(0.,0.,1.));
#14995=DIRECTION('ref_axis',(1.,0.,0.));
#14996=DIRECTION('',(-0.667289131086675,-0.241665235966725,0.704502043473784));
#14997=DIRECTION('center_axis',(0.,0.,1.));
#14998=DIRECTION('ref_axis',(0.,-1.,0.));
#14999=DIRECTION('center_axis',(0.572007532679451,0.413010049091652,0.708681932821261));
#15000=DIRECTION('ref_axis',(-0.61070367929613,0.79121991014146,0.0318130459074592));
#15001=DIRECTION('center_axis',(0.,0.,-1.));
#15002=DIRECTION('ref_axis',(0.,-1.,0.));
#15003=DIRECTION('center_axis',(-0.485956811383784,-0.511484013007649,-0.708681932821274));
#15004=DIRECTION('ref_axis',(-0.740171648217328,0.672041057042616,0.0225110822549303));
#15005=DIRECTION('',(0.458851598226975,0.540619529521448,-0.705113987313086));
#15006=DIRECTION('center_axis',(0.,0.,1.));
#15007=DIRECTION('ref_axis',(1.,0.,0.));
#15008=DIRECTION('',(-0.544392293794381,-0.455317363180406,0.704502043463136));
#15009=DIRECTION('center_axis',(0.,0.,1.));
#15010=DIRECTION('ref_axis',(0.,-1.,0.));
#15011=DIRECTION('center_axis',(0.396253501307373,0.583740593752364,0.708681932821266));
#15012=DIRECTION('ref_axis',(-0.844486887990119,0.534630551056402,0.0318130459071614));
#15013=DIRECTION('center_axis',(0.,0.,-1.));
#15014=DIRECTION('ref_axis',(0.,-1.,0.));
#15015=DIRECTION('center_axis',(-0.281712194240633,-0.646844770952699,-0.708681932821261));
#15016=DIRECTION('ref_axis',(-0.925385414595083,0.378358408959537,0.0225110822550412));
#15017=DIRECTION('',(0.246276691905924,0.664952671934695,-0.705113987317501));
#15018=DIRECTION('center_axis',(0.,0.,1.));
#15019=DIRECTION('ref_axis',(1.,0.,0.));
#15020=DIRECTION('',(-0.355833711481152,-0.614051496661014,0.704502043447652));
#15021=DIRECTION('center_axis',(0.,0.,1.));
#15022=DIRECTION('ref_axis',(0.,-1.,0.));
#15023=DIRECTION('center_axis',(0.172705449598441,0.68406340771283,0.708681932821284));
#15024=DIRECTION('ref_axis',(-0.976412514693421,0.21355685720718,0.0318130459067133));
#15025=DIRECTION('center_axis',(0.,0.,-1.));
#15026=DIRECTION('ref_axis',(0.,-1.,0.));
#15027=DIRECTION('center_axis',(-0.0434889288422669,-0.704186503108984,
-0.708681932821272));
#15028=DIRECTION('ref_axis',(-0.998984042738736,0.0390401527801138,0.0225110822546889));
#15029=DIRECTION('',(0.00399718189249243,0.709082708449077,-0.705113987320802));
#15030=DIRECTION('center_axis',(0.,0.,1.));
#15031=DIRECTION('ref_axis',(1.,0.,0.));
#15032=DIRECTION('',(-0.124356331985472,-0.698721957173194,0.704502043474098));
#15033=DIRECTION('center_axis',(0.,0.,1.));
#15034=DIRECTION('ref_axis',(0.,-1.,0.));
#15035=DIRECTION('center_axis',(-0.071673428192519,0.701878079002203,0.708681932821282));
#15036=DIRECTION('ref_axis',(-0.990568381810588,-0.13327494538465,0.0318130459068612));
#15037=DIRECTION('center_axis',(0.,0.,-1.));
#15038=DIRECTION('ref_axis',(0.,-1.,0.));
#15039=DIRECTION('center_axis',(0.199979743201945,-0.676592950304395,-0.708681932821262));
#15040=DIRECTION('ref_axis',(-0.952090451893826,-0.304986921995541,0.0225110822550975));
#15041=DIRECTION('',(-0.23876444723984,0.667686905405306,-0.70511398729889));
#15042=DIRECTION('center_axis',(0.,0.,1.));
#15043=DIRECTION('ref_axis',(1.,0.,0.));
#15044=DIRECTION('',(0.122120256422062,-0.699116237636338,0.704502043463766));
#15045=DIRECTION('center_axis',(0.,0.,1.));
#15046=DIRECTION('ref_axis',(0.,-1.,0.));
#15047=DIRECTION('center_axis',(-0.307407432755953,0.63503589534695,0.708681932821271));
#15048=DIRECTION('ref_axis',(-0.885247082849227,-0.464031822634005,0.0318130459072588));
#15049=DIRECTION('center_axis',(0.,0.,-1.));
#15050=DIRECTION('ref_axis',(0.,-1.,0.));
#15051=DIRECTION('center_axis',(0.419327906830362,-0.567392302244193,-0.708681932821278));
#15052=DIRECTION('ref_axis',(-0.790360701191684,-0.612228072851546,0.0225110822545551));
#15053=DIRECTION('',(-0.452727560269443,0.54575820751465,-0.705113987311891));
#15054=DIRECTION('center_axis',(0.,0.,1.));
#15055=DIRECTION('ref_axis',(1.,0.,0.));
#15056=DIRECTION('',(0.35386733960517,-0.615186781972065,0.704502043465889));
#15057=DIRECTION('center_axis',(0.,0.,1.));
#15058=DIRECTION('ref_axis',(0.,-1.,0.));
#15059=DIRECTION('center_axis',(-0.506063564078916,0.491599010581241,0.708681932821269));
#15060=DIRECTION('ref_axis',(-0.673151920840782,-0.73881961369367,0.0318130459073368));
#15061=DIRECTION('center_axis',(0.,0.,-1.));
#15062=DIRECTION('ref_axis',(0.,-1.,0.));
#15063=DIRECTION('center_axis',(0.588098936273506,-0.389755768715068,-0.708681932821275));
#15064=DIRECTION('ref_axis',(-0.533301785444285,-0.845625482597149,0.022511082254684));
#15065=DIRECTION('',(-0.612085047945861,0.358003015318079,-0.705113987312885));
#15066=DIRECTION('center_axis',(0.,0.,1.));
#15067=DIRECTION('ref_axis',(1.,0.,0.));
#15068=DIRECTION('',(0.542932799116209,-0.457056721221068,0.704502043453732));
#15069=DIRECTION('center_axis',(0.,0.,1.));
#15070=DIRECTION('ref_axis',(0.,-1.,0.));
#15071=DIRECTION('center_axis',(-0.643680960871258,0.288868029910839,0.708681932821265));
#15072=DIRECTION('ref_axis',(-0.379864702514675,-0.92449485552572,0.0318130459075584));
#15073=DIRECTION('center_axis',(0.,0.,-1.));
#15074=DIRECTION('ref_axis',(0.,-1.,0.));
#15075=DIRECTION('center_axis',(0.685936554586071,-0.165108937296882,-0.708681932821266));
#15076=DIRECTION('ref_axis',(-0.21191880367663,-0.977027979038457,0.022511082255061));
#15077=DIRECTION('',(-0.697616045443148,0.127067375858057,-0.705113987333119));
#15078=DIRECTION('center_axis',(0.,0.,1.));
#15079=DIRECTION('ref_axis',(1.,0.,0.));
#15080=DIRECTION('',(0.666512550199835,-0.243798874428091,0.704502043470215));
#15081=DIRECTION('center_axis',(0.,0.,1.));
#15082=DIRECTION('ref_axis',(1.,0.,0.));
#15083=DIRECTION('',(0.897353006349151,0.44131347361727,0.));
#15084=DIRECTION('',(-0.885480349083443,0.464676824671798,0.));
#15085=DIRECTION('center_axis',(0.,0.,1.));
#15086=DIRECTION('ref_axis',(0.999566449009809,0.0294434035722917,0.));
#15087=DIRECTION('center_axis',(0.,0.,1.));
#15088=DIRECTION('ref_axis',(1.,0.,0.));
#15089=DIRECTION('',(0.69228830556049,0.72162102379586,0.));
#15090=DIRECTION('',(-0.991008984713935,0.133795337049747,0.));
#15091=DIRECTION('center_axis',(0.,0.,1.));
#15092=DIRECTION('ref_axis',(0.929214979009912,0.369539609221539,0.));
#15093=DIRECTION('center_axis',(0.,0.,1.));
#15094=DIRECTION('ref_axis',(1.,0.,0.));
#15095=DIRECTION('',(0.403741491998108,0.914873110130111,0.));
#15096=DIRECTION('',(-0.977004529914168,-0.213218546395934,-1.44547855409531E-12));
#15097=DIRECTION('center_axis',(0.,0.,1.));
#15098=DIRECTION('ref_axis',(0.746786468788826,0.665063884174983,0.));
#15099=DIRECTION('center_axis',(0.,0.,1.));
#15100=DIRECTION('ref_axis',(1.,0.,0.));
#15101=DIRECTION('',(0.0664745597242861,0.997788120248714,0.));
#15102=DIRECTION('',(-0.845158910852611,-0.534515121775268,0.));
#15103=DIRECTION('center_axis',(0.,0.,1.));
#15104=DIRECTION('ref_axis',(0.474284489037475,0.880371639399215,0.));
#15105=DIRECTION('center_axis',(0.,0.,1.));
#15106=DIRECTION('ref_axis',(1.,0.,0.));
#15107=DIRECTION('',(-0.278785196504122,0.960353483989181,0.));
#15108=DIRECTION('',(-0.611374661297878,-0.79134128132109,0.));
#15109=DIRECTION('center_axis',(0.,0.,1.));
#15110=DIRECTION('ref_axis',(0.144576800214518,0.989493582010379,0.));
#15111=DIRECTION('center_axis',(0.,0.,1.));
#15112=DIRECTION('ref_axis',(1.,0.,0.));
#15113=DIRECTION('',(-0.590432628680576,0.807086929016537,0.));
#15114=DIRECTION('',(-0.303849593520484,-0.952720013706774,-1.44547855411804E-12));
#15115=DIRECTION('center_axis',(0.,0.,1.));
#15116=DIRECTION('ref_axis',(-0.202568984440614,0.979267995261102,0.));
#15117=DIRECTION('center_axis',(0.,0.,1.));
#15118=DIRECTION('ref_axis',(1.,0.,0.));
#15119=DIRECTION('',(-0.830872579903455,0.556462717497387,0.));
#15120=DIRECTION('',(0.040324221163864,-0.999186647822882,0.));
#15121=DIRECTION('center_axis',(0.,0.,1.));
#15122=DIRECTION('ref_axis',(-0.525281959972336,0.850928235826983,0.));
#15123=DIRECTION('center_axis',(0.,0.,1.));
#15124=DIRECTION('ref_axis',(1.,0.,0.));
#15125=DIRECTION('',(-0.97108310621034,0.238741703170764,0.));
#15126=DIRECTION('',(0.379634333178067,-0.92513662400342,0.));
#15127=DIRECTION('center_axis',(0.,0.,1.));
#15128=DIRECTION('ref_axis',(-0.784638178795358,0.61995397278887,0.));
#15129=DIRECTION('center_axis',(0.,0.,1.));
#15130=DIRECTION('ref_axis',(1.,0.,0.));
#15131=DIRECTION('',(-0.994174099458657,-0.107786177061661,0.));
#15132=DIRECTION('',(0.673154938045335,-0.739501473551731,1.44547855411289E-12));
#15133=DIRECTION('center_axis',(0.,0.,1.));
#15134=DIRECTION('ref_axis',(-0.949355453229469,0.3142041110862,0.));
#15135=DIRECTION('center_axis',(0.,0.,1.));
#15136=DIRECTION('ref_axis',(1.,0.,0.));
#15137=DIRECTION('',(-0.897353006349151,-0.44131347361727,0.));
#15138=DIRECTION('',(0.885483124695737,-0.464671535473257,0.));
#15139=DIRECTION('center_axis',(0.,0.,1.));
#15140=DIRECTION('ref_axis',(-0.999566449009809,-0.0294434035723091,0.));
#15141=DIRECTION('center_axis',(0.,0.,1.));
#15142=DIRECTION('ref_axis',(1.,0.,0.));
#15143=DIRECTION('',(-0.692288305561494,-0.721621023794897,0.));
#15144=DIRECTION('',(0.9910089847142,-0.133795337047783,0.));
#15145=DIRECTION('center_axis',(0.,0.,1.));
#15146=DIRECTION('ref_axis',(-0.929214979009907,-0.369539609221553,0.));
#15147=DIRECTION('center_axis',(0.,0.,1.));
#15148=DIRECTION('ref_axis',(1.,0.,0.));
#15149=DIRECTION('',(-0.403741491998464,-0.914873110129953,0.));
#15150=DIRECTION('',(0.977004530010046,0.213218545956606,0.));
#15151=DIRECTION('center_axis',(0.,0.,1.));
#15152=DIRECTION('ref_axis',(-0.746786468788919,-0.665063884174879,0.));
#15153=DIRECTION('center_axis',(0.,0.,1.));
#15154=DIRECTION('ref_axis',(1.,0.,0.));
#15155=DIRECTION('',(-0.0664745597243501,-0.99778812024871,1.44557389775539E-12));
#15156=DIRECTION('',(0.845158910606238,0.534515122164824,0.));
#15157=DIRECTION('center_axis',(0.,0.,1.));
#15158=DIRECTION('ref_axis',(-0.474284489037501,-0.880371639399201,0.));
#15159=DIRECTION('center_axis',(0.,0.,1.));
#15160=DIRECTION('ref_axis',(1.,0.,0.));
#15161=DIRECTION('',(0.278785196503829,-0.960353483989266,0.));
#15162=DIRECTION('',(0.611374661295944,0.791341281322585,0.));
#15163=DIRECTION('center_axis',(0.,0.,1.));
#15164=DIRECTION('ref_axis',(-0.144576800214509,-0.989493582010381,0.));
#15165=DIRECTION('center_axis',(0.,0.,1.));
#15166=DIRECTION('ref_axis',(1.,0.,0.));
#15167=DIRECTION('',(0.590432628680576,-0.807086929016537,0.));
#15168=DIRECTION('',(0.303849593506657,0.952720013711184,0.));
#15169=DIRECTION('center_axis',(0.,0.,1.));
#15170=DIRECTION('ref_axis',(0.202568984440597,-0.979267995261106,0.));
#15171=DIRECTION('center_axis',(0.,0.,1.));
#15172=DIRECTION('ref_axis',(1.,0.,0.));
#15173=DIRECTION('',(0.830872579905544,-0.556462717494268,1.44557389777932E-12));
#15174=DIRECTION('',(-0.0403242211638251,0.999186647822883,0.));
#15175=DIRECTION('center_axis',(0.,0.,1.));
#15176=DIRECTION('ref_axis',(0.525281959972335,-0.850928235826983,0.));
#15177=DIRECTION('center_axis',(0.,0.,1.));
#15178=DIRECTION('ref_axis',(1.,0.,0.));
#15179=DIRECTION('',(0.971083106210285,-0.238741703170988,0.));
#15180=DIRECTION('',(-0.37962882645773,0.925138883693863,0.));
#15181=DIRECTION('center_axis',(0.,0.,1.));
#15182=DIRECTION('ref_axis',(0.784638178795358,-0.61995397278887,0.));
#15183=DIRECTION('center_axis',(0.,0.,1.));
#15184=DIRECTION('ref_axis',(1.,0.,0.));
#15185=DIRECTION('',(0.994172662512016,0.107799430025248,0.));
#15186=DIRECTION('',(-0.673150528894382,0.739505487098786,1.44548415247993E-12));
#15187=DIRECTION('center_axis',(0.,0.,1.));
#15188=DIRECTION('ref_axis',(0.949355453229467,-0.314204111086206,0.));
#15189=DIRECTION('center_axis',(0.,0.,-1.));
#15190=DIRECTION('ref_axis',(-1.,0.,0.));
#15191=DIRECTION('center_axis',(0.,0.,-1.));
#15192=DIRECTION('ref_axis',(0.850763965251217,0.525547976335203,0.));
#15193=DIRECTION('center_axis',(0.,0.,-1.));
#15194=DIRECTION('ref_axis',(0.999566449009811,-0.0294434035722236,0.));
#15195=DIRECTION('center_axis',(0.,0.,1.));
#15196=DIRECTION('ref_axis',(1.,0.,0.));
#15197=DIRECTION('center_axis',(0.,0.,-1.));
#15198=DIRECTION('ref_axis',(-1.,0.,0.));
#15199=DIRECTION('center_axis',(0.,0.,-1.));
#15200=DIRECTION('ref_axis',(0.599889878870626,0.800082579005808,0.));
#15201=DIRECTION('center_axis',(0.,0.,-1.));
#15202=DIRECTION('ref_axis',(0.949355453229486,0.314204111086149,0.));
#15203=DIRECTION('center_axis',(0.,0.,-1.));
#15204=DIRECTION('ref_axis',(0.979411716378758,-0.201872954652214,0.));
#15205=DIRECTION('center_axis',(0.,0.,1.));
#15206=DIRECTION('ref_axis',(1.,0.,0.));
#15207=DIRECTION('center_axis',(0.,0.,-1.));
#15208=DIRECTION('ref_axis',(-1.,0.,0.));
#15209=DIRECTION('center_axis',(0.,0.,-1.));
#15210=DIRECTION('ref_axis',(0.314028052635586,0.949413704429161,0.));
#15211=DIRECTION('center_axis',(0.,0.,-1.));
#15212=DIRECTION('ref_axis',(0.784638178795399,0.619953972788819,0.));
#15213=DIRECTION('center_axis',(0.,0.,-1.));
#15214=DIRECTION('ref_axis',(0.989389291469206,0.145288781143156,0.));
#15215=DIRECTION('center_axis',(0.,0.,1.));
#15216=DIRECTION('ref_axis',(1.,0.,0.));
#15217=DIRECTION('center_axis',(0.,0.,-1.));
#15218=DIRECTION('ref_axis',(-1.,0.,0.));
#15219=DIRECTION('center_axis',(-1.32132775915598E-13,-9.56797466456895E-14,
-1.));
#15220=DIRECTION('ref_axis',(-0.0547306874098733,0.998501152656141,-8.8304619656333E-14));
#15221=DIRECTION('center_axis',(0.,0.,-1.));
#15222=DIRECTION('ref_axis',(0.525281959972367,0.850928235826964,0.));
#15223=DIRECTION('center_axis',(0.,0.,1.));
#15224=DIRECTION('ref_axis',(1.,0.,0.));
#15225=DIRECTION('center_axis',(0.,0.,-1.));
#15226=DIRECTION('ref_axis',(-1.,0.,0.));
#15227=DIRECTION('center_axis',(0.,0.,-1.));
#15228=DIRECTION('ref_axis',(-0.36977560838049,0.929121089765397,0.));
#15229=DIRECTION('center_axis',(0.,0.,-1.));
#15230=DIRECTION('ref_axis',(0.20256898444057,0.979267995261112,0.));
#15231=DIRECTION('center_axis',(-5.28974998245161E-12,3.849896247492E-12,
-1.));
#15232=DIRECTION('ref_axis',(0.664558246712093,0.747236466406016,-6.38564105877661E-13));
#15233=DIRECTION('center_axis',(0.,0.,1.));
#15234=DIRECTION('ref_axis',(1.,0.,0.));
#15235=DIRECTION('center_axis',(0.,0.,-1.));
#15236=DIRECTION('ref_axis',(-1.,0.,0.));
#15237=DIRECTION('center_axis',(0.,0.,-1.));
#15238=DIRECTION('ref_axis',(-0.665255506900887,0.746615771691199,0.));
#15239=DIRECTION('center_axis',(0.,0.,-1.));
#15240=DIRECTION('ref_axis',(-0.144576800214448,0.98949358201039,0.));
#15241=DIRECTION('center_axis',(0.,0.,-1.));
#15242=DIRECTION('ref_axis',(0.368892007453974,0.929472262542878,0.));
#15243=DIRECTION('center_axis',(0.,0.,1.));
#15244=DIRECTION('ref_axis',(1.,0.,0.));
#15245=DIRECTION('center_axis',(0.,0.,-1.));
#15246=DIRECTION('ref_axis',(-1.,0.,0.));
#15247=DIRECTION('center_axis',(0.,0.,-1.));
#15248=DIRECTION('ref_axis',(0.892093090490583,-0.451851654748504,0.));
#15249=DIRECTION('center_axis',(0.,0.,-1.));
#15250=DIRECTION('ref_axis',(-0.474284489037421,0.880371639399244,0.));
#15251=DIRECTION('center_axis',(0.,0.,-1.));
#15252=DIRECTION('ref_axis',(0.0287254060179531,0.999587340380571,0.));
#15253=DIRECTION('center_axis',(0.,0.,1.));
#15254=DIRECTION('ref_axis',(1.,0.,0.));
#15255=DIRECTION('center_axis',(0.,0.,-1.));
#15256=DIRECTION('ref_axis',(-1.,0.,0.));
#15257=DIRECTION('center_axis',(0.,0.,-1.));
#15258=DIRECTION('ref_axis',(0.989520239095182,-0.144394239570053,0.));
#15259=DIRECTION('center_axis',(0.,0.,-1.));
#15260=DIRECTION('ref_axis',(-0.746786468788856,0.66506388417495,0.));
#15261=DIRECTION('center_axis',(0.,0.,1.));
#15262=DIRECTION('ref_axis',(1.,0.,0.));
#15263=DIRECTION('center_axis',(0.,0.,-1.));
#15264=DIRECTION('ref_axis',(-1.,0.,0.));
#15265=DIRECTION('center_axis',(-8.27850864256961E-13,6.25380161775213E-12,
-1.));
#15266=DIRECTION('ref_axis',(0.97922431753446,0.202780018614189,4.57494310884885E-13));
#15267=DIRECTION('center_axis',(0.,0.,-1.));
#15268=DIRECTION('ref_axis',(-0.92921497900993,0.369539609221494,0.));
#15269=DIRECTION('center_axis',(-4.70972287661959E-12,-4.54062894276413E-12,
-1.));
#15270=DIRECTION('ref_axis',(-0.620501753965407,0.784205058212362,-6.38392878747627E-13));
#15271=DIRECTION('center_axis',(0.,0.,1.));
#15272=DIRECTION('ref_axis',(1.,0.,0.));
#15273=DIRECTION('center_axis',(0.,0.,-1.));
#15274=DIRECTION('ref_axis',(-1.,0.,0.));
#15275=DIRECTION('center_axis',(0.,0.,-1.));
#15276=DIRECTION('ref_axis',(0.85076379978476,0.52554824419438,0.));
#15277=DIRECTION('center_axis',(0.,0.,-1.));
#15278=DIRECTION('ref_axis',(-0.99956644900981,0.0294434035722665,0.));
#15279=DIRECTION('center_axis',(0.,0.,-1.));
#15280=DIRECTION('ref_axis',(0.851282603118517,-0.524707470527876,0.));
#15281=DIRECTION('center_axis',(0.,0.,1.));
#15282=DIRECTION('ref_axis',(1.,0.,0.));
#15283=DIRECTION('center_axis',(0.,0.,-1.));
#15284=DIRECTION('ref_axis',(-1.,0.,0.));
#15285=DIRECTION('center_axis',(4.82728718843136E-12,-4.41615259808489E-12,
-1.));
#15286=DIRECTION('ref_axis',(0.59988968881684,0.800082721505242,-6.37447579960598E-13));
#15287=DIRECTION('center_axis',(1.42286553678981E-14,5.73968510871457E-15,
-1.));
#15288=DIRECTION('ref_axis',(-0.949355453229486,-0.314204111086149,-1.53187688370636E-14));
#15289=DIRECTION('center_axis',(0.,0.,-1.));
#15290=DIRECTION('ref_axis',(0.979411667303631,-0.201873192746145,0.));
#15291=DIRECTION('center_axis',(0.,0.,1.));
#15292=DIRECTION('ref_axis',(1.,0.,0.));
#15293=DIRECTION('center_axis',(0.,0.,-1.));
#15294=DIRECTION('ref_axis',(-1.,0.,0.));
#15295=DIRECTION('center_axis',(0.,0.,-1.));
#15296=DIRECTION('ref_axis',(0.314028299832077,0.94941362266642,0.));
#15297=DIRECTION('center_axis',(0.,0.,-1.));
#15298=DIRECTION('ref_axis',(-0.784638178795399,-0.619953972788819,0.));
#15299=DIRECTION('center_axis',(0.,0.,1.));
#15300=DIRECTION('ref_axis',(1.,0.,0.));
#15301=DIRECTION('center_axis',(0.,0.,-1.));
#15302=DIRECTION('ref_axis',(-1.,0.,0.));
#15303=DIRECTION('center_axis',(0.,0.,-1.));
#15304=DIRECTION('ref_axis',(-0.0547311918692556,0.99850112500516,0.));
#15305=DIRECTION('center_axis',(0.,0.,-1.));
#15306=DIRECTION('ref_axis',(-0.525281959972365,-0.850928235826965,0.));
#15307=DIRECTION('center_axis',(0.,0.,-1.));
#15308=DIRECTION('ref_axis',(0.88003414096249,0.474910423912145,0.));
#15309=DIRECTION('center_axis',(0.,0.,1.));
#15310=DIRECTION('ref_axis',(1.,0.,0.));
#15311=DIRECTION('center_axis',(0.,0.,-1.));
#15312=DIRECTION('ref_axis',(-1.,0.,0.));
#15313=DIRECTION('center_axis',(-6.01566800664695E-12,-1.90143638812626E-12,
-1.));
#15314=DIRECTION('ref_axis',(-0.369775977307563,0.929120942938128,4.57785146442974E-13));
#15315=DIRECTION('center_axis',(0.,0.,-1.));
#15316=DIRECTION('ref_axis',(-0.202568984440568,-0.979267995261112,0.));
#15317=DIRECTION('center_axis',(-3.47775045046998E-12,2.39197982760852E-12,
-1.));
#15318=DIRECTION('ref_axis',(0.664558447941313,0.747236287441819,-5.23794315673617E-13));
#15319=DIRECTION('center_axis',(0.,0.,1.));
#15320=DIRECTION('ref_axis',(1.,0.,0.));
#15321=DIRECTION('center_axis',(0.,0.,-1.));
#15322=DIRECTION('ref_axis',(-1.,0.,0.));
#15323=DIRECTION('center_axis',(0.,0.,-1.));
#15324=DIRECTION('ref_axis',(-0.665255256778492,0.746615994557164,0.));
#15325=DIRECTION('center_axis',(0.,0.,-1.));
#15326=DIRECTION('ref_axis',(0.144576800214612,-0.989493582010366,0.));
#15327=DIRECTION('center_axis',(0.,0.,-1.));
#15328=DIRECTION('ref_axis',(0.368891975145543,0.929472275365554,0.));
#15329=DIRECTION('center_axis',(0.,0.,1.));
#15330=DIRECTION('ref_axis',(1.,0.,0.));
#15331=DIRECTION('center_axis',(0.,0.,-1.));
#15332=DIRECTION('ref_axis',(-1.,0.,0.));
#15333=DIRECTION('center_axis',(0.,0.,-1.));
#15334=DIRECTION('ref_axis',(0.892092990260699,-0.451851852632834,0.));
#15335=DIRECTION('center_axis',(0.,0.,-1.));
#15336=DIRECTION('ref_axis',(0.47428448903741,-0.88037163939925,0.));
#15337=DIRECTION('center_axis',(-6.52620372287673E-12,-4.50951246938111E-13,
-1.));
#15338=DIRECTION('ref_axis',(0.0287256757183184,0.999587332630084,-6.38234765888116E-13));
#15339=DIRECTION('center_axis',(0.,0.,1.));
#15340=DIRECTION('ref_axis',(1.,0.,0.));
#15341=DIRECTION('center_axis',(0.,0.,-1.));
#15342=DIRECTION('ref_axis',(-1.,0.,0.));
#15343=DIRECTION('center_axis',(0.,0.,-1.));
#15344=DIRECTION('ref_axis',(0.989520246610118,-0.144394188070888,0.));
#15345=DIRECTION('center_axis',(0.,0.,-1.));
#15346=DIRECTION('ref_axis',(0.746786468788917,-0.665063884174881,0.));
#15347=DIRECTION('center_axis',(0.,0.,1.));
#15348=DIRECTION('ref_axis',(1.,0.,0.));
#15349=DIRECTION('center_axis',(0.,0.,-1.));
#15350=DIRECTION('ref_axis',(-1.,0.,0.));
#15351=DIRECTION('center_axis',(0.,0.,-1.));
#15352=DIRECTION('ref_axis',(0.973825526449741,0.22729681923618,0.));
#15353=DIRECTION('center_axis',(0.,0.,-1.));
#15354=DIRECTION('ref_axis',(0.92921497900996,-0.369539609221419,0.));
#15355=DIRECTION('center_axis',(0.,0.,1.));
#15356=DIRECTION('ref_axis',(1.,0.,0.));
#15357=DIRECTION('center_axis',(0.,0.,1.));
#15358=DIRECTION('ref_axis',(1.,0.,0.));
#15359=DIRECTION('center_axis',(0.,0.,1.));
#15360=DIRECTION('ref_axis',(1.,0.,0.));
#15361=DIRECTION('center_axis',(0.,0.,1.));
#15362=DIRECTION('ref_axis',(0.889388506695126,-0.457152145525549,0.));
#15363=DIRECTION('center_axis',(0.,0.,1.));
#15364=DIRECTION('ref_axis',(0.99417501641652,0.107777719094496,0.));
#15365=DIRECTION('center_axis',(0.,0.,1.));
#15366=DIRECTION('ref_axis',(1.,0.,0.));
#15367=DIRECTION('center_axis',(0.,0.,1.));
#15368=DIRECTION('ref_axis',(1.,0.,0.));
#15369=DIRECTION('center_axis',(0.,0.,1.));
#15370=DIRECTION('ref_axis',(0.988657810802218,-0.150185662231007,0.));
#15371=DIRECTION('center_axis',(0.,0.,1.));
#15372=DIRECTION('ref_axis',(0.897356775764319,0.441305808923773,0.));
#15373=DIRECTION('center_axis',(0.,0.,1.));
#15374=DIRECTION('ref_axis',(1.,0.,0.));
#15375=DIRECTION('center_axis',(0.,0.,1.));
#15376=DIRECTION('ref_axis',(1.,0.,0.));
#15377=DIRECTION('center_axis',(0.,0.,1.));
#15378=DIRECTION('ref_axis',(0.98039945695656,0.197020061920814,0.));
#15379=DIRECTION('center_axis',(0.,0.,1.));
#15380=DIRECTION('ref_axis',(0.692304064379401,0.721605905216803,0.));
#15381=DIRECTION('center_axis',(0.,0.,1.));
#15382=DIRECTION('ref_axis',(1.,0.,0.));
#15383=DIRECTION('center_axis',(0.,0.,1.));
#15384=DIRECTION('ref_axis',(1.,0.,0.));
#15385=DIRECTION('center_axis',(0.,0.,1.));
#15386=DIRECTION('ref_axis',(0.853892973276138,0.520448643181666,0.));
#15387=DIRECTION('center_axis',(0.,0.,1.));
#15388=DIRECTION('ref_axis',(0.403749265510609,0.91486967957171,0.));
#15389=DIRECTION('center_axis',(0.,0.,1.));
#15390=DIRECTION('ref_axis',(1.,0.,0.));
#15391=DIRECTION('center_axis',(0.,0.,1.));
#15392=DIRECTION('ref_axis',(1.,0.,0.));
#15393=DIRECTION('center_axis',(0.,0.,1.));
#15394=DIRECTION('ref_axis',(-0.624419851739997,-0.7810888865891,0.));
#15395=DIRECTION('center_axis',(0.,0.,1.));
#15396=DIRECTION('ref_axis',(0.0664963465165425,0.997786668531882,0.));
#15397=DIRECTION('center_axis',(0.,0.,1.));
#15398=DIRECTION('ref_axis',(1.,0.,0.));
#15399=DIRECTION('center_axis',(0.,0.,1.));
#15400=DIRECTION('ref_axis',(1.,0.,0.));
#15401=DIRECTION('center_axis',(0.,0.,1.));
#15402=DIRECTION('ref_axis',(-0.319595441725534,-0.947554090080488,0.));
#15403=DIRECTION('center_axis',(0.,0.,1.));
#15404=DIRECTION('ref_axis',(-0.278777013248851,0.9603558595042,0.));
#15405=DIRECTION('center_axis',(0.,0.,1.));
#15406=DIRECTION('ref_axis',(1.,0.,0.));
#15407=DIRECTION('center_axis',(0.,0.,1.));
#15408=DIRECTION('ref_axis',(1.,0.,0.));
#15409=DIRECTION('center_axis',(0.,0.,1.));
#15410=DIRECTION('ref_axis',(0.0237812816597838,-0.99971718532924,0.));
#15411=DIRECTION('center_axis',(0.,0.,1.));
#15412=DIRECTION('ref_axis',(-0.590425750906046,0.807091960477263,0.));
#15413=DIRECTION('center_axis',(0.,0.,1.));
#15414=DIRECTION('ref_axis',(1.,0.,0.));
#15415=DIRECTION('center_axis',(0.,0.,1.));
#15416=DIRECTION('ref_axis',(1.,0.,0.));
#15417=DIRECTION('center_axis',(0.,0.,1.));
#15418=DIRECTION('ref_axis',(0.364271227124465,-0.93129290402603,0.));
#15419=DIRECTION('center_axis',(0.,0.,1.));
#15420=DIRECTION('ref_axis',(-0.830860429247751,0.556480859608165,0.));
#15421=DIRECTION('center_axis',(0.,0.,1.));
#15422=DIRECTION('ref_axis',(1.,0.,0.));
#15423=DIRECTION('center_axis',(0.,0.,1.));
#15424=DIRECTION('ref_axis',(1.,0.,0.));
#15425=DIRECTION('center_axis',(0.,0.,1.));
#15426=DIRECTION('ref_axis',(0.66080906094452,-0.750554052000002,0.));
#15427=DIRECTION('center_axis',(0.,0.,1.));
#15428=DIRECTION('ref_axis',(-0.971081077628326,0.238749954287344,0.));
#15429=DIRECTION('center_axis',(0.,0.,1.));
#15430=DIRECTION('ref_axis',(1.,0.,0.));
#15431=DIRECTION('center_axis',(0.,0.,1.));
#15432=DIRECTION('ref_axis',(1.,0.,0.));
#15433=DIRECTION('center_axis',(0.,0.,1.));
#15434=DIRECTION('ref_axis',(0.877651349637868,-0.479299602001534,0.));
#15435=DIRECTION('center_axis',(0.,0.,1.));
#15436=DIRECTION('ref_axis',(-0.99417501641652,-0.107777719094496,0.));
#15437=DIRECTION('center_axis',(0.,0.,1.));
#15438=DIRECTION('ref_axis',(1.,0.,0.));
#15439=DIRECTION('center_axis',(0.,0.,1.));
#15440=DIRECTION('ref_axis',(1.,0.,0.));
#15441=DIRECTION('center_axis',(-3.47737300407025E-13,-6.53322053534217E-12,
1.));
#15442=DIRECTION('ref_axis',(0.988657789032747,-0.150185805537277,-6.37403798268417E-13));
#15443=DIRECTION('center_axis',(0.,0.,1.));
#15444=DIRECTION('ref_axis',(-0.897356775764326,-0.441305808923759,0.));
#15445=DIRECTION('center_axis',(0.,0.,1.));
#15446=DIRECTION('ref_axis',(1.,0.,0.));
#15447=DIRECTION('center_axis',(0.,0.,1.));
#15448=DIRECTION('ref_axis',(1.,0.,0.));
#15449=DIRECTION('center_axis',(0.,0.,1.));
#15450=DIRECTION('ref_axis',(0.980399405327247,0.197020318835346,0.));
#15451=DIRECTION('center_axis',(0.,0.,1.));
#15452=DIRECTION('ref_axis',(-0.692304064379401,-0.721605905216803,0.));
#15453=DIRECTION('center_axis',(0.,0.,1.));
#15454=DIRECTION('ref_axis',(1.,0.,0.));
#15455=DIRECTION('center_axis',(0.,0.,1.));
#15456=DIRECTION('ref_axis',(1.,0.,0.));
#15457=DIRECTION('center_axis',(3.9330849286785E-12,-5.22825041966026E-12,
1.));
#15458=DIRECTION('ref_axis',(0.853893037802406,0.520448537314285,-6.37398554059169E-13));
#15459=DIRECTION('center_axis',(0.,0.,1.));
#15460=DIRECTION('ref_axis',(-0.403749265510619,-0.914869679571706,0.));
#15461=DIRECTION('center_axis',(0.,0.,1.));
#15462=DIRECTION('ref_axis',(1.,0.,0.));
#15463=DIRECTION('center_axis',(0.,0.,1.));
#15464=DIRECTION('ref_axis',(1.,0.,0.));
#15465=DIRECTION('center_axis',(-5.48451776394876E-12,3.56805502485972E-12,
1.));
#15466=DIRECTION('ref_axis',(-0.624419281297108,-0.781089342613509,-6.37668886649601E-13));
#15467=DIRECTION('center_axis',(0.,0.,1.));
#15468=DIRECTION('ref_axis',(-0.0664963465165425,-0.997786668531882,0.));
#15469=DIRECTION('center_axis',(0.,0.,1.));
#15470=DIRECTION('ref_axis',(1.,0.,0.));
#15471=DIRECTION('center_axis',(0.,0.,1.));
#15472=DIRECTION('ref_axis',(1.,0.,0.));
#15473=DIRECTION('center_axis',(0.,0.,1.));
#15474=DIRECTION('ref_axis',(-0.319595564366664,-0.947554048715509,0.));
#15475=DIRECTION('center_axis',(0.,0.,1.));
#15476=DIRECTION('ref_axis',(0.278777013248859,-0.960355859504197,0.));
#15477=DIRECTION('center_axis',(0.,0.,1.));
#15478=DIRECTION('ref_axis',(1.,0.,0.));
#15479=DIRECTION('center_axis',(0.,0.,1.));
#15480=DIRECTION('ref_axis',(1.,0.,0.));
#15481=DIRECTION('center_axis',(-6.49423776379365E-12,-7.9201404422884E-13,
1.));
#15482=DIRECTION('ref_axis',(0.0237818414100777,-0.999717172013738,-6.37345107913742E-13));
#15483=DIRECTION('center_axis',(0.,0.,1.));
#15484=DIRECTION('ref_axis',(0.590425750905992,-0.807091960477302,0.));
#15485=DIRECTION('center_axis',(0.,0.,1.));
#15486=DIRECTION('ref_axis',(1.,0.,0.));
#15487=DIRECTION('center_axis',(0.,0.,1.));
#15488=DIRECTION('ref_axis',(1.,0.,0.));
#15489=DIRECTION('center_axis',(0.,0.,1.));
#15490=DIRECTION('ref_axis',(0.387549166087966,-0.921849035289685,0.));
#15491=DIRECTION('center_axis',(0.,0.,1.));
#15492=DIRECTION('ref_axis',(0.830860429247751,-0.556480859608165,0.));
#15493=DIRECTION('center_axis',(0.,0.,1.));
#15494=DIRECTION('ref_axis',(1.,0.,0.));
#15495=DIRECTION('center_axis',(0.,0.,1.));
#15496=DIRECTION('ref_axis',(1.,0.,0.));
#15497=DIRECTION('center_axis',(-4.30576259291751E-12,-4.61078946408106E-12,
1.));
#15498=DIRECTION('ref_axis',(0.679434606802726,-0.733736066360939,-4.57618409888508E-13));
#15499=DIRECTION('center_axis',(0.,0.,1.));
#15500=DIRECTION('ref_axis',(0.971081077628323,-0.238749954287355,0.));
#15501=DIRECTION('center_axis',(0.,0.,1.));
#15502=DIRECTION('ref_axis',(1.,0.,0.));
#15503=DIRECTION('center_axis',(0.,0.,1.));
#15504=DIRECTION('ref_axis',(1.,0.,0.));
#15505=DIRECTION('center_axis',(0.,0.,1.));
#15506=DIRECTION('ref_axis',(1.,0.,0.));
#15507=DIRECTION('center_axis',(0.,0.,1.));
#15508=DIRECTION('ref_axis',(1.,0.,0.));
#15509=DIRECTION('center_axis',(0.,0.,1.));
#15510=DIRECTION('ref_axis',(1.,0.,0.));
#15511=DIRECTION('center_axis',(0.,0.,1.));
#15512=DIRECTION('ref_axis',(1.,0.,0.));
#15513=DIRECTION('center_axis',(0.,0.,1.));
#15514=DIRECTION('ref_axis',(1.,0.,0.));
#15515=DIRECTION('center_axis',(0.,0.,1.));
#15516=DIRECTION('ref_axis',(1.,0.,0.));
#15517=DIRECTION('center_axis',(0.,0.,1.));
#15518=DIRECTION('ref_axis',(1.,0.,0.));
#15519=DIRECTION('center_axis',(0.,0.,1.));
#15520=DIRECTION('ref_axis',(-0.999229036240747,-0.0392598157584637,0.));
#15521=DIRECTION('center_axis',(0.,0.,1.));
#15522=DIRECTION('ref_axis',(1.,0.,0.));
#15523=DIRECTION('center_axis',(0.,0.,1.));
#15524=DIRECTION('ref_axis',(1.,0.,0.));
#15525=DIRECTION('center_axis',(0.,0.,1.));
#15526=DIRECTION('ref_axis',(1.,0.,0.));
#15527=DIRECTION('center_axis',(0.,0.,1.));
#15528=DIRECTION('ref_axis',(1.,0.,0.));
#15529=DIRECTION('center_axis',(0.,0.,1.));
#15530=DIRECTION('ref_axis',(1.,0.,0.));
#15531=DIRECTION('center_axis',(0.,0.,1.));
#15532=DIRECTION('ref_axis',(1.,0.,0.));
#15533=DIRECTION('center_axis',(0.,0.,1.));
#15534=DIRECTION('ref_axis',(1.,0.,0.));
#15535=DIRECTION('center_axis',(0.,0.,1.));
#15536=DIRECTION('ref_axis',(1.,0.,0.));
#15537=DIRECTION('center_axis',(-0.378441568052335,-0.916480699435958,0.129788701863713));
#15538=DIRECTION('ref_axis',(0.924381621172865,-0.381465300242715,0.00168616385949415));
#15539=DIRECTION('center_axis',(-0.305383147490373,-0.943343005537968,0.129788701863709));
#15540=DIRECTION('ref_axis',(0.951456650156171,-0.307778183945461,0.00168296192234297));
#15541=DIRECTION('center_axis',(-0.224107897665031,-0.965883296818355,0.129788701863708));
#15542=DIRECTION('ref_axis',(0.974171131086531,-0.225804727578402,0.00168296192248745));
#15543=DIRECTION('center_axis',(-0.299184912142572,-0.945327076315269,0.129788701863708));
#15544=DIRECTION('ref_axis',(0.953456387284282,-0.30152624164116,0.00168616385952863));
#15545=DIRECTION('center_axis',(-0.66907360907623,-0.731775511004736,0.129788701863704));
#15546=DIRECTION('ref_axis',(0.738165771541167,-0.674617262287642,0.00168616385934017));
#15547=DIRECTION('center_axis',(-0.609608600176635,-0.782005273293741,0.129788701863704));
#15548=DIRECTION('ref_axis',(0.788810454557559,-0.614634228155136,0.00168296192406015));
#15549=DIRECTION('center_axis',(-0.540944081297966,-0.830983991288178,0.129788701863717));
#15550=DIRECTION('ref_axis',(0.838191657982016,-0.545373186110699,0.00168296192002916));
#15551=DIRECTION('center_axis',(-0.604462756307606,-0.785989611321642,0.129788701863707));
#15552=DIRECTION('ref_axis',(0.792827883000484,-0.609443274463194,0.00168616385667629));
#15553=DIRECTION('center_axis',(-0.879005498371115,-0.458807396084543,0.129788701863717));
#15554=DIRECTION('ref_axis',(0.462916235689704,-0.886400426210586,0.0016861638606374));
#15555=DIRECTION('center_axis',(-0.840306258803425,-0.526346163930475,0.129788701863704));
#15556=DIRECTION('ref_axis',(0.531022076545678,-0.847356313400851,0.00168296192311816));
#15557=DIRECTION('center_axis',(-0.792529856525827,-0.595861809126773,0.129788793581421));
#15558=DIRECTION('ref_axis',(0.601120180867897,-0.799156862206045,0.00168455998250973));
#15559=DIRECTION('center_axis',(-0.83683754017856,-0.531843783212709,0.129788757625188));
#15560=DIRECTION('ref_axis',(0.536565993516091,-0.843856680285777,0.00168455904000648));
#15561=DIRECTION('center_axis',(-0.98291635181688,-0.130500337928791,0.129788701863707));
#15562=DIRECTION('ref_axis',(0.131832169906145,-0.991270616849543,0.00168616386006647));
#15563=DIRECTION('center_axis',(-0.969650581024334,-0.207201939150445,0.129788701863711));
#15564=DIRECTION('ref_axis',(0.209184599046497,-0.97787472160851,0.001682961923121));
#15565=DIRECTION('center_axis',(-0.948531199288248,-0.288865769930391,0.129788793581421));
#15566=DIRECTION('ref_axis',(0.291540453620295,-0.956557016680417,0.00168455998226241));
#15567=DIRECTION('center_axis',(-0.968271348267041,-0.213554383048539,0.129788757625165));
#15568=DIRECTION('ref_axis',(0.215591121919023,-0.976482273474809,0.00168455904166718));
#15569=DIRECTION('center_axis',(-0.968272986935159,0.213546986961178,0.129788701863713));
#15570=DIRECTION('ref_axis',(-0.215152801203895,-0.9765789415022,0.00168616385887264));
#15571=DIRECTION('center_axis',(-0.982040732655837,0.136933897459027,0.129788701863709));
#15572=DIRECTION('ref_axis',(-0.137883628326555,-0.990447006496901,0.00168296192237585));
#15573=DIRECTION('center_axis',(-0.990125680589725,0.052971744330466,0.129788793581421));
#15574=DIRECTION('ref_axis',(-0.0532033550188353,-0.998582277667897,0.00168455998277433));
#15575=DIRECTION('center_axis',(-0.982917341583731,0.130492827420077,0.129788757625168));
#15576=DIRECTION('ref_axis',(-0.131387220749492,-0.991329693131685,0.00168455904115533));
#15577=DIRECTION('center_axis',(-0.836841609645931,0.531837393602351,0.129788701863704));
#15578=DIRECTION('ref_axis',(-0.53618716916805,-0.844097433043719,0.00168616385845728));
#15579=DIRECTION('center_axis',(-0.875982278548042,0.464553485121265,0.129788701863712));
#15580=DIRECTION('ref_axis',(-0.468321055193095,-0.883556764957403,0.00168296192337288));
#15581=DIRECTION('center_axis',(-0.912296392111608,0.388420084445723,0.129788793581425));
#15582=DIRECTION('ref_axis',(-0.391530053845128,-0.920163778462124,0.00168455998354657));
#15583=DIRECTION('center_axis',(-0.879008997189149,0.458800677042487,0.129788757625161));
#15584=DIRECTION('ref_axis',(-0.462518325536303,-0.886608121327528,0.00168455904187875));
#15585=DIRECTION('center_axis',(-0.60447478375946,0.785980361502429,0.129788701863699));
#15586=DIRECTION('ref_axis',(-0.792549451262032,-0.609805316601694,0.00168616385909342));
#15587=DIRECTION('center_axis',(-0.664267433537108,0.736141066379643,0.129788701863703));
#15588=DIRECTION('ref_axis',(-0.742272051101889,-0.670096537666153,0.00168296192149378));
#15589=DIRECTION('center_axis',(-0.724425523284778,0.677024780995576,0.129788701863712));
#15590=DIRECTION('ref_axis',(-0.682638195940333,-0.730754583346887,0.0016829619261111));
#15591=DIRECTION('center_axis',(-0.669084806894506,0.731765272509891,0.129788701863711));
#15592=DIRECTION('ref_axis',(-0.737857578818759,-0.674954331959692,0.00168616386059911));
#15593=DIRECTION('center_axis',(-0.299199377858597,0.945322497964352,0.12978870186371));
#15594=DIRECTION('ref_axis',(-0.953318572743403,-0.301961679214298,0.00168616385977842));
#15595=DIRECTION('center_axis',(-0.372432132484037,0.918939170762639,0.129788701863704));
#15596=DIRECTION('ref_axis',(-0.926694082893931,-0.375812778346535,0.00168296192305547));
#15597=DIRECTION('center_axis',(-0.449187964027621,0.883959864492387,0.129788793581425));
#15598=DIRECTION('ref_axis',(-0.891399297735882,-0.453215681826704,0.00168455998165862));
#15599=DIRECTION('center_axis',(-0.37844856723093,0.916477801343259,0.129788757625163));
#15600=DIRECTION('ref_axis',(-0.924210308154052,-0.381880175660676,0.00168455904140337));
#15601=DIRECTION('center_axis',(0.0421638887274789,0.990644789698058,0.12978870186371));
#15602=DIRECTION('ref_axis',(-0.999103404868771,0.0423029931691144,0.00168616385986293));
#15603=DIRECTION('center_axis',(-0.035676019747098,0.990899649048045,0.12978870186371));
#15604=DIRECTION('ref_axis',(-0.99934313173509,-0.0362004515589168,0.0016829619223935));
#15605=DIRECTION('center_axis',(-0.119766535590606,0.984281893571808,0.129788793581421));
#15606=DIRECTION('ref_axis',(-0.992650234712453,-0.121006916260922,0.00168455998244488));
#15607=DIRECTION('center_axis',(-0.0421714570058776,0.990644460241976,0.129788757625168));
#15608=DIRECTION('ref_axis',(-0.999084319039234,-0.0427514410370733,0.00168455904153955));
#15609=DIRECTION('center_axis',(0.378441568051778,0.916480699436188,0.129788701863713));
#15610=DIRECTION('ref_axis',(-0.924381621173083,0.381465300242189,0.00168616385911061));
#15611=DIRECTION('center_axis',(0.305383147489853,0.943343005538136,0.129788701863713));
#15612=DIRECTION('ref_axis',(-0.951456650156345,0.307778183944919,0.00168296192291583));
#15613=DIRECTION('center_axis',(0.22410050459774,0.965884999831614,0.129788793581424));
#15614=DIRECTION('ref_axis',(-0.974172903424311,0.225797069271315,0.00168455998189598));
#15615=DIRECTION('center_axis',(0.299192153321727,0.945324776880847,0.129788757625169));
#15616=DIRECTION('ref_axis',(-0.953454016134601,0.30153374832286,0.00168455904205274));
#15617=DIRECTION('center_axis',(0.669073609076934,0.731775511004093,0.129788701863703));
#15618=DIRECTION('ref_axis',(-0.738165771540547,0.674617262288319,0.0016861638597269));
#15619=DIRECTION('center_axis',(0.609608600175811,0.782005273294383,0.129788701863703));
#15620=DIRECTION('ref_axis',(-0.788810454558216,0.614634228154292,0.00168296192405618));
#15621=DIRECTION('center_axis',(0.540944081288723,0.830983991294197,0.129788701863706));
#15622=DIRECTION('ref_axis',(-0.838191657988026,0.545373186101464,0.00168296191918214));
#15623=DIRECTION('center_axis',(0.604462756308468,0.785989611320978,0.129788701863709));
#15624=DIRECTION('ref_axis',(-0.792827882999811,0.60944327446407,0.0016861638564983));
#15625=DIRECTION('center_axis',(0.879005498370731,0.458807396085279,0.129788701863717));
#15626=DIRECTION('ref_axis',(-0.462916235690331,0.886400426210261,0.00168616385968331));
#15627=DIRECTION('center_axis',(0.84030625880358,0.526346163930226,0.129788701863705));
#15628=DIRECTION('ref_axis',(-0.531022076545447,0.847356313400996,0.00168296192330928));
#15629=DIRECTION('center_axis',(0.792529856523363,0.595861809130046,0.129788793581438));
#15630=DIRECTION('ref_axis',(-0.601120180871209,0.799156862203554,0.00168455998284762));
#15631=DIRECTION('center_axis',(0.83683754017869,0.531843783212505,0.129788757625188));
#15632=DIRECTION('ref_axis',(-0.5365659935158,0.843856680285963,0.00168455903923744));
#15633=DIRECTION('center_axis',(0.98291635181687,0.130500337928863,0.129788701863709));
#15634=DIRECTION('ref_axis',(-0.131832169906245,0.99127061684953,0.00168616385986865));
#15635=DIRECTION('center_axis',(0.969650581024497,0.20720193914968,0.129788701863711));
#15636=DIRECTION('ref_axis',(-0.209184599045755,0.977874721608669,0.00168296192350968));
#15637=DIRECTION('center_axis',(0.948531199288787,0.288865769928619,0.129788793581424));
#15638=DIRECTION('ref_axis',(-0.291540453618539,0.956557016680951,0.00168455998264496));
#15639=DIRECTION('center_axis',(0.968271348265747,0.213554383054406,0.12978875762517));
#15640=DIRECTION('ref_axis',(-0.215591121924833,0.976482273473528,0.00168455904061127));
#15641=DIRECTION('center_axis',(0.968272986934853,-0.213546986962567,0.129788701863712));
#15642=DIRECTION('ref_axis',(0.215152801205168,0.976578941501918,0.00168616385981979));
#15643=DIRECTION('center_axis',(0.982040732655296,-0.136933897462913,0.129788701863709));
#15644=DIRECTION('ref_axis',(0.137883628330465,0.990447006496357,0.00168296192237878));
#15645=DIRECTION('center_axis',(0.990125680589855,-0.0529717443280386,0.129788793581422));
#15646=DIRECTION('ref_axis',(0.0532033550164054,0.998582277668026,0.00168455998277367));
#15647=DIRECTION('center_axis',(0.982917341583747,-0.130492827419958,0.129788757625171));
#15648=DIRECTION('ref_axis',(0.131387220749417,0.991329693131696,0.00168455904058849));
#15649=DIRECTION('center_axis',(0.836841609645931,-0.531837393602351,0.129788701863704));
#15650=DIRECTION('ref_axis',(0.53618716916805,0.844097433043719,0.00168616385845728));
#15651=DIRECTION('center_axis',(0.875982278548042,-0.464553485121265,0.129788701863712));
#15652=DIRECTION('ref_axis',(0.468321055193095,0.883556764957403,0.00168296192337288));
#15653=DIRECTION('center_axis',(0.912293431178322,-0.38842706947047,0.129788701863712));
#15654=DIRECTION('ref_axis',(0.391537288042102,0.920160703199067,0.00168296192312245));
#15655=DIRECTION('center_axis',(0.879012519102615,-0.458793945175181,0.129788701863713));
#15656=DIRECTION('ref_axis',(0.46251134465318,0.886611759970813,0.00168616386051783));
#15657=DIRECTION('center_axis',(0.60447478375946,-0.785980361502429,0.129788701863699));
#15658=DIRECTION('ref_axis',(0.792549451262032,0.609805316601694,0.00168616385909342));
#15659=DIRECTION('center_axis',(0.664267433536779,-0.736141066379941,0.129788701863701));
#15660=DIRECTION('ref_axis',(0.742272051102183,0.670096537665826,0.00168296192169911));
#15661=DIRECTION('center_axis',(0.724430694688769,-0.677019229899289,0.129788793581426));
#15662=DIRECTION('ref_axis',(0.682632449802081,0.730759947407406,0.00168455998210372));
#15663=DIRECTION('center_axis',(0.669079194957684,-0.731770393818234,0.129788757625171));
#15664=DIRECTION('ref_axis',(0.737862894201601,0.674948525164164,0.0016845590394145));
#15665=DIRECTION('center_axis',(0.29919937785432,-0.945322497965705,0.12978870186371));
#15666=DIRECTION('ref_axis',(0.953318572744759,0.301961679210016,0.00168616386027698));
#15667=DIRECTION('center_axis',(0.372432132484241,-0.918939170762557,0.129788701863703));
#15668=DIRECTION('ref_axis',(0.926694082893838,0.375812778346763,0.00168296192307007));
#15669=DIRECTION('center_axis',(0.449187964027621,-0.883959864492387,0.129788793581425));
#15670=DIRECTION('ref_axis',(0.891399297735882,0.453215681826704,0.00168455998165862));
#15671=DIRECTION('center_axis',(0.378448567230374,-0.916477801343488,0.129788757625164));
#15672=DIRECTION('ref_axis',(0.924210308154263,0.381880175660163,0.00168455904178805));
#15673=DIRECTION('center_axis',(-0.0421638887269278,-0.990644789698082,
0.12978870186371));
#15674=DIRECTION('ref_axis',(0.999103404868793,-0.0423029931685897,0.0016861638598628));
#15675=DIRECTION('center_axis',(0.0356760197477962,-0.990899649048019,0.129788701863709));
#15676=DIRECTION('ref_axis',(0.999343131735064,0.036200451559631,0.00168296192257817));
#15677=DIRECTION('center_axis',(0.119759005916489,-0.984282821840566,0.12978870186371));
#15678=DIRECTION('ref_axis',(0.992651188554834,0.120999113632468,0.00168296192272656));
#15679=DIRECTION('center_axis',(0.0421790479366033,-0.990644144374606,0.12978870186371));
#15680=DIRECTION('ref_axis',(0.999083979754942,0.0427593059867003,0.00168616385957026));
#15681=DIRECTION('',(-0.956649531312375,0.291241608016117,0.));
#15682=DIRECTION('',(0.886464649099777,-0.462796311455061,0.));
#15683=DIRECTION('center_axis',(0.,0.,1.));
#15684=DIRECTION('ref_axis',(1.,0.,0.));
#15685=DIRECTION('center_axis',(0.,0.,1.));
#15686=DIRECTION('ref_axis',(1.,0.,0.));
#15687=DIRECTION('center_axis',(0.,0.,1.));
#15688=DIRECTION('ref_axis',(1.,0.,0.));
#15689=DIRECTION('center_axis',(0.,0.,1.));
#15690=DIRECTION('ref_axis',(1.,0.,0.));
#15691=DIRECTION('',(0.674718628572079,-0.738075045139593,0.));
#15692=DIRECTION('',(-0.799346008736428,0.600870999730511,0.));
#15693=DIRECTION('',(-0.54562956041628,0.838026480965809,0.));
#15694=DIRECTION('',(0.381591583652422,-0.924331035552543,0.));
#15695=DIRECTION('center_axis',(0.,0.,1.));
#15696=DIRECTION('ref_axis',(1.,0.,0.));
#15697=DIRECTION('center_axis',(0.,0.,1.));
#15698=DIRECTION('ref_axis',(1.,0.,0.));
#15699=DIRECTION('center_axis',(0.,0.,1.));
#15700=DIRECTION('ref_axis',(1.,0.,0.));
#15701=DIRECTION('',(-0.226102134475161,0.974103600643061,0.));
#15702=DIRECTION('',(0.0424389620521028,-0.999099061404794,0.));
#15703=DIRECTION('center_axis',(0.,0.,1.));
#15704=DIRECTION('ref_axis',(1.,0.,0.));
#15705=DIRECTION('',(0.120696545795735,0.992689449844703,0.));
#15706=DIRECTION('',(-0.301832424704053,-0.953360995319859,0.));
#15707=DIRECTION('center_axis',(0.,0.,1.));
#15708=DIRECTION('ref_axis',(1.,0.,0.));
#15709=DIRECTION('',(0.452937441352379,0.891542300859113,0.));
#15710=DIRECTION('',(-0.609698366468669,-0.792633523089604,0.));
#15711=DIRECTION('center_axis',(0.,0.,1.));
#15712=DIRECTION('ref_axis',(1.,0.,0.));
#15713=DIRECTION('',(0.73054739683727,0.682861992626833,0.));
#15714=DIRECTION('',(-0.844025687047658,-0.536302749949811,0.));
#15715=DIRECTION('center_axis',(0.,0.,1.));
#15716=DIRECTION('ref_axis',(1.,0.,0.));
#15717=DIRECTION('',(0.920042554532171,0.391818450114231,0.));
#15718=DIRECTION('',(-0.976551053276238,-0.215285950180383,0.));
#15719=DIRECTION('center_axis',(0.,0.,1.));
#15720=DIRECTION('ref_axis',(1.,0.,0.));
#15721=DIRECTION('',(0.998567001768609,0.0535158198932806,0.));
#15722=DIRECTION('',(-0.991289950121085,0.131697512462977,0.));
#15723=DIRECTION('center_axis',(0.,0.,1.));
#15724=DIRECTION('ref_axis',(1.,0.,0.));
#15725=DIRECTION('',(0.956649531312375,-0.291241608016117,0.));
#15726=DIRECTION('',(-0.886464649099777,0.462796311455061,0.));
#15727=DIRECTION('center_axis',(0.,0.,1.));
#15728=DIRECTION('ref_axis',(1.,0.,0.));
#15729=DIRECTION('',(0.799346008736428,-0.600870999730511,0.));
#15730=DIRECTION('',(-0.674718628572181,0.7380750451395,0.));
#15731=DIRECTION('center_axis',(0.,0.,1.));
#15732=DIRECTION('ref_axis',(1.,0.,0.));
#15733=DIRECTION('',(0.545629560416191,-0.838026480965866,0.));
#15734=DIRECTION('',(-0.381591583652368,0.924331035552565,0.));
#15735=DIRECTION('center_axis',(0.,0.,1.));
#15736=DIRECTION('ref_axis',(1.,0.,0.));
#15737=DIRECTION('',(0.226102134475161,-0.974103600643061,0.));
#15738=DIRECTION('',(-0.0424389620521028,0.999099061404794,0.));
#15739=DIRECTION('center_axis',(0.,0.,1.));
#15740=DIRECTION('ref_axis',(1.,0.,0.));
#15741=DIRECTION('',(-0.120696545795755,-0.9926894498447,0.));
#15742=DIRECTION('',(0.301832424704055,0.953360995319859,0.));
#15743=DIRECTION('center_axis',(0.,0.,1.));
#15744=DIRECTION('ref_axis',(1.,0.,0.));
#15745=DIRECTION('',(-0.452937441352379,-0.891542300859113,0.));
#15746=DIRECTION('',(0.609698366468669,0.792633523089604,0.));
#15747=DIRECTION('center_axis',(0.,0.,1.));
#15748=DIRECTION('ref_axis',(1.,0.,0.));
#15749=DIRECTION('',(-0.730547396837178,-0.68286199262693,0.));
#15750=DIRECTION('',(0.844025687047666,0.536302749949798,0.));
#15751=DIRECTION('center_axis',(0.,0.,1.));
#15752=DIRECTION('ref_axis',(1.,0.,0.));
#15753=DIRECTION('',(-0.920042554532177,-0.391818450114216,0.));
#15754=DIRECTION('',(0.976551053276238,0.215285950180383,0.));
#15755=DIRECTION('center_axis',(0.,0.,1.));
#15756=DIRECTION('ref_axis',(1.,0.,0.));
#15757=DIRECTION('',(-0.998567001768609,-0.0535158198932787,0.));
#15758=DIRECTION('',(0.991289950121088,-0.131697512462957,0.));
#15759=DIRECTION('center_axis',(0.,0.,1.));
#15760=DIRECTION('ref_axis',(1.,0.,0.));
#15761=DIRECTION('center_axis',(0.,0.,1.));
#15762=DIRECTION('ref_axis',(1.,0.,0.));
#15763=DIRECTION('center_axis',(0.,0.,1.));
#15764=DIRECTION('ref_axis',(1.,0.,0.));
#15765=DIRECTION('center_axis',(0.,0.,1.));
#15766=DIRECTION('ref_axis',(1.,0.,0.));
#15767=DIRECTION('center_axis',(0.,0.,1.));
#15768=DIRECTION('ref_axis',(1.,0.,0.));
#15769=DIRECTION('center_axis',(0.,0.,1.));
#15770=DIRECTION('ref_axis',(1.,0.,0.));
#15771=DIRECTION('center_axis',(0.,0.,1.));
#15772=DIRECTION('ref_axis',(-0.990865895863231,0.134850941469303,0.));
#15773=DIRECTION('center_axis',(0.,0.,1.));
#15774=DIRECTION('ref_axis',(1.,0.,0.));
#15775=DIRECTION('center_axis',(0.,0.,1.));
#15776=DIRECTION('ref_axis',(1.,0.,0.));
#15777=DIRECTION('center_axis',(0.,0.,1.));
#15778=DIRECTION('ref_axis',(1.,0.,0.));
#15779=DIRECTION('center_axis',(0.,0.,1.));
#15780=DIRECTION('ref_axis',(1.,0.,0.));
#15781=DIRECTION('center_axis',(0.,0.,1.));
#15782=DIRECTION('ref_axis',(1.,0.,0.));
#15783=DIRECTION('center_axis',(0.,0.,1.));
#15784=DIRECTION('ref_axis',(1.,0.,0.));
#15785=DIRECTION('center_axis',(0.,0.,1.));
#15786=DIRECTION('ref_axis',(1.,0.,0.));
#15787=DIRECTION('center_axis',(0.,0.,1.));
#15788=DIRECTION('ref_axis',(1.,0.,0.));
#15789=DIRECTION('center_axis',(0.,0.,1.));
#15790=DIRECTION('ref_axis',(1.,0.,0.));
#15791=DIRECTION('axis',(0.,0.,1.));
#15792=DIRECTION('refdir',(1.,0.,0.));
#15793=DIRECTION('center_axis',(-1.,0.,0.));
#15794=DIRECTION('ref_axis',(0.,1.,0.));
#15795=DIRECTION('center_axis',(-1.,0.,0.));
#15796=DIRECTION('ref_axis',(0.,1.,0.));
#15797=DIRECTION('',(-1.,0.,0.));
#15798=DIRECTION('center_axis',(1.,0.,0.));
#15799=DIRECTION('ref_axis',(0.,1.,0.));
#15800=DIRECTION('center_axis',(-1.,0.,0.));
#15801=DIRECTION('ref_axis',(0.,1.,0.));
#15802=DIRECTION('center_axis',(-1.,0.,0.));
#15803=DIRECTION('ref_axis',(0.,1.,0.));
#15804=DIRECTION('',(-1.,0.,0.));
#15805=DIRECTION('center_axis',(1.,0.,0.));
#15806=DIRECTION('ref_axis',(0.,1.,0.));
#15807=DIRECTION('center_axis',(-1.,0.,0.));
#15808=DIRECTION('ref_axis',(0.,1.,0.));
#15809=DIRECTION('center_axis',(-1.,0.,0.));
#15810=DIRECTION('ref_axis',(0.,1.,0.));
#15811=DIRECTION('',(-1.,0.,0.));
#15812=DIRECTION('center_axis',(1.,0.,0.));
#15813=DIRECTION('ref_axis',(0.,1.,0.));
#15814=DIRECTION('center_axis',(1.,0.,0.));
#15815=DIRECTION('ref_axis',(0.,0.,-1.));
#15816=DIRECTION('center_axis',(-1.,0.,0.));
#15817=DIRECTION('ref_axis',(0.,0.342020143325669,0.939692620785908));
#15818=DIRECTION('center_axis',(0.,-1.,0.));
#15819=DIRECTION('ref_axis',(0.,0.,1.));
#15820=DIRECTION('center_axis',(1.,0.,0.));
#15821=DIRECTION('ref_axis',(0.,0.342020143325669,0.939692620785908));
#15822=DIRECTION('center_axis',(1.,0.,0.));
#15823=DIRECTION('ref_axis',(0.,0.342020143325669,0.939692620785908));
#15824=DIRECTION('center_axis',(1.,0.,0.));
#15825=DIRECTION('ref_axis',(0.,-0.296296296296299,-0.955096070979823));
#15826=DIRECTION('',(-1.,0.,0.));
#15827=DIRECTION('center_axis',(1.,0.,0.));
#15828=DIRECTION('ref_axis',(0.,-0.296296296296299,-0.955096070979823));
#15829=DIRECTION('center_axis',(1.,0.,0.));
#15830=DIRECTION('ref_axis',(0.,1.,0.));
#15831=DIRECTION('center_axis',(-1.,0.,0.));
#15832=DIRECTION('ref_axis',(0.,1.,0.));
#15833=DIRECTION('center_axis',(1.,0.,0.));
#15834=DIRECTION('ref_axis',(0.,1.,0.));
#15835=DIRECTION('center_axis',(-1.,0.,0.));
#15836=DIRECTION('ref_axis',(0.,1.,0.));
#15837=DIRECTION('',(1.,0.,0.));
#15838=DIRECTION('center_axis',(1.,0.,0.));
#15839=DIRECTION('ref_axis',(0.,1.,0.));
#15840=DIRECTION('axis',(0.,0.,1.));
#15841=DIRECTION('refdir',(1.,0.,0.));
#15842=DIRECTION('center_axis',(0.,0.,1.));
#15843=DIRECTION('ref_axis',(-0.457970371486214,-0.888967456570137,0.));
#15844=DIRECTION('',(0.,0.,-1.));
#15845=DIRECTION('center_axis',(0.,0.,-1.));
#15846=DIRECTION('ref_axis',(1.,-9.05137471385603E-13,0.));
#15847=DIRECTION('center_axis',(0.,0.,1.));
#15848=DIRECTION('ref_axis',(-0.457970371486214,-0.888967456570137,0.));
#15849=DIRECTION('',(0.,0.,-1.));
#15850=DIRECTION('center_axis',(0.,0.,1.));
#15851=DIRECTION('ref_axis',(-0.457970371486214,-0.888967456570137,0.));
#15852=DIRECTION('',(0.,0.,-1.));
#15853=DIRECTION('center_axis',(0.,0.,1.));
#15854=DIRECTION('ref_axis',(-0.457970371486214,-0.888967456570137,0.));
#15855=DIRECTION('',(0.,0.,-1.));
#15856=DIRECTION('center_axis',(0.,0.,1.));
#15857=DIRECTION('ref_axis',(-0.457970371486214,-0.888967456570137,0.));
#15858=DIRECTION('',(0.,0.,-1.));
#15859=DIRECTION('center_axis',(0.,0.,1.));
#15860=DIRECTION('ref_axis',(-0.457970371486214,-0.888967456570137,0.));
#15861=DIRECTION('',(0.,0.,-1.));
#15862=DIRECTION('center_axis',(0.,0.,1.));
#15863=DIRECTION('ref_axis',(-0.457970371486214,-0.888967456570137,0.));
#15864=DIRECTION('',(0.,0.,-1.));
#15865=DIRECTION('center_axis',(0.,0.,1.));
#15866=DIRECTION('ref_axis',(-0.457970371486214,-0.888967456570137,0.));
#15867=DIRECTION('',(0.,0.,-1.));
#15868=DIRECTION('center_axis',(0.,0.,1.));
#15869=DIRECTION('ref_axis',(-0.457970371486214,-0.888967456570137,0.));
#15870=DIRECTION('',(0.,0.,-1.));
#15871=DIRECTION('center_axis',(0.,0.,1.));
#15872=DIRECTION('ref_axis',(-0.457970371486214,-0.888967456570137,0.));
#15873=DIRECTION('',(0.,0.,-1.));
#15874=DIRECTION('center_axis',(0.,0.,1.));
#15875=DIRECTION('ref_axis',(-0.457970371486214,-0.888967456570137,0.));
#15876=DIRECTION('',(0.,0.,-1.));
#15877=DIRECTION('center_axis',(0.,0.,1.));
#15878=DIRECTION('ref_axis',(-0.457970371486214,-0.888967456570137,0.));
#15879=DIRECTION('',(0.,0.,-1.));
#15880=DIRECTION('center_axis',(0.,0.,1.));
#15881=DIRECTION('ref_axis',(-0.457970371486214,-0.888967456570137,0.));
#15882=DIRECTION('',(0.,0.,-1.));
#15883=DIRECTION('center_axis',(0.,0.,1.));
#15884=DIRECTION('ref_axis',(-0.457970371486214,-0.888967456570137,0.));
#15885=DIRECTION('',(0.,0.,-1.));
#15886=DIRECTION('center_axis',(0.,0.,1.));
#15887=DIRECTION('ref_axis',(-0.457970371486214,-0.888967456570137,0.));
#15888=DIRECTION('',(0.,0.,-1.));
#15889=DIRECTION('center_axis',(0.,0.,1.));
#15890=DIRECTION('ref_axis',(-0.457970371486214,-0.888967456570137,0.));
#15891=DIRECTION('',(0.,0.,-1.));
#15892=DIRECTION('center_axis',(0.,0.,1.));
#15893=DIRECTION('ref_axis',(-0.457970371486214,-0.888967456570137,0.));
#15894=DIRECTION('',(0.,0.,-1.));
#15895=DIRECTION('center_axis',(0.,0.,1.));
#15896=DIRECTION('ref_axis',(-0.457970371486214,-0.888967456570137,0.));
#15897=DIRECTION('',(0.,0.,-1.));
#15898=DIRECTION('center_axis',(0.,0.,1.));
#15899=DIRECTION('ref_axis',(-0.457970371486214,-0.888967456570137,0.));
#15900=DIRECTION('',(0.,0.,-1.));
#15901=DIRECTION('center_axis',(0.,0.,1.));
#15902=DIRECTION('ref_axis',(-0.457970371486214,-0.888967456570137,0.));
#15903=DIRECTION('',(0.,0.,-1.));
#15904=DIRECTION('center_axis',(0.,0.,1.));
#15905=DIRECTION('ref_axis',(-0.457970371486214,-0.888967456570137,0.));
#15906=DIRECTION('',(0.,0.,-1.));
#15907=DIRECTION('center_axis',(0.,0.,1.));
#15908=DIRECTION('ref_axis',(-0.457970371486214,-0.888967456570137,0.));
#15909=DIRECTION('',(0.,0.,-1.));
#15910=DIRECTION('center_axis',(0.,0.,1.));
#15911=DIRECTION('ref_axis',(-0.457970371486214,-0.888967456570137,0.));
#15912=DIRECTION('',(0.,0.,-1.));
#15913=DIRECTION('center_axis',(0.,0.,1.));
#15914=DIRECTION('ref_axis',(-0.457970371486214,-0.888967456570137,0.));
#15915=DIRECTION('',(0.,0.,-1.));
#15916=DIRECTION('center_axis',(0.,0.,1.));
#15917=DIRECTION('ref_axis',(-0.457970371486214,-0.888967456570137,0.));
#15918=DIRECTION('',(0.,0.,-1.));
#15919=DIRECTION('center_axis',(0.,0.,1.));
#15920=DIRECTION('ref_axis',(-0.457970371486214,-0.888967456570137,0.));
#15921=DIRECTION('',(0.,0.,-1.));
#15922=DIRECTION('center_axis',(0.,0.,1.));
#15923=DIRECTION('ref_axis',(-0.457970371486214,-0.888967456570137,0.));
#15924=DIRECTION('',(0.,0.,-1.));
#15925=DIRECTION('center_axis',(0.,0.,1.));
#15926=DIRECTION('ref_axis',(-0.457970371486214,-0.888967456570137,0.));
#15927=DIRECTION('',(0.,0.,-1.));
#15928=DIRECTION('center_axis',(0.,0.,1.));
#15929=DIRECTION('ref_axis',(-0.457970371486214,-0.888967456570137,0.));
#15930=DIRECTION('',(0.,0.,-1.));
#15931=DIRECTION('center_axis',(0.,0.,1.));
#15932=DIRECTION('ref_axis',(-0.457970371486214,-0.888967456570137,0.));
#15933=DIRECTION('',(0.,0.,-1.));
#15934=DIRECTION('center_axis',(0.,0.,1.));
#15935=DIRECTION('ref_axis',(-0.457970371486214,-0.888967456570137,0.));
#15936=DIRECTION('',(0.,0.,-1.));
#15937=DIRECTION('center_axis',(0.,0.,1.));
#15938=DIRECTION('ref_axis',(-0.457970371486214,-0.888967456570137,0.));
#15939=DIRECTION('',(0.,0.,-1.));
#15940=DIRECTION('center_axis',(0.,0.,1.));
#15941=DIRECTION('ref_axis',(-0.457970371486214,-0.888967456570137,0.));
#15942=DIRECTION('',(0.,0.,-1.));
#15943=DIRECTION('center_axis',(0.,0.,1.));
#15944=DIRECTION('ref_axis',(-0.457970371486214,-0.888967456570137,0.));
#15945=DIRECTION('',(0.,0.,-1.));
#15946=DIRECTION('center_axis',(0.,0.,1.));
#15947=DIRECTION('ref_axis',(-0.457970371486214,-0.888967456570137,0.));
#15948=DIRECTION('',(0.,0.,-1.));
#15949=DIRECTION('center_axis',(0.,0.,1.));
#15950=DIRECTION('ref_axis',(-0.457970371486214,-0.888967456570137,0.));
#15951=DIRECTION('',(0.,0.,-1.));
#15952=DIRECTION('center_axis',(0.,0.,1.));
#15953=DIRECTION('ref_axis',(-0.457970371486214,-0.888967456570137,0.));
#15954=DIRECTION('',(0.,0.,-1.));
#15955=DIRECTION('center_axis',(0.,0.,1.));
#15956=DIRECTION('ref_axis',(-0.457970371486214,-0.888967456570137,0.));
#15957=DIRECTION('',(0.,0.,-1.));
#15958=DIRECTION('center_axis',(0.,0.,1.));
#15959=DIRECTION('ref_axis',(-0.457970371486214,-0.888967456570137,0.));
#15960=DIRECTION('',(0.,0.,-1.));
#15961=DIRECTION('center_axis',(0.,0.,1.));
#15962=DIRECTION('ref_axis',(-0.457970371486214,-0.888967456570137,0.));
#15963=DIRECTION('',(0.,0.,-1.));
#15964=DIRECTION('center_axis',(0.,0.,1.));
#15965=DIRECTION('ref_axis',(-0.457970371486214,-0.888967456570137,0.));
#15966=DIRECTION('',(0.,0.,-1.));
#15967=DIRECTION('center_axis',(0.,0.,1.));
#15968=DIRECTION('ref_axis',(-0.457970371486214,-0.888967456570137,0.));
#15969=DIRECTION('',(0.,0.,-1.));
#15970=DIRECTION('center_axis',(0.,0.,1.));
#15971=DIRECTION('ref_axis',(-0.457970371486214,-0.888967456570137,0.));
#15972=DIRECTION('',(0.,0.,-1.));
#15973=DIRECTION('center_axis',(0.,0.,1.));
#15974=DIRECTION('ref_axis',(-0.457970371486214,-0.888967456570137,0.));
#15975=DIRECTION('',(0.,0.,-1.));
#15976=DIRECTION('center_axis',(0.,0.,1.));
#15977=DIRECTION('ref_axis',(-0.457970371486214,-0.888967456570137,0.));
#15978=DIRECTION('',(0.,0.,-1.));
#15979=DIRECTION('center_axis',(0.,0.,1.));
#15980=DIRECTION('ref_axis',(-0.457970371486214,-0.888967456570137,0.));
#15981=DIRECTION('',(0.,0.,-1.));
#15982=DIRECTION('center_axis',(0.,0.,1.));
#15983=DIRECTION('ref_axis',(-0.457970371486214,-0.888967456570137,0.));
#15984=DIRECTION('',(0.,0.,-1.));
#15985=DIRECTION('center_axis',(0.,0.,1.));
#15986=DIRECTION('ref_axis',(-0.457970371486214,-0.888967456570137,0.));
#15987=DIRECTION('',(0.,0.,-1.));
#15988=DIRECTION('center_axis',(0.,0.,1.));
#15989=DIRECTION('ref_axis',(-0.457970371486214,-0.888967456570137,0.));
#15990=DIRECTION('',(0.,0.,-1.));
#15991=DIRECTION('center_axis',(0.,0.,1.));
#15992=DIRECTION('ref_axis',(-0.457970371486214,-0.888967456570137,0.));
#15993=DIRECTION('',(0.,0.,-1.));
#15994=DIRECTION('center_axis',(0.,0.,1.));
#15995=DIRECTION('ref_axis',(-0.457970371486214,-0.888967456570137,0.));
#15996=DIRECTION('',(0.,0.,-1.));
#15997=DIRECTION('center_axis',(0.,0.,1.));
#15998=DIRECTION('ref_axis',(-0.457970371486214,-0.888967456570137,0.));
#15999=DIRECTION('',(0.,0.,-1.));
#16000=DIRECTION('center_axis',(0.,0.,1.));
#16001=DIRECTION('ref_axis',(-0.457970371486214,-0.888967456570137,0.));
#16002=DIRECTION('',(0.,0.,-1.));
#16003=DIRECTION('center_axis',(0.,0.,1.));
#16004=DIRECTION('ref_axis',(-0.457970371486214,-0.888967456570137,0.));
#16005=DIRECTION('',(0.,0.,-1.));
#16006=DIRECTION('center_axis',(0.,0.,1.));
#16007=DIRECTION('ref_axis',(-0.457970371486214,-0.888967456570137,0.));
#16008=DIRECTION('',(0.,0.,-1.));
#16009=DIRECTION('center_axis',(0.,0.,1.));
#16010=DIRECTION('ref_axis',(-0.457970371486214,-0.888967456570137,0.));
#16011=DIRECTION('',(0.,0.,-1.));
#16012=DIRECTION('center_axis',(0.,0.,1.));
#16013=DIRECTION('ref_axis',(-0.457970371486214,-0.888967456570137,0.));
#16014=DIRECTION('',(0.,0.,-1.));
#16015=DIRECTION('center_axis',(0.,0.,1.));
#16016=DIRECTION('ref_axis',(-0.457970371486214,-0.888967456570137,0.));
#16017=DIRECTION('',(0.,0.,-1.));
#16018=DIRECTION('center_axis',(0.,0.,1.));
#16019=DIRECTION('ref_axis',(-0.457970371486214,-0.888967456570137,0.));
#16020=DIRECTION('',(0.,0.,-1.));
#16021=DIRECTION('center_axis',(0.,0.,1.));
#16022=DIRECTION('ref_axis',(-0.457970371486214,-0.888967456570137,0.));
#16023=DIRECTION('',(0.,0.,-1.));
#16024=DIRECTION('center_axis',(0.,0.,1.));
#16025=DIRECTION('ref_axis',(1.,0.,0.));
#16026=DIRECTION('center_axis',(0.,0.,-1.));
#16027=DIRECTION('ref_axis',(1.,0.,0.));
#16028=DIRECTION('center_axis',(0.,0.,-1.));
#16029=DIRECTION('ref_axis',(1.,0.,0.));
#16030=DIRECTION('center_axis',(0.,0.,1.));
#16031=DIRECTION('ref_axis',(-0.457970371486214,-0.888967456570137,0.));
#16032=DIRECTION('center_axis',(0.,0.,1.));
#16033=DIRECTION('ref_axis',(1.,-9.05137471385603E-13,0.));
#16034=DIRECTION('center_axis',(0.,0.,-1.));
#16035=DIRECTION('ref_axis',(-1.,0.,0.));
#16036=DIRECTION('center_axis',(0.,0.,-1.));
#16037=DIRECTION('ref_axis',(-1.,0.,0.));
#16038=DIRECTION('',(0.,0.,-1.));
#16039=DIRECTION('center_axis',(0.,0.,1.));
#16040=DIRECTION('ref_axis',(-1.,0.,0.));
#16041=DIRECTION('center_axis',(0.,0.,-1.));
#16042=DIRECTION('ref_axis',(-1.,0.,0.));
#16043=DIRECTION('center_axis',(0.,0.,-1.));
#16044=DIRECTION('ref_axis',(-1.,0.,0.));
#16045=DIRECTION('',(0.,0.,-1.));
#16046=DIRECTION('center_axis',(0.,0.,1.));
#16047=DIRECTION('ref_axis',(-1.,0.,0.));
#16048=DIRECTION('center_axis',(0.,0.,-1.));
#16049=DIRECTION('ref_axis',(-1.,0.,0.));
#16050=DIRECTION('center_axis',(0.,0.,-1.));
#16051=DIRECTION('ref_axis',(-1.,0.,0.));
#16052=DIRECTION('',(0.,0.,-1.));
#16053=DIRECTION('center_axis',(0.,0.,1.));
#16054=DIRECTION('ref_axis',(-1.,0.,0.));
#16055=DIRECTION('center_axis',(0.,0.,-1.));
#16056=DIRECTION('ref_axis',(-1.,0.,0.));
#16057=DIRECTION('center_axis',(0.,0.,-1.));
#16058=DIRECTION('ref_axis',(-1.,0.,0.));
#16059=DIRECTION('',(0.,0.,-1.));
#16060=DIRECTION('center_axis',(0.,0.,1.));
#16061=DIRECTION('ref_axis',(-1.,0.,0.));
#16062=DIRECTION('center_axis',(0.,0.,1.));
#16063=DIRECTION('ref_axis',(1.,0.,0.));
#16064=DIRECTION('center_axis',(0.,0.,-1.));
#16065=DIRECTION('ref_axis',(-1.,0.,0.));
#16066=DIRECTION('center_axis',(1.22464679914735E-16,-1.,0.));
#16067=DIRECTION('ref_axis',(-1.,-1.22464679914735E-16,0.));
#16068=DIRECTION('center_axis',(0.,0.,1.));
#16069=DIRECTION('ref_axis',(-1.,0.,0.));
#16070=DIRECTION('center_axis',(0.,0.,-1.));
#16071=DIRECTION('ref_axis',(-1.,0.,0.));
#16072=DIRECTION('center_axis',(0.,0.,1.));
#16073=DIRECTION('ref_axis',(-1.,0.,0.));
#16074=DIRECTION('center_axis',(0.,0.,1.));
#16075=DIRECTION('ref_axis',(-1.,0.,0.));
#16076=DIRECTION('center_axis',(0.,0.,1.));
#16077=DIRECTION('ref_axis',(-1.,0.,0.));
#16078=DIRECTION('',(0.,0.,-1.));
#16079=DIRECTION('center_axis',(0.,0.,1.));
#16080=DIRECTION('ref_axis',(-1.,0.,0.));
#16081=DIRECTION('center_axis',(0.,0.,1.));
#16082=DIRECTION('ref_axis',(1.,0.,0.));
#16083=DIRECTION('center_axis',(0.,0.,-1.));
#16084=DIRECTION('ref_axis',(-1.,0.,0.));
#16085=DIRECTION('center_axis',(1.22464679914735E-16,-1.,0.));
#16086=DIRECTION('ref_axis',(-1.,-1.22464679914735E-16,0.));
#16087=DIRECTION('center_axis',(0.,0.,1.));
#16088=DIRECTION('ref_axis',(-1.,0.,0.));
#16089=DIRECTION('center_axis',(0.,0.,1.));
#16090=DIRECTION('ref_axis',(1.,0.,0.));
#16091=DIRECTION('axis',(0.,0.,1.));
#16092=DIRECTION('refdir',(1.,0.,0.));
#16093=DIRECTION('center_axis',(1.,0.,0.));
#16094=DIRECTION('ref_axis',(0.,-0.707106781186547,0.707106781186547));
#16095=DIRECTION('',(-1.,0.,0.));
#16096=DIRECTION('center_axis',(1.,0.,0.));
#16097=DIRECTION('ref_axis',(0.,-0.707106781186547,0.707106781186547));
#16098=DIRECTION('center_axis',(1.,0.,0.));
#16099=DIRECTION('ref_axis',(0.,-0.707106781186547,0.707106781186547));
#16100=DIRECTION('',(-1.,0.,0.));
#16101=DIRECTION('center_axis',(1.,0.,0.));
#16102=DIRECTION('ref_axis',(0.,-0.707106781186547,0.707106781186547));
#16103=DIRECTION('',(-1.,0.,0.));
#16104=DIRECTION('center_axis',(1.,0.,0.));
#16105=DIRECTION('ref_axis',(0.,-0.707106781186547,0.707106781186547));
#16106=DIRECTION('',(-1.,0.,0.));
#16107=DIRECTION('center_axis',(1.,0.,0.));
#16108=DIRECTION('ref_axis',(0.,-0.707106781186547,0.707106781186547));
#16109=DIRECTION('',(-1.,0.,0.));
#16110=DIRECTION('center_axis',(1.,0.,0.));
#16111=DIRECTION('ref_axis',(0.,-0.707106781186547,0.707106781186547));
#16112=DIRECTION('',(-1.,0.,0.));
#16113=DIRECTION('center_axis',(-1.,0.,0.));
#16114=DIRECTION('ref_axis',(0.,-0.707106781186547,0.707106781186547));
#16115=DIRECTION('center_axis',(1.,0.,0.));
#16116=DIRECTION('ref_axis',(0.,-0.707106781186547,0.707106781186547));
#16117=DIRECTION('center_axis',(-1.,0.,0.));
#16118=DIRECTION('ref_axis',(0.,-0.707106781186547,0.707106781186547));
#16119=DIRECTION('center_axis',(1.,0.,0.));
#16120=DIRECTION('ref_axis',(0.,1.,0.));
#16121=DIRECTION('center_axis',(1.,1.40500107149015E-14,5.65401519314285E-15));
#16122=DIRECTION('ref_axis',(-8.92539775295977E-15,0.848328765343848,-0.529469834731104));
#16123=DIRECTION('center_axis',(-1.,0.,0.));
#16124=DIRECTION('ref_axis',(0.,1.,0.));
#16125=DIRECTION('',(-0.250380004054441,-0.684583761701115,-0.684583761701115));
#16126=DIRECTION('',(-0.250380004054442,0.684583761701115,0.684583761701115));
#16127=DIRECTION('',(-1.,0.,0.));
#16128=DIRECTION('center_axis',(1.,0.,0.));
#16129=DIRECTION('ref_axis',(0.,1.,0.));
#16130=DIRECTION('center_axis',(-1.,-4.36462899777869E-14,-5.90366440881238E-14));
#16131=DIRECTION('ref_axis',(2.59961128384679E-14,0.541519248253379,-0.840688351157012));
#16132=DIRECTION('center_axis',(-1.,0.,0.));
#16133=DIRECTION('ref_axis',(0.,1.,0.));
#16134=DIRECTION('',(-1.,0.,0.));
#16135=DIRECTION('',(-0.250380004054442,0.684583761701115,0.684583761701115));
#16136=DIRECTION('',(-0.250380004054441,-0.684583761701115,-0.684583761701115));
#16137=DIRECTION('center_axis',(-1.,0.,0.));
#16138=DIRECTION('ref_axis',(0.,1.,0.));
#16139=DIRECTION('center_axis',(-1.,0.,0.));
#16140=DIRECTION('ref_axis',(0.,1.,0.));
#16141=DIRECTION('',(1.,0.,0.));
#16142=DIRECTION('center_axis',(-1.,0.,0.));
#16143=DIRECTION('ref_axis',(0.,1.,0.));
#16144=DIRECTION('',(1.,0.,0.));
#16145=DIRECTION('center_axis',(1.,0.,0.));
#16146=DIRECTION('ref_axis',(0.,1.,0.));
#16147=DIRECTION('center_axis',(1.,0.,0.));
#16148=DIRECTION('ref_axis',(0.,-0.707106781186547,0.707106781186548));
#16149=DIRECTION('',(-0.250380004054441,0.684583761701115,0.684583761701115));
#16150=DIRECTION('',(-0.250380004054441,-0.684583761701115,-0.684583761701115));
#16151=DIRECTION('',(-0.250380004054441,0.684583761701115,0.684583761701115));
#16152=DIRECTION('',(-1.,0.,0.));
#16153=DIRECTION('',(-0.250380004054441,-0.684583761701115,-0.684583761701115));
#16154=DIRECTION('',(-0.250380004054442,0.684583761701115,0.684583761701115));
#16155=DIRECTION('',(-0.250380004054441,-0.684583761701115,-0.684583761701115));
#16156=DIRECTION('',(-0.250380004054441,0.684583761701115,0.684583761701115));
#16157=DIRECTION('',(-1.,0.,0.));
#16158=DIRECTION('',(-1.,0.,0.));
#16159=DIRECTION('',(-0.250380004054441,-0.684583761701115,-0.684583761701115));
#16160=DIRECTION('',(-0.250380004054442,0.684583761701115,0.684583761701115));
#16161=DIRECTION('',(-0.250380004054441,-0.684583761701115,-0.684583761701115));
#16162=DIRECTION('',(-0.250380004054441,0.684583761701115,0.684583761701115));
#16163=DIRECTION('',(-1.,0.,0.));
#16164=DIRECTION('',(-1.,0.,0.));
#16165=DIRECTION('',(-0.250380004054441,-0.684583761701115,-0.684583761701115));
#16166=DIRECTION('',(-0.250380004054442,0.684583761701115,0.684583761701115));
#16167=DIRECTION('',(-0.250380004054441,-0.684583761701115,-0.684583761701115));
#16168=DIRECTION('',(-0.250380004054441,0.684583761701115,0.684583761701115));
#16169=DIRECTION('',(-1.,0.,0.));
#16170=DIRECTION('',(-1.,0.,0.));
#16171=DIRECTION('',(-0.250380004054441,-0.684583761701115,-0.684583761701115));
#16172=DIRECTION('',(-0.250380004054442,0.684583761701115,0.684583761701115));
#16173=DIRECTION('',(-0.250380004054441,-0.684583761701115,-0.684583761701115));
#16174=DIRECTION('',(-0.250380004054441,0.684583761701115,0.684583761701115));
#16175=DIRECTION('',(-1.,0.,0.));
#16176=DIRECTION('',(-1.,0.,0.));
#16177=DIRECTION('',(-0.250380004054441,-0.684583761701115,-0.684583761701115));
#16178=DIRECTION('center_axis',(1.,0.,0.));
#16179=DIRECTION('ref_axis',(0.,-0.707106781186547,0.707106781186548));
#16180=DIRECTION('axis',(0.,0.,1.));
#16181=DIRECTION('refdir',(1.,0.,0.));
#16182=DIRECTION('center_axis',(0.,0.,1.));
#16183=DIRECTION('ref_axis',(1.,0.,0.));
#16184=DIRECTION('center_axis',(0.,0.,-1.));
#16185=DIRECTION('ref_axis',(-1.,0.,0.));
#16186=DIRECTION('center_axis',(1.22464679914735E-16,-1.,0.));
#16187=DIRECTION('ref_axis',(-1.,-1.22464679914735E-16,0.));
#16188=DIRECTION('center_axis',(0.,0.,1.));
#16189=DIRECTION('ref_axis',(-1.,0.,0.));
#16190=DIRECTION('center_axis',(0.,0.,1.));
#16191=DIRECTION('ref_axis',(-1.,0.,0.));
#16192=DIRECTION('center_axis',(0.,0.,1.));
#16193=DIRECTION('ref_axis',(-1.,0.,0.));
#16194=DIRECTION('',(0.,0.,-1.));
#16195=DIRECTION('center_axis',(0.,0.,1.));
#16196=DIRECTION('ref_axis',(-1.,0.,0.));
#16197=DIRECTION('center_axis',(0.,0.,1.));
#16198=DIRECTION('ref_axis',(-1.,0.,0.));
#16199=DIRECTION('center_axis',(0.,0.,-1.));
#16200=DIRECTION('ref_axis',(-1.,0.,0.));
#16201=DIRECTION('center_axis',(0.,0.,-1.));
#16202=DIRECTION('ref_axis',(-1.,0.,0.));
#16203=DIRECTION('center_axis',(0.,0.,-1.));
#16204=DIRECTION('ref_axis',(-1.,0.,0.));
#16205=DIRECTION('center_axis',(0.,0.,-1.));
#16206=DIRECTION('ref_axis',(-1.,0.,0.));
#16207=DIRECTION('center_axis',(0.,0.,-1.));
#16208=DIRECTION('ref_axis',(-1.,0.,0.));
#16209=DIRECTION('center_axis',(0.,0.,-1.));
#16210=DIRECTION('ref_axis',(-1.,0.,0.));
#16211=DIRECTION('',(0.,0.,-1.));
#16212=DIRECTION('center_axis',(0.,0.,1.));
#16213=DIRECTION('ref_axis',(-1.,0.,0.));
#16214=DIRECTION('center_axis',(0.,0.,-1.));
#16215=DIRECTION('ref_axis',(-1.,0.,0.));
#16216=DIRECTION('',(0.,0.,-1.));
#16217=DIRECTION('center_axis',(0.,0.,1.));
#16218=DIRECTION('ref_axis',(-1.,0.,0.));
#16219=DIRECTION('center_axis',(0.,0.,-1.));
#16220=DIRECTION('ref_axis',(-1.,0.,0.));
#16221=DIRECTION('',(0.,0.,-1.));
#16222=DIRECTION('center_axis',(0.,0.,1.));
#16223=DIRECTION('ref_axis',(-1.,0.,0.));
#16224=DIRECTION('center_axis',(0.,0.,-1.));
#16225=DIRECTION('ref_axis',(-1.,0.,0.));
#16226=DIRECTION('',(0.,0.,-1.));
#16227=DIRECTION('center_axis',(0.,0.,1.));
#16228=DIRECTION('ref_axis',(-1.,0.,0.));
#16229=DIRECTION('center_axis',(0.,0.,1.));
#16230=DIRECTION('ref_axis',(-1.,0.,0.));
#16231=DIRECTION('center_axis',(0.,0.,-1.));
#16232=DIRECTION('ref_axis',(-1.,0.,0.));
#16233=DIRECTION('',(0.,0.,1.));
#16234=DIRECTION('center_axis',(0.,0.,1.));
#16235=DIRECTION('ref_axis',(-1.,0.,0.));
#16236=DIRECTION('axis',(0.,0.,1.));
#16237=DIRECTION('refdir',(1.,0.,0.));
#16238=DIRECTION('center_axis',(0.,0.,-1.));
#16239=DIRECTION('ref_axis',(-1.,0.,0.));
#16240=DIRECTION('center_axis',(0.,0.,-1.));
#16241=DIRECTION('ref_axis',(-1.,0.,0.));
#16242=DIRECTION('',(0.,0.,-1.));
#16243=DIRECTION('center_axis',(0.,0.,-1.));
#16244=DIRECTION('ref_axis',(-1.,0.,0.));
#16245=DIRECTION('center_axis',(0.,0.,1.));
#16246=DIRECTION('ref_axis',(-1.,0.,0.));
#16247=DIRECTION('center_axis',(0.,0.,-1.));
#16248=DIRECTION('ref_axis',(-1.,0.,0.));
#16249=DIRECTION('center_axis',(0.,0.,-1.));
#16250=DIRECTION('ref_axis',(-1.,0.,0.));
#16251=DIRECTION('',(0.,0.,-1.));
#16252=DIRECTION('center_axis',(0.,0.,-1.));
#16253=DIRECTION('ref_axis',(-1.,0.,0.));
#16254=DIRECTION('center_axis',(0.,0.,1.));
#16255=DIRECTION('ref_axis',(-1.,0.,0.));
#16256=DIRECTION('center_axis',(0.,0.,-1.));
#16257=DIRECTION('ref_axis',(-1.,0.,0.));
#16258=DIRECTION('center_axis',(0.,0.,-1.));
#16259=DIRECTION('ref_axis',(-1.,0.,0.));
#16260=DIRECTION('',(0.,0.,-1.));
#16261=DIRECTION('center_axis',(0.,0.,-1.));
#16262=DIRECTION('ref_axis',(-1.,0.,0.));
#16263=DIRECTION('center_axis',(0.,0.,1.));
#16264=DIRECTION('ref_axis',(-1.,0.,0.));
#16265=DIRECTION('center_axis',(0.,0.,-1.));
#16266=DIRECTION('ref_axis',(-1.,0.,0.));
#16267=DIRECTION('center_axis',(0.,0.,-1.));
#16268=DIRECTION('ref_axis',(-1.,0.,0.));
#16269=DIRECTION('',(0.,0.,-1.));
#16270=DIRECTION('center_axis',(0.,0.,-1.));
#16271=DIRECTION('ref_axis',(-1.,0.,0.));
#16272=DIRECTION('center_axis',(0.,0.,1.));
#16273=DIRECTION('ref_axis',(-1.,0.,0.));
#16274=DIRECTION('center_axis',(0.,0.,-1.));
#16275=DIRECTION('ref_axis',(-1.,0.,0.));
#16276=DIRECTION('center_axis',(0.,0.,-1.));
#16277=DIRECTION('ref_axis',(-1.,0.,0.));
#16278=DIRECTION('',(0.,0.,-1.));
#16279=DIRECTION('center_axis',(0.,0.,1.));
#16280=DIRECTION('ref_axis',(-1.,0.,0.));
#16281=DIRECTION('center_axis',(-1.,0.,0.));
#16282=DIRECTION('ref_axis',(0.,1.,0.));
#16283=DIRECTION('center_axis',(-1.,0.,0.));
#16284=DIRECTION('ref_axis',(0.,1.,0.));
#16285=DIRECTION('',(-1.,0.,0.));
#16286=DIRECTION('center_axis',(-1.,0.,0.));
#16287=DIRECTION('ref_axis',(0.,1.,0.));
#16288=DIRECTION('center_axis',(1.,0.,0.));
#16289=DIRECTION('ref_axis',(0.,1.,0.));
#16290=DIRECTION('center_axis',(-1.,0.,0.));
#16291=DIRECTION('ref_axis',(0.,1.,0.));
#16292=DIRECTION('center_axis',(-1.,0.,0.));
#16293=DIRECTION('ref_axis',(0.,1.,0.));
#16294=DIRECTION('',(-1.,0.,0.));
#16295=DIRECTION('center_axis',(-1.,0.,0.));
#16296=DIRECTION('ref_axis',(0.,1.,0.));
#16297=DIRECTION('center_axis',(1.,0.,0.));
#16298=DIRECTION('ref_axis',(0.,1.,0.));
#16299=DIRECTION('center_axis',(-1.,0.,0.));
#16300=DIRECTION('ref_axis',(0.,1.,0.));
#16301=DIRECTION('center_axis',(-1.,0.,0.));
#16302=DIRECTION('ref_axis',(0.,1.,0.));
#16303=DIRECTION('',(-1.,0.,0.));
#16304=DIRECTION('center_axis',(-1.,0.,0.));
#16305=DIRECTION('ref_axis',(0.,1.,0.));
#16306=DIRECTION('center_axis',(1.,0.,0.));
#16307=DIRECTION('ref_axis',(0.,1.,0.));
#16308=DIRECTION('center_axis',(0.,0.,-1.));
#16309=DIRECTION('ref_axis',(-1.,0.,0.));
#16310=DIRECTION('center_axis',(0.,0.,-1.));
#16311=DIRECTION('ref_axis',(-1.,0.,0.));
#16312=DIRECTION('',(0.,0.,-1.));
#16313=DIRECTION('center_axis',(0.,0.,1.));
#16314=DIRECTION('ref_axis',(-1.,0.,0.));
#16315=DIRECTION('center_axis',(0.,0.,-1.));
#16316=DIRECTION('ref_axis',(-1.,0.,0.));
#16317=DIRECTION('center_axis',(0.,0.,-1.));
#16318=DIRECTION('ref_axis',(-1.,0.,0.));
#16319=DIRECTION('',(0.,0.,-1.));
#16320=DIRECTION('center_axis',(0.,0.,1.));
#16321=DIRECTION('ref_axis',(-1.,0.,0.));
#16322=DIRECTION('center_axis',(0.,0.,-1.));
#16323=DIRECTION('ref_axis',(-1.,0.,0.));
#16324=DIRECTION('center_axis',(0.,0.,-1.));
#16325=DIRECTION('ref_axis',(-1.,0.,0.));
#16326=DIRECTION('',(0.,0.,-1.));
#16327=DIRECTION('center_axis',(0.,0.,1.));
#16328=DIRECTION('ref_axis',(-1.,0.,0.));
#16329=DIRECTION('center_axis',(0.,0.,-1.));
#16330=DIRECTION('ref_axis',(-1.,0.,0.));
#16331=DIRECTION('center_axis',(0.,0.,-1.));
#16332=DIRECTION('ref_axis',(-1.,0.,0.));
#16333=DIRECTION('',(0.,0.,-1.));
#16334=DIRECTION('center_axis',(0.,0.,1.));
#16335=DIRECTION('ref_axis',(-1.,0.,0.));
#16336=DIRECTION('center_axis',(0.,0.,-1.));
#16337=DIRECTION('ref_axis',(-0.707106781186548,-0.707106781186548,0.));
#16338=DIRECTION('center_axis',(0.,0.,1.));
#16339=DIRECTION('ref_axis',(-0.707106781186548,-0.707106781186548,0.));
#16340=DIRECTION('',(0.,0.,1.));
#16341=DIRECTION('center_axis',(0.,0.,-1.));
#16342=DIRECTION('ref_axis',(-0.707106781186548,-0.707106781186548,0.));
#16343=DIRECTION('',(0.,0.,-1.));
#16344=DIRECTION('center_axis',(0.,0.,1.));
#16345=DIRECTION('ref_axis',(-1.,0.,0.));
#16346=DIRECTION('',(1.,0.,0.));
#16347=DIRECTION('center_axis',(0.,0.,-1.));
#16348=DIRECTION('ref_axis',(0.707106781186548,-0.707106781186548,0.));
#16349=DIRECTION('',(-1.11022302462516E-16,1.,0.));
#16350=DIRECTION('center_axis',(0.,0.,-1.));
#16351=DIRECTION('ref_axis',(0.707106781186548,0.707106781186548,0.));
#16352=DIRECTION('',(-1.,0.,0.));
#16353=DIRECTION('',(0.,-1.,0.));
#16354=DIRECTION('',(1.,0.,0.));
#16355=DIRECTION('',(0.,-1.,0.));
#16356=DIRECTION('',(-1.,0.,0.));
#16357=DIRECTION('center_axis',(0.,0.,-1.));
#16358=DIRECTION('ref_axis',(1.,0.,0.));
#16359=DIRECTION('center_axis',(0.,0.,-1.));
#16360=DIRECTION('ref_axis',(1.,0.,0.));
#16361=DIRECTION('',(-1.,0.,0.));
#16362=DIRECTION('',(0.,1.,0.));
#16363=DIRECTION('',(1.,0.,0.));
#16364=DIRECTION('',(0.,1.,0.));
#16365=DIRECTION('',(-1.,0.,0.));
#16366=DIRECTION('center_axis',(0.,0.,-1.));
#16367=DIRECTION('ref_axis',(-0.707106781186548,0.707106781186548,0.));
#16368=DIRECTION('',(1.11022302462516E-16,1.,0.));
#16369=DIRECTION('center_axis',(0.,-1.,0.));
#16370=DIRECTION('ref_axis',(-1.,0.,0.));
#16371=DIRECTION('',(-1.,0.,0.));
#16372=DIRECTION('',(0.,0.,-1.));
#16373=DIRECTION('center_axis',(0.,0.,-1.));
#16374=DIRECTION('ref_axis',(0.707106781186548,-0.707106781186548,0.));
#16375=DIRECTION('center_axis',(0.,0.,1.));
#16376=DIRECTION('ref_axis',(0.707106781186548,-0.707106781186548,0.));
#16377=DIRECTION('',(0.,0.,1.));
#16378=DIRECTION('center_axis',(0.,0.,-1.));
#16379=DIRECTION('ref_axis',(-0.707106781186548,0.707106781186548,0.));
#16380=DIRECTION('center_axis',(0.,0.,1.));
#16381=DIRECTION('ref_axis',(-0.707106781186548,0.707106781186548,0.));
#16382=DIRECTION('',(0.,0.,1.));
#16383=DIRECTION('',(0.,0.,-1.));
#16384=DIRECTION('center_axis',(0.,1.,0.));
#16385=DIRECTION('ref_axis',(1.,0.,0.));
#16386=DIRECTION('',(-1.,0.,0.));
#16387=DIRECTION('',(0.,0.,1.));
#16388=DIRECTION('',(1.,0.,0.));
#16389=DIRECTION('center_axis',(0.,0.,-1.));
#16390=DIRECTION('ref_axis',(0.707106781186548,0.707106781186548,0.));
#16391=DIRECTION('center_axis',(0.,0.,1.));
#16392=DIRECTION('ref_axis',(0.707106781186548,0.707106781186548,0.));
#16393=DIRECTION('',(0.,0.,-1.));
#16394=DIRECTION('center_axis',(1.,1.11022302462516E-16,0.));
#16395=DIRECTION('ref_axis',(1.11022302462516E-16,-1.,0.));
#16396=DIRECTION('',(1.11022302462516E-16,-1.,0.));
#16397=DIRECTION('center_axis',(1.,0.,0.));
#16398=DIRECTION('ref_axis',(0.,1.,0.));
#16399=DIRECTION('',(0.,0.342020143325669,-0.939692620785908));
#16400=DIRECTION('center_axis',(-1.,0.,0.));
#16401=DIRECTION('ref_axis',(0.,1.,0.));
#16402=DIRECTION('',(0.,0.447213595499958,-0.894427190999916));
#16403=DIRECTION('center_axis',(0.,0.894427190999916,0.447213595499958));
#16404=DIRECTION('ref_axis',(0.,-0.447213595499958,0.894427190999916));
#16405=DIRECTION('',(-1.,0.,0.));
#16406=DIRECTION('',(0.,-0.447213595499958,0.894427190999916));
#16407=DIRECTION('center_axis',(1.,0.,0.));
#16408=DIRECTION('ref_axis',(0.,1.,0.));
#16409=DIRECTION('center_axis',(1.,0.,0.));
#16410=DIRECTION('ref_axis',(0.,1.,0.));
#16411=DIRECTION('',(0.,-0.342020143325669,0.939692620785908));
#16412=DIRECTION('center_axis',(1.,0.,0.));
#16413=DIRECTION('ref_axis',(0.,-3.82856869892695E-16,1.));
#16414=DIRECTION('',(-1.,0.,0.));
#16415=DIRECTION('center_axis',(-1.,0.,0.));
#16416=DIRECTION('ref_axis',(0.,1.,0.));
#16417=DIRECTION('',(1.,0.,0.));
#16418=DIRECTION('',(1.,0.,0.));
#16419=DIRECTION('center_axis',(-1.,0.,0.));
#16420=DIRECTION('ref_axis',(0.,1.,0.));
#16421=DIRECTION('',(-1.,0.,0.));
#16422=DIRECTION('center_axis',(0.,0.939692620785908,0.342020143325669));
#16423=DIRECTION('ref_axis',(0.,-0.342020143325669,0.939692620785908));
#16424=DIRECTION('',(0.,0.342020143325669,-0.939692620785908));
#16425=DIRECTION('center_axis',(0.,-0.939692620785908,0.342020143325669));
#16426=DIRECTION('ref_axis',(0.,-0.342020143325669,-0.939692620785908));
#16427=DIRECTION('center_axis',(0.,0.939692620785908,-0.342020143325669));
#16428=DIRECTION('ref_axis',(0.,0.342020143325669,0.939692620785908));
#16429=DIRECTION('',(0.,-0.342020143325669,-0.939692620785908));
#16430=DIRECTION('center_axis',(0.,-0.939692620785908,0.342020143325669));
#16431=DIRECTION('ref_axis',(0.,-0.342020143325669,-0.939692620785908));
#16432=DIRECTION('',(0.,0.342020143325669,0.939692620785908));
#16433=DIRECTION('center_axis',(0.,0.939692620785908,-0.342020143325669));
#16434=DIRECTION('ref_axis',(0.,0.342020143325669,0.939692620785908));
#16435=DIRECTION('center_axis',(1.,0.,0.));
#16436=DIRECTION('ref_axis',(0.,1.,0.));
#16437=DIRECTION('center_axis',(1.,0.,0.));
#16438=DIRECTION('ref_axis',(0.,1.,0.));
#16439=DIRECTION('center_axis',(-1.,0.,0.));
#16440=DIRECTION('ref_axis',(0.,1.,0.));
#16441=DIRECTION('center_axis',(0.,0.939692620785908,0.342020143325669));
#16442=DIRECTION('ref_axis',(0.,-0.342020143325669,0.939692620785908));
#16443=DIRECTION('',(0.,-0.342020143325669,0.939692620785908));
#16444=DIRECTION('center_axis',(1.,0.,0.));
#16445=DIRECTION('ref_axis',(0.,1.,0.));
#16446=DIRECTION('center_axis',(-1.,0.,0.));
#16447=DIRECTION('ref_axis',(0.,-0.342020143325665,-0.93969262078591));
#16448=DIRECTION('center_axis',(1.,0.,0.));
#16449=DIRECTION('ref_axis',(0.,1.,0.));
#16450=DIRECTION('center_axis',(1.,0.,0.));
#16451=DIRECTION('ref_axis',(0.,1.,0.));
#16452=DIRECTION('center_axis',(1.,-1.11022302462516E-16,0.));
#16453=DIRECTION('ref_axis',(-1.11022302462516E-16,-1.,0.));
#16454=DIRECTION('',(-1.11022302462516E-16,-1.,0.));
#16455=DIRECTION('center_axis',(1.,0.,0.));
#16456=DIRECTION('ref_axis',(0.,1.,0.));
#16457=DIRECTION('',(1.,0.,0.));
#16458=DIRECTION('',(1.,0.,0.));
#16459=DIRECTION('center_axis',(1.,0.,0.));
#16460=DIRECTION('ref_axis',(0.,1.,0.));
#16461=DIRECTION('center_axis',(0.,0.,1.));
#16462=DIRECTION('ref_axis',(-1.,0.,0.));
#16463=DIRECTION('center_axis',(0.,0.,1.));
#16464=DIRECTION('ref_axis',(-1.,0.,0.));
#16465=DIRECTION('center_axis',(0.,0.,1.));
#16466=DIRECTION('ref_axis',(1.,0.,0.));
#16467=DIRECTION('',(0.,0.,1.));
#16468=DIRECTION('center_axis',(0.,0.,-1.));
#16469=DIRECTION('ref_axis',(1.,0.,0.));
#16470=DIRECTION('center_axis',(0.,0.,1.));
#16471=DIRECTION('ref_axis',(1.,0.,0.));
#16472=DIRECTION('center_axis',(0.,0.,-1.));
#16473=DIRECTION('ref_axis',(1.,0.,0.));
#16474=DIRECTION('center_axis',(0.,0.,1.));
#16475=DIRECTION('ref_axis',(1.,0.,0.));
#16476=DIRECTION('',(0.,0.,-1.));
#16477=DIRECTION('center_axis',(1.,0.,0.));
#16478=DIRECTION('ref_axis',(0.,1.,0.));
#16479=DIRECTION('center_axis',(0.,0.,-1.));
#16480=DIRECTION('ref_axis',(-1.,0.,0.));
#16481=DIRECTION('axis',(0.,0.,1.));
#16482=DIRECTION('refdir',(1.,0.,0.));
#16483=DIRECTION('center_axis',(-1.,0.,0.));
#16484=DIRECTION('ref_axis',(0.,1.,0.));
#16485=DIRECTION('center_axis',(1.,0.,0.));
#16486=DIRECTION('ref_axis',(0.,1.,0.));
#16487=DIRECTION('',(-1.,0.,0.));
#16488=DIRECTION('center_axis',(-1.,0.,0.));
#16489=DIRECTION('ref_axis',(0.,1.,0.));
#16490=DIRECTION('center_axis',(-1.,0.,0.));
#16491=DIRECTION('ref_axis',(0.,1.,0.));
#16492=DIRECTION('center_axis',(1.,0.,0.));
#16493=DIRECTION('ref_axis',(0.,1.,0.));
#16494=DIRECTION('',(-1.,0.,0.));
#16495=DIRECTION('center_axis',(-1.,0.,0.));
#16496=DIRECTION('ref_axis',(0.,1.,0.));
#16497=DIRECTION('center_axis',(-1.,0.,0.));
#16498=DIRECTION('ref_axis',(0.,1.,0.));
#16499=DIRECTION('center_axis',(1.,0.,0.));
#16500=DIRECTION('ref_axis',(0.,1.,0.));
#16501=DIRECTION('',(-1.,0.,0.));
#16502=DIRECTION('center_axis',(-1.,0.,0.));
#16503=DIRECTION('ref_axis',(0.,1.,0.));
#16504=DIRECTION('center_axis',(-1.,0.,0.));
#16505=DIRECTION('ref_axis',(0.,0.,-1.));
#16506=DIRECTION('center_axis',(-1.,0.,0.));
#16507=DIRECTION('ref_axis',(0.,0.342020143325669,0.939692620785908));
#16508=DIRECTION('center_axis',(0.,1.,0.));
#16509=DIRECTION('ref_axis',(0.,0.,1.));
#16510=DIRECTION('center_axis',(1.,0.,0.));
#16511=DIRECTION('ref_axis',(0.,0.342020143325669,0.939692620785908));
#16512=DIRECTION('center_axis',(1.,0.,0.));
#16513=DIRECTION('ref_axis',(0.,0.342020143325669,0.939692620785908));
#16514=DIRECTION('center_axis',(1.,0.,0.));
#16515=DIRECTION('ref_axis',(0.,-0.296296296296299,-0.955096070979823));
#16516=DIRECTION('center_axis',(1.,0.,0.));
#16517=DIRECTION('ref_axis',(0.,-0.296296296296299,-0.955096070979823));
#16518=DIRECTION('',(-1.,0.,0.));
#16519=DIRECTION('center_axis',(1.,0.,0.));
#16520=DIRECTION('ref_axis',(0.,1.,0.));
#16521=DIRECTION('center_axis',(-1.,0.,0.));
#16522=DIRECTION('ref_axis',(0.,1.,0.));
#16523=DIRECTION('center_axis',(1.,0.,0.));
#16524=DIRECTION('ref_axis',(0.,1.,0.));
#16525=DIRECTION('',(1.,0.,0.));
#16526=DIRECTION('center_axis',(-1.,0.,0.));
#16527=DIRECTION('ref_axis',(0.,1.,0.));
#16528=DIRECTION('center_axis',(1.,0.,0.));
#16529=DIRECTION('ref_axis',(0.,1.,0.));
#16530=DIRECTION('axis',(0.,0.,1.));
#16531=DIRECTION('refdir',(1.,0.,0.));
#16532=DIRECTION('center_axis',(0.,-1.83697019872103E-16,1.));
#16533=DIRECTION('ref_axis',(0.,-1.,-1.83697019872103E-16));
#16534=DIRECTION('center_axis',(0.,-1.83697019872103E-16,1.));
#16535=DIRECTION('ref_axis',(0.,-1.,-1.83697019872103E-16));
#16536=DIRECTION('center_axis',(1.,1.22464679914735E-16,2.24963967399279E-32));
#16537=DIRECTION('ref_axis',(-1.22464679914735E-16,1.,1.83697019872103E-16));
#16538=DIRECTION('center_axis',(0.,-1.83697019872103E-16,1.));
#16539=DIRECTION('ref_axis',(0.,-1.,-1.83697019872103E-16));
#16540=DIRECTION('center_axis',(0.,1.83697019872103E-16,-1.));
#16541=DIRECTION('ref_axis',(0.,1.,1.83697019872103E-16));
#16542=DIRECTION('center_axis',(0.,-1.83697019872103E-16,1.));
#16543=DIRECTION('ref_axis',(0.,-1.,-1.83697019872103E-16));
#16544=DIRECTION('',(-3.16961915143177E-17,-0.258819045102521,-0.965925826289068));
#16545=DIRECTION('center_axis',(0.,-1.83697019872103E-16,1.));
#16546=DIRECTION('ref_axis',(0.,-1.,-1.83697019872103E-16));
#16547=DIRECTION('center_axis',(0.,-1.83697019872103E-16,1.));
#16548=DIRECTION('ref_axis',(0.,-1.,-1.83697019872103E-16));
#16549=DIRECTION('center_axis',(0.,-1.83697019872103E-16,1.));
#16550=DIRECTION('ref_axis',(0.,-1.,-1.83697019872103E-16));
#16551=DIRECTION('center_axis',(0.,-1.83697019872103E-16,1.));
#16552=DIRECTION('ref_axis',(0.,-1.,-1.83697019872103E-16));
#16553=DIRECTION('',(0.,-1.83697019872103E-16,1.));
#16554=DIRECTION('center_axis',(0.,-1.83697019872103E-16,1.));
#16555=DIRECTION('ref_axis',(0.,-1.,-1.83697019872103E-16));
#16556=DIRECTION('center_axis',(0.,-1.83697019872103E-16,1.));
#16557=DIRECTION('ref_axis',(0.,-1.,-1.83697019872103E-16));
#16558=DIRECTION('',(-3.16961915143176E-17,0.25881904510252,0.965925826289068));
#16559=DIRECTION('center_axis',(0.,-1.83697019872103E-16,1.));
#16560=DIRECTION('ref_axis',(0.,-1.,-1.83697019872103E-16));
#16561=DIRECTION('center_axis',(0.,-1.83697019872103E-16,1.));
#16562=DIRECTION('ref_axis',(0.,-1.,-1.68690289661508E-16));
#16563=DIRECTION('center_axis',(-1.,-1.22464679914735E-16,-2.24963967399279E-32));
#16564=DIRECTION('ref_axis',(-1.22464679914735E-16,1.,2.10862862076885E-16));
#16565=DIRECTION('center_axis',(0.,-1.83697019872103E-16,1.));
#16566=DIRECTION('ref_axis',(0.,-1.,-1.83697019872103E-16));
#16567=DIRECTION('center_axis',(0.,-1.83697019872103E-16,1.));
#16568=DIRECTION('ref_axis',(0.,-1.,-1.42298278189606E-16));
#16569=DIRECTION('center_axis',(0.,-1.83697019872103E-16,1.));
#16570=DIRECTION('ref_axis',(0.,-1.,-1.83697019872103E-16));
#16571=DIRECTION('center_axis',(-1.,-1.22464679914735E-16,-2.24963967399279E-32));
#16572=DIRECTION('ref_axis',(-1.22464679914735E-16,1.,1.77872847737008E-16));
#16573=DIRECTION('center_axis',(0.,-1.83697019872103E-16,1.));
#16574=DIRECTION('ref_axis',(0.,-1.,-1.83697019872103E-16));
#16575=DIRECTION('center_axis',(0.,-1.83697019872103E-16,1.));
#16576=DIRECTION('ref_axis',(0.,-1.,-1.83697019872103E-16));
#16577=DIRECTION('',(0.,1.83697019872103E-16,-1.));
#16578=DIRECTION('center_axis',(0.,-1.83697019872103E-16,1.));
#16579=DIRECTION('ref_axis',(0.,-1.,-1.83697019872103E-16));
#16580=DIRECTION('',(0.,1.83697019872103E-16,-1.));
#16581=DIRECTION('center_axis',(0.,-1.83697019872103E-16,1.));
#16582=DIRECTION('ref_axis',(0.,-1.,-1.83697019872103E-16));
#16583=DIRECTION('center_axis',(0.,-1.83697019872103E-16,1.));
#16584=DIRECTION('ref_axis',(0.,-1.,-1.42298278189606E-16));
#16585=DIRECTION('center_axis',(-1.,-1.22464679914735E-16,-2.24963967399279E-32));
#16586=DIRECTION('ref_axis',(-1.22464679914735E-16,1.,1.77872847737008E-16));
#16587=DIRECTION('center_axis',(0.,-1.83697019872103E-16,1.));
#16588=DIRECTION('ref_axis',(0.,-1.,-1.83697019872103E-16));
#16589=DIRECTION('center_axis',(0.,-1.83697019872103E-16,1.));
#16590=DIRECTION('ref_axis',(0.,-1.,-1.68690289661508E-16));
#16591=DIRECTION('center_axis',(0.,-1.83697019872103E-16,1.));
#16592=DIRECTION('ref_axis',(0.,-1.,-1.83697019872103E-16));
#16593=DIRECTION('center_axis',(-1.,-1.22464679914735E-16,-2.24963967399279E-32));
#16594=DIRECTION('ref_axis',(-1.22464679914735E-16,1.,2.10862862076885E-16));
#16595=DIRECTION('center_axis',(0.,-1.83697019872103E-16,1.));
#16596=DIRECTION('ref_axis',(0.,-1.,-1.83697019872103E-16));
#16597=DIRECTION('center_axis',(0.,1.83697019872103E-16,-1.));
#16598=DIRECTION('ref_axis',(0.,1.,1.83697019872103E-16));
#16599=DIRECTION('center_axis',(-1.,0.,0.));
#16600=DIRECTION('ref_axis',(0.,1.,0.));
#16601=DIRECTION('center_axis',(0.,1.22464679914735E-16,1.));
#16602=DIRECTION('ref_axis',(0.,-1.,1.22464679914735E-16));
#16603=DIRECTION('center_axis',(0.,-1.83697019872103E-16,1.));
#16604=DIRECTION('ref_axis',(0.,-1.,-1.83697019872103E-16));
#16605=DIRECTION('center_axis',(0.,-1.83697019872103E-16,1.));
#16606=DIRECTION('ref_axis',(0.,-1.,-1.83697019872103E-16));
#16607=DIRECTION('',(0.,-1.83697019872103E-16,1.));
#16608=DIRECTION('center_axis',(0.,-1.83697019872103E-16,1.));
#16609=DIRECTION('ref_axis',(0.,-1.,-1.83697019872103E-16));
#16610=DIRECTION('center_axis',(0.,-1.83697019872103E-16,1.));
#16611=DIRECTION('ref_axis',(0.,-1.,-2.03409989752688E-16));
#16612=DIRECTION('center_axis',(-1.,-1.22464679914735E-16,-2.24963967399279E-32));
#16613=DIRECTION('ref_axis',(-1.22464679914735E-16,1.,1.69508324793907E-16));
#16614=DIRECTION('center_axis',(0.,-1.83697019872103E-16,1.));
#16615=DIRECTION('ref_axis',(0.,-1.,-1.83697019872103E-16));
#16616=DIRECTION('center_axis',(0.,1.83697019872103E-16,-1.));
#16617=DIRECTION('ref_axis',(0.,1.,1.83697019872103E-16));
#16618=DIRECTION('center_axis',(0.,-1.83697019872103E-16,1.));
#16619=DIRECTION('ref_axis',(0.,-1.,-1.83697019872103E-16));
#16620=DIRECTION('',(6.12323399573677E-17,0.5,0.866025403784439));
#16621=DIRECTION('center_axis',(0.,-1.83697019872103E-16,1.));
#16622=DIRECTION('ref_axis',(0.,-1.,-1.83697019872103E-16));
#16623=DIRECTION('center_axis',(0.,-1.83697019872103E-16,1.));
#16624=DIRECTION('ref_axis',(0.,-1.,-1.83697019872103E-16));
#16625=DIRECTION('center_axis',(0.,-1.83697019872103E-16,1.));
#16626=DIRECTION('ref_axis',(0.,-1.,-1.83697019872103E-16));
#16627=DIRECTION('',(0.,1.83697019872103E-16,-1.));
#16628=DIRECTION('center_axis',(0.,-1.83697019872103E-16,1.));
#16629=DIRECTION('ref_axis',(0.,-1.,-1.83697019872103E-16));
#16630=DIRECTION('center_axis',(0.,-1.83697019872103E-16,1.));
#16631=DIRECTION('ref_axis',(0.,-1.,-1.83697019872103E-16));
#16632=DIRECTION('center_axis',(0.,1.83697019872103E-16,-1.));
#16633=DIRECTION('ref_axis',(0.,1.,1.83697019872103E-16));
#16634=DIRECTION('center_axis',(0.,-1.83697019872103E-16,1.));
#16635=DIRECTION('ref_axis',(0.,-1.,-1.83697019872103E-16));
#16636=DIRECTION('center_axis',(0.,-1.83697019872103E-16,1.));
#16637=DIRECTION('ref_axis',(0.,-1.,-1.83697019872103E-16));
#16638=DIRECTION('',(0.,1.83697019872103E-16,-1.));
#16639=DIRECTION('center_axis',(0.,-1.83697019872103E-16,1.));
#16640=DIRECTION('ref_axis',(0.,-1.,-1.83697019872103E-16));
#16641=DIRECTION('center_axis',(0.,-1.83697019872103E-16,1.));
#16642=DIRECTION('ref_axis',(0.,-1.,-1.83697019872103E-16));
#16643=DIRECTION('center_axis',(0.,-1.83697019872103E-16,1.));
#16644=DIRECTION('ref_axis',(0.,-1.,-1.83697019872103E-16));
#16645=DIRECTION('',(0.,-1.83697019872103E-16,1.));
#16646=DIRECTION('center_axis',(0.,-1.83697019872103E-16,1.));
#16647=DIRECTION('ref_axis',(0.,-1.,-1.83697019872103E-16));
#16648=DIRECTION('center_axis',(0.,-1.83697019872103E-16,1.));
#16649=DIRECTION('ref_axis',(0.,-1.,-2.03409989752688E-16));
#16650=DIRECTION('center_axis',(0.,-1.83697019872103E-16,1.));
#16651=DIRECTION('ref_axis',(0.,-1.,-1.83697019872103E-16));
#16652=DIRECTION('center_axis',(-1.,-1.22464679914735E-16,-2.24963967399279E-32));
#16653=DIRECTION('ref_axis',(-1.22464679914735E-16,1.,1.69508324793907E-16));
#16654=DIRECTION('center_axis',(0.,-1.83697019872103E-16,1.));
#16655=DIRECTION('ref_axis',(0.,-1.,-1.83697019872103E-16));
#16656=DIRECTION('',(6.12323399573675E-17,-0.499999999999998,-0.86602540378444));
#16657=DIRECTION('center_axis',(0.,-1.83697019872103E-16,1.));
#16658=DIRECTION('ref_axis',(0.,-1.,-1.83697019872103E-16));
#16659=DIRECTION('center_axis',(0.,-1.83697019872103E-16,1.));
#16660=DIRECTION('ref_axis',(0.,-1.,-1.83697019872103E-16));
#16661=DIRECTION('center_axis',(0.,1.83697019872103E-16,-1.));
#16662=DIRECTION('ref_axis',(0.,1.,1.83697019872103E-16));
#16663=DIRECTION('center_axis',(0.,-1.83697019872103E-16,1.));
#16664=DIRECTION('ref_axis',(0.,-1.,-1.83697019872103E-16));
#16665=DIRECTION('center_axis',(0.,-1.83697019872103E-16,1.));
#16666=DIRECTION('ref_axis',(0.,-1.,-1.83697019872103E-16));
#16667=DIRECTION('',(-4.18853873767693E-17,0.342020143325664,0.93969262078591));
#16668=DIRECTION('center_axis',(0.,-1.83697019872103E-16,1.));
#16669=DIRECTION('ref_axis',(0.,-1.,-1.83697019872103E-16));
#16670=DIRECTION('center_axis',(0.,-1.83697019872103E-16,1.));
#16671=DIRECTION('ref_axis',(0.,-1.,-1.83697019872103E-16));
#16672=DIRECTION('',(-8.65956056235486E-17,0.707106781186541,0.707106781186554));
#16673=DIRECTION('center_axis',(0.,-1.83697019872103E-16,1.));
#16674=DIRECTION('ref_axis',(0.,-1.,-1.83697019872103E-16));
#16675=DIRECTION('center_axis',(0.,1.83697019872103E-16,-1.));
#16676=DIRECTION('ref_axis',(0.,1.,1.83697019872103E-16));
#16677=DIRECTION('center_axis',(0.,-1.83697019872103E-16,1.));
#16678=DIRECTION('ref_axis',(0.,-1.,-1.83697019872103E-16));
#16679=DIRECTION('',(6.12323399573668E-17,0.499999999999993,0.866025403784443));
#16680=DIRECTION('center_axis',(0.,-1.83697019872103E-16,1.));
#16681=DIRECTION('ref_axis',(0.,-1.,-1.83697019872103E-16));
#16682=DIRECTION('center_axis',(0.,-1.83697019872103E-16,1.));
#16683=DIRECTION('ref_axis',(0.,-1.,-1.83697019872103E-16));
#16684=DIRECTION('center_axis',(0.,-1.83697019872103E-16,1.));
#16685=DIRECTION('ref_axis',(0.,-1.,-1.83697019872103E-16));
#16686=DIRECTION('',(0.,1.83697019872103E-16,-1.));
#16687=DIRECTION('center_axis',(0.,-1.83697019872103E-16,1.));
#16688=DIRECTION('ref_axis',(0.,-1.,-1.83697019872103E-16));
#16689=DIRECTION('center_axis',(0.,-1.83697019872103E-16,1.));
#16690=DIRECTION('ref_axis',(0.,-1.,-1.83697019872103E-16));
#16691=DIRECTION('',(6.12323399573667E-17,-0.499999999999992,-0.866025403784443));
#16692=DIRECTION('center_axis',(0.,-1.83697019872103E-16,1.));
#16693=DIRECTION('ref_axis',(0.,-1.,-1.83697019872103E-16));
#16694=DIRECTION('center_axis',(0.,1.83697019872103E-16,-1.));
#16695=DIRECTION('ref_axis',(0.,1.,1.83697019872103E-16));
#16696=DIRECTION('center_axis',(0.,-1.83697019872103E-16,1.));
#16697=DIRECTION('ref_axis',(0.,-1.,-1.83697019872103E-16));
#16698=DIRECTION('',(-8.65956056235486E-17,-0.707106781186542,-0.707106781186554));
#16699=DIRECTION('center_axis',(0.,-1.83697019872103E-16,1.));
#16700=DIRECTION('ref_axis',(0.,-1.,-1.83697019872103E-16));
#16701=DIRECTION('center_axis',(0.,1.83697019872103E-16,-1.));
#16702=DIRECTION('ref_axis',(0.,1.,1.83697019872103E-16));
#16703=DIRECTION('center_axis',(0.,-1.83697019872103E-16,1.));
#16704=DIRECTION('ref_axis',(0.,-1.,-1.83697019872103E-16));
#16705=DIRECTION('',(-4.18853873767694E-17,-0.342020143325664,-0.93969262078591));
#16706=DIRECTION('center_axis',(0.,-1.83697019872103E-16,1.));
#16707=DIRECTION('ref_axis',(0.,-1.,-1.83697019872103E-16));
#16708=DIRECTION('center_axis',(0.,-1.83697019872103E-16,1.));
#16709=DIRECTION('ref_axis',(0.,-1.,-1.83697019872103E-16));
#16710=DIRECTION('',(0.,-1.83697019872103E-16,1.));
#16711=DIRECTION('center_axis',(0.,-1.83697019872103E-16,1.));
#16712=DIRECTION('ref_axis',(0.,-1.,-1.83697019872103E-16));
#16713=DIRECTION('center_axis',(0.,-1.83697019872103E-16,1.));
#16714=DIRECTION('ref_axis',(0.,-1.,-1.83697019872103E-16));
#16715=DIRECTION('center_axis',(1.,1.22464679914735E-16,2.24963967399279E-32));
#16716=DIRECTION('ref_axis',(-1.22464679914735E-16,1.,1.83697019872103E-16));
#16717=DIRECTION('center_axis',(0.,-1.83697019872103E-16,1.));
#16718=DIRECTION('ref_axis',(0.,-1.,-1.83697019872103E-16));
#16719=DIRECTION('center_axis',(0.,-1.83697019872103E-16,1.));
#16720=DIRECTION('ref_axis',(0.,-1.,-1.83697019872103E-16));
#16721=DIRECTION('',(0.,-1.83697019872103E-16,1.));
#16722=DIRECTION('center_axis',(0.,-1.83697019872103E-16,1.));
#16723=DIRECTION('ref_axis',(0.,-1.,-1.83697019872103E-16));
#16724=DIRECTION('center_axis',(0.,1.83697019872103E-16,-1.));
#16725=DIRECTION('ref_axis',(0.,1.,1.83697019872103E-16));
#16726=DIRECTION('center_axis',(-0.766044443118977,0.642787609686541,1.1807816831013E-16));
#16727=DIRECTION('ref_axis',(0.642787609686541,0.766044443118977,-4.29769385815623E-17));
#16728=DIRECTION('center_axis',(1.9679694718355E-16,5.0836448945465E-17,
1.));
#16729=DIRECTION('ref_axis',(-0.642787609686541,-0.766044443118977,1.65441618496298E-16));
#16730=DIRECTION('center_axis',(-0.173648177666927,0.984807753012209,1.80906249375285E-16));
#16731=DIRECTION('ref_axis',(0.984807753012209,0.173648177666927,-1.51798367128467E-16));
#16732=DIRECTION('center_axis',(3.01510415625474E-16,-1.3053259863271E-16,
1.));
#16733=DIRECTION('ref_axis',(-0.984807753012209,-0.173648177666927,2.74263047043202E-16));
#16734=DIRECTION('center_axis',(0.500000000000004,0.866025403784436,1.59086285808736E-16));
#16735=DIRECTION('ref_axis',(0.866025403784436,-0.500000000000004,-2.75545529808155E-16));
#16736=DIRECTION('center_axis',(2.65143809681226E-16,-3.36777869765524E-16,
1.));
#16737=DIRECTION('ref_axis',(-0.866025403784436,0.500000000000004,3.9801020972289E-16));
#16738=DIRECTION('center_axis',(0.939692620785911,0.342020143325663,6.28280810651538E-17));
#16739=DIRECTION('ref_axis',(0.342020143325663,-0.939692620785911,-3.56315753906281E-16));
#16740=DIRECTION('center_axis',(1.04713468441923E-16,-4.71394909929066E-16,
1.));
#16741=DIRECTION('ref_axis',(-0.342020143325663,0.939692620785911,4.78780433821016E-16));
#16742=DIRECTION('center_axis',(0.939692620785906,-0.342020143325676,-6.28280810651561E-17));
#16743=DIRECTION('ref_axis',(-0.342020143325676,-0.939692620785906,-3.5631575390628E-16));
#16744=DIRECTION('center_axis',(-1.04713468441927E-16,-4.71394909929065E-16,
1.));
#16745=DIRECTION('ref_axis',(0.342020143325676,0.939692620785906,4.78780433821015E-16));
#16746=DIRECTION('center_axis',(0.499999999999992,-0.866025403784443,-1.59086285808737E-16));
#16747=DIRECTION('ref_axis',(-0.866025403784443,-0.499999999999992,-2.75545529808153E-16));
#16748=DIRECTION('center_axis',(-2.65143809681228E-16,-3.3677786976552E-16,
1.));
#16749=DIRECTION('ref_axis',(0.866025403784443,0.499999999999992,3.98010209722888E-16));
#16750=DIRECTION('center_axis',(-0.173648177666941,-0.984807753012206,-1.80906249375284E-16));
#16751=DIRECTION('ref_axis',(-0.984807753012206,0.173648177666941,-1.51798367128465E-16));
#16752=DIRECTION('center_axis',(-3.01510415625474E-16,-1.30532598632705E-16,
1.));
#16753=DIRECTION('ref_axis',(0.984807753012206,-0.173648177666941,2.742630470432E-16));
#16754=DIRECTION('center_axis',(-0.766044443118986,-0.64278760968653,-1.18078168310128E-16));
#16755=DIRECTION('ref_axis',(-0.64278760968653,0.766044443118986,-4.29769385815605E-17));
#16756=DIRECTION('center_axis',(-1.96796947183547E-16,5.08364489454677E-17,
1.));
#16757=DIRECTION('ref_axis',(0.64278760968653,-0.766044443118986,1.65441618496296E-16));
#16758=DIRECTION('center_axis',(0.,-1.83697019872103E-16,1.));
#16759=DIRECTION('ref_axis',(0.,-1.,-1.83697019872103E-16));
#16760=DIRECTION('center_axis',(0.,-1.83697019872103E-16,1.));
#16761=DIRECTION('ref_axis',(0.,-1.,-1.83697019872103E-16));
#16762=DIRECTION('',(0.,-1.83697019872103E-16,1.));
#16763=DIRECTION('center_axis',(0.,-1.83697019872103E-16,1.));
#16764=DIRECTION('ref_axis',(0.,-1.,-1.83697019872103E-16));
#16765=DIRECTION('center_axis',(0.,-1.83697019872103E-16,1.));
#16766=DIRECTION('ref_axis',(0.,-1.,-2.0795020232313E-16));
#16767=DIRECTION('center_axis',(-1.,-1.22464679914735E-16,-2.24963967399279E-32));
#16768=DIRECTION('ref_axis',(-1.22464679914735E-16,1.,1.73291835269275E-16));
#16769=DIRECTION('center_axis',(0.,-1.83697019872103E-16,1.));
#16770=DIRECTION('ref_axis',(0.,-1.,-1.83697019872103E-16));
#16771=DIRECTION('center_axis',(0.,-1.83697019872103E-16,1.));
#16772=DIRECTION('ref_axis',(0.,-1.,-1.83697019872103E-16));
#16773=DIRECTION('',(0.,1.83697019872103E-16,-1.));
#16774=DIRECTION('center_axis',(0.,-1.83697019872103E-16,1.));
#16775=DIRECTION('ref_axis',(0.,-1.,-1.83697019872103E-16));
#16776=DIRECTION('center_axis',(0.,-1.83697019872103E-16,1.));
#16777=DIRECTION('ref_axis',(0.,-1.,-2.06474247751558E-16));
#16778=DIRECTION('center_axis',(-1.,-1.22464679914735E-16,-2.24963967399279E-32));
#16779=DIRECTION('ref_axis',(-1.22464679914735E-16,1.,1.72061873126299E-16));
#16780=DIRECTION('center_axis',(0.,-1.83697019872103E-16,1.));
#16781=DIRECTION('ref_axis',(0.,-1.,-1.83697019872103E-16));
#16782=DIRECTION('center_axis',(0.,-1.83697019872103E-16,1.));
#16783=DIRECTION('ref_axis',(0.,-1.,-1.83697019872103E-16));
#16784=DIRECTION('center_axis',(0.,1.83697019872103E-16,-1.));
#16785=DIRECTION('ref_axis',(0.,1.,1.83697019872103E-16));
#16786=DIRECTION('center_axis',(0.,-1.83697019872103E-16,1.));
#16787=DIRECTION('ref_axis',(0.,-1.,-1.83697019872103E-16));
#16788=DIRECTION('',(2.12657684957562E-17,0.173648177666917,0.98480775301221));
#16789=DIRECTION('center_axis',(0.,-1.83697019872103E-16,1.));
#16790=DIRECTION('ref_axis',(0.,-1.,-1.83697019872103E-16));
#16791=DIRECTION('center_axis',(0.,-1.83697019872103E-16,1.));
#16792=DIRECTION('ref_axis',(0.,-1.,-1.83697019872103E-16));
#16793=DIRECTION('',(0.,1.83697019872103E-16,-1.));
#16794=DIRECTION('center_axis',(0.,-1.83697019872103E-16,1.));
#16795=DIRECTION('ref_axis',(0.,-1.,-1.83697019872103E-16));
#16796=DIRECTION('center_axis',(0.,-1.83697019872103E-16,1.));
#16797=DIRECTION('ref_axis',(0.,-1.,-1.83697019872103E-16));
#16798=DIRECTION('axis',(0.,0.,1.));
#16799=DIRECTION('refdir',(1.,0.,0.));
#16800=DIRECTION('center_axis',(0.,0.,-1.));
#16801=DIRECTION('ref_axis',(-1.,0.,0.));
#16802=DIRECTION('center_axis',(0.,0.,-1.));
#16803=DIRECTION('ref_axis',(-1.,0.,0.));
#16804=DIRECTION('center_axis',(0.,0.,-1.));
#16805=DIRECTION('ref_axis',(-1.,0.,0.));
#16806=DIRECTION('center_axis',(-1.22464679914735E-16,-1.,0.));
#16807=DIRECTION('ref_axis',(1.,-1.22464679914735E-16,0.));
#16808=DIRECTION('center_axis',(0.,0.,1.));
#16809=DIRECTION('ref_axis',(-1.,0.,0.));
#16810=DIRECTION('center_axis',(0.,0.,1.));
#16811=DIRECTION('ref_axis',(1.,0.,0.));
#16812=DIRECTION('center_axis',(0.,0.,1.));
#16813=DIRECTION('ref_axis',(1.,0.,0.));
#16814=DIRECTION('center_axis',(1.22464679914735E-16,-1.,0.));
#16815=DIRECTION('ref_axis',(-1.,-1.22464679914735E-16,0.));
#16816=DIRECTION('center_axis',(0.,0.,-1.));
#16817=DIRECTION('ref_axis',(1.,0.,0.));
#16818=DIRECTION('center_axis',(0.,0.,-1.));
#16819=DIRECTION('ref_axis',(-1.,0.,0.));
#16820=DIRECTION('center_axis',(0.,0.,1.));
#16821=DIRECTION('ref_axis',(1.,0.,0.));
#16822=DIRECTION('',(0.246660747381231,-3.02072294755719E-17,-0.96910189128973));
#16823=DIRECTION('center_axis',(0.,0.,1.));
#16824=DIRECTION('ref_axis',(1.,0.,0.));
#16825=DIRECTION('center_axis',(0.,0.,1.));
#16826=DIRECTION('ref_axis',(1.,0.,0.));
#16827=DIRECTION('',(0.,0.,-1.));
#16828=DIRECTION('center_axis',(0.,0.,-1.));
#16829=DIRECTION('ref_axis',(-1.,0.,0.));
#16830=DIRECTION('center_axis',(0.,0.,1.));
#16831=DIRECTION('ref_axis',(1.,0.,0.));
#16832=DIRECTION('center_axis',(0.,0.,1.));
#16833=DIRECTION('ref_axis',(1.,0.,0.));
#16834=DIRECTION('center_axis',(0.,0.,1.));
#16835=DIRECTION('ref_axis',(1.,0.,0.));
#16836=DIRECTION('center_axis',(0.,0.,1.));
#16837=DIRECTION('ref_axis',(1.,0.,0.));
#16838=DIRECTION('',(0.969101891289732,1.18680752921562E-16,-0.246660747381225));
#16839=DIRECTION('center_axis',(0.,0.,1.));
#16840=DIRECTION('ref_axis',(1.,0.,0.));
#16841=DIRECTION('center_axis',(0.,0.,1.));
#16842=DIRECTION('ref_axis',(1.,0.,0.));
#16843=DIRECTION('center_axis',(0.,0.,1.));
#16844=DIRECTION('ref_axis',(1.,0.,0.));
#16845=DIRECTION('center_axis',(0.,0.,1.));
#16846=DIRECTION('ref_axis',(1.,0.,0.));
#16847=DIRECTION('center_axis',(0.,0.,1.));
#16848=DIRECTION('ref_axis',(1.,0.,0.));
#16849=DIRECTION('',(0.96910189128973,1.18680752921561E-16,-0.246660747381235));
#16850=DIRECTION('center_axis',(0.,0.,1.));
#16851=DIRECTION('ref_axis',(1.,0.,0.));
#16852=DIRECTION('center_axis',(0.,0.,1.));
#16853=DIRECTION('ref_axis',(1.,0.,0.));
#16854=DIRECTION('center_axis',(0.,0.,1.));
#16855=DIRECTION('ref_axis',(1.,0.,0.));
#16856=DIRECTION('center_axis',(0.,0.,1.));
#16857=DIRECTION('ref_axis',(1.,0.,0.));
#16858=DIRECTION('center_axis',(1.22464679914735E-16,-1.,0.));
#16859=DIRECTION('ref_axis',(-1.,-1.22464679914735E-16,0.));
#16860=DIRECTION('center_axis',(0.,0.,1.));
#16861=DIRECTION('ref_axis',(1.,0.,0.));
#16862=DIRECTION('center_axis',(0.,0.,1.));
#16863=DIRECTION('ref_axis',(1.,0.,0.));
#16864=DIRECTION('center_axis',(0.,0.,1.));
#16865=DIRECTION('ref_axis',(1.,0.,0.));
#16866=DIRECTION('center_axis',(0.,0.,1.));
#16867=DIRECTION('ref_axis',(1.,0.,0.));
#16868=DIRECTION('center_axis',(0.,0.,1.));
#16869=DIRECTION('ref_axis',(1.,0.,0.));
#16870=DIRECTION('',(-0.969101891289729,-1.18680752921561E-16,0.246660747381235));
#16871=DIRECTION('center_axis',(0.,0.,-1.));
#16872=DIRECTION('ref_axis',(-1.,0.,0.));
#16873=DIRECTION('',(0.246660747381231,-3.02072294755719E-17,-0.96910189128973));
#16874=DIRECTION('center_axis',(0.,0.,-1.));
#16875=DIRECTION('ref_axis',(-1.,0.,0.));
#16876=DIRECTION('',(0.246660747381232,-3.0207229475572E-17,-0.96910189128973));
#16877=DIRECTION('center_axis',(0.24415009662832,-0.0351034843719286,-0.96910189128973));
#16878=DIRECTION('ref_axis',(0.959237831365939,-0.137917578929237,0.246660747381233));
#16879=DIRECTION('center_axis',(0.24415009662832,-0.0351034843719286,-0.96910189128973));
#16880=DIRECTION('ref_axis',(0.959237831365939,-0.137917578929239,0.246660747381233));
#16881=DIRECTION('',(0.246660747381232,-3.0207229475572E-17,-0.96910189128973));
#16882=DIRECTION('center_axis',(0.24415009662832,-0.0351034843719286,-0.96910189128973));
#16883=DIRECTION('ref_axis',(0.959237831365939,-0.137917578929239,0.246660747381233));
#16884=DIRECTION('center_axis',(0.24415009662832,-0.0351034843719286,-0.96910189128973));
#16885=DIRECTION('ref_axis',(0.959237831365939,-0.137917578929237,0.246660747381233));
#16886=DIRECTION('center_axis',(0.24415009662832,0.0351034843719251,0.96910189128973));
#16887=DIRECTION('ref_axis',(0.95923783136594,0.137917578929228,-0.246660747381232));
#16888=DIRECTION('center_axis',(0.24415009662832,0.0351034843719251,0.96910189128973));
#16889=DIRECTION('ref_axis',(0.95923783136594,0.137917578929228,-0.246660747381232));
#16890=DIRECTION('center_axis',(0.224370507816025,0.102466577580428,-0.969101891289731));
#16891=DIRECTION('ref_axis',(0.881526087075181,0.402579474771446,0.24666074738123));
#16892=DIRECTION('center_axis',(0.224370507816032,0.102466577580431,-0.969101891289729));
#16893=DIRECTION('ref_axis',(0.88152608707551,0.402579474770722,0.246660747381237));
#16894=DIRECTION('center_axis',(-0.224370507816021,0.10246657758043,-0.969101891289732));
#16895=DIRECTION('ref_axis',(0.881526087075442,-0.402579474770876,-0.246660747381227));
#16896=DIRECTION('center_axis',(-0.224370507816028,0.102466577580433,-0.96910189128973));
#16897=DIRECTION('ref_axis',(0.881526087075883,-0.402579474769905,-0.246660747381234));
#16898=DIRECTION('center_axis',(0.,0.246660747381227,-0.969101891289732));
#16899=DIRECTION('ref_axis',(8.8690509017592E-14,0.969101891289732,0.246660747381227));
#16900=DIRECTION('center_axis',(0.,0.24666074738123,-0.969101891289731));
#16901=DIRECTION('ref_axis',(3.83623821814746E-14,0.969101891289731,0.24666074738123));
#16902=DIRECTION('center_axis',(0.133354868098391,0.207504225145229,-0.969101891289734));
#16903=DIRECTION('ref_axis',(0.523936038703428,0.815260389721652,0.246660747381218));
#16904=DIRECTION('center_axis',(0.133354868098401,0.207504225145245,-0.969101891289729));
#16905=DIRECTION('ref_axis',(0.523936038704652,0.815260389720859,0.246660747381237));
#16906=DIRECTION('center_axis',(-0.133354868098395,0.207504225145243,-0.96910189128973));
#16907=DIRECTION('ref_axis',(-0.523936038705528,0.815260389720298,0.246660747381232));
#16908=DIRECTION('center_axis',(-0.133354868098395,0.207504225145243,-0.96910189128973));
#16909=DIRECTION('ref_axis',(-0.523936038704714,0.815260389720821,0.246660747381232));
#16910=DIRECTION('center_axis',(0.186413754843265,-0.161528438065564,-0.969101891289731));
#16911=DIRECTION('ref_axis',(0.732398341849721,-0.634626775795911,0.246660747381227));
#16912=DIRECTION('center_axis',(0.186413754843273,-0.161528438065571,-0.969101891289729));
#16913=DIRECTION('ref_axis',(0.73239834184858,-0.634626775797224,0.246660747381238));
#16914=DIRECTION('center_axis',(-0.0694923630321335,-0.236669253978789,
-0.969101891289731));
#16915=DIRECTION('ref_axis',(0.273027553673175,0.929846455408943,-0.246660747381229));
#16916=DIRECTION('center_axis',(-0.0694923630321349,-0.236669253978794,
-0.96910189128973));
#16917=DIRECTION('ref_axis',(0.273027553672585,0.929846455409115,-0.246660747381234));
#16918=DIRECTION('center_axis',(-0.186413754843274,-0.161528438065567,-0.969101891289729));
#16919=DIRECTION('ref_axis',(0.732398341847415,0.634626775798569,-0.246660747381236));
#16920=DIRECTION('center_axis',(-0.186413754843274,-0.161528438065567,-0.969101891289729));
#16921=DIRECTION('ref_axis',(0.732398341848765,0.634626775797011,-0.246660747381236));
#16922=DIRECTION('center_axis',(0.0694923630321279,-0.236669253978783,-0.969101891289733));
#16923=DIRECTION('ref_axis',(-0.273027553672171,0.92984645540924,-0.246660747381221));
#16924=DIRECTION('center_axis',(0.0694923630321317,-0.236669253978795,-0.96910189128973));
#16925=DIRECTION('ref_axis',(-0.273027553674098,0.929846455408671,-0.246660747381234));
#16926=DIRECTION('center_axis',(0.,0.,-1.));
#16927=DIRECTION('ref_axis',(-1.,0.,0.));
#16928=DIRECTION('',(-0.246660747381232,3.0207229475572E-17,0.96910189128973));
#16929=DIRECTION('center_axis',(-0.24415009662832,0.0351034843719286,0.96910189128973));
#16930=DIRECTION('ref_axis',(-0.959237831365939,0.137917578929236,-0.246660747381233));
#16931=DIRECTION('center_axis',(-0.24415009662832,0.0351034843719286,0.96910189128973));
#16932=DIRECTION('ref_axis',(0.959237831365939,-0.137917578929238,0.246660747381233));
#16933=DIRECTION('',(-0.246660747381232,3.0207229475572E-17,0.96910189128973));
#16934=DIRECTION('center_axis',(-0.24415009662832,0.0351034843719286,0.96910189128973));
#16935=DIRECTION('ref_axis',(0.959237831365939,-0.137917578929238,0.246660747381233));
#16936=DIRECTION('center_axis',(-0.24415009662832,0.0351034843719286,0.96910189128973));
#16937=DIRECTION('ref_axis',(-0.959237831365939,0.137917578929236,-0.246660747381233));
#16938=DIRECTION('center_axis',(-0.24415009662832,-0.0351034843719251,-0.96910189128973));
#16939=DIRECTION('ref_axis',(-0.959237831365942,-0.137917578929217,0.246660747381232));
#16940=DIRECTION('center_axis',(-0.24415009662832,-0.0351034843719251,-0.96910189128973));
#16941=DIRECTION('ref_axis',(-0.959237831365944,-0.137917578929203,0.246660747381232));
#16942=DIRECTION('center_axis',(-0.186413754843269,0.161528438065567,0.96910189128973));
#16943=DIRECTION('ref_axis',(0.732398341851905,-0.634626775793389,0.246660747381232));
#16944=DIRECTION('center_axis',(-0.18641375484327,0.161528438065568,0.96910189128973));
#16945=DIRECTION('ref_axis',(0.732398341848808,-0.634626775796962,0.246660747381234));
#16946=DIRECTION('center_axis',(0.0694923630321361,0.236669253978799,0.969101891289728));
#16947=DIRECTION('ref_axis',(-0.273027553673749,-0.929846455408772,0.246660747381239));
#16948=DIRECTION('center_axis',(0.0694923630321337,0.23666925397879,0.969101891289731));
#16949=DIRECTION('ref_axis',(-0.273027553671541,-0.929846455409422,0.24666074738123));
#16950=DIRECTION('center_axis',(0.186413754843279,0.161528438065572,0.969101891289727));
#16951=DIRECTION('ref_axis',(0.732398341849398,0.634626775796278,-0.246660747381243));
#16952=DIRECTION('center_axis',(0.186413754843268,0.161528438065562,0.969101891289731));
#16953=DIRECTION('ref_axis',(0.732398341848618,0.634626775797183,-0.246660747381228));
#16954=DIRECTION('center_axis',(-0.069492363032132,0.236669253978797,0.969101891289729));
#16955=DIRECTION('ref_axis',(0.273027553672181,-0.929846455409233,0.246660747381236));
#16956=DIRECTION('center_axis',(-0.0694923630321308,0.236669253978793,0.96910189128973));
#16957=DIRECTION('ref_axis',(0.273027553671897,-0.929846455409317,0.246660747381232));
#16958=DIRECTION('center_axis',(-0.224370507816038,-0.102466577580434,0.969101891289727));
#16959=DIRECTION('ref_axis',(0.881526087074927,0.402579474771994,0.246660747381244));
#16960=DIRECTION('center_axis',(-0.224370507816024,-0.102466577580427,0.969101891289731));
#16961=DIRECTION('ref_axis',(0.881526087075581,0.402579474770572,0.246660747381228));
#16962=DIRECTION('center_axis',(0.224370507816031,-0.102466577580435,0.969101891289729));
#16963=DIRECTION('ref_axis',(0.881526087074644,-0.402579474772618,-0.246660747381238));
#16964=DIRECTION('center_axis',(0.224370507816023,-0.102466577580431,0.969101891289731));
#16965=DIRECTION('ref_axis',(0.881526087074849,-0.402579474772174,-0.246660747381229));
#16966=DIRECTION('center_axis',(0.,-0.246660747381242,0.969101891289728));
#16967=DIRECTION('ref_axis',(-1.28897081029733E-13,-0.969101891289728,-0.246660747381242));
#16968=DIRECTION('center_axis',(0.,-0.246660747381226,0.969101891289732));
#16969=DIRECTION('ref_axis',(-1.10961688006709E-13,-0.969101891289732,-0.246660747381226));
#16970=DIRECTION('center_axis',(-0.133354868098397,-0.207504225145238,0.969101891289731));
#16971=DIRECTION('ref_axis',(-0.523936038702875,-0.815260389722004,-0.246660747381229));
#16972=DIRECTION('center_axis',(-0.133354868098399,-0.207504225145241,0.96910189128973));
#16973=DIRECTION('ref_axis',(-0.523936038705122,-0.815260389720558,-0.246660747381233));
#16974=DIRECTION('center_axis',(0.133354868098399,-0.207504225145248,0.969101891289729));
#16975=DIRECTION('ref_axis',(0.523936038703478,-0.815260389721613,-0.246660747381238));
#16976=DIRECTION('center_axis',(0.133354868098395,-0.207504225145243,0.96910189128973));
#16977=DIRECTION('ref_axis',(0.523936038706261,-0.815260389719827,-0.246660747381232));
#16978=DIRECTION('center_axis',(0.,-0.246660747381232,0.96910189128973));
#16979=DIRECTION('ref_axis',(0.,-0.96910189128973,-0.246660747381232));
#16980=DIRECTION('center_axis',(0.,-0.246660747381232,0.96910189128973));
#16981=DIRECTION('ref_axis',(0.,-0.96910189128973,-0.246660747381232));
#16982=DIRECTION('center_axis',(0.,-0.246660747381232,0.96910189128973));
#16983=DIRECTION('ref_axis',(0.,-0.96910189128973,-0.246660747381232));
#16984=DIRECTION('center_axis',(0.,-0.246660747381232,0.96910189128973));
#16985=DIRECTION('ref_axis',(0.,-0.96910189128973,-0.246660747381232));
#16986=DIRECTION('center_axis',(0.,-0.246660747381232,0.96910189128973));
#16987=DIRECTION('ref_axis',(0.,-0.96910189128973,-0.246660747381232));
#16988=DIRECTION('center_axis',(0.,-0.246660747381232,0.96910189128973));
#16989=DIRECTION('ref_axis',(0.,-0.96910189128973,-0.246660747381232));
#16990=DIRECTION('center_axis',(0.,-0.246660747381232,0.96910189128973));
#16991=DIRECTION('ref_axis',(0.,-0.96910189128973,-0.246660747381232));
#16992=DIRECTION('center_axis',(0.,-0.246660747381232,0.96910189128973));
#16993=DIRECTION('ref_axis',(0.,-0.96910189128973,-0.246660747381232));
#16994=DIRECTION('center_axis',(-0.133354868098398,-0.207504225145241,0.96910189128973));
#16995=DIRECTION('ref_axis',(6.64639222343535E-18,-0.977835574035122,-0.209374282449881));
#16996=DIRECTION('center_axis',(-0.133354868098398,-0.207504225145241,0.96910189128973));
#16997=DIRECTION('ref_axis',(-0.523936038704646,-0.815260389720864,-0.246660747381232));
#16998=DIRECTION('center_axis',(-0.133354868098398,-0.207504225145241,0.96910189128973));
#16999=DIRECTION('ref_axis',(-0.523936038704646,-0.815260389720864,-0.246660747381232));
#17000=DIRECTION('center_axis',(-0.133354868098398,-0.207504225145241,0.96910189128973));
#17001=DIRECTION('ref_axis',(6.64639222343535E-18,-0.977835574035122,-0.209374282449881));
#17002=DIRECTION('center_axis',(-0.133354868098398,-0.207504225145241,0.96910189128973));
#17003=DIRECTION('ref_axis',(-0.523936038704646,-0.815260389720864,-0.246660747381232));
#17004=DIRECTION('center_axis',(-0.133354868098398,-0.207504225145241,0.96910189128973));
#17005=DIRECTION('ref_axis',(-0.523936038704646,-0.815260389720864,-0.246660747381232));
#17006=DIRECTION('center_axis',(-0.133354868098398,-0.207504225145241,0.96910189128973));
#17007=DIRECTION('ref_axis',(-0.523936038704646,-0.815260389720864,-0.246660747381232));
#17008=DIRECTION('center_axis',(-0.133354868098398,-0.207504225145241,0.96910189128973));
#17009=DIRECTION('ref_axis',(-0.523936038704646,-0.815260389720864,-0.246660747381232));
#17010=DIRECTION('center_axis',(0.224370507816026,-0.102466577580432,0.96910189128973));
#17011=DIRECTION('ref_axis',(0.974229800751124,4.74361669806406E-17,-0.225557742780924));
#17012=DIRECTION('center_axis',(0.224370507816026,-0.102466577580432,0.96910189128973));
#17013=DIRECTION('ref_axis',(0.88152608707571,-0.402579474770286,-0.246660747381232));
#17014=DIRECTION('center_axis',(0.224370507816026,-0.102466577580432,0.96910189128973));
#17015=DIRECTION('ref_axis',(0.88152608707571,-0.402579474770287,-0.246660747381232));
#17016=DIRECTION('center_axis',(0.224370507816026,-0.102466577580432,0.96910189128973));
#17017=DIRECTION('ref_axis',(0.974229800751124,4.74361669806406E-17,-0.225557742780924));
#17018=DIRECTION('center_axis',(0.224370507816026,-0.102466577580432,0.96910189128973));
#17019=DIRECTION('ref_axis',(0.88152608707571,-0.402579474770287,-0.246660747381232));
#17020=DIRECTION('center_axis',(0.224370507816026,-0.102466577580432,0.96910189128973));
#17021=DIRECTION('ref_axis',(0.88152608707571,-0.402579474770286,-0.246660747381232));
#17022=DIRECTION('center_axis',(0.224370507816026,-0.102466577580432,0.96910189128973));
#17023=DIRECTION('ref_axis',(0.88152608707571,-0.402579474770286,-0.246660747381232));
#17024=DIRECTION('center_axis',(0.224370507816026,-0.102466577580432,0.96910189128973));
#17025=DIRECTION('ref_axis',(0.88152608707571,-0.402579474770286,-0.246660747381232));
#17026=DIRECTION('center_axis',(0.133354868098395,-0.207504225145243,0.96910189128973));
#17027=DIRECTION('ref_axis',(-9.26824837722223E-18,-0.977835574035122,-0.209374282449883));
#17028=DIRECTION('center_axis',(0.133354868098395,-0.207504225145243,0.96910189128973));
#17029=DIRECTION('ref_axis',(0.523936038704634,-0.815260389720872,-0.246660747381232));
#17030=DIRECTION('center_axis',(0.133354868098395,-0.207504225145243,0.96910189128973));
#17031=DIRECTION('ref_axis',(0.523936038704634,-0.815260389720872,-0.246660747381232));
#17032=DIRECTION('center_axis',(0.133354868098395,-0.207504225145243,0.96910189128973));
#17033=DIRECTION('ref_axis',(-9.26824837722223E-18,-0.977835574035122,-0.209374282449883));
#17034=DIRECTION('center_axis',(0.133354868098395,-0.207504225145243,0.96910189128973));
#17035=DIRECTION('ref_axis',(0.523936038704634,-0.815260389720872,-0.246660747381232));
#17036=DIRECTION('center_axis',(0.133354868098395,-0.207504225145243,0.96910189128973));
#17037=DIRECTION('ref_axis',(0.523936038704634,-0.815260389720872,-0.246660747381232));
#17038=DIRECTION('center_axis',(0.133354868098395,-0.207504225145243,0.96910189128973));
#17039=DIRECTION('ref_axis',(0.523936038704634,-0.815260389720872,-0.246660747381232));
#17040=DIRECTION('center_axis',(0.133354868098395,-0.207504225145243,0.96910189128973));
#17041=DIRECTION('ref_axis',(0.523936038704634,-0.815260389720872,-0.246660747381232));
#17042=DIRECTION('center_axis',(0.24415009662832,0.0351034843719251,0.96910189128973));
#17043=DIRECTION('ref_axis',(0.969699533821307,1.91055182786379E-17,-0.244300663336677));
#17044=DIRECTION('center_axis',(0.24415009662832,0.0351034843719251,0.96910189128973));
#17045=DIRECTION('ref_axis',(0.959237831365941,0.137917578929223,-0.246660747381232));
#17046=DIRECTION('center_axis',(0.24415009662832,0.0351034843719251,0.96910189128973));
#17047=DIRECTION('ref_axis',(0.959237831365941,0.137917578929223,-0.246660747381232));
#17048=DIRECTION('center_axis',(0.24415009662832,0.0351034843719251,0.96910189128973));
#17049=DIRECTION('ref_axis',(0.969699533821307,1.91055182786379E-17,-0.244300663336677));
#17050=DIRECTION('center_axis',(0.24415009662832,0.0351034843719251,0.96910189128973));
#17051=DIRECTION('ref_axis',(0.959237831365941,0.137917578929223,-0.246660747381232));
#17052=DIRECTION('center_axis',(0.24415009662832,0.0351034843719251,0.96910189128973));
#17053=DIRECTION('ref_axis',(0.959237831365941,0.137917578929223,-0.246660747381232));
#17054=DIRECTION('center_axis',(0.24415009662832,0.0351034843719251,0.96910189128973));
#17055=DIRECTION('ref_axis',(0.959237831365941,0.137917578929223,-0.246660747381232));
#17056=DIRECTION('center_axis',(0.24415009662832,0.0351034843719251,0.96910189128973));
#17057=DIRECTION('ref_axis',(0.959237831365941,0.137917578929223,-0.246660747381232));
#17058=DIRECTION('center_axis',(0.186413754843271,0.161528438065564,0.96910189128973));
#17059=DIRECTION('ref_axis',(0.981997424615724,-8.44807439072016E-17,-0.188894303905874));
#17060=DIRECTION('center_axis',(0.186413754843271,0.161528438065564,0.96910189128973));
#17061=DIRECTION('ref_axis',(0.732398341848126,0.63462677579775,-0.246660747381232));
#17062=DIRECTION('center_axis',(0.186413754843271,0.161528438065564,0.96910189128973));
#17063=DIRECTION('ref_axis',(0.732398341848126,0.63462677579775,-0.246660747381232));
#17064=DIRECTION('center_axis',(0.186413754843271,0.161528438065564,0.96910189128973));
#17065=DIRECTION('ref_axis',(0.981997424615724,-8.44807439072016E-17,-0.188894303905874));
#17066=DIRECTION('center_axis',(0.186413754843271,0.161528438065564,0.96910189128973));
#17067=DIRECTION('ref_axis',(0.732398341848126,0.63462677579775,-0.246660747381232));
#17068=DIRECTION('center_axis',(0.186413754843271,0.161528438065564,0.96910189128973));
#17069=DIRECTION('ref_axis',(0.732398341848126,0.63462677579775,-0.246660747381232));
#17070=DIRECTION('center_axis',(0.186413754843271,0.161528438065565,0.96910189128973));
#17071=DIRECTION('ref_axis',(0.732398341848126,0.63462677579775,-0.246660747381233));
#17072=DIRECTION('center_axis',(0.186413754843271,0.161528438065565,0.96910189128973));
#17073=DIRECTION('ref_axis',(0.732398341848126,0.63462677579775,-0.246660747381233));
#17074=DIRECTION('center_axis',(0.0694923630321343,0.236669253978792,0.96910189128973));
#17075=DIRECTION('ref_axis',(1.56176593776512E-18,-0.971450388587214,0.237242792332563));
#17076=DIRECTION('center_axis',(0.0694923630321343,0.236669253978792,0.96910189128973));
#17077=DIRECTION('ref_axis',(0.273027553672928,0.929846455409014,-0.246660747381232));
#17078=DIRECTION('center_axis',(0.0694923630321343,0.236669253978792,0.96910189128973));
#17079=DIRECTION('ref_axis',(0.273027553672928,0.929846455409015,-0.246660747381232));
#17080=DIRECTION('center_axis',(0.0694923630321343,0.236669253978792,0.96910189128973));
#17081=DIRECTION('ref_axis',(1.56176593776512E-18,-0.971450388587214,0.237242792332563));
#17082=DIRECTION('center_axis',(0.0694923630321343,0.236669253978792,0.96910189128973));
#17083=DIRECTION('ref_axis',(0.273027553672928,0.929846455409015,-0.246660747381232));
#17084=DIRECTION('center_axis',(0.0694923630321343,0.236669253978792,0.96910189128973));
#17085=DIRECTION('ref_axis',(0.273027553672928,0.929846455409014,-0.246660747381232));
#17086=DIRECTION('center_axis',(0.0694923630321343,0.236669253978792,0.96910189128973));
#17087=DIRECTION('ref_axis',(0.273027553672928,0.929846455409014,-0.246660747381232));
#17088=DIRECTION('center_axis',(0.0694923630321343,0.236669253978792,0.96910189128973));
#17089=DIRECTION('ref_axis',(0.273027553672928,0.929846455409014,-0.246660747381232));
#17090=DIRECTION('center_axis',(-0.0694923630321309,0.236669253978793,0.96910189128973));
#17091=DIRECTION('ref_axis',(4.13885935595183E-18,-0.971450388587214,0.237242792332564));
#17092=DIRECTION('center_axis',(-0.0694923630321309,0.236669253978793,0.96910189128973));
#17093=DIRECTION('ref_axis',(-0.273027553672915,0.929846455409018,-0.246660747381232));
#17094=DIRECTION('center_axis',(-0.0694923630321309,0.236669253978793,0.96910189128973));
#17095=DIRECTION('ref_axis',(-0.273027553672915,0.929846455409018,-0.246660747381232));
#17096=DIRECTION('center_axis',(-0.0694923630321309,0.236669253978793,0.96910189128973));
#17097=DIRECTION('ref_axis',(4.13885935595183E-18,-0.971450388587214,0.237242792332564));
#17098=DIRECTION('center_axis',(-0.0694923630321309,0.236669253978793,0.96910189128973));
#17099=DIRECTION('ref_axis',(-0.273027553672915,0.929846455409018,-0.246660747381232));
#17100=DIRECTION('center_axis',(-0.0694923630321309,0.236669253978793,0.96910189128973));
#17101=DIRECTION('ref_axis',(-0.273027553672915,0.929846455409018,-0.246660747381232));
#17102=DIRECTION('center_axis',(-0.0694923630321309,0.236669253978793,0.96910189128973));
#17103=DIRECTION('ref_axis',(-0.273027553672915,0.929846455409019,-0.246660747381232));
#17104=DIRECTION('center_axis',(-0.0694923630321309,0.236669253978793,0.96910189128973));
#17105=DIRECTION('ref_axis',(-0.273027553672915,0.929846455409019,-0.246660747381232));
#17106=DIRECTION('center_axis',(-0.186413754843268,0.161528438065567,0.96910189128973));
#17107=DIRECTION('ref_axis',(0.981997424615725,-7.60197659822491E-17,0.188894303905871));
#17108=DIRECTION('center_axis',(-0.186413754843269,0.161528438065567,0.96910189128973));
#17109=DIRECTION('ref_axis',(-0.732398341848117,0.63462677579776,-0.246660747381232));
#17110=DIRECTION('center_axis',(-0.186413754843269,0.161528438065567,0.96910189128973));
#17111=DIRECTION('ref_axis',(-0.732398341848117,0.63462677579776,-0.246660747381232));
#17112=DIRECTION('center_axis',(-0.186413754843268,0.161528438065567,0.96910189128973));
#17113=DIRECTION('ref_axis',(0.981997424615725,-7.60197659822491E-17,0.188894303905871));
#17114=DIRECTION('center_axis',(-0.186413754843269,0.161528438065567,0.96910189128973));
#17115=DIRECTION('ref_axis',(-0.732398341848117,0.63462677579776,-0.246660747381232));
#17116=DIRECTION('center_axis',(-0.186413754843269,0.161528438065567,0.96910189128973));
#17117=DIRECTION('ref_axis',(-0.732398341848117,0.63462677579776,-0.246660747381232));
#17118=DIRECTION('center_axis',(-0.186413754843269,0.161528438065567,0.96910189128973));
#17119=DIRECTION('ref_axis',(-0.732398341848117,0.63462677579776,-0.246660747381232));
#17120=DIRECTION('center_axis',(-0.186413754843269,0.161528438065567,0.96910189128973));
#17121=DIRECTION('ref_axis',(-0.732398341848117,0.63462677579776,-0.246660747381232));
#17122=DIRECTION('center_axis',(-0.24415009662832,0.0351034843719286,0.96910189128973));
#17123=DIRECTION('ref_axis',(0.969699533821307,2.42444443558668E-17,0.244300663336677));
#17124=DIRECTION('center_axis',(-0.24415009662832,0.0351034843719286,0.96910189128973));
#17125=DIRECTION('ref_axis',(-0.959237831365939,0.137917578929236,-0.246660747381233));
#17126=DIRECTION('center_axis',(-0.24415009662832,0.0351034843719286,0.96910189128973));
#17127=DIRECTION('ref_axis',(-0.959237831365939,0.137917578929236,-0.246660747381233));
#17128=DIRECTION('center_axis',(-0.24415009662832,0.0351034843719286,0.96910189128973));
#17129=DIRECTION('ref_axis',(0.969699533821307,2.42444443558668E-17,0.244300663336677));
#17130=DIRECTION('center_axis',(-0.24415009662832,0.0351034843719286,0.96910189128973));
#17131=DIRECTION('ref_axis',(-0.959237831365939,0.137917578929236,-0.246660747381233));
#17132=DIRECTION('center_axis',(-0.24415009662832,0.0351034843719286,0.96910189128973));
#17133=DIRECTION('ref_axis',(-0.959237831365939,0.137917578929236,-0.246660747381233));
#17134=DIRECTION('center_axis',(-0.24415009662832,0.0351034843719286,0.96910189128973));
#17135=DIRECTION('ref_axis',(-0.959237831365939,0.137917578929236,-0.246660747381233));
#17136=DIRECTION('center_axis',(-0.24415009662832,0.0351034843719286,0.96910189128973));
#17137=DIRECTION('ref_axis',(-0.959237831365939,0.137917578929236,-0.246660747381233));
#17138=DIRECTION('center_axis',(-0.224370507816027,-0.102466577580429,0.96910189128973));
#17139=DIRECTION('ref_axis',(0.974229800751124,3.55624843785764E-17,0.225557742780925));
#17140=DIRECTION('center_axis',(-0.224370507816027,-0.102466577580429,0.96910189128973));
#17141=DIRECTION('ref_axis',(-0.881526087075716,-0.402579474770274,-0.246660747381232));
#17142=DIRECTION('center_axis',(-0.224370507816027,-0.102466577580429,0.96910189128973));
#17143=DIRECTION('ref_axis',(-0.881526087075716,-0.402579474770274,-0.246660747381232));
#17144=DIRECTION('center_axis',(-0.224370507816027,-0.102466577580429,0.96910189128973));
#17145=DIRECTION('ref_axis',(0.974229800751124,3.55624843785764E-17,0.225557742780925));
#17146=DIRECTION('center_axis',(-0.224370507816027,-0.102466577580429,0.96910189128973));
#17147=DIRECTION('ref_axis',(-0.881526087075716,-0.402579474770274,-0.246660747381232));
#17148=DIRECTION('center_axis',(-0.224370507816027,-0.102466577580429,0.96910189128973));
#17149=DIRECTION('ref_axis',(-0.881526087075716,-0.402579474770274,-0.246660747381232));
#17150=DIRECTION('center_axis',(-0.224370507816027,-0.102466577580429,0.96910189128973));
#17151=DIRECTION('ref_axis',(-0.881526087075716,-0.402579474770274,-0.246660747381232));
#17152=DIRECTION('center_axis',(-0.224370507816027,-0.102466577580429,0.96910189128973));
#17153=DIRECTION('ref_axis',(-0.881526087075716,-0.402579474770274,-0.246660747381232));
#17154=DIRECTION('center_axis',(0.,0.,-1.));
#17155=DIRECTION('ref_axis',(-1.,0.,0.));
#17156=DIRECTION('center_axis',(0.,0.,-1.));
#17157=DIRECTION('ref_axis',(-1.,0.,0.));
#17158=DIRECTION('center_axis',(-1.22464679914735E-16,-1.,0.));
#17159=DIRECTION('ref_axis',(1.,-1.22464679914735E-16,0.));
#17160=DIRECTION('center_axis',(0.,0.,1.));
#17161=DIRECTION('ref_axis',(-1.,0.,0.));
#17162=DIRECTION('center_axis',(0.,0.,1.));
#17163=DIRECTION('ref_axis',(-1.,0.,0.));
#17164=DIRECTION('center_axis',(0.,0.,1.));
#17165=DIRECTION('ref_axis',(1.,0.,0.));
#17166=DIRECTION('center_axis',(0.,0.,1.));
#17167=DIRECTION('ref_axis',(1.,0.,0.));
#17168=DIRECTION('center_axis',(1.22464679914735E-16,-1.,0.));
#17169=DIRECTION('ref_axis',(-1.,-1.22464679914735E-16,0.));
#17170=DIRECTION('center_axis',(0.,0.,-1.));
#17171=DIRECTION('ref_axis',(1.,0.,0.));
#17172=DIRECTION('center_axis',(0.,0.,1.));
#17173=DIRECTION('ref_axis',(1.,0.,0.));
#17174=DIRECTION('center_axis',(0.,0.,1.));
#17175=DIRECTION('ref_axis',(1.,0.,0.));
#17176=DIRECTION('',(0.96910189128973,1.18680752921561E-16,-0.246660747381235));
#17177=DIRECTION('center_axis',(0.,0.,1.));
#17178=DIRECTION('ref_axis',(1.,0.,0.));
#17179=DIRECTION('center_axis',(0.,0.,1.));
#17180=DIRECTION('ref_axis',(1.,0.,0.));
#17181=DIRECTION('center_axis',(0.,0.,-1.));
#17182=DIRECTION('ref_axis',(-1.,0.,0.));
#17183=DIRECTION('center_axis',(0.,0.,1.));
#17184=DIRECTION('ref_axis',(1.,0.,0.));
#17185=DIRECTION('',(-0.246660747381233,3.02072294755721E-17,0.96910189128973));
#17186=DIRECTION('center_axis',(0.,0.,1.));
#17187=DIRECTION('ref_axis',(1.,0.,0.));
#17188=DIRECTION('center_axis',(0.,0.,1.));
#17189=DIRECTION('ref_axis',(1.,0.,0.));
#17190=DIRECTION('',(-0.96910189128973,-1.18680752921561E-16,0.246660747381235));
#17191=DIRECTION('center_axis',(0.,0.,1.));
#17192=DIRECTION('ref_axis',(1.,0.,0.));
#17193=DIRECTION('center_axis',(0.,0.,1.));
#17194=DIRECTION('ref_axis',(1.,0.,0.));
#17195=DIRECTION('',(0.,0.,-1.));
#17196=DIRECTION('center_axis',(0.,0.,1.));
#17197=DIRECTION('ref_axis',(1.,0.,0.));
#17198=DIRECTION('center_axis',(0.,0.,1.));
#17199=DIRECTION('ref_axis',(1.,0.,0.));
#17200=DIRECTION('',(0.,0.,1.));
#17201=DIRECTION('center_axis',(0.,0.,1.));
#17202=DIRECTION('ref_axis',(1.,0.,0.));
#17203=DIRECTION('center_axis',(0.,0.,1.));
#17204=DIRECTION('ref_axis',(1.,0.,0.));
#17205=DIRECTION('',(0.,0.,-1.));
#17206=DIRECTION('center_axis',(0.,0.,-1.));
#17207=DIRECTION('ref_axis',(-1.,0.,0.));
#17208=DIRECTION('center_axis',(0.,0.,1.));
#17209=DIRECTION('ref_axis',(1.,0.,0.));
#17210=DIRECTION('center_axis',(0.,-0.246660747381232,0.96910189128973));
#17211=DIRECTION('ref_axis',(0.,-0.96910189128973,-0.246660747381232));
#17212=DIRECTION('center_axis',(0.,-0.246660747381232,0.96910189128973));
#17213=DIRECTION('ref_axis',(0.,-0.96910189128973,-0.246660747381232));
#17214=DIRECTION('',(0.,0.246660747381232,-0.96910189128973));
#17215=DIRECTION('center_axis',(0.,-0.246660747381232,0.96910189128973));
#17216=DIRECTION('ref_axis',(0.,-0.96910189128973,-0.246660747381232));
#17217=DIRECTION('center_axis',(0.,-0.246660747381232,0.96910189128973));
#17218=DIRECTION('ref_axis',(0.,-0.96910189128973,-0.246660747381232));
#17219=DIRECTION('center_axis',(0.,-0.246660747381232,0.96910189128973));
#17220=DIRECTION('ref_axis',(0.,-0.96910189128973,-0.246660747381232));
#17221=DIRECTION('center_axis',(-0.133354868098398,-0.207504225145241,0.96910189128973));
#17222=DIRECTION('ref_axis',(-0.523936038704647,-0.815260389720864,-0.246660747381232));
#17223=DIRECTION('center_axis',(-0.133354868098398,-0.207504225145241,0.96910189128973));
#17224=DIRECTION('ref_axis',(-0.523936038704646,-0.815260389720864,-0.246660747381232));
#17225=DIRECTION('',(0.133354868098398,0.207504225145241,-0.96910189128973));
#17226=DIRECTION('center_axis',(-0.133354868098398,-0.207504225145241,0.96910189128973));
#17227=DIRECTION('ref_axis',(-0.523936038704646,-0.815260389720864,-0.246660747381232));
#17228=DIRECTION('center_axis',(-0.133354868098398,-0.207504225145241,0.96910189128973));
#17229=DIRECTION('ref_axis',(-0.523936038704646,-0.815260389720864,-0.246660747381232));
#17230=DIRECTION('center_axis',(-0.133354868098398,-0.207504225145241,0.96910189128973));
#17231=DIRECTION('ref_axis',(-0.523936038704646,-0.815260389720864,-0.246660747381232));
#17232=DIRECTION('center_axis',(-0.224370507816027,-0.102466577580429,0.96910189128973));
#17233=DIRECTION('ref_axis',(-0.881526087075716,-0.402579474770274,-0.246660747381232));
#17234=DIRECTION('center_axis',(-0.224370507816027,-0.102466577580429,0.96910189128973));
#17235=DIRECTION('ref_axis',(-0.881526087075716,-0.402579474770274,-0.246660747381232));
#17236=DIRECTION('',(0.224370507816027,0.102466577580429,-0.96910189128973));
#17237=DIRECTION('center_axis',(-0.224370507816027,-0.102466577580429,0.96910189128973));
#17238=DIRECTION('ref_axis',(-0.881526087075716,-0.402579474770274,-0.246660747381232));
#17239=DIRECTION('center_axis',(-0.224370507816027,-0.102466577580429,0.96910189128973));
#17240=DIRECTION('ref_axis',(-0.881526087075716,-0.402579474770274,-0.246660747381232));
#17241=DIRECTION('center_axis',(-0.224370507816027,-0.102466577580429,0.96910189128973));
#17242=DIRECTION('ref_axis',(-0.881526087075716,-0.402579474770274,-0.246660747381232));
#17243=DIRECTION('center_axis',(-0.244150096628319,0.0351034843719286,0.96910189128973));
#17244=DIRECTION('ref_axis',(-0.959237831365939,0.137917578929236,-0.246660747381232));
#17245=DIRECTION('center_axis',(-0.24415009662832,0.0351034843719286,0.96910189128973));
#17246=DIRECTION('ref_axis',(-0.959237831365939,0.137917578929236,-0.246660747381233));
#17247=DIRECTION('',(0.244150096628319,-0.0351034843719286,-0.96910189128973));
#17248=DIRECTION('center_axis',(-0.24415009662832,0.0351034843719286,0.96910189128973));
#17249=DIRECTION('ref_axis',(-0.959237831365939,0.137917578929236,-0.246660747381233));
#17250=DIRECTION('center_axis',(-0.24415009662832,0.0351034843719286,0.96910189128973));
#17251=DIRECTION('ref_axis',(-0.959237831365939,0.137917578929236,-0.246660747381233));
#17252=DIRECTION('center_axis',(-0.24415009662832,0.0351034843719286,0.96910189128973));
#17253=DIRECTION('ref_axis',(-0.959237831365939,0.137917578929236,-0.246660747381233));
#17254=DIRECTION('center_axis',(-0.186413754843269,0.161528438065567,0.96910189128973));
#17255=DIRECTION('ref_axis',(-0.732398341848117,0.63462677579776,-0.246660747381232));
#17256=DIRECTION('center_axis',(-0.186413754843269,0.161528438065567,0.96910189128973));
#17257=DIRECTION('ref_axis',(-0.732398341848117,0.63462677579776,-0.246660747381232));
#17258=DIRECTION('',(0.186413754843269,-0.161528438065567,-0.96910189128973));
#17259=DIRECTION('center_axis',(-0.186413754843269,0.161528438065567,0.96910189128973));
#17260=DIRECTION('ref_axis',(-0.732398341848117,0.634626775797761,-0.246660747381232));
#17261=DIRECTION('center_axis',(-0.186413754843269,0.161528438065567,0.96910189128973));
#17262=DIRECTION('ref_axis',(-0.732398341848117,0.63462677579776,-0.246660747381232));
#17263=DIRECTION('center_axis',(-0.186413754843269,0.161528438065567,0.96910189128973));
#17264=DIRECTION('ref_axis',(-0.732398341848117,0.63462677579776,-0.246660747381232));
#17265=DIRECTION('center_axis',(-0.0694923630321309,0.236669253978793,0.96910189128973));
#17266=DIRECTION('ref_axis',(-0.273027553672915,0.929846455409018,-0.246660747381232));
#17267=DIRECTION('center_axis',(-0.0694923630321309,0.236669253978793,0.96910189128973));
#17268=DIRECTION('ref_axis',(-0.273027553672915,0.929846455409018,-0.246660747381232));
#17269=DIRECTION('',(0.0694923630321309,-0.236669253978793,-0.96910189128973));
#17270=DIRECTION('center_axis',(-0.0694923630321309,0.236669253978793,0.96910189128973));
#17271=DIRECTION('ref_axis',(-0.273027553672915,0.929846455409018,-0.246660747381232));
#17272=DIRECTION('center_axis',(-0.0694923630321309,0.236669253978793,0.96910189128973));
#17273=DIRECTION('ref_axis',(-0.273027553672915,0.929846455409019,-0.246660747381232));
#17274=DIRECTION('center_axis',(-0.0694923630321309,0.236669253978793,0.96910189128973));
#17275=DIRECTION('ref_axis',(-0.273027553672915,0.929846455409019,-0.246660747381232));
#17276=DIRECTION('center_axis',(0.0694923630321343,0.236669253978792,0.96910189128973));
#17277=DIRECTION('ref_axis',(0.273027553672928,0.929846455409015,-0.246660747381232));
#17278=DIRECTION('center_axis',(0.0694923630321343,0.236669253978792,0.96910189128973));
#17279=DIRECTION('ref_axis',(0.273027553672928,0.929846455409015,-0.246660747381232));
#17280=DIRECTION('',(-0.0694923630321343,-0.236669253978792,-0.96910189128973));
#17281=DIRECTION('center_axis',(0.0694923630321343,0.236669253978792,0.96910189128973));
#17282=DIRECTION('ref_axis',(0.273027553672928,0.929846455409015,-0.246660747381232));
#17283=DIRECTION('center_axis',(0.0694923630321343,0.236669253978792,0.96910189128973));
#17284=DIRECTION('ref_axis',(0.273027553672928,0.929846455409014,-0.246660747381232));
#17285=DIRECTION('center_axis',(0.0694923630321343,0.236669253978792,0.96910189128973));
#17286=DIRECTION('ref_axis',(0.273027553672928,0.929846455409014,-0.246660747381232));
#17287=DIRECTION('center_axis',(0.186413754843271,0.161528438065564,0.96910189128973));
#17288=DIRECTION('ref_axis',(0.732398341848126,0.63462677579775,-0.246660747381232));
#17289=DIRECTION('center_axis',(0.186413754843271,0.161528438065564,0.96910189128973));
#17290=DIRECTION('ref_axis',(0.732398341848126,0.63462677579775,-0.246660747381232));
#17291=DIRECTION('',(-0.186413754843271,-0.161528438065564,-0.96910189128973));
#17292=DIRECTION('center_axis',(0.186413754843271,0.161528438065564,0.96910189128973));
#17293=DIRECTION('ref_axis',(0.732398341848126,0.63462677579775,-0.246660747381232));
#17294=DIRECTION('center_axis',(0.186413754843271,0.161528438065565,0.96910189128973));
#17295=DIRECTION('ref_axis',(0.732398341848126,0.63462677579775,-0.246660747381233));
#17296=DIRECTION('center_axis',(0.186413754843271,0.161528438065565,0.96910189128973));
#17297=DIRECTION('ref_axis',(0.732398341848126,0.63462677579775,-0.246660747381233));
#17298=DIRECTION('center_axis',(0.24415009662832,0.0351034843719251,0.96910189128973));
#17299=DIRECTION('ref_axis',(0.959237831365941,0.137917578929223,-0.246660747381232));
#17300=DIRECTION('center_axis',(0.24415009662832,0.0351034843719251,0.96910189128973));
#17301=DIRECTION('ref_axis',(0.959237831365941,0.137917578929223,-0.246660747381232));
#17302=DIRECTION('',(-0.24415009662832,-0.0351034843719251,-0.96910189128973));
#17303=DIRECTION('center_axis',(0.24415009662832,0.0351034843719251,0.96910189128973));
#17304=DIRECTION('ref_axis',(0.959237831365941,0.137917578929223,-0.246660747381232));
#17305=DIRECTION('center_axis',(0.24415009662832,0.0351034843719251,0.96910189128973));
#17306=DIRECTION('ref_axis',(0.959237831365941,0.137917578929223,-0.246660747381232));
#17307=DIRECTION('center_axis',(0.24415009662832,0.0351034843719251,0.96910189128973));
#17308=DIRECTION('ref_axis',(0.959237831365941,0.137917578929223,-0.246660747381232));
#17309=DIRECTION('center_axis',(0.224370507816026,-0.102466577580432,0.96910189128973));
#17310=DIRECTION('ref_axis',(0.88152608707571,-0.402579474770286,-0.246660747381232));
#17311=DIRECTION('center_axis',(0.224370507816026,-0.102466577580432,0.96910189128973));
#17312=DIRECTION('ref_axis',(0.88152608707571,-0.402579474770286,-0.246660747381232));
#17313=DIRECTION('',(-0.224370507816026,0.102466577580432,-0.96910189128973));
#17314=DIRECTION('center_axis',(0.224370507816026,-0.102466577580432,0.96910189128973));
#17315=DIRECTION('ref_axis',(0.88152608707571,-0.402579474770287,-0.246660747381232));
#17316=DIRECTION('center_axis',(0.224370507816026,-0.102466577580432,0.96910189128973));
#17317=DIRECTION('ref_axis',(0.88152608707571,-0.402579474770286,-0.246660747381232));
#17318=DIRECTION('center_axis',(0.224370507816026,-0.102466577580432,0.96910189128973));
#17319=DIRECTION('ref_axis',(0.88152608707571,-0.402579474770286,-0.246660747381232));
#17320=DIRECTION('center_axis',(0.133354868098395,-0.207504225145243,0.96910189128973));
#17321=DIRECTION('ref_axis',(0.523936038704634,-0.815260389720872,-0.246660747381232));
#17322=DIRECTION('center_axis',(0.133354868098395,-0.207504225145243,0.96910189128973));
#17323=DIRECTION('ref_axis',(0.523936038704634,-0.815260389720872,-0.246660747381232));
#17324=DIRECTION('',(-0.133354868098395,0.207504225145243,-0.96910189128973));
#17325=DIRECTION('center_axis',(0.133354868098395,-0.207504225145243,0.96910189128973));
#17326=DIRECTION('ref_axis',(0.523936038704634,-0.815260389720872,-0.246660747381232));
#17327=DIRECTION('center_axis',(0.133354868098395,-0.207504225145243,0.96910189128973));
#17328=DIRECTION('ref_axis',(0.523936038704634,-0.815260389720872,-0.246660747381232));
#17329=DIRECTION('center_axis',(0.133354868098395,-0.207504225145243,0.96910189128973));
#17330=DIRECTION('ref_axis',(0.523936038704634,-0.815260389720872,-0.246660747381232));
#17331=DIRECTION('',(1.,-3.79883255563056E-45,4.81559236931162E-15));
#17332=DIRECTION('',(4.81559236931162E-15,7.88860905221012E-31,-1.));
#17333=DIRECTION('',(0.,0.,1.));
#17334=DIRECTION('',(1.,0.,0.));
#17335=DIRECTION('',(0.,0.,1.));
#17336=DIRECTION('',(1.,0.,0.));
#17337=DIRECTION('',(0.,0.,1.));
#17338=DIRECTION('',(1.,0.,0.));
#17339=DIRECTION('',(0.,0.,1.));
#17340=DIRECTION('',(1.,0.,0.));
#17341=DIRECTION('',(0.,0.,1.));
#17342=DIRECTION('',(1.,0.,0.));
#17343=DIRECTION('',(0.,0.,1.));
#17344=DIRECTION('',(1.,0.,0.));
#17345=DIRECTION('',(0.,0.,1.));
#17346=DIRECTION('',(1.,0.,0.));
#17347=DIRECTION('',(0.,0.,1.));
#17348=DIRECTION('',(1.,0.,0.));
#17349=DIRECTION('',(1.,3.79883255563056E-45,-4.81559236931161E-15));
#17350=DIRECTION('',(-4.81559236931161E-15,7.88860905221012E-31,-1.));
#17351=DIRECTION('',(0.,0.,1.));
#17352=DIRECTION('',(1.,0.,0.));
#17353=CARTESIAN_POINT('',(0.,0.,0.));
#17354=CARTESIAN_POINT('',(0.,0.,0.));
#17355=CARTESIAN_POINT('Origin',(0.,0.,-16.4167025567876));
#17356=CARTESIAN_POINT('',(4.94641461892554,-6.44544214322681,11.1250611305836));
#17357=CARTESIAN_POINT('',(4.94634499595658,-6.44535064078879,11.2916505155556));
#17358=CARTESIAN_POINT('',(4.94675008185374,-6.44587862049697,-16.4167025567876));
#17359=CARTESIAN_POINT('',(2.10208451021607,7.84862588447237,12.));
#17360=CARTESIAN_POINT('Ctrl Pts',(4.94634499595713,-6.44535064078836,11.2916505155556));
#17361=CARTESIAN_POINT('Ctrl Pts',(5.46269818329968,-6.04916543688375,11.3171416411407));
#17362=CARTESIAN_POINT('Ctrl Pts',(6.90127424538504,-4.64649602035922,11.3952891090332));
#17363=CARTESIAN_POINT('Ctrl Pts',(8.32999914323059,-1.51322275430053,11.5260929192331));
#17364=CARTESIAN_POINT('Ctrl Pts',(8.04577806167976,2.63534640472438,11.6840619461554));
#17365=CARTESIAN_POINT('Ctrl Pts',(5.82000697965989,6.14913288471192,11.8420309730777));
#17366=CARTESIAN_POINT('Ctrl Pts',(3.40044170599962,7.5008890207006,11.9473436576926));
#17367=CARTESIAN_POINT('Ctrl Pts',(2.10208451021619,7.84862588447234,12.));
#17368=CARTESIAN_POINT('',(-2.10232310766211,7.84918820146781,12.));
#17369=CARTESIAN_POINT('Origin',(0.,0.,12.));
#17370=CARTESIAN_POINT('Ctrl Pts',(4.94641461892554,-6.44544214322681,11.1250611305836));
#17371=CARTESIAN_POINT('Ctrl Pts',(5.59685733717957,-5.94568272231727,11.1571897395813));
#17372=CARTESIAN_POINT('Ctrl Pts',(7.11589899816117,-4.3690230073217,11.2419746908865));
#17373=CARTESIAN_POINT('Ctrl Pts',(8.40836897789325,-0.989475114550315,
11.3794159844989));
#17374=CARTESIAN_POINT('Ctrl Pts',(7.86514495884525,3.13354651991988,11.5373850114212));
#17375=CARTESIAN_POINT('Ctrl Pts',(5.42427178070265,6.50055875679946,11.6953540383435));
#17376=CARTESIAN_POINT('Ctrl Pts',(1.76398188025238,8.25622587257004,11.8495590345364));
#17377=CARTESIAN_POINT('Ctrl Pts',(-0.896857186010099,8.17128250291834,
11.9511076884219));
#17378=CARTESIAN_POINT('Ctrl Pts',(-2.10232310766211,7.84918820146781,12.));
#17379=CARTESIAN_POINT('Origin',(0.,0.,-16.4167025567876));
#17380=CARTESIAN_POINT('',(4.94675008185374,-6.44587862049698,9.12505123879043));
#17381=CARTESIAN_POINT('',(4.94675008185378,-6.44587862049694,9.29164626296918));
#17382=CARTESIAN_POINT('',(4.94675008185374,-6.44587862049697,-16.4167025567876));
#17383=CARTESIAN_POINT('',(-8.12531051676223,4.45465981452085E-5,10.5832974437648));
#17384=CARTESIAN_POINT('Ctrl Pts',(4.94675008185378,-6.44587862049695,9.29164626296917));
#17385=CARTESIAN_POINT('Ctrl Pts',(5.10118068104462,-6.32736419846628,9.29927302275314));
#17386=CARTESIAN_POINT('Ctrl Pts',(5.25133360162953,-6.20331023734921,9.3068997825371));
#17387=CARTESIAN_POINT('Ctrl Pts',(5.39681829916228,-6.07404641144,9.31452654232107));
#17388=CARTESIAN_POINT('Ctrl Pts',(5.55368691362083,-5.93466792274758,9.32275008239372));
#17389=CARTESIAN_POINT('Ctrl Pts',(5.70517872870825,-5.78918660410757,9.33097362246638));
#17390=CARTESIAN_POINT('Ctrl Pts',(5.85082702241694,-5.63804139008004,9.33919716253903));
#17391=CARTESIAN_POINT('Ctrl Pts',(5.99644883481933,-5.48692365679126,9.34741920743397));
#17392=CARTESIAN_POINT('Ctrl Pts',(6.13622904182113,-5.3301442957319,9.35564125232891));
#17393=CARTESIAN_POINT('Ctrl Pts',(6.26973810288252,-5.16817875888239,9.36386329722384));
#17394=CARTESIAN_POINT('Ctrl Pts',(6.40323242351307,-5.00623110427828,9.37208443434156));
#17395=CARTESIAN_POINT('Ctrl Pts',(6.53045679299592,-4.83909864454014,9.38030557145927));
#17396=CARTESIAN_POINT('Ctrl Pts',(6.65102172662004,-4.66729017252282,9.38852670857699));
#17397=CARTESIAN_POINT('Ctrl Pts',(6.77159622277953,-4.49546807361966,9.39674849774927));
#17398=CARTESIAN_POINT('Ctrl Pts',(6.8855100561201,-4.31896946130181,9.40497028692155));
#17399=CARTESIAN_POINT('Ctrl Pts',(6.9924162780203,-4.13833325837549,9.41319207609382));
#17400=CARTESIAN_POINT('Ctrl Pts',(7.09932220321884,-3.95769755677698,9.42141384244779));
#17401=CARTESIAN_POINT('Ctrl Pts',(7.19922040798751,-3.77292454272602,9.42963560880176));
#17402=CARTESIAN_POINT('Ctrl Pts',(7.29180896211549,-3.58457942058929,9.43785737515573));
#17403=CARTESIAN_POINT('Ctrl Pts',(7.38441681926181,-3.39619503194298,9.44608085559746));
#17404=CARTESIAN_POINT('Ctrl Pts',(7.46971185125825,-3.20423731220333,9.45430433603919));
#17405=CARTESIAN_POINT('Ctrl Pts',(7.54743903387266,-3.00929420171497,9.46252781648091));
#17406=CARTESIAN_POINT('Ctrl Pts',(7.57884363377462,-2.93053011709735,9.46585040073506));
#17407=CARTESIAN_POINT('Ctrl Pts',(7.60901336428037,-2.8512789138126,9.46917298498921));
#17408=CARTESIAN_POINT('Ctrl Pts',(7.63793365164409,-2.77158025241607,9.47249556924336));
#17409=CARTESIAN_POINT('Ctrl Pts',(7.70951258681434,-2.5743226925063,9.48071910588856));
#17410=CARTESIAN_POINT('Ctrl Pts',(7.77345749340724,-2.37425871081297,9.48894264253376));
#17411=CARTESIAN_POINT('Ctrl Pts',(7.82956695341158,-2.17199652038058,9.49716617917896));
#17412=CARTESIAN_POINT('Ctrl Pts',(7.88566621167817,-1.96977110495586,9.50538822063308));
#17413=CARTESIAN_POINT('Ctrl Pts',(7.93393278795164,-1.76534856255913,9.5136102620872));
#17414=CARTESIAN_POINT('Ctrl Pts',(7.97421534807755,-1.55935151424699,9.52183230354132));
#17415=CARTESIAN_POINT('Ctrl Pts',(8.01449346068486,-1.35337720966573,9.53005343721594));
#17416=CARTESIAN_POINT('Ctrl Pts',(8.0467892604458,-1.14582903557047,9.53827457089056));
#17417=CARTESIAN_POINT('Ctrl Pts',(8.07100251214971,-0.937339859054906,
9.54649570456517));
#17418=CARTESIAN_POINT('Ctrl Pts',(8.09521768437924,-0.728834145776361,
9.55471749031651));
#17419=CARTESIAN_POINT('Ctrl Pts',(8.11134899094865,-0.519387573613384,
9.56293927606786));
#17420=CARTESIAN_POINT('Ctrl Pts',(8.11934794775107,-0.309639251146375,
9.5711610618192));
#17421=CARTESIAN_POINT('Ctrl Pts',(8.1273468823722,-0.0998915103161628,
9.57938282477134));
#17422=CARTESIAN_POINT('Ctrl Pts',(8.127213503792,0.11015768432331,9.58760458772348));
#17423=CARTESIAN_POINT('Ctrl Pts',(8.11895142944701,0.319867548807802,9.59582635067563));
#17424=CARTESIAN_POINT('Ctrl Pts',(8.11068763255972,0.529621135255785,9.60404982776564));
#17425=CARTESIAN_POINT('Ctrl Pts',(8.09429176592694,0.739034955460716,9.61227330485565));
#17426=CARTESIAN_POINT('Ctrl Pts',(8.06981952014667,0.947470566698362,9.62049678194566));
#17427=CARTESIAN_POINT('Ctrl Pts',(8.05993178057643,1.03168666437841,9.62381938668566));
#17428=CARTESIAN_POINT('Ctrl Pts',(8.04872618389744,1.11574312782325,9.62714199142565));
#17429=CARTESIAN_POINT('Ctrl Pts',(8.03620879910646,1.19959814090547,9.63046459616564));
#17430=CARTESIAN_POINT('Ctrl Pts',(8.00522790680143,1.40714174309708,9.63868813976847));
#17431=CARTESIAN_POINT('Ctrl Pts',(7.96619763652384,1.61351824172196,9.6469116833713));
#17432=CARTESIAN_POINT('Ctrl Pts',(7.91923047146385,1.81809689025048,9.65513522697413));
#17433=CARTESIAN_POINT('Ctrl Pts',(7.87227184577047,2.02263834317481,9.66335727540786));
#17434=CARTESIAN_POINT('Ctrl Pts',(7.81737927142266,2.22538231109902,9.6715793238416));
#17435=CARTESIAN_POINT('Ctrl Pts',(7.75471613389214,2.42570922520672,9.67980137227533));
#17436=CARTESIAN_POINT('Ctrl Pts',(7.6920599148738,2.62601402161889,9.68802251292907));
#17437=CARTESIAN_POINT('Ctrl Pts',(7.62163493351841,2.82390201562019,9.69624365358282));
#17438=CARTESIAN_POINT('Ctrl Pts',(7.54365438847455,3.01876895931911,9.70446479423656));
#17439=CARTESIAN_POINT('Ctrl Pts',(7.46566765874121,3.21365135804645,9.7126865869145));
#17440=CARTESIAN_POINT('Ctrl Pts',(7.38012427510874,3.40551195291009,9.72090837959244));
#17441=CARTESIAN_POINT('Ctrl Pts',(7.28728591611064,3.59376564891974,9.72913017227038));
#17442=CARTESIAN_POINT('Ctrl Pts',(7.19444781504218,3.78201882191059,9.737351942106));
#17443=CARTESIAN_POINT('Ctrl Pts',(7.09431491201529,3.96666485277055,9.74557371194161));
#17444=CARTESIAN_POINT('Ctrl Pts',(6.98719549945698,4.14714198151788,9.75379548177722));
#17445=CARTESIAN_POINT('Ctrl Pts',(6.88005375522472,4.32765673515784,9.76201896564281));
#17446=CARTESIAN_POINT('Ctrl Pts',(6.76592274233344,4.50400059678417,9.77024244950839));
#17447=CARTESIAN_POINT('Ctrl Pts',(6.64515542962041,4.67563865997859,9.77846593337397));
#17448=CARTESIAN_POINT('Ctrl Pts',(6.59636138562037,4.74498619301089,9.78178849661196));
#17449=CARTESIAN_POINT('Ctrl Pts',(6.54648450469863,4.8135658675388,9.78511105984995));
#17450=CARTESIAN_POINT('Ctrl Pts',(6.49555003357664,4.88134380307334,9.78843362308793));
#17451=CARTESIAN_POINT('Ctrl Pts',(6.36948432400681,5.04909804392677,9.79665715585387));
#17452=CARTESIAN_POINT('Ctrl Pts',(6.23689602737285,5.21199325894114,9.80488068861981));
#17453=CARTESIAN_POINT('Ctrl Pts',(6.09818438755089,5.36952835339665,9.81310422138575));
#17454=CARTESIAN_POINT('Ctrl Pts',(5.95949796812527,5.5270348049962,9.82132625895809));
#17455=CARTESIAN_POINT('Ctrl Pts',(5.81469062241994,5.67918285992319,9.82954829653043));
#17456=CARTESIAN_POINT('Ctrl Pts',(5.66420103359679,5.82550548995544,9.83777033410278));
#17457=CARTESIAN_POINT('Ctrl Pts',(5.51372805986296,5.97181196495939,9.84599146390542));
#17458=CARTESIAN_POINT('Ctrl Pts',(5.3575743068858,6.11229409360518,9.85421259370807));
#17459=CARTESIAN_POINT('Ctrl Pts',(5.19621496658465,6.24652203898631,9.86243372351071));
#17460=CARTESIAN_POINT('Ctrl Pts',(5.03484282687037,6.3807606316527,9.87065550543326));
#17461=CARTESIAN_POINT('Ctrl Pts',(4.86826449983262,6.50874385914892,9.8788772873558));
#17462=CARTESIAN_POINT('Ctrl Pts',(4.69698868909341,6.63008181073421,9.88709906927834));
#17463=CARTESIAN_POINT('Ctrl Pts',(4.52571335263917,6.75141942631895,9.8953208284337));
#17464=CARTESIAN_POINT('Ctrl Pts',(4.34974080072379,6.86611163451026,9.90354258758907));
#17465=CARTESIAN_POINT('Ctrl Pts',(4.16960961644487,6.97381123984228,9.91176434674443));
#17466=CARTESIAN_POINT('Ctrl Pts',(3.98944087541279,7.08153330018401,9.91998782010925));
#17467=CARTESIAN_POINT('Ctrl Pts',(3.80511202306167,7.1822596937542,9.92821129347406));
#17468=CARTESIAN_POINT('Ctrl Pts',(3.61718814284456,7.27568811190836,9.93643476683888));
#17469=CARTESIAN_POINT('Ctrl Pts',(3.54125902303476,7.31343710659426,9.93975739456266));
#17470=CARTESIAN_POINT('Ctrl Pts',(3.46474329176694,7.34999523346899,9.94308002228644));
#17471=CARTESIAN_POINT('Ctrl Pts',(3.38767928464742,7.38534471956934,9.94640265001022));
#17472=CARTESIAN_POINT('Ctrl Pts',(3.19694494112705,7.47283512238055,9.9546261935469));
#17473=CARTESIAN_POINT('Ctrl Pts',(3.00278850872504,7.55294691300247,9.96284973708356));
#17474=CARTESIAN_POINT('Ctrl Pts',(2.80579966671456,7.62542954808216,9.97107328062024));
#17475=CARTESIAN_POINT('Ctrl Pts',(2.60884664093059,7.69789900447391,9.97929532896411));
#17476=CARTESIAN_POINT('Ctrl Pts',(2.40906251004286,7.76274197206463,9.98751737730799));
#17477=CARTESIAN_POINT('Ctrl Pts',(2.20705541388873,7.81975664343363,9.99573942565187));
#17478=CARTESIAN_POINT('Ctrl Pts',(2.00507062150387,7.87676501976597,10.0039605661926));
#17479=CARTESIAN_POINT('Ctrl Pts',(1.800863637598,7.92594674539523,10.0121817067334));
#17480=CARTESIAN_POINT('Ctrl Pts',(1.59505699769923,7.96715010129662,10.0204028472742));
#17481=CARTESIAN_POINT('Ctrl Pts',(1.38923403596426,8.00835672489834,10.0286246398061));
#17482=CARTESIAN_POINT('Ctrl Pts',(1.18181145343513,8.04158365400576,10.036846432338));
#17483=CARTESIAN_POINT('Ctrl Pts',(0.97342224362766,8.06673023585832,10.04506822487));
#17484=CARTESIAN_POINT('Ctrl Pts',(0.76503361325674,8.09187674778957,10.0532899945408));
#17485=CARTESIAN_POINT('Ctrl Pts',(0.555678654114234,8.10894292475295,10.0615117642116));
#17486=CARTESIAN_POINT('Ctrl Pts',(0.345996295648056,8.11787990339213,10.0697335338824));
#17487=CARTESIAN_POINT('Ctrl Pts',(0.136270224418411,8.12681874513528,10.0779570175566));
#17488=CARTESIAN_POINT('Ctrl Pts',(-0.0737830877680571,8.12762499045848,
10.0861805012309));
#17489=CARTESIAN_POINT('Ctrl Pts',(-0.283522780993305,8.12030186601199,
10.0944039849051));
#17490=CARTESIAN_POINT('Ctrl Pts',(-0.368264671852043,8.11734307741529,
10.0977265489142));
#17491=CARTESIAN_POINT('Ctrl Pts',(-0.452955373840572,8.11305781836599,
10.1010491129234));
#17492=CARTESIAN_POINT('Ctrl Pts',(-0.537552715890539,8.10744871338319,
10.1043716769325));
#17493=CARTESIAN_POINT('Ctrl Pts',(-0.746936273138496,8.09356583803725,
10.1125952245589));
#17494=CARTESIAN_POINT('Ctrl Pts',(-0.95581573925282,8.07156504140797,10.1208187721854));
#17495=CARTESIAN_POINT('Ctrl Pts',(-1.16355327480506,8.04150678288531,10.1290423198118));
#17496=CARTESIAN_POINT('Ctrl Pts',(-1.37125304209956,8.01145398918175,10.137264372335));
#17497=CARTESIAN_POINT('Ctrl Pts',(-1.57781100145189,7.97334669958723,10.1454864248582));
#17498=CARTESIAN_POINT('Ctrl Pts',(-1.78259628568773,7.92729702009154,10.1537084773814));
#17499=CARTESIAN_POINT('Ctrl Pts',(-1.98735896129443,7.88125242455553,10.1619296221766));
#17500=CARTESIAN_POINT('Ctrl Pts',(-2.19034906486886,7.82726725440287,10.1701507669718));
#17501=CARTESIAN_POINT('Ctrl Pts',(-2.39094691996103,7.76550451602656,10.1783719117669));
#17502=CARTESIAN_POINT('Ctrl Pts',(-2.59156068571871,7.70373687886271,10.1865937086323));
#17503=CARTESIAN_POINT('Ctrl Pts',(-2.78978154120482,7.63419052513503,10.1948155054977));
#17504=CARTESIAN_POINT('Ctrl Pts',(-2.98500492896638,7.55707834659311,10.2030373023631));
#17505=CARTESIAN_POINT('Ctrl Pts',(-3.18022777478683,7.47996638211498,10.2112590764048));
#17506=CARTESIAN_POINT('Ctrl Pts',(-3.37245289621099,7.39528874569337,10.2194808504464));
#17507=CARTESIAN_POINT('Ctrl Pts',(-3.56109517563416,7.30330669714583,10.227702624488));
#17508=CARTESIAN_POINT('Ctrl Pts',(-3.74977678216303,7.2113054726863,10.23592611256));
#17509=CARTESIAN_POINT('Ctrl Pts',(-3.93487378939249,7.11199692330008,10.2441496006319));
#17510=CARTESIAN_POINT('Ctrl Pts',(-4.11582418494491,7.00568903400105,10.2523730887038));
#17511=CARTESIAN_POINT('Ctrl Pts',(-4.18893362822572,6.96273742519532,10.2556956270875));
#17512=CARTESIAN_POINT('Ctrl Pts',(-4.26136646570056,6.91864375934967,10.2590181654711));
#17513=CARTESIAN_POINT('Ctrl Pts',(-4.33308686423123,6.87343042370597,10.2623407038548));
#17514=CARTESIAN_POINT('Ctrl Pts',(-4.51059939498032,6.76152455315659,10.2705641968788));
#17515=CARTESIAN_POINT('Ctrl Pts',(-4.68380334479664,6.64272019540365,10.2787876899029));
#17516=CARTESIAN_POINT('Ctrl Pts',(-4.85216661490309,6.51737421848093,10.2870111829269));
#17517=CARTESIAN_POINT('Ctrl Pts',(-5.02049926876101,6.39205103526837,10.2952331805386));
#17518=CARTESIAN_POINT('Ctrl Pts',(-5.1839927633476,6.26018878317385,10.3034551781503));
#17519=CARTESIAN_POINT('Ctrl Pts',(-5.34214572251453,6.12218642658974,10.311677175762));
#17520=CARTESIAN_POINT('Ctrl Pts',(-5.50028121871459,5.98419930797901,10.3198982655155));
#17521=CARTESIAN_POINT('Ctrl Pts',(-5.65307713464885,5.84007363228023,10.3281193552689));
#17522=CARTESIAN_POINT('Ctrl Pts',(-5.80006617113131,5.69024779539504,10.3363404450223));
#17523=CARTESIAN_POINT('Ctrl Pts',(-5.94706687016392,5.54041007087948,10.3445621870617));
#17524=CARTESIAN_POINT('Ctrl Pts',(-6.08825956070333,5.3848714901936,10.352783929101));
#17525=CARTESIAN_POINT('Ctrl Pts',(-6.223213991623,5.2241071176774,10.3610056711403));
#17526=CARTESIAN_POINT('Ctrl Pts',(-6.35816805162263,5.06334318701944,10.3692273905823));
#17527=CARTESIAN_POINT('Ctrl Pts',(-6.48688369873636,4.89735372089354,10.3774491100243));
#17528=CARTESIAN_POINT('Ctrl Pts',(-6.60897080711255,4.72664706036257,10.3856708294663));
#17529=CARTESIAN_POINT('Ctrl Pts',(-6.73108337788995,4.55590479737089,10.3938942636243));
#17530=CARTESIAN_POINT('Ctrl Pts',(-6.84656447660069,4.38044361453761,10.4021176977823));
#17531=CARTESIAN_POINT('Ctrl Pts',(-6.95506654361545,4.20080193967545,10.4103411319402));
#17532=CARTESIAN_POINT('Ctrl Pts',(-6.99890928045173,4.12821362046178,10.4136639982192));
#17533=CARTESIAN_POINT('Ctrl Pts',(-7.04161301819278,4.05494305048928,10.4169868644981));
#17534=CARTESIAN_POINT('Ctrl Pts',(-7.08315690008883,3.98102698951213,10.4203097307771));
#17535=CARTESIAN_POINT('Ctrl Pts',(-7.18597263275045,3.7980943020025,10.4285333948984));
#17536=CARTESIAN_POINT('Ctrl Pts',(-7.28171451842812,3.61114674844409,10.4367570590196));
#17537=CARTESIAN_POINT('Ctrl Pts',(-7.37008456692655,3.42075153129413,10.4449807231409));
#17538=CARTESIAN_POINT('Ctrl Pts',(-7.45843855370341,3.23039091947729,10.4532028925679));
#17539=CARTESIAN_POINT('Ctrl Pts',(-7.53942325343114,3.03658416212785,10.4614250619949));
#17540=CARTESIAN_POINT('Ctrl Pts',(-7.61278773679275,2.83992085048825,10.4696472314219));
#17541=CARTESIAN_POINT('Ctrl Pts',(-7.68614412099281,2.6432792497346,10.4778684931525));
#17542=CARTESIAN_POINT('Ctrl Pts',(-7.7518818652997,2.44378200048974,10.4860897548832));
#17543=CARTESIAN_POINT('Ctrl Pts',(-7.80979878193991,2.24203714244655,10.4943110166138));
#17544=CARTESIAN_POINT('Ctrl Pts',(-7.86772028649138,2.04027630310532,10.5025329295948));
#17545=CARTESIAN_POINT('Ctrl Pts',(-7.91781964157207,1.83626778195898,10.5107548425759));
#17546=CARTESIAN_POINT('Ctrl Pts',(-7.95994469791944,1.63063422279928,10.518976755557));
#17547=CARTESIAN_POINT('Ctrl Pts',(-8.00206963380308,1.42500125168357,10.5271986450261));
#17548=CARTESIAN_POINT('Ctrl Pts',(-8.03622026002123,1.21774354130453,10.5354205344952));
#17549=CARTESIAN_POINT('Ctrl Pts',(-8.06229555673676,1.00949389216715,10.5436424239643));
#17550=CARTESIAN_POINT('Ctrl Pts',(-8.08837628383372,0.801200873435803,
10.5518660257053));
#17551=CARTESIAN_POINT('Ctrl Pts',(-8.10637828512661,0.591915795942659,
10.5600896274462));
#17552=CARTESIAN_POINT('Ctrl Pts',(-8.11625229777714,0.382277649526231,
10.5683132291872));
#17553=CARTESIAN_POINT('Ctrl Pts',(-8.12024080782819,0.297596387342468,
10.5716350720246));
#17554=CARTESIAN_POINT('Ctrl Pts',(-8.12290368527564,0.212857557078161,
10.574956914862));
#17555=CARTESIAN_POINT('Ctrl Pts',(-8.12424009294534,0.128103374972905,
10.5782787576994));
#17556=CARTESIAN_POINT('Ctrl Pts',(-8.12491311392995,0.0854207831386196,
10.5799516528704));
#17557=CARTESIAN_POINT('Ctrl Pts',(-8.12524976576722,0.0427328788580502,
10.5816245480414));
#17558=CARTESIAN_POINT('Ctrl Pts',(-8.12524999987781,4.45603647705344E-5,
10.5832974432124));
#17559=CARTESIAN_POINT('Ctrl Pts',(-8.12591305058771,4.44095313166514E-5,
10.5832974492654));
#17560=CARTESIAN_POINT('Ctrl Pts',(-8.12552057083844,-1.30103839990057,
10.6342808943841));
#17561=CARTESIAN_POINT('Ctrl Pts',(-7.47833086458203,-3.94627513751248,
10.7379206818104));
#17562=CARTESIAN_POINT('Ctrl Pts',(-4.73857352870345,-7.01609149949043,
10.894216811544));
#17563=CARTESIAN_POINT('Ctrl Pts',(-0.826182671114257,-8.42599612481989,
11.0521858384663));
#17564=CARTESIAN_POINT('Ctrl Pts',(2.62202662826466,-7.90340622427413,11.1846637398034));
#17565=CARTESIAN_POINT('Ctrl Pts',(4.3960810936187,-6.86755470903723,11.2644852988333));
#17566=CARTESIAN_POINT('Ctrl Pts',(4.94634499595713,-6.44535064078836,11.2916505155556));
#17567=CARTESIAN_POINT('',(-8.125249999086,-0.000121872618778703,10.4167025567876));
#17568=CARTESIAN_POINT('Ctrl Pts',(-8.12577597885438,-0.000121880508085447,
10.4167025567876));
#17569=CARTESIAN_POINT('Ctrl Pts',(-8.12586828455546,-0.126869683330212,
10.4216689788468));
#17570=CARTESIAN_POINT('Ctrl Pts',(-8.09216383980146,-1.59740819601278,
10.4792917432134));
#17571=CARTESIAN_POINT('Ctrl Pts',(-7.24824502833796,-4.37523271893839,
10.5895708498875));
#17572=CARTESIAN_POINT('Ctrl Pts',(-4.29055725454787,-7.29868675118837,
10.7475398768098));
#17573=CARTESIAN_POINT('Ctrl Pts',(-0.297666946508737,-8.46115357972005,
10.9055089037321));
#17574=CARTESIAN_POINT('Ctrl Pts',(2.94034048028108,-7.76093097353364,11.0313493216566));
#17575=CARTESIAN_POINT('Ctrl Pts',(4.53083127840292,-6.76475033712395,11.1045333972739));
#17576=CARTESIAN_POINT('Ctrl Pts',(4.94641461892554,-6.44544214322681,11.1250611305836));
#17577=CARTESIAN_POINT('Ctrl Pts',(4.94675008185374,-6.44587862049698,9.12505123879043));
#17578=CARTESIAN_POINT('Ctrl Pts',(5.11329136906744,-6.31807011297456,9.13327483954532));
#17579=CARTESIAN_POINT('Ctrl Pts',(5.27486419726295,-6.18381344106902,9.14149844030021));
#17580=CARTESIAN_POINT('Ctrl Pts',(5.43097866278426,-6.04352201343572,9.1497220410551));
#17581=CARTESIAN_POINT('Ctrl Pts',(5.5456881614843,-5.94043893729674,9.15576456323235));
#17582=CARTESIAN_POINT('Ctrl Pts',(5.65745135058914,-5.83409856845521,9.16180708540961));
#17583=CARTESIAN_POINT('Ctrl Pts',(5.76608602502051,-5.7246781144937,9.16784960758686));
#17584=CARTESIAN_POINT('Ctrl Pts',(5.91393181999677,-5.57576291695406,9.1760731467067));
#17585=CARTESIAN_POINT('Ctrl Pts',(6.05602971023113,-5.42109306343681,9.18429668582654));
#17586=CARTESIAN_POINT('Ctrl Pts',(6.19194133522727,-5.26113581497418,9.19252022494639));
#17587=CARTESIAN_POINT('Ctrl Pts',(6.32782824913167,-5.10120764951486,9.20074226888412));
#17588=CARTESIAN_POINT('Ctrl Pts',(6.4575309518339,-4.93599423248227,9.20896431282186));
#17589=CARTESIAN_POINT('Ctrl Pts',(6.58065047508811,-4.76599694578402,9.2171863567596));
#17590=CARTESIAN_POINT('Ctrl Pts',(6.70375640497549,-4.59601842812757,9.22540749291881));
#17591=CARTESIAN_POINT('Ctrl Pts',(6.82028043358262,-4.42125733406629,9.23362862907802));
#17592=CARTESIAN_POINT('Ctrl Pts',(6.92986565501094,-4.24224581631001,9.24184976523723));
#17593=CARTESIAN_POINT('Ctrl Pts',(7.0394595681963,-4.0632201002467,9.25007155345625));
#17594=CARTESIAN_POINT('Ctrl Pts',(7.14211341829752,-3.87994353705425,9.25829334167527));
#17595=CARTESIAN_POINT('Ctrl Pts',(7.23751463638086,-3.69297569050661,9.26651512989428));
#17596=CARTESIAN_POINT('Ctrl Pts',(7.33291558974847,-3.50600836275037,9.27473689529979));
#17597=CARTESIAN_POINT('Ctrl Pts',(7.4210638197075,-3.31535003606191,9.28295866070529));
#17598=CARTESIAN_POINT('Ctrl Pts',(7.50169333110056,-3.12158368919069,9.2911804261108));
#17599=CARTESIAN_POINT('Ctrl Pts',(7.58233965240079,-2.92777694527071,9.29940390561715));
#17600=CARTESIAN_POINT('Ctrl Pts',(7.65546401033655,-2.73086115905672,9.3076273851235));
#17601=CARTESIAN_POINT('Ctrl Pts',(7.72084864568379,-2.53143906759433,9.31585086462984));
#17602=CARTESIAN_POINT('Ctrl Pts',(7.74726645736075,-2.45086516474235,9.31917345458962));
#17603=CARTESIAN_POINT('Ctrl Pts',(7.77242135098286,-2.36988231555596,9.32249604454938));
#17604=CARTESIAN_POINT('Ctrl Pts',(7.79630126137023,-2.28853101452808,9.32581863450915));
#17605=CARTESIAN_POINT('Ctrl Pts',(7.85540496560554,-2.08718338980453,9.33404217350456));
#17606=CARTESIAN_POINT('Ctrl Pts',(7.90671408272067,-1.88351221563601,9.34226571249997));
#17607=CARTESIAN_POINT('Ctrl Pts',(7.95006562244418,-1.67813711040879,9.35048925149539));
#17608=CARTESIAN_POINT('Ctrl Pts',(7.99340928010374,-1.47279934594789,9.35871129530838));
#17609=CARTESIAN_POINT('Ctrl Pts',(8.02879818718711,-1.26575855719513,9.36693333912137));
#17610=CARTESIAN_POINT('Ctrl Pts',(8.05612024024124,-1.0576456104364,9.37515538293436));
#17611=CARTESIAN_POINT('Ctrl Pts',(8.08343927672539,-0.849555640987154,
9.38337651896891));
#17612=CARTESIAN_POINT('Ctrl Pts',(8.10269319894266,-0.640394042174207,
9.39159765500347));
#17613=CARTESIAN_POINT('Ctrl Pts',(8.11382154309571,-0.430798710880048,
9.39981879103802));
#17614=CARTESIAN_POINT('Ctrl Pts',(8.12495076989518,-0.221186755498332,
9.4080405791333));
#17615=CARTESIAN_POINT('Ctrl Pts',(8.12795311261308,-0.0111412932857755,
9.41626236722859));
#17616=CARTESIAN_POINT('Ctrl Pts',(8.12282014757337,0.198696785772053,9.42448415532387));
#17617=CARTESIAN_POINT('Ctrl Pts',(8.11768719677593,0.408534282598971,9.43270592060643));
#17618=CARTESIAN_POINT('Ctrl Pts',(8.10441899328247,0.618164102644243,9.44092768588898));
#17619=CARTESIAN_POINT('Ctrl Pts',(8.08305921775857,0.826946941894175,9.44914945117154));
#17620=CARTESIAN_POINT('Ctrl Pts',(8.06169498907283,1.03577330893178,9.45737293055691));
#17621=CARTESIAN_POINT('Ctrl Pts',(8.0322358483172,1.24375204896069,9.46559640994228));
#17622=CARTESIAN_POINT('Ctrl Pts',(7.99477730100009,1.45024945092688,9.47381988932766));
#17623=CARTESIAN_POINT('Ctrl Pts',(7.97964265845209,1.53368206083007,9.47714248002892));
#17624=CARTESIAN_POINT('Ctrl Pts',(7.96320273148207,1.61687294099377,9.48046507073018));
#17625=CARTESIAN_POINT('Ctrl Pts',(7.94546619198763,1.69978073717804,9.48378766143144));
#17626=CARTESIAN_POINT('Ctrl Pts',(7.90156757781221,1.90498070631346,9.49201120060057));
#17627=CARTESIAN_POINT('Ctrl Pts',(7.84970833035457,2.10851250470891,9.50023473976971));
#17628=CARTESIAN_POINT('Ctrl Pts',(7.79004015499954,2.30975365482873,9.50845827893885));
#17629=CARTESIAN_POINT('Ctrl Pts',(7.73038282835455,2.5109582158142,9.51668032292581));
#17630=CARTESIAN_POINT('Ctrl Pts',(7.66291949136707,2.70987267714272,9.52490236691278));
#17631=CARTESIAN_POINT('Ctrl Pts',(7.58785195310618,2.90588890018918,9.53312441089974));
#17632=CARTESIAN_POINT('Ctrl Pts',(7.51279270289526,3.10188348149425,9.54134554710802));
#17633=CARTESIAN_POINT('Ctrl Pts',(7.43013103300787,3.29498018804166,9.54956668331629));
#17634=CARTESIAN_POINT('Ctrl Pts',(7.34011751013447,3.48458928712085,9.55778781952457));
#17635=CARTESIAN_POINT('Ctrl Pts',(7.25009684784155,3.67421342503929,9.56600960779198));
#17636=CARTESIAN_POINT('Ctrl Pts',(7.15272329154659,3.86034913519876,9.5742313960594));
#17637=CARTESIAN_POINT('Ctrl Pts',(7.04829459525269,4.04242883190684,9.58245318432682));
#17638=CARTESIAN_POINT('Ctrl Pts',(6.94386618872948,4.22450802337678,9.59067494978027));
#17639=CARTESIAN_POINT('Ctrl Pts',(6.83238283043981,4.40253096940976,9.59889671523371));
#17640=CARTESIAN_POINT('Ctrl Pts',(6.71418733783394,4.57595628857733,9.60711848068715));
#17641=CARTESIAN_POINT('Ctrl Pts',(6.59596720345582,4.74941776400707,9.61534196024041));
#17642=CARTESIAN_POINT('Ctrl Pts',(6.47103230535662,4.91827945395025,9.62356543979366));
#17643=CARTESIAN_POINT('Ctrl Pts',(6.33976837071526,5.08202957175363,9.63178891934692));
#17644=CARTESIAN_POINT('Ctrl Pts',(6.28673288977089,5.14819067134376,9.63511150901586));
#17645=CARTESIAN_POINT('Ctrl Pts',(6.23266469135999,5.21351768872211,9.6384340986848));
#17646=CARTESIAN_POINT('Ctrl Pts',(6.17759109212934,5.27797838769204,9.64175668835373));
#17647=CARTESIAN_POINT('Ctrl Pts',(6.0412817856079,5.43752113225969,9.64998022739884));
#17648=CARTESIAN_POINT('Ctrl Pts',(5.89876649961063,5.59180647339974,9.65820376644395));
#17649=CARTESIAN_POINT('Ctrl Pts',(5.75047503249476,5.74035926255094,9.66642730548906));
#17650=CARTESIAN_POINT('Ctrl Pts',(5.60221052733612,5.88888504223203,9.67464934935233));
#17651=CARTESIAN_POINT('Ctrl Pts',(5.44817214542095,6.03168014155998,9.6828713932156));
#17652=CARTESIAN_POINT('Ctrl Pts',(5.28882691690482,6.1683058780773,9.69109343707887));
#17653=CARTESIAN_POINT('Ctrl Pts',(5.12949928134886,6.30491653004416,9.69931457316416));
#17654=CARTESIAN_POINT('Ctrl Pts',(4.96486619276775,6.43535898718115,9.70753570924944));
#17655=CARTESIAN_POINT('Ctrl Pts',(4.79542879292314,6.55923396857466,9.71575684533473));
#17656=CARTESIAN_POINT('Ctrl Pts',(4.62597795411924,6.68311877513566,9.72397863348098));
#17657=CARTESIAN_POINT('Ctrl Pts',(4.45172227920275,6.8004348889347,9.73220042162723));
#17658=CARTESIAN_POINT('Ctrl Pts',(4.27319385933427,6.91082497268219,9.74042220977348));
#17659=CARTESIAN_POINT('Ctrl Pts',(4.09466593482349,7.02121475013348,9.74864397510696));
#17660=CARTESIAN_POINT('Ctrl Pts',(3.91186554134461,7.12467838315912,9.75686574044044));
#17661=CARTESIAN_POINT('Ctrl Pts',(3.72535191994056,7.22090303459998,9.76508750577393));
#17662=CARTESIAN_POINT('Ctrl Pts',(3.53879941351825,7.31714774729588,9.77331098521008));
#17663=CARTESIAN_POINT('Ctrl Pts',(3.34853239480094,7.40615032819317,9.78153446464623));
#17664=CARTESIAN_POINT('Ctrl Pts',(3.15513374641341,7.48764439625329,9.78975794408238));
#17665=CARTESIAN_POINT('Ctrl Pts',(3.07699352643903,7.52057101936011,9.79308053448026));
#17666=CARTESIAN_POINT('Ctrl Pts',(2.9983423235223,7.55227245004202,9.79640312487814));
#17667=CARTESIAN_POINT('Ctrl Pts',(2.91921950827881,7.58273334787558,9.79972571527602));
#17668=CARTESIAN_POINT('Ctrl Pts',(2.7233875024442,7.6581252396316,9.80794925408946));
#17669=CARTESIAN_POINT('Ctrl Pts',(2.5246015167032,7.72593897414762,9.8161727929029));
#17670=CARTESIAN_POINT('Ctrl Pts',(2.32346574288007,7.78596137314865,9.82439633171635));
#17671=CARTESIAN_POINT('Ctrl Pts',(2.12236653907767,7.84597285902202,9.83261837534582));
#17672=CARTESIAN_POINT('Ctrl Pts',(1.91891868238004,7.89819575245895,9.84084041897529));
#17673=CARTESIAN_POINT('Ctrl Pts',(1.71374174143379,7.94246667013262,9.84906246260476));
#17674=CARTESIAN_POINT('Ctrl Pts',(1.50858745366323,7.9867326999428,9.85728359845484));
#17675=CARTESIAN_POINT('Ctrl Pts',(1.30170475096606,8.02304844462583,9.86550473430492));
#17676=CARTESIAN_POINT('Ctrl Pts',(1.09372443731284,8.05130141143186,9.873725870155));
#17677=CARTESIAN_POINT('Ctrl Pts',(0.885727627668747,8.07955661912634,9.88194765806574));
#17678=CARTESIAN_POINT('Ctrl Pts',(0.676633325022578,8.09974772883555,9.89016944597649));
#17679=CARTESIAN_POINT('Ctrl Pts',(0.467079577523585,8.11181386810375,9.89839123388723));
#17680=CARTESIAN_POINT('Ctrl Pts',(0.257526411458404,8.12387997389291,9.90661299898557));
#17681=CARTESIAN_POINT('Ctrl Pts',(0.0475140976898377,8.12782114007451,
9.91483476408391));
#17682=CARTESIAN_POINT('Ctrl Pts',(-0.162316629894777,8.12362855343347,
9.92305652918225));
#17683=CARTESIAN_POINT('Ctrl Pts',(-0.372191103778895,8.11943509270619,
9.93128000838511));
#17684=CARTESIAN_POINT('Ctrl Pts',(-0.581883620923186,8.10710449741623,
9.93950348758796));
#17685=CARTESIAN_POINT('Ctrl Pts',(-0.79075477812074,8.08668006312722,9.94772696679081));
#17686=CARTESIAN_POINT('Ctrl Pts',(-0.875146503029868,8.07842783116245,
9.95104955859331));
#17687=CARTESIAN_POINT('Ctrl Pts',(-0.959404188540645,8.06885490375017,
9.95437215039581));
#17688=CARTESIAN_POINT('Ctrl Pts',(-1.04348590916689,8.05796653752484,9.95769474219831));
#17689=CARTESIAN_POINT('Ctrl Pts',(-1.25159134012213,8.03101742029885,9.96591828227097));
#17690=CARTESIAN_POINT('Ctrl Pts',(-1.45868603051667,7.99599780690685,9.97414182234363));
#17691=CARTESIAN_POINT('Ctrl Pts',(-1.66413717105161,7.95300792395081,9.98236536241628));
#17692=CARTESIAN_POINT('Ctrl Pts',(-1.86955095712071,7.91002585727707,9.99058740731132));
#17693=CARTESIAN_POINT('Ctrl Pts',(-2.07332150121117,7.85907647371045,9.99880945220635));
#17694=CARTESIAN_POINT('Ctrl Pts',(-2.27482618222162,7.80031110938397,10.0070314971014));
#17695=CARTESIAN_POINT('Ctrl Pts',(-2.47630861555574,7.74155223320853,10.015252634219));
#17696=CARTESIAN_POINT('Ctrl Pts',(-2.6755254022331,7.67497918165133,10.0234737713367));
#17697=CARTESIAN_POINT('Ctrl Pts',(-2.87186827291337,7.60079339184625,10.0316949084543));
#17698=CARTESIAN_POINT('Ctrl Pts',(-3.06822671641337,7.52660171803872,10.0399166976267));
#17699=CARTESIAN_POINT('Ctrl Pts',(-3.26171051162318,7.44479620130437,10.048138486799));
#17700=CARTESIAN_POINT('Ctrl Pts',(-3.45172959808347,7.35562712106959,10.0563602759713));
#17701=CARTESIAN_POINT('Ctrl Pts',(-3.64174815717429,7.26645828831022,10.0645820423253));
#17702=CARTESIAN_POINT('Ctrl Pts',(-3.82830176090006,7.16992606066323,10.0728038086793));
#17703=CARTESIAN_POINT('Ctrl Pts',(-4.0108227752078,7.06632777532817,10.0810255750332));
#17704=CARTESIAN_POINT('Ctrl Pts',(-4.19338184180514,6.96270789164746,10.089249055475));
#17705=CARTESIAN_POINT('Ctrl Pts',(-4.37190638292323,6.85201915297229,10.0974725359167));
#17706=CARTESIAN_POINT('Ctrl Pts',(-4.54585474639135,6.73460408540927,10.1056960163584));
#17707=CARTESIAN_POINT('Ctrl Pts',(-4.61613619201214,6.68716414104035,10.1090186006125));
#17708=CARTESIAN_POINT('Ctrl Pts',(-4.68567091912808,6.63862665464677,10.1123411848665));
#17709=CARTESIAN_POINT('Ctrl Pts',(-4.75442456323019,6.58901621147296,10.1156637691206));
#17710=CARTESIAN_POINT('Ctrl Pts',(-4.92459274213244,6.46622826503502,10.1238873057658));
#17711=CARTESIAN_POINT('Ctrl Pts',(-5.09002932993603,6.33682469759667,10.1321108424109));
#17712=CARTESIAN_POINT('Ctrl Pts',(-5.25022558127162,6.20119495809164,10.1403343790561));
#17713=CARTESIAN_POINT('Ctrl Pts',(-5.41039270596633,6.06558987858133,10.1485564205103));
#17714=CARTESIAN_POINT('Ctrl Pts',(-5.56532117086996,5.92376107689451,10.1567784619644));
#17715=CARTESIAN_POINT('Ctrl Pts',(-5.71453552566292,5.77613809464736,10.1650005034185));
#17716=CARTESIAN_POINT('Ctrl Pts',(-5.86373340599093,5.62853141116482,10.1732216370932));
#17717=CARTESIAN_POINT('Ctrl Pts',(-6.00721822616031,5.47513203165639,10.1814427707678));
#17718=CARTESIAN_POINT('Ctrl Pts',(-6.14455101197339,5.31640672106233,10.1896639044424));
#17719=CARTESIAN_POINT('Ctrl Pts',(-6.28189469062889,5.1576688208322,10.1978856901938));
#17720=CARTESIAN_POINT('Ctrl Pts',(-6.41308516494823,4.99360436675842,10.2061074759451));
#17721=CARTESIAN_POINT('Ctrl Pts',(-6.53772272932725,4.82471440366555,10.2143292616965));
#17722=CARTESIAN_POINT('Ctrl Pts',(-6.66235994808432,4.65582490890724,10.2225510246487));
#17723=CARTESIAN_POINT('Ctrl Pts',(-6.78044412029115,4.48211017080621,10.2307727876009));
#17724=CARTESIAN_POINT('Ctrl Pts',(-6.89161766797295,4.3041019366394,10.2389945505531));
#17725=CARTESIAN_POINT('Ctrl Pts',(-7.00281439398958,4.12605658991714,10.2472180276431));
#17726=CARTESIAN_POINT('Ctrl Pts',(-7.10709746095352,3.94371620909176,10.2554415047331));
#17727=CARTESIAN_POINT('Ctrl Pts',(-7.20415365520637,3.75763990753195,10.263664981823));
#17728=CARTESIAN_POINT('Ctrl Pts',(-7.2433681343784,3.68245784101783,10.266987586563));
#17729=CARTESIAN_POINT('Ctrl Pts',(-7.28140336517111,3.6066661814362,10.2703101913029));
#17730=CARTESIAN_POINT('Ctrl Pts',(-7.31824083470849,3.53030291160762,10.2736327960429));
#17731=CARTESIAN_POINT('Ctrl Pts',(-7.40911983224593,3.34191273449019,10.2818297485419));
#17732=CARTESIAN_POINT('Ctrl Pts',(-7.49273708782956,3.14997699955855,10.2900267010408));
#17733=CARTESIAN_POINT('Ctrl Pts',(-7.56883154281126,2.9550764184781,10.2982236535398));
#17734=CARTESIAN_POINT('Ctrl Pts',(-7.64491133611954,2.76021339031354,10.3064190266722));
#17735=CARTESIAN_POINT('Ctrl Pts',(-7.71347111297681,2.56238693425361,10.3146143998045));
#17736=CARTESIAN_POINT('Ctrl Pts',(-7.77429815698699,2.36219722478219,10.3228097729369));
#17737=CARTESIAN_POINT('Ctrl Pts',(-7.83512569348692,2.16200589446299,10.3310052124236));
#17738=CARTESIAN_POINT('Ctrl Pts',(-7.8882202811252,1.95945155713435,10.3392006519102));
#17739=CARTESIAN_POINT('Ctrl Pts',(-7.93341893815651,1.75514999763543,10.3473960913969));
#17740=CARTESIAN_POINT('Ctrl Pts',(-7.97861499566341,1.55086018819557,10.3555910595368));
#17741=CARTESIAN_POINT('Ctrl Pts',(-8.01591596665708,1.34482364940534,10.3637860276766));
#17742=CARTESIAN_POINT('Ctrl Pts',(-8.04520979307792,1.13766732741303,10.3719809958164));
#17743=CARTESIAN_POINT('Ctrl Pts',(-8.07451001198787,0.930465799836723,
10.3801777522595));
#17744=CARTESIAN_POINT('Ctrl Pts',(-8.09579955145645,0.722144296566263,
10.3883745087025));
#17745=CARTESIAN_POINT('Ctrl Pts',(-8.10901798322321,0.513337033792121,
10.3965712651456));
#17746=CARTESIAN_POINT('Ctrl Pts',(-8.11983950377611,0.342392997043054,
10.4032816956929));
#17747=CARTESIAN_POINT('Ctrl Pts',(-8.12525256763878,0.171123594131868,
10.4099921262403));
#17748=CARTESIAN_POINT('Ctrl Pts',(-8.125249999086,-0.000121872618778703,
10.4167025567876));
#17749=CARTESIAN_POINT('Origin',(0.,0.,-16.4167025567876));
#17750=CARTESIAN_POINT('',(4.94675008185378,-6.44587862049694,7.1250592150305));
#17751=CARTESIAN_POINT('',(4.94684221335274,-6.44599857519204,7.2916588140437));
#17752=CARTESIAN_POINT('',(4.94675008185374,-6.44587862049697,-16.4167025567876));
#17753=CARTESIAN_POINT('',(-8.12524999873121,0.000143591189764823,8.58329744321241));
#17754=CARTESIAN_POINT('Ctrl Pts',(4.94684221335274,-6.44599857519204,7.2916588140437));
#17755=CARTESIAN_POINT('Ctrl Pts',(5.8049765999933,-5.78602921714794,7.33407194911367));
#17756=CARTESIAN_POINT('Ctrl Pts',(7.43356999167247,-3.92084680041933,7.42914142649105));
#17757=CARTESIAN_POINT('Ctrl Pts',(8.46465994169792,-0.171018365282867,
7.57686724617588));
#17758=CARTESIAN_POINT('Ctrl Pts',(7.52493661231736,3.8800830133467,7.73483627309817));
#17759=CARTESIAN_POINT('Ctrl Pts',(4.76963640343018,6.99501849808588,7.89280530002046));
#17760=CARTESIAN_POINT('Ctrl Pts',(0.863543566747498,8.42223294139058,8.05077432694274));
#17761=CARTESIAN_POINT('Ctrl Pts',(-3.25090049128004,7.81737559566535,8.20874335386504));
#17762=CARTESIAN_POINT('Ctrl Pts',(-6.58098448454454,5.32638324072316,8.36671238078732));
#17763=CARTESIAN_POINT('Ctrl Pts',(-7.95798473996769,2.34191872576517,8.49156374016535));
#17764=CARTESIAN_POINT('Ctrl Pts',(-8.12506463397728,0.498971488914468,
8.56375875723593));
#17765=CARTESIAN_POINT('Ctrl Pts',(-8.12474591487583,0.000143868560570458,
8.58329743199909));
#17766=CARTESIAN_POINT('Ctrl Pts',(-8.12524999873121,0.000143591189764823,
8.58329744321241));
#17767=CARTESIAN_POINT('Ctrl Pts',(-8.12525373444067,-0.211245236214326,
8.59157685916403));
#17768=CARTESIAN_POINT('Ctrl Pts',(-8.11700370973027,-0.422638087073884,
8.59985627511566));
#17769=CARTESIAN_POINT('Ctrl Pts',(-8.10052557183335,-0.633382208918111,
8.60813569106728));
#17770=CARTESIAN_POINT('Ctrl Pts',(-8.08412976794414,-0.843073335074187,
8.61637373841882));
#17771=CARTESIAN_POINT('Ctrl Pts',(-8.05958793823209,-1.05212190871435,
8.62461178577036));
#17772=CARTESIAN_POINT('Ctrl Pts',(-8.0269774401061,-1.25988917708176,8.6328498331219));
#17773=CARTESIAN_POINT('Ctrl Pts',(-7.99412130416121,-1.46922144756729,
8.64114993337356));
#17774=CARTESIAN_POINT('Ctrl Pts',(-7.95307447349202,-1.67725273047273,
8.64945003362523));
#17775=CARTESIAN_POINT('Ctrl Pts',(-7.90396883610218,-1.88333857827675,
8.6577501338769));
#17776=CARTESIAN_POINT('Ctrl Pts',(-7.85486319871234,-2.08942442608081,
8.66605023412856));
#17777=CARTESIAN_POINT('Ctrl Pts',(-7.79769883263737,-2.29356454561377,
8.67435033438023));
#17778=CARTESIAN_POINT('Ctrl Pts',(-7.73265961988368,-2.49512780544812,
8.6826504346319));
#17779=CARTESIAN_POINT('Ctrl Pts',(-7.66822033769495,-2.6948318182955,8.69087397362733));
#17780=CARTESIAN_POINT('Ctrl Pts',(-7.59603010807265,-2.89207061628817,
8.69909751262277));
#17781=CARTESIAN_POINT('Ctrl Pts',(-7.51630285168063,-3.08624027002397,
8.7073210516182));
#17782=CARTESIAN_POINT('Ctrl Pts',(-7.43659009109071,-3.28037462033905,
8.71554309543119));
#17783=CARTESIAN_POINT('Ctrl Pts',(-7.3493431507886,-3.47144066745328,8.72376513924418));
#17784=CARTESIAN_POINT('Ctrl Pts',(-7.2548243468166,-3.65885381770537,8.73198718305717));
#17785=CARTESIAN_POINT('Ctrl Pts',(-7.16031597846581,-3.84624627606796,
8.7402083190917));
#17786=CARTESIAN_POINT('Ctrl Pts',(-7.058537482107,-4.02998637952217,8.74842945512621));
#17787=CARTESIAN_POINT('Ctrl Pts',(-6.94979781843153,-4.20951278005239,
8.75665059116074));
#17788=CARTESIAN_POINT('Ctrl Pts',(-6.84104953005183,-4.38905341974846,
8.76487237925602));
#17789=CARTESIAN_POINT('Ctrl Pts',(-6.72533912169375,-4.56437943508953,
8.77309416735129));
#17790=CARTESIAN_POINT('Ctrl Pts',(-6.60302025785466,-4.73495628668956,
8.78131595544657));
#17791=CARTESIAN_POINT('Ctrl Pts',(-6.48070173341022,-4.90553266499488,
8.78953772072908));
#17792=CARTESIAN_POINT('Ctrl Pts',(-6.35177496422567,-5.07135966781209,
8.79775948601159));
#17793=CARTESIAN_POINT('Ctrl Pts',(-6.21663579505286,-5.2319333858687,8.80598125129411));
#17794=CARTESIAN_POINT('Ctrl Pts',(-6.08146845158538,-5.39254058090519,
8.81420473067949));
#17795=CARTESIAN_POINT('Ctrl Pts',(-5.94008631066937,-5.54789207754479,
8.82242821006488));
#17796=CARTESIAN_POINT('Ctrl Pts',(-5.79292491153289,-5.69751775177942,
8.83065168945026));
#17797=CARTESIAN_POINT('Ctrl Pts',(-5.73346624769379,-5.75797207416436,
8.83397428015158));
#17798=CARTESIAN_POINT('Ctrl Pts',(-5.67306457586728,-5.81749208577385,
8.83729687085289));
#17799=CARTESIAN_POINT('Ctrl Pts',(-5.611750334763,-5.87604848029587,8.8406194615542));
#17800=CARTESIAN_POINT('Ctrl Pts',(-5.45999524102061,-6.02097779818127,
8.84884300072332));
#17801=CARTESIAN_POINT('Ctrl Pts',(-5.30259807197871,-6.16004866386615,
8.85706653989244));
#17802=CARTESIAN_POINT('Ctrl Pts',(-5.14003450407988,-6.29283186326858,
8.86529007906155));
#17803=CARTESIAN_POINT('Ctrl Pts',(-4.97750049305847,-6.42559092038131,
8.87351212304855));
#17804=CARTESIAN_POINT('Ctrl Pts',(-4.80980218630475,-6.55206440643836,
8.88173416703556));
#17805=CARTESIAN_POINT('Ctrl Pts',(-4.63744861058498,-6.67186315407349,
8.88995621102256));
#17806=CARTESIAN_POINT('Ctrl Pts',(-4.46511406406289,-6.79164867497955,
8.89817734723088));
#17807=CARTESIAN_POINT('Ctrl Pts',(-4.28812551679848,-6.90476076047794,
8.9063984834392));
#17808=CARTESIAN_POINT('Ctrl Pts',(-4.10702194464438,-7.01085289452784,
8.91461961964752));
#17809=CARTESIAN_POINT('Ctrl Pts',(-3.92590400826825,-7.11695344327079,
8.92284140791492));
#17810=CARTESIAN_POINT('Ctrl Pts',(-3.74067064801074,-7.21603277668371,
8.93106319618231));
#17811=CARTESIAN_POINT('Ctrl Pts',(-3.55188738558178,-7.30778923906848,
8.9392849844497));
#17812=CARTESIAN_POINT('Ctrl Pts',(-3.36310464699317,-7.3995454468452,8.94750674990307));
#17813=CARTESIAN_POINT('Ctrl Pts',(-3.17077229237575,-7.4839786977384,8.95572851535645));
#17814=CARTESIAN_POINT('Ctrl Pts',(-2.97547835057054,-7.56083435526702,
8.96395028080983));
#17815=CARTESIAN_POINT('Ctrl Pts',(-2.78014369326115,-7.63770603590836,
8.9721737603631));
#17816=CARTESIAN_POINT('Ctrl Pts',(-2.58184648978833,-7.70699685917193,
8.98039723991638));
#17817=CARTESIAN_POINT('Ctrl Pts',(-2.38119358789019,-7.76850079870567,
8.98862071946965));
#17818=CARTESIAN_POINT('Ctrl Pts',(-2.30012239964538,-7.79335066338527,
8.9919433091386));
#17819=CARTESIAN_POINT('Ctrl Pts',(-2.21866684018557,-7.81692991511405,
8.99526589880754));
#17820=CARTESIAN_POINT('Ctrl Pts',(-2.13686763041389,-7.83922727649794,
8.99858848847649));
#17821=CARTESIAN_POINT('Ctrl Pts',(-1.93441139523571,-7.8944141157448,9.0068120275216));
#17822=CARTESIAN_POINT('Ctrl Pts',(-1.72978324732373,-7.94176276214306,
9.01503556656671));
#17823=CARTESIAN_POINT('Ctrl Pts',(-1.52360585017358,-7.98112227545831,
9.02325910561183));
#17824=CARTESIAN_POINT('Ctrl Pts',(-1.31746593964419,-8.02047463253253,
9.03148114947515));
#17825=CARTESIAN_POINT('Ctrl Pts',(-1.10977763163798,-8.05184070039555,
9.03970319333847));
#17826=CARTESIAN_POINT('Ctrl Pts',(-0.901173848330154,-8.07512063424354,
9.04792523720179));
#17827=CARTESIAN_POINT('Ctrl Pts',(-0.692593096515015,-8.09839799780437,
9.05614637328703));
#17828=CARTESIAN_POINT('Ctrl Pts',(-0.483097364193052,-8.11359097703911,
9.06436750937227));
#17829=CARTESIAN_POINT('Ctrl Pts',(-0.273325601106056,-8.12065149346282,
9.07258864545751));
#17830=CARTESIAN_POINT('Ctrl Pts',(-0.0635371999307712,-8.12771256989277,
9.08081043360376));
#17831=CARTESIAN_POINT('Ctrl Pts',(0.146526981067496,-8.1266398821167,9.08903222175));
#17832=CARTESIAN_POINT('Ctrl Pts',(0.356226009082313,-8.11743744003939,
9.09725400989625));
#17833=CARTESIAN_POINT('Ctrl Pts',(0.565924455252275,-8.10823502349579,
9.10547577522978));
#17834=CARTESIAN_POINT('Ctrl Pts',(0.775257455935232,-8.09090291339795,
9.11369754056332));
#17835=CARTESIAN_POINT('Ctrl Pts',(0.983586674719125,-8.06549718342366,
9.12191930589685));
#17836=CARTESIAN_POINT('Ctrl Pts',(1.19195932671374,-8.04008615677312,9.13014278533304));
#17837=CARTESIAN_POINT('Ctrl Pts',(1.39932748592745,-8.00659818337073,9.13836626476921));
#17838=CARTESIAN_POINT('Ctrl Pts',(1.60505941315471,-7.96514104349342,9.14658974420539));
#17839=CARTESIAN_POINT('Ctrl Pts',(1.68818273476456,-7.94839082286656,9.14991233460318));
#17840=CARTESIAN_POINT('Ctrl Pts',(1.7710390522369,-7.93034025273445,9.15323492500098));
#17841=CARTESIAN_POINT('Ctrl Pts',(1.85358718734214,-7.91099880555047,9.15655751539878));
#17842=CARTESIAN_POINT('Ctrl Pts',(2.05789534233786,-7.86312836748343,9.16478098783841));
#17843=CARTESIAN_POINT('Ctrl Pts',(2.26038124965037,-7.80733128189522,9.17300446027803));
#17844=CARTESIAN_POINT('Ctrl Pts',(2.46042550664494,-7.74377129625811,9.18122793271765));
#17845=CARTESIAN_POINT('Ctrl Pts',(2.66043274840183,-7.68022307145837,9.18944988352506));
#17846=CARTESIAN_POINT('Ctrl Pts',(2.85799896066828,-7.60891490290157,9.19767183433247));
#17847=CARTESIAN_POINT('Ctrl Pts',(3.05252005421146,-7.53006035043126,9.20589378513987));
#17848=CARTESIAN_POINT('Ctrl Pts',(3.24703585258523,-7.4512079445056,9.21411551213287));
#17849=CARTESIAN_POINT('Ctrl Pts',(3.43850642331368,-7.36480967276742,9.22233723912587));
#17850=CARTESIAN_POINT('Ctrl Pts',(3.62634687940736,-7.27112755167398,9.23055896611887));
#17851=CARTESIAN_POINT('Ctrl Pts',(3.81417466180681,-7.17745175136246,9.23878013838763));
#17852=CARTESIAN_POINT('Ctrl Pts',(3.99837255546468,-7.07649321608515,9.2470013106564));
#17853=CARTESIAN_POINT('Ctrl Pts',(4.17837898390298,-6.96856058518385,9.25522248292517));
#17854=CARTESIAN_POINT('Ctrl Pts',(4.35840773699178,-6.86061456832582,9.26344467479528));
#17855=CARTESIAN_POINT('Ctrl Pts',(4.53424373298925,-6.74569287891959,9.27166686666539));
#17856=CARTESIAN_POINT('Ctrl Pts',(4.70535225921246,-6.62414882677195,9.2798890585355));
#17857=CARTESIAN_POINT('Ctrl Pts',(4.78691031392296,-6.56621543985316,9.28380812668006));
#17858=CARTESIAN_POINT('Ctrl Pts',(4.86739475154616,-6.50677815177985,9.28772719482462));
#17859=CARTESIAN_POINT('Ctrl Pts',(4.94675008185378,-6.44587862049695,9.29164626296917));
#17860=CARTESIAN_POINT('',(-8.12524999739701,0.000205669423076638,8.41670255675951));
#17861=CARTESIAN_POINT('Ctrl Pts',(-8.12524999739703,0.000205668705097187,
8.41670255678763));
#17862=CARTESIAN_POINT('Ctrl Pts',(-8.12525529312676,-0.209010060191446,
8.42489859465923));
#17863=CARTESIAN_POINT('Ctrl Pts',(-8.11717565384267,-0.418248871417476,
8.43309463253084));
#17864=CARTESIAN_POINT('Ctrl Pts',(-8.10103180470332,-0.626874199249931,
8.44129067040245));
#17865=CARTESIAN_POINT('Ctrl Pts',(-8.08488735073895,-0.835507343174935,
8.44948701533644));
#17866=CARTESIAN_POINT('Ctrl Pts',(-8.06067810215077,-1.04352665968774,
8.45768336027043));
#17867=CARTESIAN_POINT('Ctrl Pts',(-8.02847678956486,-1.25029916496744,
8.46587970520442));
#17868=CARTESIAN_POINT('Ctrl Pts',(-7.99627686368355,-1.45706276587775,
8.47407569717425));
#17869=CARTESIAN_POINT('Ctrl Pts',(-7.95608560916812,-1.6625793679671,8.48227168914408));
#17870=CARTESIAN_POINT('Ctrl Pts',(-7.90802724461236,-1.86622417221745,
8.49046768111391));
#17871=CARTESIAN_POINT('Ctrl Pts',(-7.85995700677275,-2.06991928888659,
8.49866569798284));
#17872=CARTESIAN_POINT('Ctrl Pts',(-7.80401584222756,-2.27174139244837,
8.50686371485177));
#17873=CARTESIAN_POINT('Ctrl Pts',(-7.74037870259076,-2.47107772095079,
8.5150617317207));
#17874=CARTESIAN_POINT('Ctrl Pts',(-7.68626947378545,-2.64056891853931,
8.52203232111304));
#17875=CARTESIAN_POINT('Ctrl Pts',(-7.62659715252873,-2.80826308622982,
8.52900291050538));
#17876=CARTESIAN_POINT('Ctrl Pts',(-7.56149739431627,-2.97379298510308,
8.53597349989771));
#17877=CARTESIAN_POINT('Ctrl Pts',(-7.48469608310022,-3.16907655647114,
8.54419703897036));
#17878=CARTESIAN_POINT('Ctrl Pts',(-7.40031315177781,-3.36141504559831,
8.552420578043));
#17879=CARTESIAN_POINT('Ctrl Pts',(-7.30859986802793,-3.55021908219227,
8.56064411711565));
#17880=CARTESIAN_POINT('Ctrl Pts',(-7.21690325934615,-3.73898879093273,
8.56886616100604));
#17881=CARTESIAN_POINT('Ctrl Pts',(-7.1178790871281,-3.92422506458559,8.57708820489644));
#17882=CARTESIAN_POINT('Ctrl Pts',(-7.0118257105885,-4.10536085707822,8.58531024878684));
#17883=CARTESIAN_POINT('Ctrl Pts',(-6.90578404317839,-4.28647665075028,
8.59353138489872));
#17884=CARTESIAN_POINT('Ctrl Pts',(-6.79271486982163,-4.46349261269185,
8.60175252101061));
#17885=CARTESIAN_POINT('Ctrl Pts',(-6.67296164946673,-4.63586781382367,
8.60997365712249));
#17886=CARTESIAN_POINT('Ctrl Pts',(-6.55319893087479,-4.80825668690949,
8.61819544529449));
#17887=CARTESIAN_POINT('Ctrl Pts',(-6.42675127210854,-4.97600381998557,
8.62641723346649));
#17888=CARTESIAN_POINT('Ctrl Pts',(-6.29400507200062,-5.13859783560948,
8.63463902163849));
#17889=CARTESIAN_POINT('Ctrl Pts',(-6.16125924022752,-5.30119140007895,
8.64286078699726));
#17890=CARTESIAN_POINT('Ctrl Pts',(-6.02221509068316,-5.45863164894251,
8.65108255235602));
#17891=CARTESIAN_POINT('Ctrl Pts',(-5.87729920450196,-5.61044041259335,
8.65930431771478));
#17892=CARTESIAN_POINT('Ctrl Pts',(-5.73235310576378,-5.76228082585171,
8.66752779717516));
#17893=CARTESIAN_POINT('Ctrl Pts',(-5.58153302855493,-5.90848719506552,
8.67575127663554));
#17894=CARTESIAN_POINT('Ctrl Pts',(-5.42530305809643,-6.04861755199562,
8.68397475609592));
#17895=CARTESIAN_POINT('Ctrl Pts',(-5.36218036438097,-6.10523540563009,
8.68729734633727));
#17896=CARTESIAN_POINT('Ctrl Pts',(-5.29817493400528,-6.16086180795296,
8.69061993657863));
#17897=CARTESIAN_POINT('Ctrl Pts',(-5.23331897871228,-6.2154694134514,8.69394252681999));
#17898=CARTESIAN_POINT('Ctrl Pts',(-5.07279798642728,-6.35062534448837,
8.70216606589345));
#17899=CARTESIAN_POINT('Ctrl Pts',(-4.9070123093046,-6.47958147178438,8.71038960496692));
#17900=CARTESIAN_POINT('Ctrl Pts',(-4.7364635329758,-6.60193916688804,8.71861314404039));
#17901=CARTESIAN_POINT('Ctrl Pts',(-4.56594576537733,-6.72427461523712,
8.72683518793159));
#17902=CARTESIAN_POINT('Ctrl Pts',(-4.39066686656009,-6.84001385403544,
8.73505723182279));
#17903=CARTESIAN_POINT('Ctrl Pts',(-4.21115920295708,-6.94880030867558,
8.74327927571399));
#17904=CARTESIAN_POINT('Ctrl Pts',(-4.03167135841674,-7.05757475243263,
8.75150041182666));
#17905=CARTESIAN_POINT('Ctrl Pts',(-3.84795593335041,-7.15939779180149,
8.75972154793934));
#17906=CARTESIAN_POINT('Ctrl Pts',(-3.66057251753701,-7.25395729284042,
8.76794268405202));
#17907=CARTESIAN_POINT('Ctrl Pts',(-3.47317423939208,-7.34852429387421,
8.7761644722248));
#17908=CARTESIAN_POINT('Ctrl Pts',(-3.28210765132299,-7.43582647021802,
8.78438626039758));
#17909=CARTESIAN_POINT('Ctrl Pts',(-3.08795603174893,-7.51559812047487,
8.79260804857036));
#17910=CARTESIAN_POINT('Ctrl Pts',(-2.89380495089375,-7.5953695493867,8.80082981392988));
#17911=CARTESIAN_POINT('Ctrl Pts',(-2.6965691294845,-7.66761038441627,8.80905157928939));
#17912=CARTESIAN_POINT('Ctrl Pts',(-2.49685136875701,-7.73210325880586,
8.81727334464891));
#17913=CARTESIAN_POINT('Ctrl Pts',(-2.29709197019225,-7.79660957888901,
8.82549682411));
#17914=CARTESIAN_POINT('Ctrl Pts',(-2.09484987931887,-7.85336462073605,
8.83372030357109));
#17915=CARTESIAN_POINT('Ctrl Pts',(-1.89074363968878,-7.90220070938953,
8.84194378303218));
#17916=CARTESIAN_POINT('Ctrl Pts',(-1.80827716035315,-7.9219322977186,8.84526637326888));
#17917=CARTESIAN_POINT('Ctrl Pts',(-1.72550651753203,-7.9403717234113,8.84858896350558));
#17918=CARTESIAN_POINT('Ctrl Pts',(-1.64247305766683,-7.95751027755155,
8.85191155374228));
#17919=CARTESIAN_POINT('Ctrl Pts',(-1.43696203959017,-7.99992886055946,
8.86013509282285));
#17920=CARTESIAN_POINT('Ctrl Pts',(-1.22977350723855,-8.0343887741463,8.86835863190342));
#17921=CARTESIAN_POINT('Ctrl Pts',(-1.02153834427083,-8.06077831066482,
8.87658217098399));
#17922=CARTESIAN_POINT('Ctrl Pts',(-0.813341042072039,-8.08716304910731,
8.88480421488234));
#17923=CARTESIAN_POINT('Ctrl Pts',(-0.604097781515014,-8.10548030205177,
8.89302625878069));
#17924=CARTESIAN_POINT('Ctrl Pts',(-0.394446489696768,-8.11566999879036,
8.90124830267904));
#17925=CARTESIAN_POINT('Ctrl Pts',(-0.184818345032949,-8.12585857050614,
8.90946943879896));
#17926=CARTESIAN_POINT('Ctrl Pts',(0.0252174464794002,-8.12792136322245,
8.91769057491888));
#17927=CARTESIAN_POINT('Ctrl Pts',(0.23502017909011,-8.12185034816084,8.9259117110388));
#17928=CARTESIAN_POINT('Ctrl Pts',(0.444839552220188,-8.11577885157623,
8.93413349921875));
#17929=CARTESIAN_POINT('Ctrl Pts',(0.654425534617284,-8.10157226405988,
8.9423552873987));
#17930=CARTESIAN_POINT('Ctrl Pts',(0.863138698604562,-8.07927466728736,
8.95057707557865));
#17931=CARTESIAN_POINT('Ctrl Pts',(1.07185128346766,-8.05697713238481,8.9587988409453));
#17932=CARTESIAN_POINT('Ctrl Pts',(1.27969076178868,-8.02658866714655,8.96702060631194));
#17933=CARTESIAN_POINT('Ctrl Pts',(1.48602355292116,-7.98820515276514,8.97524237167858));
#17934=CARTESIAN_POINT('Ctrl Pts',(1.69239936101312,-7.94981363605858,8.98346585114673));
#17935=CARTESIAN_POINT('Ctrl Pts',(1.89726756438602,-7.90342379430053,8.99168933061488));
#17936=CARTESIAN_POINT('Ctrl Pts',(2.10000440007057,-7.84918270154188,8.99991281008302));
#17937=CARTESIAN_POINT('Ctrl Pts',(2.18191758837314,-7.82726729169603,9.00323540027687));
#17938=CARTESIAN_POINT('Ctrl Pts',(2.26348298004169,-7.80407077408141,9.00655799047072));
#17939=CARTESIAN_POINT('Ctrl Pts',(2.34466006978829,-7.77960517761926,9.00988058066456));
#17940=CARTESIAN_POINT('Ctrl Pts',(2.54557448666919,-7.71905248889661,9.01810403722619));
#17941=CARTESIAN_POINT('Ctrl Pts',(2.74417455196863,-7.65070264728471,9.02632749378782));
#17942=CARTESIAN_POINT('Ctrl Pts',(2.93985231848861,-7.57475781183644,9.03455095034945));
#17943=CARTESIAN_POINT('Ctrl Pts',(3.13550499087003,-7.49882271571756,9.04277335231728));
#17944=CARTESIAN_POINT('Ctrl Pts',(3.32823583684251,-7.41529467444085,9.05099575428512));
#17945=CARTESIAN_POINT('Ctrl Pts',(3.51745520753185,-7.32442464808718,9.05921815625295));
#17946=CARTESIAN_POINT('Ctrl Pts',(3.70664939863717,-7.2335667138859,9.0674394640587));
#17947=CARTESIAN_POINT('Ctrl Pts',(3.89233278190311,-7.13536887353303,9.07566077186445));
#17948=CARTESIAN_POINT('Ctrl Pts',(4.07393808722629,-7.03012916125635,9.0838820796702));
#17949=CARTESIAN_POINT('Ctrl Pts',(4.25555288501596,-6.92488394812473,9.09210381720177));
#17950=CARTESIAN_POINT('Ctrl Pts',(4.43308892276975,-6.81259627380045,9.10032555473332));
#17951=CARTESIAN_POINT('Ctrl Pts',(4.606004912716,-6.69360936315648,9.10854729226489));
#17952=CARTESIAN_POINT('Ctrl Pts',(4.72170617580161,-6.61399303700617,9.1140486077734));
#17953=CARTESIAN_POINT('Ctrl Pts',(4.83533949743165,-6.53137826299053,9.11954992328192));
#17954=CARTESIAN_POINT('Ctrl Pts',(4.94675008185374,-6.44587862049698,9.12505123879043));
#17955=CARTESIAN_POINT('Ctrl Pts',(4.94675008185378,-6.44587862049694,7.1250592150305));
#17956=CARTESIAN_POINT('Ctrl Pts',(5.11322900588198,-6.31811797225193,7.1332820268424));
#17957=CARTESIAN_POINT('Ctrl Pts',(5.27477905707631,-6.18388645837806,7.1415048386543));
#17958=CARTESIAN_POINT('Ctrl Pts',(5.43090386575413,-6.04358922854928,7.1497276504662));
#17959=CARTESIAN_POINT('Ctrl Pts',(5.5870051723591,-5.90331311820653,7.15794922446635));
#17960=CARTESIAN_POINT('Ctrl Pts',(5.73768264733383,-5.75697331156837,7.16617079846651));
#17961=CARTESIAN_POINT('Ctrl Pts',(5.88247446602308,-5.60501398027574,7.17439237246666));
#17962=CARTESIAN_POINT('Ctrl Pts',(6.02727483851187,-5.45304567175172,7.18261443216895));
#17963=CARTESIAN_POINT('Ctrl Pts',(6.16618865358631,-5.29545738600774,7.19083649187124));
#17964=CARTESIAN_POINT('Ctrl Pts',(6.29879154616042,-5.13272954874091,7.19905855157353));
#17965=CARTESIAN_POINT('Ctrl Pts',(6.4313887281217,-4.97000871943337,7.20728025718852));
#17966=CARTESIAN_POINT('Ctrl Pts',(6.55767534570129,-4.80214901067917,7.21550196280352));
#17967=CARTESIAN_POINT('Ctrl Pts',(6.67726755981736,-4.62966364837779,7.22372366841851));
#17968=CARTESIAN_POINT('Ctrl Pts',(6.79688947185335,-4.45713545338438,7.23194741570116));
#17969=CARTESIAN_POINT('Ctrl Pts',(6.90981348869871,-4.27997955088766,7.24017116298381));
#17970=CARTESIAN_POINT('Ctrl Pts',(7.01569862192865,-4.09873888028604,7.24839491026646));
#17971=CARTESIAN_POINT('Ctrl Pts',(7.11795771483149,-3.92370480319253,7.25633703501743));
#17972=CARTESIAN_POINT('Ctrl Pts',(7.21365187453952,-3.74486129647251,7.26427915976841));
#17973=CARTESIAN_POINT('Ctrl Pts',(7.3025141739088,-3.56272007072702,7.27222128451938));
#17974=CARTESIAN_POINT('Ctrl Pts',(7.39452514250719,-3.37412501161318,7.28044482359336));
#17975=CARTESIAN_POINT('Ctrl Pts',(7.47924115530385,-3.18193299646193,7.28866836266734));
#17976=CARTESIAN_POINT('Ctrl Pts',(7.55639768745436,-2.98672756567021,7.29689190174131));
#17977=CARTESIAN_POINT('Ctrl Pts',(7.63354019120711,-2.79155762661658,7.30511394563304));
#17978=CARTESIAN_POINT('Ctrl Pts',(7.70312584918836,-2.59337563960125,7.31333598952476));
#17979=CARTESIAN_POINT('Ctrl Pts',(7.76493841870277,-2.39278476178984,7.32155803341648));
#17980=CARTESIAN_POINT('Ctrl Pts',(7.82674416362197,-2.19221603079347,7.32977916952971));
#17981=CARTESIAN_POINT('Ctrl Pts',(7.88077844663869,-1.98923922172765,7.33800030564295));
#17982=CARTESIAN_POINT('Ctrl Pts',(7.92687475615988,-1.78447307703291,7.34622144175618));
#17983=CARTESIAN_POINT('Ctrl Pts',(7.97297472181362,-1.57969069129466,7.35444322992949));
#17984=CARTESIAN_POINT('Ctrl Pts',(8.01113538861028,-1.37311897351596,7.3626650181028));
#17985=CARTESIAN_POINT('Ctrl Pts',(8.04124104749046,-1.16538833813218,7.37088680627611));
#17986=CARTESIAN_POINT('Ctrl Pts',(8.07134662283547,-0.957658279145457,
7.37910857163616));
#17987=CARTESIAN_POINT('Ctrl Pts',(8.09339719534004,-0.748769601255617,
7.38733033699621));
#17988=CARTESIAN_POINT('Ctrl Pts',(8.10732868918165,-0.539359887340692,
7.39555210235626));
#17989=CARTESIAN_POINT('Ctrl Pts',(8.12126308750845,-0.32990651497671,7.4037755818179));
#17990=CARTESIAN_POINT('Ctrl Pts',(8.12707500607554,-0.119932183916431,
7.41199906127953));
#17991=CARTESIAN_POINT('Ctrl Pts',(8.12475239826843,0.0899223516781355,
7.42022254074117));
#17992=CARTESIAN_POINT('Ctrl Pts',(8.1238139787038,0.17471135536876,7.42354513097467));
#17993=CARTESIAN_POINT('Ctrl Pts',(8.12154822459675,0.259480796073226,7.42686772120818));
#17994=CARTESIAN_POINT('Ctrl Pts',(8.11795675478785,0.344188451134322,7.43019031144168));
#17995=CARTESIAN_POINT('Ctrl Pts',(8.10906772838656,0.553843166974015,7.43841385051562));
#17996=CARTESIAN_POINT('Ctrl Pts',(8.0920510902348,0.763187399131707,7.44663738958956));
#17997=CARTESIAN_POINT('Ctrl Pts',(8.06695208136577,0.971582049776792,7.45486092866349));
#17998=CARTESIAN_POINT('Ctrl Pts',(8.04185763593252,1.17993881065456,7.46308297255518));
#17999=CARTESIAN_POINT('Ctrl Pts',(8.0086837880162,1.38734604193663,7.47130501644687));
#18000=CARTESIAN_POINT('Ctrl Pts',(7.96752757674456,1.59317038521149,7.47952706033857));
#18001=CARTESIAN_POINT('Ctrl Pts',(7.92637590944327,1.79897200385541,7.48774819645176));
#18002=CARTESIAN_POINT('Ctrl Pts',(7.87724369610853,2.00319079430361,7.49596933256495));
#18003=CARTESIAN_POINT('Ctrl Pts',(7.82027912851159,2.20520337263164,7.50419046867814));
#18004=CARTESIAN_POINT('Ctrl Pts',(7.7633100427653,2.40723197360391,7.51241225685142));
#18005=CARTESIAN_POINT('Ctrl Pts',(7.69850743899205,2.60705372822604,7.5206340450247));
#18006=CARTESIAN_POINT('Ctrl Pts',(7.62606974046467,2.80405917841781,7.52885583319798));
#18007=CARTESIAN_POINT('Ctrl Pts',(7.55363224293257,3.00106408197203,7.53707759855799));
#18008=CARTESIAN_POINT('Ctrl Pts',(7.47355979733775,3.19525242084551,7.545299363918));
#18009=CARTESIAN_POINT('Ctrl Pts',(7.38609964456578,3.38603301859938,7.55352112927801));
#18010=CARTESIAN_POINT('Ctrl Pts',(7.29862125780382,3.57685339094087,7.56174460873961));
#18011=CARTESIAN_POINT('Ctrl Pts',(7.20375220988757,3.7642643347215,7.56996808820122));
#18012=CARTESIAN_POINT('Ctrl Pts',(7.10178700425989,3.94769665863847,7.57819156766283));
#18013=CARTESIAN_POINT('Ctrl Pts',(7.06058928521914,4.02181011035177,7.58151415789654));
#18014=CARTESIAN_POINT('Ctrl Pts',(7.01823367273,4.09527434525954,7.58483674813025));
#18015=CARTESIAN_POINT('Ctrl Pts',(6.97474169477012,4.16805300514942,7.58815933836396));
#18016=CARTESIAN_POINT('Ctrl Pts',(6.86709737061338,4.34818299749209,7.59638287743793));
#18017=CARTESIAN_POINT('Ctrl Pts',(6.75245376590448,4.52416997829286,7.6046064165119));
#18018=CARTESIAN_POINT('Ctrl Pts',(6.63115497203716,4.69547349042957,7.61282995558587));
#18019=CARTESIAN_POINT('Ctrl Pts',(6.50987823239749,4.86674585661227,7.6210519994776));
#18020=CARTESIAN_POINT('Ctrl Pts',(6.38194888903332,5.03333621311725,7.62927404336933));
#18021=CARTESIAN_POINT('Ctrl Pts',(6.24775384980835,5.19473381365253,7.63749608726106));
#18022=CARTESIAN_POINT('Ctrl Pts',(6.11357362677427,5.35611359461956,7.64571722337428));
#18023=CARTESIAN_POINT('Ctrl Pts',(5.97312927748498,5.51230153753551,7.65393835948751));
#18024=CARTESIAN_POINT('Ctrl Pts',(5.82684794214979,5.66282002376597,7.66215949560073));
#18025=CARTESIAN_POINT('Ctrl Pts',(5.68055500449834,5.81335044838265,7.67038128377405));
#18026=CARTESIAN_POINT('Ctrl Pts',(5.52842435941999,5.95821030446604,7.67860307194737));
#18027=CARTESIAN_POINT('Ctrl Pts',(5.37092068800271,6.09695813711104,7.68682486012069));
#18028=CARTESIAN_POINT('Ctrl Pts',(5.21341745361613,6.23570558476779,7.69504662548074));
#18029=CARTESIAN_POINT('Ctrl Pts',(5.05054144580448,6.3683408499792,7.70326839084078));
#18030=CARTESIAN_POINT('Ctrl Pts',(4.88279156918908,6.49446179866785,7.71149015620083));
#18031=CARTESIAN_POINT('Ctrl Pts',(4.7150067195091,6.62060904148066,7.71971363566247));
#18032=CARTESIAN_POINT('Ctrl Pts',(4.54234620688782,6.74023907735389,7.72793711512412));
#18033=CARTESIAN_POINT('Ctrl Pts',(4.36534002859345,6.85299160930901,7.73616059458576));
#18034=CARTESIAN_POINT('Ctrl Pts',(4.293822977689,6.89854780765837,7.73948318481926));
#18035=CARTESIAN_POINT('Ctrl Pts',(4.22159684483345,6.94298177497777,7.74280577505276));
#18036=CARTESIAN_POINT('Ctrl Pts',(4.14869787298499,6.98627178981678,7.74612836528626));
#18037=CARTESIAN_POINT('Ctrl Pts',(3.96827010388932,7.09341624746095,7.75435190436024));
#18038=CARTESIAN_POINT('Ctrl Pts',(3.78366013480724,7.19358476960094,7.76257544343422));
#18039=CARTESIAN_POINT('Ctrl Pts',(3.59542788694271,7.28646593845704,7.77079898250821));
#18040=CARTESIAN_POINT('Ctrl Pts',(3.40722986297049,7.37933021990327,7.77902102639995));
#18041=CARTESIAN_POINT('Ctrl Pts',(3.21541113904964,7.46490966210488,7.78724307029169));
#18042=CARTESIAN_POINT('Ctrl Pts',(3.02055514069819,7.54293936105161,7.79546511418343));
#18043=CARTESIAN_POINT('Ctrl Pts',(2.82572065598566,7.62096044490422,7.80368625029668));
#18044=CARTESIAN_POINT('Ctrl Pts',(2.62784984002567,7.6914333400571,7.81190738640993));
#18045=CARTESIAN_POINT('Ctrl Pts',(2.42754572333658,7.75414143046219,7.82012852252318));
#18046=CARTESIAN_POINT('Ctrl Pts',(2.22722571951015,7.81685449456459,7.82835031069651));
#18047=CARTESIAN_POINT('Ctrl Pts',(2.02447231000839,7.87180143271431,7.83657209886984));
#18048=CARTESIAN_POINT('Ctrl Pts',(1.8199043179409,7.91881530508447,7.84479388704317));
#18049=CARTESIAN_POINT('Ctrl Pts',(1.61533689349503,7.96582904700367,7.85301565240323));
#18050=CARTESIAN_POINT('Ctrl Pts',(1.40895518459802,8.00490970374414,7.8612374177633));
#18051=CARTESIAN_POINT('Ctrl Pts',(1.20138938654037,8.03594120837181,7.86945918312336));
#18052=CARTESIAN_POINT('Ctrl Pts',(0.993780314459552,8.06697918255304,7.87768266258501));
#18053=CARTESIAN_POINT('Ctrl Pts',(0.78498695180016,8.08996460861358,7.88590614204666));
#18054=CARTESIAN_POINT('Ctrl Pts',(0.575646914719905,8.10483301444721,7.89412962150832));
#18055=CARTESIAN_POINT('Ctrl Pts',(0.491065787484527,8.11084040100901,7.89745221174172));
#18056=CARTESIAN_POINT('Ctrl Pts',(0.406395473335491,8.11552330827984,7.90077480197513));
#18057=CARTESIAN_POINT('Ctrl Pts',(0.321678185702375,8.11887989240777,7.90409739220854));
#18058=CARTESIAN_POINT('Ctrl Pts',(0.11199962887258,8.12718756768263,7.91232093128234));
#18059=CARTESIAN_POINT('Ctrl Pts',(-0.0980349882997524,8.12736950028921,
7.92054447035614));
#18060=CARTESIAN_POINT('Ctrl Pts',(-0.307785009625147,8.11941844902392,
7.92876800942994));
#18061=CARTESIAN_POINT('Ctrl Pts',(-0.517496894753254,8.11146884339787,
7.93699005332149));
#18062=CARTESIAN_POINT('Ctrl Pts',(-0.726923992733384,8.09538921641806,
7.94521209721304));
#18063=CARTESIAN_POINT('Ctrl Pts',(-0.935427126214352,8.07122442099353,
7.95343414110459));
#18064=CARTESIAN_POINT('Ctrl Pts',(-1.14390723930476,8.04706229355302,7.96165527721765));
#18065=CARTESIAN_POINT('Ctrl Pts',(-1.35146329870153,8.01481681378467,7.9698764133307));
#18066=CARTESIAN_POINT('Ctrl Pts',(-1.55746187958918,7.97458463220038,7.97809754944375));
#18067=CARTESIAN_POINT('Ctrl Pts',(-1.76347679927134,7.93434925959728,7.9863193376169));
#18068=CARTESIAN_POINT('Ctrl Pts',(-1.96793370363497,7.88612597338955,7.99454112579004));
#18069=CARTESIAN_POINT('Ctrl Pts',(-2.17020893391364,7.83006262718642,8.00276291396318));
#18070=CARTESIAN_POINT('Ctrl Pts',(-2.37248360293232,7.77399943654416,8.01098467932305));
#18071=CARTESIAN_POINT('Ctrl Pts',(-2.57257632647824,7.71009631079563,8.01920644468292));
#18072=CARTESIAN_POINT('Ctrl Pts',(-2.76987766877603,7.63855125416566,8.02742821004279));
#18073=CARTESIAN_POINT('Ctrl Pts',(-2.96722014512873,7.56699128157895,8.03565168950427));
#18074=CARTESIAN_POINT('Ctrl Pts',(-3.16176980033458,7.48778629588259,8.04387516896574));
#18075=CARTESIAN_POINT('Ctrl Pts',(-3.35293523999828,7.40118320533127,8.05209864842722));
#18076=CARTESIAN_POINT('Ctrl Pts',(-3.43017315686592,7.36619234966065,8.05542123866176));
#18077=CARTESIAN_POINT('Ctrl Pts',(-3.50685884706295,7.32999432979059,8.0587438288963));
#18078=CARTESIAN_POINT('Ctrl Pts',(-3.58295431172122,7.2926076243425,8.06206641913084));
#18079=CARTESIAN_POINT('Ctrl Pts',(-3.77129352384996,7.20007408532274,8.07028995820521));
#18080=CARTESIAN_POINT('Ctrl Pts',(-3.95607674832197,7.10022553265419,8.07851349727958));
#18081=CARTESIAN_POINT('Ctrl Pts',(-4.13673716809682,6.99336064882874,8.08673703635396));
#18082=CARTESIAN_POINT('Ctrl Pts',(-4.31736474066964,6.88651519489519,8.0949590802461));
#18083=CARTESIAN_POINT('Ctrl Pts',(-4.49387075093313,6.77265610602097,8.10318112413823));
#18084=CARTESIAN_POINT('Ctrl Pts',(-4.66571448703126,6.65212717016193,8.11140316803037));
#18085=CARTESIAN_POINT('Ctrl Pts',(-4.83753925022554,6.53161154164806,8.11962430414402));
#18086=CARTESIAN_POINT('Ctrl Pts',(-5.00470252556901,6.40442770564491,8.12784544025766));
#18087=CARTESIAN_POINT('Ctrl Pts',(-5.16669332333603,6.27096225990038,8.13606657637131));
#18088=CARTESIAN_POINT('Ctrl Pts',(-5.32869696941604,6.13748622833342,8.14428836454502));
#18089=CARTESIAN_POINT('Ctrl Pts',(-5.48552708887313,5.99772777702664,8.15251015271874));
#18090=CARTESIAN_POINT('Ctrl Pts',(-5.63670566037028,5.85211387968909,8.16073194089245));
#18091=CARTESIAN_POINT('Ctrl Pts',(-5.78788381238767,5.70650038639083,8.16895370625292));
#18092=CARTESIAN_POINT('Ctrl Pts',(-5.9334102372631,5.55503168610662,8.17717547161338));
#18093=CARTESIAN_POINT('Ctrl Pts',(-6.07284330017465,5.39817208080882,8.18539723697385));
#18094=CARTESIAN_POINT('Ctrl Pts',(-6.21230543256481,5.24127977288767,8.19362071643588));
#18095=CARTESIAN_POINT('Ctrl Pts',(-6.34567146918689,5.0789945351682,8.20184419589792));
#18096=CARTESIAN_POINT('Ctrl Pts',(-6.47253892591764,4.91181508354914,8.21006767535996));
#18097=CARTESIAN_POINT('Ctrl Pts',(-6.52379807653848,4.8442683941768,8.21339026559101));
#18098=CARTESIAN_POINT('Ctrl Pts',(-6.57399682523498,4.77592311388816,8.21671285582206));
#18099=CARTESIAN_POINT('Ctrl Pts',(-6.62311055586632,4.70681358535391,8.22003544605311));
#18100=CARTESIAN_POINT('Ctrl Pts',(-6.74466893495809,4.53576483461904,8.22825898512622));
#18101=CARTESIAN_POINT('Ctrl Pts',(-6.85961724827754,4.35997672703516,8.23648252419932));
#18102=CARTESIAN_POINT('Ctrl Pts',(-6.96759927654907,4.17998180425858,8.24470606327243));
#18103=CARTESIAN_POINT('Ctrl Pts',(-7.07556167181243,4.00001960768513,8.25292810716331));
#18104=CARTESIAN_POINT('Ctrl Pts',(-7.17656015834777,3.81585237530458,8.26115015105419));
#18105=CARTESIAN_POINT('Ctrl Pts',(-7.27028294988928,3.62803988278096,8.26937219494506));
#18106=CARTESIAN_POINT('Ctrl Pts',(-7.36399539369519,3.4402481262382,8.27759333105743));
#18107=CARTESIAN_POINT('Ctrl Pts',(-7.45043361461306,3.24881217685777,8.2858144671698));
#18108=CARTESIAN_POINT('Ctrl Pts',(-7.52933234690375,3.05431530336488,8.29403560328216));
#18109=CARTESIAN_POINT('Ctrl Pts',(-7.60823733705397,2.85980300333624,8.30225739145462));
#18110=CARTESIAN_POINT('Ctrl Pts',(-7.67960153040176,2.662229566419,8.31047917962708));
#18111=CARTESIAN_POINT('Ctrl Pts',(-7.74320787749797,2.46219806846511,8.31870096779955));
#18112=CARTESIAN_POINT('Ctrl Pts',(-7.80681404810367,2.26216712554486,8.32692273315876));
#18113=CARTESIAN_POINT('Ctrl Pts',(-7.86266232871362,2.05967841711304,8.33514449851796));
#18114=CARTESIAN_POINT('Ctrl Pts',(-7.91058544077199,1.85535051856683,8.34336626387717));
#18115=CARTESIAN_POINT('Ctrl Pts',(-7.95851854400361,1.65098002104596,8.35158974333796));
#18116=CARTESIAN_POINT('Ctrl Pts',(-7.99852311057174,1.44476985459871,8.35981322279876));
#18117=CARTESIAN_POINT('Ctrl Pts',(-8.03048267586436,1.23735021523509,8.36803670225956));
#18118=CARTESIAN_POINT('Ctrl Pts',(-8.04339552378697,1.15354499965283,8.37135929249818));
#18119=CARTESIAN_POINT('Ctrl Pts',(-8.05499564268842,1.06954244622362,8.3746818827368));
#18120=CARTESIAN_POINT('Ctrl Pts',(-8.06527773840728,0.985384475649966,
8.37800447297542));
#18121=CARTESIAN_POINT('Ctrl Pts',(-8.09203917827196,0.766344648534784,
8.38665225269826));
#18122=CARTESIAN_POINT('Ctrl Pts',(-8.10987423995967,0.546205259409921,
8.3953000324211));
#18123=CARTESIAN_POINT('Ctrl Pts',(-8.11872063627548,0.325672830636386,
8.40394781214395));
#18124=CARTESIAN_POINT('Ctrl Pts',(-8.12306986537984,0.217250595927776,
8.40819939368247));
#18125=CARTESIAN_POINT('Ctrl Pts',(-8.1252472503007,0.108733441558642,8.41245097522098));
#18126=CARTESIAN_POINT('Ctrl Pts',(-8.12524999739701,0.000205669423076638,
8.4167025567595));
#18127=CARTESIAN_POINT('Origin',(0.,0.,-16.4167025567876));
#18128=CARTESIAN_POINT('',(4.94675008185377,-6.44587862049696,5.12505864308909));
#18129=CARTESIAN_POINT('',(4.94675008185375,-6.44587862049697,5.29165016466231));
#18130=CARTESIAN_POINT('',(4.94675008185374,-6.44587862049697,-16.4167025567876));
#18131=CARTESIAN_POINT('',(-8.12524999762747,-0.000196353792745782,6.58329744321239));
#18132=CARTESIAN_POINT('Ctrl Pts',(4.94675008185375,-6.44587862049697,5.29165016466231));
#18133=CARTESIAN_POINT('Ctrl Pts',(5.11327081011718,-6.31808589049612,5.29987187156593));
#18134=CARTESIAN_POINT('Ctrl Pts',(5.27483491075145,-6.18383844836398,5.30809357846955));
#18135=CARTESIAN_POINT('Ctrl Pts',(5.43095059073167,-6.04354724011746,5.31631528537316));
#18136=CARTESIAN_POINT('Ctrl Pts',(5.58710529693372,-5.90322096149353,5.32453904756141));
#18137=CARTESIAN_POINT('Ctrl Pts',(5.73780863988046,-5.75684809339947,5.33276280974965));
#18138=CARTESIAN_POINT('Ctrl Pts',(5.88260367082485,-5.60487837642335,5.3409865719379));
#18139=CARTESIAN_POINT('Ctrl Pts',(6.0253035427776,-5.45510763490172,5.3490913377132));
#18140=CARTESIAN_POINT('Ctrl Pts',(6.16226475094292,-5.29990113350262,5.35719610348851));
#18141=CARTESIAN_POINT('Ctrl Pts',(6.29308631040871,-5.13972297427074,5.36530086926381));
#18142=CARTESIAN_POINT('Ctrl Pts',(6.42582502683911,-4.97719744450756,5.37352440833777));
#18143=CARTESIAN_POINT('Ctrl Pts',(6.55228585150901,-4.80950059499723,5.38174794741173));
#18144=CARTESIAN_POINT('Ctrl Pts',(6.67207770646967,-4.63713992039602,5.38997148648569));
#18145=CARTESIAN_POINT('Ctrl Pts',(6.79184778119074,-4.46481058395874,5.39819353037743));
#18146=CARTESIAN_POINT('Ctrl Pts',(6.90495113804472,-4.2878193569373,5.40641557426917));
#18147=CARTESIAN_POINT('Ctrl Pts',(7.01103920883055,-4.10670388203735,5.41463761816091));
#18148=CARTESIAN_POINT('Ctrl Pts',(7.11711556665462,-3.92560840371775,5.422858754274));
#18149=CARTESIAN_POINT('Ctrl Pts',(7.21617803574784,-3.74038984099968,5.4310798903871));
#18150=CARTESIAN_POINT('Ctrl Pts',(7.30792289097652,-3.55161239186391,5.43930102650019));
#18151=CARTESIAN_POINT('Ctrl Pts',(7.3996750229574,-3.36281996982626,5.4475228146735));
#18152=CARTESIAN_POINT('Ctrl Pts',(7.48410825008128,-3.17046836147892,5.4557446028468));
#18153=CARTESIAN_POINT('Ctrl Pts',(7.56096562904357,-2.97514475596091,5.46396639102011));
#18154=CARTESIAN_POINT('Ctrl Pts',(7.63782279474688,-2.77982169241446,5.47218815638012));
#18155=CARTESIAN_POINT('Ctrl Pts',(7.70710404885484,-2.58152692363019,5.48040992174014));
#18156=CARTESIAN_POINT('Ctrl Pts',(7.76860106943491,-2.38086643608471,5.48863168710015));
#18157=CARTESIAN_POINT('Ctrl Pts',(7.83011091112316,-2.18016411415777,5.49685516656179));
#18158=CARTESIAN_POINT('Ctrl Pts',(7.88383319079082,-1.97709537020895,5.50507864602343));
#18159=CARTESIAN_POINT('Ctrl Pts',(7.92960950831404,-1.77228118766622,5.51330212548507));
#18160=CARTESIAN_POINT('Ctrl Pts',(7.94810483577805,-1.68952867325787,5.51662471571875));
#18161=CARTESIAN_POINT('Ctrl Pts',(7.96530359370538,-1.60649136570547,5.51994730595243));
#18162=CARTESIAN_POINT('Ctrl Pts',(7.98119769287488,-1.52321073714334,5.52326989618611));
#18163=CARTESIAN_POINT('Ctrl Pts',(8.020536201801,-1.31708796698015,5.53149343526006));
#18164=CARTESIAN_POINT('Ctrl Pts',(8.05189182966708,-1.10940696613294,5.539716974334));
#18165=CARTESIAN_POINT('Ctrl Pts',(8.07516232205342,-0.900800219243289,
5.54794051340795));
#18166=CARTESIAN_POINT('Ctrl Pts',(8.0984285834601,-0.69223140068324,5.55616255729967));
#18167=CARTESIAN_POINT('Ctrl Pts',(8.11361261069341,-0.482737464993099,
5.56438460119139));
#18168=CARTESIAN_POINT('Ctrl Pts',(8.12066388589119,-0.272957166754323,
5.57260664508311));
#18169=CARTESIAN_POINT('Ctrl Pts',(8.12771438257256,-0.0632000299157026,
5.58082778119631));
#18170=CARTESIAN_POINT('Ctrl Pts',(8.12663390997845,0.146843111696508,5.58904891730951));
#18171=CARTESIAN_POINT('Ctrl Pts',(8.11742402792945,0.356531503928758,5.59727005342272));
#18172=CARTESIAN_POINT('Ctrl Pts',(8.10821341539789,0.566236527612974,5.605491841596));
#18173=CARTESIAN_POINT('Ctrl Pts',(8.0908721153668,0.775586450921568,5.61371362976927));
#18174=CARTESIAN_POINT('Ctrl Pts',(8.06545377315046,0.983942577426666,5.62193541794256));
#18175=CARTESIAN_POINT('Ctrl Pts',(8.04003550146333,1.1922981257983,5.63015718330254));
#18176=CARTESIAN_POINT('Ctrl Pts',(8.00654027081425,1.39965959044746,5.63837894866252));
#18177=CARTESIAN_POINT('Ctrl Pts',(7.96507343273785,1.60539489646433,5.6466007140225));
#18178=CARTESIAN_POINT('Ctrl Pts',(7.92359794951369,1.8111730948791,5.65482419348415));
#18179=CARTESIAN_POINT('Ctrl Pts',(7.87414759705053,2.01532416821216,5.66304767294581));
#18180=CARTESIAN_POINT('Ctrl Pts',(7.81687876709476,2.21722662419589,5.67127115240746));
#18181=CARTESIAN_POINT('Ctrl Pts',(7.79374003901856,2.29880269324658,5.6745937426411));
#18182=CARTESIAN_POINT('Ctrl Pts',(7.7693255511162,2.38001183374261,5.67791633287475));
#18183=CARTESIAN_POINT('Ctrl Pts',(7.74364793709499,2.46081372493419,5.6812389231084));
#18184=CARTESIAN_POINT('Ctrl Pts',(7.68009485128538,2.66080152443282,5.68946246218234));
#18185=CARTESIAN_POINT('Ctrl Pts',(7.60877996240833,2.85835850389997,5.69768600125629));
#18186=CARTESIAN_POINT('Ctrl Pts',(7.52991451097841,3.0528797912556,5.70590954033023));
#18187=CARTESIAN_POINT('Ctrl Pts',(7.4510633986569,3.2473657112637,5.71413158422198));
#18188=CARTESIAN_POINT('Ctrl Pts',(7.36466457454118,3.43881676758294,5.72235362811374));
#18189=CARTESIAN_POINT('Ctrl Pts',(7.2709777597904,3.62664720908078,5.73057567200549));
#18190=CARTESIAN_POINT('Ctrl Pts',(7.17730128880249,3.81445691261722,5.73879680811878));
#18191=CARTESIAN_POINT('Ctrl Pts',(7.07633856522753,3.99864653558411,5.74701794423208));
#18192=CARTESIAN_POINT('Ctrl Pts',(6.96839605749512,4.17865336542605,5.75523908034537));
#18193=CARTESIAN_POINT('Ctrl Pts',(6.8604449882947,4.35867447252305,5.76346086851869));
#18194=CARTESIAN_POINT('Ctrl Pts',(6.74551317819972,4.53451186929834,5.77168265669199));
#18195=CARTESIAN_POINT('Ctrl Pts',(6.62395191788581,4.70562945332895,5.77990444486531));
#18196=CARTESIAN_POINT('Ctrl Pts',(6.50239099487288,4.87674656255263,5.78812621022529));
#18197=CARTESIAN_POINT('Ctrl Pts',(6.37420083144179,5.0431436463528,5.79634797558527));
#18198=CARTESIAN_POINT('Ctrl Pts',(6.23977503393361,5.20431504507546,5.80456974094526));
#18199=CARTESIAN_POINT('Ctrl Pts',(6.10532121087724,5.36552004536035,5.81279322040689));
#18200=CARTESIAN_POINT('Ctrl Pts',(5.96462934560591,5.52149695758798,5.82101669986853));
#18201=CARTESIAN_POINT('Ctrl Pts',(5.81813288836337,5.67177373101612,5.82924017933016));
#18202=CARTESIAN_POINT('Ctrl Pts',(5.75894289459634,5.73249111251439,5.83256276956367));
#18203=CARTESIAN_POINT('Ctrl Pts',(5.69880575929252,5.79227837433905,5.83588535979718));
#18204=CARTESIAN_POINT('Ctrl Pts',(5.63775179089365,5.85110607550191,5.83920795003068));
#18205=CARTESIAN_POINT('Ctrl Pts',(5.4866408625328,5.99670690652375,5.84743148910464));
#18206=CARTESIAN_POINT('Ctrl Pts',(5.32986193586128,6.13647436219046,5.85565502817858));
#18207=CARTESIAN_POINT('Ctrl Pts',(5.16788877933457,6.26997712331774,5.86387856725254));
#18208=CARTESIAN_POINT('Ctrl Pts',(5.00594507234165,6.40345561132373,5.87210061114422));
#18209=CARTESIAN_POINT('Ctrl Pts',(4.83880924788867,6.53067149067059,5.8803226550359));
#18210=CARTESIAN_POINT('Ctrl Pts',(4.66698860200944,6.65123334060789,5.88854469892759));
#18211=CARTESIAN_POINT('Ctrl Pts',(4.49518692648261,6.77178187956752,5.89676583504087));
#18212=CARTESIAN_POINT('Ctrl Pts',(4.31870170351852,6.88567768649474,5.90498697115416));
#18213=CARTESIAN_POINT('Ctrl Pts',(4.13807036707505,6.99257185873948,5.91320810726745));
#18214=CARTESIAN_POINT('Ctrl Pts',(3.95742470384393,7.09947450930331,5.92142989544075));
#18215=CARTESIAN_POINT('Ctrl Pts',(3.77263252254023,7.19937426308323,5.92965168361405));
#18216=CARTESIAN_POINT('Ctrl Pts',(3.58425800164598,7.29196695961637,5.93787347178735));
#18217=CARTESIAN_POINT('Ctrl Pts',(3.3958840034416,7.38455939922907,5.94609523714734));
#18218=CARTESIAN_POINT('Ctrl Pts',(3.20392795140517,7.46984469447034,5.95431700250735));
#18219=CARTESIAN_POINT('Ctrl Pts',(3.00897673942943,7.54756560382701,5.96253876786734));
#18220=CARTESIAN_POINT('Ctrl Pts',(2.8139848833609,7.62530271670363,5.97076224732899));
#18221=CARTESIAN_POINT('Ctrl Pts',(2.61599689391173,7.69547218396382,5.97898572679063));
#18222=CARTESIAN_POINT('Ctrl Pts',(2.41561869924228,7.75786529029546,5.98720920625227));
#18223=CARTESIAN_POINT('Ctrl Pts',(2.33465848821067,7.78307441578868,5.99053179648584));
#18224=CARTESIAN_POINT('Ctrl Pts',(2.2533082752287,7.80701464484136,5.99385438671941));
#18225=CARTESIAN_POINT('Ctrl Pts',(2.17160873081213,7.82967451959278,5.99717697695298));
#18226=CARTESIAN_POINT('Ctrl Pts',(1.96939920492885,7.88575858423208,6.00540051602693));
#18227=CARTESIAN_POINT('Ctrl Pts',(1.76498303012576,7.93401416412474,6.0136240551009));
#18228=CARTESIAN_POINT('Ctrl Pts',(1.55898219445379,7.97428755939213,6.02184759417486));
#18229=CARTESIAN_POINT('Ctrl Pts',(1.35301881331104,8.01455363225689,6.03006963806661));
#18230=CARTESIAN_POINT('Ctrl Pts',(1.14547163566338,8.04684036056402,6.03829168195836));
#18231=CARTESIAN_POINT('Ctrl Pts',(0.936973134717045,8.0710450938722,6.04651372585011));
#18232=CARTESIAN_POINT('Ctrl Pts',(0.728497653651553,8.0952471547867,6.05473486196329));
#18233=CARTESIAN_POINT('Ctrl Pts',(0.519071351836212,8.11136896818083,6.06295599807648));
#18234=CARTESIAN_POINT('Ctrl Pts',(0.309332959536304,8.11935962269467,6.07117713418966));
#18235=CARTESIAN_POINT('Ctrl Pts',(0.0995779318177861,8.12735091098795,
6.07939892236296));
#18236=CARTESIAN_POINT('Ctrl Pts',(-0.110488941216562,8.12720973790773,
6.08762071053625));
#18237=CARTESIAN_POINT('Ctrl Pts',(-0.320226715276507,8.11893727117799,
6.09584249870955));
#18238=CARTESIAN_POINT('Ctrl Pts',(-0.529963907372128,8.11066482740207,
6.10406426406966));
#18239=CARTESIAN_POINT('Ctrl Pts',(-0.739371707723339,8.09426114942689,
6.11228602942977));
#18240=CARTESIAN_POINT('Ctrl Pts',(-0.947811537538,8.06977947975097,6.12050779478988));
#18241=CARTESIAN_POINT('Ctrl Pts',(-1.15629482359629,8.04529270605341,6.12873127425156));
#18242=CARTESIAN_POINT('Ctrl Pts',(-1.36380944299606,8.01272461066221,6.13695475371323));
#18243=CARTESIAN_POINT('Ctrl Pts',(-1.56972318479993,7.97218017142121,6.14517823317491));
#18244=CARTESIAN_POINT('Ctrl Pts',(-1.65291996186244,7.95579871653089,6.14850082340836));
#18245=CARTESIAN_POINT('Ctrl Pts',(-1.7358555036824,7.93811574105068,6.15182341364181));
#18246=CARTESIAN_POINT('Ctrl Pts',(-1.81848859043681,7.91914053473931,6.15514600387527));
#18247=CARTESIAN_POINT('Ctrl Pts',(-2.02300866964623,7.87217616670896,6.16336954294922));
#18248=CARTESIAN_POINT('Ctrl Pts',(-2.22574163981204,7.81727701990729,6.17159308202317));
#18249=CARTESIAN_POINT('Ctrl Pts',(-2.42606736327293,7.75460409765463,6.17981662109712));
#18250=CARTESIAN_POINT('Ctrl Pts',(-2.62635666403652,7.6919425704282,6.18803866498878));
#18251=CARTESIAN_POINT('Ctrl Pts',(-2.82423931031158,7.62151017676951,6.19626070888043));
#18252=CARTESIAN_POINT('Ctrl Pts',(-3.01911025150712,7.54351780350153,6.20448275277209));
#18253=CARTESIAN_POINT('Ctrl Pts',(-3.21395967741587,7.46553404120587,6.21270388888535));
#18254=CARTESIAN_POINT('Ctrl Pts',(-3.40579778838885,7.37999207525797,6.22092502499861));
#18255=CARTESIAN_POINT('Ctrl Pts',(-3.59403866731135,7.28715126921151,6.22914616111186));
#18256=CARTESIAN_POINT('Ctrl Pts',(-3.78229447657336,7.1943030994895,6.23736794928514));
#18257=CARTESIAN_POINT('Ctrl Pts',(-3.96695221800712,7.09415506104298,6.24558973745842));
#18258=CARTESIAN_POINT('Ctrl Pts',(-4.14744882516031,6.98701336804048,6.25381152563171));
#18259=CARTESIAN_POINT('Ctrl Pts',(-4.32794493148387,6.87987197232742,6.26203329099174));
#18260=CARTESIAN_POINT('Ctrl Pts',(-4.50427967438332,6.76573711374006,6.27025505635178));
#18261=CARTESIAN_POINT('Ctrl Pts',(-4.67591686307836,6.64495967272033,6.27847682171181));
#18262=CARTESIAN_POINT('Ctrl Pts',(-4.84758983527764,6.52415705160934,6.28670030117342));
#18263=CARTESIAN_POINT('Ctrl Pts',(-5.01456305554396,6.39670925125489,6.29492378063502));
#18264=CARTESIAN_POINT('Ctrl Pts',(-5.17633056667184,6.26300961415826,6.30314726009662));
#18265=CARTESIAN_POINT('Ctrl Pts',(-5.24169063172759,6.20899000961815,6.30646985033027));
#18266=CARTESIAN_POINT('Ctrl Pts',(-5.30620125380452,6.15395028433812,6.30979244056392));
#18267=CARTESIAN_POINT('Ctrl Pts',(-5.36983060907314,6.09791823431253,6.31311503079757));
#18268=CARTESIAN_POINT('Ctrl Pts',(-5.52731571933501,5.95923674776865,6.32133856987151));
#18269=CARTESIAN_POINT('Ctrl Pts',(-5.67945114680157,5.8144286498553,6.32956210894545));
#18270=CARTESIAN_POINT('Ctrl Pts',(-5.82576822773381,5.66393080106274,6.33778564801939));
#18271=CARTESIAN_POINT('Ctrl Pts',(-5.97205870568036,5.51346031539206,6.34600769191115));
#18272=CARTESIAN_POINT('Ctrl Pts',(-6.11253274300237,5.35730235493905,6.3542297358029));
#18273=CARTESIAN_POINT('Ctrl Pts',(-6.24675869512846,5.19593046213448,6.36245177969466));
#18274=CARTESIAN_POINT('Ctrl Pts',(-6.38096982765176,5.03457638605846,6.37067291580799));
#18275=CARTESIAN_POINT('Ctrl Pts',(-6.50893406368367,4.86800975357322,6.37889405192132));
#18276=CARTESIAN_POINT('Ctrl Pts',(-6.63025966624038,4.69673762528056,6.38711518803465));
#18277=CARTESIAN_POINT('Ctrl Pts',(-6.75159489174576,4.52545191252702,6.39533697620796));
#18278=CARTESIAN_POINT('Ctrl Pts',(-6.8662902590413,4.34946019738865,6.40355876438126));
#18279=CARTESIAN_POINT('Ctrl Pts',(-6.97399643320615,4.16929985874461,6.41178055255457));
#18280=CARTESIAN_POINT('Ctrl Pts',(-7.08170230851493,3.98914001999775,6.42000231791461));
#18281=CARTESIAN_POINT('Ctrl Pts',(-7.18241888046251,3.80481183541026,6.42822408327464));
#18282=CARTESIAN_POINT('Ctrl Pts',(-7.27584171555407,3.61687916479154,6.43644584863467));
#18283=CARTESIAN_POINT('Ctrl Pts',(-7.36928402775632,3.4289073133299,6.44466932809633));
#18284=CARTESIAN_POINT('Ctrl Pts',(-7.45542943402357,3.23732973875257,6.45289280755799));
#18285=CARTESIAN_POINT('Ctrl Pts',(-7.53402030555906,3.04273324462132,6.46111628701965));
#18286=CARTESIAN_POINT('Ctrl Pts',(-7.56577392802695,2.9641090547187,6.46443887725305));
#18287=CARTESIAN_POINT('Ctrl Pts',(-7.59629484888616,2.88499227325942,6.46776146748644));
#18288=CARTESIAN_POINT('Ctrl Pts',(-7.62556831858584,2.80542249600304,6.47108405771984));
#18289=CARTESIAN_POINT('Ctrl Pts',(-7.69788746847904,2.60884796256347,6.47929240827029));
#18290=CARTESIAN_POINT('Ctrl Pts',(-7.76261427768914,2.40944077562039,6.48750075882073));
#18291=CARTESIAN_POINT('Ctrl Pts',(-7.81954479118166,2.2078058839499,6.49570910937118));
#18292=CARTESIAN_POINT('Ctrl Pts',(-7.87646704650205,2.00620024084121,6.50391626924254));
#18293=CARTESIAN_POINT('Ctrl Pts',(-7.92559518063946,1.80236782324838,6.5121234291139));
#18294=CARTESIAN_POINT('Ctrl Pts',(-7.96677522118852,1.59692834452788,6.52033058898526));
#18295=CARTESIAN_POINT('Ctrl Pts',(-8.00794972966339,1.39151646428526,6.52853664631721));
#18296=CARTESIAN_POINT('Ctrl Pts',(-8.04117821850922,1.18449824532056,6.53674270364917));
#18297=CARTESIAN_POINT('Ctrl Pts',(-8.06635777565389,0.976503864635504,
6.54494876098113));
#18298=CARTESIAN_POINT('Ctrl Pts',(-8.09153848603434,0.768499957708096,
6.55315519415444));
#18299=CARTESIAN_POINT('Ctrl Pts',(-8.10866949080331,0.55952009450846,6.56136162732775));
#18300=CARTESIAN_POINT('Ctrl Pts',(-8.11769960763622,0.350200860482541,
6.56956806050107));
#18301=CARTESIAN_POINT('Ctrl Pts',(-8.12273541013038,0.233470330824207,
6.57414452140484));
#18302=CARTESIAN_POINT('Ctrl Pts',(-8.12525282094382,0.116634346959204,
6.57872098230862));
#18303=CARTESIAN_POINT('Ctrl Pts',(-8.12524999762747,-0.000196353792745782,
6.58329744321239));
#18304=CARTESIAN_POINT('Ctrl Pts',(-8.12501235669361,-0.00019654038003419,
6.58329745074651));
#18305=CARTESIAN_POINT('Ctrl Pts',(-8.12536948861794,-0.389544456400672,
6.59854932871172));
#18306=CARTESIAN_POINT('Ctrl Pts',(-8.00298129759573,-2.1228738540623,6.66645754898436));
#18307=CARTESIAN_POINT('Ctrl Pts',(-6.79075267338643,-5.05622322872534,
6.78702211156442));
#18308=CARTESIAN_POINT('Ctrl Pts',(-3.56400020377475,-7.67968864976366,
6.94499113848673));
#18309=CARTESIAN_POINT('Ctrl Pts',(0.522655372263073,-8.4502394387162,7.102960165409));
#18310=CARTESIAN_POINT('Ctrl Pts',(3.41983802727889,-7.52248145840713,7.21851605726134));
#18311=CARTESIAN_POINT('Ctrl Pts',(4.73959395534349,-6.60538794581216,7.28141560680623));
#18312=CARTESIAN_POINT('Ctrl Pts',(4.94684221335274,-6.44599857519204,7.2916588140437));
#18313=CARTESIAN_POINT('',(-8.12524999939286,-9.93290792602784E-5,6.41670255680724));
#18314=CARTESIAN_POINT('Ctrl Pts',(-8.12524999939286,-9.93290792612735E-5,
6.41670255680723));
#18315=CARTESIAN_POINT('Ctrl Pts',(-8.12524737621332,-0.214678883336293,
6.42510654393496));
#18316=CARTESIAN_POINT('Ctrl Pts',(-8.11674017324388,-0.429227910625565,
6.43351053106269));
#18317=CARTESIAN_POINT('Ctrl Pts',(-8.09976162698335,-0.643077871294042,
6.44191451819041));
#18318=CARTESIAN_POINT('Ctrl Pts',(-8.08277759880984,-0.856996878325916,
6.45032121873808));
#18319=CARTESIAN_POINT('Ctrl Pts',(-8.05731678308044,-1.0702161025105,6.45872791928576));
#18320=CARTESIAN_POINT('Ctrl Pts',(-8.02346435712921,-1.28207147709367,
6.46713461983344));
#18321=CARTESIAN_POINT('Ctrl Pts',(-8.00300596344256,-1.41010427049229,
6.47221512985827));
#18322=CARTESIAN_POINT('Ctrl Pts',(-7.97948372510071,-1.53763906534455,
6.4772956398831));
#18323=CARTESIAN_POINT('Ctrl Pts',(-7.95292554614784,-1.6645308107479,6.48237614990793));
#18324=CARTESIAN_POINT('Ctrl Pts',(-7.90993729865206,-1.86992342318004,
6.49059968898189));
#18325=CARTESIAN_POINT('Ctrl Pts',(-7.85898109901696,-2.07368318179469,
6.49882322805586));
#18326=CARTESIAN_POINT('Ctrl Pts',(-7.80020589082835,-2.27518694247015,
6.50704676712982));
#18327=CARTESIAN_POINT('Ctrl Pts',(-7.7414413689935,-2.47665406626185,6.51526881102154));
#18328=CARTESIAN_POINT('Ctrl Pts',(-7.67486075856426,-2.67586572779008,
6.52349085491326));
#18329=CARTESIAN_POINT('Ctrl Pts',(-7.6006631699023,-2.87221289952377,6.53171289880498));
#18330=CARTESIAN_POINT('Ctrl Pts',(-7.52647377323958,-3.06853839298042,
6.53993403491818));
#18331=CARTESIAN_POINT('Ctrl Pts',(-7.44466918153527,-3.26199975226291,
6.54815517103138));
#18332=CARTESIAN_POINT('Ctrl Pts',(-7.35549734391185,-3.45200613936385,
6.55637630714458));
#18333=CARTESIAN_POINT('Ctrl Pts',(-7.26631843361666,-3.64202759683729,
6.56459809531788));
#18334=CARTESIAN_POINT('Ctrl Pts',(-7.16977123275741,-3.82859326646194,
6.57281988349117));
#18335=CARTESIAN_POINT('Ctrl Pts',(-7.06615097551361,-4.0111342477843,6.58104167166447));
#18336=CARTESIAN_POINT('Ctrl Pts',(-6.96253100578854,-4.19367472260383,
6.58926343702449));
#18337=CARTESIAN_POINT('Ctrl Pts',(-6.85183816687966,-4.37219027630242,
6.5974852023845));
#18338=CARTESIAN_POINT('Ctrl Pts',(-6.73441287217018,-4.54613801260462,
6.60570696774452));
#18339=CARTESIAN_POINT('Ctrl Pts',(-6.6169630962361,-4.72012201412216,6.61393044720613));
#18340=CARTESIAN_POINT('Ctrl Pts',(-6.49277822554736,-4.88953605130122,
6.62215392666773));
#18341=CARTESIAN_POINT('Ctrl Pts',(-6.36224171402828,-5.05386663207276,
6.63037740612934));
#18342=CARTESIAN_POINT('Ctrl Pts',(-6.30950012935843,-5.12026227217948,
6.63369999636296));
#18343=CARTESIAN_POINT('Ctrl Pts',(-6.25572213838534,-5.18582841745631,
6.63702258659659));
#18344=CARTESIAN_POINT('Ctrl Pts',(-6.20093491455415,-5.25053271087452,
6.64034517683022));
#18345=CARTESIAN_POINT('Ctrl Pts',(-6.06533442088806,-5.41067833454873,
6.64856871590418));
#18346=CARTESIAN_POINT('Ctrl Pts',(-5.92350469539871,-5.56559412612467,
6.65679225497815));
#18347=CARTESIAN_POINT('Ctrl Pts',(-5.77587342523036,-5.71480303582002,
6.66501579405212));
#18348=CARTESIAN_POINT('Ctrl Pts',(-5.62826899699123,-5.86398481674387,
6.67323783794384));
#18349=CARTESIAN_POINT('Ctrl Pts',(-5.47486533671266,-6.0074615771866,6.68145988183557));
#18350=CARTESIAN_POINT('Ctrl Pts',(-5.31612752467578,-6.14479256801111,
6.68968192572729));
#18351=CARTESIAN_POINT('Ctrl Pts',(-5.15740723854511,-6.28210839641128,
6.69790306184053));
#18352=CARTESIAN_POINT('Ctrl Pts',(-4.99335419939815,-6.41327961698362,
6.70612419795378));
#18353=CARTESIAN_POINT('Ctrl Pts',(-4.82446777350828,-6.53790473048361,
6.71434533406702));
#18354=CARTESIAN_POINT('Ctrl Pts',(-4.65556795237824,-6.6625397286343,6.72256712224032));
#18355=CARTESIAN_POINT('Ctrl Pts',(-4.48183421426568,-6.78062740503495,
6.73078891041362));
#18356=CARTESIAN_POINT('Ctrl Pts',(-4.30379706053266,-6.8918080664112,6.73901069858692));
#18357=CARTESIAN_POINT('Ctrl Pts',(-4.12576040080534,-7.00298841929072,
6.74723246394694));
#18358=CARTESIAN_POINT('Ctrl Pts',(-3.94342060093207,-7.10726164154992,
6.75545422930696));
#18359=CARTESIAN_POINT('Ctrl Pts',(-3.75733550922104,-7.20431241921439,
6.76367599466699));
#18360=CARTESIAN_POINT('Ctrl Pts',(-3.57121162185707,-7.30138343035512,
6.77189947412863));
#18361=CARTESIAN_POINT('Ctrl Pts',(-3.38134114432983,-7.39122885241546,
6.78012295359026));
#18362=CARTESIAN_POINT('Ctrl Pts',(-3.18830577230109,-7.47357972224901,
6.7883464330519));
#18363=CARTESIAN_POINT('Ctrl Pts',(-3.11031233353567,-7.5068525232706,6.79166902328544));
#18364=CARTESIAN_POINT('Ctrl Pts',(-3.03180248393373,-7.53890240992644,
6.79499161351897));
#18365=CARTESIAN_POINT('Ctrl Pts',(-2.95281552569253,-7.56971386736178,
6.79831420375251));
#18366=CARTESIAN_POINT('Ctrl Pts',(-2.7573197552922,-7.6459734137806,6.80653774282647));
#18367=CARTESIAN_POINT('Ctrl Pts',(-2.55883642947032,-7.71466797602978,
6.81476128190043));
#18368=CARTESIAN_POINT('Ctrl Pts',(-2.35796878883899,-7.77558169871304,
6.82298482097439));
#18369=CARTESIAN_POINT('Ctrl Pts',(-2.15713766943384,-7.83648434622343,
6.8312068648661));
#18370=CARTESIAN_POINT('Ctrl Pts',(-1.95392338255781,-7.88960889218248,
6.83942890875781));
#18371=CARTESIAN_POINT('Ctrl Pts',(-1.74894476630273,-7.93478920746621,
6.84765095264953));
#18372=CARTESIAN_POINT('Ctrl Pts',(-1.5439887813034,-7.97996453448684,6.85587208876275));
#18373=CARTESIAN_POINT('Ctrl Pts',(-1.33726914373695,-8.01719731848192,
6.86409322487598));
#18374=CARTESIAN_POINT('Ctrl Pts',(-1.12941615257612,-8.04637227058257,
6.87231436098921));
#18375=CARTESIAN_POINT('Ctrl Pts',(-0.921546675538772,-8.07554953669688,
6.8805361491625));
#18376=CARTESIAN_POINT('Ctrl Pts',(-0.712543957006131,-8.09666765029956,
6.88875793733578));
#18377=CARTESIAN_POINT('Ctrl Pts',(-0.503045768961866,-8.10966291018496,
6.89697972550907));
#18378=CARTESIAN_POINT('Ctrl Pts',(-0.293548162218716,-8.12265813401201,
6.90520149086911));
#18379=CARTESIAN_POINT('Ctrl Pts',(-0.0835553832472526,-8.12753053363892,
6.91342325622916));
#18380=CARTESIAN_POINT('Ctrl Pts',(0.126291879406771,-8.12426845467922,
6.9216450215892));
#18381=CARTESIAN_POINT('Ctrl Pts',(0.336182891731384,-8.12100569563021,
6.92986850105082));
#18382=CARTESIAN_POINT('Ctrl Pts',(0.545928032182363,-8.10960507465031,
6.93809198051246));
#18383=CARTESIAN_POINT('Ctrl Pts',(0.754887711811087,-8.09010705152019,
6.94631545997408));
#18384=CARTESIAN_POINT('Ctrl Pts',(0.839315160555174,-8.08222912812676,
6.94963805020766));
#18385=CARTESIAN_POINT('Ctrl Pts',(0.923614427795624,-8.07302992913747,
6.95296064044122));
#18386=CARTESIAN_POINT('Ctrl Pts',(1.00774356520921,-8.06251452521355,6.95628323067479));
#18387=CARTESIAN_POINT('Ctrl Pts',(1.21596642753791,-8.03648849462657,6.96450676974876));
#18388=CARTESIAN_POINT('Ctrl Pts',(1.4232143473262,-8.00238756714075,6.97273030882273));
#18389=CARTESIAN_POINT('Ctrl Pts',(1.62885407719636,-7.96030916219344,6.98095384789669));
#18390=CARTESIAN_POINT('Ctrl Pts',(1.83445641819157,-7.91823840783107,6.98917589178841));
#18391=CARTESIAN_POINT('Ctrl Pts',(2.03845086405484,-7.86819313002325,6.99739793568012));
#18392=CARTESIAN_POINT('Ctrl Pts',(2.24021412886317,-7.81032190241489,7.00561997957184));
#18393=CARTESIAN_POINT('Ctrl Pts',(2.44195511741554,-7.75245706424656,7.01384111568505));
#18394=CARTESIAN_POINT('Ctrl Pts',(2.64146513332877,-7.68676808259966,7.02206225179827));
#18395=CARTESIAN_POINT('Ctrl Pts',(2.83813502013096,-7.61345369526907,7.03028338791148));
#18396=CARTESIAN_POINT('Ctrl Pts',(3.03482050582152,-7.54013349300177,7.03850517608479));
#18397=CARTESIAN_POINT('Ctrl Pts',(3.22866513500992,-7.45918677712556,7.0467269642581));
#18398=CARTESIAN_POINT('Ctrl Pts',(3.41907774333964,-7.37086120799323,7.0549487524314));
#18399=CARTESIAN_POINT('Ctrl Pts',(3.60948982332529,-7.28253588394074,7.06317051779145));
#18400=CARTESIAN_POINT('Ctrl Pts',(3.79646963508711,-7.18683187414066,7.07139228315149));
#18401=CARTESIAN_POINT('Ctrl Pts',(3.97944823178316,-7.08404399570315,7.07961404851153));
#18402=CARTESIAN_POINT('Ctrl Pts',(4.16246497647897,-6.98123468769939,7.08783752797316));
#18403=CARTESIAN_POINT('Ctrl Pts',(4.34147858245787,-6.87133870517064,7.09606100743479));
#18404=CARTESIAN_POINT('Ctrl Pts',(4.51594588412085,-6.75469616890293,7.10428448689642));
#18405=CARTESIAN_POINT('Ctrl Pts',(4.5864371348482,-6.70756826475614,7.10760707712998));
#18406=CARTESIAN_POINT('Ctrl Pts',(4.65618653868655,-6.65933951416623,7.11092966736354));
#18407=CARTESIAN_POINT('Ctrl Pts',(4.7251596222561,-6.6100343498881,7.1142522575971));
#18408=CARTESIAN_POINT('Ctrl Pts',(4.79993955054399,-6.55657818324849,7.11785457674156));
#18409=CARTESIAN_POINT('Ctrl Pts',(4.87381758274083,-6.50184908894628,7.12145689588603));
#18410=CARTESIAN_POINT('Ctrl Pts',(4.94675008185378,-6.44587862049694,7.1250592150305));
#18411=CARTESIAN_POINT('Ctrl Pts',(4.94675008185377,-6.44587862049696,5.12505864308909));
#18412=CARTESIAN_POINT('Ctrl Pts',(5.11327330421413,-6.31808397645537,5.13328059944019));
#18413=CARTESIAN_POINT('Ctrl Pts',(5.27484659373271,-6.18382917332942,5.1415025557913));
#18414=CARTESIAN_POINT('Ctrl Pts',(5.43097679848903,-6.04352368877411,5.1497245121424));
#18415=CARTESIAN_POINT('Ctrl Pts',(5.58710221449753,-5.90322250759869,5.15794621631375));
#18416=CARTESIAN_POINT('Ctrl Pts',(5.73778466133417,-5.75687121453366,5.16616792048511));
#18417=CARTESIAN_POINT('Ctrl Pts',(5.8825659940448,-5.60491791984572,5.17438962465647));
#18418=CARTESIAN_POINT('Ctrl Pts',(6.02738129098646,-5.45292897845727,5.18261325755616));
#18419=CARTESIAN_POINT('Ctrl Pts',(6.16629250319627,-5.29533562228945,5.19083689045586));
#18420=CARTESIAN_POINT('Ctrl Pts',(6.29887929555683,-5.1326218624116,5.19906052335556));
#18421=CARTESIAN_POINT('Ctrl Pts',(6.40401733559483,-5.00359388386116,5.20558166041357));
#18422=CARTESIAN_POINT('Ctrl Pts',(6.50517923101827,-4.87134688198783,5.2121027974716));
#18423=CARTESIAN_POINT('Ctrl Pts',(6.60217363942672,-4.73613669538359,5.21862393452961));
#18424=CARTESIAN_POINT('Ctrl Pts',(6.72448931848791,-4.56562866237569,5.22684747360358));
#18425=CARTESIAN_POINT('Ctrl Pts',(6.84021601287271,-4.39035200757339,5.23507101267753));
#18426=CARTESIAN_POINT('Ctrl Pts',(6.94899514531588,-4.21083768778568,5.24329455175149));
#18427=CARTESIAN_POINT('Ctrl Pts',(7.05775449982326,-4.03135600681953,5.2515165956432));
#18428=CARTESIAN_POINT('Ctrl Pts',(7.15956866079511,-3.8476384507736,5.25973863953492));
#18429=CARTESIAN_POINT('Ctrl Pts',(7.25412336277317,-3.66024340722969,5.26796068342663));
#18430=CARTESIAN_POINT('Ctrl Pts',(7.34866762516637,-3.47286905357661,5.27618181953985));
#18431=CARTESIAN_POINT('Ctrl Pts',(7.43595389592423,-3.2818182862483,5.28440295565307));
#18432=CARTESIAN_POINT('Ctrl Pts',(7.51571432548066,-3.08767319194646,5.29262409176629));
#18433=CARTESIAN_POINT('Ctrl Pts',(7.59548108124206,-2.89351269901063,5.30084587993959));
#18434=CARTESIAN_POINT('Ctrl Pts',(7.6677206885832,-2.69625766052627,5.30906766811289));
#18435=CARTESIAN_POINT('Ctrl Pts',(7.73221342592157,-2.49651018393641,5.31728945628619));
#18436=CARTESIAN_POINT('Ctrl Pts',(7.79670598430982,-2.29676326159246,5.32551122164622));
#18437=CARTESIAN_POINT('Ctrl Pts',(7.85345162764113,-2.09452419647121,5.33373298700625));
#18438=CARTESIAN_POINT('Ctrl Pts',(7.90228033600609,-1.89041081611153,5.34195475236629));
#18439=CARTESIAN_POINT('Ctrl Pts',(7.95111922434617,-1.68625488150042,5.35017823182791));
#18440=CARTESIAN_POINT('Ctrl Pts',(7.99203781176432,-1.48022413790811,5.35840171128954));
#18441=CARTESIAN_POINT('Ctrl Pts',(8.02491684026517,-1.2729482587004,5.36662519075116));
#18442=CARTESIAN_POINT('Ctrl Pts',(8.03820118535247,-1.18920112768048,5.36994778098474));
#18443=CARTESIAN_POINT('Ctrl Pts',(8.05017368940018,-1.10525083961553,5.37327037121832));
#18444=CARTESIAN_POINT('Ctrl Pts',(8.06082887240659,-1.02113929131937,5.37659296145191));
#18445=CARTESIAN_POINT('Ctrl Pts',(8.08720086161786,-0.812959962735982,
5.38481650052586));
#18446=CARTESIAN_POINT('Ctrl Pts',(8.10550815197252,-0.603724648719067,
5.39304003959982));
#18447=CARTESIAN_POINT('Ctrl Pts',(8.11568824050388,-0.394070990364645,
5.40126357867378));
#18448=CARTESIAN_POINT('Ctrl Pts',(8.12586647811832,-0.184455450687011,
5.40948562256549));
#18449=CARTESIAN_POINT('Ctrl Pts',(8.12792044886564,0.0255779870747951,
5.41770766645721));
#18450=CARTESIAN_POINT('Ctrl Pts',(8.12183967716184,0.235388659411679,5.42592971034892));
#18451=CARTESIAN_POINT('Ctrl Pts',(8.1157595768232,0.445176166995444,5.43415084646213));
#18452=CARTESIAN_POINT('Ctrl Pts',(8.10154653567723,0.654740663561258,5.44237198257534));
#18453=CARTESIAN_POINT('Ctrl Pts',(8.07924217894022,0.863442746528816,5.45059311868856));
#18454=CARTESIAN_POINT('Ctrl Pts',(8.05693605313133,1.07216138271922,5.45881490686185));
#18455=CARTESIAN_POINT('Ctrl Pts',(8.02653735813692,1.28001717508234,5.46703669503515));
#18456=CARTESIAN_POINT('Ctrl Pts',(7.98813957405315,1.48637603181224,5.47525848320845));
#18457=CARTESIAN_POINT('Ctrl Pts',(7.94974189651298,1.69273431595145,5.48348024856849));
#18458=CARTESIAN_POINT('Ctrl Pts',(7.90334523088579,1.89759538330417,5.49170201392852));
#18459=CARTESIAN_POINT('Ctrl Pts',(7.84909424822766,2.10033498398221,5.49992377928855));
#18460=CARTESIAN_POINT('Ctrl Pts',(7.79483195514024,2.30311685250138,5.50814725875018));
#18461=CARTESIAN_POINT('Ctrl Pts',(7.73271215002935,2.50377608581617,5.5163707382118));
#18462=CARTESIAN_POINT('Ctrl Pts',(7.66292978250387,2.70170218768004,5.52459421767343));
#18463=CARTESIAN_POINT('Ctrl Pts',(7.63473512184973,2.7816716624132,5.52791680790702));
#18464=CARTESIAN_POINT('Ctrl Pts',(7.60529014342423,2.86119514928919,5.5312393981406));
#18465=CARTESIAN_POINT('Ctrl Pts',(7.57460997759708,2.94023319649765,5.53456198837419));
#18466=CARTESIAN_POINT('Ctrl Pts',(7.49867538297727,3.13585541406091,5.54278552744815));
#18467=CARTESIAN_POINT('Ctrl Pts',(7.41514618317771,3.32856619812029,5.55100906652211));
#18468=CARTESIAN_POINT('Ctrl Pts',(7.32427102991529,3.51777506996164,5.55923260559608));
#18469=CARTESIAN_POINT('Ctrl Pts',(7.23341239933428,3.70694954034342,5.56745464948779));
#18470=CARTESIAN_POINT('Ctrl Pts',(7.13521060866594,3.89262310357579,5.5756766933795));
#18471=CARTESIAN_POINT('Ctrl Pts',(7.02996149969404,4.07422739612304,5.58389873727121));
#18472=CARTESIAN_POINT('Ctrl Pts',(6.92472401105381,4.25581163812419,5.59211987338444));
#18473=CARTESIAN_POINT('Ctrl Pts',(6.81244090534801,4.43332725133232,5.60034100949766));
#18474=CARTESIAN_POINT('Ctrl Pts',(6.69345323946345,4.60623178895898,5.60856214561088));
#18475=CARTESIAN_POINT('Ctrl Pts',(6.57445613606251,4.77915004052309,5.61678393378418));
#18476=CARTESIAN_POINT('Ctrl Pts',(6.44875357497336,4.94745624127609,5.62500572195748));
#18477=CARTESIAN_POINT('Ctrl Pts',(6.31672968358794,5.11063730536407,5.63322751013078));
#18478=CARTESIAN_POINT('Ctrl Pts',(6.18470615853356,5.2738179166682,5.64144927549082));
#18479=CARTESIAN_POINT('Ctrl Pts',(6.04636152587247,5.43187319216415,5.64967104085084));
#18480=CARTESIAN_POINT('Ctrl Pts',(5.9021202421595,5.58432307532355,5.65789280621088));
#18481=CARTESIAN_POINT('Ctrl Pts',(5.7578488865334,5.73680474175279,5.6661162856725));
#18482=CARTESIAN_POINT('Ctrl Pts',(5.60767862669683,5.88367846697999,5.67433976513413));
#18483=CARTESIAN_POINT('Ctrl Pts',(5.45207158345308,6.02450022918112,5.68256324459576));
#18484=CARTESIAN_POINT('Ctrl Pts',(5.389200575558,6.08139743600792,5.68588583482933));
#18485=CARTESIAN_POINT('Ctrl Pts',(5.32544244321428,6.1373071156651,5.6892084250629));
#18486=CARTESIAN_POINT('Ctrl Pts',(5.26082927658751,6.19220178006981,5.69253101529648));
#18487=CARTESIAN_POINT('Ctrl Pts',(5.10090919523702,6.32806819330439,5.70075455437044));
#18488=CARTESIAN_POINT('Ctrl Pts',(4.93569698852641,6.45775820936455,5.70897809344439));
#18489=CARTESIAN_POINT('Ctrl Pts',(4.76569246948587,6.58087097949698,5.71720163251835));
#18490=CARTESIAN_POINT('Ctrl Pts',(4.59571886022002,6.70396136558925,5.72542367641005));
#18491=CARTESIAN_POINT('Ctrl Pts',(4.42095491644826,6.82047671964672,5.73364572030177));
#18492=CARTESIAN_POINT('Ctrl Pts',(4.24193141818231,6.93005810985289,5.74186776419347));
#18493=CARTESIAN_POINT('Ctrl Pts',(4.06292768552231,7.03962740140945,5.75008890030669));
#18494=CARTESIAN_POINT('Ctrl Pts',(3.87966558873464,7.14226410361958,5.75831003641991));
#18495=CARTESIAN_POINT('Ctrl Pts',(3.69270332797605,7.23765360417688,5.76653117253313));
#18496=CARTESIAN_POINT('Ctrl Pts',(3.50572623829061,7.33305067056014,5.77475296070643));
#18497=CARTESIAN_POINT('Ctrl Pts',(3.31504865975612,7.42119925035857,5.78297474887973));
#18498=CARTESIAN_POINT('Ctrl Pts',(3.12125268683624,7.50183105830953,5.79119653705303));
#18499=CARTESIAN_POINT('Ctrl Pts',(2.92745725164848,7.58246264252875,5.79941830241306));
#18500=CARTESIAN_POINT('Ctrl Pts',(2.73054371272274,7.6555773858157,5.80764006777308));
#18501=CARTESIAN_POINT('Ctrl Pts',(2.53111390148152,7.72095525050023,5.81586183313311));
#18502=CARTESIAN_POINT('Ctrl Pts',(2.33164251243531,7.78634674538423,5.82408531259473));
#18503=CARTESIAN_POINT('Ctrl Pts',(2.12965408337915,7.8439980474413,5.83230879205635));
#18504=CARTESIAN_POINT('Ctrl Pts',(1.92576640824912,7.89373874050562,5.84053227151798));
#18505=CARTESIAN_POINT('Ctrl Pts',(1.84338823714769,7.9138358224962,5.84385486175158));
#18506=CARTESIAN_POINT('Ctrl Pts',(1.76070017561212,7.93264210333362,5.84717745198518));
#18507=CARTESIAN_POINT('Ctrl Pts',(1.67774353105856,7.95014869084165,5.85050004221878));
#18508=CARTESIAN_POINT('Ctrl Pts',(1.47242263381648,7.9934781706457,5.85872358129273));
#18509=CARTESIAN_POINT('Ctrl Pts',(1.26538894703182,8.02885649802595,5.86694712036669));
#18510=CARTESIAN_POINT('Ctrl Pts',(1.05727285280546,8.05616916885567,5.87517065944065));
#18511=CARTESIAN_POINT('Ctrl Pts',(0.849194597700014,8.0834768737674,5.88339270333236));
#18512=CARTESIAN_POINT('Ctrl Pts',(0.64003462022648,8.10272181068945,5.89161474722407));
#18513=CARTESIAN_POINT('Ctrl Pts',(0.430430574832467,8.1138410806935,5.89983679111578));
#18514=CARTESIAN_POINT('Ctrl Pts',(0.220849671378751,8.12495912304241,5.90805792722898));
#18515=CARTESIAN_POINT('Ctrl Pts',(0.0108250922942836,8.12795327395779,
5.91627906334217));
#18516=CARTESIAN_POINT('Ctrl Pts',(-0.19900249857376,8.12281266360744,5.92450019945537));
#18517=CARTESIAN_POINT('Ctrl Pts',(-0.40884673193482,8.11767164552915,5.93272198762866));
#18518=CARTESIAN_POINT('Ctrl Pts',(-0.618493650941377,8.10439458157231,
5.94094377580196));
#18519=CARTESIAN_POINT('Ctrl Pts',(-0.827303638729489,8.08302271751385,
5.94916556397526));
#18520=CARTESIAN_POINT('Ctrl Pts',(-1.03611304712544,8.06165091275662,5.95738732933529));
#18521=CARTESIAN_POINT('Ctrl Pts',(-1.24408523582356,8.03218438553973,5.96560909469531));
#18522=CARTESIAN_POINT('Ctrl Pts',(-1.45058620523406,7.99471620657573,5.97383086005534));
#18523=CARTESIAN_POINT('Ctrl Pts',(-1.65713022666894,7.95724021611836,5.98205433951696));
#18524=CARTESIAN_POINT('Ctrl Pts',(-1.86220212582129,7.91175929396889,5.99027781897859));
#18525=CARTESIAN_POINT('Ctrl Pts',(-2.06517749367339,7.85841774673024,5.99850129844022));
#18526=CARTESIAN_POINT('Ctrl Pts',(-2.14718705885023,7.83686578630671,6.00182388867383));
#18527=CARTESIAN_POINT('Ctrl Pts',(-2.22885451172286,7.81403118841705,6.00514647890743));
#18528=CARTESIAN_POINT('Ctrl Pts',(-2.31013929405932,7.7899258022489,6.00846906914104));
#18529=CARTESIAN_POINT('Ctrl Pts',(-2.51132226778267,7.73026404105987,6.016692608215));
#18530=CARTESIAN_POINT('Ctrl Pts',(-2.71022544243532,7.66279478417243,6.02491614728895));
#18531=CARTESIAN_POINT('Ctrl Pts',(-2.90623996210263,7.58771749903604,6.0331396863629));
#18532=CARTESIAN_POINT('Ctrl Pts',(-3.10221884292558,7.51265386425415,6.04136173025461));
#18533=CARTESIAN_POINT('Ctrl Pts',(-3.29530984173093,7.42998506751543,6.04958377414633));
#18534=CARTESIAN_POINT('Ctrl Pts',(-3.48492227952547,7.33995941870028,6.05780581803804));
#18535=CARTESIAN_POINT('Ctrl Pts',(-3.67451378261095,7.24994370942702,6.06602695415124));
#18536=CARTESIAN_POINT('Ctrl Pts',(-3.86062722512228,7.15257289616183,6.07424809026443));
#18537=CARTESIAN_POINT('Ctrl Pts',(-4.04269405550415,7.04814247416235,6.08246922637763));
#18538=CARTESIAN_POINT('Ctrl Pts',(-4.22477532653196,6.94370376925518,6.09069101455093));
#18539=CARTESIAN_POINT('Ctrl Pts',(-4.40280908696486,6.83220448126467,6.09891280272423));
#18540=CARTESIAN_POINT('Ctrl Pts',(-4.57625252091034,6.71398543544456,6.10713459089753));
#18541=CARTESIAN_POINT('Ctrl Pts',(-4.74969547359642,6.59576671765087,6.11535635625755));
#18542=CARTESIAN_POINT('Ctrl Pts',(-4.91854788308649,6.47082844766323,6.12357812161758));
#18543=CARTESIAN_POINT('Ctrl Pts',(-5.08229654968902,6.339554348968,6.1317998869776));
#18544=CARTESIAN_POINT('Ctrl Pts',(-5.24607935517029,6.20825288180235,6.14002336643922));
#18545=CARTESIAN_POINT('Ctrl Pts',(-5.40475606194957,6.07061313163142,6.14824684590084));
#18546=CARTESIAN_POINT('Ctrl Pts',(-5.55784630003058,5.92705931029346,6.15647032536246));
#18547=CARTESIAN_POINT('Ctrl Pts',(-5.61970042543883,5.86905825040111,6.15979291559608));
#18548=CARTESIAN_POINT('Ctrl Pts',(-5.68064297885062,5.81009218470904,6.16311550582971));
#18549=CARTESIAN_POINT('Ctrl Pts',(-5.74064393689372,5.75019084485945,6.16643809606334));
#18550=CARTESIAN_POINT('Ctrl Pts',(-5.8891486239747,5.60193271665247,6.1746616351373));
#18551=CARTESIAN_POINT('Ctrl Pts',(-6.03193098122543,5.4478945007128,6.18288517421126));
#18552=CARTESIAN_POINT('Ctrl Pts',(-6.16855058045022,5.2885415096156,6.19110871328523));
#18553=CARTESIAN_POINT('Ctrl Pts',(-6.30514533985905,5.12921749165983,6.19933075717696));
#18554=CARTESIAN_POINT('Ctrl Pts',(-6.43557938575343,4.96458085100612,6.2075528010687));
#18555=CARTESIAN_POINT('Ctrl Pts',(-6.5594515304958,4.79513119544985,6.21577484496043));
#18556=CARTESIAN_POINT('Ctrl Pts',(-6.68330999877533,4.62570024847347,6.2239959810736));
#18557=CARTESIAN_POINT('Ctrl Pts',(-6.80060783832332,4.45145758551055,6.23221711718678));
#18558=CARTESIAN_POINT('Ctrl Pts',(-6.91098578698644,4.27293377137669,6.24043825329995));
#18559=CARTESIAN_POINT('Ctrl Pts',(-7.02137249028616,4.09439579761098,6.24866004147324));
#18560=CARTESIAN_POINT('Ctrl Pts',(-7.12483804868518,3.91157624367483,6.25688182964653));
#18561=CARTESIAN_POINT('Ctrl Pts',(-7.22106741500805,3.7250332817854,6.26510361781983));
#18562=CARTESIAN_POINT('Ctrl Pts',(-7.31729651432003,3.53849083750306,6.27332538317985));
#18563=CARTESIAN_POINT('Ctrl Pts',(-7.40628932890439,3.34822526928211,6.28154714853988));
#18564=CARTESIAN_POINT('Ctrl Pts',(-7.48777728107325,3.15481837061079,6.2897689138999));
#18565=CARTESIAN_POINT('Ctrl Pts',(-7.56928222212754,2.96137114981138,6.29799239336153));
#18566=CARTESIAN_POINT('Ctrl Pts',(-7.64327906053075,2.76478156207116,6.30621587282316));
#18567=CARTESIAN_POINT('Ctrl Pts',(-7.70954736643835,2.56565137287657,6.31443935228479));
#18568=CARTESIAN_POINT('Ctrl Pts',(-7.73632221606669,2.48519540227155,6.31776194251841));
#18569=CARTESIAN_POINT('Ctrl Pts',(-7.76183597327306,2.40432488902521,6.32108453275202));
#18570=CARTESIAN_POINT('Ctrl Pts',(-7.78607639342532,2.32308027374107,6.32440712298563));
#18571=CARTESIAN_POINT('Ctrl Pts',(-7.84637220828773,2.12099176822143,6.3326717604932));
#18572=CARTESIAN_POINT('Ctrl Pts',(-7.89880495416801,1.916524583584,6.34093639800078));
#18573=CARTESIAN_POINT('Ctrl Pts',(-7.94320769728739,1.71030378595568,6.34920103550835));
#18574=CARTESIAN_POINT('Ctrl Pts',(-7.98760119827069,1.50412591181677,6.35746395278651));
#18575=CARTESIAN_POINT('Ctrl Pts',(-8.02396797252378,1.2961954355431,6.36572687006468));
#18576=CARTESIAN_POINT('Ctrl Pts',(-8.05219193447165,1.08714884580252,6.37398978734284));
#18577=CARTESIAN_POINT('Ctrl Pts',(-8.0804132772077,0.878121655793909,6.38225193781404));
#18578=CARTESIAN_POINT('Ctrl Pts',(-8.1004932758947,0.667978844956448,6.39051408828524));
#18579=CARTESIAN_POINT('Ctrl Pts',(-8.11236743935685,0.457364287371444,
6.39877623875644));
#18580=CARTESIAN_POINT('Ctrl Pts',(-8.1209551967177,0.305041412335285,6.40475167810016));
#18581=CARTESIAN_POINT('Ctrl Pts',(-8.12525186452795,0.152471955905835,
6.41072711744389));
#18582=CARTESIAN_POINT('Ctrl Pts',(-8.12524999939287,-9.93285784619588E-5,
6.41670255678762));
#18583=CARTESIAN_POINT('Origin',(0.,0.,-16.4167025567876));
#18584=CARTESIAN_POINT('',(4.94669362673306,-6.44580471440964,3.12504817176739));
#18585=CARTESIAN_POINT('',(4.94675008185372,-6.44587862049699,3.29164655258555));
#18586=CARTESIAN_POINT('',(4.94675008185374,-6.44587862049697,-16.4167025567876));
#18587=CARTESIAN_POINT('',(-8.12524999971641,6.78850738286463E-5,4.58329744324838));
#18588=CARTESIAN_POINT('Ctrl Pts',(4.94675008185374,-6.44587862049698,3.29164655258555));
#18589=CARTESIAN_POINT('Ctrl Pts',(5.08212104463498,-6.34199110404742,3.29833220814838));
#18590=CARTESIAN_POINT('Ctrl Pts',(5.21420479585878,-6.23384795954413,3.30501786371122));
#18591=CARTESIAN_POINT('Ctrl Pts',(5.3427373285523,-6.12167014797382,3.31170351927405));
#18592=CARTESIAN_POINT('Ctrl Pts',(5.50083585680398,-5.98368837370932,3.31992705834802));
#18593=CARTESIAN_POINT('Ctrl Pts',(5.65361192257898,-5.83955632578681,3.32815059742199));
#18594=CARTESIAN_POINT('Ctrl Pts',(5.8005949295409,-5.68970878216841,3.33637413649596));
#18595=CARTESIAN_POINT('Ctrl Pts',(5.94755121243908,-5.53988848343627,3.34459618038769));
#18596=CARTESIAN_POINT('Ctrl Pts',(6.0887163323222,-5.38435497353434,3.35281822427941));
#18597=CARTESIAN_POINT('Ctrl Pts',(6.22365654899584,-5.22357987616167,3.36104026817114));
#18598=CARTESIAN_POINT('Ctrl Pts',(6.35858186720471,-5.06282252962847,3.36926140428433));
#18599=CARTESIAN_POINT('Ctrl Pts',(6.48728346479563,-4.89682497682462,3.37748254039753));
#18600=CARTESIAN_POINT('Ctrl Pts',(6.60936736013709,-4.72609253625597,3.38570367651073));
#18601=CARTESIAN_POINT('Ctrl Pts',(6.73146093857325,-4.55534655402907,3.39392546468404));
#18602=CARTESIAN_POINT('Ctrl Pts',(6.8469355922835,-4.37986517203383,3.40214725285737));
#18603=CARTESIAN_POINT('Ctrl Pts',(6.95543960683962,-4.20018421478233,3.41036904103068));
#18604=CARTESIAN_POINT('Ctrl Pts',(7.06394332032602,-4.0205037560976,3.41859080639073));
#18605=CARTESIAN_POINT('Ctrl Pts',(7.16547628319758,-3.83662399933009,3.42681257175077));
#18606=CARTESIAN_POINT('Ctrl Pts',(7.25973156458414,-3.64910744877165,3.43503433711082));
#18607=CARTESIAN_POINT('Ctrl Pts',(7.35400649663197,-3.46155180412571,3.44325781657244));
#18608=CARTESIAN_POINT('Ctrl Pts',(7.4410005836328,-3.27035811456371,3.45148129603406));
#18609=CARTESIAN_POINT('Ctrl Pts',(7.52045359721303,-3.07611203545411,3.45970477549568));
#18610=CARTESIAN_POINT('Ctrl Pts',(7.55255555699539,-2.99762942619271,3.46302736572923));
#18611=CARTESIAN_POINT('Ctrl Pts',(7.58342701162677,-2.91864876395072,3.46634995596279));
#18612=CARTESIAN_POINT('Ctrl Pts',(7.61305303611869,-2.83920957869332,3.46967254619634));
#18613=CARTESIAN_POINT('Ctrl Pts',(7.68637859024654,-2.64259452897409,3.47789608527028));
#18614=CARTESIAN_POINT('Ctrl Pts',(7.75209530064891,-2.44310546289366,3.48611962434423));
#18615=CARTESIAN_POINT('Ctrl Pts',(7.80999636316043,-2.24134878363917,3.49434316341818));
#18616=CARTESIAN_POINT('Ctrl Pts',(7.86788689825338,-2.03962878725234,3.50256520730992));
#18617=CARTESIAN_POINT('Ctrl Pts',(7.9179645403325,-1.83564228392911,3.51078725120166));
#18618=CARTESIAN_POINT('Ctrl Pts',(7.96007243934189,-1.63001052847204,3.51900929509341));
#18619=CARTESIAN_POINT('Ctrl Pts',(8.00217568930684,-1.42440147638395,3.52723043120661));
#18620=CARTESIAN_POINT('Ctrl Pts',(8.03631089379098,-1.21714782364372,3.53545156731982));
#18621=CARTESIAN_POINT('Ctrl Pts',(8.0623722088047,-1.00888152386375,3.54367270343301));
#18622=CARTESIAN_POINT('Ctrl Pts',(8.08843559087381,-0.800598705424667,
3.55189449160631));
#18623=CARTESIAN_POINT('Ctrl Pts',(8.10642376468057,-0.591303371794449,
3.56011627977961));
#18624=CARTESIAN_POINT('Ctrl Pts',(8.11628257995049,-0.381634176787381,
3.56833806795291));
#18625=CARTESIAN_POINT('Ctrl Pts',(8.12614136786481,-0.171965563556886,
3.57655983331292));
#18626=CARTESIAN_POINT('Ctrl Pts',(8.12787083120482,0.0380766142421395,
3.58478159867294));
#18627=CARTESIAN_POINT('Ctrl Pts',(8.12146890433173,0.247851565403032,3.59300336403296));
#18628=CARTESIAN_POINT('Ctrl Pts',(8.11506564276316,0.457670251159153,3.60122684349457));
#18629=CARTESIAN_POINT('Ctrl Pts',(8.10052761333665,0.667221304131454,3.60945032295619));
#18630=CARTESIAN_POINT('Ctrl Pts',(8.07790484229059,0.875865812438278,3.61767380241781));
#18631=CARTESIAN_POINT('Ctrl Pts',(8.06876440502367,0.960165920297958,3.62099639265142));
#18632=CARTESIAN_POINT('Ctrl Pts',(8.05830475824943,1.04431808906881,3.62431898288502));
#18633=CARTESIAN_POINT('Ctrl Pts',(8.0465315997878,1.12828045100338,3.62764157311863));
#18634=CARTESIAN_POINT('Ctrl Pts',(8.0173925781733,1.33609053758197,3.63586511219259));
#18635=CARTESIAN_POINT('Ctrl Pts',(7.98019415312815,1.5428049557683,3.64408865126656));
#18636=CARTESIAN_POINT('Ctrl Pts',(7.93504320927252,1.74779198690176,3.65231219034052));
#18637=CARTESIAN_POINT('Ctrl Pts',(7.8899004746428,1.95274174783213,3.66053423423223));
#18638=CARTESIAN_POINT('Ctrl Pts',(7.83680817047664,2.15596446066753,3.66875627812394));
#18639=CARTESIAN_POINT('Ctrl Pts',(7.77592418080798,2.35683913257263,3.67697832201565));
#18640=CARTESIAN_POINT('Ctrl Pts',(7.71504691321255,2.55769162632774,3.68519945812879));
#18641=CARTESIAN_POINT('Ctrl Pts',(7.64637976311568,2.75619631457534,3.69342059424192));
#18642=CARTESIAN_POINT('Ctrl Pts',(7.57013056164728,2.95174708301944,3.70164173035506));
#18643=CARTESIAN_POINT('Ctrl Pts',(7.49387531246663,3.14731336159029,3.70986351852835));
#18644=CARTESIAN_POINT('Ctrl Pts',(7.41003691499807,3.33992497646865,3.71808530670165));
#18645=CARTESIAN_POINT('Ctrl Pts',(7.31887184821249,3.52899453555013,3.72630709487493));
#18646=CARTESIAN_POINT('Ctrl Pts',(7.22770703438496,3.71806357001544,3.73452886023501));
#18647=CARTESIAN_POINT('Ctrl Pts',(7.12921572243173,3.903590303853,3.74275062559509));
#18648=CARTESIAN_POINT('Ctrl Pts',(7.02370121033173,4.08501026565228,3.75097239095517));
#18649=CARTESIAN_POINT('Ctrl Pts',(6.91816470020808,4.26646805050104,3.7591958704168));
#18650=CARTESIAN_POINT('Ctrl Pts',(6.80560221315041,4.44381709788767,3.76741934987843));
#18651=CARTESIAN_POINT('Ctrl Pts',(6.68636195994309,4.61651939269468,3.77564282934006));
#18652=CARTESIAN_POINT('Ctrl Pts',(6.63818448195345,4.68629751529189,3.77896541957368));
#18653=CARTESIAN_POINT('Ctrl Pts',(6.58891738198813,4.75531740069121,3.7822880098073));
#18654=CARTESIAN_POINT('Ctrl Pts',(6.53858560593556,4.82354494499142,3.78561060004092));
#18655=CARTESIAN_POINT('Ctrl Pts',(6.4140125174933,4.9924107505897,3.79383413911488));
#18656=CARTESIAN_POINT('Ctrl Pts',(6.28287399612001,5.15647556011302,3.80205767818884));
#18657=CARTESIAN_POINT('Ctrl Pts',(6.14556482666594,5.31523475716232,3.8102812172628));
#18658=CARTESIAN_POINT('Ctrl Pts',(6.00828062240444,5.47396508903138,3.81850326115448));
#18659=CARTESIAN_POINT('Ctrl Pts',(5.86482820214791,5.62739151079798,3.82672530504616));
#18660=CARTESIAN_POINT('Ctrl Pts',(5.71564209059604,5.77504312145866,3.83494734893784));
#18661=CARTESIAN_POINT('Ctrl Pts',(5.5664724503674,5.9226784302171,3.84316848505104));
#18662=CARTESIAN_POINT('Ctrl Pts',(5.41157059223792,6.06453999339521,3.85138962116423));
#18663=CARTESIAN_POINT('Ctrl Pts',(5.25140787806196,6.20019377606287,3.85961075727743));
#18664=CARTESIAN_POINT('Ctrl Pts',(5.09123246056684,6.33585831812173,3.86783254545073));
#18665=CARTESIAN_POINT('Ctrl Pts',(4.92579557664273,6.46531390322236,3.87605433362403));
#18666=CARTESIAN_POINT('Ctrl Pts',(4.75560245261724,6.58816612382846,3.88427612179732));
#18667=CARTESIAN_POINT('Ctrl Pts',(4.58540980083205,6.71101800355257,3.89249788715736));
#18668=CARTESIAN_POINT('Ctrl Pts',(4.41046117606165,6.82726638500032,3.9007196525174));
#18669=CARTESIAN_POINT('Ctrl Pts',(4.23129206177159,6.93655930923168,3.90894141787744));
#18670=CARTESIAN_POINT('Ctrl Pts',(4.05208559369574,7.04587501922328,3.91716489733906));
#18671=CARTESIAN_POINT('Ctrl Pts',(3.86865713013893,7.14823222150355,3.92538837680069));
#18672=CARTESIAN_POINT('Ctrl Pts',(3.68156905197642,7.24332360715918,3.93361185626231));
#18673=CARTESIAN_POINT('Ctrl Pts',(3.60597854017021,7.28174404837952,3.93693444649594));
#18674=CARTESIAN_POINT('Ctrl Pts',(3.5297908921433,7.31897889775098,3.94025703672957));
#18675=CARTESIAN_POINT('Ctrl Pts',(3.45304428304078,7.35501004362736,3.9435796269632));
#18676=CARTESIAN_POINT('Ctrl Pts',(3.26309346323797,7.44418852040556,3.95180316603715));
#18677=CARTESIAN_POINT('Ctrl Pts',(3.06965525391331,7.52601903234945,3.96002670511109));
#18678=CARTESIAN_POINT('Ctrl Pts',(2.87331708854787,7.60024581649559,3.96825024418503));
#18679=CARTESIAN_POINT('Ctrl Pts',(2.67701462087164,7.67445910492293,3.97647228807672));
#18680=CARTESIAN_POINT('Ctrl Pts',(2.47781352525126,7.7410713205985,3.9846943319684));
#18681=CARTESIAN_POINT('Ctrl Pts',(2.2763201272324,7.79987527085252,3.99291637586009));
#18682=CARTESIAN_POINT('Ctrl Pts',(2.07484897567346,7.85867272868676,4.00113751197329));
#18683=CARTESIAN_POINT('Ctrl Pts',(1.87108631001129,7.90966355964353,4.0093586480865));
#18684=CARTESIAN_POINT('Ctrl Pts',(1.6656532951312,7.9526905298093,4.01757978419971));
#18685=CARTESIAN_POINT('Ctrl Pts',(1.46020398631403,7.99572091266288,4.02580157237302));
#18686=CARTESIAN_POINT('Ctrl Pts',(1.2530843517001,8.03078610956598,4.03402336054634));
#18687=CARTESIAN_POINT('Ctrl Pts',(1.04492646663933,8.05777985811332,4.04224514871966));
#18688=CARTESIAN_POINT('Ctrl Pts',(0.836769159161336,8.08477353176017,4.0504669140797));
#18689=CARTESIAN_POINT('Ctrl Pts',(0.627573899829079,8.10369576659661,4.05868867943974));
#18690=CARTESIAN_POINT('Ctrl Pts',(0.417979158978247,8.1144920349434,4.06691044479978));
#18691=CARTESIAN_POINT('Ctrl Pts',(0.208340721103928,8.12529055413288,4.07513392426139));
#18692=CARTESIAN_POINT('Ctrl Pts',(-0.0016970700738789,8.12795970727399,
4.083357403723));
#18693=CARTESIAN_POINT('Ctrl Pts',(-0.211493351870177,8.12249703752576,
4.09158088318461));
#18694=CARTESIAN_POINT('Ctrl Pts',(-0.29625881887258,8.12028991665438,4.09490347341824));
#18695=CARTESIAN_POINT('Ctrl Pts',(-0.380984862473706,8.1167559026096,4.09822606365188));
#18696=CARTESIAN_POINT('Ctrl Pts',(-0.465629288968856,8.11189724588239,
4.10154865388551));
#18697=CARTESIAN_POINT('Ctrl Pts',(-0.675127511659835,8.09987188294756,
4.10977219295946));
#18698=CARTESIAN_POINT('Ctrl Pts',(-0.88419366157695,8.0797244644846,4.11799573203341));
#18699=CARTESIAN_POINT('Ctrl Pts',(-1.09218938944958,8.05150979009985,4.12621927110737));
#18700=CARTESIAN_POINT('Ctrl Pts',(-1.30014730008499,8.02330024563312,4.13444131499905));
#18701=CARTESIAN_POINT('Ctrl Pts',(-1.50703488500452,7.98702641236962,4.14266335889072));
#18702=CARTESIAN_POINT('Ctrl Pts',(-1.71222030883513,7.94279479632406,4.15088540278239));
#18703=CARTESIAN_POINT('Ctrl Pts',(-1.91738307858027,7.89856806379698,4.15910653889572));
#18704=CARTESIAN_POINT('Ctrl Pts',(-2.12084377423616,7.84638536471089,4.16732767500905));
#18705=CARTESIAN_POINT('Ctrl Pts',(-2.32198129926246,7.7864042027354,4.17554881112237));
#18706=CARTESIAN_POINT('Ctrl Pts',(-2.52313477752521,7.72641828334996,4.18377059929566));
#18707=CARTESIAN_POINT('Ctrl Pts',(-2.7219644335846,7.65863274693165,4.19199238746896));
#18708=CARTESIAN_POINT('Ctrl Pts',(-2.91786384686345,7.58325511463693,4.20021417564225));
#18709=CARTESIAN_POINT('Ctrl Pts',(-3.11376271657489,7.50787769149458,4.20843594100233));
#18710=CARTESIAN_POINT('Ctrl Pts',(-3.30673108547964,7.42490832304518,4.21665770636239));
#18711=CARTESIAN_POINT('Ctrl Pts',(-3.49618154311534,7.33460306902014,4.22487947172247));
#18712=CARTESIAN_POINT('Ctrl Pts',(-3.6856714980252,7.24427898784936,4.23310295118408));
#18713=CARTESIAN_POINT('Ctrl Pts',(-3.87164181020962,7.14661609270801,4.2413264306457));
#18714=CARTESIAN_POINT('Ctrl Pts',(-4.05352775913069,7.04191737160107,4.24954991010731));
#18715=CARTESIAN_POINT('Ctrl Pts',(-4.12701641807567,6.99961521108211,4.25287250034081));
#18716=CARTESIAN_POINT('Ctrl Pts',(-4.19983860586707,6.9561650018275,4.2561950905743));
#18717=CARTESIAN_POINT('Ctrl Pts',(-4.27195829051431,6.91158881347885,4.2595176808078));
#18718=CARTESIAN_POINT('Ctrl Pts',(-4.45045729370785,6.80126102675432,4.26774121988178));
#18719=CARTESIAN_POINT('Ctrl Pts',(-4.6247090100639,6.68399674037906,4.27596475895575));
#18720=CARTESIAN_POINT('Ctrl Pts',(-4.79417819205573,6.56014809477021,4.28418829802973));
#18721=CARTESIAN_POINT('Ctrl Pts',(-4.96361656160669,6.43632196699632,4.29241034192147));
#18722=CARTESIAN_POINT('Ctrl Pts',(-5.12827389430558,6.30591404330055,4.30063238581321));
#18723=CARTESIAN_POINT('Ctrl Pts',(-5.28764529084683,6.16931883117458,4.30885442970495));
#18724=CARTESIAN_POINT('Ctrl Pts',(-5.44699909152857,6.03273870023768,4.31707556581817));
#18725=CARTESIAN_POINT('Ctrl Pts',(-5.6010678973565,5.88997283656444,4.3252967019314));
#18726=CARTESIAN_POINT('Ctrl Pts',(-5.74938053502141,5.74145547975572,4.33351783804462));
#18727=CARTESIAN_POINT('Ctrl Pts',(-5.89770493611548,5.59292634328051,4.34173962621794));
#18728=CARTESIAN_POINT('Ctrl Pts',(-6.04027204652823,5.4386450090076,4.34996141439125));
#18729=CARTESIAN_POINT('Ctrl Pts',(-6.17664741440262,5.27908271204889,4.35818320256457));
#18730=CARTESIAN_POINT('Ctrl Pts',(-6.31302240387277,5.11952085783178,4.36640496792468));
#18731=CARTESIAN_POINT('Ctrl Pts',(-6.4432054956,4.95467829619373,4.37462673328479));
#18732=CARTESIAN_POINT('Ctrl Pts',(-6.56680206628266,4.78505989354008,4.3828484986449));
#18733=CARTESIAN_POINT('Ctrl Pts',(-6.69042440479803,4.61540612826592,4.39107197810657));
#18734=CARTESIAN_POINT('Ctrl Pts',(-6.80745730532773,4.44097477129257,4.39929545756824));
#18735=CARTESIAN_POINT('Ctrl Pts',(-6.91754844226356,4.26230115212863,4.40751893702991));
#18736=CARTESIAN_POINT('Ctrl Pts',(-6.96202933846692,4.19011039336715,4.41084152726329));
#18737=CARTESIAN_POINT('Ctrl Pts',(-7.00537751839709,4.11722742543054,4.41416411749668));
#18738=CARTESIAN_POINT('Ctrl Pts',(-7.04757180538556,4.04368881226468,4.41748670773006));
#18739=CARTESIAN_POINT('Ctrl Pts',(-7.15200429430959,3.86167790621401,4.42571024680401));
#18740=CARTESIAN_POINT('Ctrl Pts',(-7.24939904522159,3.67558965831389,4.43393378587795));
#18741=CARTESIAN_POINT('Ctrl Pts',(-7.33945305402924,3.48598858721609,4.4421573249519));
#18742=CARTESIAN_POINT('Ctrl Pts',(-7.42949068945407,3.29642198888592,4.45037936884362));
#18743=CARTESIAN_POINT('Ctrl Pts',(-7.5121901201584,3.10334410839429,4.45860141273533));
#18744=CARTESIAN_POINT('Ctrl Pts',(-7.58729520233631,2.9073422700302,4.46682345662705));
#18745=CARTESIAN_POINT('Ctrl Pts',(-7.66239199232013,2.71136207181669,4.47504459274021));
#18746=CARTESIAN_POINT('Ctrl Pts',(-7.72989600227281,2.5124588355455,4.48326572885336));
#18747=CARTESIAN_POINT('Ctrl Pts',(-7.7895996643185,2.31123876571616,4.49148686496651));
#18748=CARTESIAN_POINT('Ctrl Pts',(-7.84930806176531,2.11000273609957,4.49970865313979));
#18749=CARTESIAN_POINT('Ctrl Pts',(-7.90121478867765,1.90644978776118,4.50793044131307));
#18750=CARTESIAN_POINT('Ctrl Pts',(-7.94516218416331,1.70120117265459,4.51615222948634));
#18751=CARTESIAN_POINT('Ctrl Pts',(-7.98910945770717,1.49595312705577,4.52437399484644));
#18752=CARTESIAN_POINT('Ctrl Pts',(-8.02509738488821,1.28900971306024,4.53259576020654));
#18753=CARTESIAN_POINT('Ctrl Pts',(-8.05301934218722,1.08100279225286,4.54081752556664));
#18754=CARTESIAN_POINT('Ctrl Pts',(-8.0809471207503,0.872952505459324,4.54904100502818));
#18755=CARTESIAN_POINT('Ctrl Pts',(-8.10080553078993,0.663838561277428,
4.55726448448973));
#18756=CARTESIAN_POINT('Ctrl Pts',(-8.11253964888555,0.454299469248954,
4.56548796395127));
#18757=CARTESIAN_POINT('Ctrl Pts',(-8.11728066713311,0.369637916434513,
4.56881055418497));
#18758=CARTESIAN_POINT('Ctrl Pts',(-8.12069601977494,0.284907006571542,
4.57213314441867));
#18759=CARTESIAN_POINT('Ctrl Pts',(-8.12278449485915,0.200148975954921,
4.57545573465237));
#18760=CARTESIAN_POINT('Ctrl Pts',(-8.12442751148105,0.133469294594977,
4.57806963750571));
#18761=CARTESIAN_POINT('Ctrl Pts',(-8.12524944242962,0.0667693416606271,
4.58068354035906));
#18762=CARTESIAN_POINT('Ctrl Pts',(-8.12524999971641,6.78859918389947E-5,
4.5832974432124));
#18763=CARTESIAN_POINT('Ctrl Pts',(-8.12524999971641,6.78850738330637E-5,
4.58329744324837));
#18764=CARTESIAN_POINT('Ctrl Pts',(-8.12525174938836,-0.209352554230827,
4.59150423091677));
#18765=CARTESIAN_POINT('Ctrl Pts',(-8.11715274258138,-0.418809030230974,
4.59971101858517));
#18766=CARTESIAN_POINT('Ctrl Pts',(-8.1009706810933,-0.627663593469262,
4.60791780625356));
#18767=CARTESIAN_POINT('Ctrl Pts',(-8.08479158305025,-0.836479908860154,
4.6161230910007));
#18768=CARTESIAN_POINT('Ctrl Pts',(-8.06053240758662,-1.04469423516969,
4.62432837574785));
#18769=CARTESIAN_POINT('Ctrl Pts',(-8.02826285212299,-1.25167213747131,
4.63253366049499));
#18770=CARTESIAN_POINT('Ctrl Pts',(-7.99519766829729,-1.46375322409101,
4.64094125225162));
#18771=CARTESIAN_POINT('Ctrl Pts',(-7.95372205275651,-1.67453581134853,
4.64934884400826));
#18772=CARTESIAN_POINT('Ctrl Pts',(-7.90396714321867,-1.88334568293228,
4.6577564357649));
#18773=CARTESIAN_POINT('Ctrl Pts',(-7.8554106962377,-2.08712588377755,4.66596151114663));
#18774=CARTESIAN_POINT('Ctrl Pts',(-7.79896928620375,-2.2890270092906,4.67416658652835));
#18775=CARTESIAN_POINT('Ctrl Pts',(-7.73481614457164,-2.4884346027521,4.68237166191008));
#18776=CARTESIAN_POINT('Ctrl Pts',(-7.66828787637243,-2.69522481631387,
4.69088051185417));
#18777=CARTESIAN_POINT('Ctrl Pts',(-7.59346606056834,-2.89933301398041,
4.69938936179826));
#18778=CARTESIAN_POINT('Ctrl Pts',(-7.5106000776987,-3.10009258496779,4.70789821174236));
#18779=CARTESIAN_POINT('Ctrl Pts',(-7.42773409482906,-3.30085215595517,
4.71640706168646));
#18780=CARTESIAN_POINT('Ctrl Pts',(-7.33682408930247,-3.49826277449,4.72491591163056));
#18781=CARTESIAN_POINT('Ctrl Pts',(-7.23817473186267,-3.69168174596954,
4.73342476157465));
#18782=CARTESIAN_POINT('Ctrl Pts',(-7.14283319324639,-3.87861517176193,
4.74164830064859));
#18783=CARTESIAN_POINT('Ctrl Pts',(-7.04023067284676,-4.06188354415428,
4.74987183972253));
#18784=CARTESIAN_POINT('Ctrl Pts',(-6.93067430172067,-4.24092457914176,
4.75809537879648));
#18785=CARTESIAN_POINT('Ctrl Pts',(-6.82113784984571,-4.41993306135935,
4.76631742268818));
#18786=CARTESIAN_POINT('Ctrl Pts',(-6.70465022456719,-4.59471548876772,
4.77453946657988));
#18787=CARTESIAN_POINT('Ctrl Pts',(-6.58156326671015,-4.7647363545942,4.78276151047158));
#18788=CARTESIAN_POINT('Ctrl Pts',(-6.45848989862347,-4.93473844877693,
4.79098264658483));
#18789=CARTESIAN_POINT('Ctrl Pts',(-6.32881882550354,-5.09997979213808,
4.79920378269808));
#18790=CARTESIAN_POINT('Ctrl Pts',(-6.19294424840373,-5.25995523732505,
4.80742491881133));
#18791=CARTESIAN_POINT('Ctrl Pts',(-6.0570588944014,-5.41994337097673,4.81564670698462));
#18792=CARTESIAN_POINT('Ctrl Pts',(-5.9149692422097,-5.57466454540419,4.82386849515791));
#18793=CARTESIAN_POINT('Ctrl Pts',(-5.767109370974,-5.72364718214915,4.8320902833312));
#18794=CARTESIAN_POINT('Ctrl Pts',(-5.61924991000991,-5.87262940550712,
4.84031204869123));
#18795=CARTESIAN_POINT('Ctrl Pts',(-5.46562047170121,-6.01587291559778,
4.84853381405125));
#18796=CARTESIAN_POINT('Ctrl Pts',(-5.30669191477893,-6.15294307499427,
4.85675557941128));
#18797=CARTESIAN_POINT('Ctrl Pts',(-5.14773022389095,-6.29004181124344,
4.86497905887289));
#18798=CARTESIAN_POINT('Ctrl Pts',(-4.98346743074074,-6.42096443300091,
4.87320253833451));
#18799=CARTESIAN_POINT('Ctrl Pts',(-4.8144082182703,-6.5453159641343,4.88142601779612));
#18800=CARTESIAN_POINT('Ctrl Pts',(-4.74610203584738,-6.59555858768641,
4.88474860802973));
#18801=CARTESIAN_POINT('Ctrl Pts',(-4.67701322007725,-6.6447289777089,4.88807119826334));
#18802=CARTESIAN_POINT('Ctrl Pts',(-4.60717647814811,-6.69280303473057,
4.89139378849695));
#18803=CARTESIAN_POINT('Ctrl Pts',(-4.43432784630585,-6.8117881814279,4.8996173275709));
#18804=CARTESIAN_POINT('Ctrl Pts',(-4.25683930315909,-6.92409308142546,
4.90784086664485));
#18805=CARTESIAN_POINT('Ctrl Pts',(-4.07524866129991,-7.02936952443626,
4.9160644057188));
#18806=CARTESIAN_POINT('Ctrl Pts',(-3.89369103577317,-7.13462682636136,
4.92428644961053));
#18807=CARTESIAN_POINT('Ctrl Pts',(-3.70803305516046,-7.23285807398075,
4.93250849350227));
#18808=CARTESIAN_POINT('Ctrl Pts',(-3.51883909810416,-7.32375989257932,
4.940730537394));
#18809=CARTESIAN_POINT('Ctrl Pts',(-3.32966602955252,-7.41465167490036,
4.94895167350725));
#18810=CARTESIAN_POINT('Ctrl Pts',(-3.13695802971415,-7.49821551611294,
4.9571728096205));
#18811=CARTESIAN_POINT('Ctrl Pts',(-2.94130227151591,-7.57419490837642,
4.96539394573375));
#18812=CARTESIAN_POINT('Ctrl Pts',(-2.74563099486588,-7.65018032695136,
4.97361573390705));
#18813=CARTESIAN_POINT('Ctrl Pts',(-2.5470117666796,-7.71857998536448,4.98183752208036));
#18814=CARTESIAN_POINT('Ctrl Pts',(-2.34605084327077,-7.77918588306569,
4.99005931025366));
#18815=CARTESIAN_POINT('Ctrl Pts',(-2.1450904774757,-7.83979161260145,4.99828107561367));
#18816=CARTESIAN_POINT('Ctrl Pts',(-1.94178871260472,-7.89260354210846,
5.00650284097367));
#18817=CARTESIAN_POINT('Ctrl Pts',(-1.73676655799566,-7.93746366829656,
5.01472460633368));
#18818=CARTESIAN_POINT('Ctrl Pts',(-1.53170165967014,-7.98233314707642,
5.0229480857953));
#18819=CARTESIAN_POINT('Ctrl Pts',(-1.32491594324953,-8.01924744763745,
5.03117156525693));
#18820=CARTESIAN_POINT('Ctrl Pts',(-1.11704127698926,-8.04809954883774,
5.03939504471856));
#18821=CARTESIAN_POINT('Ctrl Pts',(-1.03305221382633,-8.05975686617077,
5.04271763495212));
#18822=CARTESIAN_POINT('Ctrl Pts',(-0.948885478957651,-8.0700986484556,
5.04604022518568));
#18823=CARTESIAN_POINT('Ctrl Pts',(-0.864583067614918,-8.07912022943671,
5.04936281541924));
#18824=CARTESIAN_POINT('Ctrl Pts',(-0.65593134562326,-8.10144899058145,
5.05758635449319));
#18825=CARTESIAN_POINT('Ctrl Pts',(-0.446380276048424,-8.1156940862947,
5.06580989356714));
#18826=CARTESIAN_POINT('Ctrl Pts',(-0.236568592441918,-8.12180539434245,
5.0740334326411));
#18827=CARTESIAN_POINT('Ctrl Pts',(-0.0267950562442058,-8.12791559124823,
5.08225547653279));
#18828=CARTESIAN_POINT('Ctrl Pts',(0.183238704748132,-8.12589494354887,
5.09047752042449));
#18829=CARTESIAN_POINT('Ctrl Pts',(0.392891944367202,-8.11574540523243,
5.09869956431618));
#18830=CARTESIAN_POINT('Ctrl Pts',(0.602522036615081,-8.10559698750508,
5.10692070042939));
#18831=CARTESIAN_POINT('Ctrl Pts',(0.811771396891179,-8.08732148522944,
5.11514183654259));
#18832=CARTESIAN_POINT('Ctrl Pts',(1.02000155037131,-8.06097291893107,5.12336297265579));
#18833=CARTESIAN_POINT('Ctrl Pts',(1.22824821964307,-8.03462226279402,5.13158476082908));
#18834=CARTESIAN_POINT('Ctrl Pts',(1.43547522765356,-8.00019729762124,5.13980654900237));
#18835=CARTESIAN_POINT('Ctrl Pts',(1.6410504152354,-7.95780378604271,5.14802833717566));
#18836=CARTESIAN_POINT('Ctrl Pts',(1.84662503240088,-7.91541039209488,5.15625010253567));
#18837=CARTESIAN_POINT('Ctrl Pts',(2.05054754999661,-7.86504855817847,5.16447186789569));
#18838=CARTESIAN_POINT('Ctrl Pts',(2.25219664192422,-7.80687503733762,5.1726936332557));
#18839=CARTESIAN_POINT('Ctrl Pts',(2.45388777434055,-7.74868938828324,5.18091711271733));
#18840=CARTESIAN_POINT('Ctrl Pts',(2.65330425080242,-7.68268888058018,5.18914059217896));
#18841=CARTESIAN_POINT('Ctrl Pts',(2.84983947156939,-7.60908026957168,5.19736407164059));
#18842=CARTESIAN_POINT('Ctrl Pts',(2.92924697883384,-7.5793396648568,5.20068666187423));
#18843=CARTESIAN_POINT('Ctrl Pts',(3.00818432847376,-7.54835762890888,5.20400925210788));
#18844=CARTESIAN_POINT('Ctrl Pts',(3.08661236960119,-7.51615005453756,5.20733184234153));
#18845=CARTESIAN_POINT('Ctrl Pts',(3.28072594193355,-7.43643459527703,5.21555542985409));
#18846=CARTESIAN_POINT('Ctrl Pts',(3.47178127225479,-7.34918234703222,5.22377901736665));
#18847=CARTESIAN_POINT('Ctrl Pts',(3.6591928060199,-7.25465337358528,5.23200260487921));
#18848=CARTESIAN_POINT('Ctrl Pts',(3.84656772804117,-7.16014286682761,5.24022458587443));
#18849=CARTESIAN_POINT('Ctrl Pts',(4.03030001128134,-7.05835860533478,5.24844656686964));
#18850=CARTESIAN_POINT('Ctrl Pts',(4.20982715084995,-6.9496073934048,5.25666854786486));
#18851=CARTESIAN_POINT('Ctrl Pts',(4.38934121253718,-6.84086410359429,5.26488992991947));
#18852=CARTESIAN_POINT('Ctrl Pts',(4.56465048924521,-6.72515502819134,5.2731113119741));
#18853=CARTESIAN_POINT('Ctrl Pts',(4.73521920437887,-6.60283171442234,5.28133269402872));
#18854=CARTESIAN_POINT('Ctrl Pts',(4.80657126731715,-6.55166159933984,5.28477185090658));
#18855=CARTESIAN_POINT('Ctrl Pts',(4.87709411933547,-6.4993345818291,5.28821100778445));
#18856=CARTESIAN_POINT('Ctrl Pts',(4.94675008185375,-6.44587862049697,5.29165016466231));
#18857=CARTESIAN_POINT('',(-8.12526471614247,-0.000101443950621347,4.41670255650755));
#18858=CARTESIAN_POINT('Ctrl Pts',(-8.12524999936665,-0.000101450914391436,
4.41670255678762));
#18859=CARTESIAN_POINT('Ctrl Pts',(-8.12524871677588,-0.102824730074738,
4.42072797116447));
#18860=CARTESIAN_POINT('Ctrl Pts',(-8.12329924737115,-0.205542899283528,
4.42475338554132));
#18861=CARTESIAN_POINT('Ctrl Pts',(-8.11940320204833,-0.308186964466829,
4.42877879991817));
#18862=CARTESIAN_POINT('Ctrl Pts',(-8.11144395165902,-0.517879036318932,
4.43700233899213));
#18863=CARTESIAN_POINT('Ctrl Pts',(-8.09535579262662,-0.727296668458236,
4.44522587806608));
#18864=CARTESIAN_POINT('Ctrl Pts',(-8.07118113153707,-0.935800568721758,
4.45344941714004));
#18865=CARTESIAN_POINT('Ctrl Pts',(-8.04701086582079,-1.14426655935471,
4.46167146103176));
#18866=CARTESIAN_POINT('Ctrl Pts',(-8.01475706648258,-1.35181885686601,
4.46989350492348));
#18867=CARTESIAN_POINT('Ctrl Pts',(-7.97451396314443,-1.55782367876292,
4.4781155488152));
#18868=CARTESIAN_POINT('Ctrl Pts',(-7.93427530296225,-1.76380575610296,
4.48633668492844));
#18869=CARTESIAN_POINT('Ctrl Pts',(-7.88604915634932,-1.9682404095808,4.49455782104168));
#18870=CARTESIAN_POINT('Ctrl Pts',(-7.82998094929889,-2.17050360426248,
4.50277895715491));
#18871=CARTESIAN_POINT('Ctrl Pts',(-7.7739082951942,-2.37278284146538,4.51100074532821));
#18872=CARTESIAN_POINT('Ctrl Pts',(-7.7099924140863,-2.57288999080897,4.5192225335015));
#18873=CARTESIAN_POINT('Ctrl Pts',(-7.63842902472862,-2.77021472032103,
4.5274443216748));
#18874=CARTESIAN_POINT('Ctrl Pts',(-7.56686583394015,-2.9675389023099,4.53566608703483));
#18875=CARTESIAN_POINT('Ctrl Pts',(-7.48765528043779,-3.16208040356892,
4.54388785239487));
#18876=CARTESIAN_POINT('Ctrl Pts',(-7.40104198117546,-3.35324695711164,
4.5521096177549));
#18877=CARTESIAN_POINT('Ctrl Pts',(-7.31441062447808,-3.54445336570725,
4.56033309721653));
#18878=CARTESIAN_POINT('Ctrl Pts',(-7.22037356058989,-3.73228315226096,
4.56855657667816));
#18879=CARTESIAN_POINT('Ctrl Pts',(-7.11922276604786,-3.91616582512613,
4.57678005613979));
#18880=CARTESIAN_POINT('Ctrl Pts',(-7.07835409924694,-3.99046123448811,
4.58010264637334));
#18881=CARTESIAN_POINT('Ctrl Pts',(-7.03632467150822,-4.06411256796687,
4.5834252366069));
#18882=CARTESIAN_POINT('Ctrl Pts',(-6.99315584937157,-4.13708337224428,
4.58674782684045));
#18883=CARTESIAN_POINT('Ctrl Pts',(-6.88631134834553,-4.3176889293709,4.59497136591442));
#18884=CARTESIAN_POINT('Ctrl Pts',(-6.77244926389735,-4.49418255315695,
4.60319490498838));
#18885=CARTESIAN_POINT('Ctrl Pts',(-6.6519112874456,-4.66602226596207,4.61141844406236));
#18886=CARTESIAN_POINT('Ctrl Pts',(-6.53139522689179,-4.83783073532244,
4.61964048795407));
#18887=CARTESIAN_POINT('Ctrl Pts',(-6.40420586621263,-5.00498674120909,
4.62786253184579));
#18888=CARTESIAN_POINT('Ctrl Pts',(-6.27072784462478,-5.1669778266553,4.63608457573751));
#18889=CARTESIAN_POINT('Ctrl Pts',(-6.13726456006332,-5.32895102700796,
4.64430571185073));
#18890=CARTESIAN_POINT('Ctrl Pts',(-5.99751418825371,-5.48576021786953,
4.65252684796396));
#18891=CARTESIAN_POINT('Ctrl Pts',(-5.8519017472633,-5.63692589119963,4.66074798407718));
#18892=CARTESIAN_POINT('Ctrl Pts',(-5.70627775701031,-5.78810355424738,
4.66896977225048));
#18893=CARTESIAN_POINT('Ctrl Pts',(-5.55479097127226,-5.93363659112568,
4.67719156042378));
#18894=CARTESIAN_POINT('Ctrl Pts',(-5.39790410898977,-6.0730814906974,4.68541334859708));
#18895=CARTESIAN_POINT('Ctrl Pts',(-5.24101768202619,-6.21252600334697,
4.69363511395712));
#18896=CARTESIAN_POINT('Ctrl Pts',(-5.07873143072443,-6.34588221856302,
4.70185687931717));
#18897=CARTESIAN_POINT('Ctrl Pts',(-4.91154247158541,-6.47274579388938,
4.71007864467722));
#18898=CARTESIAN_POINT('Ctrl Pts',(-4.74431865632401,-6.59963581816506,
4.71830212413885));
#18899=CARTESIAN_POINT('Ctrl Pts',(-4.57219032628825,-6.72003032011855,
4.72652560360047));
#18900=CARTESIAN_POINT('Ctrl Pts',(-4.39568587584185,-6.83356665610459,
4.7347490830621));
#18901=CARTESIAN_POINT('Ctrl Pts',(-4.32437154156672,-6.87943954030895,
4.73807167329565));
#18902=CARTESIAN_POINT('Ctrl Pts',(-4.25234315591362,-6.9241933488556,4.74139426352919));
#18903=CARTESIAN_POINT('Ctrl Pts',(-4.17963686516321,-6.96780619979263,
4.74471685376274));
#18904=CARTESIAN_POINT('Ctrl Pts',(-3.99968598922559,-7.07574968923837,
4.75294039283671));
#18905=CARTESIAN_POINT('Ctrl Pts',(-3.81552202047381,-7.17673585722949,
4.76116393191067));
#18906=CARTESIAN_POINT('Ctrl Pts',(-3.62770349366205,-7.27045080614484,
4.76938747098463));
#18907=CARTESIAN_POINT('Ctrl Pts',(-3.43991911552068,-7.36414871605475,
4.77760951487635));
#18908=CARTESIAN_POINT('Ctrl Pts',(-3.24848176928581,-7.4505779139023,4.78583155876808));
#18909=CARTESIAN_POINT('Ctrl Pts',(-3.05397370005434,-7.52947091115149,
4.79405360265981));
#18910=CARTESIAN_POINT('Ctrl Pts',(-2.8594871060484,-7.60835519799129,4.80227473877301));
#18911=CARTESIAN_POINT('Ctrl Pts',(-2.66193073911324,-7.67970483459022,
4.81049587488622));
#18912=CARTESIAN_POINT('Ctrl Pts',(-2.46190666328045,-7.74330053296366,
4.81871701099942));
#18913=CARTESIAN_POINT('Ctrl Pts',(-2.26186672252148,-7.8069012754352,4.82693879917272));
#18914=CARTESIAN_POINT('Ctrl Pts',(-2.05935896206095,-7.8627467589547,4.83516058734602));
#18915=CARTESIAN_POINT('Ctrl Pts',(-1.85500145864965,-7.91066730123999,
4.84338237551932));
#18916=CARTESIAN_POINT('Ctrl Pts',(-1.65064452227567,-7.95858771055862,
4.85160414087936));
#18917=CARTESIAN_POINT('Ctrl Pts',(-1.44443814097656,-7.99858315792208,
4.8598259062394));
#18918=CARTESIAN_POINT('Ctrl Pts',(-1.23701198916193,-8.03053478301225,
4.86804767159944));
#18919=CARTESIAN_POINT('Ctrl Pts',(-1.02954259243837,-8.06249306948579,
4.87627115106106));
#18920=CARTESIAN_POINT('Ctrl Pts',(-0.820853208724146,-8.08640413860473,
4.88449463052268));
#18921=CARTESIAN_POINT('Ctrl Pts',(-0.611581162014199,-8.10220069146459,
4.89271810998429));
#18922=CARTESIAN_POINT('Ctrl Pts',(-0.527027505401506,-8.10858308379637,
4.89604070021787));
#18923=CARTESIAN_POINT('Ctrl Pts',(-0.442378789507941,-8.11364140534786,
4.89936329045145));
#18924=CARTESIAN_POINT('Ctrl Pts',(-0.35767721917171,-8.11737362509485,
4.90268588068503));
#18925=CARTESIAN_POINT('Ctrl Pts',(-0.148037563265098,-8.12661101302548,
4.91090941975899));
#18926=CARTESIAN_POINT('Ctrl Pts',(0.0619941821116159,-8.12772431708582,
4.91913295883295));
#18927=CARTESIAN_POINT('Ctrl Pts',(0.27177739917805,-8.12070345523071,4.92735649790691));
#18928=CARTESIAN_POINT('Ctrl Pts',(0.481522474011634,-8.11368386989024,
4.93557854179862));
#18929=CARTESIAN_POINT('Ctrl Pts',(0.691018816098849,-8.09853308027499,
4.94380058569034));
#18930=CARTESIAN_POINT('Ctrl Pts',(0.899627055477995,-8.07529310449794,
4.95202262958205));
#18931=CARTESIAN_POINT('Ctrl Pts',(1.10821226286226,-8.0520556945975,4.96024376569527));
#18932=CARTESIAN_POINT('Ctrl Pts',(1.31590927029149,-8.02073091423877,4.96846490180849));
#18933=CARTESIAN_POINT('Ctrl Pts',(1.5220842305929,-7.98141260413722,4.97668603792171));
#18934=CARTESIAN_POINT('Ctrl Pts',(1.72827554367802,-7.94209117550071,4.98490782609501));
#18935=CARTESIAN_POINT('Ctrl Pts',(1.93294427820473,-7.89477500296424,4.99312961426832));
#18936=CARTESIAN_POINT('Ctrl Pts',(2.13546612589927,-7.83960917314356,5.00135140244162));
#18937=CARTESIAN_POINT('Ctrl Pts',(2.33798741164973,-7.78444349639335,5.00957316780165));
#18938=CARTESIAN_POINT('Ctrl Pts',(2.53836153862907,-7.7214282860434,5.01779493316167));
#18939=CARTESIAN_POINT('Ctrl Pts',(2.73597819902793,-7.65075884190215,5.0260166985217));
#18940=CARTESIAN_POINT('Ctrl Pts',(2.93363605921998,-7.58007466435493,5.03424017798333));
#18941=CARTESIAN_POINT('Ctrl Pts',(3.12853502661477,-7.50173316443347,5.04246365744495));
#18942=CARTESIAN_POINT('Ctrl Pts',(3.32008261774654,-7.4159786254976,5.05068713690658));
#18943=CARTESIAN_POINT('Ctrl Pts',(3.39747493793533,-7.38133061611386,5.05400972714016));
#18944=CARTESIAN_POINT('Ctrl Pts',(3.47432038990769,-7.34547300561736,5.05733231737374));
#18945=CARTESIAN_POINT('Ctrl Pts',(3.55058089322787,-7.30842410394643,5.06065490760732));
#18946=CARTESIAN_POINT('Ctrl Pts',(3.73932684629326,-7.21672748575672,5.06887837103831));
#18947=CARTESIAN_POINT('Ctrl Pts',(3.92454934907012,-7.11770029217112,5.0771018344693));
#18948=CARTESIAN_POINT('Ctrl Pts',(4.10568028118637,-7.01163868087749,5.08532529790029));
#18949=CARTESIAN_POINT('Ctrl Pts',(4.28678357617951,-6.90559325256141,5.09354750658773));
#18950=CARTESIAN_POINT('Ctrl Pts',(4.46379629155707,-6.79251569672306,5.10176971527516));
#18951=CARTESIAN_POINT('Ctrl Pts',(4.63617616371462,-6.67274742077837,5.10999192396259));
#18952=CARTESIAN_POINT('Ctrl Pts',(4.74146819312724,-6.59959128789795,5.11501416367142));
#18953=CARTESIAN_POINT('Ctrl Pts',(4.8450322541169,-6.52393976658856,5.12003640338026));
#18954=CARTESIAN_POINT('Ctrl Pts',(4.94675008185377,-6.44587862049696,5.12505864308909));
#18955=CARTESIAN_POINT('Ctrl Pts',(4.94669362673306,-6.44580471440964,3.12504817176739));
#18956=CARTESIAN_POINT('Ctrl Pts',(5.21676564029461,-6.2389782961655,3.13837430935821));
#18957=CARTESIAN_POINT('Ctrl Pts',(6.4896144375474,-5.13135356726175,3.20435678925645));
#18958=CARTESIAN_POINT('Ctrl Pts',(8.10215992848685,-2.45656664941747,3.32299561146213));
#18959=CARTESIAN_POINT('Ctrl Pts',(8.29443749013271,1.69765188778186,3.48096463838442));
#18960=CARTESIAN_POINT('Ctrl Pts',(6.4854770730954,5.44226996244785,3.63893366530671));
#18961=CARTESIAN_POINT('Ctrl Pts',(3.11173507273828,7.87380594419869,3.796902692229));
#18962=CARTESIAN_POINT('Ctrl Pts',(-1.01278989687652,8.40559170044518,3.95487171915129));
#18963=CARTESIAN_POINT('Ctrl Pts',(-4.8929542804399,6.90932077843641,4.11284074607358));
#18964=CARTESIAN_POINT('Ctrl Pts',(-7.52378000230581,3.82661413385391,4.2667843549656));
#18965=CARTESIAN_POINT('Ctrl Pts',(-8.12504676703811,1.2409840046644,4.36807162155021));
#18966=CARTESIAN_POINT('Ctrl Pts',(-8.12582592545285,-0.000101178394316476,
4.41670254582737));
#18967=CARTESIAN_POINT('Origin',(0.,0.,-16.4167025567876));
#18968=CARTESIAN_POINT('',(4.94675008185375,-6.44587862049697,1.12505977544705));
#18969=CARTESIAN_POINT('',(4.94675008185373,-6.44587862049698,1.2916563605374));
#18970=CARTESIAN_POINT('',(4.94675008185374,-6.44587862049697,-16.4167025567876));
#18971=CARTESIAN_POINT('',(-8.1252499990086,0.000126927995773117,2.58329744318944));
#18972=CARTESIAN_POINT('Ctrl Pts',(4.94675008185373,-6.44587862049698,1.2916563605374));
#18973=CARTESIAN_POINT('Ctrl Pts',(5.11324136688352,-6.31810848606874,1.29987801001623));
#18974=CARTESIAN_POINT('Ctrl Pts',(5.27479522180978,-6.18387253167384,1.30809965949505));
#18975=CARTESIAN_POINT('Ctrl Pts',(5.43091670084337,-6.04357769462763,1.31632130897387));
#18976=CARTESIAN_POINT('Ctrl Pts',(5.58876949804491,-5.90172704987481,1.32463413290993));
#18977=CARTESIAN_POINT('Ctrl Pts',(5.74106847034745,-5.75368252541814,1.33294695684599));
#18978=CARTESIAN_POINT('Ctrl Pts',(5.88733799517582,-5.59990525750742,1.34125978078205));
#18979=CARTESIAN_POINT('Ctrl Pts',(6.0320043272919,-5.44781347121373,1.34948149169392));
#18980=CARTESIAN_POINT('Ctrl Pts',(6.17077252345175,-5.29011420496733,1.3577032026058));
#18981=CARTESIAN_POINT('Ctrl Pts',(6.30322044694293,-5.12728968946953,1.36592491351767));
#18982=CARTESIAN_POINT('Ctrl Pts',(6.4378700528428,-4.9617585413419,1.37428329396582));
#18983=CARTESIAN_POINT('Ctrl Pts',(6.56598720440906,-4.79093048482667,1.38264167441398));
#18984=CARTESIAN_POINT('Ctrl Pts',(6.68717150955179,-4.61534665700626,1.39100005486213));
#18985=CARTESIAN_POINT('Ctrl Pts',(6.80835581469451,-4.43976282918586,1.39935843531028));
#18986=CARTESIAN_POINT('Ctrl Pts',(6.92260709824771,-4.25942349788531,1.40771681575842));
#18987=CARTESIAN_POINT('Ctrl Pts',(7.02957126271241,-4.07490066442704,1.41607519620657));
#18988=CARTESIAN_POINT('Ctrl Pts',(7.13480983033269,-3.89335464119984,1.42429873528053));
#18989=CARTESIAN_POINT('Ctrl Pts',(7.23302880961726,-3.70770010820867,1.43252227435448));
#18990=CARTESIAN_POINT('Ctrl Pts',(7.32392269616285,-3.5185002349198,1.44074581342844));
#18991=CARTESIAN_POINT('Ctrl Pts',(7.41480005662104,-3.32933476145429,1.44896785732015));
#18992=CARTESIAN_POINT('Ctrl Pts',(7.49835485486565,-3.13662549996389,1.45718990121187));
#18993=CARTESIAN_POINT('Ctrl Pts',(7.57432834519024,-2.94095863312419,1.46541194510358));
#18994=CARTESIAN_POINT('Ctrl Pts',(7.65029344744221,-2.74531336945002,1.47363308121679));
#18995=CARTESIAN_POINT('Ctrl Pts',(7.71867880617511,-2.54671142718753,1.48185421733));
#18996=CARTESIAN_POINT('Ctrl Pts',(7.77927416741292,-2.34575808444135,1.49007535344321));
#18997=CARTESIAN_POINT('Ctrl Pts',(7.8398743347768,-2.14478880306424,1.4982971416165));
#18998=CARTESIAN_POINT('Ctrl Pts',(7.89268318240884,-1.94146803017562,1.5065189297898));
#18999=CARTESIAN_POINT('Ctrl Pts',(7.93754029609987,-1.73641631249272,1.5147407179631));
#19000=CARTESIAN_POINT('Ctrl Pts',(7.98239728532437,-1.53136516377361,1.52296248332313));
#19001=CARTESIAN_POINT('Ctrl Pts',(8.01930252434898,-1.32458336856255,1.53118424868316));
#19002=CARTESIAN_POINT('Ctrl Pts',(8.0481465887886,-1.1167023094229,1.53940601404319));
#19003=CARTESIAN_POINT('Ctrl Pts',(8.07699666673683,-0.90877791053336,1.54762949350481));
#19004=CARTESIAN_POINT('Ctrl Pts',(8.09778217215948,-0.699754082069268,
1.55585297296643));
#19005=CARTESIAN_POINT('Ctrl Pts',(8.11044535078226,-0.49026908374332,1.56407645242805));
#19006=CARTESIAN_POINT('Ctrl Pts',(8.11556174388749,-0.405629386791053,
1.56739904266166));
#19007=CARTESIAN_POINT('Ctrl Pts',(8.11935279197638,-0.320914454967553,
1.57072163289526));
#19008=CARTESIAN_POINT('Ctrl Pts',(8.12181709581718,-0.236166518778118,
1.57404422312887));
#19009=CARTESIAN_POINT('Ctrl Pts',(8.12791634294069,-0.0264121055970575,
1.58226776220283));
#19010=CARTESIAN_POINT('Ctrl Pts',(8.12588654852,0.183612782086546,1.59049130127679));
#19011=CARTESIAN_POINT('Ctrl Pts',(8.1157272180226,0.393267447352448,1.59871484035075));
#19012=CARTESIAN_POINT('Ctrl Pts',(8.10556973466795,0.602883993758469,1.60693688424246));
#19013=CARTESIAN_POINT('Ctrl Pts',(8.0872856796049,0.81213015765241,1.61515892813417));
#19014=CARTESIAN_POINT('Ctrl Pts',(8.06092663395265,1.02036726943433,1.62338097202588));
#19015=CARTESIAN_POINT('Ctrl Pts',(8.03457049854694,1.22858139019665,1.6316021081391));
#19016=CARTESIAN_POINT('Ctrl Pts',(8.00014118950747,1.43578638878158,1.63982324425231));
#19017=CARTESIAN_POINT('Ctrl Pts',(7.95774202210878,1.64134989324762,1.64804438036553));
#19018=CARTESIAN_POINT('Ctrl Pts',(7.91533949181666,1.84692970199986,1.65626616853883));
#19019=CARTESIAN_POINT('Ctrl Pts',(7.86496589709659,2.05086746709314,1.66448795671213));
#19020=CARTESIAN_POINT('Ctrl Pts',(7.80677565064256,2.25254112127492,1.67270974488543));
#19021=CARTESIAN_POINT('Ctrl Pts',(7.74858556565089,2.45421421586626,1.68093151024546));
#19022=CARTESIAN_POINT('Ctrl Pts',(7.68257895666524,2.65362292948847,1.6891532756055));
#19023=CARTESIAN_POINT('Ctrl Pts',(7.60896023444299,2.85015994518997,1.69737504096554));
#19024=CARTESIAN_POINT('Ctrl Pts',(7.53532616393932,3.04673793559647,1.70559852042716));
#19025=CARTESIAN_POINT('Ctrl Pts',(7.45407691330428,3.24044275580677,1.71382199988878));
#19026=CARTESIAN_POINT('Ctrl Pts',(7.3654656046334,3.43068564422074,1.7220454793504));
#19027=CARTESIAN_POINT('Ctrl Pts',(7.32966335448509,3.50755081619593,1.72536806958398));
#19028=CARTESIAN_POINT('Ctrl Pts',(7.29265982215346,3.58385108037853,1.72869065981756));
#19029=CARTESIAN_POINT('Ctrl Pts',(7.25447388537293,3.65954863459173,1.73201325005114));
#19030=CARTESIAN_POINT('Ctrl Pts',(7.15996221793444,3.84690300305528,1.74023678912509));
#19031=CARTESIAN_POINT('Ctrl Pts',(7.0581733878635,4.03062455210347,1.74846032819905));
#19032=CARTESIAN_POINT('Ctrl Pts',(6.94941202981653,4.21014964132408,1.75668386727301));
#19033=CARTESIAN_POINT('Ctrl Pts',(6.84067044647371,4.389642089765,1.76490591116471));
#19034=CARTESIAN_POINT('Ctrl Pts',(6.72495901813897,4.56493934908913,1.77312795505642));
#19035=CARTESIAN_POINT('Ctrl Pts',(6.60262720753773,4.73550435759302,1.78134999894813));
#19036=CARTESIAN_POINT('Ctrl Pts',(6.48030890333319,4.90605053437477,1.78957113506134));
#19037=CARTESIAN_POINT('Ctrl Pts',(6.35137184798668,5.07186526387154,1.79779227117456));
#19038=CARTESIAN_POINT('Ctrl Pts',(6.21620799866067,5.23244165566011,1.80601340728777));
#19039=CARTESIAN_POINT('Ctrl Pts',(6.08103342880286,5.39303078357836,1.81423519546107));
#19040=CARTESIAN_POINT('Ctrl Pts',(5.93963126605871,5.5483805162706,1.82245698363437));
#19041=CARTESIAN_POINT('Ctrl Pts',(5.79243349414781,5.69801735504329,1.83067877180767));
#19042=CARTESIAN_POINT('Ctrl Pts',(5.64523613067152,5.84765377861362,1.8389005371677));
#19043=CARTESIAN_POINT('Ctrl Pts',(5.49224339894691,5.99157713160955,1.84712230252773));
#19044=CARTESIAN_POINT('Ctrl Pts',(5.33392422572816,6.12935069291114,1.85534406788776));
#19045=CARTESIAN_POINT('Ctrl Pts',(5.17557204558999,6.26715297771313,1.86356754734938));
#19046=CARTESIAN_POINT('Ctrl Pts',(5.01189142807282,6.39880271584666,1.87179102681099));
#19047=CARTESIAN_POINT('Ctrl Pts',(4.84338529968251,6.52390269710696,1.88001450627261));
#19048=CARTESIAN_POINT('Ctrl Pts',(4.77530258370977,6.57444772222682,1.88333709650622));
#19049=CARTESIAN_POINT('Ctrl Pts',(4.706432487394,6.62392399485261,1.88665968673983));
#19050=CARTESIAN_POINT('Ctrl Pts',(4.63680961071596,6.67230726184519,1.88998227697344));
#19051=CARTESIAN_POINT('Ctrl Pts',(4.46449030362483,6.79205771515557,1.8982058160474));
#19052=CARTESIAN_POINT('Ctrl Pts',(4.28750150809802,6.90514856257424,1.90642935512136));
#19053=CARTESIAN_POINT('Ctrl Pts',(4.10637948734327,7.01122921237257,1.91465289419532));
#19054=CARTESIAN_POINT('Ctrl Pts',(3.92529039771805,7.1172905748661,1.92287493808703));
#19055=CARTESIAN_POINT('Ctrl Pts',(3.74006983712862,7.21634413466484,1.93109698197874));
#19056=CARTESIAN_POINT('Ctrl Pts',(3.55128083338975,7.30808401736724,1.93931902587045));
#19057=CARTESIAN_POINT('Ctrl Pts',(3.36251267344561,7.39981377126318,1.94754016198368));
#19058=CARTESIAN_POINT('Ctrl Pts',(3.17017712209659,7.48423133132588,1.95576129809691));
#19059=CARTESIAN_POINT('Ctrl Pts',(2.97486020904337,7.56107758848899,1.96398243421014));
#19060=CARTESIAN_POINT('Ctrl Pts',(2.77952780441349,7.63792994071915,1.97220422238344));
#19061=CARTESIAN_POINT('Ctrl Pts',(2.58121383909049,7.70720967970647,1.98042601055674));
#19062=CARTESIAN_POINT('Ctrl Pts',(2.380523641074,7.7687061185752,1.98864779873004));
#19063=CARTESIAN_POINT('Ctrl Pts',(2.17983399991929,7.83020238680771,1.99686956409007));
#19064=CARTESIAN_POINT('Ctrl Pts',(1.97676842204044,7.88391531429189,2.00509132945011));
#19065=CARTESIAN_POINT('Ctrl Pts',(1.77194721002299,7.92968414549985,2.01331309481014));
#19066=CARTESIAN_POINT('Ctrl Pts',(1.56708329618284,7.97546251874937,2.02153657427177));
#19067=CARTESIAN_POINT('Ctrl Pts',(1.36046330488571,8.01329342275546,2.02976005373339));
#19068=CARTESIAN_POINT('Ctrl Pts',(1.1527186236022,8.0430670354847,2.03798353319502));
#19069=CARTESIAN_POINT('Ctrl Pts',(1.06878207918339,8.05509667760076,2.04130612342859));
#19070=CARTESIAN_POINT('Ctrl Pts',(0.98466203122376,8.06581158546664,2.04462871366216));
#19071=CARTESIAN_POINT('Ctrl Pts',(0.900400453850177,8.07520690664991,2.04795130389573));
#19072=CARTESIAN_POINT('Ctrl Pts',(0.691849797508385,8.09846068922064,2.05617484296969));
#19073=CARTESIAN_POINT('Ctrl Pts',(0.482363956383825,8.11363487388641,2.06439838204366));
#19074=CARTESIAN_POINT('Ctrl Pts',(0.272581435487024,8.12067650651889,2.07262192111762));
#19075=CARTESIAN_POINT('Ctrl Pts',(0.0628370566964013,8.12771685886025,
2.08084396500934));
#19076=CARTESIAN_POINT('Ctrl Pts',(-0.147203599582602,8.1266276004737,2.08906600890105));
#19077=CARTESIAN_POINT('Ctrl Pts',(-0.356899784817117,8.11740784401631,
2.09728805279277));
#19078=CARTESIAN_POINT('Ctrl Pts',(-0.566572817939022,8.10818910549274,
2.105509188906));
#19079=CARTESIAN_POINT('Ctrl Pts',(-0.775901161411214,8.09084167401546,
2.11373032501923));
#19080=CARTESIAN_POINT('Ctrl Pts',(-0.984246107139381,8.06541673833913,
2.12195146113246));
#19081=CARTESIAN_POINT('Ctrl Pts',(-1.19260757776358,8.03998978608198,2.13017324930576));
#19082=CARTESIAN_POINT('Ctrl Pts',(-1.39998520170378,8.00648408260978,2.13839503747905));
#19083=CARTESIAN_POINT('Ctrl Pts',(-1.60574635701631,7.96500258627886,2.14661682565235));
#19084=CARTESIAN_POINT('Ctrl Pts',(-1.8115069413964,7.92352120504804,2.15483859101237));
#19085=CARTESIAN_POINT('Ctrl Pts',(-2.01565077753847,7.87406413615681,2.1630603563724));
#19086=CARTESIAN_POINT('Ctrl Pts',(-2.21755585035044,7.81678537591231,2.17128212173242));
#19087=CARTESIAN_POINT('Ctrl Pts',(-2.41950301701857,7.75949467399709,2.17950560119405));
#19088=CARTESIAN_POINT('Ctrl Pts',(-2.61921020414699,7.69437910358001,2.18772908065567));
#19089=CARTESIAN_POINT('Ctrl Pts',(-2.81606990112761,7.62164272807793,2.1959525601173));
#19090=CARTESIAN_POINT('Ctrl Pts',(-2.8956085087966,7.59225453880882,2.19927515035087));
#19091=CARTESIAN_POINT('Ctrl Pts',(-2.97468246844109,7.56162284565495,2.20259774058444));
#19092=CARTESIAN_POINT('Ctrl Pts',(-3.05325255908329,7.52976336765979,2.20592033081802));
#19093=CARTESIAN_POINT('Ctrl Pts',(-3.24771656608354,7.4509099299046,2.21414386989198));
#19094=CARTESIAN_POINT('Ctrl Pts',(-3.43915581777879,7.36450630485182,2.22236740896594));
#19095=CARTESIAN_POINT('Ctrl Pts',(-3.62698362246535,7.27080995246527,2.2305909480399));
#19096=CARTESIAN_POINT('Ctrl Pts',(-3.8147772767944,7.17713063570312,2.23881299193161));
#19097=CARTESIAN_POINT('Ctrl Pts',(-3.99896053087167,7.07616136962983,2.24703503582332));
#19098=CARTESIAN_POINT('Ctrl Pts',(-4.17896951186102,6.96820646805446,2.25525707971503));
#19099=CARTESIAN_POINT('Ctrl Pts',(-4.35895861843857,6.86026348555201,2.26347821582822));
#19100=CARTESIAN_POINT('Ctrl Pts',(-4.53477411920625,6.74533655898958,2.27169935194142));
#19101=CARTESIAN_POINT('Ctrl Pts',(-4.70587873178468,6.62377482439104,2.27992048805461));
#19102=CARTESIAN_POINT('Ctrl Pts',(-4.87699691553992,6.50220344811325,2.28814227622791));
#19103=CARTESIAN_POINT('Ctrl Pts',(-5.04340322255487,6.37399638098395,2.29636406440121));
#19104=CARTESIAN_POINT('Ctrl Pts',(-5.2045903726162,6.23954538534425,2.30458585257451));
#19105=CARTESIAN_POINT('Ctrl Pts',(-5.3657770754266,6.10509476276985,2.31280761793456));
#19106=CARTESIAN_POINT('Ctrl Pts',(-5.52174442549491,5.96440043732968,2.32102938329461));
#19107=CARTESIAN_POINT('Ctrl Pts',(-5.67201877173187,5.81789400175194,2.32925114865466));
#19108=CARTESIAN_POINT('Ctrl Pts',(-5.82232444767511,5.67135702201474,2.33747462811628));
#19109=CARTESIAN_POINT('Ctrl Pts',(-5.96693453749004,5.51900571737564,2.34569810757791));
#19110=CARTESIAN_POINT('Ctrl Pts',(-6.10541198437529,5.36130880136059,2.35392158703954));
#19111=CARTESIAN_POINT('Ctrl Pts',(-6.16136200100031,5.29759340747361,2.35724417727313));
#19112=CARTESIAN_POINT('Ctrl Pts',(-6.21631132585167,5.23300576610325,2.36056676750671));
#19113=CARTESIAN_POINT('Ctrl Pts',(-6.2702329541306,5.1675783751613,2.36388935774031));
#19114=CARTESIAN_POINT('Ctrl Pts',(-6.40369106539566,5.00564305720415,2.37211289681426));
#19115=CARTESIAN_POINT('Ctrl Pts',(-6.53089427821922,4.83850863178803,2.38033643588821));
#19116=CARTESIAN_POINT('Ctrl Pts',(-6.65144926807356,4.66668085439145,2.38855997496216));
#19117=CARTESIAN_POINT('Ctrl Pts',(-6.77198233893676,4.49488431826937,2.39678201885387));
#19118=CARTESIAN_POINT('Ctrl Pts',(-6.88586943007247,4.31839637464006,2.40500406274559));
#19119=CARTESIAN_POINT('Ctrl Pts',(-6.9927595925948,4.1377531152394,2.4132261066373));
#19120=CARTESIAN_POINT('Ctrl Pts',(-7.09963795360082,3.95712980027819,2.42144724275056));
#19121=CARTESIAN_POINT('Ctrl Pts',(-7.19952077815735,3.77235233921032,2.42966837886383));
#19122=CARTESIAN_POINT('Ctrl Pts',(-7.29210184224885,3.58398357763689,2.4378895149771));
#19123=CARTESIAN_POINT('Ctrl Pts',(-7.38469024941451,3.39559987558077,2.44611130315041));
#19124=CARTESIAN_POINT('Ctrl Pts',(-7.4699756064655,3.20362456740546,2.4543330913237));
#19125=CARTESIAN_POINT('Ctrl Pts',(-7.5476983688039,3.0086436970926,2.46255487949701));
#19126=CARTESIAN_POINT('Ctrl Pts',(-7.62542091548221,2.81366336780001,2.47077664485702));
#19127=CARTESIAN_POINT('Ctrl Pts',(-7.6955808027202,2.61567776801857,2.47899841021705));
#19128=CARTESIAN_POINT('Ctrl Pts',(-7.75796702345944,2.4152919544883,2.48722017557707));
#19129=CARTESIAN_POINT('Ctrl Pts',(-7.82036625069022,2.2148643638419,2.4954436550387));
#19130=CARTESIAN_POINT('Ctrl Pts',(-7.87498848608079,2.01203584143313,2.50366713450033));
#19131=CARTESIAN_POINT('Ctrl Pts',(-7.92167257738839,1.80742666217823,2.51189061396197));
#19132=CARTESIAN_POINT('Ctrl Pts',(-7.94053467907712,1.7247569766932,2.51521320419551));
#19133=CARTESIAN_POINT('Ctrl Pts',(-7.95810148685798,1.64179675138254,2.51853579442906));
#19134=CARTESIAN_POINT('Ctrl Pts',(-7.97436472768614,1.55858742210219,2.5218583846626));
#19135=CARTESIAN_POINT('Ctrl Pts',(-8.01566387109975,1.34728427166554,2.53029582539226));
#19136=CARTESIAN_POINT('Ctrl Pts',(-8.04856370238538,1.13432059785419,2.53873326612193));
#19137=CARTESIAN_POINT('Ctrl Pts',(-8.07295618582614,0.920361876780752,
2.54717070685159));
#19138=CARTESIAN_POINT('Ctrl Pts',(-8.09734200868676,0.706461579000405,
2.55560584366454));
#19139=CARTESIAN_POINT('Ctrl Pts',(-8.11322509376166,0.491567035436145,
2.5640409804775));
#19140=CARTESIAN_POINT('Ctrl Pts',(-8.12054913382223,0.276350009370382,
2.57247611729046));
#19141=CARTESIAN_POINT('Ctrl Pts',(-8.12368110532627,0.184316980161344,
2.57608322592345));
#19142=CARTESIAN_POINT('Ctrl Pts',(-8.12524856030468,0.092225042011402,
2.57969033455644));
#19143=CARTESIAN_POINT('Ctrl Pts',(-8.1252499990086,0.000126927995783942,
2.58329744318944));
#19144=CARTESIAN_POINT('Ctrl Pts',(-8.12524999900861,0.000126927409469058,
2.5832974432124));
#19145=CARTESIAN_POINT('Ctrl Pts',(-8.12525328844262,-0.210445980594937,
2.59154472777903));
#19146=CARTESIAN_POINT('Ctrl Pts',(-8.11706646380963,-0.421019864585635,
2.59979201234565));
#19147=CARTESIAN_POINT('Ctrl Pts',(-8.1007153570126,-0.630950288976996,
2.60803929691228));
#19148=CARTESIAN_POINT('Ctrl Pts',(-8.08436443564097,-0.840878332708048,
2.61628648795277));
#19149=CARTESIAN_POINT('Ctrl Pts',(-8.05984944240335,-1.05016264135977,
2.62453367899326));
#19150=CARTESIAN_POINT('Ctrl Pts',(-8.02724816546579,-1.2581631263577,2.63278087003375));
#19151=CARTESIAN_POINT('Ctrl Pts',(-7.99463828803845,-1.46621848362481,
2.64103023675228));
#19152=CARTESIAN_POINT('Ctrl Pts',(-7.95393790784404,-1.67298905246805,
2.6492796034708));
#19153=CARTESIAN_POINT('Ctrl Pts',(-7.90527631458381,-1.87784289880177,
2.65752897018933));
#19154=CARTESIAN_POINT('Ctrl Pts',(-7.86143142634161,-2.06241955149075,
2.66496178398785));
#19155=CARTESIAN_POINT('Ctrl Pts',(-7.81112407879475,-2.24544011732185,
2.67239459778637));
#19156=CARTESIAN_POINT('Ctrl Pts',(-7.75448398467238,-2.42645125522018,
2.67982741158489));
#19157=CARTESIAN_POINT('Ctrl Pts',(-7.69181834554913,-2.62671890697087,
2.68805095065885));
#19158=CARTESIAN_POINT('Ctrl Pts',(-7.62138020049275,-2.82459018137162,
2.69627448973282));
#19159=CARTESIAN_POINT('Ctrl Pts',(-7.54337810570844,-3.0194592755688,2.70449802880679));
#19160=CARTESIAN_POINT('Ctrl Pts',(-7.46539019305993,-3.21429293917961,
2.7127200726985));
#19161=CARTESIAN_POINT('Ctrl Pts',(-7.37984118508777,-3.40612523836004,
2.72094211659021));
#19162=CARTESIAN_POINT('Ctrl Pts',(-7.28698820295463,-3.59436927603441,
2.72916416048192));
#19163=CARTESIAN_POINT('Ctrl Pts',(-7.19414547252293,-3.78259253008256,
2.73738529659515));
#19164=CARTESIAN_POINT('Ctrl Pts',(-7.09400050833028,-3.96722804916409,
2.74560643270837));
#19165=CARTESIAN_POINT('Ctrl Pts',(-6.98685728051198,-4.14771176725876,
2.7538275688216));
#19166=CARTESIAN_POINT('Ctrl Pts',(-6.87970555461987,-4.32820980043416,
2.7620493569949));
#19167=CARTESIAN_POINT('Ctrl Pts',(-6.7655546043071,-4.50455511967747,2.77027114516821));
#19168=CARTESIAN_POINT('Ctrl Pts',(-6.64475333951376,-4.67621007008033,
2.77849293334152));
#19169=CARTESIAN_POINT('Ctrl Pts',(-6.52395240991147,-4.84786454418683,
2.78671469870157));
#19170=CARTESIAN_POINT('Ctrl Pts',(-6.3965013746841,-5.01482843584574,2.79493646406162));
#19171=CARTESIAN_POINT('Ctrl Pts',(-6.26279159401588,-5.1765943449747,2.80315822942167));
#19172=CARTESIAN_POINT('Ctrl Pts',(-6.12905393707836,-5.33839397960992,
2.8113817088833));
#19173=CARTESIAN_POINT('Ctrl Pts',(-5.98905511593022,-5.49499323943775,
2.81960518834492));
#19174=CARTESIAN_POINT('Ctrl Pts',(-5.84322648330132,-5.64591815627415,
2.82782866780654));
#19175=CARTESIAN_POINT('Ctrl Pts',(-5.78430631540832,-5.70689741171206,
2.83115125804009));
#19176=CARTESIAN_POINT('Ctrl Pts',(-5.72443489078691,-5.76695075660639,
2.83447384827363));
#19177=CARTESIAN_POINT('Ctrl Pts',(-5.66364238702835,-5.82604861585928,
2.83779643850717));
#19178=CARTESIAN_POINT('Ctrl Pts',(-5.51317859374565,-5.97231809858025,
2.84601997758114));
#19179=CARTESIAN_POINT('Ctrl Pts',(-5.35702099047824,-6.11277939735596,
2.85424351665511));
#19180=CARTESIAN_POINT('Ctrl Pts',(-5.19564142839055,-6.24699909637354,
2.86246705572907));
#19181=CARTESIAN_POINT('Ctrl Pts',(-5.03429120791019,-6.38119439191862,
2.8706890996208));
#19182=CARTESIAN_POINT('Ctrl Pts',(-4.86772115023346,-6.50915016419816,
2.87891114351254));
#19183=CARTESIAN_POINT('Ctrl Pts',(-4.69643681069821,-6.63047274676692,
2.88713318740427));
#19184=CARTESIAN_POINT('Ctrl Pts',(-4.52517138230544,-6.75178193436535,
2.89535432351748));
#19185=CARTESIAN_POINT('Ctrl Pts',(-4.34919295178381,-6.86645922396823,
2.90357545963069));
#19186=CARTESIAN_POINT('Ctrl Pts',(-4.16903740064043,-6.97415333316965,
2.91179659574391));
#19187=CARTESIAN_POINT('Ctrl Pts',(-3.98886756044491,-7.08185598413805,
2.9200183839172));
#19188=CARTESIAN_POINT('Ctrl Pts',(-3.80452018944167,-7.18257419440997,
2.92824017209049));
#19189=CARTESIAN_POINT('Ctrl Pts',(-3.61655811180281,-7.27600130473142,
2.93646196026378));
#19190=CARTESIAN_POINT('Ctrl Pts',(-3.42859655570825,-7.36942815581772,
2.94468372562382));
#19191=CARTESIAN_POINT('Ctrl Pts',(-3.23702057834738,-7.45556381856249,
2.95290549098386));
#19192=CARTESIAN_POINT('Ctrl Pts',(-3.0424159271361,-7.53414845147138,2.9611272563439));
#19193=CARTESIAN_POINT('Ctrl Pts',(-2.84777070408543,-7.61274946797175,
2.96935073580553));
#19194=CARTESIAN_POINT('Ctrl Pts',(-2.65009581929774,-7.68379619925315,
2.97757421526716));
#19195=CARTESIAN_POINT('Ctrl Pts',(-2.44999626945303,-7.74707724514002,
2.9857976947288));
#19196=CARTESIAN_POINT('Ctrl Pts',(-2.36914864124961,-7.77264513109556,
2.98912028496235));
#19197=CARTESIAN_POINT('Ctrl Pts',(-2.28790538816167,-7.79694586250298,
2.99244287519591));
#19198=CARTESIAN_POINT('Ctrl Pts',(-2.20630712949662,-7.8199678012657,2.99576546542946));
#19199=CARTESIAN_POINT('Ctrl Pts',(-2.00434828975688,-7.87694798830823,
3.00398900450342));
#19200=CARTESIAN_POINT('Ctrl Pts',(-1.80014810831906,-7.92610955269224,
3.01221254357739));
#19201=CARTESIAN_POINT('Ctrl Pts',(-1.59432788555514,-7.96729603791909,
3.02043608265135));
#19202=CARTESIAN_POINT('Ctrl Pts',(-1.388545084483,-8.00847503472748,3.02865812654305));
#19203=CARTESIAN_POINT('Ctrl Pts',(-1.18114311903416,-8.04168178858559,
3.03688017043476));
#19204=CARTESIAN_POINT('Ctrl Pts',(-0.972754001005447,-8.06681084543501,
3.04510221432647));
#19205=CARTESIAN_POINT('Ctrl Pts',(-0.764387890778811,-8.09193712783837,
3.05332335043969));
#19206=CARTESIAN_POINT('Ctrl Pts',(-0.555035138265151,-8.10898745846579,
3.06154448655291));
#19207=CARTESIAN_POINT('Ctrl Pts',(-0.345334241689457,-8.11790809408537,
3.06976562266613));
#19208=CARTESIAN_POINT('Ctrl Pts',(-0.135616712669919,-8.1268294372459,
3.07798741083943));
#19209=CARTESIAN_POINT('Ctrl Pts',(0.0744487210210313,-8.12761978183108,
3.08620919901274));
#19210=CARTESIAN_POINT('Ctrl Pts',(0.284221116216748,-8.12027745336306,
3.09443098718604));
#19211=CARTESIAN_POINT('Ctrl Pts',(0.493992929349538,-8.11293514526807,
3.10265275254606));
#19212=CARTESIAN_POINT('Ctrl Pts',(0.703471410956348,-8.09746022227151,
3.11087451790608));
#19213=CARTESIAN_POINT('Ctrl Pts',(0.91201775242604,-8.07390309464758,3.1190962832661));
#19214=CARTESIAN_POINT('Ctrl Pts',(1.12060757234675,-8.05034105575351,3.12731976272774));
#19215=CARTESIAN_POINT('Ctrl Pts',(1.32826457078167,-8.01869347918493,3.13554324218938));
#19216=CARTESIAN_POINT('Ctrl Pts',(1.53435607749764,-7.9790625382902,3.14376672165102));
#19217=CARTESIAN_POINT('Ctrl Pts',(1.61762467817113,-7.96305017055966,3.1470893118846));
#19218=CARTESIAN_POINT('Ctrl Pts',(1.700637817607,-7.9457351366193,3.15041190211817));
#19219=CARTESIAN_POINT('Ctrl Pts',(1.78335423519316,-7.92712654335218,3.15373449235175));
#19220=CARTESIAN_POINT('Ctrl Pts',(1.98807904402292,-7.88106989812531,3.16195797047423));
#19221=CARTESIAN_POINT('Ctrl Pts',(2.1910519731871,-7.82707074522186,3.1701814485967));
#19222=CARTESIAN_POINT('Ctrl Pts',(2.39165219092882,-7.76528733274728,3.17840492671917));
#19223=CARTESIAN_POINT('Ctrl Pts',(2.59221537026594,-7.70351532783274,3.18662688647585));
#19224=CARTESIAN_POINT('Ctrl Pts',(2.79040643087923,-7.63396201884482,3.19484884623252));
#19225=CARTESIAN_POINT('Ctrl Pts',(2.98561941136611,-7.55683560049932,3.2030708059892));
#19226=CARTESIAN_POINT('Ctrl Pts',(3.18082858102689,-7.47971068776767,3.2112926052419));
#19227=CARTESIAN_POINT('Ctrl Pts',(3.3730595111537,-7.39501306610892,3.2195144044946));
#19228=CARTESIAN_POINT('Ctrl Pts',(3.56172499869025,-7.30299956156407,3.22773620374729));
#19229=CARTESIAN_POINT('Ctrl Pts',(3.75037759399235,-7.21099234465395,3.235957441173));
#19230=CARTESIAN_POINT('Ctrl Pts',(3.93546496886292,-7.11167037386672,3.24417867859872));
#19231=CARTESIAN_POINT('Ctrl Pts',(4.11642281865087,-7.0053373038413,3.25239991602442));
#19232=CARTESIAN_POINT('Ctrl Pts',(4.29740606490845,-6.89898931053629,3.26062230725698));
#19233=CARTESIAN_POINT('Ctrl Pts',(4.47425837329976,-6.7856284006226,3.26884469848954));
#19234=CARTESIAN_POINT('Ctrl Pts',(4.64644188055243,-6.6656031544901,3.27706708972209));
#19235=CARTESIAN_POINT('Ctrl Pts',(4.74821045284433,-6.59466257410128,3.28192691067657));
#19236=CARTESIAN_POINT('Ctrl Pts',(4.84834856604575,-6.52139473475173,3.28678673163106));
#19237=CARTESIAN_POINT('Ctrl Pts',(4.94675008185374,-6.44587862049698,3.29164655258555));
#19238=CARTESIAN_POINT('',(-8.12524999744415,0.000203798425227694,2.41670255624515));
#19239=CARTESIAN_POINT('Ctrl Pts',(-8.125117379974,0.000203781251170848,
2.41670255678762));
#19240=CARTESIAN_POINT('Ctrl Pts',(-8.12415321314374,-0.990648431134313,
2.45551853014197));
#19241=CARTESIAN_POINT('Ctrl Pts',(-7.69622348325201,-3.32646489320684,
2.54699084580375));
#19242=CARTESIAN_POINT('Ctrl Pts',(-5.51026191012776,-6.42780902731277,
2.69111950377297));
#19243=CARTESIAN_POINT('Ctrl Pts',(-1.78490025904692,-8.27610091015463,
2.84908853069526));
#19244=CARTESIAN_POINT('Ctrl Pts',(2.02051483585045,-8.14010815660882,2.99373142002673));
#19245=CARTESIAN_POINT('Ctrl Pts',(4.14961438984119,-7.05622354844238,3.08571796705077));
#19246=CARTESIAN_POINT('Ctrl Pts',(4.94669362673306,-6.44580471440964,3.12504817176739));
#19247=CARTESIAN_POINT('Ctrl Pts',(4.94675008185375,-6.44587862049697,1.12505977544705));
#19248=CARTESIAN_POINT('Ctrl Pts',(5.11323077301675,-6.31811661610258,1.13328241581699));
#19249=CARTESIAN_POINT('Ctrl Pts',(5.27478151473168,-6.18388435476994,1.14150505618694));
#19250=CARTESIAN_POINT('Ctrl Pts',(5.43090611222471,-6.04358720982003,1.14972769655688));
#19251=CARTESIAN_POINT('Ctrl Pts',(5.58700848365971,-5.90331003771576,1.1579491663433));
#19252=CARTESIAN_POINT('Ctrl Pts',(5.73768603355537,-5.75696990251955,1.16617063612971));
#19253=CARTESIAN_POINT('Ctrl Pts',(5.88247713338117,-5.60501118087624,1.17439210591613));
#19254=CARTESIAN_POINT('Ctrl Pts',(6.02727738266826,-5.45304285684409,1.18261409522356));
#19255=CARTESIAN_POINT('Ctrl Pts',(6.16619023247752,-5.29545544791427,1.190836084531));
#19256=CARTESIAN_POINT('Ctrl Pts',(6.2987915383268,-5.13272955835418,1.19905807383843));
#19257=CARTESIAN_POINT('Ctrl Pts',(6.43138822169437,-4.97000934141884,1.20727977652731));
#19258=CARTESIAN_POINT('Ctrl Pts',(6.55767361594782,-4.8021512317033,1.21550147921619));
#19259=CARTESIAN_POINT('Ctrl Pts',(6.67726411910909,-4.6296686108358,1.22372318190506));
#19260=CARTESIAN_POINT('Ctrl Pts',(6.79688321455685,-4.45714475197381,1.23194685027911));
#19261=CARTESIAN_POINT('Ctrl Pts',(6.90980405111591,-4.27999441430689,1.24017051865315));
#19262=CARTESIAN_POINT('Ctrl Pts',(7.01568590929727,-4.09876064007009,1.24839418702719));
#19263=CARTESIAN_POINT('Ctrl Pts',(7.10583020705181,-3.94446422339785,1.25539554517558));
#19264=CARTESIAN_POINT('Ctrl Pts',(7.19087314623396,-3.78720860347607,1.26239690332397));
#19265=CARTESIAN_POINT('Ctrl Pts',(7.2706303882144,-3.6273435625087,1.26939826147236));
#19266=CARTESIAN_POINT('Ctrl Pts',(7.36431032601451,-3.43957193547693,1.27762180054632));
#19267=CARTESIAN_POINT('Ctrl Pts',(7.45072749512893,-3.24813879729511,1.28584533962027));
#19268=CARTESIAN_POINT('Ctrl Pts',(7.52961220588782,-3.05362531942691,1.29406887869423));
#19269=CARTESIAN_POINT('Ctrl Pts',(7.60848257403608,-2.85914720748768,1.30229092258595));
#19270=CARTESIAN_POINT('Ctrl Pts',(7.67982310647036,-2.66159014685487,1.31051296647766));
#19271=CARTESIAN_POINT('Ctrl Pts',(7.74341221979638,-2.4615553531879,1.31873501036937));
#19272=CARTESIAN_POINT('Ctrl Pts',(7.80699431238271,-2.26154264494003,1.32695614648258));
#19273=CARTESIAN_POINT('Ctrl Pts',(7.86282660515338,-2.05905303077812,1.33517728259579));
#19274=CARTESIAN_POINT('Ctrl Pts',(7.91073710563994,-1.85470375207241,1.343398418709));
#19275=CARTESIAN_POINT('Ctrl Pts',(7.95865140615179,-1.65033826538681,1.3516202068823));
#19276=CARTESIAN_POINT('Ctrl Pts',(7.99864258903827,-1.44411310599154,1.3598419950556));
#19277=CARTESIAN_POINT('Ctrl Pts',(8.03058935885154,-1.23665763734365,1.3680637832289));
#19278=CARTESIAN_POINT('Ctrl Pts',(8.06253604002105,-1.02920274432932,1.37628554858893));
#19279=CARTESIAN_POINT('Ctrl Pts',(8.08643831054409,-0.820517840797621,
1.38450731394896));
#19280=CARTESIAN_POINT('Ctrl Pts',(8.10222644260455,-0.611239916284599,
1.392729079309));
#19281=CARTESIAN_POINT('Ctrl Pts',(8.11801786622845,-0.401918360798402,
1.40095255877062));
#19282=CARTESIAN_POINT('Ctrl Pts',(8.12569174974096,-0.19200383149342,1.40917603823225));
#19283=CARTESIAN_POINT('Ctrl Pts',(8.12523036436275,0.0178630495050401,
1.41739951769387));
#19284=CARTESIAN_POINT('Ctrl Pts',(8.12504394758397,0.102657041198461,1.42072210792747));
#19285=CARTESIAN_POINT('Ctrl Pts',(8.12353007496566,0.187443242370045,1.42404469816106));
#19286=CARTESIAN_POINT('Ctrl Pts',(8.12068999082584,0.272179417666121,1.42736728839465));
#19287=CARTESIAN_POINT('Ctrl Pts',(8.1136606729578,0.481904722183047,1.43559082746861));
#19288=CARTESIAN_POINT('Ctrl Pts',(8.09850130939948,0.691391636352905,1.44381436654256));
#19289=CARTESIAN_POINT('Ctrl Pts',(8.07525147145568,0.900000686251279,1.45203790561652));
#19290=CARTESIAN_POINT('Ctrl Pts',(8.05200586073628,1.10857180740081,1.46025994950824));
#19291=CARTESIAN_POINT('Ctrl Pts',(8.0206727442093,1.31626508986942,1.46848199339995));
#19292=CARTESIAN_POINT('Ctrl Pts',(7.98134354013807,1.52244633954577,1.47670403729166));
#19293=CARTESIAN_POINT('Ctrl Pts',(7.94201867832116,1.72860482518594,1.48492517340488));
#19294=CARTESIAN_POINT('Ctrl Pts',(7.89469954674085,1.93325132172575,1.4931463095181));
#19295=CARTESIAN_POINT('Ctrl Pts',(7.83952880275268,2.13576115549259,1.50136744563132));
#19296=CARTESIAN_POINT('Ctrl Pts',(7.78435368289246,2.33828705134343,1.50958923380462));
#19297=CARTESIAN_POINT('Ctrl Pts',(7.72132578128062,2.53867566053733,1.51781102197792));
#19298=CARTESIAN_POINT('Ctrl Pts',(7.65063810830258,2.73631578921154,1.52603281015121));
#19299=CARTESIAN_POINT('Ctrl Pts',(7.57995063146392,2.93395536948725,1.53425457551125));
#19300=CARTESIAN_POINT('Ctrl Pts',(7.50160352763663,3.12884620770216,1.54247634087128));
#19301=CARTESIAN_POINT('Ctrl Pts',(7.41583878503286,3.32039495796847,1.55069810623131));
#19302=CARTESIAN_POINT('Ctrl Pts',(7.33005616190401,3.51198364296934,1.55892158569294));
#19303=CARTESIAN_POINT('Ctrl Pts',(7.23685293117237,3.7002285788446,1.56714506515456));
#19304=CARTESIAN_POINT('Ctrl Pts',(7.13651853672765,3.88455798482178,1.57536854461619));
#19305=CARTESIAN_POINT('Ctrl Pts',(7.09597972579851,3.95903389090508,1.57869113484977));
#19306=CARTESIAN_POINT('Ctrl Pts',(7.05427730926703,4.03287087469238,1.58201372508336));
#19307=CARTESIAN_POINT('Ctrl Pts',(7.01143249181514,4.10603238847661,1.58533631531694));
#19308=CARTESIAN_POINT('Ctrl Pts',(6.90538991489095,4.2871099589918,1.5935598543909));
#19309=CARTESIAN_POINT('Ctrl Pts',(6.79231158966716,4.46410675522406,1.60178339346486));
#19310=CARTESIAN_POINT('Ctrl Pts',(6.67253680086821,4.63647928967222,1.61000693253882));
#19311=CARTESIAN_POINT('Ctrl Pts',(6.55278378920634,4.80882048379953,1.61822897643053));
#19312=CARTESIAN_POINT('Ctrl Pts',(6.42633691224082,4.97653885214234,1.62645102032225));
#19313=CARTESIAN_POINT('Ctrl Pts',(6.29357853297781,5.13912023713601,1.63467306421396));
#19314=CARTESIAN_POINT('Ctrl Pts',(6.16083481128717,5.30168367186222,1.64289420032717));
#19315=CARTESIAN_POINT('Ctrl Pts',(6.02178116498362,5.45911102720148,1.65111533644038));
#19316=CARTESIAN_POINT('Ctrl Pts',(5.87684048163505,5.61092091513644,1.65933647255359));
#19317=CARTESIAN_POINT('Ctrl Pts',(5.73188830230415,5.76274284388524,1.66755826072689));
#19318=CARTESIAN_POINT('Ctrl Pts',(5.58104835471498,5.90894619982334,1.67578004890019));
#19319=CARTESIAN_POINT('Ctrl Pts',(5.42478138656193,6.04908542430268,1.68400183707348));
#19320=CARTESIAN_POINT('Ctrl Pts',(5.26851485200798,6.18922425993312,1.69222360243352));
#19321=CARTESIAN_POINT('Ctrl Pts',(5.10682154838389,6.32329880286109,1.70044536779355));
#19322=CARTESIAN_POINT('Ctrl Pts',(4.94019679429501,6.45090251020253,1.70866713315358));
#19323=CARTESIAN_POINT('Ctrl Pts',(4.77353730171102,6.57853282079862,1.7168906126152));
#19324=CARTESIAN_POINT('Ctrl Pts',(4.6019445389611,6.69968942141668,1.72511409207682));
#19325=CARTESIAN_POINT('Ctrl Pts',(4.42594528711422,6.81400732887567,1.73333757153845));
#19326=CARTESIAN_POINT('Ctrl Pts',(4.35483507178077,6.86019599689882,1.73666016177204));
#19327=CARTESIAN_POINT('Ctrl Pts',(4.28300584968343,6.90526876664184,1.73998275200564));
#19328=CARTESIAN_POINT('Ctrl Pts',(4.2104936697146,6.94920359608159,1.74330534223923));
#19329=CARTESIAN_POINT('Ctrl Pts',(4.03102322545611,7.05794399474789,1.75152888131319));
#19330=CARTESIAN_POINT('Ctrl Pts',(3.84730887840118,7.15974582281657,1.75975242038716));
#19331=CARTESIAN_POINT('Ctrl Pts',(3.6599077658713,7.25429270899755,1.76797595946112));
#19332=CARTESIAN_POINT('Ctrl Pts',(3.47254072611889,7.3488224049123,1.77619800335284));
#19333=CARTESIAN_POINT('Ctrl Pts',(3.28148852195944,7.43609965887759,1.78442004724455));
#19334=CARTESIAN_POINT('Ctrl Pts',(3.08733220661952,7.5158544030915,1.79264209113626));
#19335=CARTESIAN_POINT('Ctrl Pts',(2.8931973276681,7.59560034175262,1.80086322724948));
#19336=CARTESIAN_POINT('Ctrl Pts',(2.69595929446911,7.6678253167916,1.80908436336271));
#19337=CARTESIAN_POINT('Ctrl Pts',(2.4962191927285,7.73230737259932,1.81730549947593));
#19338=CARTESIAN_POINT('Ctrl Pts',(2.29646324858557,7.79679454280652,1.82552728764923));
#19339=CARTESIAN_POINT('Ctrl Pts',(2.0942051192416,7.85353747356029,1.83374907582253));
#19340=CARTESIAN_POINT('Ctrl Pts',(1.89006212293483,7.90236374345974,1.84197086399583));
#19341=CARTESIAN_POINT('Ctrl Pts',(1.68591969307024,7.95118987787937,1.85019262935586));
#19342=CARTESIAN_POINT('Ctrl Pts',(1.47989269417367,7.99209932940237,1.8584143947159));
#19343=CARTESIAN_POINT('Ctrl Pts',(1.27261026739207,8.02497044666385,1.86663616007593));
#19344=CARTESIAN_POINT('Ctrl Pts',(1.06528462566549,8.05784841700761,1.87485963953756));
#19345=CARTESIAN_POINT('Ctrl Pts',(0.856703324525786,8.0826846590018,1.88308311899918));
#19346=CARTESIAN_POINT('Ctrl Pts',(0.647503383272865,8.09940904826705,1.89130659846081));
#19347=CARTESIAN_POINT('Ctrl Pts',(0.562978859935354,8.10616632086613,1.89462918869438));
#19348=CARTESIAN_POINT('Ctrl Pts',(0.478353406818998,8.11159995723201,1.89795177892795));
#19349=CARTESIAN_POINT('Ctrl Pts',(0.393669219340714,8.11570773920819,1.90127436916152));
#19350=CARTESIAN_POINT('Ctrl Pts',(0.184072586677869,8.12587465815208,1.90949790823548));
#19351=CARTESIAN_POINT('Ctrl Pts',(-0.0259521568726862,8.12791931177454,
1.91772144730944));
#19352=CARTESIAN_POINT('Ctrl Pts',(-0.235764444536679,8.12182877738704,
1.9259449863834));
#19353=CARTESIAN_POINT('Ctrl Pts',(-0.445538584682319,8.11573935036449,
1.93416703027511));
#19354=CARTESIAN_POINT('Ctrl Pts',(-0.655100051374277,8.10151769603698,
1.94238907416682));
#19355=CARTESIAN_POINT('Ctrl Pts',(-0.86380929461282,8.07920299689521,1.95061111805854));
#19356=CARTESIAN_POINT('Ctrl Pts',(-1.07249549470422,8.05689076147227,1.95883225417173));
#19357=CARTESIAN_POINT('Ctrl Pts',(-1.28032936604469,8.02648729648953,1.96705339028493));
#19358=CARTESIAN_POINT('Ctrl Pts',(-1.486676651568,7.98808363102081,1.97527452639813));
#19359=CARTESIAN_POINT('Ctrl Pts',(-1.69304030354357,7.94967691956213,1.98349631457143));
#19360=CARTESIAN_POINT('Ctrl Pts',(-1.89791684366065,7.90326879111565,1.99171810274472));
#19361=CARTESIAN_POINT('Ctrl Pts',(-2.10068132641448,7.8490015624507,1.99993989091802));
#19362=CARTESIAN_POINT('Ctrl Pts',(-2.30344524655115,7.79473448436278,2.00816165627806));
#19363=CARTESIAN_POINT('Ctrl Pts',(-2.50409683683983,7.73260842853375,2.01638342163809));
#19364=CARTESIAN_POINT('Ctrl Pts',(-2.70202492943812,7.66281598651533,2.02460518699813));
#19365=CARTESIAN_POINT('Ctrl Pts',(-2.89999428675781,7.59300899393141,2.03282866645975));
#19366=CARTESIAN_POINT('Ctrl Pts',(-3.0952387338803,7.51553252028115,2.04105214592138));
#19367=CARTESIAN_POINT('Ctrl Pts',(-3.28716470991994,7.43062821922594,2.049275625383));
#19368=CARTESIAN_POINT('Ctrl Pts',(-3.36470991162445,7.39632373743164,2.0525982156166));
#19369=CARTESIAN_POINT('Ctrl Pts',(-3.44171361431989,7.36080724139594,2.0559208058502));
#19370=CARTESIAN_POINT('Ctrl Pts',(-3.51813765675171,7.32409687201402,2.05924339608381));
#19371=CARTESIAN_POINT('Ctrl Pts',(-3.70729011159588,7.23323729084203,2.06746693515776));
#19372=CARTESIAN_POINT('Ctrl Pts',(-3.89295159308986,7.13503144681388,2.07569047423172));
#19373=CARTESIAN_POINT('Ctrl Pts',(-4.07455265756765,7.02977298376046,2.08391401330567));
#19374=CARTESIAN_POINT('Ctrl Pts',(-4.25612070381756,6.92453365852393,2.09213605719738));
#19375=CARTESIAN_POINT('Ctrl Pts',(-4.43362955147839,6.81224442139068,2.10035810108909));
#19376=CARTESIAN_POINT('Ctrl Pts',(-4.60653546101629,6.69324425140002,2.1085801449808));
#19377=CARTESIAN_POINT('Ctrl Pts',(-4.77942228037852,6.57425721996637,2.11680128109403));
#19378=CARTESIAN_POINT('Ctrl Pts',(-4.94770693336127,6.4485609020799,2.12502241720726));
#19379=CARTESIAN_POINT('Ctrl Pts',(-5.11087502172616,6.31653734848419,2.1332435533205));
#19380=CARTESIAN_POINT('Ctrl Pts',(-5.27405605178104,6.18450332342975,2.1414653414938));
#19381=CARTESIAN_POINT('Ctrl Pts',(-5.43211947539644,6.04614124339584,2.14968712966711));
#19382=CARTESIAN_POINT('Ctrl Pts',(-5.5845835033449,5.90187382588513,2.15790891784042));
#19383=CARTESIAN_POINT('Ctrl Pts',(-5.73704710824618,5.75760680867819,2.16613068320044));
#19384=CARTESIAN_POINT('Ctrl Pts',(-5.88391113618556,5.60743469144081,2.17435244856047));
#19385=CARTESIAN_POINT('Ctrl Pts',(-6.02472985196757,5.45181784117104,2.1825742139205));
#19386=CARTESIAN_POINT('Ctrl Pts',(-6.16557792611431,5.29616854737113,2.19079769338212));
#19387=CARTESIAN_POINT('Ctrl Pts',(-6.30037797236411,5.13507247158846,2.19902117284375));
#19388=CARTESIAN_POINT('Ctrl Pts',(-6.42872309947458,4.96902474060875,2.20724465230538));
#19389=CARTESIAN_POINT('Ctrl Pts',(-6.48057928369124,4.90193530822983,2.21056724253895));
#19390=CARTESIAN_POINT('Ctrl Pts',(-6.53138219012593,4.83403791198284,2.21388983277253));
#19391=CARTESIAN_POINT('Ctrl Pts',(-6.58110689903197,4.76536667487547,2.2172124230061));
#19392=CARTESIAN_POINT('Ctrl Pts',(-6.70417747285668,4.59540271245138,2.22543596208006));
#19393=CARTESIAN_POINT('Ctrl Pts',(-6.82068027266697,4.42064095705765,2.23365950115403));
#19394=CARTESIAN_POINT('Ctrl Pts',(-6.93025437025903,4.24161077021521,2.24188304022799));
#19395=CARTESIAN_POINT('Ctrl Pts',(-7.039808545377,4.06261313417023,2.25010508411972));
#19396=CARTESIAN_POINT('Ctrl Pts',(-7.14243637872241,3.87934886706699,2.25832712801145));
#19397=CARTESIAN_POINT('Ctrl Pts',(-7.23782113182425,3.69237495742487,2.26654917190318));
#19398=CARTESIAN_POINT('Ctrl Pts',(-7.33319535369666,3.50542169117781,2.27477030801638));
#19399=CARTESIAN_POINT('Ctrl Pts',(-7.42132795790786,3.31475986271094,2.28299144412958));
#19400=CARTESIAN_POINT('Ctrl Pts',(-7.50194851633176,3.12097036525625,2.29121258024279));
#19401=CARTESIAN_POINT('Ctrl Pts',(-7.58257546918197,2.9271654973714,2.29943436841608));
#19402=CARTESIAN_POINT('Ctrl Pts',(-7.65568907000813,2.73023273612918,2.30765615658938));
#19403=CARTESIAN_POINT('Ctrl Pts',(-7.721066929415,2.53077320872379,2.31587794476268));
#19404=CARTESIAN_POINT('Ctrl Pts',(-7.78644460741566,2.33131423476562,2.3240997101227));
#19405=CARTESIAN_POINT('Ctrl Pts',(-7.84408649763372,2.12932878976982,2.33232147548272));
#19406=CARTESIAN_POINT('Ctrl Pts',(-7.8938198421495,1.925433941268,2.34054324084274));
#19407=CARTESIAN_POINT('Ctrl Pts',(-7.94356355524215,1.72149658407445,2.34876672030437));
#19408=CARTESIAN_POINT('Ctrl Pts',(-7.98539535889943,1.51564931471102,2.35699019976601));
#19409=CARTESIAN_POINT('Ctrl Pts',(-8.01919320408771,1.30852127151739,2.36521367922764));
#19410=CARTESIAN_POINT('Ctrl Pts',(-8.03284878514227,1.22483387172174,2.36853626946123));
#19411=CARTESIAN_POINT('Ctrl Pts',(-8.0451934389306,1.14093749967722,2.37185885969482));
#19412=CARTESIAN_POINT('Ctrl Pts',(-8.05622149971853,1.0568740274853,2.37518144992841));
#19413=CARTESIAN_POINT('Ctrl Pts',(-8.0848220889386,0.838860644823607,2.38379838088706));
#19414=CARTESIAN_POINT('Ctrl Pts',(-8.10457002472343,0.619675802307401,
2.39241531184572));
#19415=CARTESIAN_POINT('Ctrl Pts',(-8.11539718216024,0.400020172348403,
2.40103224280438));
#19416=CARTESIAN_POINT('Ctrl Pts',(-8.1219604218845,0.266868644385693,2.40625568061797));
#19417=CARTESIAN_POINT('Ctrl Pts',(-8.1252466529842,0.133544246018425,2.41147911843156));
#19418=CARTESIAN_POINT('Ctrl Pts',(-8.12524999744415,0.000203798425227694,
2.41670255624514));
#19419=CARTESIAN_POINT('Origin',(0.,0.,-16.4167025567876));
#19420=CARTESIAN_POINT('',(4.94675008185375,-6.44587862049697,-0.874941805641416));
#19421=CARTESIAN_POINT('',(4.94635340022636,-6.44536135767517,-0.708351351910811));
#19422=CARTESIAN_POINT('',(4.94675008185374,-6.44587862049697,-16.4167025567876));
#19423=CARTESIAN_POINT('',(-8.12524999749084,-0.000201928347416534,0.583297443881996));
#19424=CARTESIAN_POINT('Ctrl Pts',(4.94635340024336,-6.44536135766213,-0.708351351909972));
#19425=CARTESIAN_POINT('Ctrl Pts',(5.42466120603632,-6.07850642233277,-0.684741619201049));
#19426=CARTESIAN_POINT('Ctrl Pts',(6.83911309263365,-4.72344623181886,-0.608475544184695));
#19427=CARTESIAN_POINT('Ctrl Pts',(8.30188397303846,-1.66085451139327,-0.479553126860913));
#19428=CARTESIAN_POINT('Ctrl Pts',(8.09118691949813,2.49247055018721,-0.321584099938621));
#19429=CARTESIAN_POINT('Ctrl Pts',(5.92829110923838,6.0444255090069,-0.163615073016332));
#19430=CARTESIAN_POINT('Ctrl Pts',(2.33504859606946,8.13801347159135,-0.00564604609403982));
#19431=CARTESIAN_POINT('Ctrl Pts',(-1.82158208393826,8.26810461480037,0.152322980828249));
#19432=CARTESIAN_POINT('Ctrl Pts',(-5.53871107959393,6.40331123611773,0.310292007750539));
#19433=CARTESIAN_POINT('Ctrl Pts',(-7.70380757957238,3.30246000310552,0.453950161878586));
#19434=CARTESIAN_POINT('Ctrl Pts',(-8.1241451581117,0.978652145372449,0.544951973699204));
#19435=CARTESIAN_POINT('Ctrl Pts',(-8.12508170520043,-0.000201907072085276,
0.583297443212393));
#19436=CARTESIAN_POINT('Ctrl Pts',(-8.12524999749084,-0.000201928347416534,
0.583297443881996));
#19437=CARTESIAN_POINT('Ctrl Pts',(-8.12524454021968,-0.219793150063702,
0.591899496739723));
#19438=CARTESIAN_POINT('Ctrl Pts',(-8.11633280779128,-0.43934077896469,
0.600501549597456));
#19439=CARTESIAN_POINT('Ctrl Pts',(-8.09855135892644,-0.658143942713689,
0.609103602455193));
#19440=CARTESIAN_POINT('Ctrl Pts',(-8.08675056119947,-0.803354375060902,
0.614812422168505));
#19441=CARTESIAN_POINT('Ctrl Pts',(-8.07104424286953,-0.948236954424036,
0.620521241881815));
#19442=CARTESIAN_POINT('Ctrl Pts',(-8.05145571094098,-1.09258798147143,
0.626230061595127));
#19443=CARTESIAN_POINT('Ctrl Pts',(-8.02323848464808,-1.30052523836575,
0.634453600669086));
#19444=CARTESIAN_POINT('Ctrl Pts',(-7.9869570755542,-1.50740257609528,0.642677139743043));
#19445=CARTESIAN_POINT('Ctrl Pts',(-7.94271556594821,-1.71258780824344,
0.650900678817003));
#19446=CARTESIAN_POINT('Ctrl Pts',(-7.8984821002171,-1.9177357341525,0.659122722708722));
#19447=CARTESIAN_POINT('Ctrl Pts',(-7.84629148472197,-2.12119188035655,
0.667344766600445));
#19448=CARTESIAN_POINT('Ctrl Pts',(-7.78629884822644,-2.32233456000802,
0.675566810492164));
#19449=CARTESIAN_POINT('Ctrl Pts',(-7.7263128353911,-2.52345503192138,0.683787946605395));
#19450=CARTESIAN_POINT('Ctrl Pts',(-7.65852660558248,-2.7222622647074,0.692009082718634));
#19451=CARTESIAN_POINT('Ctrl Pts',(-7.58314530014621,-2.91814922842722,
0.700230218831866));
#19452=CARTESIAN_POINT('Ctrl Pts',(-7.50775801583566,-3.11405172893727,
0.708452007005168));
#19453=CARTESIAN_POINT('Ctrl Pts',(-7.42477455569331,-3.30703322136361,
0.716673795178469));
#19454=CARTESIAN_POINT('Ctrl Pts',(-7.33444879144874,-3.49650518205193,
0.724895583351771));
#19455=CARTESIAN_POINT('Ctrl Pts',(-7.24412327783427,-3.68597661700571,
0.733117348711786));
#19456=CARTESIAN_POINT('Ctrl Pts',(-7.14645563022167,-3.87193827463395,
0.741339114071796));
#19457=CARTESIAN_POINT('Ctrl Pts',(-7.04174664052734,-4.05382434413752,
0.749560879431812));
#19458=CARTESIAN_POINT('Ctrl Pts',(-6.93701582074652,-4.23574833386779,
0.757784358893447));
#19459=CARTESIAN_POINT('Ctrl Pts',(-6.82524087340846,-4.41359478238217,
0.766007838355089));
#19460=CARTESIAN_POINT('Ctrl Pts',(-6.70676762011063,-4.58682413575401,
0.774231317816724));
#19461=CARTESIAN_POINT('Ctrl Pts',(-6.65890003848872,-4.65681520952821,
0.777553908050289));
#19462=CARTESIAN_POINT('Ctrl Pts',(-6.60993948329258,-4.72605288535702,
0.780876498283847));
#19463=CARTESIAN_POINT('Ctrl Pts',(-6.55991074893576,-4.794502949055,0.784199088517411));
#19464=CARTESIAN_POINT('Ctrl Pts',(-6.43608770038518,-4.96391949875449,
0.792422627591374));
#19465=CARTESIAN_POINT('Ctrl Pts',(-6.30567799401478,-5.12856421320448,
0.800646166665331));
#19466=CARTESIAN_POINT('Ctrl Pts',(-6.1690741731326,-5.28793073034135,0.808869705739294));
#19467=CARTESIAN_POINT('Ctrl Pts',(-6.03249518919806,-5.44726827187697,
0.817091749630999));
#19468=CARTESIAN_POINT('Ctrl Pts',(-5.8897245303625,-5.60132930766949,0.825313793522708));
#19469=CARTESIAN_POINT('Ctrl Pts',(-5.74119462889958,-5.74964101449774,
0.833535837414413));
#19470=CARTESIAN_POINT('Ctrl Pts',(-5.59268112630853,-5.89793634654453,
0.841756973527664));
#19471=CARTESIAN_POINT('Ctrl Pts',(-5.43840985919502,-6.04048340860856,
0.84997810964091));
#19472=CARTESIAN_POINT('Ctrl Pts',(-5.27885026010335,-6.17684607982964,
0.858199245754161));
#19473=CARTESIAN_POINT('Ctrl Pts',(-5.11927800552985,-6.31321956666644,
0.866421033927452));
#19474=CARTESIAN_POINT('Ctrl Pts',(-4.95441680338497,-6.44340748893084,
0.874642822100743));
#19475=CARTESIAN_POINT('Ctrl Pts',(-4.78477012607616,-6.56701320259897,
0.882864610274034));
#19476=CARTESIAN_POINT('Ctrl Pts',(-4.61512391949124,-6.69061857329449,
0.891086375634074));
#19477=CARTESIAN_POINT('Ctrl Pts',(-4.4406925042627,-6.80764160042871,0.899308140994116));
#19478=CARTESIAN_POINT('Ctrl Pts',(-4.26200979787171,-6.917727953985,0.907529906354156));
#19479=CARTESIAN_POINT('Ctrl Pts',(-4.08328983910292,-7.02783725871836,
0.915753385815777));
#19480=CARTESIAN_POINT('Ctrl Pts',(-3.90031706969813,-7.13100684608687,
0.923976865277399));
#19481=CARTESIAN_POINT('Ctrl Pts',(-3.71365250227889,-7.2269269163883,0.932200344739019));
#19482=CARTESIAN_POINT('Ctrl Pts',(-3.63823310449802,-7.26568217689248,
0.935522934972579));
#19483=CARTESIAN_POINT('Ctrl Pts',(-3.56221131900306,-7.30325450513318,
0.938845525206136));
#19484=CARTESIAN_POINT('Ctrl Pts',(-3.48562524024981,-7.33962562035922,
0.942168115439696));
#19485=CARTESIAN_POINT('Ctrl Pts',(-3.29607173925316,-7.4296455344021,0.950391654513652));
#19486=CARTESIAN_POINT('Ctrl Pts',(-3.10299829935624,-7.51233302026449,
0.958615193587611));
#19487=CARTESIAN_POINT('Ctrl Pts',(-2.90699121411446,-7.58742971259447,
0.966838732661568));
#19488=CARTESIAN_POINT('Ctrl Pts',(-2.71101976636533,-7.66251275104139,
0.975060776553282));
#19489=CARTESIAN_POINT('Ctrl Pts',(-2.51211601312836,-7.73000764508645,
0.983282820444989));
#19490=CARTESIAN_POINT('Ctrl Pts',(-2.31088535521694,-7.7897045154193,0.991504864336704));
#19491=CARTESIAN_POINT('Ctrl Pts',(-2.10967691475733,-7.84939479474681,
0.999726000449923));
#19492=CARTESIAN_POINT('Ctrl Pts',(-1.9061423651767,-7.9012886853945,1.00794713656314));
#19493=CARTESIAN_POINT('Ctrl Pts',(-1.70090216801825,-7.94522620051379,
1.01616827267636));
#19494=CARTESIAN_POINT('Ctrl Pts',(-1.49564569221677,-7.98916720054069,
1.02439006084967));
#19495=CARTESIAN_POINT('Ctrl Pts',(-1.28868358638215,-8.02515049978894,
1.03261184902297));
#19496=CARTESIAN_POINT('Ctrl Pts',(-1.08064744844194,-8.05306703403591,
1.04083363719628));
#19497=CARTESIAN_POINT('Ctrl Pts',(-0.872611887746392,-8.08098349082196,
1.04905540255631));
#19498=CARTESIAN_POINT('Ctrl Pts',(-0.663502593577219,-8.10083319082789,
1.05727716791634));
#19499=CARTESIAN_POINT('Ctrl Pts',(-0.453957788196302,-8.11255877569068,
1.06549893327638));
#19500=CARTESIAN_POINT('Ctrl Pts',(-0.244369296202404,-8.12428680514325,
1.07372241273799));
#19501=CARTESIAN_POINT('Ctrl Pts',(-0.0343454061356596,-8.12788731935881,
1.08194589219961));
#19502=CARTESIAN_POINT('Ctrl Pts',(0.175473036514424,-8.12335501969207,
1.09016937166123));
#19503=CARTESIAN_POINT('Ctrl Pts',(0.260247457321311,-8.12152380278703,
1.09349196189481));
#19504=CARTESIAN_POINT('Ctrl Pts',(0.344988339062686,-8.11836553093617,
1.0968145521284));
#19505=CARTESIAN_POINT('Ctrl Pts',(0.429653478469153,-8.11388226750545,
1.10013714236199));
#19506=CARTESIAN_POINT('Ctrl Pts',(0.639202966417737,-8.10278601746875,
1.10836068143595));
#19507=CARTESIAN_POINT('Ctrl Pts',(0.848356402118719,-8.08356587578453,
1.1165842205099));
#19508=CARTESIAN_POINT('Ctrl Pts',(1.05647519957539,-8.05627381083725,1.12480775958386));
#19509=CARTESIAN_POINT('Ctrl Pts',(1.26455615741984,-8.02898670806142,1.13302980347558));
#19510=CARTESIAN_POINT('Ctrl Pts',(1.47160256019026,-7.99363064954546,1.1412518473673));
#19511=CARTESIAN_POINT('Ctrl Pts',(1.67698210643768,-7.95030933845897,1.14947389125902));
#19512=CARTESIAN_POINT('Ctrl Pts',(1.88233897716292,-7.90699281038699,1.15769502737223));
#19513=CARTESIAN_POINT('Ctrl Pts',(2.08602907031019,-7.85571284633579,1.16591616348543));
#19514=CARTESIAN_POINT('Ctrl Pts',(2.28743059701466,-7.79662419424851,1.17413729959864));
#19515=CARTESIAN_POINT('Ctrl Pts',(2.48884809789793,-7.73753085553987,1.18235908777194));
#19516=CARTESIAN_POINT('Ctrl Pts',(2.68797638588887,-7.67062767177349,1.19058087594524));
#19517=CARTESIAN_POINT('Ctrl Pts',(2.88420812614501,-7.59611947296638,1.19880266411855));
#19518=CARTESIAN_POINT('Ctrl Pts',(3.08043932191014,-7.52161148089976,1.20702442947857));
#19519=CARTESIAN_POINT('Ctrl Pts',(3.27377371124921,-7.43949862321621,1.21524619483858));
#19520=CARTESIAN_POINT('Ctrl Pts',(3.46362275400914,-7.35003435232858,1.2234679601986));
#19521=CARTESIAN_POINT('Ctrl Pts',(3.65351137714319,-7.26055142962547,1.23169143966023));
#19522=CARTESIAN_POINT('Ctrl Pts',(3.83991293524429,-7.16371415767408,1.23991491912185));
#19523=CARTESIAN_POINT('Ctrl Pts',(4.02226136976297,-7.05982301731513,1.24813839858348));
#19524=CARTESIAN_POINT('Ctrl Pts',(4.09593689001824,-7.01784714932338,1.25146098881708));
#19525=CARTESIAN_POINT('Ctrl Pts',(4.16895103655659,-6.97472028849727,1.25478357905068));
#19526=CARTESIAN_POINT('Ctrl Pts',(4.24126767987653,-6.93046434448189,1.25810616928428));
#19527=CARTESIAN_POINT('Ctrl Pts',(4.42025268512709,-6.82093007950061,1.26632964043981));
#19528=CARTESIAN_POINT('Ctrl Pts',(4.59502127405933,-6.70444066393231,1.27455311159534));
#19529=CARTESIAN_POINT('Ctrl Pts',(4.76503665606771,-6.58134585239456,1.28277658275087));
#19530=CARTESIAN_POINT('Ctrl Pts',(4.82623136667004,-6.53703955916557,1.28573650867971));
#19531=CARTESIAN_POINT('Ctrl Pts',(4.88681054383818,-6.4918779220727,1.28869643460856));
#19532=CARTESIAN_POINT('Ctrl Pts',(4.94675008185373,-6.44587862049698,1.2916563605374));
#19533=CARTESIAN_POINT('',(-8.12524999914245,-0.000118049505365691,0.416702556809683));
#19534=CARTESIAN_POINT('Ctrl Pts',(-8.12524999914245,-0.000118049505388336,
0.416702556809685));
#19535=CARTESIAN_POINT('Ctrl Pts',(-8.12524687413322,-0.215209854325447,
0.425126747983452));
#19536=CARTESIAN_POINT('Ctrl Pts',(-8.11669853744178,-0.430268792361165,
0.433550939157217));
#19537=CARTESIAN_POINT('Ctrl Pts',(-8.09963879299085,-0.644623134535036,
0.441975130330984));
#19538=CARTESIAN_POINT('Ctrl Pts',(-8.0825735898145,-0.859046065162715,
0.450402017051954));
#19539=CARTESIAN_POINT('Ctrl Pts',(-8.05699155812681,-1.07276368770188,
0.458828903772924));
#19540=CARTESIAN_POINT('Ctrl Pts',(-8.02297843455734,-1.28510878960804,
0.467255790493894));
#19541=CARTESIAN_POINT('Ctrl Pts',(-8.00643334361702,-1.38840036218568,
0.471354902616232));
#19542=CARTESIAN_POINT('Ctrl Pts',(-7.98789409470883,-1.49136727577943,
0.475454014738572));
#19543=CARTESIAN_POINT('Ctrl Pts',(-7.96737495602483,-1.59393345927877,
0.47955312686091));
#19544=CARTESIAN_POINT('Ctrl Pts',(-7.92620995889962,-1.79969924281946,
0.487776665934872));
#19545=CARTESIAN_POINT('Ctrl Pts',(-7.87706284174904,-2.00390290191428,
0.496000205008835));
#19546=CARTESIAN_POINT('Ctrl Pts',(-7.82007701584039,-2.20591999601636,
0.504223744082797));
#19547=CARTESIAN_POINT('Ctrl Pts',(-7.76310155094478,-2.40790035990155,
0.512445787974506));
#19548=CARTESIAN_POINT('Ctrl Pts',(-7.69829030188612,-2.6076946685525,0.520667831866216));
#19549=CARTESIAN_POINT('Ctrl Pts',(-7.62583696993005,-2.8046921525451,0.528889875757926));
#19550=CARTESIAN_POINT('Ctrl Pts',(-7.55339163739346,-3.00166788646123,
0.537111011871121));
#19551=CARTESIAN_POINT('Ctrl Pts',(-7.47330600823432,-3.19584713551087,
0.545332147984315));
#19552=CARTESIAN_POINT('Ctrl Pts',(-7.38582278187531,-3.38663688594329,
0.553553284097511));
#19553=CARTESIAN_POINT('Ctrl Pts',(-7.29833261677692,-3.57744176888064,
0.561775072270801));
#19554=CARTESIAN_POINT('Ctrl Pts',(-7.20344380264089,-3.76485634683022,
0.569996860444087));
#19555=CARTESIAN_POINT('Ctrl Pts',(-7.10144651664431,-3.94830912337678,
0.578218648617376));
#19556=CARTESIAN_POINT('Ctrl Pts',(-6.9994495136629,-4.13176139089098,0.586440413977404));
#19557=CARTESIAN_POINT('Ctrl Pts',(-6.89034422394947,-4.31125162253243,
0.594662179337436));
#19558=CARTESIAN_POINT('Ctrl Pts',(-6.77446623273054,-4.48623392436168,
0.602883944697464));
#19559=CARTESIAN_POINT('Ctrl Pts',(-6.65856408287404,-4.66125270709613,
0.611107424159086));
#19560=CARTESIAN_POINT('Ctrl Pts',(-6.53588657362123,-4.83176143656474,
0.619330903620711));
#19561=CARTESIAN_POINT('Ctrl Pts',(-6.40681258982334,-4.99724324016563,
0.627554383082334));
#19562=CARTESIAN_POINT('Ctrl Pts',(-6.35466192051321,-5.06410401692719,
0.630876973315957));
#19563=CARTESIAN_POINT('Ctrl Pts',(-6.30146752914131,-5.13014452302852,
0.634199563549582));
#19564=CARTESIAN_POINT('Ctrl Pts',(-6.24725630112025,-5.19533216172107,
0.637522153783205));
#19565=CARTESIAN_POINT('Ctrl Pts',(-6.11308141931654,-5.35667408360554,
0.645745692857165));
#19566=CARTESIAN_POINT('Ctrl Pts',(-5.97263116900281,-5.51284162408282,
0.653969231931124));
#19567=CARTESIAN_POINT('Ctrl Pts',(-5.82632898970532,-5.66335395911463,
0.662192771005085));
#19568=CARTESIAN_POINT('Ctrl Pts',(-5.68005341068557,-5.81383892838926,
0.670414814896784));
#19569=CARTESIAN_POINT('Ctrl Pts',(-5.52792823173882,-5.95867053303468,
0.678636858788479));
#19570=CARTESIAN_POINT('Ctrl Pts',(-5.37041460599619,-6.09740391660277,
0.686858902680179));
#19571=CARTESIAN_POINT('Ctrl Pts',(-5.21291837099923,-6.23612198291194,
0.695080038793433));
#19572=CARTESIAN_POINT('Ctrl Pts',(-5.05003509819688,-6.36874297748343,
0.703301174906686));
#19573=CARTESIAN_POINT('Ctrl Pts',(-4.88226057345853,-6.49486098814689,
0.711522311019941));
#19574=CARTESIAN_POINT('Ctrl Pts',(-4.71447274167077,-6.62098900187012,
0.719744099193243));
#19575=CARTESIAN_POINT('Ctrl Pts',(-4.54179311695569,-6.74061282175792,
0.727965887366544));
#19576=CARTESIAN_POINT('Ctrl Pts',(-4.36474898981035,-6.85336806383909,
0.736187675539846));
#19577=CARTESIAN_POINT('Ctrl Pts',(-4.1877053539147,-6.96612299305487,0.744409440899902));
#19578=CARTESIAN_POINT('Ctrl Pts',(-4.00629749002726,-7.0720092264295,0.752631206259964));
#19579=CARTESIAN_POINT('Ctrl Pts',(-3.82108042810118,-7.17070651501525,
0.760852971620022));
#19580=CARTESIAN_POINT('Ctrl Pts',(-3.63582475149297,-7.26942438034692,
0.769076451081645));
#19581=CARTESIAN_POINT('Ctrl Pts',(-3.4467585506843,-7.36095016804224,0.777299930543269));
#19582=CARTESIAN_POINT('Ctrl Pts',(-3.25446111311436,-7.44500976666428,
0.785523410004892));
#19583=CARTESIAN_POINT('Ctrl Pts',(-3.17676582719734,-7.47897295739391,
0.788846000238426));
#19584=CARTESIAN_POINT('Ctrl Pts',(-3.09854330512629,-7.51171786173033,
0.792168590471956));
#19585=CARTESIAN_POINT('Ctrl Pts',(-3.01983270995662,-7.54322861687063,
0.79549118070549));
#19586=CARTESIAN_POINT('Ctrl Pts',(-2.82502094882545,-7.62121895210089,
0.803714719779445));
#19587=CARTESIAN_POINT('Ctrl Pts',(-2.62715465840083,-7.69167109632274,
0.8119382588534));
#19588=CARTESIAN_POINT('Ctrl Pts',(-2.4268351412202,-7.75436385268571,0.820161797927355));
#19589=CARTESIAN_POINT('Ctrl Pts',(-2.22655204560707,-7.81704521041668,
0.828383841819075));
#19590=CARTESIAN_POINT('Ctrl Pts',(-2.02381689481391,-7.87196990802028,
0.836605885710796));
#19591=CARTESIAN_POINT('Ctrl Pts',(-1.81924702925051,-7.91896633463378,
0.844827929602516));
#19592=CARTESIAN_POINT('Ctrl Pts',(-1.61469974981416,-7.96595757247102,
0.853049065715726));
#19593=CARTESIAN_POINT('Ctrl Pts',(-1.40831844736009,-8.00502222089918,
0.86127020182893));
#19594=CARTESIAN_POINT('Ctrl Pts',(-1.20073237361383,-8.03603940566842,
0.86949133794214));
#19595=CARTESIAN_POINT('Ctrl Pts',(-0.993129835160831,-8.06705905056826,
0.877713126115445));
#19596=CARTESIAN_POINT('Ctrl Pts',(-0.784322625798179,-8.09002991024968,
0.885934914288751));
#19597=CARTESIAN_POINT('Ctrl Pts',(-0.574947927482478,-8.10488262982158,
0.894156702462055));
#19598=CARTESIAN_POINT('Ctrl Pts',(-0.365573810125681,-8.11973530818115,
0.902378467822092));
#19599=CARTESIAN_POINT('Ctrl Pts',(-0.155632501349239,-8.12646987331069,
0.91060023318213));
#19600=CARTESIAN_POINT('Ctrl Pts',(0.0542354388566744,-8.12506898922538,
0.918821998542168));
#19601=CARTESIAN_POINT('Ctrl Pts',(0.264147133044124,-8.123667813079,0.927045478003794));
#19602=CARTESIAN_POINT('Ctrl Pts',(0.473985133124605,-8.11412780135323,
0.935268957465419));
#19603=CARTESIAN_POINT('Ctrl Pts',(0.683109516478365,-8.09648373993283,
0.943492436927045));
#19604=CARTESIAN_POINT('Ctrl Pts',(0.767603511626854,-8.08935488572584,
0.946815027160623));
#19605=CARTESIAN_POINT('Ctrl Pts',(0.851981048272906,-8.08090367108565,
0.950137617394203));
#19606=CARTESIAN_POINT('Ctrl Pts',(0.936200134772983,-8.07113479444812,
0.953460207627781));
#19607=CARTESIAN_POINT('Ctrl Pts',(1.14464562456212,-8.04695644770961,0.961683746701744));
#19608=CARTESIAN_POINT('Ctrl Pts',(1.35218782376651,-8.01469487519154,0.969907285775705));
#19609=CARTESIAN_POINT('Ctrl Pts',(1.55819264593138,-7.97444187643658,0.978130824849668));
#19610=CARTESIAN_POINT('Ctrl Pts',(1.76416001284117,-7.93419619637601,0.986352868741379));
#19611=CARTESIAN_POINT('Ctrl Pts',(1.96859027128783,-7.88596204659278,0.994574912633096));
#19612=CARTESIAN_POINT('Ctrl Pts',(2.17085884220969,-7.82988246717025,1.00279695652481));
#19613=CARTESIAN_POINT('Ctrl Pts',(2.3731050810857,-7.77380907937566,1.01101809263801));
#19614=CARTESIAN_POINT('Ctrl Pts',(2.57318982482481,-7.70989207004109,1.01923922875122));
#19615=CARTESIAN_POINT('Ctrl Pts',(2.77050217837134,-7.63832476673646,1.02746036486442));
#19616=CARTESIAN_POINT('Ctrl Pts',(2.96783018176366,-7.56675178706521,1.03568215303772));
#19617=CARTESIAN_POINT('Ctrl Pts',(3.16238507742671,-7.48752739909126,1.04390394121103));
#19618=CARTESIAN_POINT('Ctrl Pts',(3.35357352783447,-7.40089401058466,1.05212572938433));
#19619=CARTESIAN_POINT('Ctrl Pts',(3.54476144774538,-7.31426086246256,1.06034749474437));
#19620=CARTESIAN_POINT('Ctrl Pts',(3.73258267355998,-7.22021887911594,1.0685692601044));
#19621=CARTESIAN_POINT('Ctrl Pts',(3.91646566617528,-7.11905782025755,1.07679102546444));
#19622=CARTESIAN_POINT('Ctrl Pts',(4.1003869953419,-7.01787567099776,1.08501450492607));
#19623=CARTESIAN_POINT('Ctrl Pts',(4.28036819261821,-6.90957162338873,1.0932379843877));
#19624=CARTESIAN_POINT('Ctrl Pts',(4.45586309734674,-6.79448096768278,1.10146146384933));
#19625=CARTESIAN_POINT('Ctrl Pts',(4.52676953776714,-6.74798008075171,1.10478405408291));
#19626=CARTESIAN_POINT('Ctrl Pts',(4.59694392351972,-6.70037181147411,1.10810664431649));
#19627=CARTESIAN_POINT('Ctrl Pts',(4.66635156589433,-6.65168028591088,1.11142923455007));
#19628=CARTESIAN_POINT('Ctrl Pts',(4.76126383227299,-6.58509650800792,1.1159727481824));
#19629=CARTESIAN_POINT('Ctrl Pts',(4.85475927892587,-6.51647497185647,1.12051626181472));
#19630=CARTESIAN_POINT('Ctrl Pts',(4.94675008185375,-6.44587862049697,1.12505977544705));
#19631=CARTESIAN_POINT('Ctrl Pts',(4.94675008185375,-6.44587862049697,-0.874941805641418));
#19632=CARTESIAN_POINT('Ctrl Pts',(5.11327314749972,-6.31808409672245,-0.86671990801957));
#19633=CARTESIAN_POINT('Ctrl Pts',(5.27484531963509,-6.18383017067312,-0.858498010397723));
#19634=CARTESIAN_POINT('Ctrl Pts',(5.43097363732824,-6.04352652953106,-0.850276112775875));
#19635=CARTESIAN_POINT('Ctrl Pts',(5.58709844738019,-5.90322604050668,-0.842054399870465));
#19636=CARTESIAN_POINT('Ctrl Pts',(5.73777942951179,-5.75687630682174,-0.833832686965053));
#19637=CARTESIAN_POINT('Ctrl Pts',(5.88255864950201,-5.60492562820142,-0.825610974059643));
#19638=CARTESIAN_POINT('Ctrl Pts',(6.02737062138856,-5.45294057536032,-0.817387401241679));
#19639=CARTESIAN_POINT('Ctrl Pts',(6.16627795939731,-5.29535225899986,-0.809163828423718));
#19640=CARTESIAN_POINT('Ctrl Pts',(6.2988605775536,-5.13264483351821,-0.800940255605756));
#19641=CARTESIAN_POINT('Ctrl Pts',(6.38882908689042,-5.02223409693612,-0.795359866576308));
#19642=CARTESIAN_POINT('Ctrl Pts',(6.47588600295847,-4.90946686505836,-0.789779477546862));
#19643=CARTESIAN_POINT('Ctrl Pts',(6.55991074893582,-4.79450294905492,-0.784199088517413));
#19644=CARTESIAN_POINT('Ctrl Pts',(6.68373379748634,-4.6250863993555,-0.775975549443454));
#19645=CARTESIAN_POINT('Ctrl Pts',(6.80101041183197,-4.45084297985416,-0.767752010369493));
#19646=CARTESIAN_POINT('Ctrl Pts',(6.91137731992751,-4.27230044637449,-0.759528471295534));
#19647=CARTESIAN_POINT('Ctrl Pts',(7.02172416140205,-4.09379037502874,-0.751306427403823));
#19648=CARTESIAN_POINT('Ctrl Pts',(7.12516364906538,-3.91098300054452,-0.743084383512117));
#19649=CARTESIAN_POINT('Ctrl Pts',(7.22137657766206,-3.72443390142633,-0.734862339620406));
#19650=CARTESIAN_POINT('Ctrl Pts',(7.3175788835926,-3.53790539879999,-0.726641203507188));
#19651=CARTESIAN_POINT('Ctrl Pts',(7.40655608823384,-3.34763625833373,-0.718420067393964));
#19652=CARTESIAN_POINT('Ctrl Pts',(7.48803519021739,-3.15420616836724,-0.710198931280747));
#19653=CARTESIAN_POINT('Ctrl Pts',(7.56952075472257,-2.96076073647738,-0.701977143107448));
#19654=CARTESIAN_POINT('Ctrl Pts',(7.6435069113411,-2.7641541249276,-0.69375535493415));
#19655=CARTESIAN_POINT('Ctrl Pts',(7.70976860723802,-2.56498646884289,-0.685533566760851));
#19656=CARTESIAN_POINT('Ctrl Pts',(7.7760301192764,-2.36581936539532,-0.677311801400822));
#19657=CARTESIAN_POINT('Ctrl Pts',(7.83456712292162,-2.16409151232984,-0.669090036040793));
#19658=CARTESIAN_POINT('Ctrl Pts',(7.88520412564079,-1.96041920503689,-0.660868270680764));
#19659=CARTESIAN_POINT('Ctrl Pts',(7.93585168533444,-1.75670443544888,-0.65264479121914));
#19660=CARTESIAN_POINT('Ctrl Pts',(7.97859588265768,-1.55104468805848,-0.644421311757514));
#19661=CARTESIAN_POINT('Ctrl Pts',(8.01331187993856,-1.344068553808,-0.63619783229589));
#19662=CARTESIAN_POINT('Ctrl Pts',(8.02733842843948,-1.26044253085067,-0.6328752420623));
#19663=CARTESIAN_POINT('Ctrl Pts',(8.0400549892254,-1.17660172454979,-0.629552651828708));
#19664=CARTESIAN_POINT('Ctrl Pts',(8.05145571094102,-1.09258798147116,-0.626230061595118));
#19665=CARTESIAN_POINT('Ctrl Pts',(8.07967293723391,-0.88465072457684,-0.618006522521159));
#19666=CARTESIAN_POINT('Ctrl Pts',(8.09983514702286,-0.675586000607633,
-0.609782983447201));
#19667=CARTESIAN_POINT('Ctrl Pts',(8.11187418476942,-0.466030871264436,
-0.601559444373242));
#19668=CARTESIAN_POINT('Ctrl Pts',(8.12391103360979,-0.256513842683761,
-0.593337400481531));
#19669=CARTESIAN_POINT('Ctrl Pts',(8.12782764129082,-0.046506880994045,
-0.585115356589818));
#19670=CARTESIAN_POINT('Ctrl Pts',(8.12360785080587,0.163349468395798,-0.576893312698108));
#19671=CARTESIAN_POINT('Ctrl Pts',(8.11938852621907,0.373182647989396,-0.568672176584895));
#19672=CARTESIAN_POINT('Ctrl Pts',(8.10703460286112,0.582864953721563,-0.560451040471686));
#19673=CARTESIAN_POINT('Ctrl Pts',(8.08658203365941,0.791756638997664,-0.552229904358473));
#19674=CARTESIAN_POINT('Ctrl Pts',(8.06612784226048,1.00066489253497,-0.544008116185173));
#19675=CARTESIAN_POINT('Ctrl Pts',(8.03757374765707,1.20878210652183,-0.53578632801187));
#19676=CARTESIAN_POINT('Ctrl Pts',(8.00100760271659,1.41547338504518,-0.52756453983857));
#19677=CARTESIAN_POINT('Ctrl Pts',(7.96444155923741,1.6221640900554,-0.519342774478538));
#19678=CARTESIAN_POINT('Ctrl Pts',(7.91986356392611,1.82742857756414,-0.511121009118508));
#19679=CARTESIAN_POINT('Ctrl Pts',(7.86741274588157,2.03064133919318,-0.502899243758476));
#19680=CARTESIAN_POINT('Ctrl Pts',(7.81495099271218,2.23389646730957,-0.494675764296853));
#19681=CARTESIAN_POINT('Ctrl Pts',(7.75461321157937,2.43509872939787,-0.486452284835224));
#19682=CARTESIAN_POINT('Ctrl Pts',(7.68658893013407,2.63363592427662,-0.4782288053736));
#19683=CARTESIAN_POINT('Ctrl Pts',(7.65910460136156,2.71385230321782,-0.474906215140009));
#19684=CARTESIAN_POINT('Ctrl Pts',(7.63036604866938,2.79363380049986,-0.471583624906421));
#19685=CARTESIAN_POINT('Ctrl Pts',(7.60038805194703,2.87294083167766,-0.46826103467283));
#19686=CARTESIAN_POINT('Ctrl Pts',(7.52619135296413,3.06922879494708,-0.460037495598869));
#19687=CARTESIAN_POINT('Ctrl Pts',(7.44437452692853,3.26267279327572,-0.451813956524908));
#19688=CARTESIAN_POINT('Ctrl Pts',(7.35518097901611,3.45268016596088,-0.443590417450947));
#19689=CARTESIAN_POINT('Ctrl Pts',(7.26600364803999,3.64265299200525,-0.435368373559233));
#19690=CARTESIAN_POINT('Ctrl Pts',(7.16945239736635,3.82919017266169,-0.427146329667522));
#19691=CARTESIAN_POINT('Ctrl Pts',(7.06581801651437,4.01172074302299,-0.418924285775809));
#19692=CARTESIAN_POINT('Ctrl Pts',(6.96219507771549,4.19423116056954,-0.410703149662595));
#19693=CARTESIAN_POINT('Ctrl Pts',(6.8514907156021,4.3727355946001,-0.402482013549381));
#19694=CARTESIAN_POINT('Ctrl Pts',(6.73404116286537,4.54668859493752,-0.394260877436167));
#19695=CARTESIAN_POINT('Ctrl Pts',(6.61658229460772,4.72065539237142,-0.386039089262869));
#19696=CARTESIAN_POINT('Ctrl Pts',(6.49237732960357,4.89006978888062,-0.377817301089569));
#19697=CARTESIAN_POINT('Ctrl Pts',(6.36180582974787,5.05441531208962,-0.36959551291627));
#19698=CARTESIAN_POINT('Ctrl Pts',(6.23123469219314,5.21876037928376,-0.361373747556233));
#19699=CARTESIAN_POINT('Ctrl Pts',(6.09429724070153,5.37803637206743,-0.353151982196201));
#19700=CARTESIAN_POINT('Ctrl Pts',(5.95141365767106,5.53175948842557,-0.344930216836165));
#19701=CARTESIAN_POINT('Ctrl Pts',(5.8085002857856,5.68551465350145,-0.336706737374544));
#19702=CARTESIAN_POINT('Ctrl Pts',(5.65963850668627,5.8337144133691,-0.328483257912925));
#19703=CARTESIAN_POINT('Ctrl Pts',(5.50528648511832,5.97591066526882,-0.320259778451305));
#19704=CARTESIAN_POINT('Ctrl Pts',(5.4429225524558,6.03336321683408,-0.316937188217719));
#19705=CARTESIAN_POINT('Ctrl Pts',(5.37966277217823,6.08983614768258,-0.313614597984127));
#19706=CARTESIAN_POINT('Ctrl Pts',(5.31553898940635,6.14530168621532,-0.31029200775054));
#19707=CARTESIAN_POINT('Ctrl Pts',(5.15683015198659,6.28258103495103,-0.302068468676578));
#19708=CARTESIAN_POINT('Ctrl Pts',(4.99277462089054,6.4137311635393,-0.293844929602612));
#19709=CARTESIAN_POINT('Ctrl Pts',(4.82386863449584,6.53834680631329,-0.28562139052865));
#19710=CARTESIAN_POINT('Ctrl Pts',(4.6549933581435,6.66293979179875,-0.277399346636941));
#19711=CARTESIAN_POINT('Ctrl Pts',(4.48126962387305,6.7810004877351,-0.269177302745237));
#19712=CARTESIAN_POINT('Ctrl Pts',(4.30322500757334,6.89216526910777,-0.260955258853528));
#19713=CARTESIAN_POINT('Ctrl Pts',(4.12520004880356,7.0033177770118,-0.252734122740314));
#19714=CARTESIAN_POINT('Ctrl Pts',(3.94285541051428,7.10757573424601,-0.244512986627104));
#19715=CARTESIAN_POINT('Ctrl Pts',(3.75674648071624,7.2046195903827,-0.23629185051389));
#19716=CARTESIAN_POINT('Ctrl Pts',(3.57062278967321,7.30167114356077,-0.228070062340593));
#19717=CARTESIAN_POINT('Ctrl Pts',(3.38073447086042,7.39150731364108,-0.21984827416729));
#19718=CARTESIAN_POINT('Ctrl Pts',(3.1876612165152,7.47385466350697,-0.211626485993992));
#19719=CARTESIAN_POINT('Ctrl Pts',(2.99458849789658,7.55620178488101,-0.203404720633957));
#19720=CARTESIAN_POINT('Ctrl Pts',(2.79833113376881,7.63106001438087,-0.195182955273926));
#19721=CARTESIAN_POINT('Ctrl Pts',(2.59948898044392,7.69820398554433,-0.186961189913891));
#19722=CARTESIAN_POINT('Ctrl Pts',(2.4006053718309,7.76536195511117,-0.178737710452262));
#19723=CARTESIAN_POINT('Ctrl Pts',(2.1991361769637,7.82480235905585,-0.17051423099063));
#19724=CARTESIAN_POINT('Ctrl Pts',(1.99569765411705,7.87634930890268,-0.162290751529));
#19725=CARTESIAN_POINT('Ctrl Pts',(1.91350095717157,7.89717618552239,-0.158968161295416));
#19726=CARTESIAN_POINT('Ctrl Pts',(1.83098293428684,7.91671506006955,-0.155645571061832));
#19727=CARTESIAN_POINT('Ctrl Pts',(1.74818481239271,7.9349566743757,-0.152322980828249));
#19728=CARTESIAN_POINT('Ctrl Pts',(1.54325626485029,7.98010537387601,-0.144099441754288));
#19729=CARTESIAN_POINT('Ctrl Pts',(1.33654447896043,8.01731842382004,-0.135875902680326));
#19730=CARTESIAN_POINT('Ctrl Pts',(1.12867879653315,8.046475733932,-0.127652363606366));
#19731=CARTESIAN_POINT('Ctrl Pts',(0.920850907697369,8.07562774273854,-0.119430319714644));
#19732=CARTESIAN_POINT('Ctrl Pts',(0.711869832988523,8.09672689408454,-0.11120827582293));
#19733=CARTESIAN_POINT('Ctrl Pts',(0.502372643946926,8.10970463636708,-0.102986231931208));
#19734=CARTESIAN_POINT('Ctrl Pts',(0.292898585047747,8.12268094580449,-0.0947650958179964));
#19735=CARTESIAN_POINT('Ctrl Pts',(0.0829088198363098,8.12753761811397,
-0.0865439597047853));
#19736=CARTESIAN_POINT('Ctrl Pts',(-0.12695610943686,8.12425810205317,-0.0783228235915736));
#19737=CARTESIAN_POINT('Ctrl Pts',(-0.336837684164142,8.12097832587729,
-0.0701010354182755));
#19738=CARTESIAN_POINT('Ctrl Pts',(-0.546594108220713,8.10956107387643,
-0.061879247244974));
#19739=CARTESIAN_POINT('Ctrl Pts',(-0.755585424101854,8.09004191765314,
-0.0536574590716761));
#19740=CARTESIAN_POINT('Ctrl Pts',(-0.96457616008799,8.07052281559028,-0.0454356937116414));
#19741=CARTESIAN_POINT('Ctrl Pts',(-1.17280149874207,8.04290188438544,-0.0372139283516024));
#19742=CARTESIAN_POINT('Ctrl Pts',(-1.37962663999424,8.00726656835641,-0.0289921629915675));
#19743=CARTESIAN_POINT('Ctrl Pts',(-1.58649490085494,7.97162382295555,-0.0207686835299415));
#19744=CARTESIAN_POINT('Ctrl Pts',(-1.7919620904431,7.92796340490616,-0.0125452040683227));
#19745=CARTESIAN_POINT('Ctrl Pts',(-1.99540254448947,7.87642407745704,-0.00432172460669733));
#19746=CARTESIAN_POINT('Ctrl Pts',(-2.07760002171104,7.8556002805683,-0.000999134373119851));
#19747=CARTESIAN_POINT('Ctrl Pts',(-2.15946677537406,7.83349086257444,0.00232345586046502));
#19748=CARTESIAN_POINT('Ctrl Pts',(-2.24096214375505,7.81010731249941,0.00564604609404284));
#19749=CARTESIAN_POINT('Ctrl Pts',(-2.44266632606883,7.75223212350183,0.013869585168));
#19750=CARTESIAN_POINT('Ctrl Pts',(-2.64216004109066,7.68652952706406,0.022093124241958));
#19751=CARTESIAN_POINT('Ctrl Pts',(-2.83883268783922,7.61319358304749,0.0303166633159151));
#19752=CARTESIAN_POINT('Ctrl Pts',(-3.03546957608432,7.53987097277942,0.0385387072076221));
#19753=CARTESIAN_POINT('Ctrl Pts',(-3.22928614357328,7.45891788796716,0.0467607510993229));
#19754=CARTESIAN_POINT('Ctrl Pts',(-3.41968953236387,7.37057739018735,0.0549827949910302));
#19755=CARTESIAN_POINT('Ctrl Pts',(-3.61007189911896,7.28224664589508,0.0632039311042589));
#19756=CARTESIAN_POINT('Ctrl Pts',(-3.79704157208945,7.18653024108916,0.0714250672174895));
#19757=CARTESIAN_POINT('Ctrl Pts',(-3.98002740142911,7.08371861710878,0.0796462033307179));
#19758=CARTESIAN_POINT('Ctrl Pts',(-4.16302774430435,6.98089883861626,0.0878679915040102));
#19759=CARTESIAN_POINT('Ctrl Pts',(-4.34204335375989,6.87098285867043,0.0960897796773056));
#19760=CARTESIAN_POINT('Ctrl Pts',(-4.51652841258331,6.754306675065,0.104311567850598));
#19761=CARTESIAN_POINT('Ctrl Pts',(-4.69101298725775,6.63763081520452,0.112533333210645));
#19762=CARTESIAN_POINT('Ctrl Pts',(-4.86096679277625,6.51419495539005,0.120755098570688));
#19763=CARTESIAN_POINT('Ctrl Pts',(-5.0258732465123,6.38437825261724,0.128976863930735));
#19764=CARTESIAN_POINT('Ctrl Pts',(-5.19081408050607,6.2545344852172,0.137200343392356));
#19765=CARTESIAN_POINT('Ctrl Pts',(-5.35070522876196,6.11830739976473,0.14542382285398));
#19766=CARTESIAN_POINT('Ctrl Pts',(-5.50506257797969,5.97611693117091,0.153647302315601));
#19767=CARTESIAN_POINT('Ctrl Pts',(-5.56742866320986,5.91866671627553,0.156969892549181));
#19768=CARTESIAN_POINT('Ctrl Pts',(-5.6288917706135,5.86024344909845,0.160292482782762));
#19769=CARTESIAN_POINT('Ctrl Pts',(-5.68942161431893,5.80087659384515,0.163615073016341));
#19770=CARTESIAN_POINT('Ctrl Pts',(-5.83923531383011,5.65394133564222,0.171838612090299));
#19771=CARTESIAN_POINT('Ctrl Pts',(-5.98337817025907,5.50117546755519,0.18006215116426));
#19772=CARTESIAN_POINT('Ctrl Pts',(-6.12140564602634,5.34304037784638,0.188285690238217));
#19773=CARTESIAN_POINT('Ctrl Pts',(-6.259408026001,5.18493403984367,0.196507734129929));
#19774=CARTESIAN_POINT('Ctrl Pts',(-6.39129705065561,5.02146065072623,0.204729778021638));
#19775=CARTESIAN_POINT('Ctrl Pts',(-6.51666711727254,4.85311624063949,0.21295182191335));
#19776=CARTESIAN_POINT('Ctrl Pts',(-6.64202334204516,4.68479041710358,0.221172958026559));
#19777=CARTESIAN_POINT('Ctrl Pts',(-6.76086186963076,4.51159488274793,0.229394094139772));
#19778=CARTESIAN_POINT('Ctrl Pts',(-6.87281874659945,4.3340569953441,0.237615230252981));
#19779=CARTESIAN_POINT('Ctrl Pts',(-6.98478450343718,4.15650502650792,0.245837018426287));
#19780=CARTESIAN_POINT('Ctrl Pts',(-7.08986735949618,3.97461026451954,0.254058806599588));
#19781=CARTESIAN_POINT('Ctrl Pts',(-7.18774732974459,3.78892806559447,0.262280594772893));
#19782=CARTESIAN_POINT('Ctrl Pts',(-7.285627028402,3.60324638188835,0.270502360132912));
#19783=CARTESIAN_POINT('Ctrl Pts',(-7.37630374608216,3.41377754442737,0.278724125492935));
#19784=CARTESIAN_POINT('Ctrl Pts',(-7.45950375592395,3.22110094189184,0.286945890852955));
#19785=CARTESIAN_POINT('Ctrl Pts',(-7.54272111158676,3.0283841694829,0.29516937031458));
#19786=CARTESIAN_POINT('Ctrl Pts',(-7.61845852849534,2.83245856681313,0.303392849776207));
#19787=CARTESIAN_POINT('Ctrl Pts',(-7.68649024861327,2.63392392078306,0.311616329237832));
#19788=CARTESIAN_POINT('Ctrl Pts',(-7.713977582885,2.55370857167107,0.314938919471426));
#19789=CARTESIAN_POINT('Ctrl Pts',(-7.74020755077312,2.47306751200538,0.318261509705021));
#19790=CARTESIAN_POINT('Ctrl Pts',(-7.7651675494726,2.39204107220542,0.321584099938615));
#19791=CARTESIAN_POINT('Ctrl Pts',(-7.82717535069625,2.19074813812044,0.329838367786659));
#19792=CARTESIAN_POINT('Ctrl Pts',(-7.88136145535427,1.98701200604582,0.338092635634704));
#19793=CARTESIAN_POINT('Ctrl Pts',(-7.92755364808531,1.78145466381532,0.346346903482747));
#19794=CARTESIAN_POINT('Ctrl Pts',(-7.97373622309538,1.57594012087713,0.354599452701727));
#19795=CARTESIAN_POINT('Ctrl Pts',(-8.01192814537018,1.3686054079537,0.362852001920708));
#19796=CARTESIAN_POINT('Ctrl Pts',(-8.04200794311919,1.16008439576948,0.371104551139688));
#19797=CARTESIAN_POINT('Ctrl Pts',(-8.07208563879751,0.951577955688139,
0.379356523644623));
#19798=CARTESIAN_POINT('Ctrl Pts',(-8.09405229791888,0.741885668826661,
0.387608496149557));
#19799=CARTESIAN_POINT('Ctrl Pts',(-8.10783797364475,0.531649278777049,
0.395860468654494));
#19800=CARTESIAN_POINT('Ctrl Pts',(-8.11944417924312,0.354650572605817,
0.402807831365534));
#19801=CARTESIAN_POINT('Ctrl Pts',(-8.12525257630012,0.177266432657982,
0.409755194076573));
#19802=CARTESIAN_POINT('Ctrl Pts',(-8.12524999914245,-0.000118048941944703,
0.416702556787612));
#19803=CARTESIAN_POINT('Origin',(0.,0.,-16.4167025567876));
#19804=CARTESIAN_POINT('',(4.94673849251696,-6.44586330438811,-2.8749518510811));
#19805=CARTESIAN_POINT('',(4.94675008185376,-6.44587862049696,-2.70835307946025));
#19806=CARTESIAN_POINT('',(4.94675008185374,-6.44587862049697,-16.4167025567876));
#19807=CARTESIAN_POINT('',(-8.12527573348029,9.06015700713918E-5,-1.41670255634212));
#19808=CARTESIAN_POINT('Ctrl Pts',(4.94675008185376,-6.44587862049696,-2.70835307946025));
#19809=CARTESIAN_POINT('Ctrl Pts',(5.06306175751159,-6.35661774157638,-2.70260855423116));
#19810=CARTESIAN_POINT('Ctrl Pts',(5.17694645893466,-6.2642158434986,-2.69686402900206));
#19811=CARTESIAN_POINT('Ctrl Pts',(5.28823612645863,-6.16881238435064,-2.69111950377297));
#19812=CARTESIAN_POINT('Ctrl Pts',(5.44755215222471,-6.0322381605799,-2.682895964699));
#19813=CARTESIAN_POINT('Ctrl Pts',(5.60160046959401,-5.8894667018507,-2.67467242562504));
#19814=CARTESIAN_POINT('Ctrl Pts',(5.74990664483424,-5.7409285954618,-2.66644888655107));
#19815=CARTESIAN_POINT('Ctrl Pts',(5.89818585543617,-5.59241749588032,-2.65822684265933));
#19816=CARTESIAN_POINT('Ctrl Pts',(6.04072479937175,-5.43814204988859,-2.65000479876759));
#19817=CARTESIAN_POINT('Ctrl Pts',(6.17708557082848,-5.27857001593827,-2.64178275487584));
#19818=CARTESIAN_POINT('Ctrl Pts',(6.31343128697988,-5.11901559999985,-2.63356161876263));
#19819=CARTESIAN_POINT('Ctrl Pts',(6.44360000094805,-4.95416598773666,-2.62534048264943));
#19820=CARTESIAN_POINT('Ctrl Pts',(6.56719326509157,-4.78452298368771,-2.61711934653622));
#19821=CARTESIAN_POINT('Ctrl Pts',(6.69079633204521,-4.61486652438965,-2.60889755836291));
#19822=CARTESIAN_POINT('Ctrl Pts',(6.80782273128667,-4.44041615048072,-2.6006757701896));
#19823=CARTESIAN_POINT('Ctrl Pts',(6.91791601016778,-4.2617045461604,-2.59245398201628));
#19824=CARTESIAN_POINT('Ctrl Pts',(7.02800898356961,-4.08299343771681,-2.58423221665623));
#19825=CARTESIAN_POINT('Ctrl Pts',(7.13116872269657,-3.9000213750359,-2.57601045129617));
#19826=CARTESIAN_POINT('Ctrl Pts',(7.22708332008315,-3.71334811821837,-2.56778868593612));
#19827=CARTESIAN_POINT('Ctrl Pts',(7.32301791407054,-3.52663594312667,-2.55956520647452));
#19828=CARTESIAN_POINT('Ctrl Pts',(7.41170421397583,-3.33622129476586,-2.55134172701291));
#19829=CARTESIAN_POINT('Ctrl Pts',(7.49287680767403,-3.14268749759192,-2.54311824755131));
#19830=CARTESIAN_POINT('Ctrl Pts',(7.52567354150333,-3.06449267660979,-2.53979565731777));
#19831=CARTESIAN_POINT('Ctrl Pts',(7.5572442356429,-2.98578890928741,-2.53647306708422));
#19832=CARTESIAN_POINT('Ctrl Pts',(7.58757361511294,-2.90661559167049,-2.53315047685068));
#19833=CARTESIAN_POINT('Ctrl Pts',(7.66263999996019,-2.7106585746225,-2.52492693777672));
#19834=CARTESIAN_POINT('Ctrl Pts',(7.73012332902734,-2.51176017390019,-2.51670339870277));
#19835=CARTESIAN_POINT('Ctrl Pts',(7.78981142829103,-2.31052493476405,-2.50847985962881));
#19836=CARTESIAN_POINT('Ctrl Pts',(7.84948867522159,-2.10932628368951,-2.50025781573709));
#19837=CARTESIAN_POINT('Ctrl Pts',(7.90137343730657,-1.9057919248274,-2.49203577184536));
#19838=CARTESIAN_POINT('Ctrl Pts',(7.94530336095335,-1.70054169749622,-2.48381372795363));
#19839=CARTESIAN_POINT('Ctrl Pts',(7.98922843438995,-1.49531413140961,-2.47559259184043));
#19840=CARTESIAN_POINT('Ctrl Pts',(8.0252003611327,-1.28837136336534,-2.46737145572723));
#19841=CARTESIAN_POINT('Ctrl Pts',(8.05310769676512,-1.08034438342702,-2.45915031961402));
#19842=CARTESIAN_POINT('Ctrl Pts',(8.08101724587018,-0.872300903811568,
-2.45092853144073));
#19843=CARTESIAN_POINT('Ctrl Pts',(8.10086088395555,-0.663173332449556,
-2.44270674326743));
#19844=CARTESIAN_POINT('Ctrl Pts',(8.112578798865,-0.453599817797638,-2.43448495509413));
#19845=CARTESIAN_POINT('Ctrl Pts',(8.12429668126033,-0.244026884656978,
-2.42626318973413));
#19846=CARTESIAN_POINT('Ctrl Pts',(8.12788887180866,-0.0340083053242616,
-2.41804142437413));
#19847=CARTESIAN_POINT('Ctrl Pts',(8.12334762198528,0.175815172514029,-2.40981965901413));
#19848=CARTESIAN_POINT('Ctrl Pts',(8.11880542538668,0.385682395064902,-2.40159617955251));
#19849=CARTESIAN_POINT('Ctrl Pts',(8.10612640730235,0.595354139946849,-2.39337270009089));
#19850=CARTESIAN_POINT('Ctrl Pts',(8.08535492570326,0.80419107673868,-2.38514922062928));
#19851=CARTESIAN_POINT('Ctrl Pts',(8.07696247792963,0.88856893283274,-2.38182663039565));
#19852=CARTESIAN_POINT('Ctrl Pts',(8.06724956050654,0.972810555292713,-2.37850404016202));
#19853=CARTESIAN_POINT('Ctrl Pts',(8.05622149971848,1.05687402748562,-2.37518144992839));
#19854=CARTESIAN_POINT('Ctrl Pts',(8.02892662360567,1.26493436585477,-2.36695791085444));
#19855=CARTESIAN_POINT('Ctrl Pts',(7.99356294389417,1.47197055512868,-2.35873437178049));
#19856=CARTESIAN_POINT('Ctrl Pts',(7.95023173849494,1.67734995356596,-2.35051083270654));
#19857=CARTESIAN_POINT('Ctrl Pts',(7.90690841146144,1.88269201046153,-2.34228878881483));
#19858=CARTESIAN_POINT('Ctrl Pts',(7.85562051090432,2.0863775893089,-2.33406674492311));
#19859=CARTESIAN_POINT('Ctrl Pts',(7.79652040726645,2.28778432147304,-2.32584470103139));
#19860=CARTESIAN_POINT('Ctrl Pts',(7.73742682874643,2.48916881674446,-2.31762356491821));
#19861=CARTESIAN_POINT('Ctrl Pts',(7.67052285216363,2.68827468475593,-2.30940242880502));
#19862=CARTESIAN_POINT('Ctrl Pts',(7.5960109250455,2.88449399186225,-2.30118129269183));
#19863=CARTESIAN_POINT('Ctrl Pts',(7.52149308800743,3.08072886211985,-2.29295950451853));
#19864=CARTESIAN_POINT('Ctrl Pts',(7.43936619696353,3.27407643734074,-2.28473771634522));
#19865=CARTESIAN_POINT('Ctrl Pts',(7.34988151140998,3.46394707389327,-2.27651592817192));
#19866=CARTESIAN_POINT('Ctrl Pts',(7.26039707415217,3.65381718360626,-2.26829416281184));
#19867=CARTESIAN_POINT('Ctrl Pts',(7.16355501139801,3.84021010831143,-2.26007239745177));
#19868=CARTESIAN_POINT('Ctrl Pts',(7.05965360308662,4.02255870894709,-2.2518506320917));
#19869=CARTESIAN_POINT('Ctrl Pts',(6.95573053305696,4.20494532623794,-2.24362715263008));
#19870=CARTESIAN_POINT('Ctrl Pts',(6.84474532336131,4.38328567873918,-2.23540367316846));
#19871=CARTESIAN_POINT('Ctrl Pts',(6.72704139961008,4.55703868432473,-2.22718019370684));
#19872=CARTESIAN_POINT('Ctrl Pts',(6.67948465561444,4.62724133298553,-2.22385760347326));
#19873=CARTESIAN_POINT('Ctrl Pts',(6.63083160793803,4.69669543776809,-2.22053501323968));
#19874=CARTESIAN_POINT('Ctrl Pts',(6.58110689903192,4.76536667487555,-2.2172124230061));
#19875=CARTESIAN_POINT('Ctrl Pts',(6.45803632520719,4.93533063729968,-2.20898888393214));
#19876=CARTESIAN_POINT('Ctrl Pts',(6.3283579981927,5.10055201913228,-2.20076534485817));
#19877=CARTESIAN_POINT('Ctrl Pts',(6.19246221203539,5.26052272260217,-2.19254180578421));
#19878=CARTESIAN_POINT('Ctrl Pts',(6.05659113409252,5.42046434061946,-2.18431976189249));
#19879=CARTESIAN_POINT('Ctrl Pts',(5.91450504409466,5.57515696100924,-2.17609771800078));
#19880=CARTESIAN_POINT('Ctrl Pts',(5.76663427338612,5.72412584763023,-2.16787567410906));
#19881=CARTESIAN_POINT('Ctrl Pts',(5.61877982877697,5.87307828691117,-2.15965453799584));
#19882=CARTESIAN_POINT('Ctrl Pts',(5.46514218624349,6.01630804483998,-2.15143340188261));
#19883=CARTESIAN_POINT('Ctrl Pts',(5.30618883978909,6.15337692320223,-2.14321226576939));
#19884=CARTESIAN_POINT('Ctrl Pts',(5.14722288593736,6.29045667319348,-2.13499047759611));
#19885=CARTESIAN_POINT('Ctrl Pts',(4.98294060737273,6.42137437262999,-2.12676868942282));
#19886=CARTESIAN_POINT('Ctrl Pts',(4.81384371268235,6.54573114879985,-2.11854690124953));
#19887=CARTESIAN_POINT('Ctrl Pts',(4.64474728719106,6.6700875799126,-2.11032513588953));
#19888=CARTESIAN_POINT('Ctrl Pts',(4.47083651149325,6.78788295161319,-2.10210337052952));
#19889=CARTESIAN_POINT('Ctrl Pts',(4.29264372658684,6.8987605697759,-2.09388160516952));
#19890=CARTESIAN_POINT('Ctrl Pts',(4.11441379144225,7.00966130408175,-2.0856581257079));
#19891=CARTESIAN_POINT('Ctrl Pts',(3.93190031413309,7.11364124783058,-2.07743464624627));
#19892=CARTESIAN_POINT('Ctrl Pts',(3.74566292799559,7.21038811662309,-2.06921116678465));
#19893=CARTESIAN_POINT('Ctrl Pts',(3.67041612727074,7.24947743433618,-2.06588857655103));
#19894=CARTESIAN_POINT('Ctrl Pts',(3.59456169918358,7.28738650263208,-2.06256598631742));
#19895=CARTESIAN_POINT('Ctrl Pts',(3.51813765675159,7.32409687201408,-2.05924339608381));
#19896=CARTESIAN_POINT('Ctrl Pts',(3.32898520190726,7.41495645318615,-2.05101985700985));
#19897=CARTESIAN_POINT('Ctrl Pts',(3.13628032799971,7.4984992870151,-2.0427963179359));
#19898=CARTESIAN_POINT('Ctrl Pts',(2.94060817712988,7.574464410841,-2.03457277886194));
#19899=CARTESIAN_POINT('Ctrl Pts',(2.74497160285539,7.65041572288807,-2.0263507349702));
#19900=CARTESIAN_POINT('Ctrl Pts',(2.54636910320972,7.71879196809515,-2.01812869107846));
#19901=CARTESIAN_POINT('Ctrl Pts',(2.34540514236945,7.77938058463827,-2.00990664718673));
#19902=CARTESIAN_POINT('Ctrl Pts',(2.14446336953325,7.83996251172094,-2.0016855110734));
#19903=CARTESIAN_POINT('Ctrl Pts',(1.94116093829837,7.89275844162801,-1.99346437496007));
#19904=CARTESIAN_POINT('Ctrl Pts',(1.73611759466528,7.93760563772185,-1.98524323884674));
#19905=CARTESIAN_POINT('Ctrl Pts',(1.53105798800579,7.98245639087401,-1.97702145067345));
#19906=CARTESIAN_POINT('Ctrl Pts',(1.32425748061597,8.01935708489814,-1.96879966250016));
#19907=CARTESIAN_POINT('Ctrl Pts',(1.11634718058141,8.04819585589888,-1.96057787432687));
#19908=CARTESIAN_POINT('Ctrl Pts',(0.908437457442484,8.07703454687973,-1.95235610896685));
#19909=CARTESIAN_POINT('Ctrl Pts',(0.699418240324269,8.09781132173404,-1.94413434360683));
#19910=CARTESIAN_POINT('Ctrl Pts',(0.48992749086497,8.11046599254289,-1.93591257824681));
#19911=CARTESIAN_POINT('Ctrl Pts',(0.280393066061586,8.12312330164056,-1.92768909878518));
#19912=CARTESIAN_POINT('Ctrl Pts',(0.0703872069775901,8.12765510613058,
-1.91946561932356));
#19913=CARTESIAN_POINT('Ctrl Pts',(-0.139449270694467,8.1240532656675,-1.91124213986193));
#19914=CARTESIAN_POINT('Ctrl Pts',(-0.224230978314887,8.12259798873747,
-1.90791954962846));
#19915=CARTESIAN_POINT('Ctrl Pts',(-0.308985031865068,8.11981552118424,
-1.90459695939499));
#19916=CARTESIAN_POINT('Ctrl Pts',(-0.393669219340797,8.11570773920818,
-1.90127436916152));
#19917=CARTESIAN_POINT('Ctrl Pts',(-0.603265852003794,8.10554082026428,
-1.89305083008756));
#19918=CARTESIAN_POINT('Ctrl Pts',(-0.812502460733349,8.08724833330016,
-1.88482729101359));
#19919=CARTESIAN_POINT('Ctrl Pts',(-1.02074023536371,8.06087941445656,-1.87660375193962));
#19920=CARTESIAN_POINT('Ctrl Pts',(-1.22894014874827,8.03451528994061,-1.86838170804795));
#19921=CARTESIAN_POINT('Ctrl Pts',(-1.43614129804398,8.00007770140785,-1.86015966415628));
#19922=CARTESIAN_POINT('Ctrl Pts',(-1.64171092815941,7.95766754714357,-1.85193762026462));
#19923=CARTESIAN_POINT('Ctrl Pts',(-1.84725786176637,7.91526207529481,-1.84371648415144));
#19924=CARTESIAN_POINT('Ctrl Pts',(-2.05117334708184,7.86488585463802,-1.83549534803826));
#19925=CARTESIAN_POINT('Ctrl Pts',(-2.25283491514321,7.80669087434693,-1.82727421192509));
#19926=CARTESIAN_POINT('Ctrl Pts',(-2.45451247800942,7.74849127831592,-1.81905242375178));
#19927=CARTESIAN_POINT('Ctrl Pts',(-2.65393548230901,7.68247176277367,-1.81083063557848));
#19928=CARTESIAN_POINT('Ctrl Pts',(-2.8504956908767,7.60883446257003,-1.80260884740517));
#19929=CARTESIAN_POINT('Ctrl Pts',(-3.0470553540411,7.53519736669069,-1.79438708204519));
#19930=CARTESIAN_POINT('Ctrl Pts',(-3.24075196212233,7.45394263442523,-1.7861653166852));
#19931=CARTESIAN_POINT('Ctrl Pts',(-3.43099585684955,7.36532110588406,-1.77794355132522));
#19932=CARTESIAN_POINT('Ctrl Pts',(-3.62127941427141,7.27668110122501,-1.76972007186361));
#19933=CARTESIAN_POINT('Ctrl Pts',(-3.80810855292187,7.18067135665459,-1.76149659240199));
#19934=CARTESIAN_POINT('Ctrl Pts',(-3.99091588737073,7.0775898399407,-1.75327311294038));
#19935=CARTESIAN_POINT('Ctrl Pts',(-4.06477682019452,7.03594108988189,-1.74995052270666));
#19936=CARTESIAN_POINT('Ctrl Pts',(-4.13798148974316,6.99313842552292,-1.74662793247295));
#19937=CARTESIAN_POINT('Ctrl Pts',(-4.2104936697147,6.94920359608152,-1.74330534223923));
#19938=CARTESIAN_POINT('Ctrl Pts',(-4.38996411397347,6.84046319741505,-1.73508180316526));
#19939=CARTESIAN_POINT('Ctrl Pts',(-4.56524895597131,6.72474890409797,-1.72685826409128));
#19940=CARTESIAN_POINT('Ctrl Pts',(-4.73580984621355,6.60240809576376,-1.7186347250173));
#19941=CARTESIAN_POINT('Ctrl Pts',(-4.90633972552256,6.48008953111408,-1.71041268112561));
#19942=CARTESIAN_POINT('Ctrl Pts',(-5.07214712779607,6.3511470279392,-1.70219063723391));
#19943=CARTESIAN_POINT('Ctrl Pts',(-5.23272367482728,6.21597060042935,-1.69396859334222));
#19944=CARTESIAN_POINT('Ctrl Pts',(-5.39328249294177,6.0808090974628,-1.68574745722899));
#19945=CARTESIAN_POINT('Ctrl Pts',(-5.54861138328381,5.93941523414199,-1.67752632111576));
#19946=CARTESIAN_POINT('Ctrl Pts',(-5.69823533994547,5.79221905430868,-1.66930518500253));
#19947=CARTESIAN_POINT('Ctrl Pts',(-5.84787116404307,5.64501119959874,-1.66108339682924));
#19948=CARTESIAN_POINT('Ctrl Pts',(-5.99180093823563,5.49200031378658,-1.65286160865596));
#19949=CARTESIAN_POINT('Ctrl Pts',(-6.1295860485223,5.33365376044046,-1.64463982048267));
#19950=CARTESIAN_POINT('Ctrl Pts',(-6.26737077649119,5.17530764646479,-1.6364180551227));
#19951=CARTESIAN_POINT('Ctrl Pts',(-6.39901068309201,5.01162611883369,-1.62819628976273));
#19952=CARTESIAN_POINT('Ctrl Pts',(-6.52410668304801,4.84311052431268,-1.61997452440276));
#19953=CARTESIAN_POINT('Ctrl Pts',(-6.64922876344443,4.6745597970862,-1.61175104494113));
#19954=CARTESIAN_POINT('Ctrl Pts',(-6.76780403589574,4.50117322648551,-1.6035275654795));
#19955=CARTESIAN_POINT('Ctrl Pts',(-6.87947544098783,4.32348299630579,-1.59530408601787));
#19956=CARTESIAN_POINT('Ctrl Pts',(-6.92459482405033,4.25168956310478,-1.59198149578423));
#19957=CARTESIAN_POINT('Ctrl Pts',(-6.96858767436257,4.17919390226202,-1.58865890555058));
#19958=CARTESIAN_POINT('Ctrl Pts',(-7.0114324918152,4.1060323884765,-1.58533631531694));
#19959=CARTESIAN_POINT('Ctrl Pts',(-7.11747506873956,3.92495481796101,-1.57711277624297));
#19960=CARTESIAN_POINT('Ctrl Pts',(-7.21651634503643,3.73973765055601,-1.56888923716899));
#19961=CARTESIAN_POINT('Ctrl Pts',(-7.30824832199898,3.55094269546822,-1.56066569809502));
#19962=CARTESIAN_POINT('Ctrl Pts',(-7.39996362049496,3.36218206658217,-1.55244365420328));
#19963=CARTESIAN_POINT('Ctrl Pts',(-7.48437214327375,3.16984521349217,-1.54422161031153));
#19964=CARTESIAN_POINT('Ctrl Pts',(-7.56121254781631,2.97451716573382,-1.53599956641978));
#19965=CARTESIAN_POINT('Ctrl Pts',(-7.63804446857178,2.77921068373347,-1.52777843030657));
#19966=CARTESIAN_POINT('Ctrl Pts',(-7.70730983136704,2.58091394075382,-1.51955729419336));
#19967=CARTESIAN_POINT('Ctrl Pts',(-7.76879570026032,2.38023127660249,-1.51133615808014));
#19968=CARTESIAN_POINT('Ctrl Pts',(-7.83028644591053,2.17953269528856,-1.50311436990682));
#19969=CARTESIAN_POINT('Ctrl Pts',(-7.88399637583863,1.97644809591272,-1.49489258173349));
#19970=CARTESIAN_POINT('Ctrl Pts',(-7.92976232567285,1.77159730775352,-1.48667079356017));
#19971=CARTESIAN_POINT('Ctrl Pts',(-7.97552814851867,1.56674708800103,-1.47844902820013));
#19972=CARTESIAN_POINT('Ctrl Pts',(-8.01334997368914,1.36013097769249,-1.4702272628401));
#19973=CARTESIAN_POINT('Ctrl Pts',(-8.043115578085,1.15237986795429,-1.46200549748006));
#19974=CARTESIAN_POINT('Ctrl Pts',(-8.0728873881153,0.944585445558167,-1.45378201801842));
#19975=CARTESIAN_POINT('Ctrl Pts',(-8.09459958019832,0.735655843020287,
-1.44555853855677));
#19976=CARTESIAN_POINT('Ctrl Pts',(-8.10819157034168,0.526229057673656,
-1.43733505909513));
#19977=CARTESIAN_POINT('Ctrl Pts',(-8.11368323769669,0.441612880923745,
-1.43401246886163));
#19978=CARTESIAN_POINT('Ctrl Pts',(-8.11784990668612,0.356915592959289,
-1.43068987862813));
#19979=CARTESIAN_POINT('Ctrl Pts',(-8.12068999082585,0.272179417665621,
-1.42736728839464));
#19980=CARTESIAN_POINT('Ctrl Pts',(-8.12372865774564,0.181518366758098,
-1.42381237785896));
#19981=CARTESIAN_POINT('Ctrl Pts',(-8.125248987835,0.0908062923927736,-1.42025746732329));
#19982=CARTESIAN_POINT('Ctrl Pts',(-8.12524999949474,9.06126520568907E-5,
-1.41670255678761));
#19983=CARTESIAN_POINT('Ctrl Pts',(-8.12584796001076,9.03551486182587E-5,
-1.41670254643617));
#19984=CARTESIAN_POINT('Ctrl Pts',(-8.12513209299635,-1.25299245336929,
-1.3676011181149));
#19985=CARTESIAN_POINT('Ctrl Pts',(-7.51481976840467,-3.850553756064,-1.2658433474862));
#19986=CARTESIAN_POINT('Ctrl Pts',(-4.8622676215541,-6.9309500637499,-1.11142923455007));
#19987=CARTESIAN_POINT('Ctrl Pts',(-0.975506354015658,-8.41000015238307,
-0.953460207627781));
#19988=CARTESIAN_POINT('Ctrl Pts',(2.5305352297047,-7.94214230500563,-0.819100913414416));
#19989=CARTESIAN_POINT('Ctrl Pts',(4.35790031294788,-6.89669607699888,-0.737397961508479));
#19990=CARTESIAN_POINT('Ctrl Pts',(4.94635340024336,-6.44536135766213,-0.708351351909972));
#19991=CARTESIAN_POINT('',(-8.12528566984828,-7.93977388155583E-5,-1.58329744376396));
#19992=CARTESIAN_POINT('Ctrl Pts',(-8.12524999961194,-7.94114662834033E-5,
-1.58329744321239));
#19993=CARTESIAN_POINT('Ctrl Pts',(-8.12524923036167,-0.078787827428694,
-1.58021303651788));
#19994=CARTESIAN_POINT('Ctrl Pts',(-8.12410474332392,-0.157493831703078,
-1.57712862982337));
#19995=CARTESIAN_POINT('Ctrl Pts',(-8.12181709581716,-0.236166518778639,
-1.57404422312885));
#19996=CARTESIAN_POINT('Ctrl Pts',(-8.11571784869364,-0.445920931959764,
-1.56582068405489));
#19997=CARTESIAN_POINT('Ctrl Pts',(-8.10148757870039,-0.655473008847223,
-1.55759714498093));
#19998=CARTESIAN_POINT('Ctrl Pts',(-8.07916302108297,-0.86418310632966,
-1.54937360590697));
#19999=CARTESIAN_POINT('Ctrl Pts',(-8.056842522458,-1.07285525669011,-1.54115156201529));
#20000=CARTESIAN_POINT('Ctrl Pts',(-8.02643070487113,-1.28068544007206,
-1.53292951812361));
#20001=CARTESIAN_POINT('Ctrl Pts',(-7.98801617342936,-1.48703906321621,
-1.52470747423194));
#20002=CARTESIAN_POINT('Ctrl Pts',(-7.94960588325472,-1.6933699032935,-1.51648633811873));
#20003=CARTESIAN_POINT('Ctrl Pts',(-7.90319469718185,-1.89822421876373,
-1.50826520200552));
#20004=CARTESIAN_POINT('Ctrl Pts',(-7.84892250112346,-2.10097670949914,
-1.50004406589231));
#20005=CARTESIAN_POINT('Ctrl Pts',(-7.79464600046137,-2.30374528156509,
-1.49182227771901));
#20006=CARTESIAN_POINT('Ctrl Pts',(-7.73250731771493,-2.5044114102037,-1.4836004895457));
#20007=CARTESIAN_POINT('Ctrl Pts',(-7.66269675110625,-2.70236305168009,
-1.4753787013724));
#20008=CARTESIAN_POINT('Ctrl Pts',(-7.59288637820341,-2.90031414389308,
-1.46715693601239));
#20009=CARTESIAN_POINT('Ctrl Pts',(-7.51540426465473,-3.09555048676511,
-1.45893517065238));
#20010=CARTESIAN_POINT('Ctrl Pts',(-7.43048976517222,-3.28747766717448,
-1.45071340529236));
#20011=CARTESIAN_POINT('Ctrl Pts',(-7.34555756242592,-3.47944486121545,
-1.44248992583073));
#20012=CARTESIAN_POINT('Ctrl Pts',(-7.25318999758232,-3.66810124479795,
-1.4342664463691));
#20013=CARTESIAN_POINT('Ctrl Pts',(-7.15367397619229,-3.85287375926712,
-1.42604296690747));
#20014=CARTESIAN_POINT('Ctrl Pts',(-7.1134658182826,-3.92752869759137,-1.42272037667384));
#20015=CARTESIAN_POINT('Ctrl Pts',(-7.07209123298693,-4.00154987977049,
-1.4193977864402));
#20016=CARTESIAN_POINT('Ctrl Pts',(-7.02957126271235,-4.07490066442714,
-1.41607519620657));
#20017=CARTESIAN_POINT('Ctrl Pts',(-6.92433269509206,-4.25644668765432,
-1.40785165713262));
#20018=CARTESIAN_POINT('Ctrl Pts',(-6.81204035264438,-4.43394317589982,
-1.39962811805866));
#20019=CARTESIAN_POINT('Ctrl Pts',(-6.69303110672799,-4.60684514248867,
-1.3914045789847));
#20020=CARTESIAN_POINT('Ctrl Pts',(-6.5740434987594,-4.77971567249713,-1.38318253509297));
#20021=CARTESIAN_POINT('Ctrl Pts',(-6.44834159193582,-4.94799310531268,
-1.37496049120124));
#20022=CARTESIAN_POINT('Ctrl Pts',(-6.31630546553415,-5.11116159288311,
-1.36673844730951));
#20023=CARTESIAN_POINT('Ctrl Pts',(-6.18428391696299,-5.27431206536463,
-1.35851731119632));
#20024=CARTESIAN_POINT('Ctrl Pts',(-6.04592973049139,-5.43235448955832,
-1.35029617508313));
#20025=CARTESIAN_POINT('Ctrl Pts',(-5.90166365487219,-5.58480560693572,
-1.34207503896994));
#20026=CARTESIAN_POINT('Ctrl Pts',(-5.75738613677688,-5.7372688159865,-1.33385325079664));
#20027=CARTESIAN_POINT('Ctrl Pts',(-5.60719599342608,-5.88413961606792,
-1.32563146262334));
#20028=CARTESIAN_POINT('Ctrl Pts',(-5.45155199220795,-6.0249704097824,-1.31740967445004));
#20029=CARTESIAN_POINT('Ctrl Pts',(-5.29590842286007,-6.1658008127293,-1.30918790908999));
#20030=CARTESIAN_POINT('Ctrl Pts',(-5.13481124642108,-6.30059104695188,
-1.30096614372994));
#20031=CARTESIAN_POINT('Ctrl Pts',(-4.96875397386089,-6.42893237713243,
-1.29274437836989));
#20032=CARTESIAN_POINT('Ctrl Pts',(-4.80266208111646,-6.55730046434943,
-1.28452089890827));
#20033=CARTESIAN_POINT('Ctrl Pts',(-4.63160825982146,-6.67921678123042,
-1.27629741944665));
#20034=CARTESIAN_POINT('Ctrl Pts',(-4.45611766739158,-6.79431401223557,
-1.26807393998502));
#20035=CARTESIAN_POINT('Ctrl Pts',(-4.38521296929947,-6.84081755583104,
-1.26475134975144));
#20036=CARTESIAN_POINT('Ctrl Pts',(-4.31358432319599,-6.88620840046679,
-1.26142875951786));
#20037=CARTESIAN_POINT('Ctrl Pts',(-4.24126767987644,-6.93046434448194,
-1.25810616928428));
#20038=CARTESIAN_POINT('Ctrl Pts',(-4.06228119637158,-7.03999951411719,
-1.24988263021032));
#20039=CARTESIAN_POINT('Ctrl Pts',(-3.87902008353936,-7.14261500045062,
-1.24165909113635));
#20040=CARTESIAN_POINT('Ctrl Pts',(-3.6920400703131,-7.23799196474426,-1.23343555206239));
#20041=CARTESIAN_POINT('Ctrl Pts',(-3.50509405330119,-7.33335158784903,
-1.22521350817067));
#20042=CARTESIAN_POINT('Ctrl Pts',(-3.3144307480331,-7.42147518172794,-1.21699146427896));
#20043=CARTESIAN_POINT('Ctrl Pts',(-3.12063000443933,-7.50209010462371,
-1.20876942038725));
#20044=CARTESIAN_POINT('Ctrl Pts',(-2.92685065797582,-7.58269612699632,
-1.20054828427402));
#20045=CARTESIAN_POINT('Ctrl Pts',(-2.72993483696624,-7.6557950202564,-1.19232714816078));
#20046=CARTESIAN_POINT('Ctrl Pts',(-2.5304826369713,-7.72116216553485,-1.18410601204754));
#20047=CARTESIAN_POINT('Ctrl Pts',(-2.33101461740929,-7.7865344954136,-1.17588422387424));
#20048=CARTESIAN_POINT('Ctrl Pts',(-2.12901009634928,-7.84417375761885,
-1.16766243570095));
#20049=CARTESIAN_POINT('Ctrl Pts',(-1.92508562137813,-7.89390479502148,
-1.15944064752765));
#20050=CARTESIAN_POINT('Ctrl Pts',(-1.72116171224275,-7.94363569443381,
-1.15121888216761));
#20051=CARTESIAN_POINT('Ctrl Pts',(-1.51531814702637,-7.98545834568029,
-1.14299711680757));
#20052=CARTESIAN_POINT('Ctrl Pts',(-1.30818352124196,-8.01924830874135,
-1.13477535144753));
#20053=CARTESIAN_POINT('Ctrl Pts',(-1.10100571132674,-8.05304531644875,
-1.12655187198591));
#20054=CARTESIAN_POINT('Ctrl Pts',(-0.892536594266989,-8.07880624294275,
-1.11832839252428));
#20055=CARTESIAN_POINT('Ctrl Pts',(-0.683412872141368,-8.09645813974799,
-1.11010491306265));
#20056=CARTESIAN_POINT('Ctrl Pts',(-0.598919144154128,-8.10359015974056,
-1.1067823228291));
#20057=CARTESIAN_POINT('Ctrl Pts',(-0.514318617874732,-8.10939900407478,
-1.10345973259555));
#20058=CARTESIAN_POINT('Ctrl Pts',(-0.42965347846909,-8.11388226750545,
-1.10013714236199));
#20059=CARTESIAN_POINT('Ctrl Pts',(-0.220103990520467,-8.12497851754215,
-1.09191360328803));
#20060=CARTESIAN_POINT('Ctrl Pts',(-0.0100903786848266,-8.12795448052103,
-1.08369006421408));
#20061=CARTESIAN_POINT('Ctrl Pts',(0.199746853865668,-8.12279439336432,
-1.07546652514012));
#20062=CARTESIAN_POINT('Ctrl Pts',(0.409545934362378,-8.11763524440108,
-1.0672444812484));
#20063=CARTESIAN_POINT('Ctrl Pts',(0.61916840488007,-8.10434300501338,-1.05902243735669));
#20064=CARTESIAN_POINT('Ctrl Pts',(0.827974547956963,-8.08295402129911,
-1.05080039346498));
#20065=CARTESIAN_POINT('Ctrl Pts',(1.03675763718865,-8.06156739909736,-1.04257925735176));
#20066=CARTESIAN_POINT('Ctrl Pts',(1.24472428563353,-8.03208584733869,-1.03435812123855));
#20067=CARTESIAN_POINT('Ctrl Pts',(1.45123983880385,-7.99459758166529,-1.02613698512534));
#20068=CARTESIAN_POINT('Ctrl Pts',(1.65777177177236,-7.957106342607,-1.01791519695204));
#20069=CARTESIAN_POINT('Ctrl Pts',(1.86285208882459,-7.91160717081146,-1.00969340877873));
#20070=CARTESIAN_POINT('Ctrl Pts',(2.06585521951359,-7.85823961040311,-1.00147162060542));
#20071=CARTESIAN_POINT('Ctrl Pts',(2.268857786923,-7.80487219807552,-0.99324985524539));
#20072=CARTESIAN_POINT('Ctrl Pts',(2.46978289494403,-7.74363651840299,-0.985028089885358));
#20073=CARTESIAN_POINT('Ctrl Pts',(2.66801852771913,-7.67472245089342,-0.976806324525324));
#20074=CARTESIAN_POINT('Ctrl Pts',(2.86629548933278,-7.6057940159448,-0.968582845063701));
#20075=CARTESIAN_POINT('Ctrl Pts',(3.06188157693146,-7.52918409204903,-0.960359365602076));
#20076=CARTESIAN_POINT('Ctrl Pts',(3.25418216388124,-7.44513169841724,-0.952135886140454));
#20077=CARTESIAN_POINT('Ctrl Pts',(3.33187872226552,-7.41117141876996,-0.948813295906869));
#20078=CARTESIAN_POINT('Ctrl Pts',(3.40903916149606,-7.3759967355855,-0.945490705673285));
#20079=CARTESIAN_POINT('Ctrl Pts',(3.48562524024988,-7.33962562035918,-0.942168115439701));
#20080=CARTESIAN_POINT('Ctrl Pts',(3.67517718563534,-7.24960644508391,-0.93394464385397));
#20081=CARTESIAN_POINT('Ctrl Pts',(3.8612708249081,-7.15222571977221,-0.92572117226824));
#20082=CARTESIAN_POINT('Ctrl Pts',(4.04333543182722,-7.04777455288055,-0.91749770068251));
#20083=CARTESIAN_POINT('Ctrl Pts',(4.22537413651904,-6.94333824619654,-0.90927539904537));
#20084=CARTESIAN_POINT('Ctrl Pts',(4.4033846964227,-6.83183365095716,-0.901053097408225));
#20085=CARTESIAN_POINT('Ctrl Pts',(4.57682182311896,-6.71359736370316,-0.892830795771085));
#20086=CARTESIAN_POINT('Ctrl Pts',(4.70260229937768,-6.62784976856503,-0.886867799061196));
#20087=CARTESIAN_POINT('Ctrl Pts',(4.82597790270025,-6.53856261631617,-0.880904802351308));
#20088=CARTESIAN_POINT('Ctrl Pts',(4.94675008185375,-6.44587862049697,-0.874941805641418));
#20089=CARTESIAN_POINT('Ctrl Pts',(4.94673849251696,-6.44586330438811,-2.8749518510811));
#20090=CARTESIAN_POINT('Ctrl Pts',(5.19773710945893,-6.25365150213958,-2.86256671355646));
#20091=CARTESIAN_POINT('Ctrl Pts',(6.4568287000089,-5.16760485441946,-2.79752523372439));
#20092=CARTESIAN_POINT('Ctrl Pts',(8.08005480686637,-2.52832543946459,-2.67982741158489));
#20093=CARTESIAN_POINT('Ctrl Pts',(8.30916720919218,1.62402447626065,-2.5218583846626));
#20094=CARTESIAN_POINT('Ctrl Pts',(6.5334877241783,5.38453836162577,-2.36388935774031));
#20095=CARTESIAN_POINT('Ctrl Pts',(3.18144290005129,7.84589932917326,-2.20592033081802));
#20096=CARTESIAN_POINT('Ctrl Pts',(-0.938203628973559,8.41424323159183,
-2.04795130389573));
#20097=CARTESIAN_POINT('Ctrl Pts',(-4.83148535191313,6.95244306010894,-1.88998227697344));
#20098=CARTESIAN_POINT('Ctrl Pts',(-7.50579500816724,3.87448934127983,-1.73509765993017));
#20099=CARTESIAN_POINT('Ctrl Pts',(-8.12522203952541,1.26500204491867,-1.63286938519434));
#20100=CARTESIAN_POINT('Ctrl Pts',(-8.1258678326399,-7.91736970983551E-5,
-1.58329745276593));
#20101=CARTESIAN_POINT('Origin',(0.,0.,-16.4167025567876));
#20102=CARTESIAN_POINT('',(4.94675008185375,-6.44587862049697,-4.87493975109638));
#20103=CARTESIAN_POINT('',(4.94675083769988,-6.44587978308508,-4.70834087481909));
#20104=CARTESIAN_POINT('',(4.94675008185374,-6.44587862049697,-16.4167025567876));
#20105=CARTESIAN_POINT('',(-8.12522972379081,0.000108848713032344,-3.41670255712189));
#20106=CARTESIAN_POINT('Ctrl Pts',(4.94675083769988,-6.44587978308508,-4.70834087481909));
#20107=CARTESIAN_POINT('Ctrl Pts',(5.76684755869603,-5.81516257124187,-4.66780985882621));
#20108=CARTESIAN_POINT('Ctrl Pts',(7.3768399998997,-4.00454199459098,-4.5746225005259));
#20109=CARTESIAN_POINT('Ctrl Pts',(8.46029510168218,-0.321126146958935,
-4.42877879991817));
#20110=CARTESIAN_POINT('Ctrl Pts',(7.59257255154836,3.74600550710789,-4.27080977299587));
#20111=CARTESIAN_POINT('Ctrl Pts',(4.89295428043989,6.9093207784364,-4.11284074607359));
#20112=CARTESIAN_POINT('Ctrl Pts',(1.01278989687648,8.4055917004452,-3.95487171915129));
#20113=CARTESIAN_POINT('Ctrl Pts',(-3.11173507273836,7.87380594419866,-3.79690269222901));
#20114=CARTESIAN_POINT('Ctrl Pts',(-6.48547707309547,5.44226996244777,-3.63893366530671));
#20115=CARTESIAN_POINT('Ctrl Pts',(-7.93674675436804,2.43808555436179,-3.51220029005247));
#20116=CARTESIAN_POINT('Ctrl Pts',(-8.12492425771545,0.547001067506262,
-3.43812325710566));
#20117=CARTESIAN_POINT('Ctrl Pts',(-8.12466295576038,0.000109079692641577,
-3.41670256646628));
#20118=CARTESIAN_POINT('Ctrl Pts',(-8.12524999927102,0.000108840450000125,
-3.41670255678761));
#20119=CARTESIAN_POINT('Ctrl Pts',(-8.12525282338782,-0.210719532315853,
-3.40844541790656));
#20120=CARTESIAN_POINT('Ctrl Pts',(-8.11704565989559,-0.42154584143425,
-3.4001882790255));
#20121=CARTESIAN_POINT('Ctrl Pts',(-8.10065504422437,-0.631724162101,-3.39193114014445));
#20122=CARTESIAN_POINT('Ctrl Pts',(-8.08426436384872,-0.841903312478525,
-3.3836739686671));
#20123=CARTESIAN_POINT('Ctrl Pts',(-8.05969019230419,-1.05143418077564,
-3.37541679718974));
#20124=CARTESIAN_POINT('Ctrl Pts',(-8.02701101511336,-1.25967524614433,
-3.36715962571238));
#20125=CARTESIAN_POINT('Ctrl Pts',(-7.99432344888107,-1.46796976888498,
-3.35890033454415));
#20126=CARTESIAN_POINT('Ctrl Pts',(-7.95352676351121,-1.67497354070713,
-3.35064104337591));
#20127=CARTESIAN_POINT('Ctrl Pts',(-7.90475092986181,-1.8800532703487,-3.34238175220767));
#20128=CARTESIAN_POINT('Ctrl Pts',(-7.86658885045947,-2.04050709226893,
-3.33591970529249));
#20129=CARTESIAN_POINT('Ctrl Pts',(-7.82354340356189,-2.19978325012226,
-3.32945765837732));
#20130=CARTESIAN_POINT('Ctrl Pts',(-7.77569842141607,-2.35758385252523,
-3.32299561146214));
#20131=CARTESIAN_POINT('Ctrl Pts',(-7.71481135492858,-2.55839938927245,
-3.31477207238817));
#20132=CARTESIAN_POINT('Ctrl Pts',(-7.64613083549557,-2.75688757472043,
-3.3065485333142));
#20133=CARTESIAN_POINT('Ctrl Pts',(-7.56986003845332,-2.95244078022363,
-3.29832499424023));
#20134=CARTESIAN_POINT('Ctrl Pts',(-7.49360310876675,-3.14795843075743,
-3.2901029503485));
#20135=CARTESIAN_POINT('Ctrl Pts',(-7.40975876299778,-3.34054189177276,
-3.28188090645677));
#20136=CARTESIAN_POINT('Ctrl Pts',(-7.31857890719936,-3.52960200895179,
-3.27365886256504));
#20137=CARTESIAN_POINT('Ctrl Pts',(-7.22740911837657,-3.71864125240194,
-3.26543772645184));
#20138=CARTESIAN_POINT('Ctrl Pts',(-7.12890556452571,-3.90415766309951,
-3.25721659033864));
#20139=CARTESIAN_POINT('Ctrl Pts',(-7.02336720131108,-4.08558450139607,
-3.24899545422544));
#20140=CARTESIAN_POINT('Ctrl Pts',(-6.91782046731242,-4.26702572957735,
-3.24077366605215));
#20141=CARTESIAN_POINT('Ctrl Pts',(-6.80523795509613,-4.44437648096923,
-3.23255187787885));
#20142=CARTESIAN_POINT('Ctrl Pts',(-6.68596379259542,-4.61709602744009,
-3.22433008970556));
#20143=CARTESIAN_POINT('Ctrl Pts',(-6.56668996104819,-4.78981509466101,
-3.2161083243455));
#20144=CARTESIAN_POINT('Ctrl Pts',(-6.44072468616938,-4.95790274150987,
-3.20788655898544));
#20145=CARTESIAN_POINT('Ctrl Pts',(-6.30845481278701,-5.12084811701386,
-3.19966479362538));
#20146=CARTESIAN_POINT('Ctrl Pts',(-6.17615736333197,-5.28382746392345,
-3.19144131416374));
#20147=CARTESIAN_POINT('Ctrl Pts',(-6.03755287548238,-5.44166216875608,
-3.1832178347021));
#20148=CARTESIAN_POINT('Ctrl Pts',(-5.89306848153566,-5.59387445644171,
-3.17499435524046));
#20149=CARTESIAN_POINT('Ctrl Pts',(-5.8346914358501,-5.65537385737634,-3.17167176500692));
#20150=CARTESIAN_POINT('Ctrl Pts',(-5.77535495924955,-5.71595582056519,
-3.16834917477338));
#20151=CARTESIAN_POINT('Ctrl Pts',(-5.71508896584658,-5.77559050443837,
-3.16502658453984));
#20152=CARTESIAN_POINT('Ctrl Pts',(-5.56592830601656,-5.92318864881475,
-3.1568030454659));
#20153=CARTESIAN_POINT('Ctrl Pts',(-5.41102254924536,-6.06502933420128,
-3.14857950639195));
#20154=CARTESIAN_POINT('Ctrl Pts',(-5.25083968431792,-6.20067497713693,
-3.140355967318));
#20155=CARTESIAN_POINT('Ctrl Pts',(-5.09068594341744,-6.33629595733875,
-3.13213392342629));
#20156=CARTESIAN_POINT('Ctrl Pts',(-4.92525723431693,-6.46572395268463,
-3.12391187953457));
#20157=CARTESIAN_POINT('Ctrl Pts',(-4.75505560117337,-6.58856082860663,
-3.11568983564286));
#20158=CARTESIAN_POINT('Ctrl Pts',(-4.58487275963417,-6.71138414236751,
-3.10746869952971));
#20159=CARTESIAN_POINT('Ctrl Pts',(-4.40991828518714,-6.82761761701956,
-3.09924756341657));
#20160=CARTESIAN_POINT('Ctrl Pts',(-4.23072492285598,-6.93690523141446,
-3.09102642730343));
#20161=CARTESIAN_POINT('Ctrl Pts',(-4.05151734778677,-7.04620151396657,
-3.08280463913012));
#20162=CARTESIAN_POINT('Ctrl Pts',(-3.86807046348638,-7.14855067965373,
-3.07458285095681));
#20163=CARTESIAN_POINT('Ctrl Pts',(-3.68094435233206,-7.243641089779,-3.0663610627835));
#20164=CARTESIAN_POINT('Ctrl Pts',(-3.4938187604034,-7.33873123605344,-3.05813929742349));
#20165=CARTESIAN_POINT('Ctrl Pts',(-3.30301422619502,-7.42656253584763,
-3.04991753206347));
#20166=CARTESIAN_POINT('Ctrl Pts',(-3.10911416963784,-7.50686996308429,
-3.04169576670346));
#20167=CARTESIAN_POINT('Ctrl Pts',(-2.91517368813687,-7.58719413308674,
-3.03347228724182));
#20168=CARTESIAN_POINT('Ctrl Pts',(-2.71813666756841,-7.6599911840378,-3.02524880778018));
#20169=CARTESIAN_POINT('Ctrl Pts',(-2.51860620598059,-7.72504435855847,
-3.01702532831853));
#20170=CARTESIAN_POINT('Ctrl Pts',(-2.43798851050486,-7.75132825010818,
-3.01370273808487));
#20171=CARTESIAN_POINT('Ctrl Pts',(-2.35696396772518,-7.77634854561106,
-3.01038014785121));
#20172=CARTESIAN_POINT('Ctrl Pts',(-2.27557309213706,-7.80009324718889,
-3.00705755761755));
#20173=CARTESIAN_POINT('Ctrl Pts',(-2.07412753352353,-7.85886230009434,
-2.99883401854358));
#20174=CARTESIAN_POINT('Ctrl Pts',(-1.87037138055673,-7.90983291555254,
-2.99061047946961));
#20175=CARTESIAN_POINT('Ctrl Pts',(-1.66492452161307,-7.95284313310853,
-2.98238694039564));
#20176=CARTESIAN_POINT('Ctrl Pts',(-1.45951501647798,-7.99584553065967,
-2.97416489650396));
#20177=CARTESIAN_POINT('Ctrl Pts',(-1.25241570743435,-8.03089035862664,
-2.96594285261227));
#20178=CARTESIAN_POINT('Ctrl Pts',(-1.04425764618611,-8.05786656199281,
-2.95772080872059));
#20179=CARTESIAN_POINT('Ctrl Pts',(-0.836122567227863,-8.08483978697359,
-2.94949967260733));
#20180=CARTESIAN_POINT('Ctrl Pts',(-0.626929261815653,-8.10374612799193,
-2.94127853649407));
#20181=CARTESIAN_POINT('Ctrl Pts',(-0.417315726432918,-8.11452618129806,
-2.93305740038081));
#20182=CARTESIAN_POINT('Ctrl Pts',(-0.207685565536802,-8.12530708962494,
-2.92483561220752));
#20183=CARTESIAN_POINT('Ctrl Pts',(0.00236459750956827,-8.1279604046004,
-2.91661382403423));
#20184=CARTESIAN_POINT('Ctrl Pts',(0.212193859596608,-8.12247876749761,
-2.90839203586094));
#20185=CARTESIAN_POINT('Ctrl Pts',(0.42202253946395,-8.11699714560488,-2.9001702705009));
#20186=CARTESIAN_POINT('Ctrl Pts',(0.631630024836994,-8.10338062718437,
-2.89194850514086));
#20187=CARTESIAN_POINT('Ctrl Pts',(0.840377085155128,-8.08167395514359,
-2.88372673978081));
#20188=CARTESIAN_POINT('Ctrl Pts',(1.04916766576987,-8.05996275762204,-2.87550326031919));
#20189=CARTESIAN_POINT('Ctrl Pts',(1.25709716956753,-8.03015806752157,-2.86727978085756));
#20190=CARTESIAN_POINT('Ctrl Pts',(1.46353204505432,-7.99235644322744,-2.85905630139593));
#20191=CARTESIAN_POINT('Ctrl Pts',(1.54693937942639,-7.97708318714668,-2.85573371116237));
#20192=CARTESIAN_POINT('Ctrl Pts',(1.63010281552708,-7.96050505048469,-2.85241112092882));
#20193=CARTESIAN_POINT('Ctrl Pts',(1.71298101360102,-7.94263077383951,-2.84908853069526));
#20194=CARTESIAN_POINT('Ctrl Pts',(1.91810638711379,-7.89839154376067,-2.84086504637095));
#20195=CARTESIAN_POINT('Ctrl Pts',(2.12155038681738,-7.84619456950808,-2.83264156204664));
#20196=CARTESIAN_POINT('Ctrl Pts',(2.32269080051696,-7.78619258737503,-2.82441807772233));
#20197=CARTESIAN_POINT('Ctrl Pts',(2.52379415594392,-7.72620166005573,-2.81619610849943));
#20198=CARTESIAN_POINT('Ctrl Pts',(2.72259449000077,-7.65840867929775,-2.80797413927652));
#20199=CARTESIAN_POINT('Ctrl Pts',(2.91848401662767,-7.58301645832243,-2.79975217005362));
#20200=CARTESIAN_POINT('Ctrl Pts',(3.11437128332761,-7.50762510712772,-2.79153029568546));
#20201=CARTESIAN_POINT('Ctrl Pts',(3.30734753312896,-7.42463479330348,-2.7833084213173));
#20202=CARTESIAN_POINT('Ctrl Pts',(3.49682329234003,-7.33429713228529,-2.77508654694913));
#20203=CARTESIAN_POINT('Ctrl Pts',(3.68628594035273,-7.24396572238333,-2.76686524151193));
#20204=CARTESIAN_POINT('Ctrl Pts',(3.87224831595824,-7.14628810893926,-2.75864393607473));
#20205=CARTESIAN_POINT('Ctrl Pts',(4.05414342998451,-7.04156293812769,-2.75042263063753));
#20206=CARTESIAN_POINT('Ctrl Pts',(4.23606724799523,-6.93682124114557,-2.74220002783605));
#20207=CARTESIAN_POINT('Ctrl Pts',(4.41392226563831,-6.82502991067713,-2.73397742503457));
#20208=CARTESIAN_POINT('Ctrl Pts',(4.58716750850335,-6.70653277121876,-2.72575482223309));
#20209=CARTESIAN_POINT('Ctrl Pts',(4.70938222265734,-6.62293974558946,-2.71995424130881));
#20210=CARTESIAN_POINT('Ctrl Pts',(4.82930342435198,-6.53601051667679,-2.71415366038453));
#20211=CARTESIAN_POINT('Ctrl Pts',(4.94675008185376,-6.44587862049696,-2.70835307946025));
#20212=CARTESIAN_POINT('',(-8.12524999755206,0.000199449834196055,-3.58329744397444));
#20213=CARTESIAN_POINT('Ctrl Pts',(-8.12504666895516,0.00019942538992946,
-3.58329744321239));
#20214=CARTESIAN_POINT('Ctrl Pts',(-8.12413961048046,-0.966655941748394,
-3.54542247754037));
#20215=CARTESIAN_POINT('Ctrl Pts',(-7.71133025888803,-3.27845306278411,
-3.45489116956092));
#20216=CARTESIAN_POINT('Ctrl Pts',(-5.56705133684236,-6.37868753136333,
-3.31170351927405));
#20217=CARTESIAN_POINT('Ctrl Pts',(-1.85822808956723,-8.25994573692536,
-3.15373449235176));
#20218=CARTESIAN_POINT('Ctrl Pts',(1.97300710128673,-8.15704218041728,-3.00815060295411));
#20219=CARTESIAN_POINT('Ctrl Pts',(4.13059763958269,-7.07085441446827,-2.91522305586389));
#20220=CARTESIAN_POINT('Ctrl Pts',(4.94673849251696,-6.44586330438811,-2.8749518510811));
#20221=CARTESIAN_POINT('Ctrl Pts',(4.94675008185375,-6.44587862049697,-4.87493975109638));
#20222=CARTESIAN_POINT('Ctrl Pts',(5.1132324741457,-6.31811531060797,-4.86671727446932));
#20223=CARTESIAN_POINT('Ctrl Pts',(5.27478384445414,-6.18388235747323,-4.85849479784226));
#20224=CARTESIAN_POINT('Ctrl Pts',(5.43090817343691,-6.04358535756683,-4.8502723212152));
#20225=CARTESIAN_POINT('Ctrl Pts',(5.58701155230035,-5.90330718393119,-4.84205094795152));
#20226=CARTESIAN_POINT('Ctrl Pts',(5.73768912429145,-5.75696678494614,-4.83382957468783));
#20227=CARTESIAN_POINT('Ctrl Pts',(5.88247945748213,-5.60500874172385,-4.82560820142415));
#20228=CARTESIAN_POINT('Ctrl Pts',(6.02727953633488,-5.4530404703896,-4.81738627478978));
#20229=CARTESIAN_POINT('Ctrl Pts',(6.16619137864326,-5.29545401045529,-4.80916434815541));
#20230=CARTESIAN_POINT('Ctrl Pts',(6.29879106094806,-5.13273014418456,-4.80094242152104));
#20231=CARTESIAN_POINT('Ctrl Pts',(6.43138720887069,-4.97001061524195,-4.79272071403826));
#20232=CARTESIAN_POINT('Ctrl Pts',(6.55767134834218,-4.80215418362125,-4.78449900655548));
#20233=CARTESIAN_POINT('Ctrl Pts',(6.67726011485629,-4.6296743860718,-4.7762772990727));
#20234=CARTESIAN_POINT('Ctrl Pts',(6.7968764370129,-4.45715484572897,-4.76805369714416));
#20235=CARTESIAN_POINT('Ctrl Pts',(6.90979413463771,-4.2800100527293,-4.75983009521562));
#20236=CARTESIAN_POINT('Ctrl Pts',(7.01567275688913,-4.09878315244215,-4.75160649328707));
#20237=CARTESIAN_POINT('Ctrl Pts',(7.09370250267782,-3.96522371750828,-4.7455459160496));
#20238=CARTESIAN_POINT('Ctrl Pts',(7.16791000112718,-3.82944779232662,-4.73948533881213));
#20239=CARTESIAN_POINT('Ctrl Pts',(7.23817473186266,-3.69168174596956,-4.73342476157466));
#20240=CARTESIAN_POINT('Ctrl Pts',(7.33351627047917,-3.50474832017674,-4.7252012225007));
#20241=CARTESIAN_POINT('Ctrl Pts',(7.4216277987783,-3.31408911611699,-4.71697768342674));
#20242=CARTESIAN_POINT('Ctrl Pts',(7.50223448347721,-3.12028289060871,-4.70875414435278));
#20243=CARTESIAN_POINT('Ctrl Pts',(7.5828265124807,-2.92651190243866,-4.70053210046107));
#20244=CARTESIAN_POINT('Ctrl Pts',(7.65591630808611,-2.72959530701753,-4.69231005656936));
#20245=CARTESIAN_POINT('Ctrl Pts',(7.72127696362888,-2.53013233120998,-4.68408801267765));
#20246=CARTESIAN_POINT('Ctrl Pts',(7.78663040283976,-2.33069137768815,-4.67586687656443));
#20247=CARTESIAN_POINT('Ctrl Pts',(7.84425631388144,-2.12870488522847,-4.66764574045121));
#20248=CARTESIAN_POINT('Ctrl Pts',(7.89397723693811,-1.92478854558182,-4.65942460433799));
#20249=CARTESIAN_POINT('Ctrl Pts',(7.94370210361384,-1.72085603229403,-4.65120281616469));
#20250=CARTESIAN_POINT('Ctrl Pts',(7.98552065708786,-1.51499365189972,-4.64298102799139));
#20251=CARTESIAN_POINT('Ctrl Pts',(8.01930602506436,-1.3078296673751,-4.63475923981809));
#20252=CARTESIAN_POINT('Ctrl Pts',(8.05309129929548,-1.10066625767523,-4.62653747445805));
#20253=CARTESIAN_POINT('Ctrl Pts',(8.07884338780635,-0.892201542590064,
-4.61831570909802));
#20254=CARTESIAN_POINT('Ctrl Pts',(8.09648691627167,-0.683071868211351,
-4.61009394373799));
#20255=CARTESIAN_POINT('Ctrl Pts',(8.11413412311977,-0.473898593767195,
-4.60187046427636));
#20256=CARTESIAN_POINT('Ctrl Pts',(8.12366936798904,-0.264060377022058,
-4.59364698481474));
#20257=CARTESIAN_POINT('Ctrl Pts',(8.12506924132972,-0.0541976576764842,
-4.58542350535312));
#20258=CARTESIAN_POINT('Ctrl Pts',(8.12563484199933,0.0305946525547484,
-4.58210091511954));
#20259=CARTESIAN_POINT('Ctrl Pts',(8.12487296994328,0.11539094534123,-4.57877832488595));
#20260=CARTESIAN_POINT('Ctrl Pts',(8.12278449485915,0.200148975954851,-4.57545573465237));
#20261=CARTESIAN_POINT('Ctrl Pts',(8.11761543841465,0.409928373227015,-4.56723219557842));
#20262=CARTESIAN_POINT('Ctrl Pts',(8.10431454180795,0.619541492237617,-4.55900865650445));
#20263=CARTESIAN_POINT('Ctrl Pts',(8.08291570350302,0.828348533266186,-4.55078511743049));
#20264=CARTESIAN_POINT('Ctrl Pts',(8.06152075587859,1.0371176095477,-4.54256307353878));
#20265=CARTESIAN_POINT('Ctrl Pts',(8.03203083524404,1.24508060710941,-4.53434102964707));
#20266=CARTESIAN_POINT('Ctrl Pts',(7.99453173180774,1.45160254602257,-4.52611898575536));
#20267=CARTESIAN_POINT('Ctrl Pts',(7.95703676856823,1.65810168328472,-4.51789784964215));
#20268=CARTESIAN_POINT('Ctrl Pts',(7.91153444062383,1.8631597894672,-4.50967671352893));
#20269=CARTESIAN_POINT('Ctrl Pts',(7.85816185969371,2.06615095028293,-4.50145557741572));
#20270=CARTESIAN_POINT('Ctrl Pts',(7.80478504551296,2.26915821135924,-4.49323378924242));
#20271=CARTESIAN_POINT('Ctrl Pts',(7.74353680351568,2.47009791357987,-4.48501200106911));
#20272=CARTESIAN_POINT('Ctrl Pts',(7.67460471601866,2.66835717537292,-4.47679021289581));
#20273=CARTESIAN_POINT('Ctrl Pts',(7.60567281978979,2.86661588704942,-4.46856844753578));
#20274=CARTESIAN_POINT('Ctrl Pts',(7.52905722011355,3.06219389548709,-4.46034668217575));
#20275=CARTESIAN_POINT('Ctrl Pts',(7.44499463349515,3.25449573201878,-4.45212491681572));
#20276=CARTESIAN_POINT('Ctrl Pts',(7.36091452122291,3.44683766029109,-4.4439014373541));
#20277=CARTESIAN_POINT('Ctrl Pts',(7.2693844385665,3.63590178187527,-4.43567795789247));
#20278=CARTESIAN_POINT('Ctrl Pts',(7.1706887470963,3.82111377150256,-4.42745447843085));
#20279=CARTESIAN_POINT('Ctrl Pts',(7.13081203285308,3.8959462740644,-4.42413188819726));
#20280=CARTESIAN_POINT('Ctrl Pts',(7.08976609237674,3.97015019909408,-4.42080929796367));
#20281=CARTESIAN_POINT('Ctrl Pts',(7.04757180538567,4.04368881226449,-4.41748670773008));
#20282=CARTESIAN_POINT('Ctrl Pts',(6.94313931646145,4.22569971831549,-4.40926316865612));
#20283=CARTESIAN_POINT('Ctrl Pts',(6.83163516488619,4.40369240831537,-4.40103962958216));
#20284=CARTESIAN_POINT('Ctrl Pts',(6.71339380202864,4.57712040713192,-4.3928160905082));
#20285=CARTESIAN_POINT('Ctrl Pts',(6.59517393750472,4.75051687372583,-4.38459404661648));
#20286=CARTESIAN_POINT('Ctrl Pts',(6.47021947260325,4.91935006203631,-4.37637200272477));
#20287=CARTESIAN_POINT('Ctrl Pts',(6.33890819539813,5.08310244366709,-4.36814995883306));
#20288=CARTESIAN_POINT('Ctrl Pts',(6.20761141599382,5.24683674574323,-4.35992882271985));
#20289=CARTESIAN_POINT('Ctrl Pts',(6.06995940992534,5.40549113107433,-4.35170768660663));
#20290=CARTESIAN_POINT('Ctrl Pts',(5.92637077885693,5.55858048012356,-4.34348655049342));
#20291=CARTESIAN_POINT('Ctrl Pts',(5.78277075904442,5.71168197146712,-4.33526476232012));
#20292=CARTESIAN_POINT('Ctrl Pts',(5.63323337324402,5.85921732765079,-4.32704297414682));
#20293=CARTESIAN_POINT('Ctrl Pts',(5.47821539951651,6.00073692132893,-4.31882118597352));
#20294=CARTESIAN_POINT('Ctrl Pts',(5.32319785592232,6.14225612232813,-4.31059942061348));
#20295=CARTESIAN_POINT('Ctrl Pts',(5.16269997445483,6.27775939735401,-4.30237765525344));
#20296=CARTESIAN_POINT('Ctrl Pts',(4.99721344874421,6.40683582669245,-4.2941558898934));
#20297=CARTESIAN_POINT('Ctrl Pts',(4.83169242184021,6.53593916632363,-4.28593241043177));
#20298=CARTESIAN_POINT('Ctrl Pts',(4.66118090557146,6.65861280212723,-4.27770893097014));
#20299=CARTESIAN_POINT('Ctrl Pts',(4.48620242337377,6.77448709342746,-4.26948545150851));
#20300=CARTESIAN_POINT('Ctrl Pts',(4.41550463678005,6.82130459815806,-4.26616286127494));
#20301=CARTESIAN_POINT('Ctrl Pts',(4.34407797516309,6.86701262512926,-4.26284027104136));
#20302=CARTESIAN_POINT('Ctrl Pts',(4.2719582905141,6.91158881347899,-4.25951768080778));
#20303=CARTESIAN_POINT('Ctrl Pts',(4.09345928732092,7.02191660020329,-4.25129414173382));
#20304=CARTESIAN_POINT('Ctrl Pts',(3.91065501232499,7.12534372698899,-4.24307060265986));
#20305=CARTESIAN_POINT('Ctrl Pts',(3.72409977514372,7.22154889391981,-4.2348470635859));
#20306=CARTESIAN_POINT('Ctrl Pts',(3.53757845694513,7.31773656908015,-4.22662501969419));
#20307=CARTESIAN_POINT('Ctrl Pts',(3.34730779973729,7.4067047700262,-4.21840297580247));
#20308=CARTESIAN_POINT('Ctrl Pts',(3.15386643875261,7.48817828640651,-4.21018093191076));
#20309=CARTESIAN_POINT('Ctrl Pts',(2.96044643521978,7.56964280746806,-4.20195979579754));
#20310=CARTESIAN_POINT('Ctrl Pts',(2.7638566985175,7.64361418154556,-4.19373865968432));
#20311=CARTESIAN_POINT('Ctrl Pts',(2.56469632226102,7.70986513092679,-4.18551752357109));
#20312=CARTESIAN_POINT('Ctrl Pts',(2.36552014958323,7.77612133500741,-4.1772957353978));
#20313=CARTESIAN_POINT('Ctrl Pts',(2.16377320898779,7.8346557952561,-4.1690739472245));
#20314=CARTESIAN_POINT('Ctrl Pts',(1.9600712652865,7.88529062225979,-4.16085215905121));
#20315=CARTESIAN_POINT('Ctrl Pts',(1.75636988680338,7.93592530876543,-4.15263039369117));
#20316=CARTESIAN_POINT('Ctrl Pts',(1.55071380293803,7.97866033734236,-4.14440862833113));
#20317=CARTESIAN_POINT('Ctrl Pts',(1.34373105120879,8.01336848176329,-4.13618686297108));
#20318=CARTESIAN_POINT('Ctrl Pts',(1.136705147012,8.04808386225614,-4.12796338350946));
#20319=CARTESIAN_POINT('Ctrl Pts',(0.928352313331279,8.0747689666918,-4.11973990404783));
#20320=CARTESIAN_POINT('Ctrl Pts',(0.719308922504071,8.09334802393336,-4.1115164245862));
#20321=CARTESIAN_POINT('Ctrl Pts',(0.634847651335928,8.10085465107674,-4.10819383435263));
#20322=CARTESIAN_POINT('Ctrl Pts',(0.550273715462386,8.10703858915528,-4.10487124411907));
#20323=CARTESIAN_POINT('Ctrl Pts',(0.465629288968813,8.1118972458824,-4.1015486538855));
#20324=CARTESIAN_POINT('Ctrl Pts',(0.25613106627784,8.12392260881723,-4.09332511481154));
#20325=CARTESIAN_POINT('Ctrl Pts',(0.0461327158269894,8.12782982263373,
-4.08510157573759));
#20326=CARTESIAN_POINT('Ctrl Pts',(-0.16372533540842,8.12360028417483,-4.07687803666363));
#20327=CARTESIAN_POINT('Ctrl Pts',(-0.373545230804828,8.11937151471949,
-4.06865599277192));
#20328=CARTESIAN_POINT('Ctrl Pts',(-0.583224583169709,8.10700895164779,
-4.06043394888021));
#20329=CARTESIAN_POINT('Ctrl Pts',(-0.792123520158524,8.08654610395017,
-4.0522119049885));
#20330=CARTESIAN_POINT('Ctrl Pts',(-1.00099939305715,8.06608551551232,-4.04399076887528));
#20331=CARTESIAN_POINT('Ctrl Pts',(-1.20909472918742,8.03752645669771,-4.03576963276207));
#20332=CARTESIAN_POINT('Ctrl Pts',(-1.41577448911982,8.00095432798222,-4.02754849664885));
#20333=CARTESIAN_POINT('Ctrl Pts',(-1.6224706418742,7.96437929854537,-4.01932670847555));
#20334=CARTESIAN_POINT('Ctrl Pts',(-1.82775070319881,7.91978997808841,-4.01110492030225));
#20335=CARTESIAN_POINT('Ctrl Pts',(-2.03098849000564,7.8673231353469,-4.00288313212895));
#20336=CARTESIAN_POINT('Ctrl Pts',(-2.23422571288189,7.81485643818687,-3.99466136676892));
#20337=CARTESIAN_POINT('Ctrl Pts',(-2.43542038768013,7.75451233879826,-3.98643960140889));
#20338=CARTESIAN_POINT('Ctrl Pts',(-2.63395966256229,7.68647800091139,-3.97821783604886));
#20339=CARTESIAN_POINT('Ctrl Pts',(-2.83254032958749,7.61842947899445,-3.96999435658723));
#20340=CARTESIAN_POINT('Ctrl Pts',(-3.02846421169279,7.54268761129695,-3.9617708771256));
#20341=CARTESIAN_POINT('Ctrl Pts',(-3.22113562818867,7.45948877787973,-3.95354739766397));
#20342=CARTESIAN_POINT('Ctrl Pts',(-3.29898201544212,7.42587336816808,-3.95022480743039));
#20343=CARTESIAN_POINT('Ctrl Pts',(-3.3762976739393,7.39104118950326,-3.9469022171968));
#20344=CARTESIAN_POINT('Ctrl Pts',(-3.45304428304078,7.35501004362736,-3.94357962696321));
#20345=CARTESIAN_POINT('Ctrl Pts',(-3.64299510284388,7.26583156684903,-3.93535608788926));
#20346=CARTESIAN_POINT('Ctrl Pts',(-3.82952023818505,7.16927615582599,-3.9271325488153));
#20347=CARTESIAN_POINT('Ctrl Pts',(-4.01204766356215,7.06563239263164,-3.91890900974134));
#20348=CARTESIAN_POINT('Ctrl Pts',(-4.1945419022827,6.9620074736738,-3.91068696584964));
#20349=CARTESIAN_POINT('Ctrl Pts',(-4.37303962540975,6.8512969203726,-3.90246492195793));
#20350=CARTESIAN_POINT('Ctrl Pts',(-4.54699410849938,6.73383487618845,-3.89424287806623));
#20351=CARTESIAN_POINT('Ctrl Pts',(-4.7209293856421,6.6163858007404,-3.88602174195302));
#20352=CARTESIAN_POINT('Ctrl Pts',(-4.8903221798591,6.49218688759362,-3.87780060583981));
#20353=CARTESIAN_POINT('Ctrl Pts',(-5.05465472485914,6.36161561043727,-3.8695794697266));
#20354=CARTESIAN_POINT('Ctrl Pts',(-5.2190003039085,6.23103397700934,-3.8613576815533));
#20355=CARTESIAN_POINT('Ctrl Pts',(-5.37828459922607,6.09407915109421,-3.85313589337999));
#20356=CARTESIAN_POINT('Ctrl Pts',(-5.53202209158898,5.95116956073943,-3.84491410520669));
#20357=CARTESIAN_POINT('Ctrl Pts',(-5.68575915737158,5.80826036692043,-3.83669233984665));
#20358=CARTESIAN_POINT('Ctrl Pts',(-5.83394923680583,5.65939664449093,-3.82847057448661));
#20359=CARTESIAN_POINT('Ctrl Pts',(-5.97614252938187,5.50503478926457,-3.82024880912657));
#20360=CARTESIAN_POINT('Ctrl Pts',(-6.11836546689877,5.35064075215407,-3.81202532966495));
#20361=CARTESIAN_POINT('Ctrl Pts',(-6.25458892009618,5.19074650929195,-3.80380185020333));
#20362=CARTESIAN_POINT('Ctrl Pts',(-6.38440162261658,5.0258435594068,-3.7955783707417));
#20363=CARTESIAN_POINT('Ctrl Pts',(-6.43685076164627,4.95921666098309,-3.79225578050811));
#20364=CARTESIAN_POINT('Ctrl Pts',(-6.4882538298834,4.89177248929108,-3.78893319027452));
#20365=CARTESIAN_POINT('Ctrl Pts',(-6.53858560593557,4.82354494499141,-3.78561060004092));
#20366=CARTESIAN_POINT('Ctrl Pts',(-6.66315869437788,4.65467913939306,-3.77738706096696));
#20367=CARTESIAN_POINT('Ctrl Pts',(-6.78120681715271,4.48095748207517,-3.769163521893));
#20368=CARTESIAN_POINT('Ctrl Pts',(-6.89236436551681,4.30290611278634,-3.76093998281904));
#20369=CARTESIAN_POINT('Ctrl Pts',(-7.00350170350785,4.12488711632912,-3.75271793892732));
#20370=CARTESIAN_POINT('Ctrl Pts',(-7.10775081147395,3.9425402291546,-3.7444958950356));
#20371=CARTESIAN_POINT('Ctrl Pts',(-7.20479002365202,3.75641960882758,-3.73627385114388));
#20372=CARTESIAN_POINT('Ctrl Pts',(-7.30181852193517,3.57031953768601,-3.7280527150307));
#20373=CARTESIAN_POINT('Ctrl Pts',(-7.39163857737415,3.38044682663969,-3.71983157891752));
#20374=CARTESIAN_POINT('Ctrl Pts',(-7.47397462072646,3.18737994773712,-3.71161044280434));
#20375=CARTESIAN_POINT('Ctrl Pts',(-7.55631719456911,2.99429775571852,-3.70338865463104));
#20376=CARTESIAN_POINT('Ctrl Pts',(-7.63117445212954,2.79802115989834,-3.69516686645774));
#20377=CARTESIAN_POINT('Ctrl Pts',(-7.69831868155846,2.59914929153136,-3.68694507828445));
#20378=CARTESIAN_POINT('Ctrl Pts',(-7.76546272468028,2.40027797498013,-3.6787233129244));
#20379=CARTESIAN_POINT('Ctrl Pts',(-7.82489369069168,2.19881168058482,-3.67050154756434));
#20380=CARTESIAN_POINT('Ctrl Pts',(-7.87643335589743,1.995365919476,-3.66227978220429));
#20381=CARTESIAN_POINT('Ctrl Pts',(-7.92798376626765,1.79187774330387,-3.65405630274267));
#20382=CARTESIAN_POINT('Ctrl Pts',(-7.97163951674269,1.58640956194257,-3.64583282328105));
#20383=CARTESIAN_POINT('Ctrl Pts',(-8.00727298346709,1.37958940657647,-3.63760934381942));
#20384=CARTESIAN_POINT('Ctrl Pts',(-8.02167022359886,1.29602640486445,-3.63428675358583));
#20385=CARTESIAN_POINT('Ctrl Pts',(-8.0347584413262,1.21224281293768,-3.63096416335223));
#20386=CARTESIAN_POINT('Ctrl Pts',(-8.0465315997878,1.1282804510034,-3.62764157311864));
#20387=CARTESIAN_POINT('Ctrl Pts',(-8.07696037224254,0.911272278184235,
-3.61905404390901));
#20388=CARTESIAN_POINT('Ctrl Pts',(-8.09860760385926,0.693021489309309,
-3.61046651469939));
#20389=CARTESIAN_POINT('Ctrl Pts',(-8.11139938405216,0.474223148842588,
-3.60187898548977));
#20390=CARTESIAN_POINT('Ctrl Pts',(-8.12062559215414,0.316412508644634,
-3.59568513831799));
#20391=CARTESIAN_POINT('Ctrl Pts',(-8.125246116249,0.158317193216755,-3.58949129114622));
#20392=CARTESIAN_POINT('Ctrl Pts',(-8.12524999755206,0.000199449834196055,
-3.58329744397444));
#20393=CARTESIAN_POINT('Origin',(0.,0.,-16.4167025567876));
#20394=CARTESIAN_POINT('',(4.94635656995632,-6.44536625007808,-6.87494113800006));
#20395=CARTESIAN_POINT('',(4.94675008185374,-6.44587862049698,-6.70835078220711));
#20396=CARTESIAN_POINT('',(4.94675008185374,-6.44587862049697,-16.4167025567876));
#20397=CARTESIAN_POINT('',(-8.12524999741292,-0.000205039998872057,-5.41670255678761));
#20398=CARTESIAN_POINT('Ctrl Pts',(4.94675008185374,-6.44587862049698,-6.70835078220711));
#20399=CARTESIAN_POINT('Ctrl Pts',(5.11326951467367,-6.3180868846562,-6.70012907610502));
#20400=CARTESIAN_POINT('Ctrl Pts',(5.27483045724498,-6.18384202628876,-6.69190737000293));
#20401=CARTESIAN_POINT('Ctrl Pts',(5.43094150658574,-6.04355540344789,-6.68368566390084));
#20402=CARTESIAN_POINT('Ctrl Pts',(5.587088754445,-5.90323625140468,-6.67546205137649));
#20403=CARTESIAN_POINT('Ctrl Pts',(5.73778336380036,-5.75687273201702,-6.66723843885213));
#20404=CARTESIAN_POINT('Ctrl Pts',(5.88256886172007,-5.60491491011428,-6.65901482632778));
#20405=CARTESIAN_POINT('Ctrl Pts',(5.99213524715329,-5.48992087049424,-6.65279160982859));
#20406=CARTESIAN_POINT('Ctrl Pts',(6.09831836201026,-5.37172394965353,-6.6465683933294));
#20407=CARTESIAN_POINT('Ctrl Pts',(6.20093491455416,-5.25053271087451,-6.64034517683022));
#20408=CARTESIAN_POINT('Ctrl Pts',(6.33653540822028,-5.09038708720026,-6.63212163775625));
#20409=CARTESIAN_POINT('Ctrl Pts',(6.46595071955236,-4.92495960851299,-6.62389809868228));
#20410=CARTESIAN_POINT('Ctrl Pts',(6.58878083086729,-4.75475075322521,-6.61567455960831));
#20411=CARTESIAN_POINT('Ctrl Pts',(6.71158860953403,-4.58457284486441,-6.60745251571662));
#20412=CARTESIAN_POINT('Ctrl Pts',(6.82781340535999,-4.40961553404571,-6.59923047182492));
#20413=CARTESIAN_POINT('Ctrl Pts',(6.93709716899744,-4.23041019646886,-6.59100842793323));
#20414=CARTESIAN_POINT('Ctrl Pts',(7.04636886684463,-4.05122464457604,-6.58278729182009));
#20415=CARTESIAN_POINT('Ctrl Pts',(7.14870090898439,-3.86779225400607,-6.57456615570695));
#20416=CARTESIAN_POINT('Ctrl Pts',(7.24377961108072,-3.68067174692219,-6.56634501959381));
#20417=CARTESIAN_POINT('Ctrl Pts',(7.33886585435287,-3.49353639835843,-6.55812323142052));
#20418=CARTESIAN_POINT('Ctrl Pts',(7.4266974721114,-3.30271261053811,-6.54990144324723));
#20419=CARTESIAN_POINT('Ctrl Pts',(7.50700714670423,-3.10878292291882,-6.54167965507394));
#20420=CARTESIAN_POINT('Ctrl Pts',(7.58731659845966,-2.91485377340139,-6.53345788971386));
#20421=CARTESIAN_POINT('Ctrl Pts',(7.66010403844753,-2.71781901484677,-6.52523612435379));
#20422=CARTESIAN_POINT('Ctrl Pts',(7.72515042933764,-2.51828084347326,-6.51701435899371));
#20423=CARTESIAN_POINT('Ctrl Pts',(7.79021038131989,-2.31870107170516,-6.50879087953212));
#20424=CARTESIAN_POINT('Ctrl Pts',(7.84752596870894,-2.1166171249319,-6.50056740007052));
#20425=CARTESIAN_POINT('Ctrl Pts',(7.89692780213458,-1.91264707940956,-6.49234392060892));
#20426=CARTESIAN_POINT('Ctrl Pts',(7.91688797228293,-1.83023562761756,-6.48902133037526));
#20427=CARTESIAN_POINT('Ctrl Pts',(7.93555682812912,-1.74751643068539,-6.4856987401416));
#20428=CARTESIAN_POINT('Ctrl Pts',(7.95292554614784,-1.66453081074789,-6.48237614990794));
#20429=CARTESIAN_POINT('Ctrl Pts',(7.99591379364358,-1.45913819831596,-6.47415261083398));
#20430=CARTESIAN_POINT('Ctrl Pts',(8.03094805362722,-1.25204601077799,-6.46592907176003));
#20431=CARTESIAN_POINT('Ctrl Pts',(8.05791486960765,-1.04388481963096,-6.45770553268607));
#20432=CARTESIAN_POINT('Ctrl Pts',(8.08487678255251,-0.835761475804336,
-6.44948348879436));
#20433=CARTESIAN_POINT('Ctrl Pts',(8.10377414118939,-0.626569808641515,
-6.44126144490266));
#20434=CARTESIAN_POINT('Ctrl Pts',(8.1145451062385,-0.416947576226108,-6.43303940101096));
#20435=CARTESIAN_POINT('Ctrl Pts',(8.12531488208813,-0.207348487758192,
-6.42481826489773));
#20436=CARTESIAN_POINT('Ctrl Pts',(8.12796004048379,0.00268077662337693,
-6.41659712878451));
#20437=CARTESIAN_POINT('Ctrl Pts',(8.12247077617056,0.212499535893956,-6.40837599267128));
#20438=CARTESIAN_POINT('Ctrl Pts',(8.11698107647588,0.422334936956949,-6.40015420449796));
#20439=CARTESIAN_POINT('Ctrl Pts',(8.1033556700032,0.63195950463673,-6.39193241632464));
#20440=CARTESIAN_POINT('Ctrl Pts',(8.08163686529504,0.840733691488665,-6.38371062815132));
#20441=CARTESIAN_POINT('Ctrl Pts',(8.05991812085099,1.04950729904586,-6.37548886279135));
#20442=CARTESIAN_POINT('Ctrl Pts',(8.03010605629281,1.25743023742523,-6.36726709743138));
#20443=CARTESIAN_POINT('Ctrl Pts',(7.99229479569316,1.46386866256367,-6.35904533207141));
#20444=CARTESIAN_POINT('Ctrl Pts',(7.95447565207312,1.67035012668813,-6.35082185260979));
#20445=CARTESIAN_POINT('Ctrl Pts',(7.90865403397151,1.87534616912787,-6.34259837314818));
#20446=CARTESIAN_POINT('Ctrl Pts',(7.85497528534438,2.07823262151497,-6.33437489368657));
#20447=CARTESIAN_POINT('Ctrl Pts',(7.83328708307246,2.16020626155208,-6.33105230345293));
#20448=CARTESIAN_POINT('Ctrl Pts',(7.81031681357776,2.24183565845636,-6.32772971321928));
#20449=CARTESIAN_POINT('Ctrl Pts',(7.78607639342532,2.32308027374109,-6.32440712298564));
#20450=CARTESIAN_POINT('Ctrl Pts',(7.72608041791378,2.52416383245887,-6.3161835839117));
#20451=CARTESIAN_POINT('Ctrl Pts',(7.65828074572195,2.72295462188927,-6.30796004483777));
#20452=CARTESIAN_POINT('Ctrl Pts',(7.58287785573238,2.91884411840432,-6.29973650576383));
#20453=CARTESIAN_POINT('Ctrl Pts',(7.5074886752977,3.11469799880699,-6.2915144618721));
#20454=CARTESIAN_POINT('Ctrl Pts',(7.42449914206898,3.30765136402373,-6.28329241798038));
#20455=CARTESIAN_POINT('Ctrl Pts',(7.33415854708852,3.49711394848214,-6.27507037408866));
#20456=CARTESIAN_POINT('Ctrl Pts',(7.24382792642313,3.68655561477513,-6.26684923797551));
#20457=CARTESIAN_POINT('Ctrl Pts',(7.14614799125664,3.87250700365054,-6.25862810186236));
#20458=CARTESIAN_POINT('Ctrl Pts',(7.04141518117523,4.05440005534913,-6.25040696574921));
#20459=CARTESIAN_POINT('Ctrl Pts',(6.93667406420138,4.2363075339118,-6.24218517757589));
#20460=CARTESIAN_POINT('Ctrl Pts',(6.82487909945776,4.41415577521435,-6.23396338940258));
#20461=CARTESIAN_POINT('Ctrl Pts',(6.7063720137003,4.58740253044764,-6.22574160122926));
#20462=CARTESIAN_POINT('Ctrl Pts',(6.5878652567695,4.76064880496577,-6.21751983586929));
#20463=CARTESIAN_POINT('Ctrl Pts',(6.46264658482042,4.92929337704814,-6.20929807050932));
#20464=CARTESIAN_POINT('Ctrl Pts',(6.33110057357052,5.09282368532772,-6.20107630514935));
#20465=CARTESIAN_POINT('Ctrl Pts',(6.19952713715985,5.25638808696333,-6.19285282568771));
#20466=CARTESIAN_POINT('Ctrl Pts',(6.06162391106848,5.41483586490666,-6.18462934622608));
#20467=CARTESIAN_POINT('Ctrl Pts',(5.91781590475822,5.56768735471836,-6.17640586676445));
#20468=CARTESIAN_POINT('Ctrl Pts',(5.85971214472291,5.62944501698576,-6.17308327653075));
#20469=CARTESIAN_POINT('Ctrl Pts',(5.80064489493821,5.69028950500846,-6.16976068629705));
#20470=CARTESIAN_POINT('Ctrl Pts',(5.74064393689378,5.75019084485938,-6.16643809606335));
#20471=CARTESIAN_POINT('Ctrl Pts',(5.59213924981279,5.89844897306637,-6.15821455698939));
#20472=CARTESIAN_POINT('Ctrl Pts',(5.43786399151661,6.04097517483154,-6.14999101791542));
#20473=CARTESIAN_POINT('Ctrl Pts',(5.27828420577773,6.1773297957562,-6.14176747884146));
#20474=CARTESIAN_POINT('Ctrl Pts',(5.11873343441515,6.31365962504285,-6.13354543494971));
#20475=CARTESIAN_POINT('Ctrl Pts',(4.95388028466916,6.44381992157428,-6.12532339105795));
#20476=CARTESIAN_POINT('Ctrl Pts',(4.78422503028089,6.56741032844254,-6.1171013471662));
#20477=CARTESIAN_POINT('Ctrl Pts',(4.6145885071715,6.6909870899546,-6.10888021105298));
#20478=CARTESIAN_POINT('Ctrl Pts',(4.44015117621969,6.80799523638049,-6.10065907493975));
#20479=CARTESIAN_POINT('Ctrl Pts',(4.26144419847832,6.91807638767855,-6.09243793882653));
#20480=CARTESIAN_POINT('Ctrl Pts',(4.08272304657839,7.02816627007213,-6.08421615065322));
#20481=CARTESIAN_POINT('Ctrl Pts',(3.89973182097379,7.13132790261098,-6.07599436247992));
#20482=CARTESIAN_POINT('Ctrl Pts',(3.7130292166108,7.22724716604425,-6.06777257430661));
#20483=CARTESIAN_POINT('Ctrl Pts',(3.52632713029842,7.32316616332679,-6.0595508089466));
#20484=CARTESIAN_POINT('Ctrl Pts',(3.33591394939592,7.41184269932437,-6.05132904358659));
#20485=CARTESIAN_POINT('Ctrl Pts',(3.14237191287177,7.49300916345994,-6.04310727822659));
#20486=CARTESIAN_POINT('Ctrl Pts',(2.94878952604574,7.57419254945594,-6.03488379876498));
#20487=CARTESIAN_POINT('Ctrl Pts',(2.7520772524932,7.64786262163657,-6.02666031930337));
#20488=CARTESIAN_POINT('Ctrl Pts',(2.55283722314821,7.7137999503882,-6.01843683984177));
#20489=CARTESIAN_POINT('Ctrl Pts',(2.47233687305581,7.74044107298848,-6.0151142496082));
#20490=CARTESIAN_POINT('Ctrl Pts',(2.39142407639492,7.76582041608099,-6.01179165937464));
#20491=CARTESIAN_POINT('Ctrl Pts',(2.31013929405954,7.78992580224883,-6.00846906914107));
#20492=CARTESIAN_POINT('Ctrl Pts',(2.10895632033603,7.84958756343791,-6.00024553006711));
#20493=CARTESIAN_POINT('Ctrl Pts',(1.90542819374412,7.90146120990598,-5.99202199099315));
#20494=CARTESIAN_POINT('Ctrl Pts',(1.70017407837136,7.94538203397005,-5.98379845191919));
#20495=CARTESIAN_POINT('Ctrl Pts',(1.49495728176153,7.98929487246551,-5.97557640802745));
#20496=CARTESIAN_POINT('Ctrl Pts',(1.28801541097213,8.02525771284695,-5.96735436413572));
#20497=CARTESIAN_POINT('Ctrl Pts',(1.07997901904253,8.05315670286677,-5.95913232024398));
#20498=CARTESIAN_POINT('Ctrl Pts',(0.871965595972208,8.08105261261793,-5.95091118413078));
#20499=CARTESIAN_POINT('Ctrl Pts',(0.662858185225844,8.10088641029755,-5.94269004801757));
#20500=CARTESIAN_POINT('Ctrl Pts',(0.453294513595352,8.11259586362123,-5.93446891190436));
#20501=CARTESIAN_POINT('Ctrl Pts',(0.243714220404542,8.1243062456812,-5.92624712373105));
#20502=CARTESIAN_POINT('Ctrl Pts',(0.0336778883579213,8.12789097674848,
-5.91802533555773));
#20503=CARTESIAN_POINT('Ctrl Pts',(-0.176173618367589,8.12333985616084,
-5.90980354738442));
#20504=CARTESIAN_POINT('Ctrl Pts',(-0.386024542812005,8.11878874820134,
-5.90158178202434));
#20505=CARTESIAN_POINT('Ctrl Pts',(-0.595690348156888,8.10610184283517,
-5.89336001666426));
#20506=CARTESIAN_POINT('Ctrl Pts',(-0.804531611719473,8.08532104793892,
-5.88513825130418));
#20507=CARTESIAN_POINT('Ctrl Pts',(-1.01341641521735,8.06453592059203,-5.87691477184256));
#20508=CARTESIAN_POINT('Ctrl Pts',(-1.22147603998337,8.03565356189918,-5.86869129238094));
#20509=CARTESIAN_POINT('Ctrl Pts',(-1.42807651257622,7.99876771988837,-5.86046781291932));
#20510=CARTESIAN_POINT('Ctrl Pts',(-1.51155075431057,7.9838644737634,-5.85714522268581));
#20511=CARTESIAN_POINT('Ctrl Pts',(-1.59478688650748,7.96765527834915,-5.85382263245229));
#20512=CARTESIAN_POINT('Ctrl Pts',(-1.67774353105893,7.95014869084157,-5.85050004221878));
#20513=CARTESIAN_POINT('Ctrl Pts',(-1.88306442830071,7.90681921103757,-5.84227650314483));
#20514=CARTESIAN_POINT('Ctrl Pts',(-2.08673923399196,7.8555245033341,-5.83405296407088));
#20515=CARTESIAN_POINT('Ctrl Pts',(-2.28814505236409,7.79641454656188,-5.82582942499694));
#20516=CARTESIAN_POINT('Ctrl Pts',(-2.48951425166124,7.73731533700619,-5.81760738110519));
#20517=CARTESIAN_POINT('Ctrl Pts',(-2.6886150041662,7.67040379744663,-5.80938533721345));
#20518=CARTESIAN_POINT('Ctrl Pts',(-2.88483861404142,7.59588004996364,-5.8011632933217));
#20519=CARTESIAN_POINT('Ctrl Pts',(-3.08104055927825,7.52136453049174,-5.79294215720862));
#20520=CARTESIAN_POINT('Ctrl Pts',(-3.27436572046839,7.43923858569441,-5.78472102109554));
#20521=CARTESIAN_POINT('Ctrl Pts',(-3.46422367242602,7.34975114612074,-5.77649988498246));
#20522=CARTESIAN_POINT('Ctrl Pts',(-3.65409668298617,7.26025660884182,-5.76827809680914));
#20523=CARTESIAN_POINT('Ctrl Pts',(-3.84050166691176,7.16339953349815,-5.76005630863583));
#20524=CARTESIAN_POINT('Ctrl Pts',(-4.02287021511202,7.05947609917794,-5.75183452046252));
#20525=CARTESIAN_POINT('Ctrl Pts',(-4.20523825728861,6.9555529532173,-5.74361275510245));
#20526=CARTESIAN_POINT('Ctrl Pts',(-4.38356963123258,6.84456363586739,-5.73539098974239));
#20527=CARTESIAN_POINT('Ctrl Pts',(-4.55732200706753,6.72684946214778,-5.72716922438233));
#20528=CARTESIAN_POINT('Ctrl Pts',(-4.73111060738766,6.60911074697762,-5.71894574492071));
#20529=CARTESIAN_POINT('Ctrl Pts',(-4.90031805827466,6.48464454005489,-5.71072226545909));
#20530=CARTESIAN_POINT('Ctrl Pts',(-5.06443150553653,6.35383514802115,-5.70249878599748));
#20531=CARTESIAN_POINT('Ctrl Pts',(-5.13073941566506,6.30098330951763,-5.69917619576382));
#20532=CARTESIAN_POINT('Ctrl Pts',(-5.19621610995916,6.24709644447586,-5.69585360553015));
#20533=CARTESIAN_POINT('Ctrl Pts',(-5.26082927658764,6.1922017800697,-5.69253101529649));
#20534=CARTESIAN_POINT('Ctrl Pts',(-5.42074935793885,6.05633536683449,-5.6843074762225));
#20535=CARTESIAN_POINT('Ctrl Pts',(-5.57542926357776,5.91424842055227,-5.67608393714851));
#20536=CARTESIAN_POINT('Ctrl Pts',(-5.72439265504912,5.76636942046897,-5.66786039807451));
#20537=CARTESIAN_POINT('Ctrl Pts',(-5.87332896238828,5.61851730735668,-5.65963835418277));
#20538=CARTESIAN_POINT('Ctrl Pts',(-6.0165506207996,5.46487544998669,-5.65141631029103));
#20539=CARTESIAN_POINT('Ctrl Pts',(-6.15361765455743,5.30590966037108,-5.64319426639929));
#20540=CARTESIAN_POINT('Ctrl Pts',(-6.29066955503286,5.14696142183336,-5.63497313028609));
#20541=CARTESIAN_POINT('Ctrl Pts',(-6.42156799496789,4.98269064785968,-5.62675199417289));
#20542=CARTESIAN_POINT('Ctrl Pts',(-6.54591230544676,4.81359737118724,-5.61853085805969));
#20543=CARTESIAN_POINT('Ctrl Pts',(-6.67026647830487,4.6444906828676,-5.6103090698864));
#20544=CARTESIAN_POINT('Ctrl Pts',(-6.78806530614967,4.47056096362867,-5.60208728171312));
#20545=CARTESIAN_POINT('Ctrl Pts',(-6.8989499777136,4.29233931178623,-5.59386549353983));
#20546=CARTESIAN_POINT('Ctrl Pts',(-7.00983434160183,4.11411815446185,-5.58564372817984));
#20547=CARTESIAN_POINT('Ctrl Pts',(-7.11380443407122,3.9316053402002,-5.57742196281984));
#20548=CARTESIAN_POINT('Ctrl Pts',(-7.21054586853405,3.74535924048235,-5.56920019745984));
#20549=CARTESIAN_POINT('Ctrl Pts',(-7.30730747198066,3.55907431154324,-5.5609767179982));
#20550=CARTESIAN_POINT('Ctrl Pts',(-7.39683727078198,3.36905480404923,-5.55275323853656));
#20551=CARTESIAN_POINT('Ctrl Pts',(-7.47886726874041,3.17588285978297,-5.54452975907492));
#20552=CARTESIAN_POINT('Ctrl Pts',(-7.5120104256423,3.09783424077528,-5.54120716884134));
#20553=CARTESIAN_POINT('Ctrl Pts',(-7.54392981177007,3.01927124370574,-5.53788457860777));
#20554=CARTESIAN_POINT('Ctrl Pts',(-7.57460997759708,2.94023319649765,-5.5345619883742));
#20555=CARTESIAN_POINT('Ctrl Pts',(-7.65032303275941,2.74518170746946,-5.52636244150556));
#20556=CARTESIAN_POINT('Ctrl Pts',(-7.71851174710653,2.54716866060428,-5.51816289463691));
#20557=CARTESIAN_POINT('Ctrl Pts',(-7.77896172904498,2.34679397914549,-5.50996334776827));
#20558=CARTESIAN_POINT('Ctrl Pts',(-7.83940391141622,2.14644515105746,-5.50176485884729));
#20559=CARTESIAN_POINT('Ctrl Pts',(-7.8921092654707,1.94373558132762,-5.4935663699263));
#20560=CARTESIAN_POINT('Ctrl Pts',(-7.9369131001647,1.73928088672702,-5.48536788100532));
#20561=CARTESIAN_POINT('Ctrl Pts',(-7.98171097779131,1.53485337619231,-5.47717048214618));
#20562=CARTESIAN_POINT('Ctrl Pts',(-8.01860937032492,1.32868149561549,-5.46897308328705));
#20563=CARTESIAN_POINT('Ctrl Pts',(-8.04749445669988,1.12139222927782,-5.46077568442792));
#20564=CARTESIAN_POINT('Ctrl Pts',(-8.07638215447811,0.914084222616474,
-5.45257754446959));
#20565=CARTESIAN_POINT('Ctrl Pts',(-8.09725505496413,0.705658923625393,
-5.44437940451127));
#20566=CARTESIAN_POINT('Ctrl Pts',(-8.11005094317767,0.496750703636092,
-5.43618126455294));
#20567=CARTESIAN_POINT('Ctrl Pts',(-8.12018524877937,0.33129601157046,-5.4296883619645));
#20568=CARTESIAN_POINT('Ctrl Pts',(-8.12525417993961,0.165538596538109,
-5.42319545937606));
#20569=CARTESIAN_POINT('Ctrl Pts',(-8.12524999741292,-0.000205039998872057,
-5.41670255678761));
#20570=CARTESIAN_POINT('Ctrl Pts',(-8.12515360481363,-0.000205119571382809,
-5.41670255357508));
#20571=CARTESIAN_POINT('Ctrl Pts',(-8.12549042833445,-0.341492182439963,
-5.40333268953402));
#20572=CARTESIAN_POINT('Ctrl Pts',(-8.02126726985289,-2.02671189518092,
-5.33730648318554));
#20573=CARTESIAN_POINT('Ctrl Pts',(-6.87936488829688,-4.93498266901478,
-5.21862393452961));
#20574=CARTESIAN_POINT('Ctrl Pts',(-3.69965148811969,-7.61526717037964,
-5.06065490760733));
#20575=CARTESIAN_POINT('Ctrl Pts',(0.372694242426441,-8.45818031325121,
-4.90268588068503));
#20576=CARTESIAN_POINT('Ctrl Pts',(3.3333249850863,-7.56768303558379,-4.78524786975563));
#20577=CARTESIAN_POINT('Ctrl Pts',(4.70140933544592,-6.63456619566222,-4.72046620113364));
#20578=CARTESIAN_POINT('Ctrl Pts',(4.94675083769988,-6.44587978308508,-4.70834087481909));
#20579=CARTESIAN_POINT('',(-8.12524999887038,-0.000135487633930348,-5.58329744173371));
#20580=CARTESIAN_POINT('Ctrl Pts',(-8.12524999887038,-0.000135487633930348,
-5.58329744173372));
#20581=CARTESIAN_POINT('Ctrl Pts',(-8.12524640323817,-0.215767052978142,
-5.57485194371586));
#20582=CARTESIAN_POINT('Ctrl Pts',(-8.11665467706683,-0.431363576694395,
-5.56640644569801));
#20583=CARTESIAN_POINT('Ctrl Pts',(-8.09950915629719,-0.646249943565126,
-5.55796094768016));
#20584=CARTESIAN_POINT('Ctrl Pts',(-8.08235819985755,-0.861204436181145,
-5.54951277217348));
#20585=CARTESIAN_POINT('Ctrl Pts',(-8.0566480513228,-1.07544806406917,-5.5410645966668));
#20586=CARTESIAN_POINT('Ctrl Pts',(-8.0224649720171,-1.28831026358508,-5.53261642116012));
#20587=CARTESIAN_POINT('Ctrl Pts',(-8.00985897584013,-1.36680933762468,
-5.52950091283546));
#20588=CARTESIAN_POINT('Ctrl Pts',(-7.99610118526879,-1.44512061066931,
-5.52638540451079));
#20589=CARTESIAN_POINT('Ctrl Pts',(-7.98119769287493,-1.52321073714307,
-5.52326989618613));
#20590=CARTESIAN_POINT('Ctrl Pts',(-7.94185918394878,-1.72933350730643,
-5.51504635711217));
#20591=CARTESIAN_POINT('Ctrl Pts',(-7.89452501494402,-1.93396500526429,
-5.50682281803822));
#20592=CARTESIAN_POINT('Ctrl Pts',(-7.83933305352944,-2.13647954315989,
-5.49859927896427));
#20593=CARTESIAN_POINT('Ctrl Pts',(-7.78415112697202,-2.33895726039526,
-5.49037723507254));
#20594=CARTESIAN_POINT('Ctrl Pts',(-7.7211143370056,-2.53931850136954,-5.48215519118081));
#20595=CARTESIAN_POINT('Ctrl Pts',(-7.65041096056426,-2.73695080280561,
-5.47393314728908));
#20596=CARTESIAN_POINT('Ctrl Pts',(-7.57971539033323,-2.93456128407708,
-5.46571201117584));
#20597=CARTESIAN_POINT('Ctrl Pts',(-7.50135502284532,-3.12944314974693,
-5.45749087506261));
#20598=CARTESIAN_POINT('Ctrl Pts',(-7.4155672887339,-3.32100125696448,-5.44926973894936));
#20599=CARTESIAN_POINT('Ctrl Pts',(-7.32977275036152,-3.51257455762857,
-5.44104795077606));
#20600=CARTESIAN_POINT('Ctrl Pts',(-7.23654978641785,-3.70082330282996,
-5.43282616260275));
#20601=CARTESIAN_POINT('Ctrl Pts',(-7.13618349425367,-3.88517344514264,
-5.42460437442944));
#20602=CARTESIAN_POINT('Ctrl Pts',(-7.03581748057934,-4.06952307593254,
-5.41638260906941));
#20603=CARTESIAN_POINT('Ctrl Pts',(-6.92830832172635,-4.2499738677314,-5.40816084370939));
#20604=CARTESIAN_POINT('Ctrl Pts',(-6.81398674836912,-4.425976971873,-5.39993907834937));
#20605=CARTESIAN_POINT('Ctrl Pts',(-6.69964134086152,-4.60201676974024,
-5.39171559888774));
#20606=CARTESIAN_POINT('Ctrl Pts',(-6.57848084223118,-4.77360678015207,
-5.38349211942612));
#20607=CARTESIAN_POINT('Ctrl Pts',(-6.45087953845506,-4.94022679062833,
-5.3752686399645));
#20608=CARTESIAN_POINT('Ctrl Pts',(-6.39932388641089,-5.00754744511616,
-5.37194604973094));
#20609=CARTESIAN_POINT('Ctrl Pts',(-6.34671727864032,-5.0740571176318,-5.36862345949738));
#20610=CARTESIAN_POINT('Ctrl Pts',(-6.29308631040874,-5.13972297427071,
-5.36530086926382));
#20611=CARTESIAN_POINT('Ctrl Pts',(-6.16034759397832,-5.30224850403392,
-5.35707733018986));
#20612=CARTESIAN_POINT('Ctrl Pts',(-6.02128786593954,-5.45965551007142,
-5.3488537911159));
#20613=CARTESIAN_POINT('Ctrl Pts',(-5.8763262848951,-5.61145943190815,-5.34063025204194));
#20614=CARTESIAN_POINT('Ctrl Pts',(-5.73139106038399,-5.76323575315515,
-5.33240820815022));
#20615=CARTESIAN_POINT('Ctrl Pts',(-5.58055632815796,-5.90941081028956,
-5.3241861642585));
#20616=CARTESIAN_POINT('Ctrl Pts',(-5.42427927792612,-6.04953567454241,
-5.31596412036679));
#20617=CARTESIAN_POINT('Ctrl Pts',(-5.2680194819138,-6.18964506790452,-5.30774298425359));
#20618=CARTESIAN_POINT('Ctrl Pts',(-5.10631878702397,-6.32370540518375,
-5.29952184814041));
#20619=CARTESIAN_POINT('Ctrl Pts',(-4.93966935972606,-6.45130639321088,
-5.29130071202721));
#20620=CARTESIAN_POINT('Ctrl Pts',(-4.77300671461452,-6.57891750192132,
-5.28307892385391));
#20621=CARTESIAN_POINT('Ctrl Pts',(-4.60139478539431,-6.7000680562976,-5.2748571356806));
#20622=CARTESIAN_POINT('Ctrl Pts',(-4.4253576102235,-6.81438901033225,-5.26663534750729));
#20623=CARTESIAN_POINT('Ctrl Pts',(-4.24932092350857,-6.92870964715696,
-5.25841358214723));
#20624=CARTESIAN_POINT('Ctrl Pts',(-4.06885926422392,-7.03620056317625,
-5.25019181678718));
#20625=CARTESIAN_POINT('Ctrl Pts',(-3.88452480031184,-7.13653659965829,
-5.24197005142712));
#20626=CARTESIAN_POINT('Ctrl Pts',(-3.70015190572471,-7.23689355453795,
-5.23374657196551));
#20627=CARTESIAN_POINT('Ctrl Pts',(-3.51190485261628,-7.33009250891737,
-5.22552309250389));
#20628=CARTESIAN_POINT('Ctrl Pts',(-3.32036047463938,-7.41585422462932,
-5.21729961304227));
#20629=CARTESIAN_POINT('Ctrl Pts',(-3.2429694526841,-7.45050513369639,-5.21397702280869));
#20630=CARTESIAN_POINT('Ctrl Pts',(-3.16504041072694,-7.48394248016693,
-5.21065443257512));
#20631=CARTESIAN_POINT('Ctrl Pts',(-3.08661236960116,-7.51615005453757,
-5.20733184234154));
#20632=CARTESIAN_POINT('Ctrl Pts',(-2.89249994063715,-7.59586504425786,
-5.19910830326758));
#20633=CARTESIAN_POINT('Ctrl Pts',(-2.69526624876149,-7.66806922904659,
-5.19088476419362));
#20634=CARTESIAN_POINT('Ctrl Pts',(-2.49551061114153,-7.73253608799727,
-5.18266122511966));
#20635=CARTESIAN_POINT('Ctrl Pts',(-2.29579129256633,-7.79699122575317,
-5.17443918122795));
#20636=CARTESIAN_POINT('Ctrl Pts',(-2.09355122396812,-7.85371175490497,
-5.16621713733624));
#20637=CARTESIAN_POINT('Ctrl Pts',(-1.88940619951778,-7.90252059634923,
-5.15799509344453));
#20638=CARTESIAN_POINT('Ctrl Pts',(-1.68528371428788,-7.95132404891252,
-5.14977395733129));
#20639=CARTESIAN_POINT('Ctrl Pts',(-1.47925697984454,-7.99221748914817,
-5.14155282121806));
#20640=CARTESIAN_POINT('Ctrl Pts',(-1.27195415117231,-8.02507446693272,
-5.13333168510483));
#20641=CARTESIAN_POINT('Ctrl Pts',(-1.06463488025978,-8.05793405077108,
-5.12510989693153));
#20642=CARTESIAN_POINT('Ctrl Pts',(-0.856039603776485,-8.08275584976062,
-5.11688810875824));
#20643=CARTESIAN_POINT('Ctrl Pts',(-0.646804863534513,-8.09946486077988,
-5.10866632058494));
#20644=CARTESIAN_POINT('Ctrl Pts',(-0.437570703863254,-8.11617382543609,
-5.10044455522492));
#20645=CARTESIAN_POINT('Ctrl Pts',(-0.227697378193396,-8.12477002636174,
-5.0922227898649));
#20646=CARTESIAN_POINT('Ctrl Pts',(-0.0178252675763609,-8.12523044733722,
-5.08400102450488));
#20647=CARTESIAN_POINT('Ctrl Pts',(0.192090597892018,-8.12569096430283,
-5.07577754504326));
#20648=CARTESIAN_POINT('Ctrl Pts',(0.402004952816498,-8.1180123121998,-5.06755406558164));
#20649=CARTESIAN_POINT('Ctrl Pts',(0.611277591239238,-8.1022236002809,-5.05933058612001));
#20650=CARTESIAN_POINT('Ctrl Pts',(0.695831486926034,-8.09584437597962,
-5.05600799588642));
#20651=CARTESIAN_POINT('Ctrl Pts',(0.780280656271626,-8.08814181041789,
-5.05268540565284));
#20652=CARTESIAN_POINT('Ctrl Pts',(0.864583067615009,-8.07912022943671,
-5.04936281541925));
#20653=CARTESIAN_POINT('Ctrl Pts',(1.07323478960695,-8.05679146829194,-5.04113927634528));
#20654=CARTESIAN_POINT('Ctrl Pts',(1.28105494401805,-8.02637178827214,-5.03291573727132));
#20655=CARTESIAN_POINT('Ctrl Pts',(1.48740865519046,-7.98794736180481,-5.02469219819735));
#20656=CARTESIAN_POINT('Ctrl Pts',(1.69372484767351,-7.94952992156571,-5.01647015430565));
#20657=CARTESIAN_POINT('Ctrl Pts',(1.89857483926335,-7.90311069365899,-5.00824811041394));
#20658=CARTESIAN_POINT('Ctrl Pts',(2.1013328068858,-7.84882717335561,-5.00002606652223));
#20659=CARTESIAN_POINT('Ctrl Pts',(2.30406838842982,-7.79454964638092,-4.99180493040901));
#20660=CARTESIAN_POINT('Ctrl Pts',(2.50471212235133,-7.73240963674396,-4.98358379429578));
#20661=CARTESIAN_POINT('Ctrl Pts',(2.70265142306076,-7.66259504658361,-4.97536265818255));
#20662=CARTESIAN_POINT('Ctrl Pts',(2.9006064233417,-7.59277491907344,-4.96714087000925));
#20663=CARTESIAN_POINT('Ctrl Pts',(3.09585628278475,-7.5152790903875,-4.95891908183595));
#20664=CARTESIAN_POINT('Ctrl Pts',(3.28780553736328,-7.43034469664654,-4.95069729366265));
#20665=CARTESIAN_POINT('Ctrl Pts',(3.47975425933399,-7.34541053857579,-4.94247552830262));
#20666=CARTESIAN_POINT('Ctrl Pts',(3.66840212614289,-7.25303797854477,-4.93425376294258));
#20667=CARTESIAN_POINT('Ctrl Pts',(3.85317505138024,-7.15351169607773,-4.92603199758255));
#20668=CARTESIAN_POINT('Ctrl Pts',(4.03798649870529,-7.05396466403292,-4.91780851812091));
#20669=CARTESIAN_POINT('Ctrl Pts',(4.21892113087728,-6.94726106998677,-4.90958503865928));
#20670=CARTESIAN_POINT('Ctrl Pts',(4.39542983513849,-6.83373134728564,-4.90136155919765));
#20671=CARTESIAN_POINT('Ctrl Pts',(4.46674588811264,-6.78786113509309,-4.89803896896409));
#20672=CARTESIAN_POINT('Ctrl Pts',(4.53733973621985,-6.74087709175163,-4.89471637873052));
#20673=CARTESIAN_POINT('Ctrl Pts',(4.60717647814807,-6.6928030347306,-4.89139378849695));
#20674=CARTESIAN_POINT('Ctrl Pts',(4.7224576576741,-6.61344603947325,-4.88590910936343));
#20675=CARTESIAN_POINT('Ctrl Pts',(4.8357005107187,-6.53110121115441,-4.8804244302299));
#20676=CARTESIAN_POINT('Ctrl Pts',(4.94675008185375,-6.44587862049697,-4.87493975109638));
#20677=CARTESIAN_POINT('Ctrl Pts',(4.94635656996294,-6.445366250073,-6.87494113799973));
#20678=CARTESIAN_POINT('Ctrl Pts',(5.53980426391237,-5.98964994661794,-6.84563479585463));
#20679=CARTESIAN_POINT('Ctrl Pts',(7.02552761858039,-4.48811509720809,-6.76367211140211));
#20680=CARTESIAN_POINT('Ctrl Pts',(8.37906827853382,-1.21281902750414,-6.62905308464214));
#20681=CARTESIAN_POINT('Ctrl Pts',(7.94572663628765,2.92320772973764,-6.47108405771986));
#20682=CARTESIAN_POINT('Ctrl Pts',(5.59528212459546,6.35393839724545,-6.31311503079756));
#20683=CARTESIAN_POINT('Ctrl Pts',(1.89483755533364,8.25162443696425,-6.15514600387528));
#20684=CARTESIAN_POINT('Ctrl Pts',(-2.26278339070844,8.15840220487702,-5.99717697695297));
#20685=CARTESIAN_POINT('Ctrl Pts',(-5.87445193619213,6.09676386775613,-5.8392079500307));
#20686=CARTESIAN_POINT('Ctrl Pts',(-7.79082080228488,3.01159239845082,-5.70124810545049));
#20687=CARTESIAN_POINT('Ctrl Pts',(-8.12422248499541,0.833362078616152,
-5.61594460317773));
#20688=CARTESIAN_POINT('Ctrl Pts',(-8.12472295983679,-0.000135441094342992,
-5.58329744321239));
#20689=CARTESIAN_POINT('Origin',(0.,0.,-16.4167025567876));
#20690=CARTESIAN_POINT('',(4.94675008185375,-6.44587862049697,-8.87494907190769));
#20691=CARTESIAN_POINT('',(4.94707560568286,-6.44630337360393,-8.7083535696852));
#20692=CARTESIAN_POINT('',(4.94675008185374,-6.44587862049697,-16.4167025567876));
#20693=CARTESIAN_POINT('',(-8.12525269526789,0.000111890383953636,-7.41670255678762));
#20694=CARTESIAN_POINT('Ctrl Pts',(4.94707560569883,-6.44630337359169,-8.70835356968441));
#20695=CARTESIAN_POINT('Ctrl Pts',(5.04438551388885,-6.37173728721331,-8.70354988872961));
#20696=CARTESIAN_POINT('Ctrl Pts',(6.18791126886723,-5.45321389914109,-8.64608986546737));
#20697=CARTESIAN_POINT('Ctrl Pts',(7.8789657040664,-3.09864722800698,-8.5359734998977));
#20698=CARTESIAN_POINT('Ctrl Pts',(8.40389718874569,1.02675569189956,-8.37800447297542));
#20699=CARTESIAN_POINT('Ctrl Pts',(6.90118083796468,4.90442843270839,-8.22003544605311));
#20700=CARTESIAN_POINT('Ctrl Pts',(3.73338409962977,7.59878663829889,-8.06206641913084));
#20701=CARTESIAN_POINT('Ctrl Pts',(-0.335183795052036,8.45974982096853,
-7.90409739220853));
#20702=CARTESIAN_POINT('Ctrl Pts',(-4.32288031764655,7.27958934069048,-7.74612836528627));
#20703=CARTESIAN_POINT('Ctrl Pts',(-7.26757515637083,4.34304807207066,-7.58815933836395));
#20704=CARTESIAN_POINT('Ctrl Pts',(-8.09561982062734,1.57337616034462,-7.47835073553109));
#20705=CARTESIAN_POINT('Ctrl Pts',(-8.1258799154099,0.114850934707135,-7.42119847500564));
#20706=CARTESIAN_POINT('Ctrl Pts',(-8.12580188385528,0.000111897946662807,
-7.41670255678762));
#20707=CARTESIAN_POINT('Ctrl Pts',(-8.1252499992296,0.000111890346827312,
-7.41670255678762));
#20708=CARTESIAN_POINT('Ctrl Pts',(-8.12525288020884,-0.209098977576592,
-7.40850431079129));
#20709=CARTESIAN_POINT('Ctrl Pts',(-8.1171712012911,-0.418345744962354,
-7.40030606479496));
#20710=CARTESIAN_POINT('Ctrl Pts',(-8.101022710918,-0.626991706237579,-7.39210781879863));
#20711=CARTESIAN_POINT('Ctrl Pts',(-8.0848770728534,-0.835600814368282,
-7.38391102085881));
#20712=CARTESIAN_POINT('Ctrl Pts',(-8.06066749005515,-1.04360903066591,
-7.375714222919));
#20713=CARTESIAN_POINT('Ctrl Pts',(-8.02846370555508,-1.25038317770383,
-7.36751742497919));
#20714=CARTESIAN_POINT('Ctrl Pts',(-7.99625877375556,-1.45716469132523,
-7.35932033501836));
#20715=CARTESIAN_POINT('Ctrl Pts',(-7.95605911297337,-1.66271175218541,
-7.35112324505753));
#20716=CARTESIAN_POINT('Ctrl Pts',(-7.90798604134617,-1.86639876027982,
-7.34292615509671));
#20717=CARTESIAN_POINT('Ctrl Pts',(-7.85991515707825,-2.07007650046912,
-7.33472943810936));
#20718=CARTESIAN_POINT('Ctrl Pts',(-7.80397164799632,-2.27189406677244,
-7.32653272112201));
#20719=CARTESIAN_POINT('Ctrl Pts',(-7.74032753703739,-2.47123798568261,
-7.31833600413466));
#20720=CARTESIAN_POINT('Ctrl Pts',(-7.67666767317294,-2.67063124530748,
-7.3101372583326));
#20721=CARTESIAN_POINT('Ctrl Pts',(-7.60530348806353,-2.86754934899659,
-7.30193851253055));
#20722=CARTESIAN_POINT('Ctrl Pts',(-7.52645666268727,-3.06139472580561,
-7.29373976672849));
#20723=CARTESIAN_POINT('Ctrl Pts',(-7.4574760303618,-3.23098400986169,-7.28656693932545));
#20724=CARTESIAN_POINT('Ctrl Pts',(-7.38276901200279,-3.39822157489473,
-7.27939411192241));
#20725=CARTESIAN_POINT('Ctrl Pts',(-7.30251417390863,-3.56272007072735,
-7.27222128451937));
#20726=CARTESIAN_POINT('Ctrl Pts',(-7.21050320531049,-3.75131512984065,
-7.26399774544542));
#20727=CARTESIAN_POINT('Ctrl Pts',(-7.11116739137222,-3.93637449756095,
-7.25577420637147));
#20728=CARTESIAN_POINT('Ctrl Pts',(-7.00480384180409,-4.11733053085936,
-7.24755066729751));
#20729=CARTESIAN_POINT('Ctrl Pts',(-6.89845963097652,-4.2982536632082,-7.23932862340579));
#20730=CARTESIAN_POINT('Ctrl Pts',(-6.78509038416978,-4.47507469604229,
-7.23110657951406));
#20731=CARTESIAN_POINT('Ctrl Pts',(-6.66503838876746,-4.6472519663513,-7.22288453562233));
#20732=CARTESIAN_POINT('Ctrl Pts',(-6.54499964805273,-4.81941022693107,
-7.21466339950913));
#20733=CARTESIAN_POINT('Ctrl Pts',(-6.41827980041197,-4.98692550675144,
-7.20644226339592));
#20734=CARTESIAN_POINT('Ctrl Pts',(-6.28526402526786,-5.14928574611796,
-7.19822112728272));
#20735=CARTESIAN_POINT('Ctrl Pts',(-6.15223769996644,-5.31165886310043,
-7.18999933910942));
#20736=CARTESIAN_POINT('Ctrl Pts',(-6.01291463425759,-5.46887589283249,
-7.18177755093612));
#20737=CARTESIAN_POINT('Ctrl Pts',(-5.86772047478252,-5.6204576319298,-7.17355576276282));
#20738=CARTESIAN_POINT('Ctrl Pts',(-5.72252671818263,-5.77203895042811,
-7.16533399740279));
#20739=CARTESIAN_POINT('Ctrl Pts',(-5.57146210636364,-5.91798479844755,
-7.15711223204277));
#20740=CARTESIAN_POINT('Ctrl Pts',(-5.4149897149768,-6.05785225547764,-7.14889046668274));
#20741=CARTESIAN_POINT('Ctrl Pts',(-5.25848470169381,-6.19774887255069,
-7.14066698722112));
#20742=CARTESIAN_POINT('Ctrl Pts',(-5.09656987648587,-6.33156437045485,
-7.1324435077595));
#20743=CARTESIAN_POINT('Ctrl Pts',(-4.92974283735278,-6.45889488380706,
-7.12422002829788));
#20744=CARTESIAN_POINT('Ctrl Pts',(-4.86233853562022,-6.51034112649261,
-7.12089743806429));
#20745=CARTESIAN_POINT('Ctrl Pts',(-4.79413270582646,-6.56072918560938,
-7.1175748478307));
#20746=CARTESIAN_POINT('Ctrl Pts',(-4.72515962225625,-6.61003434988799,
-7.11425225759711));
#20747=CARTESIAN_POINT('Ctrl Pts',(-4.55444857818667,-6.73206653456559,
-7.10602871852314));
#20748=CARTESIAN_POINT('Ctrl Pts',(-4.37897986752514,-6.84750181985908,
-7.09780517944917));
#20749=CARTESIAN_POINT('Ctrl Pts',(-4.19928504217936,-6.9559825112653,-7.0895816403752));
#20750=CARTESIAN_POINT('Ctrl Pts',(-4.01962288847436,-7.06444347899736,
-7.08135959648349));
#20751=CARTESIAN_POINT('Ctrl Pts',(-3.83573640605279,-7.16595222421921,
-7.07313755259177));
#20752=CARTESIAN_POINT('Ctrl Pts',(-3.64818450392634,-7.26019540975391,
-7.06491550870006));
#20753=CARTESIAN_POINT('Ctrl Pts',(-3.46065330900949,-7.35442819009744,
-7.05669437258686));
#20754=CARTESIAN_POINT('Ctrl Pts',(-3.26945776577081,-7.44139687989461,
-7.04847323647366));
#20755=CARTESIAN_POINT('Ctrl Pts',(-3.07518040518192,-7.52083459717638,
-7.04025210036045));
#20756=CARTESIAN_POINT('Ctrl Pts',(-2.88088763546822,-7.60027861506721,
-7.03203031218717));
#20757=CARTESIAN_POINT('Ctrl Pts',(-2.68351283200177,-7.67219035286242,
-7.02380852401388));
#20758=CARTESIAN_POINT('Ctrl Pts',(-2.48365846649581,-7.73635108977764,
-7.01558673584059));
#20759=CARTESIAN_POINT('Ctrl Pts',(-2.28380465553227,-7.80051164866398,
-7.00736497048057));
#20760=CARTESIAN_POINT('Ctrl Pts',(-2.08147157793189,-7.85692116210695,
-6.99914320512054));
#20761=CARTESIAN_POINT('Ctrl Pts',(-1.87727734289502,-7.90541063704808,
-6.99092143976052));
#20762=CARTESIAN_POINT('Ctrl Pts',(-1.67304053675,-7.95391022123976,-6.9826979602989));
#20763=CARTESIAN_POINT('Ctrl Pts',(-1.46694208501947,-7.99448640015824,
-6.97447448083729));
#20764=CARTESIAN_POINT('Ctrl Pts',(-1.25961185836555,-8.02702096227267,
-6.96625100137568));
#20765=CARTESIAN_POINT('Ctrl Pts',(-1.17584276896352,-8.04016613018381,
-6.96292841114206));
#20766=CARTESIAN_POINT('Ctrl Pts',(-1.09187270262411,-8.05199912128946,
-6.95960582090843));
#20767=CARTESIAN_POINT('Ctrl Pts',(-1.00774356520918,-8.06251452521355,
-6.95628323067481));
#20768=CARTESIAN_POINT('Ctrl Pts',(-0.799520702880655,-8.08854055580051,
-6.94805969160085));
#20769=CARTESIAN_POINT('Ctrl Pts',(-0.590255257323399,-8.10650014398112,
-6.93983615252689));
#20770=CARTESIAN_POINT('Ctrl Pts',(-0.380584972611504,-8.11633184641451,
-6.93161261345293));
#20771=CARTESIAN_POINT('Ctrl Pts',(-0.170952809599473,-8.1261617612736,
-6.92339056956122));
#20772=CARTESIAN_POINT('Ctrl Pts',(0.0390837511913653,-8.1278667260791,
-6.91516852566952));
#20773=CARTESIAN_POINT('Ctrl Pts',(0.248884029729575,-8.12143732982319,
-6.90694648177781));
#20774=CARTESIAN_POINT('Ctrl Pts',(0.458661144662935,-8.11500864342331,
-6.89872534566457));
#20775=CARTESIAN_POINT('Ctrl Pts',(0.668201734744688,-8.10044739801135,
-6.89050420955133));
#20776=CARTESIAN_POINT('Ctrl Pts',(0.876866467443997,-8.07779628121261,
-6.8822830734381));
#20777=CARTESIAN_POINT('Ctrl Pts',(1.08554775040333,-8.05514336783872,-6.87406128526479));
#20778=CARTESIAN_POINT('Ctrl Pts',(1.29335274366877,-8.02439933020023,-6.86583949709148));
#20779=CARTESIAN_POINT('Ctrl Pts',(1.49964751164141,-7.98565870190604,-6.85761770891817));
#20780=CARTESIAN_POINT('Ctrl Pts',(1.70594170720096,-7.94691818110679,-6.84939594355814));
#20781=CARTESIAN_POINT('Ctrl Pts',(1.91072539648266,-7.90018117112124,-6.8411741781981));
#20782=CARTESIAN_POINT('Ctrl Pts',(2.11337457085352,-7.84559338009367,-6.83295241283807));
#20783=CARTESIAN_POINT('Ctrl Pts',(2.31606599421294,-7.79099420841792,-6.82472893337645));
#20784=CARTESIAN_POINT('Ctrl Pts',(2.51662172882447,-7.72854106265373,-6.81650545391484));
#20785=CARTESIAN_POINT('Ctrl Pts',(2.71443160322337,-7.65842990657499,-6.80828197445322));
#20786=CARTESIAN_POINT('Ctrl Pts',(2.79435411775613,-7.63010240316981,-6.80495938421965));
#20787=CARTESIAN_POINT('Ctrl Pts',(2.87382856745068,-7.60052532479736,-6.80163679398608));
#20788=CARTESIAN_POINT('Ctrl Pts',(2.95281552569261,-7.56971386736174,-6.79831420375251));
#20789=CARTESIAN_POINT('Ctrl Pts',(3.14831395442207,-7.49345328397432,-6.79009055285581));
#20790=CARTESIAN_POINT('Ctrl Pts',(3.34088825448533,-7.40960273717027,-6.78186690195911));
#20791=CARTESIAN_POINT('Ctrl Pts',(3.52994833722337,-7.31841187000527,-6.7736432510624));
#20792=CARTESIAN_POINT('Ctrl Pts',(3.71897116032074,-7.2272389745818,-6.76542122086888));
#20793=CARTESIAN_POINT('Ctrl Pts',(3.90448088313136,-7.12872877469039,-6.75719919067535));
#20794=CARTESIAN_POINT('Ctrl Pts',(4.08590963763387,-7.023178055239,-6.74897716048182));
#20795=CARTESIAN_POINT('Ctrl Pts',(4.26732931736639,-6.9176326152622,-6.74075554154082));
#20796=CARTESIAN_POINT('Ctrl Pts',(4.44466818034,-6.80504750518394,-6.73253392259982));
#20797=CARTESIAN_POINT('Ctrl Pts',(4.61738425291033,-6.68576474484974,-6.72431230365881));
#20798=CARTESIAN_POINT('Ctrl Pts',(4.72915507392777,-6.60857255388933,-6.71899179650824));
#20799=CARTESIAN_POINT('Ctrl Pts',(4.83899047307838,-6.52857640072433,-6.71367128935767));
#20800=CARTESIAN_POINT('Ctrl Pts',(4.94675008185374,-6.44587862049698,-6.70835078220711));
#20801=CARTESIAN_POINT('',(-8.12530198328732,-5.60780087209094E-5,-7.58329744321239));
#20802=CARTESIAN_POINT('Ctrl Pts',(-8.125900459786,-5.60821392014618E-5,
-7.58329744321239));
#20803=CARTESIAN_POINT('Ctrl Pts',(-8.12592100724276,-0.0547552239322313,
-7.58115404420023));
#20804=CARTESIAN_POINT('Ctrl Pts',(-8.11209200002685,-1.4532239507054,-7.52635430288063));
#20805=CARTESIAN_POINT('Ctrl Pts',(-7.36207492018725,-4.18085733783256,
-7.41889821925358));
#20806=CARTESIAN_POINT('Ctrl Pts',(-4.48320742627557,-7.18196117942933,
-7.2609291923313));
#20807=CARTESIAN_POINT('Ctrl Pts',(-0.522655372263062,-8.45023943871622,
-7.10296016540901));
#20808=CARTESIAN_POINT('Ctrl Pts',(2.80584571694962,-7.82264088224354,-6.97429748063182));
#20809=CARTESIAN_POINT('Ctrl Pts',(4.47352363566336,-6.80846089037195,-6.89829113816206));
#20810=CARTESIAN_POINT('Ctrl Pts',(4.94635656996294,-6.445366250073,-6.87494113799973));
#20811=CARTESIAN_POINT('Ctrl Pts',(4.94675008185375,-6.44587862049697,-8.87494907190769));
#20812=CARTESIAN_POINT('Ctrl Pts',(5.11327935064553,-6.31807933625242,-8.86672559489486));
#20813=CARTESIAN_POINT('Ctrl Pts',(5.27483796520581,-6.18383505470868,-8.85850211788203));
#20814=CARTESIAN_POINT('Ctrl Pts',(5.43093669428508,-6.04355972793914,-8.8502786408692));
#20815=CARTESIAN_POINT('Ctrl Pts',(5.49205381107422,-5.98863792569657,-8.84705891443087));
#20816=CARTESIAN_POINT('Ctrl Pts',(5.55233432452382,-5.93279202427241,-8.84383918799255));
#20817=CARTESIAN_POINT('Ctrl Pts',(5.61175033476285,-5.87604848029601,-8.84061946155422));
#20818=CARTESIAN_POINT('Ctrl Pts',(5.76350542534024,-5.73111916543326,-8.83239592255661));
#20819=CARTESIAN_POINT('Ctrl Pts',(5.90966773813315,-5.58028431867139,-8.82417238355901));
#20820=CARTESIAN_POINT('Ctrl Pts',(6.04978663715039,-5.42399937384368,-8.8159488445614));
#20821=CARTESIAN_POINT('Ctrl Pts',(6.18988006009988,-5.26774284435372,-8.80772680074709));
#20822=CARTESIAN_POINT('Ctrl Pts',(6.32393206556385,-5.10603841405696,-8.79950475693277));
#20823=CARTESIAN_POINT('Ctrl Pts',(6.45153048813366,-4.93937667354716,-8.79128271311846));
#20824=CARTESIAN_POINT('Ctrl Pts',(6.57911482282054,-4.77273333382196,-8.78306157708332));
#20825=CARTESIAN_POINT('Ctrl Pts',(6.70024681792474,-4.60113401069098,-8.77484044104818));
#20826=CARTESIAN_POINT('Ctrl Pts',(6.81455553689492,-4.42510117365409,-8.76661930501304));
#20827=CARTESIAN_POINT('Ctrl Pts',(6.92887332226324,-4.24905437456951,-8.75839751691835));
#20828=CARTESIAN_POINT('Ctrl Pts',(7.03636658730184,-4.06857360488389,-8.75017572882365));
#20829=CARTESIAN_POINT('Ctrl Pts',(7.13670798750923,-3.88420991496622,-8.74195394072896));
#20830=CARTESIAN_POINT('Ctrl Pts',(7.23704910929327,-3.69984673661364,-8.73373217544775));
#20831=CARTESIAN_POINT('Ctrl Pts',(7.33023826732112,-3.51160091992,-8.72551041016656));
#20832=CARTESIAN_POINT('Ctrl Pts',(7.41599405146985,-3.32004816095548,-8.71728864488535));
#20833=CARTESIAN_POINT('Ctrl Pts',(7.50176771427936,-3.12845546641303,-8.70906516550225));
#20834=CARTESIAN_POINT('Ctrl Pts',(7.58010478674925,-2.93355472152726,-8.70084168611915));
#20835=CARTESIAN_POINT('Ctrl Pts',(7.65077155198343,-2.73594265690293,-8.69261820673605));
#20836=CARTESIAN_POINT('Ctrl Pts',(7.67932354635531,-2.65610005284044,-8.68929561603467));
#20837=CARTESIAN_POINT('Ctrl Pts',(7.70662394838959,-2.57581504928362,-8.68597302533329));
#20838=CARTESIAN_POINT('Ctrl Pts',(7.73265961988366,-2.49512780544818,-8.68265043463192));
#20839=CARTESIAN_POINT('Ctrl Pts',(7.79709890303887,-2.2954237896056,-8.67442689551314));
#20840=CARTESIAN_POINT('Ctrl Pts',(7.85380817147139,-2.09318968547407,-8.66620335639438));
#20841=CARTESIAN_POINT('Ctrl Pts',(7.90260800874881,-1.88904055609168,-8.65797981727561));
#20842=CARTESIAN_POINT('Ctrl Pts',(7.95139897337147,-1.68492854455323,-8.64975777333853));
#20843=CARTESIAN_POINT('Ctrl Pts',(7.99228330852968,-1.47890248941189,-8.64153572940146));
#20844=CARTESIAN_POINT('Ctrl Pts',(8.02513216736883,-1.2715900513774,-8.63331368546439));
#20845=CARTESIAN_POINT('Ctrl Pts',(8.05797739943628,-1.06430050226239,-8.62509254930547));
#20846=CARTESIAN_POINT('Ctrl Pts',(8.08278888026715,-0.855725144992614,
-8.61687141314655));
#20847=CARTESIAN_POINT('Ctrl Pts',(8.09948919734929,-0.646500042167216,
-8.60865027698762));
#20848=CARTESIAN_POINT('Ctrl Pts',(8.11619083901902,-0.437258344628318,
-8.60042848876833));
#20849=CARTESIAN_POINT('Ctrl Pts',(8.12478000538259,-0.227367092360067,
-8.59220670054903));
#20850=CARTESIAN_POINT('Ctrl Pts',(8.12523122600442,-0.0174667244402944,
-8.58398491232973));
#20851=CARTESIAN_POINT('Ctrl Pts',(8.12568244537425,0.192433061064505,-8.5757631469236));
#20852=CARTESIAN_POINT('Ctrl Pts',(8.11799576623392,0.402341667233051,-8.56754138151748));
#20853=CARTESIAN_POINT('Ctrl Pts',(8.10219784624027,0.611618854254461,-8.55931961611135));
#20854=CARTESIAN_POINT('Ctrl Pts',(8.08639663264302,0.820939672089145,-8.55109613660386));
#20855=CARTESIAN_POINT('Ctrl Pts',(8.0624808221466,1.02962851364811,-8.54287265709637));
#20856=CARTESIAN_POINT('Ctrl Pts',(8.03052902769919,1.23704935139254,-8.53464917758888));
#20857=CARTESIAN_POINT('Ctrl Pts',(8.01761932064266,1.32085504365521,-8.53132658762913));
#20858=CARTESIAN_POINT('Ctrl Pts',(8.00339836093629,1.40445381659858,-8.52800399766938));
#20859=CARTESIAN_POINT('Ctrl Pts',(7.98787371724669,1.48780409994712,-8.52468140770963));
#20860=CARTESIAN_POINT('Ctrl Pts',(7.94944962182064,1.69409928489361,-8.51645786865599));
#20861=CARTESIAN_POINT('Ctrl Pts',(7.90302333210066,1.89893866810336,-8.50823432960235));
#20862=CARTESIAN_POINT('Ctrl Pts',(7.84872993986047,2.10169595651651,-8.50001079054871));
#20863=CARTESIAN_POINT('Ctrl Pts',(7.79444641910373,2.30441638012652,-8.49178874667757));
#20864=CARTESIAN_POINT('Ctrl Pts',(7.73229872694468,2.50505517974816,-8.48356670280642));
#20865=CARTESIAN_POINT('Ctrl Pts',(7.66247242256954,2.70299906323721,-8.47534465893528));
#20866=CARTESIAN_POINT('Ctrl Pts',(7.59265382757021,2.90092109215727,-8.46712352284276));
#20867=CARTESIAN_POINT('Ctrl Pts',(7.51515841099195,3.09614852094415,-8.45890238675023));
#20868=CARTESIAN_POINT('Ctrl Pts',(7.43022096204239,3.28808515974356,-8.45068125065771));
#20869=CARTESIAN_POINT('Ctrl Pts',(7.34527677627344,3.48003702201021,-8.44245946250523));
#20870=CARTESIAN_POINT('Ctrl Pts',(7.25288949566177,3.66869730198269,-8.43423767435275));
#20871=CARTESIAN_POINT('Ctrl Pts',(7.15334166920894,3.85349069365154,-8.42601588620027));
#20872=CARTESIAN_POINT('Ctrl Pts',(7.05379411897472,4.03828357256813,-8.41779412086105));
#20873=CARTESIAN_POINT('Ctrl Pts',(6.94708620489238,4.21920932626937,-8.40957235552184));
#20874=CARTESIAN_POINT('Ctrl Pts',(6.83354622057933,4.39571764490235,-8.40135059018262));
#20875=CARTESIAN_POINT('Ctrl Pts',(6.71998256506317,4.57226276259153,-8.39312711074173));
#20876=CARTESIAN_POINT('Ctrl Pts',(6.59958415341269,4.74438835730398,-8.38490363130084));
#20877=CARTESIAN_POINT('Ctrl Pts',(6.47272296110334,4.91157256195056,-8.37668015185995));
#20878=CARTESIAN_POINT('Ctrl Pts',(6.42146633945766,4.97912117446721,-8.37335756150241));
#20879=CARTESIAN_POINT('Ctrl Pts',(6.36915517613709,5.04586347326246,-8.37003497114487));
#20880=CARTESIAN_POINT('Ctrl Pts',(6.31581592055058,5.11176650681736,-8.36671238078733));
#20881=CARTESIAN_POINT('Ctrl Pts',(6.18379920899772,5.27487905264517,-8.35848884170685));
#20882=CARTESIAN_POINT('Ctrl Pts',(6.04543885049741,5.4329011548279,-8.35026530262637));
#20883=CARTESIAN_POINT('Ctrl Pts',(5.90115185080704,5.58534639894578,-8.34204176354589));
#20884=CARTESIAN_POINT('Ctrl Pts',(5.75689108499793,5.73776392587195,-8.33381971964757));
#20885=CARTESIAN_POINT('Ctrl Pts',(5.60670603133728,5.88460640440353,-8.32559767574925));
#20886=CARTESIAN_POINT('Ctrl Pts',(5.45105188431948,6.02542288283213,-8.31737563185093));
#20887=CARTESIAN_POINT('Ctrl Pts',(5.29541492274622,6.16622381401174,-8.30915449573105));
#20888=CARTESIAN_POINT('Ctrl Pts',(5.13431029197106,6.3009998755828,-8.30093335961117));
#20889=CARTESIAN_POINT('Ctrl Pts',(4.96822833422969,6.42933859595661,-8.2927122234913));
#20890=CARTESIAN_POINT('Ctrl Pts',(4.80213320368471,6.55768749552617,-8.28449043531136));
#20891=CARTESIAN_POINT('Ctrl Pts',(4.63106018913466,6.67959785127481,-8.27626864713142));
#20892=CARTESIAN_POINT('Ctrl Pts',(4.45553168709605,6.79469829703888,-8.26804685895148));
#20893=CARTESIAN_POINT('Ctrl Pts',(4.28000367210317,6.90979842342928,-8.25982509358486));
#20894=CARTESIAN_POINT('Ctrl Pts',(4.10002044246582,7.01808851816036,-8.25160332821823));
#20895=CARTESIAN_POINT('Ctrl Pts',(3.91613271882103,7.11924097717442,-8.2433815628516));
#20896=CARTESIAN_POINT('Ctrl Pts',(3.73220665763841,7.22041452479705,-8.23515808338338));
#20897=CARTESIAN_POINT('Ctrl Pts',(3.54437473472822,7.31444732177401,-8.22693460391516));
#20898=CARTESIAN_POINT('Ctrl Pts',(3.35321253982474,7.40105757478363,-8.21871112444694));
#20899=CARTESIAN_POINT('Ctrl Pts',(3.27597593496695,7.4360513238966,-8.21538853425297));
#20900=CARTESIAN_POINT('Ctrl Pts',(3.19819593401293,7.46983390815843,-8.21206594405901));
#20901=CARTESIAN_POINT('Ctrl Pts',(3.11991148553179,7.50238894519251,-8.20874335386504));
#20902=CARTESIAN_POINT('Ctrl Pts',(2.92615445160806,7.58296391937171,-8.20051981479161));
#20903=CARTESIAN_POINT('Ctrl Pts',(2.72924287970012,7.65604200333074,-8.19229627571818));
#20904=CARTESIAN_POINT('Ctrl Pts',(2.5297750766031,7.7213940207904,-8.18407273664475));
#20905=CARTESIAN_POINT('Ctrl Pts',(2.3303435402179,7.78673415611797,-8.17585069275358));
#20906=CARTESIAN_POINT('Ctrl Pts',(2.12835698040241,7.84435093685115,-8.16762864886241));
#20907=CARTESIAN_POINT('Ctrl Pts',(1.92443040003701,7.89406455496238,-8.15940660497124));
#20908=CARTESIAN_POINT('Ctrl Pts',(1.7205263347752,7.94377268429789,-8.15118546885859));
#20909=CARTESIAN_POINT('Ctrl Pts',(1.51468296302451,7.98557932324147,-8.14296433274595));
#20910=CARTESIAN_POINT('Ctrl Pts',(1.3075278728656,8.01935523743521,-8.13474319663331));
#20911=CARTESIAN_POINT('Ctrl Pts',(1.10035635218153,8.05313383056872,-8.12652140846049));
#20912=CARTESIAN_POINT('Ctrl Pts',(0.891873195882433,8.07888037617433,-8.11829962028767));
#20913=CARTESIAN_POINT('Ctrl Pts',(0.682714606929592,8.09651704919992,-8.11007783211486));
#20914=CARTESIAN_POINT('Ctrl Pts',(0.473556598334639,8.11415367328857,-8.10185606675525));
#20915=CARTESIAN_POINT('Ctrl Pts',(0.263723454950581,8.1236804477162,-8.09363430139565));
#20916=CARTESIAN_POINT('Ctrl Pts',(0.0538554494699272,8.12507151679678,
-8.08541253603605));
#20917=CARTESIAN_POINT('Ctrl Pts',(-0.156056310004045,8.12646287589216,
-8.07718905657493));
#20918=CARTESIAN_POINT('Ctrl Pts',(-0.366002651115076,8.11971513924518,
-8.06896557711381));
#20919=CARTESIAN_POINT('Ctrl Pts',(-0.575343245118352,8.10485457690616,
-8.06074209765269));
#20920=CARTESIAN_POINT('Ctrl Pts',(-0.659924597459199,8.0988503594004,-8.05741950741604));
#20921=CARTESIAN_POINT('Ctrl Pts',(-0.74440709268594,8.09152234924638,-8.0540969171794));
#20922=CARTESIAN_POINT('Ctrl Pts',(-0.828748680368289,8.08287468585823,
-8.05077432694275));
#20923=CARTESIAN_POINT('Ctrl Pts',(-1.03749736508767,8.06147138521168,-8.04255078787003));
#20924=CARTESIAN_POINT('Ctrl Pts',(-1.24545036860925,8.03197355775538,-8.03432724879731));
#20925=CARTESIAN_POINT('Ctrl Pts',(-1.45197243939619,7.99446455978972,-8.02610370972459));
#20926=CARTESIAN_POINT('Ctrl Pts',(-1.65845696088148,7.95696238161177,-8.01788166583419));
#20927=CARTESIAN_POINT('Ctrl Pts',(-1.86351077885487,7.91145199275005,-8.0096596219438));
#20928=CARTESIAN_POINT('Ctrl Pts',(-2.06650746668915,7.85806811198643,-8.0014375780534));
#20929=CARTESIAN_POINT('Ctrl Pts',(-2.26948174208708,7.80469012522454,-7.99321644194153));
#20930=CARTESIAN_POINT('Ctrl Pts',(-2.47039905566403,7.74344045705942,-7.98499530582966));
#20931=CARTESIAN_POINT('Ctrl Pts',(-2.66864599462405,7.67450429134527,-7.9767741697178));
#20932=CARTESIAN_POINT('Ctrl Pts',(-2.86690865755784,7.60556265795295,-7.96855238154578));
#20933=CARTESIAN_POINT('Ctrl Pts',(-3.06250024322519,7.52893340323221,-7.96033059337377));
#20934=CARTESIAN_POINT('Ctrl Pts',(-3.25482424190259,7.44485102045858,-7.95210880520175));
#20935=CARTESIAN_POINT('Ctrl Pts',(-3.44714770693051,7.36076887099187,-7.94388703984308));
#20936=CARTESIAN_POINT('Ctrl Pts',(-3.63620333395049,7.26923375545565,-7.9356652744844));
#20937=CARTESIAN_POINT('Ctrl Pts',(-3.82141577982019,7.17052780485797,-7.92744350912573));
#20938=CARTESIAN_POINT('Ctrl Pts',(-4.0066668394108,7.07180127570786,-7.91922002966543));
#20939=CARTESIAN_POINT('Ctrl Pts',(-4.18807285687975,6.96590106365069,-7.91099655020514));
#20940=CARTESIAN_POINT('Ctrl Pts',(-4.36508325960138,6.85315516380942,-7.90277307074485));
#20941=CARTESIAN_POINT('Ctrl Pts',(-4.43660201751401,6.80760164496302,-7.89945048050339));
#20942=CARTESIAN_POINT('Ctrl Pts',(-4.50740351680724,6.76093110338285,-7.89612789026193));
#20943=CARTESIAN_POINT('Ctrl Pts',(-4.57745275089621,6.71316720153854,-7.89280530002047));
#20944=CARTESIAN_POINT('Ctrl Pts',(-4.75082730865321,6.59494970113748,-7.88458176094523));
#20945=CARTESIAN_POINT('Ctrl Pts',(-4.91964794377508,6.46999304191955,-7.87635822186999));
#20946=CARTESIAN_POINT('Ctrl Pts',(-5.08339573011157,6.33867300099819,-7.86813468279475));
#20947=CARTESIAN_POINT('Ctrl Pts',(-5.24711374425553,6.20737683634186,-7.8599126389018));
#20948=CARTESIAN_POINT('Ctrl Pts',(-5.40576052051277,6.06971978359707,-7.85169059500884));
#20949=CARTESIAN_POINT('Ctrl Pts',(-5.55884934941008,5.9261185841209,-7.84346855111588));
#20950=CARTESIAN_POINT('Ctrl Pts',(-5.71192127609631,5.78253323934689,-7.83524741500125));
#20951=CARTESIAN_POINT('Ctrl Pts',(-5.85943626550875,5.63300525978098,-7.82702627888662));
#20952=CARTESIAN_POINT('Ctrl Pts',(-6.00094308112869,5.47798956730968,-7.818805142772));
#20953=CARTESIAN_POINT('Ctrl Pts',(-6.14246112037178,5.3229615797577,-7.81058335459737));
#20954=CARTESIAN_POINT('Ctrl Pts',(-6.27796983284836,5.16244522565936,-7.80236156642275));
#20955=CARTESIAN_POINT('Ctrl Pts',(-6.40705632478139,4.99693073932177,-7.79413977824813));
#20956=CARTESIAN_POINT('Ctrl Pts',(-6.53614245853388,4.83141671224267,-7.78591801288677));
#20957=CARTESIAN_POINT('Ctrl Pts',(-6.65880622813568,4.66090481488924,-7.77769624752541));
#20958=CARTESIAN_POINT('Ctrl Pts',(-6.7746760357427,4.48591709388767,-7.76947448216406));
#20959=CARTESIAN_POINT('Ctrl Pts',(-6.8905700002809,4.31089289085146,-7.76125100270112));
#20960=CARTESIAN_POINT('Ctrl Pts',(-6.99966701034645,4.13139124598455,-7.75302752323819));
#20961=CARTESIAN_POINT('Ctrl Pts',(-7.10163908868174,3.94796274255566,-7.74480404377525));
#20962=CARTESIAN_POINT('Ctrl Pts',(-7.14283958444483,3.87385083465178,-7.74148145354956));
#20963=CARTESIAN_POINT('Ctrl Pts',(-7.18287747645796,3.79909818327198,-7.73815886332387));
#20964=CARTESIAN_POINT('Ctrl Pts',(-7.2217332481857,3.72374226478542,-7.73483627309817));
#20965=CARTESIAN_POINT('Ctrl Pts',(-7.31773817055224,3.53755270317142,-7.72662681019241));
#20966=CARTESIAN_POINT('Ctrl Pts',(-7.40655543191432,3.34761605895886,-7.71841734728665));
#20967=CARTESIAN_POINT('Ctrl Pts',(-7.48790814557763,3.15450775334158,-7.71020788438089));
#20968=CARTESIAN_POINT('Ctrl Pts',(-7.56924560136053,2.96143566561184,-7.70199996117796));
#20969=CARTESIAN_POINT('Ctrl Pts',(-7.64312118829713,2.765193377224,-7.69379203797503));
#20970=CARTESIAN_POINT('Ctrl Pts',(-7.70930583954445,2.56637702508145,-7.6855841147721));
#20971=CARTESIAN_POINT('Ctrl Pts',(-7.77803828579436,2.35990718683786,-7.67706022547546));
#20972=CARTESIAN_POINT('Ctrl Pts',(-7.83847581120739,2.15066149345176,-7.66853633617881));
#20973=CARTESIAN_POINT('Ctrl Pts',(-7.89041817182838,1.93932685130188,-7.66001244688217));
#20974=CARTESIAN_POINT('Ctrl Pts',(-7.94043323609318,1.73583367959891,-7.65180483240604));
#20975=CARTESIAN_POINT('Ctrl Pts',(-7.98257211352486,1.53040408927546,-7.6435972179299));
#20976=CARTESIAN_POINT('Ctrl Pts',(-8.01670761297762,1.32366408522956,-7.63538960345376));
#20977=CARTESIAN_POINT('Ctrl Pts',(-8.05084356618041,1.11692133306856,-7.62718187987697));
#20978=CARTESIAN_POINT('Ctrl Pts',(-8.07697588355815,0.908868425877369,
-7.61897415630018));
#20979=CARTESIAN_POINT('Ctrl Pts',(-8.09502886037525,0.700139494809234,
-7.61076643272339));
#20980=CARTESIAN_POINT('Ctrl Pts',(-8.11308536121284,0.491369818935635,
-7.60255710696286));
#20981=CARTESIAN_POINT('Ctrl Pts',(-8.12305934678764,0.281924151546433,
-7.59434778120232));
#20982=CARTESIAN_POINT('Ctrl Pts',(-8.12492707114278,0.0724406730452409,
-7.58613845544179));
#20983=CARTESIAN_POINT('Ctrl Pts',(-8.1251425264225,0.0482752648400622,
-7.58519145136532));
#20984=CARTESIAN_POINT('Ctrl Pts',(-8.12525016658789,0.0241093546043511,
-7.58424444728886));
#20985=CARTESIAN_POINT('Ctrl Pts',(-8.12524999980648,-5.6077649948665E-5,
-7.58329744321239));
#20986=CARTESIAN_POINT('Origin',(0.,0.,-16.4167025567876));
#20987=CARTESIAN_POINT('',(4.94701442880054,-6.44622255101802,-10.8749380057189));
#20988=CARTESIAN_POINT('',(4.94675008185374,-6.44587862049698,-10.708343763603));
#20989=CARTESIAN_POINT('',(4.94675008185374,-6.44587862049697,-16.4167025567876));
#20990=CARTESIAN_POINT('',(-8.12477737866023,-0.000175769160715919,-11.5832974432124));
#20991=CARTESIAN_POINT('Ctrl Pts',(-8.12477737866023,-0.000175769160715919,
-11.5832974432124));
#20992=CARTESIAN_POINT('Ctrl Pts',(-8.12510001228012,-0.486965488702826,
-11.5642292685526));
#20993=CARTESIAN_POINT('Ctrl Pts',(-7.96312717430326,-2.31779341310246,
-11.4925047515855));
#20994=CARTESIAN_POINT('Ctrl Pts',(-6.60455795380853,-5.2972113717909,-11.3681238923108));
#20995=CARTESIAN_POINT('Ctrl Pts',(-3.28552397693065,-7.80285054932884,
-11.2101548653885));
#20996=CARTESIAN_POINT('Ctrl Pts',(0.826182671114322,-8.42599612481988,
-11.0521858384663));
#20997=CARTESIAN_POINT('Ctrl Pts',(3.59360149709808,-7.42870399706383,-10.9404468852431));
#20998=CARTESIAN_POINT('Ctrl Pts',(4.81699001004096,-6.54618702099177,-10.8813642743273));
#20999=CARTESIAN_POINT('Ctrl Pts',(4.94701442880054,-6.44622255101802,-10.8749380057189));
#21000=CARTESIAN_POINT('',(-2.10208451021623,7.84862588447232,-12.));
#21001=CARTESIAN_POINT('Ctrl Pts',(-2.10208451021617,7.84862588447234,-12.));
#21002=CARTESIAN_POINT('Ctrl Pts',(-3.40044170599961,7.5008890207006,-11.9473436576926));
#21003=CARTESIAN_POINT('Ctrl Pts',(-5.82000697965988,6.14913288471193,-11.8420309730777));
#21004=CARTESIAN_POINT('Ctrl Pts',(-7.77710899046075,3.05948964104654,-11.7031301208152));
#21005=CARTESIAN_POINT('Ctrl Pts',(-8.1242090666793,0.85729354821751,-11.6168856108601));
#21006=CARTESIAN_POINT('Ctrl Pts',(-8.12477737866023,-0.000175769160715919,
-11.5832974432124));
#21007=CARTESIAN_POINT('',(2.10216660754842,7.84860389601923,-12.));
#21008=CARTESIAN_POINT('Origin',(0.,0.,-12.));
#21009=CARTESIAN_POINT('',(-8.12524999739639,-0.00020569387470909,-11.4167025567622));
#21010=CARTESIAN_POINT('Ctrl Pts',(2.10216660754842,7.84860389601924,-12.));
#21011=CARTESIAN_POINT('Ctrl Pts',(1.89996534114966,7.90276139407352,-11.9917970169686));
#21012=CARTESIAN_POINT('Ctrl Pts',(1.69563573139414,7.94911002038602,-11.9835940339371));
#21013=CARTESIAN_POINT('Ctrl Pts',(1.48979808132141,7.98750206506333,-11.9753910509057));
#21014=CARTESIAN_POINT('Ctrl Pts',(1.28399710640837,8.0258872692313,-11.9671895294422));
#21015=CARTESIAN_POINT('Ctrl Pts',(1.07668892013284,8.0563186665635,-11.9589880079787));
#21016=CARTESIAN_POINT('Ctrl Pts',(0.868503869052085,8.07869968447531,-11.9507864865152));
#21017=CARTESIAN_POINT('Ctrl Pts',(0.660311461804441,8.10108149321482,-11.942584675253));
#21018=CARTESIAN_POINT('Ctrl Pts',(0.451242423565235,8.11541231797868,-11.9343828639908));
#21019=CARTESIAN_POINT('Ctrl Pts',(0.241933137304118,8.12164736488689,-11.9261810527286));
#21020=CARTESIAN_POINT('Ctrl Pts',(0.0326345503735735,8.12788209307619,
-11.917979660721));
#21021=CARTESIAN_POINT('Ctrl Pts',(-0.176903962194337,8.12602186296263,
-11.9097782687135));
#21022=CARTESIAN_POINT('Ctrl Pts',(-0.386044600651898,8.11607399724815,
-11.9015768767059));
#21023=CARTESIAN_POINT('Ctrl Pts',(-0.59523794315302,8.10612362464284,-11.8933734179239));
#21024=CARTESIAN_POINT('Ctrl Pts',(-0.804032913327771,8.08808155585036,
-11.8851699591419));
#21025=CARTESIAN_POINT('Ctrl Pts',(-1.0117941832255,8.06200720002724,-11.87696650036));
#21026=CARTESIAN_POINT('Ctrl Pts',(-1.21139251650028,8.03695730518365,-11.8690853553286));
#21027=CARTESIAN_POINT('Ctrl Pts',(-1.41003656919329,8.00449424540528,-11.8612042102972));
#21028=CARTESIAN_POINT('Ctrl Pts',(-1.60716938183343,7.96471557185799,-11.8533230652658));
#21029=CARTESIAN_POINT('Ctrl Pts',(-1.81286241034718,7.92320956520887,-11.8450996925662));
#21030=CARTESIAN_POINT('Ctrl Pts',(-2.01698012426594,7.87372435936419,-11.8368763198665));
#21031=CARTESIAN_POINT('Ctrl Pts',(-2.21889834609129,7.8164043966656,-11.8286529471669));
#21032=CARTESIAN_POINT('Ctrl Pts',(-2.42077987259646,7.75909485092871,-11.8204310689302));
#21033=CARTESIAN_POINT('Ctrl Pts',(-2.62046242119952,7.69395347066466,-11.8122091906935));
#21034=CARTESIAN_POINT('Ctrl Pts',(-2.81733556906005,7.62117496543736,-11.8039873124568));
#21035=CARTESIAN_POINT('Ctrl Pts',(-3.01418701026522,7.54840448455439,-11.7957663407403));
#21036=CARTESIAN_POINT('Ctrl Pts',(-3.20822939259246,7.46799866205816,-11.7875453690237));
#21037=CARTESIAN_POINT('Ctrl Pts',(-3.39887013048231,7.38020117602597,-11.7793243973072));
#21038=CARTESIAN_POINT('Ctrl Pts',(-3.58952606142905,7.29239669299925,-11.7711027704227));
#21039=CARTESIAN_POINT('Ctrl Pts',(-3.77677953724081,7.19719949038884,-11.7628811435383));
#21040=CARTESIAN_POINT('Ctrl Pts',(-3.96005956871056,7.0949006881537,-11.7546595166538));
#21041=CARTESIAN_POINT('Ctrl Pts',(-4.14333913846275,6.99260214362888,-11.7464379104812));
#21042=CARTESIAN_POINT('Ctrl Pts',(-4.32264502766298,6.88320218138654,-11.7382163043087));
#21043=CARTESIAN_POINT('Ctrl Pts',(-4.49743192566566,6.76703728647207,-11.7299946981361));
#21044=CARTESIAN_POINT('Ctrl Pts',(-4.67225535284077,6.65084811395141,-11.7217713737084));
#21045=CARTESIAN_POINT('Ctrl Pts',(-4.84255765641126,6.52789134764352,-11.7135480492808));
#21046=CARTESIAN_POINT('Ctrl Pts',(-5.00782261952502,6.39854672358291,-11.7053247248532));
#21047=CARTESIAN_POINT('Ctrl Pts',(-5.07461657667055,6.34627043274828,-11.7020011626833));
#21048=CARTESIAN_POINT('Ctrl Pts',(-5.14058805180424,6.29295117663334,-11.6986776005134));
#21049=CARTESIAN_POINT('Ctrl Pts',(-5.20570446436953,6.2386159195885,-11.6953540383435));
#21050=CARTESIAN_POINT('Ctrl Pts',(-5.36681564989789,6.10417949513553,-11.6871308727809));
#21051=CARTESIAN_POINT('Ctrl Pts',(-5.52274263827381,5.96347680179788,-11.6789077072183));
#21052=CARTESIAN_POINT('Ctrl Pts',(-5.67300533197767,5.81693201489006,-11.6706845416556));
#21053=CARTESIAN_POINT('Ctrl Pts',(-5.82324059656644,5.67041397842659,-11.6624628771586));
#21054=CARTESIAN_POINT('Ctrl Pts',(-5.96781341907526,5.51805618270177,-11.6542412126615));
#21055=CARTESIAN_POINT('Ctrl Pts',(-6.10627973000892,5.36032045883287,-11.6460195481645));
#21056=CARTESIAN_POINT('Ctrl Pts',(-6.24473067440802,5.20260223995442,-11.6377987960806));
#21057=CARTESIAN_POINT('Ctrl Pts',(-6.3770762656581,5.03950750607002,-11.6295780439968));
#21058=CARTESIAN_POINT('Ctrl Pts',(-6.50291143441447,4.87153265807195,-11.6213572919129));
#21059=CARTESIAN_POINT('Ctrl Pts',(-6.62875652253558,4.70354456891244,-11.6131358918017));
#21060=CARTESIAN_POINT('Ctrl Pts',(-6.74808998373867,4.5306758314968,-11.6049144916904));
#21061=CARTESIAN_POINT('Ctrl Pts',(-6.86054832813189,4.35345428365415,-11.5966930915792));
#21062=CARTESIAN_POINT('Ctrl Pts',(-6.97300633836633,4.1762332624077,-11.588471715897));
#21063=CARTESIAN_POINT('Ctrl Pts',(-7.07858911687302,3.99465970711972,-11.5802503402148));
#21064=CARTESIAN_POINT('Ctrl Pts',(-7.17697735404496,3.80928912292382,-11.5720289645327));
#21065=CARTESIAN_POINT('Ctrl Pts',(-7.27538610556852,3.62387988819965,-11.5638058746599));
#21066=CARTESIAN_POINT('Ctrl Pts',(-7.36659718068259,3.4346723035936,-11.5555827847871));
#21067=CARTESIAN_POINT('Ctrl Pts',(-7.450337447084,3.24224605591215,-11.5473596949143));
#21068=CARTESIAN_POINT('Ctrl Pts',(-7.48419668434161,3.16444112102446,-11.5440348004166));
#21069=CARTESIAN_POINT('Ctrl Pts',(-7.51683507421775,3.08611022310206,-11.5407099059189));
#21070=CARTESIAN_POINT('Ctrl Pts',(-7.54823678541172,3.00729263522149,-11.5373850114212));
#21071=CARTESIAN_POINT('Ctrl Pts',(-7.62564901103827,2.8129896923448,-11.5291884045086));
#21072=CARTESIAN_POINT('Ctrl Pts',(-7.69556892011692,2.61566045847154,-11.520991797596));
#21073=CARTESIAN_POINT('Ctrl Pts',(-7.75777691501068,2.4159025020533,-11.5127951906835));
#21074=CARTESIAN_POINT('Ctrl Pts',(-7.81997745567985,2.21616848211898,-11.5045995659493));
#21075=CARTESIAN_POINT('Ctrl Pts',(-7.87446783475686,2.01400660477959,-11.4964039412151));
#21076=CARTESIAN_POINT('Ctrl Pts',(-7.92107800867631,1.81003059172064,-11.4882083164809));
#21077=CARTESIAN_POINT('Ctrl Pts',(-7.9676820176964,1.60608155756963,-11.4800137757418));
#21078=CARTESIAN_POINT('Ctrl Pts',(-8.00640783658789,1.40031915819125,-11.4718192350027));
#21079=CARTESIAN_POINT('Ctrl Pts',(-8.037136191185,1.19336893157322,-11.4636246942637));
#21080=CARTESIAN_POINT('Ctrl Pts',(-8.06786804751145,0.986395121405414,
-11.4554292196945));
#21081=CARTESIAN_POINT('Ctrl Pts',(-8.09060057175316,0.778233508789898,
-11.4472337451252));
#21082=CARTESIAN_POINT('Ctrl Pts',(-8.10526602692919,0.569517510887509,
-11.439038270556));
#21083=CARTESIAN_POINT('Ctrl Pts',(-8.11858896535206,0.379907958743068,
-11.4315930326332));
#21084=CARTESIAN_POINT('Ctrl Pts',(-8.1252548084907,0.189841129461651,-11.4241477947104));
#21085=CARTESIAN_POINT('Ctrl Pts',(-8.12524999739641,-0.000205693225322712,
-11.4167025567876));
#21086=CARTESIAN_POINT('Ctrl Pts',(-8.12524999739639,-0.000205693874714312,
-11.4167025567622));
#21087=CARTESIAN_POINT('Ctrl Pts',(-8.12524439842859,-0.221374229701558,
-11.4080381005666));
#21088=CARTESIAN_POINT('Ctrl Pts',(-8.11620418154541,-0.442498629493132,
-11.3993736443711));
#21089=CARTESIAN_POINT('Ctrl Pts',(-8.09816610723247,-0.662867454451679,
-11.3907091881756));
#21090=CARTESIAN_POINT('Ctrl Pts',(-8.090329198889,-0.758609951849022,-11.38694478695));
#21091=CARTESIAN_POINT('Ctrl Pts',(-8.08079452229166,-0.854209868966177,
-11.3831803857244));
#21092=CARTESIAN_POINT('Ctrl Pts',(-8.0695681467729,-0.949609123317658,
-11.3794159844989));
#21093=CARTESIAN_POINT('Ctrl Pts',(-8.04504425623296,-1.15800771709347,
-11.3711926925335));
#21094=CARTESIAN_POINT('Ctrl Pts',(-8.0124391408174,-1.36548973226526,-11.362969400568));
#21095=CARTESIAN_POINT('Ctrl Pts',(-7.97184563020018,-1.57142127093859,
-11.3547461086026));
#21096=CARTESIAN_POINT('Ctrl Pts',(-7.93125951566936,-1.77731528914547,
-11.3465243149106));
#21097=CARTESIAN_POINT('Ctrl Pts',(-7.8826879679138,-1.98165910542167,-11.3383025212187));
#21098=CARTESIAN_POINT('Ctrl Pts',(-7.826275041556,-2.1838284127691,-11.3300807275267));
#21099=CARTESIAN_POINT('Ctrl Pts',(-7.76986835938902,-2.38597534255496,
-11.3218598438823));
#21100=CARTESIAN_POINT('Ctrl Pts',(-7.70562211067602,-2.58594795993353,
-11.3136389602379));
#21101=CARTESIAN_POINT('Ctrl Pts',(-7.63373061504855,-2.78313572420937,
-11.3054180765935));
#21102=CARTESIAN_POINT('Ctrl Pts',(-7.56183343020747,-2.98033909315865,
-11.2971965423803));
#21103=CARTESIAN_POINT('Ctrl Pts',(-7.48228988812273,-3.17475689061642,
-11.2889750081672));
#21104=CARTESIAN_POINT('Ctrl Pts',(-7.39534335969,-3.36579621409095,-11.280753473954));
#21105=CARTESIAN_POINT('Ctrl Pts',(-7.30839707666393,-3.55683499835681,
-11.2725319629461));
#21106=CARTESIAN_POINT('Ctrl Pts',(-7.21404797372757,-3.74449506035948,
-11.2643104519382));
#21107=CARTESIAN_POINT('Ctrl Pts',(-7.11258673769472,-3.9282053741205,-11.2560889409303));
#21108=CARTESIAN_POINT('Ctrl Pts',(-7.01110433511271,-4.11195401299502,
-11.2478657147746));
#21109=CARTESIAN_POINT('Ctrl Pts',(-6.90250697803266,-4.2917509992888,-11.2396424886189));
#21110=CARTESIAN_POINT('Ctrl Pts',(-6.78713084177567,-4.46705076075004,
-11.2314192624633));
#21111=CARTESIAN_POINT('Ctrl Pts',(-6.74049196851533,-4.53791275719571,
-11.2280951608344));
#21112=CARTESIAN_POINT('Ctrl Pts',(-6.69274591559649,-4.60804020206745,
-11.2247710592055));
#21113=CARTESIAN_POINT('Ctrl Pts',(-6.64391690075673,-4.67739839850521,
-11.2214469575766));
#21114=CARTESIAN_POINT('Ctrl Pts',(-6.52311635522553,-4.84898711464533,
-11.2132232960612));
#21115=CARTESIAN_POINT('Ctrl Pts',(-6.39564537172317,-5.01592139574531,
-11.2049996345459));
#21116=CARTESIAN_POINT('Ctrl Pts',(-6.26188746879502,-5.17768798699264,
-11.1967759730305));
#21117=CARTESIAN_POINT('Ctrl Pts',(-6.12815386162119,-5.33942519499404,
-11.1885538052591));
#21118=CARTESIAN_POINT('Ctrl Pts',(-5.98813580207213,-5.49599635942735,
-11.1803316374877));
#21119=CARTESIAN_POINT('Ctrl Pts',(-5.84225728576869,-5.64692105216486,
-11.1721094697163));
#21120=CARTESIAN_POINT('Ctrl Pts',(-5.69639485706507,-5.79782910080615,
-11.1638882086922));
#21121=CARTESIAN_POINT('Ctrl Pts',(-5.54467346679687,-5.94309170897547,
-11.155666947668));
#21122=CARTESIAN_POINT('Ctrl Pts',(-5.38755475559963,-6.08226448930953,
-11.1474456866439));
#21123=CARTESIAN_POINT('Ctrl Pts',(-5.23042357122042,-6.22144831815209,
-11.1392237729586));
#21124=CARTESIAN_POINT('Ctrl Pts',(-5.06789442878962,-6.35454115563913,
-11.1310018592732));
#21125=CARTESIAN_POINT('Ctrl Pts',(-4.90046370332159,-6.48113748156353,
-11.1227799455879));
#21126=CARTESIAN_POINT('Ctrl Pts',(-4.73303344008498,-6.60773345798936,
-11.1145580546011));
#21127=CARTESIAN_POINT('Ctrl Pts',(-4.56070185774561,-6.72783278301322,
-11.1063361636142));
#21128=CARTESIAN_POINT('Ctrl Pts',(-4.38399652189535,-6.84107170394446,
-11.0981142726274));
#21129=CARTESIAN_POINT('Ctrl Pts',(-4.2072543601162,-6.95433422421087,-11.0898906681735));
#21130=CARTESIAN_POINT('Ctrl Pts',(-4.026136872252,-7.06073332504557,-11.0816670637196));
#21131=CARTESIAN_POINT('Ctrl Pts',(-3.84119950444942,-7.15994929657449,
-11.0734434592657));
#21132=CARTESIAN_POINT('Ctrl Pts',(-3.76649590213428,-7.20002659716805,
-11.0701216163953));
#21133=CARTESIAN_POINT('Ctrl Pts',(-3.69116931179321,-7.23893236081685,
-11.0667997735248));
#21134=CARTESIAN_POINT('Ctrl Pts',(-3.61525747148042,-7.27664764691853,
-11.0634779306543));
#21135=CARTESIAN_POINT('Ctrl Pts',(-3.42733150203513,-7.37001492235752,
-11.0552544369383));
#21136=CARTESIAN_POINT('Ctrl Pts',(-3.2357561229959,-7.45611344327543,-11.0470309432224));
#21137=CARTESIAN_POINT('Ctrl Pts',(-3.04111294558001,-7.53467448631497,
-11.0388074495064));
#21138=CARTESIAN_POINT('Ctrl Pts',(-2.8465051692872,-7.61322124090529,-11.030585451455));
#21139=CARTESIAN_POINT('Ctrl Pts',(-2.64883098161428,-7.68423314342852,
-11.0223634534037));
#21140=CARTESIAN_POINT('Ctrl Pts',(-2.44869195825795,-7.74748960993578,
-11.0141414553523));
#21141=CARTESIAN_POINT('Ctrl Pts',(-2.24857504002964,-7.81073908983809,
-11.0059203654113));
#21142=CARTESIAN_POINT('Ctrl Pts',(-2.04599411075093,-7.86623475500108,
-10.9976992754703));
#21143=CARTESIAN_POINT('Ctrl Pts',(-1.84156668959712,-7.91380563889879,
-10.9894781855293));
#21144=CARTESIAN_POINT('Ctrl Pts',(-1.63712305787383,-7.96138029504542,
-10.981256443677));
#21145=CARTESIAN_POINT('Ctrl Pts',(-1.43083292838439,-8.00102884486518,
-10.9730347018247));
#21146=CARTESIAN_POINT('Ctrl Pts',(-1.22332585827275,-8.03263103889263,
-10.9648129599724));
#21147=CARTESIAN_POINT('Ctrl Pts',(-1.01581936394145,-8.06423314523187,
-10.9565912409333));
#21148=CARTESIAN_POINT('Ctrl Pts',(-0.807096227725382,-8.08778889870032,
-10.9483695218943));
#21149=CARTESIAN_POINT('Ctrl Pts',(-0.597793547226755,-8.10322963005455,
-10.9401478028553));
#21150=CARTESIAN_POINT('Ctrl Pts',(-0.388447222788129,-8.11867358112079,
-10.9319243694177));
#21151=CARTESIAN_POINT('Ctrl Pts',(-0.178521406842369,-8.12599910793916,
-10.9237009359801));
#21152=CARTESIAN_POINT('Ctrl Pts',(0.0313432567839139,-8.12518954626624,
-10.9154775025425));
#21153=CARTESIAN_POINT('Ctrl Pts',(0.116143871679868,-8.12486242436551,
-10.9121546362724));
#21154=CARTESIAN_POINT('Ctrl Pts',(0.200934490792732,-8.12320764064176,
-10.9088317700022));
#21155=CARTESIAN_POINT('Ctrl Pts',(0.285672870119704,-8.12022651000436,
-10.905508903732));
#21156=CARTESIAN_POINT('Ctrl Pts',(0.495386426716496,-8.11284870181857,
-10.8972853560415));
#21157=CARTESIAN_POINT('Ctrl Pts',(0.704848081338482,-8.09734123816306,
-10.889061808351));
#21158=CARTESIAN_POINT('Ctrl Pts',(0.913418425414848,-8.07374475337267,
-10.8808382606605));
#21159=CARTESIAN_POINT('Ctrl Pts',(1.12195084923025,-8.05015255866898,-10.8726162080966));
#21160=CARTESIAN_POINT('Ctrl Pts',(1.32959199301364,-8.01847431125548,-10.8643941555327));
#21161=CARTESIAN_POINT('Ctrl Pts',(1.53570781418867,-7.97880248357733,-10.8561721029688));
#21162=CARTESIAN_POINT('Ctrl Pts',(1.74180087925786,-7.93913503584589,-10.8479509581562));
#21163=CARTESIAN_POINT('Ctrl Pts',(1.94636866842304,-7.8914758255043,-10.8397298133436));
#21164=CARTESIAN_POINT('Ctrl Pts',(2.14878674469931,-7.83596854819521,-10.831508668531));
#21165=CARTESIAN_POINT('Ctrl Pts',(2.35122087515886,-7.78045686849272,-10.8232868716829));
#21166=CARTESIAN_POINT('Ctrl Pts',(2.55150466691681,-7.7170959535628,-10.8150650748348));
#21167=CARTESIAN_POINT('Ctrl Pts',(2.74902724646548,-7.64607982960487,-10.8068432779868));
#21168=CARTESIAN_POINT('Ctrl Pts',(2.94654927721182,-7.57506390296015,-10.7986215039823));
#21169=CARTESIAN_POINT('Ctrl Pts',(3.14130983446964,-7.49639291215554,-10.7903997299779));
#21170=CARTESIAN_POINT('Ctrl Pts',(3.33271597406544,-7.41030983149214,-10.7821779559735));
#21171=CARTESIAN_POINT('Ctrl Pts',(3.52416201627601,-7.32420880500938,-10.7739544679683));
#21172=CARTESIAN_POINT('Ctrl Pts',(3.71225197479779,-7.23069272278405,-10.7657309799631));
#21173=CARTESIAN_POINT('Ctrl Pts',(3.89641454939461,-7.13005197889651,-10.7575074919578));
#21174=CARTESIAN_POINT('Ctrl Pts',(3.97082181093149,-7.08939006825532,-10.7541849535751));
#21175=CARTESIAN_POINT('Ctrl Pts',(4.04458823726234,-7.04756565169544,-10.7508624151925));
#21176=CARTESIAN_POINT('Ctrl Pts',(4.11767731770119,-7.0045999935606,-10.7475398768098));
#21177=CARTESIAN_POINT('Ctrl Pts',(4.29857842557853,-6.89825667783403,-10.7393163382075));
#21178=CARTESIAN_POINT('Ctrl Pts',(4.47538707246437,-6.78488440581811,-10.7310927996053));
#21179=CARTESIAN_POINT('Ctrl Pts',(4.64756033596046,-6.66482336495927,-10.722869261003));
#21180=CARTESIAN_POINT('Ctrl Pts',(4.74893203705017,-6.5941341551521,-10.7180274285364));
#21181=CARTESIAN_POINT('Ctrl Pts',(4.84869734040954,-6.52112707541245,-10.7131855960697));
#21182=CARTESIAN_POINT('Ctrl Pts',(4.94675008185374,-6.44587862049698,-10.7083437636031));
#21183=CARTESIAN_POINT('Origin',(0.,0.,0.));
#21184=CARTESIAN_POINT('',(-6.5722715952584,-2.44189939200198,11.3396960824468));
#21185=CARTESIAN_POINT('',(-6.5722717076903,-2.44189908939612,11.8869527148536));
#21186=CARTESIAN_POINT('',(-6.57227159525839,-2.441899392002,0.));
#21187=CARTESIAN_POINT('',(-5.31037376991248,-4.57794244025911,12.));
#21188=CARTESIAN_POINT('Ctrl Pts',(-6.57227170769031,-2.44189908939611,
11.8869527148536));
#21189=CARTESIAN_POINT('Ctrl Pts',(-6.48361520701476,-2.68051444153043,
11.8986804082385));
#21190=CARTESIAN_POINT('Ctrl Pts',(-6.38199333019113,-2.91422192491829,
11.9103615063067));
#21191=CARTESIAN_POINT('Ctrl Pts',(-6.18969751160504,-3.29782778585046,
11.9298963196887));
#21192=CARTESIAN_POINT('Ctrl Pts',(-6.10577998828279,-3.45072098239082,
11.9377875875726));
#21193=CARTESIAN_POINT('Ctrl Pts',(-5.80946526690376,-3.94587121303711,
11.9638060428799));
#21194=CARTESIAN_POINT('Ctrl Pts',(-5.57329951969572,-4.27295083686872,
11.9817184539604));
#21195=CARTESIAN_POINT('Ctrl Pts',(-5.31037376991251,-4.57794244025908,
12.));
#21196=CARTESIAN_POINT('',(5.31042129803496,-4.57788730746801,11.9999999751457));
#21197=CARTESIAN_POINT('Origin',(0.,0.,12.));
#21198=CARTESIAN_POINT('Ctrl Pts',(5.31042129803496,-4.57788730746801,11.9999999751457));
#21199=CARTESIAN_POINT('Ctrl Pts',(5.18805357552032,-4.71983579072877,11.9914889449188));
#21200=CARTESIAN_POINT('Ctrl Pts',(5.0599695362356,-4.85690008843993,11.9829779146919));
#21201=CARTESIAN_POINT('Ctrl Pts',(4.92658399091152,-4.9886267391933,11.974466884465));
#21202=CARTESIAN_POINT('Ctrl Pts',(4.79322289753619,-5.12032924210287,11.9659574144617));
#21203=CARTESIAN_POINT('Ctrl Pts',(4.65456245732618,-5.24669583361785,11.9574479444583));
#21204=CARTESIAN_POINT('Ctrl Pts',(4.51105444164968,-5.36730979047909,11.948938474455));
#21205=CARTESIAN_POINT('Ctrl Pts',(4.3675415572123,-5.48792783938017,11.940428715753));
#21206=CARTESIAN_POINT('Ctrl Pts',(4.21918100264951,-5.60279266164602,11.931918957051));
#21207=CARTESIAN_POINT('Ctrl Pts',(4.06645841569416,-5.71152716144554,11.9234091983491));
#21208=CARTESIAN_POINT('Ctrl Pts',(3.91374276690221,-5.82025672145363,11.9148998262441));
#21209=CARTESIAN_POINT('Ctrl Pts',(3.75666573453365,-5.92285633767202,11.9063904541391));
#21210=CARTESIAN_POINT('Ctrl Pts',(3.59574305338647,-6.01899148167889,11.8978810820341));
#21211=CARTESIAN_POINT('Ctrl Pts',(3.43478164633629,-6.11514976052439,11.8893696621562));
#21212=CARTESIAN_POINT('Ctrl Pts',(3.26997300630207,-6.204840299288,11.8808582422782));
#21213=CARTESIAN_POINT('Ctrl Pts',(3.10185952256609,-6.28777337892883,11.8723468224002));
#21214=CARTESIAN_POINT('Ctrl Pts',(2.97661014657212,-6.34956090627902,11.8660055700221));
#21215=CARTESIAN_POINT('Ctrl Pts',(2.84952692432497,-6.4075985053793,11.859664317644));
#21216=CARTESIAN_POINT('Ctrl Pts',(2.72084227075256,-6.46178333745307,11.8533230652658));
#21217=CARTESIAN_POINT('Ctrl Pts',(2.54769645008476,-6.53468928976913,11.8447908796742));
#21218=CARTESIAN_POINT('Ctrl Pts',(2.37158945434072,-6.60064426719468,11.8362586940826));
#21219=CARTESIAN_POINT('Ctrl Pts',(2.19309726907259,-6.65942572080254,11.827726508491));
#21220=CARTESIAN_POINT('Ctrl Pts',(2.01463849137951,-6.71819617255157,11.8191959198299));
#21221=CARTESIAN_POINT('Ctrl Pts',(1.83379570559365,-6.76979568421087,11.8106653311689));
#21222=CARTESIAN_POINT('Ctrl Pts',(1.65116165701798,-6.81405105241322,11.8021347425078));
#21223=CARTESIAN_POINT('Ctrl Pts',(1.46065319109038,-6.86021452724741,11.7932363504941));
#21224=CARTESIAN_POINT('Ctrl Pts',(1.26819591201722,-6.89838641697431,11.7843379584804));
#21225=CARTESIAN_POINT('Ctrl Pts',(1.07447724055565,-6.9284287700768,11.7754395664667));
#21226=CARTESIAN_POINT('Ctrl Pts',(0.888771302404243,-6.95722848940732,
11.7669092362488));
#21227=CARTESIAN_POINT('Ctrl Pts',(0.701906544640717,-6.97855761093532,
11.7583789060309));
#21228=CARTESIAN_POINT('Ctrl Pts',(0.514496804174811,-6.99234721685029,
11.749848575813));
#21229=CARTESIAN_POINT('Ctrl Pts',(0.327085093881319,-7.00613696770513,
11.7413181559344));
#21230=CARTESIAN_POINT('Ctrl Pts',(0.139128694855618,-7.01238702537379,
11.7327877360559));
#21231=CARTESIAN_POINT('Ctrl Pts',(-0.0487550931711929,-7.01108048045306,
11.7242573161773));
#21232=CARTESIAN_POINT('Ctrl Pts',(-0.236676153219624,-7.00977367634248,
11.7157252040506));
#21233=CARTESIAN_POINT('Ctrl Pts',(-0.424524267500988,-7.00090727872107,
11.7071930919239));
#21234=CARTESIAN_POINT('Ctrl Pts',(-0.611682912612513,-6.98451648841335,
11.6986609797971));
#21235=CARTESIAN_POINT('Ctrl Pts',(-0.635863040297116,-6.9823988656754,
11.6975586659792));
#21236=CARTESIAN_POINT('Ctrl Pts',(-0.660031664932469,-6.98015572005915,
11.6964563521614));
#21237=CARTESIAN_POINT('Ctrl Pts',(-0.6841874625102,-6.97778719069619,11.6953540383435));
#21238=CARTESIAN_POINT('Ctrl Pts',(-0.871154688398204,-6.95945464079793,
11.6868220676675));
#21239=CARTESIAN_POINT('Ctrl Pts',(-1.05741630635565,-6.93360008947338,
11.6782900969915));
#21240=CARTESIAN_POINT('Ctrl Pts',(-1.24235987700682,-6.90030205849741,
11.6697581263155));
#21241=CARTESIAN_POINT('Ctrl Pts',(-1.42726867797124,-6.86701028760446,
11.6612277596636));
#21242=CARTESIAN_POINT('Ctrl Pts',(-1.610859625064,-6.82627788391762,11.6526973930118));
#21243=CARTESIAN_POINT('Ctrl Pts',(-1.79252903411854,-6.77823474249322,
11.6441670263599));
#21244=CARTESIAN_POINT('Ctrl Pts',(-1.98203852750899,-6.7281182620158,11.635268525115));
#21245=CARTESIAN_POINT('Ctrl Pts',(-2.16945660525274,-6.67004611011735,
11.6263700238701));
#21246=CARTESIAN_POINT('Ctrl Pts',(-2.3541130366864,-6.60422428245764,11.6174715226253));
#21247=CARTESIAN_POINT('Ctrl Pts',(-2.53112450467776,-6.54112754518476,
11.6089414283521));
#21248=CARTESIAN_POINT('Ctrl Pts',(-2.7055980832415,-6.47091000800959,11.6004113340789));
#21249=CARTESIAN_POINT('Ctrl Pts',(-2.87696119327688,-6.39380331687478,
11.5918812398057));
#21250=CARTESIAN_POINT('Ctrl Pts',(-3.04832602678408,-6.31669585024511,
11.5833510597417));
#21251=CARTESIAN_POINT('Ctrl Pts',(-3.21658005149229,-6.23269921972729,
11.5748208796777));
#21252=CARTESIAN_POINT('Ctrl Pts',(-3.38117240538391,-6.14209245514673,
11.5662906996137));
#21253=CARTESIAN_POINT('Ctrl Pts',(-3.54579733378653,-6.05146775856034,
11.5577588313398));
#21254=CARTESIAN_POINT('Ctrl Pts',(-3.70675887635521,-5.95423046350902,
11.5492269630659));
#21255=CARTESIAN_POINT('Ctrl Pts',(-3.86353166493297,-5.85070505465455,
11.540695094792));
#21256=CARTESIAN_POINT('Ctrl Pts',(-3.88380588795173,-5.8373169070923,11.5395917336684));
#21257=CARTESIAN_POINT('Ctrl Pts',(-3.90401009570616,-5.82382365557448,
11.5384883725449));
#21258=CARTESIAN_POINT('Ctrl Pts',(-3.9241431869757,-5.8102260550354,11.5373850114213));
#21259=CARTESIAN_POINT('Ctrl Pts',(-4.07984083597495,-5.70507010021346,
11.5288522565334));
#21260=CARTESIAN_POINT('Ctrl Pts',(-4.23133535648263,-5.59363451442266,
11.5203195016455));
#21261=CARTESIAN_POINT('Ctrl Pts',(-4.37812552338029,-5.47628007538202,
11.5117867467576));
#21262=CARTESIAN_POINT('Ctrl Pts',(-4.5248882993246,-5.35894753460632,11.5032555840765));
#21263=CARTESIAN_POINT('Ctrl Pts',(-4.66694823463972,-5.23569853562443,
11.4947244213953));
#21264=CARTESIAN_POINT('Ctrl Pts',(-4.80383626920622,-5.10693485969411,
11.4861932587141));
#21265=CARTESIAN_POINT('Ctrl Pts',(-4.94661215011428,-4.97263278341599,
11.4772951525295));
#21266=CARTESIAN_POINT('Ctrl Pts',(-5.0837611095287,-4.83233136739081,11.4683970463449));
#21267=CARTESIAN_POINT('Ctrl Pts',(-5.21479200244674,-4.68653079939923,
11.4594989401603));
#21268=CARTESIAN_POINT('Ctrl Pts',(-5.34041562011959,-4.54674700947027,
11.4509680337118));
#21269=CARTESIAN_POINT('Ctrl Pts',(-5.46041576835826,-4.40190906956675,
11.4424371272633));
#21270=CARTESIAN_POINT('Ctrl Pts',(-5.57439918826281,-4.25249341591436,
11.4339062208148));
#21271=CARTESIAN_POINT('Ctrl Pts',(-5.68838378442128,-4.10307622036448,
11.4253752263315));
#21272=CARTESIAN_POINT('Ctrl Pts',(-5.79635134520065,-3.94908146185761,
11.4168442318482));
#21273=CARTESIAN_POINT('Ctrl Pts',(-5.89795027185349,-3.79101690226295,
11.4083132373648));
#21274=CARTESIAN_POINT('Ctrl Pts',(-5.99956928600698,-3.6329210911379,11.3997805561869));
#21275=CARTESIAN_POINT('Ctrl Pts',(-6.0948169865471,-3.47075412969225,11.391247875009));
#21276=CARTESIAN_POINT('Ctrl Pts',(-6.18338583687873,-3.30505161151647,
11.3827151938311));
#21277=CARTESIAN_POINT('Ctrl Pts',(-6.19480105215372,-3.28369500691449,
11.3816154573871));
#21278=CARTESIAN_POINT('Ctrl Pts',(-6.206105384523,-3.26227970605504,11.380515720943));
#21279=CARTESIAN_POINT('Ctrl Pts',(-6.21729823109895,-3.24080688534105,
11.379415984499));
#21280=CARTESIAN_POINT('Ctrl Pts',(-6.30401649225029,-3.07444297945732,
11.3708956111063));
#21281=CARTESIAN_POINT('Ctrl Pts',(-6.38406895189986,-2.90456677305934,
11.3623752377136));
#21282=CARTESIAN_POINT('Ctrl Pts',(-6.4571870356737,-2.73173244459035,11.3538548643209));
#21283=CARTESIAN_POINT('Ctrl Pts',(-6.49768850790942,-2.63599628200822,
11.3491352703629));
#21284=CARTESIAN_POINT('Ctrl Pts',(-6.53606315568444,-2.53935291514877,
11.3444156764049));
#21285=CARTESIAN_POINT('Ctrl Pts',(-6.5722715952584,-2.44189939200198,11.3396960824468));
#21286=CARTESIAN_POINT('Origin',(0.,0.,0.));
#21287=CARTESIAN_POINT('',(-6.57271212262447,-2.44206338026677,9.33970533813071));
#21288=CARTESIAN_POINT('',(-6.57227161595961,-2.44189933628552,9.88702363219766));
#21289=CARTESIAN_POINT('',(-6.57227159525839,-2.441899392002,0.));
#21290=CARTESIAN_POINT('Ctrl Pts',(-6.57227161595961,-2.44189933628553,
9.88702363219766));
#21291=CARTESIAN_POINT('Ctrl Pts',(-6.51762240584789,-2.58898543730319,
9.89408880535383));
#21292=CARTESIAN_POINT('Ctrl Pts',(-6.45804127549252,-2.73422160451104,
9.90112533428217));
#21293=CARTESIAN_POINT('Ctrl Pts',(-6.32050475483063,-3.03983391538899,
9.9161417230889));
#21294=CARTESIAN_POINT('Ctrl Pts',(-6.24121965749755,-3.19946044381868,
9.92411325297914));
#21295=CARTESIAN_POINT('Ctrl Pts',(-6.11223957183643,-3.43605736682013,
9.9362397569631));
#21296=CARTESIAN_POINT('Ctrl Pts',(-6.06697651764124,-3.51536036210359,
9.94035982170694));
#21297=CARTESIAN_POINT('Ctrl Pts',(-5.98324838294239,-3.65561982138901,
9.94776882569942));
#21298=CARTESIAN_POINT('Ctrl Pts',(-5.9453677641879,-3.71690992711833,9.95105047946258));
#21299=CARTESIAN_POINT('Ctrl Pts',(-5.75005793117126,-4.02229054076895,
9.96761214156557));
#21300=CARTESIAN_POINT('Ctrl Pts',(-5.57851329092103,-4.25701494818049,
9.98101286913493));
#21301=CARTESIAN_POINT('Ctrl Pts',(-5.25091078917215,-4.65133717236473,
10.0045529312005));
#21302=CARTESIAN_POINT('Ctrl Pts',(-5.10086799233868,-4.81540753602125,
10.0147087041653));
#21303=CARTESIAN_POINT('Ctrl Pts',(-4.79578592306985,-5.11872300716941,
10.0342419513189));
#21304=CARTESIAN_POINT('Ctrl Pts',(-4.6418321302037,-5.2587340838535,10.0436185698762));
#21305=CARTESIAN_POINT('Ctrl Pts',(-4.2556159616202,-5.57977871216393,10.0661751552068));
#21306=CARTESIAN_POINT('Ctrl Pts',(-4.01773809173377,-5.75343168441,10.079291564606));
#21307=CARTESIAN_POINT('Ctrl Pts',(-3.67642124952051,-5.97107872646848,
10.0975306483328));
#21308=CARTESIAN_POINT('Ctrl Pts',(-3.58179319708035,-6.0283174766224,10.1025332653719));
#21309=CARTESIAN_POINT('Ctrl Pts',(-3.31669639046982,-6.18022328041213,
10.1164484658459));
#21310=CARTESIAN_POINT('Ctrl Pts',(-3.14357478625064,-6.27005350110009,
10.1254083506845));
#21311=CARTESIAN_POINT('Ctrl Pts',(-2.7699440223517,-6.44455645268922,10.1443775580678));
#21312=CARTESIAN_POINT('Ctrl Pts',(-2.56877648051099,-6.52734911140884,
10.1543776019011));
#21313=CARTESIAN_POINT('Ctrl Pts',(-2.18760876375722,-6.66386780209054,
10.172901260487));
#21314=CARTESIAN_POINT('Ctrl Pts',(-2.00866512548279,-6.71997263185898,
10.1814318230404));
#21315=CARTESIAN_POINT('Ctrl Pts',(-1.57069367109145,-6.83823139087503,
10.2019655360749));
#21316=CARTESIAN_POINT('Ctrl Pts',(-1.30995575265783,-6.89293156931636,
10.213900741442));
#21317=CARTESIAN_POINT('Ctrl Pts',(-0.878476050524959,-6.95807903350122,
10.2334512641542));
#21318=CARTESIAN_POINT('Ctrl Pts',(-0.709346064056967,-6.97734989399436,
10.2410676747381));
#21319=CARTESIAN_POINT('Ctrl Pts',(-0.424049143539064,-6.99937568506481,
10.2539486733267));
#21320=CARTESIAN_POINT('Ctrl Pts',(-0.308212743978904,-7.00543234021471,
10.2591890117709));
#21321=CARTESIAN_POINT('Ctrl Pts',(-0.0264193122047767,-7.01316324078707,
10.2720173889338));
#21322=CARTESIAN_POINT('Ctrl Pts',(0.139547824788628,-7.01182443707065,
10.2796303008101));
#21323=CARTESIAN_POINT('Ctrl Pts',(0.541243966839384,-6.99431573436788,
10.2981157264964));
#21324=CARTESIAN_POINT('Ctrl Pts',(0.776510315685194,-6.97211808650129,
10.3089888385472));
#21325=CARTESIAN_POINT('Ctrl Pts',(1.2004806249356,-6.91038668517117,10.32860773548));
#21326=CARTESIAN_POINT('Ctrl Pts',(1.38953526965262,-6.87486663744936,10.337366492301));
#21327=CARTESIAN_POINT('Ctrl Pts',(1.95067873795822,-6.74534202977916,10.3634537381735));
#21328=CARTESIAN_POINT('Ctrl Pts',(2.31675378507399,-6.6285323656769,10.3805621416503));
#21329=CARTESIAN_POINT('Ctrl Pts',(2.7433928068384,-6.45271105158333,10.4012659490627));
#21330=CARTESIAN_POINT('Ctrl Pts',(2.81485236618666,-6.42186032725736,10.4047623547499));
#21331=CARTESIAN_POINT('Ctrl Pts',(2.98710269862579,-6.34406837018094,10.4132771180454));
#21332=CARTESIAN_POINT('Ctrl Pts',(3.08731764523307,-6.29590783916845,10.4183057844006));
#21333=CARTESIAN_POINT('Ctrl Pts',(3.36251317937058,-6.15550524957702,10.4323746978447));
#21334=CARTESIAN_POINT('Ctrl Pts',(3.53479713651178,-6.05821322771792,10.4414645134852));
#21335=CARTESIAN_POINT('Ctrl Pts',(3.88664415092642,-5.83939447952108,10.4605244610784));
#21336=CARTESIAN_POINT('Ctrl Pts',(4.06515577942432,-5.7165584402882,10.470485048554));
#21337=CARTESIAN_POINT('Ctrl Pts',(4.38687543276301,-5.47247791034489,10.4889598807142));
#21338=CARTESIAN_POINT('Ctrl Pts',(4.53146252602292,-5.35336711657016,10.4974807945599));
#21339=CARTESIAN_POINT('Ctrl Pts',(4.86244014367859,-5.05768000030014,10.517568447996));
#21340=CARTESIAN_POINT('Ctrl Pts',(5.04424571542985,-4.87637556642389,10.5290762249333));
#21341=CARTESIAN_POINT('Ctrl Pts',(5.33309355258108,-4.55484295693266,10.5484421446617));
#21342=CARTESIAN_POINT('Ctrl Pts',(5.44552842118192,-4.41980777611782,10.5563020944382));
#21343=CARTESIAN_POINT('Ctrl Pts',(5.62455298352339,-4.18758311307204,10.5694986651677));
#21344=CARTESIAN_POINT('Ctrl Pts',(5.69397864543999,-4.09268316264512,10.574809189654));
#21345=CARTESIAN_POINT('Ctrl Pts',(5.8870366916296,-3.81435938653101,10.5902206386414));
#21346=CARTESIAN_POINT('Ctrl Pts',(6.0044176776675,-3.62677611370168,10.6003915984051));
#21347=CARTESIAN_POINT('Ctrl Pts',(6.18450929334813,-3.30619818116145,10.6173072410649));
#21348=CARTESIAN_POINT('Ctrl Pts',(6.25226028079838,-3.17621524770333,10.6240471438371));
#21349=CARTESIAN_POINT('Ctrl Pts',(6.40518254887975,-2.85894354132475,10.640200270286));
#21350=CARTESIAN_POINT('Ctrl Pts',(6.48628323939134,-2.66984145280694,10.6495855553476));
#21351=CARTESIAN_POINT('Ctrl Pts',(6.70458493281666,-2.09189512656837,10.677608857111));
#21352=CARTESIAN_POINT('Ctrl Pts',(6.81593652484964,-1.69425410793386,10.6959802067608));
#21353=CARTESIAN_POINT('Ctrl Pts',(6.91991948936726,-1.13836269427626,10.7213591962988));
#21354=CARTESIAN_POINT('Ctrl Pts',(6.94316715844705,-0.986703622890623,
10.7282597266194));
#21355=CARTESIAN_POINT('Ctrl Pts',(6.97706241459874,-0.703916761765895,
10.7411871259644));
#21356=CARTESIAN_POINT('Ctrl Pts',(6.98903082294839,-0.573014812917868,
10.7471972471737));
#21357=CARTESIAN_POINT('Ctrl Pts',(7.0142992367176,-0.172859458991969,10.7655938370517));
#21358=CARTESIAN_POINT('Ctrl Pts',(7.01575989333482,0.0968931036385455,
10.7780201520149));
#21359=CARTESIAN_POINT('Ctrl Pts',(6.99120461956265,0.566566323511386,10.7995799439267));
#21360=CARTESIAN_POINT('Ctrl Pts',(6.97211369562239,0.766532399307416,10.8087374299901));
#21361=CARTESIAN_POINT('Ctrl Pts',(6.89084093122266,1.35115325549083,10.835499824254));
#21362=CARTESIAN_POINT('Ctrl Pts',(6.80516743311891,1.73176318492726,10.8528774873014));
#21363=CARTESIAN_POINT('Ctrl Pts',(6.65253299002974,2.21713180387593,10.8756986023177));
#21364=CARTESIAN_POINT('Ctrl Pts',(6.61383188627202,2.33004205718452,10.881059826954));
#21365=CARTESIAN_POINT('Ctrl Pts',(6.53593583032247,2.53969519001638,10.8911609701844));
#21366=CARTESIAN_POINT('Ctrl Pts',(6.49742638804987,2.63665673149079,10.8958964342839));
#21367=CARTESIAN_POINT('Ctrl Pts',(6.43397333021965,2.78658106661638,10.903327387717));
#21368=CARTESIAN_POINT('Ctrl Pts',(6.41050585578187,2.84015166289279,10.9060035418419));
#21369=CARTESIAN_POINT('Ctrl Pts',(6.30886895009647,3.06448498182338,10.9172924716424));
#21370=CARTESIAN_POINT('Ctrl Pts',(6.2245253379365,3.23236440123658,10.9259407930786));
#21371=CARTESIAN_POINT('Ctrl Pts',(6.01710439291466,3.60691695122986,10.9456273632757));
#21372=CARTESIAN_POINT('Ctrl Pts',(5.88992825716127,3.81105536776905,10.9566414549474));
#21373=CARTESIAN_POINT('Ctrl Pts',(5.64487538177079,4.16274687558152,10.9761461698522));
#21374=CARTESIAN_POINT('Ctrl Pts',(5.53105151068204,4.31283553272978,10.9846603269234));
#21375=CARTESIAN_POINT('Ctrl Pts',(5.27110849168164,4.62835474488067,11.003064908825));
#21376=CARTESIAN_POINT('Ctrl Pts',(5.12294230223431,4.79183839937538,11.0129301723434));
#21377=CARTESIAN_POINT('Ctrl Pts',(4.83664867131311,5.07924584703895,11.0311089472987));
#21378=CARTESIAN_POINT('Ctrl Pts',(4.70083553667646,5.20519475819294,11.0394115609546));
#21379=CARTESIAN_POINT('Ctrl Pts',(4.47787191605606,5.39611312201303,11.0527001027281));
#21380=CARTESIAN_POINT('Ctrl Pts',(4.39392325949565,5.46468767089453,11.0576373113752));
#21381=CARTESIAN_POINT('Ctrl Pts',(4.08061042854539,5.70873269425712,11.0758079697497));
#21382=CARTESIAN_POINT('Ctrl Pts',(3.84205659407507,5.87193422859419,11.089131372587));
#21383=CARTESIAN_POINT('Ctrl Pts',(3.41072574415941,6.12945339580312,11.112187510178));
#21384=CARTESIAN_POINT('Ctrl Pts',(3.2224210313739,6.23050992419217,11.1219433703731));
#21385=CARTESIAN_POINT('Ctrl Pts',(2.83684123565165,6.41527384596874,11.1413490694916));
#21386=CARTESIAN_POINT('Ctrl Pts',(2.63975436000385,6.49885417451629,11.1509885745107));
#21387=CARTESIAN_POINT('Ctrl Pts',(2.18345875332125,6.66817185658736,11.172837904468));
#21388=CARTESIAN_POINT('Ctrl Pts',(1.9224485876417,6.7480514094493,11.1850045331482));
#21389=CARTESIAN_POINT('Ctrl Pts',(1.54662906275811,6.83948637163849,11.2024213306914));
#21390=CARTESIAN_POINT('Ctrl Pts',(1.43516671663417,6.86374034430369,11.2075771295441));
#21391=CARTESIAN_POINT('Ctrl Pts',(1.11587999504838,6.92509861165761,11.2223769349407));
#21392=CARTESIAN_POINT('Ctrl Pts',(0.9069072500884,6.95555148905481,11.2320809534955));
#21393=CARTESIAN_POINT('Ctrl Pts',(0.391244118470795,7.00706081258822,11.2559179448643));
#21394=CARTESIAN_POINT('Ctrl Pts',(0.0839256937663981,7.01747353883307,
11.2700204760206));
#21395=CARTESIAN_POINT('Ctrl Pts',(-0.413636373146145,7.00163392910981,
11.292665735672));
#21396=CARTESIAN_POINT('Ctrl Pts',(-0.603861598999197,6.98779832665097,
11.3012831167896));
#21397=CARTESIAN_POINT('Ctrl Pts',(-1.01987667185492,6.94042407261498,11.3201271543642));
#21398=CARTESIAN_POINT('Ctrl Pts',(-1.24507170085294,6.90358108477314,11.3303252104165));
#21399=CARTESIAN_POINT('Ctrl Pts',(-1.64721206087191,6.81746889605279,11.3487590302395));
#21400=CARTESIAN_POINT('Ctrl Pts',(-1.82477901356867,6.77210230553286,11.3569804818862));
#21401=CARTESIAN_POINT('Ctrl Pts',(-2.11069775697616,6.68698991719773,11.3705028475107));
#21402=CARTESIAN_POINT('Ctrl Pts',(-2.22020526724276,6.65143344332621,11.3757565415309));
#21403=CARTESIAN_POINT('Ctrl Pts',(-2.48733894101406,6.55736440888498,11.3887319458267));
#21404=CARTESIAN_POINT('Ctrl Pts',(-2.64383223071761,6.49584742068739,11.3964699746497));
#21405=CARTESIAN_POINT('Ctrl Pts',(-3.04502846612994,6.32123662186997,11.4166011836916));
#21406=CARTESIAN_POINT('Ctrl Pts',(-3.28569351286677,6.19955261298194,11.4289646091));
#21407=CARTESIAN_POINT('Ctrl Pts',(-3.67912501766784,5.97126797665015,11.4496685080679));
#21408=CARTESIAN_POINT('Ctrl Pts',(-3.83573818057884,5.87189204844748,11.4580554812727));
#21409=CARTESIAN_POINT('Ctrl Pts',(-4.16331957965394,5.64532706820208,11.475992771616));
#21410=CARTESIAN_POINT('Ctrl Pts',(-4.33280375077929,5.51631761760486,11.4855211136814));
#21411=CARTESIAN_POINT('Ctrl Pts',(-4.65538494494174,5.24672094438443,11.5043566661358));
#21412=CARTESIAN_POINT('Ctrl Pts',(-4.80862572420868,5.10664333334677,11.513654565168));
#21413=CARTESIAN_POINT('Ctrl Pts',(-5.03673802868101,4.87874039587905,11.5282644410476));
#21414=CARTESIAN_POINT('Ctrl Pts',(-5.11603891018911,4.7955169476786,11.5335072557764));
#21415=CARTESIAN_POINT('Ctrl Pts',(-5.30451285525896,4.58772204805573,11.5463541632336));
#21416=CARTESIAN_POINT('Ctrl Pts',(-5.41138774546143,4.46115819730193,11.5539736695724));
#21417=CARTESIAN_POINT('Ctrl Pts',(-5.68441422288503,4.11356984621427,11.5743030093896));
#21418=CARTESIAN_POINT('Ctrl Pts',(-5.84214761820814,3.88630120225712,11.5869823553165));
#21419=CARTESIAN_POINT('Ctrl Pts',(-6.08535813166758,3.48746661279745,11.6082379413393));
#21420=CARTESIAN_POINT('Ctrl Pts',(-6.1779768905738,3.32063398571776,11.6168620472632));
#21421=CARTESIAN_POINT('Ctrl Pts',(-6.36500977153988,2.94875209548686,11.6356014570337));
#21422=CARTESIAN_POINT('Ctrl Pts',(-6.45656080620148,2.74250096205975,11.6456896942329));
#21423=CARTESIAN_POINT('Ctrl Pts',(-6.60388423113676,2.36211877169742,11.6639736233574));
#21424=CARTESIAN_POINT('Ctrl Pts',(-6.66309359073516,2.18953746448094,11.6721564786899));
#21425=CARTESIAN_POINT('Ctrl Pts',(-6.74793885066732,1.9067472804535,11.6855299257916));
#21426=CARTESIAN_POINT('Ctrl Pts',(-6.77775634056871,1.79788265699346,11.6906754748465));
#21427=CARTESIAN_POINT('Ctrl Pts',(-6.82430473967137,1.61026801188825,11.6995247280581));
#21428=CARTESIAN_POINT('Ctrl Pts',(-6.84233144297624,1.53186114772224,11.703216886361));
#21429=CARTESIAN_POINT('Ctrl Pts',(-6.93580265587684,1.09067180451096,11.7239392513773));
#21430=CARTESIAN_POINT('Ctrl Pts',(-6.98374533615733,0.722656878633498,
11.740987542979));
#21431=CARTESIAN_POINT('Ctrl Pts',(-7.01103032324011,0.180763667780065,
11.7656614780392));
#21432=CARTESIAN_POINT('Ctrl Pts',(-7.01335493138627,0.00868728982689054,
11.7734403708871));
#21433=CARTESIAN_POINT('Ctrl Pts',(-7.00437694985596,-0.376671595304211,
11.7907988943065));
#21434=CARTESIAN_POINT('Ctrl Pts',(-6.98966581540148,-0.589703733476513,
11.8003510528075));
#21435=CARTESIAN_POINT('Ctrl Pts',(-6.94176054474013,-1.00589288757262,
11.8191213762882));
#21436=CARTESIAN_POINT('Ctrl Pts',(-6.90929625709629,-1.20891814052628,
11.828330230728));
#21437=CARTESIAN_POINT('Ctrl Pts',(-6.84831033691245,-1.50592764867967,
11.8420686108816));
#21438=CARTESIAN_POINT('Ctrl Pts',(-6.82666055077586,-1.60121131827594,
11.8465213691738));
#21439=CARTESIAN_POINT('Ctrl Pts',(-6.77259581639827,-1.81807547267181,
11.856753370197));
#21440=CARTESIAN_POINT('Ctrl Pts',(-6.73888511412836,-1.93929871884705,
11.8625411399511));
#21441=CARTESIAN_POINT('Ctrl Pts',(-6.66237564907765,-2.18826650712128,
11.8745430404549));
#21442=CARTESIAN_POINT('Ctrl Pts',(-6.61913498672279,-2.31576848709062,
11.8807535285185));
#21443=CARTESIAN_POINT('Ctrl Pts',(-6.5722717076903,-2.44189908939613,11.8869527148536));
#21444=CARTESIAN_POINT('',(-7.0113586937745,3.84368575559509E-5,11.2264656437582));
#21445=CARTESIAN_POINT('Ctrl Pts',(-6.5722715952584,-2.44189939200198,11.3396960824468));
#21446=CARTESIAN_POINT('Ctrl Pts',(-6.63762197368278,-2.26601154123109,
11.3311779785242));
#21447=CARTESIAN_POINT('Ctrl Pts',(-6.695913184144,-2.0874837403581,11.3226598746016));
#21448=CARTESIAN_POINT('Ctrl Pts',(-6.74695164053556,-1.90690065886363,
11.314141770679));
#21449=CARTESIAN_POINT('Ctrl Pts',(-6.79799297831796,-1.72630738249899,
11.3056231858644));
#21450=CARTESIAN_POINT('Ctrl Pts',(-6.84178065721233,-1.54365888898769,
11.2971046010498));
#21451=CARTESIAN_POINT('Ctrl Pts',(-6.87817116927801,-1.35955431249099,
11.2885860162351));
#21452=CARTESIAN_POINT('Ctrl Pts',(-6.91456102987243,-1.17545303187645,
11.2800675839221));
#21453=CARTESIAN_POINT('Ctrl Pts',(-6.94355393105551,-0.989896022773728,
11.2715491516092));
#21454=CARTESIAN_POINT('Ctrl Pts',(-6.9650575549051,-0.80349226465435,11.2630307192962));
#21455=CARTESIAN_POINT('Ctrl Pts',(-6.98656581623424,-0.617048306630923,
11.2545104498949));
#21456=CARTESIAN_POINT('Ctrl Pts',(-7.00058153847027,-0.429757540599929,
11.2459901804936));
#21457=CARTESIAN_POINT('Ctrl Pts',(-7.00706421654034,-0.242234654374432,
11.2374699110923));
#21458=CARTESIAN_POINT('Ctrl Pts',(-7.00985509548824,-0.161503563032406,
11.2338018220332));
#21459=CARTESIAN_POINT('Ctrl Pts',(-7.01125044263142,-0.0807294898144902,
11.2301337329741));
#21460=CARTESIAN_POINT('Ctrl Pts',(-7.01124999989467,3.84328085378804E-5,
11.226465643915));
#21461=CARTESIAN_POINT('Ctrl Pts',(-7.01182214408909,3.84541218094794E-5,
11.2264656430896));
#21462=CARTESIAN_POINT('Ctrl Pts',(-7.01183325597241,0.036877061846341,
11.2247927479186));
#21463=CARTESIAN_POINT('Ctrl Pts',(-7.01154895025294,0.0737154962315686,
11.2231198527476));
#21464=CARTESIAN_POINT('Ctrl Pts',(-6.99268714592644,1.26993509149134,11.1687906152692));
#21465=CARTESIAN_POINT('Ctrl Pts',(-6.36864378850638,3.57944046714196,11.0634779306544));
#21466=CARTESIAN_POINT('Ctrl Pts',(-3.89598737047602,6.18007435040298,10.9055089037321));
#21467=CARTESIAN_POINT('Ctrl Pts',(-0.483327077985568,7.28961040383802,
10.7475398768098));
#21468=CARTESIAN_POINT('Ctrl Pts',(3.04594747324975,6.64034897205148,10.5895708498875));
#21469=CARTESIAN_POINT('Ctrl Pts',(5.84031211439899,4.3889387019149,10.4316018229652));
#21470=CARTESIAN_POINT('Ctrl Pts',(7.22555706859702,1.07858883068963,10.2736327960429));
#21471=CARTESIAN_POINT('Ctrl Pts',(6.86745790157161,-2.49199739961005,10.1156637691206));
#21472=CARTESIAN_POINT('Ctrl Pts',(4.85241481466244,-5.46132760686174,9.95769474219825));
#21473=CARTESIAN_POINT('Ctrl Pts',(1.66660677536437,-7.11297763457679,9.79972571527604));
#21474=CARTESIAN_POINT('Ctrl Pts',(-1.92131133239526,-7.04844604350416,
9.64175668835372));
#21475=CARTESIAN_POINT('Ctrl Pts',(-4.95411394330101,-5.3350259731329,9.48841656263841));
#21476=CARTESIAN_POINT('Ctrl Pts',(-6.2036482880654,-3.43323261796278,9.3877327792305));
#21477=CARTESIAN_POINT('Ctrl Pts',(-6.57271212262969,-2.44206338025277,
9.33970533813003));
#21478=CARTESIAN_POINT('Origin',(0.,0.,0.));
#21479=CARTESIAN_POINT('',(-6.5722715952584,-2.44189939200199,7.33970278241542));
#21480=CARTESIAN_POINT('',(-6.57280081548431,-2.44209581534386,7.88676746742487));
#21481=CARTESIAN_POINT('',(-6.57227159525839,-2.441899392002,0.));
#21482=CARTESIAN_POINT('',(-7.01170386511408,-0.000104878804555574,9.77353434367529));
#21483=CARTESIAN_POINT('Ctrl Pts',(-6.57280081548428,-2.44209581534395,
7.88676746742488));
#21484=CARTESIAN_POINT('Ctrl Pts',(-6.55738010449231,-2.48364608990916,
7.88878007829007));
#21485=CARTESIAN_POINT('Ctrl Pts',(-6.12762765860759,-3.60823497536755,
7.9434490314627));
#21486=CARTESIAN_POINT('Ctrl Pts',(-4.70540847483628,-5.58848458735646,
8.05077432694275));
#21487=CARTESIAN_POINT('Ctrl Pts',(-1.47678875996353,-7.15479726159574,
8.20874335386504));
#21488=CARTESIAN_POINT('Ctrl Pts',(2.10814273077403,-6.99483832025251,8.36671238078733));
#21489=CARTESIAN_POINT('Ctrl Pts',(5.18443270117429,-5.14720180894841,8.52468140770962));
#21490=CARTESIAN_POINT('Ctrl Pts',(7.00985018797118,-2.05767568861079,8.68265043463191));
#21491=CARTESIAN_POINT('Ctrl Pts',(7.14396812247892,1.5283155343373,8.8406194615542));
#21492=CARTESIAN_POINT('Ctrl Pts',(5.55442723662981,4.74556286831861,8.99858848847649));
#21493=CARTESIAN_POINT('Ctrl Pts',(2.62474354776114,6.81782592049456,9.15655751539878));
#21494=CARTESIAN_POINT('Ctrl Pts',(-0.938224379280222,7.24511999742922,
9.31452654232109));
#21495=CARTESIAN_POINT('Ctrl Pts',(-4.27482248085003,5.9243499075208,9.47249556924335));
#21496=CARTESIAN_POINT('Ctrl Pts',(-6.50754058792984,3.26064708099906,9.62549816969478));
#21497=CARTESIAN_POINT('Ctrl Pts',(-7.01093898172325,1.05011949196855,9.72584442783875));
#21498=CARTESIAN_POINT('Ctrl Pts',(-7.01170386511407,-0.000104878804555574,
9.77353434367529));
#21499=CARTESIAN_POINT('Ctrl Pts',(-7.01124999902501,-0.000116926258460787,
9.77327286327579));
#21500=CARTESIAN_POINT('Ctrl Pts',(-7.01124832255164,-0.100643310223616,
9.77779485366763));
#21501=CARTESIAN_POINT('Ctrl Pts',(-7.00908464412642,-0.201157219552033,
9.78232974651185));
#21502=CARTESIAN_POINT('Ctrl Pts',(-7.00040283391986,-0.402802601350129,
9.79148686211807));
#21503=CARTESIAN_POINT('Ctrl Pts',(-6.99385196405524,-0.503908655088689,
9.79611034983023));
#21504=CARTESIAN_POINT('Ctrl Pts',(-6.95413787236706,-0.962557765689151,
9.81719252923423));
#21505=CARTESIAN_POINT('Ctrl Pts',(-6.89572929599919,-1.31737321865183,
9.83376990625039));
#21506=CARTESIAN_POINT('Ctrl Pts',(-6.76873539423717,-1.83646088146557,
9.85820301925403));
#21507=CARTESIAN_POINT('Ctrl Pts',(-6.72069575740167,-2.00514768445086,
9.86617845663394));
#21508=CARTESIAN_POINT('Ctrl Pts',(-6.6368466352524,-2.26251737183206,9.87842964187306));
#21509=CARTESIAN_POINT('Ctrl Pts',(-6.60546909578075,-2.35254968492693,
9.8827317871224));
#21510=CARTESIAN_POINT('Ctrl Pts',(-6.57227161595961,-2.44189933628552,
9.88702363219766));
#21511=CARTESIAN_POINT('',(-7.01124999890517,0.000123904338948809,9.22646564308964));
#21512=CARTESIAN_POINT('Ctrl Pts',(-6.57271212262969,-2.44206338025277,
9.33970533813003));
#21513=CARTESIAN_POINT('Ctrl Pts',(-6.60828262128868,-2.3465341499709,9.33507643692307));
#21514=CARTESIAN_POINT('Ctrl Pts',(-6.88115023186467,-1.56117498902781,
9.29732987190961));
#21515=CARTESIAN_POINT('Ctrl Pts',(-7.01034884492464,-0.729457585781793,
9.25958330689615));
#21516=CARTESIAN_POINT('Ctrl Pts',(-7.01081502653957,0.000123896652022004,
9.22646564308964));
#21517=CARTESIAN_POINT('Ctrl Pts',(-7.01124999890517,0.000123904338948809,
9.22646564308964));
#21518=CARTESIAN_POINT('Ctrl Pts',(-7.01124658275476,0.193430165674024,
9.21769149676437));
#21519=CARTESIAN_POINT('Ctrl Pts',(-7.00324439628698,0.386702906863349,
9.20891735043909));
#21520=CARTESIAN_POINT('Ctrl Pts',(-6.98727771593147,0.579289809117614,
9.20014320411381));
#21521=CARTESIAN_POINT('Ctrl Pts',(-6.97130597709455,0.771937725762138,
9.1913662780087));
#21522=CARTESIAN_POINT('Ctrl Pts',(-6.94736472578101,0.963899103762233,
9.18258935190358));
#21523=CARTESIAN_POINT('Ctrl Pts',(-6.91554014229809,1.15452635429589,9.17381242579847));
#21524=CARTESIAN_POINT('Ctrl Pts',(-6.90833320736833,1.19769544058329,9.17182481972793));
#21525=CARTESIAN_POINT('Ctrl Pts',(-6.90072219846778,1.24079613936,9.1698372136574));
#21526=CARTESIAN_POINT('Ctrl Pts',(-6.89270848282156,1.28382098960083,9.16784960758686));
#21527=CARTESIAN_POINT('Ctrl Pts',(-6.85830735406572,1.46851726261298,9.15931724939412));
#21528=CARTESIAN_POINT('Ctrl Pts',(-6.81647250719612,1.65186114390348,9.15078489120138));
#21529=CARTESIAN_POINT('Ctrl Pts',(-6.76733506680133,1.83324920732045,9.14225253300863));
#21530=CARTESIAN_POINT('Ctrl Pts',(-6.7182068275768,2.0146033051413,9.13372177253201));
#21531=CARTESIAN_POINT('Ctrl Pts',(-6.6617788037032,2.1940020207426,9.12519101205538));
#21532=CARTESIAN_POINT('Ctrl Pts',(-6.59823254511356,2.3708550869052,9.11666025157876));
#21533=CARTESIAN_POINT('Ctrl Pts',(-6.5319484137181,2.55532781803658,9.10776194566924));
#21534=CARTESIAN_POINT('Ctrl Pts',(-6.45791918342226,2.73703034380715,9.09886363975973));
#21535=CARTESIAN_POINT('Ctrl Pts',(-6.37640791234427,2.91531279589232,9.08996533385021));
#21536=CARTESIAN_POINT('Ctrl Pts',(-6.2982658840008,3.08622599893454,9.08143483661474));
#21537=CARTESIAN_POINT('Ctrl Pts',(-6.21324805037836,3.25399588188927,9.07290433937927));
#21538=CARTESIAN_POINT('Ctrl Pts',(-6.121634643497,3.41807194980407,9.06437384214381));
#21539=CARTESIAN_POINT('Ctrl Pts',(-6.03002029908661,3.58214969679708,9.0558432576112));
#21540=CARTESIAN_POINT('Ctrl Pts',(-5.93181039853669,3.74253328763762,9.04731267307858));
#21541=CARTESIAN_POINT('Ctrl Pts',(-5.82733050628654,3.89869795354838,9.03878208854597));
#21542=CARTESIAN_POINT('Ctrl Pts',(-5.72282993987773,4.0548935208413,9.03024981600762));
#21543=CARTESIAN_POINT('Ctrl Pts',(-5.61205707474818,4.20686824205592,9.02171754346927));
#21544=CARTESIAN_POINT('Ctrl Pts',(-5.49538056018055,4.35412667033123,9.01318527093092));
#21545=CARTESIAN_POINT('Ctrl Pts',(-5.48031697892598,4.37313854523996,9.0120837075088));
#21546=CARTESIAN_POINT('Ctrl Pts',(-5.46515505065842,4.39207185135154,9.01098214408669));
#21547=CARTESIAN_POINT('Ctrl Pts',(-5.4498956183453,4.41092556178867,9.00988058066457));
#21548=CARTESIAN_POINT('Ctrl Pts',(-5.33170093238843,4.55696037740384,9.00134822244397));
#21549=CARTESIAN_POINT('Ctrl Pts',(-5.2076132572532,4.69826636571517,8.99281586422336));
#21550=CARTESIAN_POINT('Ctrl Pts',(-5.07803522196381,4.83437533162196,8.98428350600275));
#21551=CARTESIAN_POINT('Ctrl Pts',(-4.94848145064301,4.97045881061915,8.97575274549793));
#21552=CARTESIAN_POINT('Ctrl Pts',(-4.81343958175058,5.10134698776302,8.96722198499311));
#21553=CARTESIAN_POINT('Ctrl Pts',(-4.67335032081439,5.22660724958783,8.95869122448828));
#21554=CARTESIAN_POINT('Ctrl Pts',(-4.52722535390439,5.35726431417628,8.94979291859278));
#21555=CARTESIAN_POINT('Ctrl Pts',(-4.37560867694897,5.48179751437576,8.94089461269728));
#21556=CARTESIAN_POINT('Ctrl Pts',(-4.21904104994549,5.59976063607855,8.93199630680178));
#21557=CARTESIAN_POINT('Ctrl Pts',(-4.06894509578705,5.7128477898303,8.92346580953782));
#21558=CARTESIAN_POINT('Ctrl Pts',(-3.91429951543427,5.81989689243582,8.91493531227385));
#21559=CARTESIAN_POINT('Ctrl Pts',(-3.75561285408614,5.92055729241116,8.90640481500988));
#21560=CARTESIAN_POINT('Ctrl Pts',(-3.5969245688119,6.02121872249862,8.89787423044874));
#21561=CARTESIAN_POINT('Ctrl Pts',(-3.43419538001805,6.11549115814567,8.8893436458876));
#21562=CARTESIAN_POINT('Ctrl Pts',(-3.26796144695351,6.20306815565697,8.88081306132646));
#21563=CARTESIAN_POINT('Ctrl Pts',(-3.10169462003571,6.29066248263194,8.8722807887598));
#21564=CARTESIAN_POINT('Ctrl Pts',(-2.93192193489967,6.37155858359133,8.86374851619314));
#21565=CARTESIAN_POINT('Ctrl Pts',(-2.75920347628835,6.44549631439956,8.85521624362648));
#21566=CARTESIAN_POINT('Ctrl Pts',(-2.73690457375769,6.45504208192138,8.85411468033174));
#21567=CARTESIAN_POINT('Ctrl Pts',(-2.71455659928903,6.46447193081478,8.85301311703701));
#21568=CARTESIAN_POINT('Ctrl Pts',(-2.69216078310632,6.47378535946353,8.85191155374228));
#21569=CARTESIAN_POINT('Ctrl Pts',(-2.51868992849126,6.54592420959144,8.84337919552899));
#21570=CARTESIAN_POINT('Ctrl Pts',(-2.34228864292468,6.61109874328733,8.8348468373157));
#21571=CARTESIAN_POINT('Ctrl Pts',(-2.16353391566274,6.66908896014119,8.82631447910241));
#21572=CARTESIAN_POINT('Ctrl Pts',(-1.98481266088958,6.72706831811085,8.81778371860499));
#21573=CARTESIAN_POINT('Ctrl Pts',(-1.80373913480668,6.77786594956174,8.80925295810757));
#21574=CARTESIAN_POINT('Ctrl Pts',(-1.62090686743586,6.82131127347223,8.80072219761014));
#21575=CARTESIAN_POINT('Ctrl Pts',(-1.43019732356839,6.86662842686801,8.79182389171097));
#21576=CARTESIAN_POINT('Ctrl Pts',(-1.23757446921328,6.90394559042813,8.78292558581179));
#21577=CARTESIAN_POINT('Ctrl Pts',(-1.04372629453956,6.93312786443368,8.77402727991261));
#21578=CARTESIAN_POINT('Ctrl Pts',(-0.857890772477837,6.96110389842987,
8.76549678265607));
#21579=CARTESIAN_POINT('Ctrl Pts',(-0.670929513079274,6.9816039792824,8.75696628539953));
#21580=CARTESIAN_POINT('Ctrl Pts',(-0.483456675624474,6.99456190231341,
8.748435788143));
#21581=CARTESIAN_POINT('Ctrl Pts',(-0.295981919659145,7.00751995794982,
8.73990520358929));
#21582=CARTESIAN_POINT('Ctrl Pts',(-0.107995880649334,7.01293568366323,
8.73137461903558));
#21583=CARTESIAN_POINT('Ctrl Pts',(0.0798840490155643,7.0107948979565,8.72284403448187));
#21584=CARTESIAN_POINT('Ctrl Pts',(0.267801155778221,7.00865368863773,8.71431176192254));
#21585=CARTESIAN_POINT('Ctrl Pts',(0.455611805303478,6.9989529859322,8.70577948936322));
#21586=CARTESIAN_POINT('Ctrl Pts',(0.642699611673814,6.98173071463332,8.6972472168039));
#21587=CARTESIAN_POINT('Ctrl Pts',(0.666853676745562,6.97950722465978,8.69614565347593));
#21588=CARTESIAN_POINT('Ctrl Pts',(0.690995698884943,6.97715843443401,8.69504409014796));
#21589=CARTESIAN_POINT('Ctrl Pts',(0.715124357432948,6.97468448862786,8.69394252681999));
#21590=CARTESIAN_POINT('Ctrl Pts',(0.902017251097917,6.95552209343868,8.68541016860746));
#21591=CARTESIAN_POINT('Ctrl Pts',(1.08817097862681,6.92884020609057,8.67687781039493));
#21592=CARTESIAN_POINT('Ctrl Pts',(1.27297340344457,6.89472010139808,8.6683454521824));
#21593=CARTESIAN_POINT('Ctrl Pts',(1.45774122331942,6.86060638582239,8.65981469168575));
#21594=CARTESIAN_POINT('Ctrl Pts',(1.64115794467901,6.81905728801807,8.65128393118911));
#21595=CARTESIAN_POINT('Ctrl Pts',(1.82262041678906,6.77020541629305,8.64275317069246));
#21596=CARTESIAN_POINT('Ctrl Pts',(2.01190114817992,6.71924877549342,8.63385486479289));
#21597=CARTESIAN_POINT('Ctrl Pts',(2.19905515706665,6.66034621462148,8.62495655889333));
#21598=CARTESIAN_POINT('Ctrl Pts',(2.38341321773614,6.59370669623852,8.61605825299377));
#21599=CARTESIAN_POINT('Ctrl Pts',(2.56015089661138,6.52982170115017,8.60752775573805));
#21600=CARTESIAN_POINT('Ctrl Pts',(2.73431881202718,6.4588266093185,8.59899725848233));
#21601=CARTESIAN_POINT('Ctrl Pts',(2.90534537172126,6.38095563638534,8.59046676122661));
#21602=CARTESIAN_POINT('Ctrl Pts',(3.07637368162198,6.3030838665567,8.58193617667373));
#21603=CARTESIAN_POINT('Ctrl Pts',(3.2442602944321,6.21833620475762,8.57340559212086));
#21604=CARTESIAN_POINT('Ctrl Pts',(3.40845554578905,6.12699415332509,8.56487500756798));
#21605=CARTESIAN_POINT('Ctrl Pts',(3.57268328759253,6.03563402741104,8.55634273500952));
#21606=CARTESIAN_POINT('Ctrl Pts',(3.73321794214793,5.93767705528345,8.54781046245106));
#21607=CARTESIAN_POINT('Ctrl Pts',(3.88953554069426,5.83345008037064,8.5392781898926));
#21608=CARTESIAN_POINT('Ctrl Pts',(3.90971700272182,5.81999380445538,8.53817662656096));
#21609=CARTESIAN_POINT('Ctrl Pts',(3.92982821259818,5.80643307845208,8.53707506322933));
#21610=CARTESIAN_POINT('Ctrl Pts',(3.94986807787101,5.79276865841504,8.5359734998977));
#21611=CARTESIAN_POINT('Ctrl Pts',(4.1050904824131,5.6869284191746,8.52744114168254));
#21612=CARTESIAN_POINT('Ctrl Pts',(4.25608246582144,5.57482777531395,8.51890878346739));
#21613=CARTESIAN_POINT('Ctrl Pts',(4.40234443727481,5.45682966731558,8.51037642525224));
#21614=CARTESIAN_POINT('Ctrl Pts',(4.54857902062949,5.33885365490225,8.50184566475292));
#21615=CARTESIAN_POINT('Ctrl Pts',(4.69008512153923,5.21498257421762,8.49331490425361));
#21616=CARTESIAN_POINT('Ctrl Pts',(4.82639549357391,5.08562022786892,8.4847841437543));
#21617=CARTESIAN_POINT('Ctrl Pts',(4.96857875936425,4.95068434148251,8.47588583785606));
#21618=CARTESIAN_POINT('Ctrl Pts',(5.10510839400903,4.80977375433093,8.46698753195782));
#21619=CARTESIAN_POINT('Ctrl Pts',(5.23549540348985,4.66339087387458,8.45808922605958));
#21620=CARTESIAN_POINT('Ctrl Pts',(5.36049290746771,4.52305868315257,8.44955872880114));
#21621=CARTESIAN_POINT('Ctrl Pts',(5.47984516611268,4.37769773859499,8.44102823154271));
#21622=CARTESIAN_POINT('Ctrl Pts',(5.59316106493631,4.22778616585329,8.43249773428427));
#21623=CARTESIAN_POINT('Ctrl Pts',(5.70647812338238,4.07787305898599,8.42396714972868));
#21624=CARTESIAN_POINT('Ctrl Pts',(5.81375851664481,3.92340947692052,8.41543656517308));
#21625=CARTESIAN_POINT('Ctrl Pts',(5.91465292849583,3.76490468643441,8.40690598061749));
#21626=CARTESIAN_POINT('Ctrl Pts',(6.01556730501989,3.60636853151234,8.3983737080563));
#21627=CARTESIAN_POINT('Ctrl Pts',(6.11009301282587,3.44378982968665,8.38984143549512));
#21628=CARTESIAN_POINT('Ctrl Pts',(6.1979249207185,3.27770548396841,8.38130916293393));
#21629=CARTESIAN_POINT('Ctrl Pts',(6.20926450314781,3.25626308138743,8.38020759961442));
#21630=CARTESIAN_POINT('Ctrl Pts',(6.22049257427684,3.23476228004916,8.37910603629492));
#21631=CARTESIAN_POINT('Ctrl Pts',(6.2316085334411,3.21320426497352,8.37800447297541));
#21632=CARTESIAN_POINT('Ctrl Pts',(6.31770920853686,3.04622275448865,8.36947211476243));
#21633=CARTESIAN_POINT('Ctrl Pts',(6.39710890112773,2.8757504042213,8.36093975654946));
#21634=CARTESIAN_POINT('Ctrl Pts',(6.4695411047759,2.70234425196255,8.35240739833648));
#21635=CARTESIAN_POINT('Ctrl Pts',(6.54195974522404,2.52897057065198,8.34387663783937));
#21636=CARTESIAN_POINT('Ctrl Pts',(6.60741338252163,2.35266446590524,8.33534587734227));
#21637=CARTESIAN_POINT('Ctrl Pts',(6.66568340928876,2.17400350727236,8.32681511684516));
#21638=CARTESIAN_POINT('Ctrl Pts',(6.7264639836716,1.98764499178909,8.31791681094582));
#21639=CARTESIAN_POINT('Ctrl Pts',(6.77942809646649,1.79872453902279,8.30901850504649));
#21640=CARTESIAN_POINT('Ctrl Pts',(6.82438496723768,1.60791678312045,8.30012019914715));
#21641=CARTESIAN_POINT('Ctrl Pts',(6.86748356005959,1.42499600509848,8.29158970189097));
#21642=CARTESIAN_POINT('Ctrl Pts',(6.90322348059718,1.24034112726373,8.28305920463477));
#21643=CARTESIAN_POINT('Ctrl Pts',(6.93148845816996,1.05455882565013,8.27452870737859));
#21644=CARTESIAN_POINT('Ctrl Pts',(6.95975372499345,0.868774622826431,8.26599812282524));
#21645=CARTESIAN_POINT('Ctrl Pts',(6.98054385317258,0.681863276153072,8.25746753827189));
#21646=CARTESIAN_POINT('Ctrl Pts',(6.99379415578536,0.494438943654839,8.24893695371854));
#21647=CARTESIAN_POINT('Ctrl Pts',(7.0070470803269,0.306977524211316,8.2404046811596));
#21648=CARTESIAN_POINT('Ctrl Pts',(7.01275717886277,0.119003221499164,8.23187240860065));
#21649=CARTESIAN_POINT('Ctrl Pts',(7.01091177820364,-0.0688665430052387,
8.2233401360417));
#21650=CARTESIAN_POINT('Ctrl Pts',(7.01067352682567,-0.0931215632094089,
8.22223857271217));
#21651=CARTESIAN_POINT('Ctrl Pts',(7.01030940985087,-0.117374840699323,
8.22113700938265));
#21652=CARTESIAN_POINT('Ctrl Pts',(7.00981946332768,-0.1416250474047,8.22003544605312));
#21653=CARTESIAN_POINT('Ctrl Pts',(7.00602449382425,-0.329459414103322,
8.21150308783887));
#21654=CARTESIAN_POINT('Ctrl Pts',(6.99467475803301,-0.51717280440197,8.20297072962462));
#21655=CARTESIAN_POINT('Ctrl Pts',(6.9758011351623,-0.704148482330555,8.19443837141036));
#21656=CARTESIAN_POINT('Ctrl Pts',(6.95693104644776,-0.891089148367108,
8.18590761091196));
#21657=CARTESIAN_POINT('Ctrl Pts',(6.93053991296919,-1.07729207340012,8.17737685041356));
#21658=CARTESIAN_POINT('Ctrl Pts',(6.89671051082845,-1.26214527386048,8.16884608991516));
#21659=CARTESIAN_POINT('Ctrl Pts',(6.86142357847646,-1.45496282211506,8.15994778401646));
#21660=CARTESIAN_POINT('Ctrl Pts',(6.81804326857906,-1.64631141349988,8.15104947811777));
#21661=CARTESIAN_POINT('Ctrl Pts',(6.76672304477732,-1.83550695933837,8.14215117221907));
#21662=CARTESIAN_POINT('Ctrl Pts',(6.71752412608659,-2.01688216752755,8.13362067496157));
#21663=CARTESIAN_POINT('Ctrl Pts',(6.66102856965722,-2.19627842708316,8.12509017770407));
#21664=CARTESIAN_POINT('Ctrl Pts',(6.59742300179105,-2.373106887171,8.11655968044657));
#21665=CARTESIAN_POINT('Ctrl Pts',(6.53381678301494,-2.54993715683943,8.10802909589191));
#21666=CARTESIAN_POINT('Ctrl Pts',(6.46310051401775,-2.72419928770746,8.09949851133725));
#21667=CARTESIAN_POINT('Ctrl Pts',(6.38550974450136,-2.89532241130036,8.09096792678259));
#21668=CARTESIAN_POINT('Ctrl Pts',(6.30790362156429,-3.06647939620591,8.08243565422233));
#21669=CARTESIAN_POINT('Ctrl Pts',(6.22342040846619,-3.2344958549851,8.07390338166207));
#21670=CARTESIAN_POINT('Ctrl Pts',(6.13234294774363,-3.39882281588185,8.06537110910181));
#21671=CARTESIAN_POINT('Ctrl Pts',(6.12058434654617,-3.42003833049816,8.06426954577815));
#21672=CARTESIAN_POINT('Ctrl Pts',(6.10871589364357,-3.44119238140111,8.06316798245449));
#21673=CARTESIAN_POINT('Ctrl Pts',(6.09673825309964,-3.46228381789991,8.06206641913083));
#21674=CARTESIAN_POINT('Ctrl Pts',(6.00396326914703,-3.62565135890573,8.05353406091716));
#21675=CARTESIAN_POINT('Ctrl Pts',(5.90460250915252,-3.78531529587458,8.04500170270348));
#21676=CARTESIAN_POINT('Ctrl Pts',(5.79897678759855,-3.94074799744835,8.03646934448981));
#21677=CARTESIAN_POINT('Ctrl Pts',(5.6933708448544,-4.09615159366976,8.02793858399199));
#21678=CARTESIAN_POINT('Ctrl Pts',(5.58150245361073,-4.24732528269289,8.01940782349418));
#21679=CARTESIAN_POINT('Ctrl Pts',(5.46373580167137,-4.39377032308637,8.01087706299636));
#21680=CARTESIAN_POINT('Ctrl Pts',(5.34089520687048,-4.54652490658968,8.00197875709737));
#21681=CARTESIAN_POINT('Ctrl Pts',(5.21163704586447,-4.69413406121,7.99308045119839));
#21682=CARTESIAN_POINT('Ctrl Pts',(5.07642199947609,-4.8360692970361,7.9841821452994));
#21683=CARTESIAN_POINT('Ctrl Pts',(4.94679602399237,-4.9721376850661,7.9756516480425));
#21684=CARTESIAN_POINT('Ctrl Pts',(4.81169593945423,-5.10299154626926,7.96712115078559));
#21685=CARTESIAN_POINT('Ctrl Pts',(4.67156624093936,-5.22820192982404,7.95859065352869));
#21686=CARTESIAN_POINT('Ctrl Pts',(4.53143510840219,-5.35341359472376,7.95006006897463));
#21687=CARTESIAN_POINT('Ctrl Pts',(4.38627448935698,-5.47298146511146,7.94152948442058));
#21688=CARTESIAN_POINT('Ctrl Pts',(4.23656333794403,-5.58651569818689,7.93299889986653));
#21689=CARTESIAN_POINT('Ctrl Pts',(4.08682256215286,-5.70007239706416,7.92446662730686));
#21690=CARTESIAN_POINT('Ctrl Pts',(3.93252969996467,-5.80759288994331,7.9159343547472));
#21691=CARTESIAN_POINT('Ctrl Pts',(3.7741948668916,-5.90872910778867,7.90740208218754));
#21692=CARTESIAN_POINT('Ctrl Pts',(3.75375296888909,-5.92178634989661,7.90630051886121));
#21693=CARTESIAN_POINT('Ctrl Pts',(3.73324373750947,-5.93473723693103,7.90519895553487));
#21694=CARTESIAN_POINT('Ctrl Pts',(3.71266830461015,-5.94758107321315,7.90409739220854));
#21695=CARTESIAN_POINT('Ctrl Pts',(3.55329756331394,-6.0470653328826,7.89556503399468));
#21696=CARTESIAN_POINT('Ctrl Pts',(3.38989901740822,-6.14015694685801,7.88703267578082));
#21697=CARTESIAN_POINT('Ctrl Pts',(3.22300601222923,-6.22654469249473,7.87850031756695));
#21698=CARTESIAN_POINT('Ctrl Pts',(3.05614425838705,-6.31291626170432,7.86996955706895));
#21699=CARTESIAN_POINT('Ctrl Pts',(2.88578962273823,-6.392586327142,7.86143879657094));
#21700=CARTESIAN_POINT('Ctrl Pts',(2.71249983548278,-6.46528972320699,7.85290803607293));
#21701=CARTESIAN_POINT('Ctrl Pts',(2.53174390680414,-6.54112552450812,7.84400973017404));
#21702=CARTESIAN_POINT('Ctrl Pts',(2.3477946196699,-6.60938088676141,7.83511142427515));
#21703=CARTESIAN_POINT('Ctrl Pts',(2.1613087214537,-6.66981043006982,7.82621311837626));
#21704=CARTESIAN_POINT('Ctrl Pts',(1.98253115847744,-6.72774213744172,7.81768262111916));
#21705=CARTESIAN_POINT('Ctrl Pts',(1.80142277919043,-6.77848187322731,7.80915212386206));
#21706=CARTESIAN_POINT('Ctrl Pts',(1.61857870202646,-6.82186408160162,7.80062162660496));
#21707=CARTESIAN_POINT('Ctrl Pts',(1.43573275372108,-6.86524673392932,7.79209104205071));
#21708=CARTESIAN_POINT('Ctrl Pts',(1.25115137050542,-6.90127164090224,7.78356045749647));
#21709=CARTESIAN_POINT('Ctrl Pts',(1.06544135143817,-6.92982404460212,7.77502987294222));
#21710=CARTESIAN_POINT('Ctrl Pts',(0.87969458464844,-6.95838209816307,7.76649760038236));
#21711=CARTESIAN_POINT('Ctrl Pts',(0.692819038538371,-6.97946464968945,
7.75796532782251));
#21712=CARTESIAN_POINT('Ctrl Pts',(0.505429023624814,-6.99300851312064,
7.74943305526265));
#21713=CARTESIAN_POINT('Ctrl Pts',(0.48123594182401,-6.9947571003975,7.74833149193718));
#21714=CARTESIAN_POINT('Ctrl Pts',(0.457034290815553,-6.99638010203042,
7.74722992861172));
#21715=CARTESIAN_POINT('Ctrl Pts',(0.432825397161842,-6.99787744520235,
7.74612836528625));
#21716=CARTESIAN_POINT('Ctrl Pts',(0.245311027502743,-7.00947538788665,
7.7375960070724));
#21717=CARTESIAN_POINT('Ctrl Pts',(0.0572986320455093,-7.01353402693959,
7.72906364885856));
#21718=CARTESIAN_POINT('Ctrl Pts',(-0.1305945957598,-7.01003363858251,7.72053129064471));
#21719=CARTESIAN_POINT('Ctrl Pts',(-0.318452639858229,-7.00653390568619,
7.71200053014672));
#21720=CARTESIAN_POINT('Ctrl Pts',(-0.506191255034217,-6.99547797580645,
7.70346976964874));
#21721=CARTESIAN_POINT('Ctrl Pts',(-0.693193734882397,-6.97689823692591,
7.69493900915075));
#21722=CARTESIAN_POINT('Ctrl Pts',(-0.888253163632606,-6.9575179952558,
7.68604070325185));
#21723=CARTESIAN_POINT('Ctrl Pts',(-1.08251126646201,-6.92995127258633,
7.67714239735295));
#21724=CARTESIAN_POINT('Ctrl Pts',(-1.27527368597644,-6.89429500299748,
7.66824409145405));
#21725=CARTESIAN_POINT('Ctrl Pts',(-1.46006833224076,-6.86011257396192,
7.65971359419696));
#21726=CARTESIAN_POINT('Ctrl Pts',(-1.64348813504849,-6.81849596942113,
7.65118309693986));
#21727=CARTESIAN_POINT('Ctrl Pts',(-1.82493093963575,-6.76958297297996,
7.64265259968277));
#21728=CARTESIAN_POINT('Ctrl Pts',(-2.00637560102454,-6.72066947598587,
7.63412201512852));
#21729=CARTESIAN_POINT('Ctrl Pts',(-2.18584292917541,-6.66445952065229,
7.62559143057427));
#21730=CARTESIAN_POINT('Ctrl Pts',(-2.36274468537664,-6.60114112212612,
7.61706084602002));
#21731=CARTESIAN_POINT('Ctrl Pts',(-2.53968144634822,-6.53781019435182,
7.60852857346018));
#21732=CARTESIAN_POINT('Ctrl Pts',(-2.71405133366301,-6.46736811807306,
7.59999630090035));
#21733=CARTESIAN_POINT('Ctrl Pts',(-2.88528405938972,-6.39005183540256,
7.59146402834051));
#21734=CARTESIAN_POINT('Ctrl Pts',(-2.90739114627262,-6.3800698779747,7.59036246501499));
#21735=CARTESIAN_POINT('Ctrl Pts',(-2.92944597066077,-6.3699734049718,7.58926090168947));
#21736=CARTESIAN_POINT('Ctrl Pts',(-2.9514473313527,-6.35976298400743,7.58815933836396));
#21737=CARTESIAN_POINT('Ctrl Pts',(-3.12186285469646,-6.28067631947939,
7.57962698015016));
#21738=CARTESIAN_POINT('Ctrl Pts',(-3.28912646399832,-6.19472273666056,
7.57109462193637));
#21739=CARTESIAN_POINT('Ctrl Pts',(-3.45268603086347,-6.1021787694872,7.56256226372258));
#21740=CARTESIAN_POINT('Ctrl Pts',(-3.61621497059052,-6.00965213151639,
7.55403150322464));
#21741=CARTESIAN_POINT('Ctrl Pts',(-3.77604098584443,-5.91053772256712,
7.5455007427267));
#21742=CARTESIAN_POINT('Ctrl Pts',(-3.93163718967202,-5.80515766980432,
7.53696998222876));
#21743=CARTESIAN_POINT('Ctrl Pts',(-4.09393721189208,-5.69523734730144,
7.52807167632984));
#21744=CARTESIAN_POINT('Ctrl Pts',(-4.25163456349199,-5.5784996926556,7.51917337043091));
#21745=CARTESIAN_POINT('Ctrl Pts',(-4.4041648079342,-5.45536056618203,7.51027506453199));
#21746=CARTESIAN_POINT('Ctrl Pts',(-4.55039026327477,-5.33731135630445,
7.50174456727495));
#21747=CARTESIAN_POINT('Ctrl Pts',(-4.69186693034422,-5.21337944552277,
7.49321407001791));
#21748=CARTESIAN_POINT('Ctrl Pts',(-4.82813090276307,-5.08397271317267,
7.48468357276087));
#21749=CARTESIAN_POINT('Ctrl Pts',(-4.96439626964382,-4.95456465653447,
7.4761529882067));
#21750=CARTESIAN_POINT('Ctrl Pts',(-5.09544861563702,-4.81968187942328,
7.46762240365254));
#21751=CARTESIAN_POINT('Ctrl Pts',(-5.220860189501,-4.67976980675156,7.45909181909837));
#21752=CARTESIAN_POINT('Ctrl Pts',(-5.34629657941822,-4.53983004871288,
7.45055954653859));
#21753=CARTESIAN_POINT('Ctrl Pts',(-5.46608976439216,-4.39485923597475,
7.44202727397881));
#21754=CARTESIAN_POINT('Ctrl Pts',(-5.57985107513084,-4.2453372706843,7.43349500141903));
#21755=CARTESIAN_POINT('Ctrl Pts',(-5.59453828617866,-4.2260331624049,7.43239343809325));
#21756=CARTESIAN_POINT('Ctrl Pts',(-5.60912501264739,-4.20665323833119,
7.43129187476746));
#21757=CARTESIAN_POINT('Ctrl Pts',(-5.62361046851604,-4.1871985695566,7.43019031144167));
#21758=CARTESIAN_POINT('Ctrl Pts',(-5.73581180460668,-4.03650674118037,
7.42165783044403));
#21759=CARTESIAN_POINT('Ctrl Pts',(-5.84197158997454,-3.88127706288372,
7.41312534944638));
#21760=CARTESIAN_POINT('Ctrl Pts',(-5.9417359609281,-3.72201562773638,7.40459286844873));
#21761=CARTESIAN_POINT('Ctrl Pts',(-6.04148005497682,-3.56278656215078,
7.39606212166043));
#21762=CARTESIAN_POINT('Ctrl Pts',(-6.13483116679695,-3.39952763456354,
7.38753137487214));
#21763=CARTESIAN_POINT('Ctrl Pts',(-6.22147935548776,-3.23277298796862,
7.37900062808384));
#21764=CARTESIAN_POINT('Ctrl Pts',(-6.30812283662519,-3.06602740107147,
7.37047034476682));
#21765=CARTESIAN_POINT('Ctrl Pts',(-6.38806397881865,-2.8957867448778,7.36194006144979));
#21766=CARTESIAN_POINT('Ctrl Pts',(-6.46103893650285,-2.72260948787999,
7.35340977813276));
#21767=CARTESIAN_POINT('Ctrl Pts',(-6.50012585367688,-2.62985211856445,
7.34884077956032));
#21768=CARTESIAN_POINT('Ctrl Pts',(-6.53721504204028,-2.5362526604854,7.34427178098787));
#21769=CARTESIAN_POINT('Ctrl Pts',(-6.57227159525839,-2.441899392002,7.33970278241542));
#21770=CARTESIAN_POINT('Origin',(0.,0.,0.));
#21771=CARTESIAN_POINT('',(-6.57226144972351,-2.44189579807461,5.33969278385492));
#21772=CARTESIAN_POINT('',(-6.57227159525839,-2.44189939200201,5.88677413144118));
#21773=CARTESIAN_POINT('',(-6.57227159525839,-2.441899392002,0.));
#21774=CARTESIAN_POINT('',(-7.0112499977539,0.000177470811686547,7.77353435691036));
#21775=CARTESIAN_POINT('Ctrl Pts',(-6.57227159525839,-2.44189939200201,
5.88677413144118));
#21776=CARTESIAN_POINT('Ctrl Pts',(-6.50682880781099,-2.61803595785062,
5.8953040437753));
#21777=CARTESIAN_POINT('Ctrl Pts',(-6.43429692169323,-2.79155192492353,
5.90383395610941));
#21778=CARTESIAN_POINT('Ctrl Pts',(-6.35491245195174,-2.96187681893234,
5.91236386844353));
#21779=CARTESIAN_POINT('Ctrl Pts',(-6.2755220179471,-3.13221450968202,5.92089442164155));
#21780=CARTESIAN_POINT('Ctrl Pts',(-6.18927809852885,-3.29936036986028,
5.92942497483958));
#21781=CARTESIAN_POINT('Ctrl Pts',(-6.09646455045238,-3.46276573674535,
5.93795552803761));
#21782=CARTESIAN_POINT('Ctrl Pts',(-6.00365137626517,-3.6261704453697,5.94648604687123));
#21783=CARTESIAN_POINT('Ctrl Pts',(-5.90426877993716,-3.78583442615979,
5.95501656570485));
#21784=CARTESIAN_POINT('Ctrl Pts',(-5.79864578738953,-3.94123503421068,
5.96354708453847));
#21785=CARTESIAN_POINT('Ctrl Pts',(-5.69300088556608,-4.09666787686032,
5.97207937284942));
#21786=CARTESIAN_POINT('Ctrl Pts',(-5.58111317421822,-4.24783532738211,
5.98061166116036));
#21787=CARTESIAN_POINT('Ctrl Pts',(-5.4633546053563,-4.3942443057518,5.9891439494713));
#21788=CARTESIAN_POINT('Ctrl Pts',(-5.42639860225383,-4.44019162585896,
5.99182162529853));
#21789=CARTESIAN_POINT('Ctrl Pts',(-5.38886469319287,-4.4856705278481,5.99449930112576));
#21790=CARTESIAN_POINT('Ctrl Pts',(-5.35076519733763,-4.53066643723199,
5.99717697695298));
#21791=CARTESIAN_POINT('Ctrl Pts',(-5.22936194788609,-4.67404496465363,
6.00570933516681));
#21792=CARTESIAN_POINT('Ctrl Pts',(-5.1021719965233,-4.81256517858897,6.01424169338064));
#21793=CARTESIAN_POINT('Ctrl Pts',(-4.96960825326884,-4.94576792536227,
6.02277405159447));
#21794=CARTESIAN_POINT('Ctrl Pts',(-4.83706933306923,-5.07894572942494,
6.03130481209243));
#21795=CARTESIAN_POINT('Ctrl Pts',(-4.69915884485961,-5.2068078366158,6.03983557259039));
#21796=CARTESIAN_POINT('Ctrl Pts',(-4.55632697695416,-5.32893151031046,
6.04836633308835));
#21797=CARTESIAN_POINT('Ctrl Pts',(-4.40734123845651,-5.45631684791237,
6.05726463898726));
#21798=CARTESIAN_POINT('Ctrl Pts',(-4.25300090672483,-5.57745807423381,
6.06616294488617));
#21799=CARTESIAN_POINT('Ctrl Pts',(-4.09385650148087,-5.69192107357286,
6.07506125078508));
#21800=CARTESIAN_POINT('Ctrl Pts',(-3.94129027956909,-5.8016527812699,6.08359174804215));
#21801=CARTESIAN_POINT('Ctrl Pts',(-3.78430941424043,-5.90524705599592,
6.09212224529923));
#21802=CARTESIAN_POINT('Ctrl Pts',(-3.62343009969628,-6.00236460697907,
6.1006527425563));
#21803=CARTESIAN_POINT('Ctrl Pts',(-3.46254913878823,-6.09948315181797,
6.1091833271105));
#21804=CARTESIAN_POINT('Ctrl Pts',(-3.29776991256634,-6.19012468511022,
6.1177139116647));
#21805=CARTESIAN_POINT('Ctrl Pts',(-3.12963524240122,-6.27399472521457,
6.12624449621891));
#21806=CARTESIAN_POINT('Ctrl Pts',(-2.96146730226921,-6.35788136126226,
6.13477676877872));
#21807=CARTESIAN_POINT('Ctrl Pts',(-2.78994286632788,-6.43499369223092,
6.14330904133853));
#21808=CARTESIAN_POINT('Ctrl Pts',(-2.61562764909289,-6.50508405509113,
6.15184131389834));
#21809=CARTESIAN_POINT('Ctrl Pts',(-2.59312259559609,-6.51413310652106,
6.15294287722398));
#21810=CARTESIAN_POINT('Ctrl Pts',(-2.57057105215388,-6.52306517987497,
6.15404444054963));
#21811=CARTESIAN_POINT('Ctrl Pts',(-2.54797425980885,-6.53187980093415,
6.15514600387527));
#21812=CARTESIAN_POINT('Ctrl Pts',(-2.37294671279207,-6.60015504453133,
6.16367836208909));
#21813=CARTESIAN_POINT('Ctrl Pts',(-2.19514385506042,-6.66140271533437,
6.17221072030292));
#21814=CARTESIAN_POINT('Ctrl Pts',(-2.01514741149616,-6.71541565894773,
6.18074307851674));
#21815=CARTESIAN_POINT('Ctrl Pts',(-1.83518467293613,-6.76941848843629,
6.18927383901472));
#21816=CARTESIAN_POINT('Ctrl Pts',(-1.65302946121357,-6.81618920636936,
6.1978045995127));
#21817=CARTESIAN_POINT('Ctrl Pts',(-1.46927894227537,-6.85557043230439,
6.20633536001069));
#21818=CARTESIAN_POINT('Ctrl Pts',(-1.27761158425004,-6.89664838720967,
6.21523366590959));
#21819=CARTESIAN_POINT('Ctrl Pts',(-1.08420874701755,-6.92968590019265,
6.2241319718085));
#21820=CARTESIAN_POINT('Ctrl Pts',(-0.88976124239467,-6.95456335753959,
6.2330302777074));
#21821=CARTESIAN_POINT('Ctrl Pts',(-0.70335116347931,-6.97841251310603,
6.24156077496447));
#21822=CARTESIAN_POINT('Ctrl Pts',(-0.515981366956735,-6.99476259525729,
6.25009127222153));
#21823=CARTESIAN_POINT('Ctrl Pts',(-0.328267328922525,-7.00356103159401,
6.2586217694786));
#21824=CARTESIAN_POINT('Ctrl Pts',(-0.14055136991003,-7.01235955796983,
6.26715235403281));
#21825=CARTESIAN_POINT('Ctrl Pts',(0.0475085318593298,-7.01360627301243,
6.27568293858702));
#21826=CARTESIAN_POINT('Ctrl Pts',(0.235294821337802,-7.00730068639499,
6.28421352314123));
#21827=CARTESIAN_POINT('Ctrl Pts',(0.423118269384501,-7.00099385204763,
6.29274579570104));
#21828=CARTESIAN_POINT('Ctrl Pts',(0.610667691222674,-6.98713174251941,
6.30127806826084));
#21829=CARTESIAN_POINT('Ctrl Pts',(0.797327693233565,-6.96576593865333,
6.30981034082065));
#21830=CARTESIAN_POINT('Ctrl Pts',(0.82142652635651,-6.96300749583559,6.31091190414629));
#21831=CARTESIAN_POINT('Ctrl Pts',(0.845510541581198,-6.96012405055713,
6.31201346747193));
#21832=CARTESIAN_POINT('Ctrl Pts',(0.869578421780628,-6.95711577673345,
6.31311503079756));
#21833=CARTESIAN_POINT('Ctrl Pts',(1.05600054616517,-6.93381464708294,6.3216473890114));
#21834=CARTESIAN_POINT('Ctrl Pts',(1.24151697778743,-6.90301226090025,6.33017974722523));
#21835=CARTESIAN_POINT('Ctrl Pts',(1.42551753240329,-6.86480344418621,6.33871210543906));
#21836=CARTESIAN_POINT('Ctrl Pts',(1.60948363222983,-6.82660178221544,6.34724286593703));
#21837=CARTESIAN_POINT('Ctrl Pts',(1.79193412205059,-6.78099651960513,6.355773626435));
#21838=CARTESIAN_POINT('Ctrl Pts',(1.97226893932507,-6.72813360401483,6.36430438693298));
#21839=CARTESIAN_POINT('Ctrl Pts',(2.16037343114771,-6.6729931046722,6.37320269283188));
#21840=CARTESIAN_POINT('Ctrl Pts',(2.3461755609127,-6.60995578803778,6.38210099873079));
#21841=CARTESIAN_POINT('Ctrl Pts',(2.52901090012722,-6.53924540214983,6.39099930462969));
#21842=CARTESIAN_POINT('Ctrl Pts',(2.70428879879527,-6.47145780755411,6.39952980188677));
#21843=CARTESIAN_POINT('Ctrl Pts',(2.87683993367598,-6.39661883584323,6.40806029914384));
#21844=CARTESIAN_POINT('Ctrl Pts',(3.04609804559447,-6.31497531738055,6.41659079640092));
#21845=CARTESIAN_POINT('Ctrl Pts',(3.21535788962182,-6.23333096341604,6.42512138095514));
#21846=CARTESIAN_POINT('Ctrl Pts',(3.38132436916103,-6.14488205940167,6.43365196550936));
#21847=CARTESIAN_POINT('Ctrl Pts',(3.54345419590065,-6.04992222462852,6.44218255006357));
#21848=CARTESIAN_POINT('Ctrl Pts',(3.70561610438746,-5.95494359949782,6.4507148226234));
#21849=CARTESIAN_POINT('Ctrl Pts',(3.86393958024118,-5.85345162589316,6.45924709518324));
#21850=CARTESIAN_POINT('Ctrl Pts',(4.01790802965527,-5.74578468337717,6.46777936774306));
#21851=CARTESIAN_POINT('Ctrl Pts',(4.03778620349278,-5.73188428879614,6.46888093106866));
#21852=CARTESIAN_POINT('Ctrl Pts',(4.05759182677243,-5.71788102730183,6.46998249439426));
#21853=CARTESIAN_POINT('Ctrl Pts',(4.07732382407226,-5.70377567898255,6.47108405771985));
#21854=CARTESIAN_POINT('Ctrl Pts',(4.23016158230585,-5.5945201493235,6.47961641593367));
#21855=CARTESIAN_POINT('Ctrl Pts',(4.37863116505627,-5.47909954286938,6.4881487741475));
#21856=CARTESIAN_POINT('Ctrl Pts',(4.52224115074249,-5.35788778690178,6.49668113236132));
#21857=CARTESIAN_POINT('Ctrl Pts',(4.66582424492394,-5.23669872828699,6.50521189285928));
#21858=CARTESIAN_POINT('Ctrl Pts',(4.80454932429202,-5.10972088152682,6.51374265335725));
#21859=CARTESIAN_POINT('Ctrl Pts',(4.93795820962652,-4.97736830890402,6.52227341385521));
#21860=CARTESIAN_POINT('Ctrl Pts',(5.07711497901682,-4.83931336315956,6.53117171975412));
#21861=CARTESIAN_POINT('Ctrl Pts',(5.21048704681651,-4.69541052703548,6.54007002565303));
#21862=CARTESIAN_POINT('Ctrl Pts',(5.33759667764691,-4.54617292557957,6.54896833155194));
#21863=CARTESIAN_POINT('Ctrl Pts',(5.45945227234803,-4.40310401287505,6.557498828809));
#21864=CARTESIAN_POINT('Ctrl Pts',(5.57555252100228,-4.25513273830584,6.56602932606606));
#21865=CARTESIAN_POINT('Ctrl Pts',(5.68551700537223,-4.10274578107432,6.57455982332311));
#21866=CARTESIAN_POINT('Ctrl Pts',(5.79548261506783,-3.95035726438521,6.58309040787733));
#21867=CARTESIAN_POINT('Ctrl Pts',(5.89931215858357,-3.79355322475207,6.59162099243155));
#21868=CARTESIAN_POINT('Ctrl Pts',(5.99666769607275,-3.63285054817529,6.60015157698577));
#21869=CARTESIAN_POINT('Ctrl Pts',(6.09404249797358,-3.47211607225157,6.60868384954558));
#21870=CARTESIAN_POINT('Ctrl Pts',(6.18494057752728,-3.30748168080824,6.6172161221054));
#21871=CARTESIAN_POINT('Ctrl Pts',(6.26906878175907,-3.13949090969761,6.62574839466522));
#21872=CARTESIAN_POINT('Ctrl Pts',(6.27993019573572,-3.11780237698791,6.62684995799086));
#21873=CARTESIAN_POINT('Ctrl Pts',(6.29067883110952,-3.09605793209677,6.6279515213165));
#21874=CARTESIAN_POINT('Ctrl Pts',(6.30131411363566,-3.07425877306971,6.62905308464214));
#21875=CARTESIAN_POINT('Ctrl Pts',(6.38369162031749,-2.9054094393547,6.63758544285598));
#21876=CARTESIAN_POINT('Ctrl Pts',(6.45929239905691,-2.73321868568166,6.64611780106983));
#21877=CARTESIAN_POINT('Ctrl Pts',(6.52786235853414,-2.5582493214175,6.65465015928367));
#21878=CARTESIAN_POINT('Ctrl Pts',(6.59641947803105,-2.38331272081854,6.66318091978166));
#21879=CARTESIAN_POINT('Ctrl Pts',(6.65794829400971,-2.20559883273443,6.67171168027964));
#21880=CARTESIAN_POINT('Ctrl Pts',(6.71224305762752,-2.02568993131505,6.68024244077763));
#21881=CARTESIAN_POINT('Ctrl Pts',(6.76887709576443,-1.83802970581198,6.68914074667653));
#21882=CARTESIAN_POINT('Ctrl Pts',(6.81763979496159,-1.64798146488188,6.69803905257543));
#21883=CARTESIAN_POINT('Ctrl Pts',(6.8583553784182,-1.45622390648628,6.70693735847433));
#21884=CARTESIAN_POINT('Ctrl Pts',(6.89738799619325,-1.27239258572658,6.71546785573141));
#21885=CARTESIAN_POINT('Ctrl Pts',(6.92902530509543,-1.0869907342772,6.7239983529885));
#21886=CARTESIAN_POINT('Ctrl Pts',(6.9531645131237,-0.900627456797393,6.73252885024558));
#21887=CARTESIAN_POINT('Ctrl Pts',(6.97730396818145,-0.714262272162066,
6.74105943479982));
#21888=CARTESIAN_POINT('Ctrl Pts',(6.99394513293989,-0.526935945694958,
6.74959001935406));
#21889=CARTESIAN_POINT('Ctrl Pts',(7.00303695235466,-0.339263918587315,
6.75812060390831));
#21890=CARTESIAN_POINT('Ctrl Pts',(7.01213057083044,-0.151554755521377,
6.76665287646815));
#21891=CARTESIAN_POINT('Ctrl Pts',(7.01367184653439,0.0364999391338565,
6.77518514902799));
#21892=CARTESIAN_POINT('Ctrl Pts',(7.00766179772167,0.224282614690158,6.78371742158783));
#21893=CARTESIAN_POINT('Ctrl Pts',(7.00688586735725,0.248526391141561,6.78481898491336));
#21894=CARTESIAN_POINT('Ctrl Pts',(7.00598414096941,0.272765634847337,6.7859205482389));
#21895=CARTESIAN_POINT('Ctrl Pts',(7.00495668404128,0.29699901886284,6.78702211156443));
#21896=CARTESIAN_POINT('Ctrl Pts',(6.99699833034799,0.484703083042002,6.79555446977824));
#21897=CARTESIAN_POINT('Ctrl Pts',(6.9814897493047,0.672118710219353,6.80408682799206));
#21898=CARTESIAN_POINT('Ctrl Pts',(6.95847548566177,0.858630000608037,6.81261918620587));
#21899=CARTESIAN_POINT('Ctrl Pts',(6.93546553152544,1.04510636606285,6.82114994670383));
#21900=CARTESIAN_POINT('Ctrl Pts',(6.90495273704113,1.23067842911714,6.82968070720178));
#21901=CARTESIAN_POINT('Ctrl Pts',(6.86703342573563,1.41473619177908,6.83821146769974));
#21902=CARTESIAN_POINT('Ctrl Pts',(6.82748037163766,1.60672403103774,6.84710977359866));
#21903=CARTESIAN_POINT('Ctrl Pts',(6.77986849625049,1.7970638430474,6.85600807949757));
#21904=CARTESIAN_POINT('Ctrl Pts',(6.72436639184739,1.98507510958485,6.86490638539648));
#21905=CARTESIAN_POINT('Ctrl Pts',(6.67115844926261,2.16531499026689,6.87343688265354));
#21906=CARTESIAN_POINT('Ctrl Pts',(6.61069953596366,2.34341464113093,6.88196737991059));
#21907=CARTESIAN_POINT('Ctrl Pts',(6.54318928729587,2.5187894936093,6.89049787716764));
#21908=CARTESIAN_POINT('Ctrl Pts',(6.47567834775942,2.69416614079279,6.89902846172186));
#21909=CARTESIAN_POINT('Ctrl Pts',(6.40111604160243,2.86681764948153,6.90755904627607));
#21910=CARTESIAN_POINT('Ctrl Pts',(6.31975051687379,3.03617851368682,6.91608963083029));
#21911=CARTESIAN_POINT('Ctrl Pts',(6.23836889178763,3.2055728904943,6.9246219033901));
#21912=CARTESIAN_POINT('Ctrl Pts',(6.15018149279767,3.37167504692766,6.93315417594991));
#21913=CARTESIAN_POINT('Ctrl Pts',(6.05548326370981,3.53394241682436,6.94168644850973));
#21914=CARTESIAN_POINT('Ctrl Pts',(6.04325720137559,3.55489202695198,6.94278801183539));
#21915=CARTESIAN_POINT('Ctrl Pts',(6.03092267699611,3.57577775304378,6.94388957516106));
#21916=CARTESIAN_POINT('Ctrl Pts',(6.01848037998295,3.59659845941416,6.94499113848673));
#21917=CARTESIAN_POINT('Ctrl Pts',(5.92210631537353,3.75786901089114,6.95352349670056));
#21918=CARTESIAN_POINT('Ctrl Pts',(5.81923020290133,3.91529086095971,6.96205585491439));
#21919=CARTESIAN_POINT('Ctrl Pts',(5.71018447586521,4.06834362045391,6.97058821312823));
#21920=CARTESIAN_POINT('Ctrl Pts',(5.6011591680477,4.22136772024872,6.9791189736262));
#21921=CARTESIAN_POINT('Ctrl Pts',(5.48596672866222,4.37002411305445,6.98764973412417));
#21922=CARTESIAN_POINT('Ctrl Pts',(5.36498231317421,4.51382225412432,6.99618049462214));
#21923=CARTESIAN_POINT('Ctrl Pts',(5.2387853183965,4.66381589739185,7.00507880052105));
#21924=CARTESIAN_POINT('Ctrl Pts',(5.10628640972892,4.80852309802665,7.01397710641995));
#21925=CARTESIAN_POINT('Ctrl Pts',(4.96795787146739,4.94742570937909,7.02287541231886));
#21926=CARTESIAN_POINT('Ctrl Pts',(4.83534709930238,5.08058682550653,7.03140590957593));
#21927=CARTESIAN_POINT('Ctrl Pts',(4.69737917041945,5.20841333463145,7.039936406833));
#21928=CARTESIAN_POINT('Ctrl Pts',(4.55450798055072,5.33048624588787,7.04846690409006));
#21929=CARTESIAN_POINT('Ctrl Pts',(4.41163532860432,5.45256040638202,7.0569974886443));
#21930=CARTESIAN_POINT('Ctrl Pts',(4.2638595501344,5.56888065504789,7.06552807319853));
#21931=CARTESIAN_POINT('Ctrl Pts',(4.1116681244352,5.67906786339128,7.07405865775276));
#21932=CARTESIAN_POINT('Ctrl Pts',(3.95944658356889,5.78927687523757,7.0825909303126));
#21933=CARTESIAN_POINT('Ctrl Pts',(3.80280789877415,5.89335024425383,7.09112320287243));
#21934=CARTESIAN_POINT('Ctrl Pts',(3.64226977692717,5.99095129629535,7.09965547543227));
#21935=CARTESIAN_POINT('Ctrl Pts',(3.6215434222375,6.00355212904102,7.10075703875785));
#21936=CARTESIAN_POINT('Ctrl Pts',(3.60075210862899,6.01604514006274,7.10185860208343));
#21937=CARTESIAN_POINT('Ctrl Pts',(3.57989698310413,6.02842965894618,7.10296016540901));
#21938=CARTESIAN_POINT('Ctrl Pts',(3.41835983181994,6.12435619259717,7.11149252362287));
#21939=CARTESIAN_POINT('Ctrl Pts',(3.25293759185595,6.21380235473935,7.12002488183674));
#21940=CARTESIAN_POINT('Ctrl Pts',(3.0841703773126,6.29646882357147,7.1285572400506));
#21941=CARTESIAN_POINT('Ctrl Pts',(2.91543476505874,6.37911981279941,7.13708800054861));
#21942=CARTESIAN_POINT('Ctrl Pts',(2.74335570288163,6.45499350767554,7.14561876104662));
#21943=CARTESIAN_POINT('Ctrl Pts',(2.5684966626602,6.52383717273841,7.15414952154463));
#21944=CARTESIAN_POINT('Ctrl Pts',(2.38610387019588,6.5956469476199,7.16304782744352));
#21945=CARTESIAN_POINT('Ctrl Pts',(2.20068656367103,6.6598073493845,7.17194613334241));
#21946=CARTESIAN_POINT('Ctrl Pts',(2.01290676914888,6.7160876186374,7.1808444392413));
#21947=CARTESIAN_POINT('Ctrl Pts',(1.83288879265856,6.77004156087608,7.1893749364984));
#21948=CARTESIAN_POINT('Ctrl Pts',(1.65070001986629,6.81675362467141,7.1979054337555));
#21949=CARTESIAN_POINT('Ctrl Pts',(1.4669390933311,6.85607148875775,7.2064359310126));
#21950=CARTESIAN_POINT('Ctrl Pts',(1.28317628627127,6.895389755205,7.21496651556688));
#21951=CARTESIAN_POINT('Ctrl Pts',(1.09784159320238,6.92731360988328,7.22349710012115));
#21952=CARTESIAN_POINT('Ctrl Pts',(0.911544208239945,6.95174177590942,7.23202768467543));
#21953=CARTESIAN_POINT('Ctrl Pts',(0.725209959329432,6.9761747757052,7.24055995723529));
#21954=CARTESIAN_POINT('Ctrl Pts',(0.537912941574896,6.99310908564368,7.24909222979515));
#21955=CARTESIAN_POINT('Ctrl Pts',(0.350268715347714,7.00249515455375,7.25762450235502));
#21956=CARTESIAN_POINT('Ctrl Pts',(0.326042813468689,7.00370694768491,7.25872606568044));
#21957=CARTESIAN_POINT('Ctrl Pts',(0.301811128741358,7.00479299605894,7.25982762900587));
#21958=CARTESIAN_POINT('Ctrl Pts',(0.277574989016439,7.00575325628676,7.2609291923313));
#21959=CARTESIAN_POINT('Ctrl Pts',(0.0898495799762925,7.01319112577005,
7.26946155054498));
#21960=CARTESIAN_POINT('Ctrl Pts',(-0.0982065849261312,7.01308050338434,
7.27799390875865));
#21961=CARTESIAN_POINT('Ctrl Pts',(-0.285976026660372,7.00541535347302,
7.28652626697233));
#21962=CARTESIAN_POINT('Ctrl Pts',(-0.473710307867084,6.99775163888959,
7.29505702747014));
#21963=CARTESIAN_POINT('Ctrl Pts',(-0.661157667450308,6.98253623230388,
7.30358778796795));
#21964=CARTESIAN_POINT('Ctrl Pts',(-0.847702268630366,6.95981518621428,
7.31211854846576));
#21965=CARTESIAN_POINT('Ctrl Pts',(-1.0422840911455,6.93611521028575,7.32101685436475));
#21966=CARTESIAN_POINT('Ctrl Pts',(-1.23588328914684,6.90424853101671,7.32991516026374));
#21967=CARTESIAN_POINT('Ctrl Pts',(-1.42780782494848,6.86432745267269,7.33881346616272));
#21968=CARTESIAN_POINT('Ctrl Pts',(-1.61179922115094,6.82605649939542,7.34734396341964));
#21969=CARTESIAN_POINT('Ctrl Pts',(-1.79425129499676,6.78038367833697,7.35587446067656));
#21970=CARTESIAN_POINT('Ctrl Pts',(-1.97456509440836,6.7274600891008,7.36440495793347));
#21971=CARTESIAN_POINT('Ctrl Pts',(-2.15488073906802,6.67453595826908,7.37293554248755));
#21972=CARTESIAN_POINT('Ctrl Pts',(-2.33305777288539,6.61436100026425,7.38146612704163));
#21973=CARTESIAN_POINT('Ctrl Pts',(-2.50851227005572,6.54713622536448,7.38999671159571));
#21974=CARTESIAN_POINT('Ctrl Pts',(-2.68400148561738,6.47989814823491,7.39852898415539));
#21975=CARTESIAN_POINT('Ctrl Pts',(-2.85676680316761,6.40560757842252,7.40706125671506));
#21976=CARTESIAN_POINT('Ctrl Pts',(-3.02624332798837,6.32451404317406,7.41559352927474));
#21977=CARTESIAN_POINT('Ctrl Pts',(-3.04812367968867,6.31404442165135,7.41669509260102));
#21978=CARTESIAN_POINT('Ctrl Pts',(-3.06994924291164,6.30346147136759,7.41779665592731));
#21979=CARTESIAN_POINT('Ctrl Pts',(-3.09171882933512,6.29276578642767,7.41889821925359));
#21980=CARTESIAN_POINT('Ctrl Pts',(-3.26033910300386,6.20992042195635,7.42743057746785));
#21981=CARTESIAN_POINT('Ctrl Pts',(-3.42565599669303,6.12027970542182,7.4359629356821));
#21982=CARTESIAN_POINT('Ctrl Pts',(-3.58712364851452,6.0241323435635,7.44449529389636));
#21983=CARTESIAN_POINT('Ctrl Pts',(-3.74856106491702,5.92800298565668,7.45302605439477));
#21984=CARTESIAN_POINT('Ctrl Pts',(-3.90615041507955,5.82536957037436,7.46155681489318));
#21985=CARTESIAN_POINT('Ctrl Pts',(-4.05937208316045,5.71656582687172,7.47008757539159));
#21986=CARTESIAN_POINT('Ctrl Pts',(-4.21919526342033,5.60307430489202,7.47898588129028));
#21987=CARTESIAN_POINT('Ctrl Pts',(-4.37426576303427,5.48286916830799,7.48788418718898));
#21988=CARTESIAN_POINT('Ctrl Pts',(-4.52402850388408,5.35637868886661,7.49678249308767));
#21989=CARTESIAN_POINT('Ctrl Pts',(-4.66760084952371,5.23511665311973,7.50531299034516));
#21990=CARTESIAN_POINT('Ctrl Pts',(-4.80629515369875,5.10807864373607,7.51384348760265));
#21991=CARTESIAN_POINT('Ctrl Pts',(-4.93965666680029,4.97568272467563,7.52237398486015));
#21992=CARTESIAN_POINT('Ctrl Pts',(-5.0730195446616,4.84328545073686,7.53090456941479));
#21993=CARTESIAN_POINT('Ctrl Pts',(-5.2010493075339,4.70553037542458,7.53943515396942));
#21994=CARTESIAN_POINT('Ctrl Pts',(-5.32332818445081,4.56287229748233,7.54796573852406));
#21995=CARTESIAN_POINT('Ctrl Pts',(-5.44563125753255,4.42018599080216,7.55649801108431));
#21996=CARTESIAN_POINT('Ctrl Pts',(-5.56218097344242,4.27259497672134,7.56503028364456));
#21997=CARTESIAN_POINT('Ctrl Pts',(-5.67259939792344,4.1205876562911,7.57356255620481));
#21998=CARTESIAN_POINT('Ctrl Pts',(-5.6868550239374,4.10096267502895,7.5746641195285));
#21999=CARTESIAN_POINT('Ctrl Pts',(-5.70100850922268,4.08126412436603,7.57576568285219));
#22000=CARTESIAN_POINT('Ctrl Pts',(-5.71505909169781,4.06149309255872,7.57686724617588));
#22001=CARTESIAN_POINT('Ctrl Pts',(-5.82389042277067,3.90835298522994,7.58539960438882));
#22002=CARTESIAN_POINT('Ctrl Pts',(-5.92658126006227,3.75081021222684,7.59393196260177));
#22003=CARTESIAN_POINT('Ctrl Pts',(-6.0227890614943,3.58937856505058,7.60246432081471));
#22004=CARTESIAN_POINT('Ctrl Pts',(-6.11897884765724,3.42797714655143,7.6109950813118));
#22005=CARTESIAN_POINT('Ctrl Pts',(-6.20868786402214,3.26268856984593,7.61952584180889));
#22006=CARTESIAN_POINT('Ctrl Pts',(-6.29161808584567,3.0940537203416,7.62805660230599));
#22007=CARTESIAN_POINT('Ctrl Pts',(-6.37812133281153,2.91815328606126,7.63695490820534));
#22008=CARTESIAN_POINT('Ctrl Pts',(-6.45724854463065,2.73861215131085,7.64585321410469));
#22009=CARTESIAN_POINT('Ctrl Pts',(-6.52871552906283,2.5560712241786,7.65475152000403));
#22010=CARTESIAN_POINT('Ctrl Pts',(-6.59722844843226,2.38107556819003,7.66328201726022));
#22011=CARTESIAN_POINT('Ctrl Pts',(-6.6587015552587,2.20332342906014,7.67181251451641));
#22012=CARTESIAN_POINT('Ctrl Pts',(-6.71293402198084,2.02339896684566,7.68034301177259));
#22013=CARTESIAN_POINT('Ctrl Pts',(-6.767167043693,1.84347266336737,7.68887359632595));
#22014=CARTESIAN_POINT('Ctrl Pts',(-6.81415919203053,1.66137428627552,7.6974041808793));
#22015=CARTESIAN_POINT('Ctrl Pts',(-6.85375964843323,1.47770269134507,7.70593476543265));
#22016=CARTESIAN_POINT('Ctrl Pts',(-6.89336794085143,1.29399475204902,7.71446703799162));
#22017=CARTESIAN_POINT('Ctrl Pts',(-6.92558155650827,1.10871327247893,7.7229993105506));
#22018=CARTESIAN_POINT('Ctrl Pts',(-6.95030070758529,0.922467688669611,
7.73153158310957));
#22019=CARTESIAN_POINT('Ctrl Pts',(-6.95349208598717,0.898422359128844,
7.7326331464391));
#22020=CARTESIAN_POINT('Ctrl Pts',(-6.95655861538189,0.874360969982549,
7.73373470976863));
#22021=CARTESIAN_POINT('Ctrl Pts',(-6.95950014379961,0.850284841069851,
7.73483627309817));
#22022=CARTESIAN_POINT('Ctrl Pts',(-6.98345968606632,0.654178277955419,
7.74380880349918));
#22023=CARTESIAN_POINT('Ctrl Pts',(-6.9991270096246,0.45705027964632,7.75278133390019));
#22024=CARTESIAN_POINT('Ctrl Pts',(-7.00644302121596,0.259581881020636,
7.7617538643012));
#22025=CARTESIAN_POINT('Ctrl Pts',(-7.0096448760859,0.173159771664506,7.76568069517092));
#22026=CARTESIAN_POINT('Ctrl Pts',(-7.01124780836569,0.0866725284477343,
7.76960752604064));
#22027=CARTESIAN_POINT('Ctrl Pts',(-7.0112499977539,0.000177470811686547,
7.77353435691036));
#22028=CARTESIAN_POINT('Ctrl Pts',(-7.01119847445136,0.000177469507514665,
7.77353435691036));
#22029=CARTESIAN_POINT('Ctrl Pts',(-7.01036852730354,-0.831199708459484,
7.81127872708187));
#22030=CARTESIAN_POINT('Ctrl Pts',(-6.86199980275722,-1.66286473245636,
7.84902309725337));
#22031=CARTESIAN_POINT('Ctrl Pts',(-6.57280081548428,-2.44209581534395,
7.88676746742488));
#22032=CARTESIAN_POINT('',(-7.01124999795275,-0.00016943300568554,7.22646564308963));
#22033=CARTESIAN_POINT('Ctrl Pts',(-6.57227159525839,-2.441899392002,7.33970278241542));
#22034=CARTESIAN_POINT('Ctrl Pts',(-6.63772323604687,-2.26573899775066,
7.33117232445892));
#22035=CARTESIAN_POINT('Ctrl Pts',(-6.69608654756327,-2.08695006746432,
7.32264186650241));
#22036=CARTESIAN_POINT('Ctrl Pts',(-6.74717209576847,-1.90612047693302,
7.31411140854591));
#22037=CARTESIAN_POINT('Ctrl Pts',(-6.79826929134116,-1.72524965774176,
7.30557900566795));
#22038=CARTESIAN_POINT('Ctrl Pts',(-6.84208532452037,-1.54233754315333,
7.29704660278999));
#22039=CARTESIAN_POINT('Ctrl Pts',(-6.8784809730595,-1.35798603297619,7.28851419991204));
#22040=CARTESIAN_POINT('Ctrl Pts',(-6.901647218676,-1.24064419305973,7.28308322811449));
#22041=CARTESIAN_POINT('Ctrl Pts',(-6.92180813642338,-1.12271944697059,
7.27765225631694));
#22042=CARTESIAN_POINT('Ctrl Pts',(-6.93893863521853,-1.00436904530736,
7.27222128451938));
#22043=CARTESIAN_POINT('Ctrl Pts',(-6.96699642709752,-0.810524664103404,
7.263325975736));
#22044=CARTESIAN_POINT('Ctrl Pts',(-6.98692870444038,-0.615493148353179,
7.25443066695261));
#22045=CARTESIAN_POINT('Ctrl Pts',(-6.99866239872024,-0.419941890312867,
7.24553535816922));
#22046=CARTESIAN_POINT('Ctrl Pts',(-7.00704727559547,-0.280201312251252,
7.23917878647602));
#22047=CARTESIAN_POINT('Ctrl Pts',(-7.01124661409999,-0.140195501486346,
7.23282221478283));
#22048=CARTESIAN_POINT('Ctrl Pts',(-7.01124999795275,-0.00016943300568554,
7.22646564308963));
#22049=CARTESIAN_POINT('Ctrl Pts',(-7.0110449382642,-0.000169428050237619,
7.22646564308963));
#22050=CARTESIAN_POINT('Ctrl Pts',(-7.01028915262695,0.823772614993853,
7.18906118125878));
#22051=CARTESIAN_POINT('Ctrl Pts',(-6.66051850280413,2.80824854701764,7.09900037712055));
#22052=CARTESIAN_POINT('Ctrl Pts',(-4.82814950876211,5.48279137105804,6.95628323067478));
#22053=CARTESIAN_POINT('Ctrl Pts',(-1.63504874432568,7.12029806266455,6.7983142037525));
#22054=CARTESIAN_POINT('Ctrl Pts',(1.95254792752263,7.0398569224263,6.64034517683023));
#22055=CARTESIAN_POINT('Ctrl Pts',(5.06904416942584,5.26087636291873,6.48237614990793));
#22056=CARTESIAN_POINT('Ctrl Pts',(6.96250826242842,2.21257939815105,6.32440712298563));
#22057=CARTESIAN_POINT('Ctrl Pts',(7.17609521147244,-1.36955701355905,6.16643809606336));
#22058=CARTESIAN_POINT('Ctrl Pts',(5.65827188791764,-4.62125395752143,6.00846906914106));
#22059=CARTESIAN_POINT('Ctrl Pts',(2.77525067007686,-6.75795920494823,5.85050004221877));
#22060=CARTESIAN_POINT('Ctrl Pts',(-0.777368341216584,-7.26413982241399,
5.69253101529648));
#22061=CARTESIAN_POINT('Ctrl Pts',(-4.14242803342189,-6.01766722953563,
5.53456198837419));
#22062=CARTESIAN_POINT('Ctrl Pts',(-5.90368661682782,-4.00863867080895,
5.41694924456034));
#22063=CARTESIAN_POINT('Ctrl Pts',(-6.47816622693472,-2.69595371960147,
5.35199284305391));
#22064=CARTESIAN_POINT('Ctrl Pts',(-6.57226144972351,-2.44189579807461,
5.33969278385492));
#22065=CARTESIAN_POINT('Origin',(0.,0.,0.));
#22066=CARTESIAN_POINT('',(-6.5722715952584,-2.44189939200197,3.33970491700474));
#22067=CARTESIAN_POINT('',(-6.57188903190969,-2.44175767753665,3.88676355207028));
#22068=CARTESIAN_POINT('',(-6.57227159525839,-2.441899392002,0.));
#22069=CARTESIAN_POINT('',(-7.01105936472711,-8.57079543653067E-5,5.77353435691036));
#22070=CARTESIAN_POINT('Ctrl Pts',(-6.57188903190969,-2.44175767753665,
3.88676355207028));
#22071=CARTESIAN_POINT('Ctrl Pts',(-6.42685604719305,-2.83295247522456,
3.90570224370127));
#22072=CARTESIAN_POINT('Ctrl Pts',(-5.74776975712297,-4.26300939817711,
3.97729727763977));
#22073=CARTESIAN_POINT('Ctrl Pts',(-3.75801643412087,-6.26492947912218,
4.10154865388543));
#22074=CARTESIAN_POINT('Ctrl Pts',(-0.321596567147127,-7.29853441079176,
4.25951768080783));
#22075=CARTESIAN_POINT('Ctrl Pts',(3.19241641747391,-6.57118758786775,4.41748670773006));
#22076=CARTESIAN_POINT('Ctrl Pts',(5.93618006499142,-4.25837940224982,4.57545573465238));
#22077=CARTESIAN_POINT('Ctrl Pts',(7.2476936041087,-0.918131972250711,4.73342476157467));
#22078=CARTESIAN_POINT('Ctrl Pts',(6.81052198939154,2.64363748072991,4.89139378849694));
#22079=CARTESIAN_POINT('Ctrl Pts',(4.7301436742755,5.56756407401104,5.04936281541924));
#22080=CARTESIAN_POINT('Ctrl Pts',(1.50850132807235,7.14817827426755,5.20733184234154));
#22081=CARTESIAN_POINT('Ctrl Pts',(-2.07710423471086,7.00411785278149,5.36530086926381));
#22082=CARTESIAN_POINT('Ctrl Pts',(-5.16155708097404,5.17014094559845,5.52326989618611));
#22083=CARTESIAN_POINT('Ctrl Pts',(-6.7457960670029,2.51575743913742,5.65934772540162));
#22084=CARTESIAN_POINT('Ctrl Pts',(-7.01043408368973,0.677693690487587,
5.7427692123097));
#22085=CARTESIAN_POINT('Ctrl Pts',(-7.01072884945883,-8.57039139217561E-5,
5.77353435691036));
#22086=CARTESIAN_POINT('Ctrl Pts',(-7.01124999947611,-8.57102848142028E-5,
5.77353435691036));
#22087=CARTESIAN_POINT('Ctrl Pts',(-7.01124765095286,-0.192198986928101,
5.78225393955636));
#22088=CARTESIAN_POINT('Ctrl Pts',(-7.00334490103907,-0.384283885227448,
5.79097352220236));
#22089=CARTESIAN_POINT('Ctrl Pts',(-6.9875747245799,-0.575696127233885,
5.79969310484836));
#22090=CARTESIAN_POINT('Ctrl Pts',(-6.97179945475511,-0.767170190522794,
5.80841550369763));
#22091=CARTESIAN_POINT('Ctrl Pts',(-6.94815170444357,-0.95797088838034,
5.81713790254689));
#22092=CARTESIAN_POINT('Ctrl Pts',(-6.91671637063173,-1.14745858780829,
5.82586030139616));
#22093=CARTESIAN_POINT('Ctrl Pts',(-6.90068149315975,-1.24411453747826,
5.83030951760767));
#22094=CARTESIAN_POINT('Ctrl Pts',(-6.88262117299095,-1.34042896470014,
5.83475873381918));
#22095=CARTESIAN_POINT('Ctrl Pts',(-6.86255182738119,-1.43631785444836,
5.83920795003069));
#22096=CARTESIAN_POINT('Ctrl Pts',(-6.82406356285709,-1.62021009614443,
5.84774049582481));
#22097=CARTESIAN_POINT('Ctrl Pts',(-6.7781730643909,-1.80258540508638,5.85627304161894));
#22098=CARTESIAN_POINT('Ctrl Pts',(-6.7250248124813,-1.98284337102325,5.86480558741307));
#22099=CARTESIAN_POINT('Ctrl Pts',(-6.67941162972341,-2.13754534612922,
5.87212843542244));
#22100=CARTESIAN_POINT('Ctrl Pts',(-6.62845360124105,-2.29068783787579,
5.87945128343181));
#22101=CARTESIAN_POINT('Ctrl Pts',(-6.57227159525839,-2.44189939200201,
5.88677413144118));
#22102=CARTESIAN_POINT('',(-7.01128832852494,5.85639662721804E-5,5.22646564376811));
#22103=CARTESIAN_POINT('Ctrl Pts',(-6.57226144972351,-2.44189579807461,
5.33969278385492));
#22104=CARTESIAN_POINT('Ctrl Pts',(-6.86098992792226,-1.66232639080036,
5.30195040683487));
#22105=CARTESIAN_POINT('Ctrl Pts',(-7.01142817074718,-0.831069413347963,
5.26420802981482));
#22106=CARTESIAN_POINT('Ctrl Pts',(-7.01179827228896,5.836945010246E-5,
5.22646565279477));
#22107=CARTESIAN_POINT('Ctrl Pts',(-7.01124999975529,5.85785866401273E-5,
5.22646564308964));
#22108=CARTESIAN_POINT('Ctrl Pts',(-7.01124951887446,0.0576150329797373,
5.2238517402363));
#22109=CARTESIAN_POINT('Ctrl Pts',(-7.01054027751411,0.115170190668486,
5.22123783738296));
#22110=CARTESIAN_POINT('Ctrl Pts',(-7.00912252417848,0.172707856086104,
5.21862393452962));
#22111=CARTESIAN_POINT('Ctrl Pts',(-7.00449466308461,0.36052354766447,5.210091576316));
#22112=CARTESIAN_POINT('Ctrl Pts',(-6.99231264643713,0.548184763330246,
5.20155921810237));
#22113=CARTESIAN_POINT('Ctrl Pts',(-6.97261008798218,0.735074910107246,
5.19302685988874));
#22114=CARTESIAN_POINT('Ctrl Pts',(-6.95291121890469,0.921930061008123,
5.18449609939096));
#22115=CARTESIAN_POINT('Ctrl Pts',(-6.92569465043421,1.10801412699093,5.17596533889318));
#22116=CARTESIAN_POINT('Ctrl Pts',(-6.89104587162625,1.29271549756429,5.1674345783954));
#22117=CARTESIAN_POINT('Ctrl Pts',(-6.85490425999147,1.48537467440484,5.1585362724964));
#22118=CARTESIAN_POINT('Ctrl Pts',(-6.81067586429655,1.6765290197093,5.14963796659739));
#22119=CARTESIAN_POINT('Ctrl Pts',(-6.75851718018267,1.8654951320429,5.14073966069838));
#22120=CARTESIAN_POINT('Ctrl Pts',(-6.7085144586752,2.04665039026863,5.13220916344149));
#22121=CARTESIAN_POINT('Ctrl Pts',(-6.65122394657964,2.22579436325577,5.1236786661846));
#22122=CARTESIAN_POINT('Ctrl Pts',(-6.58683487955106,2.40233903353161,5.11514816892771));
#22123=CARTESIAN_POINT('Ctrl Pts',(-6.52244515359446,2.57888551048419,5.10661758437365));
#22124=CARTESIAN_POINT('Ctrl Pts',(-6.45095683542565,2.75283234522419,5.09808699981958));
#22125=CARTESIAN_POINT('Ctrl Pts',(-6.37260800387816,2.92360971940647,5.08955641526551));
#22126=CARTESIAN_POINT('Ctrl Pts',(-6.29424366890735,3.09442088648488,5.08102414270588));
#22127=CARTESIAN_POINT('Ctrl Pts',(-6.2090162376767,3.26206106268585,5.07249187014626));
#22128=CARTESIAN_POINT('Ctrl Pts',(-6.11721098429106,3.42598253588204,5.06395959758663));
#22129=CARTESIAN_POINT('Ctrl Pts',(-6.10535842102635,3.4471456998607,5.06285803426018));
#22130=CARTESIAN_POINT('Ctrl Pts',(-6.09339627968944,3.46824691360584,5.06175647093374));
#22131=CARTESIAN_POINT('Ctrl Pts',(-6.08132522944022,3.48928502938265,5.06065490760729));
#22132=CARTESIAN_POINT('Ctrl Pts',(-5.98782672393285,3.65223956467251,5.05212254939338));
#22133=CARTESIAN_POINT('Ctrl Pts',(-5.88775893032056,3.81146132850706,5.04359019117947));
#22134=CARTESIAN_POINT('Ctrl Pts',(-5.78144499964938,3.96642411732901,5.03505783296557));
#22135=CARTESIAN_POINT('Ctrl Pts',(-5.67515097665782,4.1213578887914,5.02652707246753));
#22136=CARTESIAN_POINT('Ctrl Pts',(-5.5626133237529,4.27203402456879,5.01799631196949));
#22137=CARTESIAN_POINT('Ctrl Pts',(-5.44419843676668,4.4179554030804,5.00946555147145));
#22138=CARTESIAN_POINT('Ctrl Pts',(-5.32068167790026,4.57016376287194,5.00056724557258));
#22139=CARTESIAN_POINT('Ctrl Pts',(-5.19077023271126,4.71719828644467,4.99166893967371));
#22140=CARTESIAN_POINT('Ctrl Pts',(-5.05492712101795,4.85853253191714,4.98277063377484));
#22141=CARTESIAN_POINT('Ctrl Pts',(-4.92469904110363,4.99402477134385,4.97424013651771));
#22142=CARTESIAN_POINT('Ctrl Pts',(-4.78902002914748,5.12427826093411,4.96570963926059));
#22143=CARTESIAN_POINT('Ctrl Pts',(-4.64833647798779,5.24886602514373,4.95717914200346));
#22144=CARTESIAN_POINT('Ctrl Pts',(-4.50765148713798,5.37345506432665,4.94864855744918));
#22145=CARTESIAN_POINT('Ctrl Pts',(-4.36196208595718,5.49237806183363,4.94011797289491));
#22146=CARTESIAN_POINT('Ctrl Pts',(-4.21174895258767,5.60524730256183,4.93158738834063));
#22147=CARTESIAN_POINT('Ctrl Pts',(-4.06150609550943,5.71813887750516,4.92305511578076));
#22148=CARTESIAN_POINT('Ctrl Pts',(-3.906737963619,5.82497412011798,4.91452284322088));
#22149=CARTESIAN_POINT('Ctrl Pts',(-3.74795621088343,5.92540722683263,4.905990570661));
#22150=CARTESIAN_POINT('Ctrl Pts',(-3.72745661311323,5.93837369341327,4.90488900733568));
#22151=CARTESIAN_POINT('Ctrl Pts',(-3.70689015424685,5.95123350738451,4.90378744401036));
#22152=CARTESIAN_POINT('Ctrl Pts',(-3.68625796921544,5.96398597809348,4.90268588068505));
#22153=CARTESIAN_POINT('Ctrl Pts',(-3.52644764385761,6.06276254926201,4.89415352247125));
#22154=CARTESIAN_POINT('Ctrl Pts',(-3.36263790090961,6.15512867677351,4.88562116425744));
#22155=CARTESIAN_POINT('Ctrl Pts',(-3.19536346054325,6.24077550609899,4.87708880604364));
#22156=CARTESIAN_POINT('Ctrl Pts',(-3.02812034293867,6.32640629773678,4.86855804554568));
#22157=CARTESIAN_POINT('Ctrl Pts',(-2.85741409488146,6.40532016272714,4.86002728504772));
#22158=CARTESIAN_POINT('Ctrl Pts',(-2.68380361693303,6.47725441126387,4.85149652454976));
#22159=CARTESIAN_POINT('Ctrl Pts',(-2.50271318069211,6.55228792653388,4.84259821865084));
#22160=CARTESIAN_POINT('Ctrl Pts',(-2.3184630319374,6.61972691672231,4.83369991275192));
#22161=CARTESIAN_POINT('Ctrl Pts',(-2.1317109996931,6.67932891661187,4.82480160685301));
#22162=CARTESIAN_POINT('Ctrl Pts',(-1.95267830325577,6.73646728680816,4.81627110959596));
#22163=CARTESIAN_POINT('Ctrl Pts',(-1.7713467053569,6.78640342040452,4.80774061233891));
#22164=CARTESIAN_POINT('Ctrl Pts',(-1.58831205271651,6.82897440218482,4.79921011508187));
#22165=CARTESIAN_POINT('Ctrl Pts',(-1.40527552698445,6.87154581961678,4.79067953052767));
#22166=CARTESIAN_POINT('Ctrl Pts',(-1.22053621044141,6.90675186845741,4.78214894597348));
#22167=CARTESIAN_POINT('Ctrl Pts',(-1.03470140506026,6.93448048269417,4.77361836141928));
#22168=CARTESIAN_POINT('Ctrl Pts',(-0.848829827264217,6.96221458378311,
4.76508608885947));
#22169=CARTESIAN_POINT('Ctrl Pts',(-0.661862630460365,6.98246825089994,
4.75655381629967));
#22170=CARTESIAN_POINT('Ctrl Pts',(-0.474414399316689,6.99518102269134,
4.74802154373986));
#22171=CARTESIAN_POINT('Ctrl Pts',(-0.45021380147482,6.99682231146585,4.74691998041415));
#22172=CARTESIAN_POINT('Ctrl Pts',(-0.426005191403975,6.998337977832,4.74581841708844));
#22173=CARTESIAN_POINT('Ctrl Pts',(-0.401789895976411,6.99972795485591,
4.74471685376273));
#22174=CARTESIAN_POINT('Ctrl Pts',(-0.214225940260526,7.01049427359601,
4.7361844955489));
#22175=CARTESIAN_POINT('Ctrl Pts',(-0.026197395778026,7.01371915439505,
4.72765213733507));
#22176=CARTESIAN_POINT('Ctrl Pts',(0.161678462626507,7.0093856105384,4.71911977912124));
#22177=CARTESIAN_POINT('Ctrl Pts',(0.349519140576629,7.00505287815397,4.71058901862328));
#22178=CARTESIAN_POINT('Ctrl Pts',(0.537206883732021,6.9931645526712,4.70205825812531));
#22179=CARTESIAN_POINT('Ctrl Pts',(0.724125135371328,6.97375575646462,4.69352749762734));
#22180=CARTESIAN_POINT('Ctrl Pts',(0.91909670696476,6.95351073776824,4.68462919172844));
#22181=CARTESIAN_POINT('Ctrl Pts',(1.11323065855079,6.92508287194462,4.67573088582953));
#22182=CARTESIAN_POINT('Ctrl Pts',(1.30583306940464,6.88857217116503,4.66683257993062));
#22183=CARTESIAN_POINT('Ctrl Pts',(1.49047432091466,6.85357062858015,4.65830208267355));
#22184=CARTESIAN_POINT('Ctrl Pts',(1.67370777652848,6.81114108016015,4.64977158541649));
#22185=CARTESIAN_POINT('Ctrl Pts',(1.8549318983874,6.76142397833806,4.64124108815942));
#22186=CARTESIAN_POINT('Ctrl Pts',(2.03615787481013,6.71170636773416,4.63271050360519));
#22187=CARTESIAN_POINT('Ctrl Pts',(2.21537418216918,6.65470113877529,4.62417991905096));
#22188=CARTESIAN_POINT('Ctrl Pts',(2.39199342126689,6.5905989132336,4.61564933449673));
#22189=CARTESIAN_POINT('Ctrl Pts',(2.56864760923149,6.52648400334247,4.60711706193691));
#22190=CARTESIAN_POINT('Ctrl Pts',(2.74270341524402,6.45526939735551,4.59858478937708));
#22191=CARTESIAN_POINT('Ctrl Pts',(2.91359160767148,6.37719456392906,4.59005251681726));
#22192=CARTESIAN_POINT('Ctrl Pts',(2.93565421341179,6.36711467342487,4.58895095349166));
#22193=CARTESIAN_POINT('Ctrl Pts',(2.95766404936562,6.35692050022327,4.58784939016606));
#22194=CARTESIAN_POINT('Ctrl Pts',(2.97961991686035,6.34661261725884,4.58674782684045));
#22195=CARTESIAN_POINT('Ctrl Pts',(3.14968306439527,6.26677104316607,4.57821546862661));
#22196=CARTESIAN_POINT('Ctrl Pts',(3.3165638783545,6.18007659508099,4.56968311041277));
#22197=CARTESIAN_POINT('Ctrl Pts',(3.4797114620282,6.08680825256798,4.56115075219893));
#22198=CARTESIAN_POINT('Ctrl Pts',(3.64282849570919,5.99355737489948,4.55261999170095));
#22199=CARTESIAN_POINT('Ctrl Pts',(3.80221342864592,5.89373521119594,4.54408923120296));
#22200=CARTESIAN_POINT('Ctrl Pts',(3.95734080749966,5.78766622187198,4.53555847070498));
#22201=CARTESIAN_POINT('Ctrl Pts',(4.11915180555327,5.67702728017215,4.52666016480608));
#22202=CARTESIAN_POINT('Ctrl Pts',(4.27632994760052,5.55959148334597,4.51776185890717));
#22203=CARTESIAN_POINT('Ctrl Pts',(4.42831264673592,5.43577719054587,4.50886355300827));
#22204=CARTESIAN_POINT('Ctrl Pts',(4.57401318938176,5.31708072212603,4.50033305575119));
#22205=CARTESIAN_POINT('Ctrl Pts',(4.71493890431663,5.19252266857053,4.4918025584941));
#22206=CARTESIAN_POINT('Ctrl Pts',(4.85062769841396,5.06251296234185,4.48327206123702));
#22207=CARTESIAN_POINT('Ctrl Pts',(4.98631788108777,4.93250192565387,4.47474147668276));
#22208=CARTESIAN_POINT('Ctrl Pts',(5.11677081713854,4.79703933883374,4.46621089212851));
#22209=CARTESIAN_POINT('Ctrl Pts',(5.2415607347134,4.656572519226,4.45768030757425));
#22210=CARTESIAN_POINT('Ctrl Pts',(5.36637534532973,4.51607790448007,4.44914803501441));
#22211=CARTESIAN_POINT('Ctrl Pts',(5.48552449687935,4.37057730861295,4.44061576245457));
#22212=CARTESIAN_POINT('Ctrl Pts',(5.59862165195997,4.22055235256063,4.43208348989472));
#22213=CARTESIAN_POINT('Ctrl Pts',(5.61322311685505,4.20118330541155,4.4309819265692));
#22214=CARTESIAN_POINT('Ctrl Pts',(5.62772376196302,4.18173888880038,4.42988036324368));
#22215=CARTESIAN_POINT('Ctrl Pts',(5.64212280602026,4.16222017729554,4.42877879991815));
#22216=CARTESIAN_POINT('Ctrl Pts',(5.75365320920836,4.01103446279999,4.42024644170434));
#22217=CARTESIAN_POINT('Ctrl Pts',(5.8591221730809,3.85533786342847,4.41171408349054));
#22218=CARTESIAN_POINT('Ctrl Pts',(5.95817809650529,3.69563801431155,4.40318172527673));
#22219=CARTESIAN_POINT('Ctrl Pts',(6.05721547133908,3.53596806958618,4.39465096477877));
#22220=CARTESIAN_POINT('Ctrl Pts',(6.14984204099429,3.37229663100463,4.38612020428082));
#22221=CARTESIAN_POINT('Ctrl Pts',(6.23575023411537,3.20515921293001,4.37758944378287));
#22222=CARTESIAN_POINT('Ctrl Pts',(6.32535975741612,3.03082072651491,4.36869113788395));
#22223=CARTESIAN_POINT('Ctrl Pts',(6.40765897968901,2.85271128620633,4.35979283198503));
#22224=CARTESIAN_POINT('Ctrl Pts',(6.48235238583884,2.67146665865579,4.35089452608612));
#22225=CARTESIAN_POINT('Ctrl Pts',(6.55395836382148,2.49771372009221,4.34236402882907));
#22226=CARTESIAN_POINT('Ctrl Pts',(6.61857452743737,2.32107986933111,4.33383353157203));
#22227=CARTESIAN_POINT('Ctrl Pts',(6.67598971967607,2.14214561252951,4.32530303431498));
#22228=CARTESIAN_POINT('Ctrl Pts',(6.7334054994753,1.96320952459746,4.31677244976077));
#22229=CARTESIAN_POINT('Ctrl Pts',(6.78362007023891,1.7819732759193,4.30824186520656));
#22230=CARTESIAN_POINT('Ctrl Pts',(6.82647201543804,1.59903295305049,4.29971128065235));
#22231=CARTESIAN_POINT('Ctrl Pts',(6.86933244004708,1.41605643051839,4.29117900809254));
#22232=CARTESIAN_POINT('Ctrl Pts',(6.90482726045359,1.23137545847014,4.28264673553274));
#22233=CARTESIAN_POINT('Ctrl Pts',(6.93284589518463,1.04559760717099,4.27411446297293));
#22234=CARTESIAN_POINT('Ctrl Pts',(6.93646325506608,1.02161266455678,4.27301289964725));
#22235=CARTESIAN_POINT('Ctrl Pts',(6.93995607042438,0.997609450460709,4.27191133632156));
#22236=CARTESIAN_POINT('Ctrl Pts',(6.94332416590407,0.973589281818827,4.27080977299588));
#22237=CARTESIAN_POINT('Ctrl Pts',(6.96941235934794,0.787536715951268,4.26227741478204));
#22238=CARTESIAN_POINT('Ctrl Pts',(6.98802247973373,0.60040361675269,4.2537450565682));
#22239=CARTESIAN_POINT('Ctrl Pts',(6.9990870539665,0.412803795402279,4.24521269835437));
#22240=CARTESIAN_POINT('Ctrl Pts',(7.01014955631654,0.225239102817181,4.23668193785639));
#22241=CARTESIAN_POINT('Ctrl Pts',(7.01366931419739,0.0372081678141407,
4.22815117735841));
#22242=CARTESIAN_POINT('Ctrl Pts',(7.00963084742555,-0.150671647366538,
4.21962041686043));
#22243=CARTESIAN_POINT('Ctrl Pts',(7.00541838445617,-0.346646211193886,
4.21072211096152));
#22244=CARTESIAN_POINT('Ctrl Pts',(6.99298196617915,-0.542455991884459,
4.20182380506262));
#22245=CARTESIAN_POINT('Ctrl Pts',(6.97236444962771,-0.73740120970049,4.19292549916372));
#22246=CARTESIAN_POINT('Ctrl Pts',(6.95259915155997,-0.924288428992888,
4.18439500190664));
#22247=CARTESIAN_POINT('Ctrl Pts',(6.92531551788594,-1.11038079629712,4.17586450464957));
#22248=CARTESIAN_POINT('Ctrl Pts',(6.89060427455715,-1.29506729321484,4.16733400739249));
#22249=CARTESIAN_POINT('Ctrl Pts',(6.85589267600955,-1.4797556801287,4.15880342283826));
#22250=CARTESIAN_POINT('Ctrl Pts',(6.81375337561684,-1.66303786779166,4.15027283828402));
#22251=CARTESIAN_POINT('Ctrl Pts',(6.76432825789992,-1.84431282104653,4.14174225372979));
#22252=CARTESIAN_POINT('Ctrl Pts',(6.71489336009411,-2.02562364442655,4.13320998116996));
#22253=CARTESIAN_POINT('Ctrl Pts',(6.65816984694882,-2.20492614515935,4.12467770861013));
#22254=CARTESIAN_POINT('Ctrl Pts',(6.594349773433,-2.38163339498844,4.1161454360503));
#22255=CARTESIAN_POINT('Ctrl Pts',(6.58611025085242,-2.40444727305077,4.11504387272472));
#22256=CARTESIAN_POINT('Ctrl Pts',(6.57775250845608,-2.42721791616829,4.11394230939915));
#22257=CARTESIAN_POINT('Ctrl Pts',(6.56927701910553,-2.44994408278067,4.11284074607358));
#22258=CARTESIAN_POINT('Ctrl Pts',(6.50362858156439,-2.62597372162438,4.10430838785975));
#22259=CARTESIAN_POINT('Ctrl Pts',(6.43088970711191,-2.79939283689084,4.09577602964591));
#22260=CARTESIAN_POINT('Ctrl Pts',(6.35129333024201,-2.96962953846491,4.08724367143208));
#22261=CARTESIAN_POINT('Ctrl Pts',(6.27171185809015,-3.13983436258256,4.0787129109341));
#22262=CARTESIAN_POINT('Ctrl Pts',(6.18527557564355,-3.30685768517691,4.07018215043612));
#22263=CARTESIAN_POINT('Ctrl Pts',(6.09226482886744,-3.47014925002438,4.06165138993814));
#22264=CARTESIAN_POINT('Ctrl Pts',(5.99524674039861,-3.64047618571409,4.05275308403924));
#22265=CARTESIAN_POINT('Ctrl Pts',(5.89107527475306,-3.80674235923989,4.04385477814033));
#22266=CARTESIAN_POINT('Ctrl Pts',(5.78012132077429,-3.96835281692927,4.03495647224143));
#22267=CARTESIAN_POINT('Ctrl Pts',(5.67375361316453,-4.12328315779367,4.02642597498436));
#22268=CARTESIAN_POINT('Ctrl Pts',(5.56115303293269,-4.27393466016512,4.01789547772729));
#22269=CARTESIAN_POINT('Ctrl Pts',(5.4426902991149,-4.41981321668921,4.00936498047022));
#22270=CARTESIAN_POINT('Ctrl Pts',(5.32422635300424,-4.56569326606702,4.00083439591599));
#22271=CARTESIAN_POINT('Ctrl Pts',(5.19990032882851,-4.70680003650974,3.99230381136175));
#22272=CARTESIAN_POINT('Ctrl Pts',(5.07012317901214,-4.84267255884019,3.98377322680751));
#22273=CARTESIAN_POINT('Ctrl Pts',(4.94032034929621,-4.97857196720361,3.97524095424769));
#22274=CARTESIAN_POINT('Ctrl Pts',(4.80506445163746,-5.10923483821557,3.96670868168786));
#22275=CARTESIAN_POINT('Ctrl Pts',(4.66480383944029,-5.23423649657169,3.95817640912803));
#22276=CARTESIAN_POINT('Ctrl Pts',(4.6466954227979,-5.25037489832999,3.95707484580245));
#22277=CARTESIAN_POINT('Ctrl Pts',(4.62850363449858,-5.26641899021547,3.95597328247687));
#22278=CARTESIAN_POINT('Ctrl Pts',(4.61022948153133,-5.28236790560061,3.95487171915129));
#22279=CARTESIAN_POINT('Ctrl Pts',(4.46868372056602,-5.4059031178103,3.94633936093747));
#22280=CARTESIAN_POINT('Ctrl Pts',(4.3221459019274,-5.5237666028468,3.93780700272365));
#22281=CARTESIAN_POINT('Ctrl Pts',(4.17109316649641,-5.63556637427925,3.92927464450982));
#22282=CARTESIAN_POINT('Ctrl Pts',(4.0200687162526,-5.74734521078819,3.92074388401185));
#22283=CARTESIAN_POINT('Ctrl Pts',(3.86453128223682,-5.85306241768181,3.91221312351388));
#22284=CARTESIAN_POINT('Ctrl Pts',(3.7049893961723,-5.95236760766259,3.90368236301591));
#22285=CARTESIAN_POINT('Ctrl Pts',(3.53857369311416,-6.05595133363967,3.894784057117));
#22286=CARTESIAN_POINT('Ctrl Pts',(3.36780111999562,-6.15255807762872,3.88588575121809));
#22287=CARTESIAN_POINT('Ctrl Pts',(3.19328111137326,-6.24184125929575,3.87698744531918));
#22288=CARTESIAN_POINT('Ctrl Pts',(3.02597483175454,-6.32743394906898,3.86845694806211));
#22289=CARTESIAN_POINT('Ctrl Pts',(2.85522497701625,-6.40629618934995,3.85992645080505));
#22290=CARTESIAN_POINT('Ctrl Pts',(2.68159281415216,-6.47816999943561,3.85139595354799));
#22291=CARTESIAN_POINT('Ctrl Pts',(2.50795887441703,-6.55004454504451,3.84286536899377));
#22292=CARTESIAN_POINT('Ctrl Pts',(2.33144285156694,-6.61493040351266,3.83433478443955));
#22293=CARTESIAN_POINT('Ctrl Pts',(2.15262561350387,-6.67261789184628,3.82580419988533));
#22294=CARTESIAN_POINT('Ctrl Pts',(1.97377299164063,-6.73031679520108,3.81727192732552));
#22295=CARTESIAN_POINT('Ctrl Pts',(1.79261853660373,-6.78081439051758,3.8087396547657));
#22296=CARTESIAN_POINT('Ctrl Pts',(1.6097587238965,-6.82395071885335,3.80020738220588));
#22297=CARTESIAN_POINT('Ctrl Pts',(1.58615051611865,-6.82951985614517,3.79910581888026));
#22298=CARTESIAN_POINT('Ctrl Pts',(1.56251390031482,-6.83496636322313,3.79800425555463));
#22299=CARTESIAN_POINT('Ctrl Pts',(1.53885017464052,-6.84028995748783,3.796902692229));
#22300=CARTESIAN_POINT('Ctrl Pts',(1.35555850231485,-6.88152482088127,3.78837033401517));
#22301=CARTESIAN_POINT('Ctrl Pts',(1.17057760880845,-6.91539519781985,3.77983797580134));
#22302=CARTESIAN_POINT('Ctrl Pts',(0.984513719362816,-6.94178358196843,
3.77130561758751));
#22303=CARTESIAN_POINT('Ctrl Pts',(0.798484671073654,-6.96816702479376,
3.76277485708954));
#22304=CARTESIAN_POINT('Ctrl Pts',(0.611373334374456,-6.98707122782371,
3.75424409659157));
#22305=CARTESIAN_POINT('Ctrl Pts',(0.423793730903746,-6.99843021227952,
3.7457133360936));
#22306=CARTESIAN_POINT('Ctrl Pts',(0.228132313322538,-7.01027859536479,
3.7368150301947));
#22307=CARTESIAN_POINT('Ctrl Pts',(0.0319617353463715,-7.01391714592579,
3.72791672429579));
#22308=CARTESIAN_POINT('Ctrl Pts',(-0.164017063899415,-7.00933127803572,
3.71901841839688));
#22309=CARTESIAN_POINT('Ctrl Pts',(-0.351895141861999,-7.00493496553512,
3.71048792113981));
#22310=CARTESIAN_POINT('Ctrl Pts',(-0.539596649862154,-6.99298047977504,
3.70195742388274));
#22311=CARTESIAN_POINT('Ctrl Pts',(-0.726505192478232,-6.9735082109224,
3.69342692662567));
#22312=CARTESIAN_POINT('Ctrl Pts',(-0.913415647829727,-6.9540357427996,
3.68489634207145));
#22313=CARTESIAN_POINT('Ctrl Pts',(-1.09953281758575,-6.92704537277552,
3.67636575751722));
#22314=CARTESIAN_POINT('Ctrl Pts',(-1.28424606709989,-6.89262929524274,
3.667835172963));
#22315=CARTESIAN_POINT('Ctrl Pts',(-1.46899586709867,-6.85820640756334,
3.65930290040317));
#22316=CARTESIAN_POINT('Ctrl Pts',(-1.65234089137648,-6.81635493464879,
3.65077062784334));
#22317=CARTESIAN_POINT('Ctrl Pts',(-1.83368045678355,-6.76721822796562,
3.64223835528352));
#22318=CARTESIAN_POINT('Ctrl Pts',(-1.85709239227112,-6.76087440881972,
3.64113679195791));
#22319=CARTESIAN_POINT('Ctrl Pts',(-1.88047091801555,-6.75440922668789,
3.64003522863231));
#22320=CARTESIAN_POINT('Ctrl Pts',(-1.90381475790692,-6.74782305118294,
3.63893366530671));
#22321=CARTESIAN_POINT('Ctrl Pts',(-2.08462869697902,-6.69680863615906,
3.63040130709288));
#22322=CARTESIAN_POINT('Ctrl Pts',(-2.26342145439311,-6.63851383971342,
3.62186894887905));
#22323=CARTESIAN_POINT('Ctrl Pts',(-2.43960398736489,-6.57312398691317,
3.61333659066523));
#22324=CARTESIAN_POINT('Ctrl Pts',(-2.61575352950101,-6.50774637860647,
3.60480583016726));
#22325=CARTESIAN_POINT('Ctrl Pts',(-2.78929353586576,-6.43527647171771,
3.59627506966929));
#22326=CARTESIAN_POINT('Ctrl Pts',(-2.95965264279651,-6.35594861499742,
3.58774430917133));
#22327=CARTESIAN_POINT('Ctrl Pts',(-3.13735162361963,-6.27320294002855,
3.57884600327242));
#22328=CARTESIAN_POINT('Ctrl Pts',(-3.31158920764694,-6.18299540693946,
3.56994769737351));
#22329=CARTESIAN_POINT('Ctrl Pts',(-3.48174207006675,-6.08564694342576,
3.5610493914746));
#22330=CARTESIAN_POINT('Ctrl Pts',(-3.64486171808113,-5.99232234766365,
3.55251889421753));
#22331=CARTESIAN_POINT('Ctrl Pts',(-3.80422725291711,-5.8924354509167,3.54398839696047));
#22332=CARTESIAN_POINT('Ctrl Pts',(-3.95931587135017,-5.7863152690961,3.5354578997034));
#22333=CARTESIAN_POINT('Ctrl Pts',(-4.11440607688823,-5.68019400129077,
3.52692731514918));
#22334=CARTESIAN_POINT('Ctrl Pts',(-4.26521902787035,-5.56783949640536,
3.51839673059496));
#22335=CARTESIAN_POINT('Ctrl Pts',(-4.41126165360132,-5.44962358204368,
3.50986614604074));
#22336=CARTESIAN_POINT('Ctrl Pts',(-4.55733317779396,-5.33138427548364,
3.50133387348092));
#22337=CARTESIAN_POINT('Ctrl Pts',(-4.69863225422205,-5.20728143622081,
3.49280160092109));
#22338=CARTESIAN_POINT('Ctrl Pts',(-4.83469892174064,-5.07772713904754,
3.48426932836127));
#22339=CARTESIAN_POINT('Ctrl Pts',(-4.85226587705371,-5.06100096657222,
3.48316776503565));
#22340=CARTESIAN_POINT('Ctrl Pts',(-4.86974566578051,-5.04418398015781,
3.48206620171004));
#22341=CARTESIAN_POINT('Ctrl Pts',(-4.88713734174978,-5.02727711245113,
3.48096463838442));
#22342=CARTESIAN_POINT('Ctrl Pts',(-5.0218468407324,-4.89632275922165,3.4724323356924));
#22343=CARTESIAN_POINT('Ctrl Pts',(-5.15131248351839,-4.75992877233467,
3.46390003300037));
#22344=CARTESIAN_POINT('Ctrl Pts',(-5.27510453917352,-4.61853858523353,
3.45536773030835));
#22345=CARTESIAN_POINT('Ctrl Pts',(-5.39887311251369,-4.47717521866533,
3.44683704612261));
#22346=CARTESIAN_POINT('Ctrl Pts',(-5.51697004508846,-4.33081777338997,
3.43830636193686));
#22347=CARTESIAN_POINT('Ctrl Pts',(-5.62900449685822,-4.17994437006642,
3.42977567775112));
#22348=CARTESIAN_POINT('Ctrl Pts',(-5.74103758216335,-4.02907280691941,
3.42124509761264));
#22349=CARTESIAN_POINT('Ctrl Pts',(-5.84700814907071,-3.87368563925147,
3.41271451747416));
#22350=CARTESIAN_POINT('Ctrl Pts',(-5.94656695937722,-3.71429239023305,
3.40418393733567));
#22351=CARTESIAN_POINT('Ctrl Pts',(-6.04611930050683,-3.55490949834046,
3.39565391150105));
#22352=CARTESIAN_POINT('Ctrl Pts',(-6.13926055637389,-3.39152130535483,
3.38712388566642));
#22353=CARTESIAN_POINT('Ctrl Pts',(-6.22568574525753,-3.22466487619989,
3.37859385983179));
#22354=CARTESIAN_POINT('Ctrl Pts',(-6.31212407181111,-3.05778308285747,
3.37006253733046));
#22355=CARTESIAN_POINT('Ctrl Pts',(-6.39184415037769,-2.88743227152021,
3.36153121482914));
#22356=CARTESIAN_POINT('Ctrl Pts',(-6.46458732400406,-2.71417340876113,
3.35299989232781));
#22357=CARTESIAN_POINT('Ctrl Pts',(-6.50237430244478,-2.62417281371743,
3.34856823388679));
#22358=CARTESIAN_POINT('Ctrl Pts',(-6.53827943706638,-2.53338788513101,
3.34413657544576));
#22359=CARTESIAN_POINT('Ctrl Pts',(-6.5722715952584,-2.44189939200197,3.33970491700474));
#22360=CARTESIAN_POINT('Origin',(0.,0.,0.));
#22361=CARTESIAN_POINT('',(-6.57174751820833,-2.4417044432219,1.33970341751611));
#22362=CARTESIAN_POINT('',(-6.57227159525839,-2.441899392002,1.88676850238605));
#22363=CARTESIAN_POINT('',(-6.57227159525839,-2.441899392002,0.));
#22364=CARTESIAN_POINT('',(-7.01126267432566,-8.75058266332513E-5,3.77353435527672));
#22365=CARTESIAN_POINT('Ctrl Pts',(-6.5722715952584,-2.44189939200199,1.88676850238605));
#22366=CARTESIAN_POINT('Ctrl Pts',(-6.56405595980073,-2.46401143631154,
1.88783976058185));
#22367=CARTESIAN_POINT('Ctrl Pts',(-6.55572891713045,-2.48608151822896,
1.88891101877765));
#22368=CARTESIAN_POINT('Ctrl Pts',(-6.54729091522851,-2.50810849722778,
1.88998227697344));
#22369=CARTESIAN_POINT('Ctrl Pts',(-6.48008391030787,-2.68354899880218,
1.89851463518728));
#22370=CARTESIAN_POINT('Ctrl Pts',(-6.40580989920254,-2.8563161967038,1.90704699340112));
#22371=CARTESIAN_POINT('Ctrl Pts',(-6.3247068791517,-3.02584028912816,1.91557935161496));
#22372=CARTESIAN_POINT('Ctrl Pts',(-6.24361904594361,-3.19533263753446,
1.92411011211292));
#22373=CARTESIAN_POINT('Ctrl Pts',(-6.15570488771711,-3.36158281647229,
1.93264087261089));
#22374=CARTESIAN_POINT('Ctrl Pts',(-6.06124961945423,-3.5240430776547,1.94117163310885));
#22375=CARTESIAN_POINT('Ctrl Pts',(-5.96272477269912,-3.69350289319662,
1.95006993900776));
#22376=CARTESIAN_POINT('Ctrl Pts',(-5.85708284365987,-3.85883866531672,
1.95896824490667));
#22377=CARTESIAN_POINT('Ctrl Pts',(-5.74469998304298,-4.01945875303206,
1.96786655080557));
#22378=CARTESIAN_POINT('Ctrl Pts',(-5.63696243219612,-4.17343966055005,
1.97639704806265));
#22379=CARTESIAN_POINT('Ctrl Pts',(-5.52303020146616,-4.3230866205467,1.98492754531972));
#22380=CARTESIAN_POINT('Ctrl Pts',(-5.40327837738593,-4.46790883288521,
1.99345804257679));
#22381=CARTESIAN_POINT('Ctrl Pts',(-5.28352532782082,-4.61273252726739,
2.00198862713103));
#22382=CARTESIAN_POINT('Ctrl Pts',(-5.15795276337739,-4.75273114158654,
2.01051921168528));
#22383=CARTESIAN_POINT('Ctrl Pts',(-5.02697570850291,-4.8874473693966,2.01904979623952));
#22384=CARTESIAN_POINT('Ctrl Pts',(-4.89597273629508,-5.02219025443594,
2.02758206879937));
#22385=CARTESIAN_POINT('Ctrl Pts',(-4.7595633517329,-5.15164844659135,2.03611434135923));
#22386=CARTESIAN_POINT('Ctrl Pts',(-4.61819965689422,-5.27540126355921,
2.04464661391908));
#22387=CARTESIAN_POINT('Ctrl Pts',(-4.59994882621505,-5.29137843302361,
2.04574817724463));
#22388=CARTESIAN_POINT('Ctrl Pts',(-4.5816154635611,-5.30726055692826,2.04684974057018));
#22389=CARTESIAN_POINT('Ctrl Pts',(-4.5632005835676,-5.32304677761039,2.04795130389573));
#22390=CARTESIAN_POINT('Ctrl Pts',(-4.42056479593313,-5.44532180853984,
2.05648366210955));
#22391=CARTESIAN_POINT('Ctrl Pts',(-4.27298744763936,-5.56188106242753,
2.06501602032336));
#22392=CARTESIAN_POINT('Ctrl Pts',(-4.12094913720164,-5.6723367998645,2.07354837853718));
#22393=CARTESIAN_POINT('Ctrl Pts',(-3.96893929650412,-5.78277185405303,
2.08207913903513));
#22394=CARTESIAN_POINT('Ctrl Pts',(-3.81247040812485,-5.88710549284097,
2.09060989953307));
#22395=CARTESIAN_POINT('Ctrl Pts',(-3.6520540912579,-5.98499185271179,2.09914066003102));
#22396=CARTESIAN_POINT('Ctrl Pts',(-3.48472628279308,-6.08709561868571,
2.10803896592994));
#22397=CARTESIAN_POINT('Ctrl Pts',(-3.31310365217863,-6.1821840374061,2.11693727182885));
#22398=CARTESIAN_POINT('Ctrl Pts',(-3.13779868371105,-6.26991594704437,
2.12583557772777));
#22399=CARTESIAN_POINT('Ctrl Pts',(-2.96973989031241,-6.35402148612434,
2.13436607498484));
#22400=CARTESIAN_POINT('Ctrl Pts',(-2.79829734737156,-6.4313663004645,2.14289657224191));
#22401=CARTESIAN_POINT('Ctrl Pts',(-2.62403458775532,-6.5016973972005,2.15142706949898));
#22402=CARTESIAN_POINT('Ctrl Pts',(-2.44977004481376,-6.57202921367275,
2.15995765405326));
#22403=CARTESIAN_POINT('Ctrl Pts',(-2.27268551247757,-6.63534705760097,
2.16848823860754));
#22404=CARTESIAN_POINT('Ctrl Pts',(-2.09336369541439,-6.69144640576468,
2.17701882316181));
#22405=CARTESIAN_POINT('Ctrl Pts',(-1.91400639470832,-6.74755685469275,
2.1855510957216));
#22406=CARTESIAN_POINT('Ctrl Pts',(-1.73241121739424,-6.79644586458776,
2.19408336828139));
#22407=CARTESIAN_POINT('Ctrl Pts',(-1.54917603414106,-6.83795877274374,
2.20261564084119));
#22408=CARTESIAN_POINT('Ctrl Pts',(-1.52551936396098,-6.84331831755945,
2.2037172041668));
#22409=CARTESIAN_POINT('Ctrl Pts',(-1.5018353744393,-6.84855498504257,2.20481876749241));
#22410=CARTESIAN_POINT('Ctrl Pts',(-1.47812536618678,-6.85366850411772,
2.20592033081802));
#22411=CARTESIAN_POINT('Ctrl Pts',(-1.29447520376752,-6.89327619208995,
2.21445268903187));
#22412=CARTESIAN_POINT('Ctrl Pts',(-1.1092011998166,-6.92550470208483,2.22298504724571));
#22413=CARTESIAN_POINT('Ctrl Pts',(-0.922910597859375,-6.95024190880137,
2.23151740545955));
#22414=CARTESIAN_POINT('Ctrl Pts',(-0.736654879511946,-6.97497448338371,
2.24004816595751));
#22415=CARTESIAN_POINT('Ctrl Pts',(-0.549383246244183,-6.99221851384896,
2.24857892645547));
#22416=CARTESIAN_POINT('Ctrl Pts',(-0.361710280690892,-7.00191346956977,
2.25710968695342));
#22417=CARTESIAN_POINT('Ctrl Pts',(-0.165951478547931,-7.01202612971311,
2.26600799285233));
#22418=CARTESIAN_POINT('Ctrl Pts',(0.030243653652506,-7.01392476462728,
2.27490629875124));
#22419=CARTESIAN_POINT('Ctrl Pts',(0.226174074993435,-7.00760100535846,
2.28380460465015));
#22420=CARTESIAN_POINT('Ctrl Pts',(0.414005774736144,-7.00153863666605,
2.2923351019072));
#22421=CARTESIAN_POINT('Ctrl Pts',(0.601593880499382,-6.98791995789897,
2.30086559916426));
#22422=CARTESIAN_POINT('Ctrl Pts',(0.788322379309909,-6.96679082424463,
2.30939609642131));
#22423=CARTESIAN_POINT('Ctrl Pts',(0.975052789013054,-6.94566147436457,
2.31792668097551));
#22424=CARTESIAN_POINT('Ctrl Pts',(1.16092327051103,-6.91702155363308,2.3264572655297));
#22425=CARTESIAN_POINT('Ctrl Pts',(1.34532403081394,-6.88096866833548,2.3349878500839));
#22426=CARTESIAN_POINT('Ctrl Pts',(1.52976127976858,-6.84490864900452,2.34352012264377));
#22427=CARTESIAN_POINT('Ctrl Pts',(1.71272792656109,-6.80143279508103,2.35205239520363));
#22428=CARTESIAN_POINT('Ctrl Pts',(1.89362458300221,-6.75068977965583,2.3605846677635));
#22429=CARTESIAN_POINT('Ctrl Pts',(1.91697933650567,-6.74413857721466,2.3616862310891));
#22430=CARTESIAN_POINT('Ctrl Pts',(1.94029960525135,-6.73746631286051,2.36278779441471));
#22431=CARTESIAN_POINT('Ctrl Pts',(1.96358411645753,-6.73067336750906,2.36388935774031));
#22432=CARTESIAN_POINT('Ctrl Pts',(2.14393851445478,-6.67805737919648,2.37242171595415));
#22433=CARTESIAN_POINT('Ctrl Pts',(2.32220724296558,-6.61817922097852,2.38095407416798));
#22434=CARTESIAN_POINT('Ctrl Pts',(2.49780292595847,-6.55122943466136,2.38948643238182));
#22435=CARTESIAN_POINT('Ctrl Pts',(2.67336572800529,-6.48429218494119,2.39801719287978));
#22436=CARTESIAN_POINT('Ctrl Pts',(2.84625619763583,-6.41028605867833,2.40654795337774));
#22437=CARTESIAN_POINT('Ctrl Pts',(3.01590507201999,-6.32945046264398,2.4150787138757));
#22438=CARTESIAN_POINT('Ctrl Pts',(3.1928632201284,-6.24513208783953,2.42397701977461));
#22439=CARTESIAN_POINT('Ctrl Pts',(3.36629393079521,-6.15338284636422,2.43287532567352));
#22440=CARTESIAN_POINT('Ctrl Pts',(3.53557674992503,-6.05452918135585,2.44177363157243));
#22441=CARTESIAN_POINT('Ctrl Pts',(3.69786231761193,-5.95976160112368,2.4503041288295));
#22442=CARTESIAN_POINT('Ctrl Pts',(3.85633572086378,-5.85846527198439,2.45883462608657));
#22443=CARTESIAN_POINT('Ctrl Pts',(4.01047709495085,-5.75097383348026,2.46736512334363));
#22444=CARTESIAN_POINT('Ctrl Pts',(4.16462004644966,-5.64348129495831,2.47589570789788));
#22445=CARTESIAN_POINT('Ctrl Pts',(4.31443063106958,-5.52979369806212,2.48442629245213));
#22446=CARTESIAN_POINT('Ctrl Pts',(4.45941909512374,-5.41028722865485,2.49295687700637));
#22447=CARTESIAN_POINT('Ctrl Pts',(4.60443624904525,-5.29075711167826,2.50148914956621));
#22448=CARTESIAN_POINT('Ctrl Pts',(4.74462914114087,-5.16540601787146,2.51002142212606));
#22449=CARTESIAN_POINT('Ctrl Pts',(4.87954148291101,-5.03465008506556,2.5185536946859));
#22450=CARTESIAN_POINT('Ctrl Pts',(4.89695940841886,-5.0177687748204,2.51965525801147));
#22451=CARTESIAN_POINT('Ctrl Pts',(4.91428936536944,-5.00079742725952,2.52075682133704));
#22452=CARTESIAN_POINT('Ctrl Pts',(4.93153041590004,-4.98373698338434,2.5218583846626));
#22453=CARTESIAN_POINT('Ctrl Pts',(5.06507409486585,-4.85159222597303,2.53039074287643));
#22454=CARTESIAN_POINT('Ctrl Pts',(5.19332581262223,-4.71405448464751,2.53892310109026));
#22455=CARTESIAN_POINT('Ctrl Pts',(5.31585977961177,-4.57157099540256,2.54745545930409));
#22456=CARTESIAN_POINT('Ctrl Pts',(5.43837080165949,-4.42911418672179,2.55598621980206));
#22457=CARTESIAN_POINT('Ctrl Pts',(5.55516601017619,-4.28171371019237,2.56451698030003));
#22458=CARTESIAN_POINT('Ctrl Pts',(5.66585881085924,-4.12985114718542,2.573047740798));
#22459=CARTESIAN_POINT('Ctrl Pts',(5.78132077952185,-3.97144562864463,2.5819460466969));
#22460=CARTESIAN_POINT('Ctrl Pts',(5.89014262468045,-3.80818528217321,2.59084435259581));
#22461=CARTESIAN_POINT('Ctrl Pts',(5.9919341789416,-3.64065260052803,2.59974265849472));
#22462=CARTESIAN_POINT('Ctrl Pts',(6.08951821170951,-3.48004482894987,2.60827315575179));
#22463=CARTESIAN_POINT('Ctrl Pts',(6.18064128844554,-3.3155110916146,2.61680365300887));
#22464=CARTESIAN_POINT('Ctrl Pts',(6.26500512287398,-3.14759231363638,2.62533415026594));
#22465=CARTESIAN_POINT('Ctrl Pts',(6.34936982064302,-2.97967181725478,2.63386473482019));
#22466=CARTESIAN_POINT('Ctrl Pts',(6.42697500341061,-2.80836648587293,2.64239531937444));
#22467=CARTESIAN_POINT('Ctrl Pts',(6.49756912197041,-2.63424032079776,2.65092590392869));
#22468=CARTESIAN_POINT('Ctrl Pts',(6.56817720947545,-2.46007970017709,2.65945817648856));
#22469=CARTESIAN_POINT('Ctrl Pts',(6.6317713478514,-2.28309741497011,2.66799044904842));
#22470=CARTESIAN_POINT('Ctrl Pts',(6.68814843916256,-2.10387666421478,2.67652272160829));
#22471=CARTESIAN_POINT('Ctrl Pts',(6.69542703179458,-2.08073827935638,2.67762428493382));
#22472=CARTESIAN_POINT('Ctrl Pts',(6.70258539665775,-2.05756260550653,2.67872584825936));
#22473=CARTESIAN_POINT('Ctrl Pts',(6.70962315709093,-2.03435091671253,2.67982741158489));
#22474=CARTESIAN_POINT('Ctrl Pts',(6.76413540495461,-1.85456057788433,2.68835976979873));
#22475=CARTESIAN_POINT('Ctrl Pts',(6.81142621627836,-1.6725476317491,2.69689212801257));
#22476=CARTESIAN_POINT('Ctrl Pts',(6.85133412022972,-1.48890810175647,2.70542448622642));
#22477=CARTESIAN_POINT('Ctrl Pts',(6.89123455127736,-1.30530295895008,2.71395524672439));
#22478=CARTESIAN_POINT('Ctrl Pts',(6.92375476891662,-1.12007213900288,2.72248600722237));
#22479=CARTESIAN_POINT('Ctrl Pts',(6.94878412279961,-0.933823204481489,
2.73101676772034));
#22480=CARTESIAN_POINT('Ctrl Pts',(6.97489185930863,-0.739549787344818,
2.73991507361924));
#22481=CARTESIAN_POINT('Ctrl Pts',(6.99284888010694,-0.544168928206322,
2.74881337951815));
#22482=CARTESIAN_POINT('Ctrl Pts',(7.00258944202674,-0.348378628672426,
2.75771168541705));
#22483=CARTESIAN_POINT('Ctrl Pts',(7.01192738092019,-0.160681258845915,
2.76624218267413));
#22484=CARTESIAN_POINT('Ctrl Pts',(7.01371443746118,0.0273920573483055,
2.7747726799312));
#22485=CARTESIAN_POINT('Ctrl Pts',(7.00794587276197,0.215223620772818,2.78330317718828));
#22486=CARTESIAN_POINT('Ctrl Pts',(7.0021772490299,0.40305710637946,2.79183376174255));
#22487=CARTESIAN_POINT('Ctrl Pts',(6.98885286217811,0.590648528537988,2.80036434629683));
#22488=CARTESIAN_POINT('Ctrl Pts',(6.96802005994193,0.777382149748008,2.8088949308511));
#22489=CARTESIAN_POINT('Ctrl Pts',(6.94718313537557,0.964152721226848,2.81742720341094));
#22490=CARTESIAN_POINT('Ctrl Pts',(6.91883486290099,1.15006484875056,2.82595947597079));
#22491=CARTESIAN_POINT('Ctrl Pts',(6.88307433754139,1.3345089832516,2.83449174853063));
#22492=CARTESIAN_POINT('Ctrl Pts',(6.87845745699039,1.35832173568631,2.83559331185615));
#22493=CARTESIAN_POINT('Ctrl Pts',(6.8737170973787,1.3821100318977,2.83669487518166));
#22494=CARTESIAN_POINT('Ctrl Pts',(6.86885353412558,1.405872572188,2.83779643850718));
#22495=CARTESIAN_POINT('Ctrl Pts',(6.83118192423267,1.58992963103396,2.846328796721));
#22496=CARTESIAN_POINT('Ctrl Pts',(6.78610175245774,1.77250266165203,2.85486115493483));
#22497=CARTESIAN_POINT('Ctrl Pts',(6.73375482552113,1.95299065852117,2.86339351314865));
#22498=CARTESIAN_POINT('Ctrl Pts',(6.68141770074137,2.13344485834129,2.87192427364665));
#22499=CARTESIAN_POINT('Ctrl Pts',(6.62181662150668,2.31181450981782,2.88045503414464));
#22500=CARTESIAN_POINT('Ctrl Pts',(6.55514357855421,2.48751265866919,2.88898579464264));
#22501=CARTESIAN_POINT('Ctrl Pts',(6.48559794642201,2.67078071252176,2.89788410054154));
#22502=CARTESIAN_POINT('Ctrl Pts',(6.40835756792077,2.8511416247024,2.90678240644045));
#22503=CARTESIAN_POINT('Ctrl Pts',(6.32369698627195,3.02795029488846,2.91568071233935));
#22504=CARTESIAN_POINT('Ctrl Pts',(6.24253582281654,3.19745063497386,2.92421120959642));
#22505=CARTESIAN_POINT('Ctrl Pts',(6.15455568761851,3.36368619568767,2.93274170685348));
#22506=CARTESIAN_POINT('Ctrl Pts',(6.06004653255181,3.52611153904792,2.94127220411055));
#22507=CARTESIAN_POINT('Ctrl Pts',(5.96553641032296,3.68853854459256,2.94980278866471));
#22508=CARTESIAN_POINT('Ctrl Pts',(5.86449729139241,3.84715499202844,2.95833337321886));
#22509=CARTESIAN_POINT('Ctrl Pts',(5.75726399662617,4.00144196954698,2.96686395777301));
#22510=CARTESIAN_POINT('Ctrl Pts',(5.65000948286777,4.15575947689467,2.97539623033281));
#22511=CARTESIAN_POINT('Ctrl Pts',(5.53655852069095,4.30574555255997,2.98392850289261));
#22512=CARTESIAN_POINT('Ctrl Pts',(5.41728848895509,4.45091136621869,2.99246077545241));
#22513=CARTESIAN_POINT('Ctrl Pts',(5.40189007172301,4.46965307135633,2.9935623387781));
#22514=CARTESIAN_POINT('Ctrl Pts',(5.38639471651263,4.488314475724,2.99466390210378));
#22515=CARTESIAN_POINT('Ctrl Pts',(5.37080328437187,4.50689456755762,2.99576546542947));
#22516=CARTESIAN_POINT('Ctrl Pts',(5.25003702337753,4.65081003339936,3.0042978236433));
#22517=CARTESIAN_POINT('Ctrl Pts',(5.12346257375957,4.78989289395479,3.01283018185713));
#22518=CARTESIAN_POINT('Ctrl Pts',(4.99149080541615,4.92368216906271,3.02136254007096));
#22519=CARTESIAN_POINT('Ctrl Pts',(4.85954374927805,5.05744639163039,3.02989330056892));
#22520=CARTESIAN_POINT('Ctrl Pts',(4.72220160612443,5.18591878916185,3.03842406106688));
#22521=CARTESIAN_POINT('Ctrl Pts',(4.57991268526853,5.3086746328831,3.04695482156484));
#22522=CARTESIAN_POINT('Ctrl Pts',(4.43149328654036,5.43671937737818,3.05585312746375));
#22523=CARTESIAN_POINT('Ctrl Pts',(4.27769165846373,5.5585438162839,3.06475143336266));
#22524=CARTESIAN_POINT('Ctrl Pts',(4.11905639031389,5.67371139695299,3.07364973926157));
#22525=CARTESIAN_POINT('Ctrl Pts',(3.96697826047658,5.78411856233504,3.08218023651864));
#22526=CARTESIAN_POINT('Ctrl Pts',(3.8104583149186,5.8884079312939,3.09071073377571));
#22527=CARTESIAN_POINT('Ctrl Pts',(3.65001123822204,5.98623792739253,3.09924123103278));
#22528=CARTESIAN_POINT('Ctrl Pts',(3.48956251958513,6.0840689246376,3.10777181558697));
#22529=CARTESIAN_POINT('Ctrl Pts',(3.32518685243327,6.17544026040601,3.11630240014116));
#22530=CARTESIAN_POINT('Ctrl Pts',(3.15742574695669,6.26005504887577,3.12483298469535));
#22531=CARTESIAN_POINT('Ctrl Pts',(2.98963144543196,6.3446865806579,3.13336525725519));
#22532=CARTESIAN_POINT('Ctrl Pts',(2.81845064125773,6.42255875794218,3.14189752981504));
#22533=CARTESIAN_POINT('Ctrl Pts',(2.6444479451557,6.49342141154121,3.15042980237489));
#22534=CARTESIAN_POINT('Ctrl Pts',(2.62198323985695,6.50257016995387,3.15153136570051));
#22535=CARTESIAN_POINT('Ctrl Pts',(2.59947152634468,6.5116021575947,3.15263292902614));
#22536=CARTESIAN_POINT('Ctrl Pts',(2.5769140435464,6.52051689474641,3.15373449235176));
#22537=CARTESIAN_POINT('Ctrl Pts',(2.40219097573927,6.5895676056688,3.16226685056557));
#22538=CARTESIAN_POINT('Ctrl Pts',(2.22466146157776,6.65160311967304,3.17079920877938));
#22539=CARTESIAN_POINT('Ctrl Pts',(2.0449063016234,6.70641370481131,3.17933156699318));
#22540=CARTESIAN_POINT('Ctrl Pts',(1.86518480149153,6.76121402646358,3.18786232749117));
#22541=CARTESIAN_POINT('Ctrl Pts',(1.68323877982464,6.8087920299243,3.19639308798916));
#22542=CARTESIAN_POINT('Ctrl Pts',(1.49966469881372,6.84898768823773,3.20492384848714));
#22543=CARTESIAN_POINT('Ctrl Pts',(1.30818138049391,6.89091516510983,3.21382215438605));
#22544=CARTESIAN_POINT('Ctrl Pts',(1.11492694565757,6.9248099748863,3.22272046028496));
#22545=CARTESIAN_POINT('Ctrl Pts',(0.92059166891686,6.95054944170753,3.23161876618387));
#22546=CARTESIAN_POINT('Ctrl Pts',(0.734289178979928,6.97522497586103,3.24014926344093));
#22547=CARTESIAN_POINT('Ctrl Pts',(0.546993727132722,6.99240576608184,3.248679760698));
#22548=CARTESIAN_POINT('Ctrl Pts',(0.359320550293526,7.00203651123277,3.25721025795506));
#22549=CARTESIAN_POINT('Ctrl Pts',(0.171645452895992,7.01166735494018,3.26574084250919));
#22550=CARTESIAN_POINT('Ctrl Pts',(-0.0164070714756707,7.01374798673602,
3.27427142706331));
#22551=CARTESIAN_POINT('Ctrl Pts',(-0.204219476019748,7.00827517782473,
3.28280201161744));
#22552=CARTESIAN_POINT('Ctrl Pts',(-0.392069044302411,7.00280128597091,
3.2913342841773));
#22553=CARTESIAN_POINT('Ctrl Pts',(-0.579678092029639,6.98977097808267,
3.29986655673715));
#22554=CARTESIAN_POINT('Ctrl Pts',(-0.766431002904122,6.96923310560692,
3.30839882929701));
#22555=CARTESIAN_POINT('Ctrl Pts',(-0.790541831073335,6.96658155328623,
3.30950039262269));
#22556=CARTESIAN_POINT('Ctrl Pts',(-0.81463839579834,6.96380493402564,3.31060195594837));
#22557=CARTESIAN_POINT('Ctrl Pts',(-0.838719379193902,6.9609034158983,3.31170351927405));
#22558=CARTESIAN_POINT('Ctrl Pts',(-1.02524299674915,6.93842918182638,3.32023587748788));
#22559=CARTESIAN_POINT('Ctrl Pts',(-1.21089419386651,6.90844974878836,3.32876823570171));
#22560=CARTESIAN_POINT('Ctrl Pts',(-1.39506237180662,6.87105723606413,3.33730059391554));
#22561=CARTESIAN_POINT('Ctrl Pts',(-1.57919606356934,6.83367172522721,3.34583135441351));
#22562=CARTESIAN_POINT('Ctrl Pts',(-1.76184699060401,6.78887596575204,3.35436211491148));
#22563=CARTESIAN_POINT('Ctrl Pts',(-1.94241444908253,6.73681324295808,3.36289287540945));
#22564=CARTESIAN_POINT('Ctrl Pts',(-2.13076160538968,6.68250741249187,3.37179118130836));
#22565=CARTESIAN_POINT('Ctrl Pts',(-2.31684143976208,6.6202946328271,3.38068948720727));
#22566=CARTESIAN_POINT('Ctrl Pts',(-2.49998853805577,6.55039570347393,3.38958779310617));
#22567=CARTESIAN_POINT('Ctrl Pts',(-2.6755653093409,6.48338602411535,3.39811829036326));
#22568=CARTESIAN_POINT('Ctrl Pts',(-2.84844661213151,6.40931294546411,3.40664878762034));
#22569=CARTESIAN_POINT('Ctrl Pts',(-3.01806509828058,6.32842078444857,3.41517928487743));
#22570=CARTESIAN_POINT('Ctrl Pts',(-3.18768532022673,6.2475277956201,3.42370986943168));
#22571=CARTESIAN_POINT('Ctrl Pts',(-3.35404238402338,6.15981571961481,3.43224045398592));
#22572=CARTESIAN_POINT('Ctrl Pts',(-3.51659170468122,6.0655757636903,3.44077103854017));
#22573=CARTESIAN_POINT('Ctrl Pts',(-3.67917319009338,5.97131715985625,3.44930331109997));
#22574=CARTESIAN_POINT('Ctrl Pts',(-3.83794516327184,5.87052825051918,3.45783558365977));
#22575=CARTESIAN_POINT('Ctrl Pts',(-3.9923895349857,5.76354512114173,3.46636785621957));
#22576=CARTESIAN_POINT('Ctrl Pts',(-4.01232915301025,5.74973301059873,3.46746941954516));
#22577=CARTESIAN_POINT('Ctrl Pts',(-4.0321966773412,5.73581771243711,3.46857098287075));
#22578=CARTESIAN_POINT('Ctrl Pts',(-4.05199102910796,5.72180000196867,3.46967254619634));
#22579=CARTESIAN_POINT('Ctrl Pts',(-4.20531176515773,5.61322328715232,3.47820490441019));
#22580=CARTESIAN_POINT('Ctrl Pts',(-4.35429170696321,5.49846218600666,3.48673726262403));
#22581=CARTESIAN_POINT('Ctrl Pts',(-4.49843777963941,5.37788844298698,3.49526962083788));
#22582=CARTESIAN_POINT('Ctrl Pts',(-4.64255686042606,5.25733727785022,3.50380038133584));
#22583=CARTESIAN_POINT('Ctrl Pts',(-4.78184364384754,5.13097583920066,3.5123311418338));
#22584=CARTESIAN_POINT('Ctrl Pts',(-4.91583811907906,4.9992161535094,3.52086190233176));
#22585=CARTESIAN_POINT('Ctrl Pts',(-5.05560570834129,4.86177963906208,3.52976020823066));
#22586=CARTESIAN_POINT('Ctrl Pts',(-5.18961458465397,4.71846964016777,3.53865851412957));
#22587=CARTESIAN_POINT('Ctrl Pts',(-5.31738474194418,4.56979715836921,3.54755682002847));
#22588=CARTESIAN_POINT('Ctrl Pts',(-5.43987356045443,4.42727000628055,3.55608731728555));
#22589=CARTESIAN_POINT('Ctrl Pts',(-5.55662882843779,4.27981501913708,3.56461781454262));
#22590=CARTESIAN_POINT('Ctrl Pts',(-5.66726797327666,4.12791718443728,3.57314831179969));
#22591=CARTESIAN_POINT('Ctrl Pts',(-5.77790825034554,3.97601779528509,3.58167889635394));
#22592=CARTESIAN_POINT('Ctrl Pts',(-5.88243210166907,3.81967571695454,3.59020948090819));
#22593=CARTESIAN_POINT('Ctrl Pts',(-5.98049929865436,3.65940633181049,3.59874006546243));
#22594=CARTESIAN_POINT('Ctrl Pts',(-6.07858590087249,3.4991052330575,3.6072723380223));
#22595=CARTESIAN_POINT('Ctrl Pts',(-6.17021313812817,3.33487553688238,3.61580461058217));
#22596=CARTESIAN_POINT('Ctrl Pts',(-6.25508545008453,3.16725947384184,3.62433688314204));
#22597=CARTESIAN_POINT('Ctrl Pts',(-6.26604293246077,3.14561931800767,3.62543844646756));
#22598=CARTESIAN_POINT('Ctrl Pts',(-6.27688788527885,3.12392275043866,3.62654000979309));
#22599=CARTESIAN_POINT('Ctrl Pts',(-6.28761972898703,3.1021709666221,3.62764157311862));
#22600=CARTESIAN_POINT('Ctrl Pts',(-6.37051092536119,2.93416335927575,3.63614988766531));
#22601=CARTESIAN_POINT('Ctrl Pts',(-6.44667990653279,2.76280004359039,3.644658202212));
#22602=CARTESIAN_POINT('Ctrl Pts',(-6.51587084808528,2.58863934405171,3.65316651675868));
#22603=CARTESIAN_POINT('Ctrl Pts',(-6.58504816965121,2.41451292741672,3.66167315647443));
#22604=CARTESIAN_POINT('Ctrl Pts',(-6.64725007839304,2.2375905132263,3.67017979619017));
#22605=CARTESIAN_POINT('Ctrl Pts',(-6.70226898252104,2.05845015689872,3.67868643590592));
#22606=CARTESIAN_POINT('Ctrl Pts',(-6.75728864378276,1.87930733536022,3.68719319268441));
#22607=CARTESIAN_POINT('Ctrl Pts',(-6.80512500802915,1.69794680530732,3.69569994946289));
#22608=CARTESIAN_POINT('Ctrl Pts',(-6.84562017724716,1.51496235971942,3.70420670624138));
#22609=CARTESIAN_POINT('Ctrl Pts',(-6.88611314149592,1.33198787766744,3.71271299982543));
#22610=CARTESIAN_POINT('Ctrl Pts',(-6.91926564402742,1.14738995929416,3.72121929340949));
#22611=CARTESIAN_POINT('Ctrl Pts',(-6.94497071526182,0.961773531896027,
3.72972558699354));
#22612=CARTESIAN_POINT('Ctrl Pts',(-6.97068151815061,0.776115716197457,
3.73823377729029));
#22613=CARTESIAN_POINT('Ctrl Pts',(-6.98894152821702,0.589439244279225,
3.74674196758704));
#22614=CARTESIAN_POINT('Ctrl Pts',(-6.99969543066941,0.402356111381252,
3.75525015788378));
#22615=CARTESIAN_POINT('Ctrl Pts',(-7.00739885007534,0.26834152059714,3.76134489033384));
#22616=CARTESIAN_POINT('Ctrl Pts',(-7.01125167442655,0.1341184071921,3.7674396227839));
#22617=CARTESIAN_POINT('Ctrl Pts',(-7.01124999945394,-8.75047268976489E-5,
3.77353435523396));
#22618=CARTESIAN_POINT('Ctrl Pts',(-7.01174696422417,-8.75478460599835E-5,
3.77353435691035));
#22619=CARTESIAN_POINT('Ctrl Pts',(-7.01180261336239,-0.0887333921737332,
3.77755977128721));
#22620=CARTESIAN_POINT('Ctrl Pts',(-6.99636440224467,-0.919874595891691,
3.81530283634042));
#22621=CARTESIAN_POINT('Ctrl Pts',(-6.83009966285127,-1.7452908997936,3.85304590139378));
#22622=CARTESIAN_POINT('Ctrl Pts',(-6.57188903190969,-2.44175767753665,
3.88676355207028));
#22623=CARTESIAN_POINT('',(-7.01086833367197,0.000109686007034688,3.2264656355206));
#22624=CARTESIAN_POINT('Ctrl Pts',(-6.5722715952584,-2.44189939200197,3.33970491700474));
#22625=CARTESIAN_POINT('Ctrl Pts',(-6.61499340131524,-2.32691541134939,
3.33413514849053));
#22626=CARTESIAN_POINT('Ctrl Pts',(-6.6546932255011,-2.21082002405903,3.32856537997633));
#22627=CARTESIAN_POINT('Ctrl Pts',(-6.69131729331829,-2.0937763592704,3.32299561146213));
#22628=CARTESIAN_POINT('Ctrl Pts',(-6.74759831376839,-1.91391275361073,
3.31443642417538));
#22629=CARTESIAN_POINT('Ctrl Pts',(-6.79663212228337,-1.73174958693402,
3.30587723688862));
#22630=CARTESIAN_POINT('Ctrl Pts',(-6.83825110391958,-1.54788513858188,
3.29731804960187));
#22631=CARTESIAN_POINT('Ctrl Pts',(-6.87986114213862,-1.36406020048205,
3.28876070158123));
#22632=CARTESIAN_POINT('Ctrl Pts',(-6.91405946739486,-1.17853500489088,
3.28020335356059));
#22633=CARTESIAN_POINT('Ctrl Pts',(-6.94072919079019,-0.991919786380446,
3.27164600553994));
#22634=CARTESIAN_POINT('Ctrl Pts',(-6.96739714357071,-0.805316957337377,
3.26308922564544));
#22635=CARTESIAN_POINT('Ctrl Pts',(-6.98653744714038,-0.617624548411278,
3.25453244575094));
#22636=CARTESIAN_POINT('Ctrl Pts',(-6.99808475054815,-0.429460576357655,
3.24597566585644));
#22637=CARTESIAN_POINT('Ctrl Pts',(-7.0068609551157,-0.286451819016622,
3.23947232493417));
#22638=CARTESIAN_POINT('Ctrl Pts',(-7.01125223737829,-0.143170865468828,
3.2329689840119));
#22639=CARTESIAN_POINT('Ctrl Pts',(-7.01124999914453,0.00010952522091514,
3.22646564308963));
#22640=CARTESIAN_POINT('Ctrl Pts',(-7.01077666039611,0.000109724626693396,
3.22646563370257));
#22641=CARTESIAN_POINT('Ctrl Pts',(-7.01102961718175,0.451283813389737,
3.20598595064833));
#22642=CARTESIAN_POINT('Ctrl Pts',(-6.85785257182463,2.06232469578677,3.13284992528664));
#22643=CARTESIAN_POINT('Ctrl Pts',(-5.63772386156061,4.64629944776454,3.00705755761756));
#22644=CARTESIAN_POINT('Ctrl Pts',(-2.74525602695119,6.77019927653496,2.84908853069525));
#22645=CARTESIAN_POINT('Ctrl Pts',(0.809572652366525,7.26062125565349,2.69111950377297));
#22646=CARTESIAN_POINT('Ctrl Pts',(4.16907192684548,5.9992389655935,2.53315047685068));
#22647=CARTESIAN_POINT('Ctrl Pts',(6.52267959194278,3.29039204933995,2.37518144992839));
#22648=CARTESIAN_POINT('Ctrl Pts',(7.30252964686993,-0.212343245930207,
2.2172124230061));
#22649=CARTESIAN_POINT('Ctrl Pts',(6.32046399778932,-3.66384548666503,2.05924339608381));
#22650=CARTESIAN_POINT('Ctrl Pts',(3.81343024685451,-6.23135447955594,1.90127436916152));
#22651=CARTESIAN_POINT('Ctrl Pts',(0.386312228825965,-7.29539524353313,
1.74330534223923));
#22652=CARTESIAN_POINT('Ctrl Pts',(-3.13401315918718,-6.59924165458034,
1.58533631531694));
#22653=CARTESIAN_POINT('Ctrl Pts',(-5.48811015356693,-4.65034471123624,
1.45080234040949));
#22654=CARTESIAN_POINT('Ctrl Pts',(-6.34735191580087,-3.04510780294658,
1.36892470780946));
#22655=CARTESIAN_POINT('Ctrl Pts',(-6.57174751820247,-2.44170444323764,
1.33970341751688));
#22656=CARTESIAN_POINT('Origin',(0.,0.,0.));
#22657=CARTESIAN_POINT('',(-6.5722715952584,-2.44189939200198,-0.660303821598748));
#22658=CARTESIAN_POINT('',(-6.57227163891168,-2.44189927451098,-0.113051811211838));
#22659=CARTESIAN_POINT('',(-6.57227159525839,-2.441899392002,0.));
#22660=CARTESIAN_POINT('',(-7.01124999779487,0.000175845004380833,1.77353435691035));
#22661=CARTESIAN_POINT('Ctrl Pts',(-6.57227163891168,-2.44189927451098,
-0.113051811211839));
#22662=CARTESIAN_POINT('Ctrl Pts',(-6.51379048013646,-2.59929891226057,
-0.105346661399166));
#22663=CARTESIAN_POINT('Ctrl Pts',(-6.44965919248067,-2.75458629304454,
-0.0976675531015183));
#22664=CARTESIAN_POINT('Ctrl Pts',(-6.30177438124679,-3.07909809577218,
-0.0814412978830712));
#22665=CARTESIAN_POINT('Ctrl Pts',(-6.21665974009033,-3.24751422428018,
-0.0729127710991782));
#22666=CARTESIAN_POINT('Ctrl Pts',(-6.01680152855583,-3.60624728191609,
-0.0544264990385142));
#22667=CARTESIAN_POINT('Ctrl Pts',(-5.89959433231979,-3.79495816685282,
-0.0444946513980189));
#22668=CARTESIAN_POINT('Ctrl Pts',(-5.67134537880492,-4.12625400191001,
-0.0264653376106269));
#22669=CARTESIAN_POINT('Ctrl Pts',(-5.5633724974678,-4.27071604468818,-0.0183795479634319));
#22670=CARTESIAN_POINT('Ctrl Pts',(-5.38196222462781,-4.49486255913974,
-0.00532741689756344));
#22671=CARTESIAN_POINT('Ctrl Pts',(-5.31203897582476,-4.57728609272316,
-0.000405389684517453));
#22672=CARTESIAN_POINT('Ctrl Pts',(-5.04791538435022,-4.87442074824541,
0.0177810171590431));
#22673=CARTESIAN_POINT('Ctrl Pts',(-4.84237642232889,-5.07866300543721,
0.0311369266982347));
#22674=CARTESIAN_POINT('Ctrl Pts',(-4.46558505942067,-5.4093486242146,0.0541445575416953));
#22675=CARTESIAN_POINT('Ctrl Pts',(-4.30011501631266,-5.54179713015967,
0.0638205079324956));
#22676=CARTESIAN_POINT('Ctrl Pts',(-3.95709046738012,-5.79174002262208,
0.0830855683209048));
#22677=CARTESIAN_POINT('Ctrl Pts',(-3.77967410863643,-5.90905094017359,
0.0926643195028018));
#22678=CARTESIAN_POINT('Ctrl Pts',(-3.36346120301389,-6.15783313652653,
0.114435063300481));
#22679=CARTESIAN_POINT('Ctrl Pts',(-3.12178243662828,-6.2838088051756,0.126583180726194));
#22680=CARTESIAN_POINT('Ctrl Pts',(-2.76799658910346,-6.4427612088298,0.144043701559189));
#22681=CARTESIAN_POINT('Ctrl Pts',(-2.6614484738719,-6.48750097104497,0.149264869801388));
#22682=CARTESIAN_POINT('Ctrl Pts',(-2.35034634210553,-6.6091787839831,0.164467345759501));
#22683=CARTESIAN_POINT('Ctrl Pts',(-2.14324232001506,-6.6792127271797,0.174516156026655));
#22684=CARTESIAN_POINT('Ctrl Pts',(-1.6426784502937,-6.82279909339829,0.198472689701524));
#22685=CARTESIAN_POINT('Ctrl Pts',(-1.34705857149823,-6.88726492567702,
0.212349851066077));
#22686=CARTESIAN_POINT('Ctrl Pts',(-0.861236024399551,-6.96072221549327,
0.234704280016186));
#22687=CARTESIAN_POINT('Ctrl Pts',(-0.673203222455418,-6.98141677634236,
0.243252959396741));
#22688=CARTESIAN_POINT('Ctrl Pts',(-0.261265577008079,-7.00995488939356,
0.261840069161537));
#22689=CARTESIAN_POINT('Ctrl Pts',(-0.0373558298317422,-7.01472254986739,
0.271851739318829));
#22690=CARTESIAN_POINT('Ctrl Pts',(0.367065798118773,-7.00396695262904,
0.289983082135156));
#22691=CARTESIAN_POINT('Ctrl Pts',(0.547477948887577,-6.99217825859279,
0.298090263095312));
#22692=CARTESIAN_POINT('Ctrl Pts',(0.836614686634072,-6.96202538606241,
0.311253950360317));
#22693=CARTESIAN_POINT('Ctrl Pts',(0.945713287992123,-6.94804628486296,
0.316265662383899));
#22694=CARTESIAN_POINT('Ctrl Pts',(1.12922444502119,-6.92013015898074,0.324760691432349));
#22695=CARTESIAN_POINT('Ctrl Pts',(1.203823279825,-6.90754360712728,0.328231581556242));
#22696=CARTESIAN_POINT('Ctrl Pts',(1.68318192553285,-6.81866343687492,0.35062969928556));
#22697=CARTESIAN_POINT('Ctrl Pts',(2.08076607353137,-6.70803228930215,0.369588048055639));
#22698=CARTESIAN_POINT('Ctrl Pts',(2.65884688568928,-6.49079760841058,0.397632534543466));
#22699=CARTESIAN_POINT('Ctrl Pts',(2.84808301716799,-6.4100191331999,0.406906207846296));
#22700=CARTESIAN_POINT('Ctrl Pts',(3.1655757366444,-6.25765287957744,0.422725912084332));
#22701=CARTESIAN_POINT('Ctrl Pts',(3.29563640355392,-6.19014298728567,0.429286249465989));
#22702=CARTESIAN_POINT('Ctrl Pts',(3.61664409924359,-6.01053259762188,0.445766322371894));
#22703=CARTESIAN_POINT('Ctrl Pts',(3.80457288852243,-5.89337247774327,0.455678894857876));
#22704=CARTESIAN_POINT('Ctrl Pts',(4.08340943689875,-5.70063433761663,0.471045311444189));
#22705=CARTESIAN_POINT('Ctrl Pts',(4.17847651131669,-5.63132290016994,0.476414920780977));
#22706=CARTESIAN_POINT('Ctrl Pts',(4.41122355758142,-5.4524919920581,0.489863841851319));
#22707=CARTESIAN_POINT('Ctrl Pts',(4.54661161064246,-5.34012028570029,0.497960924407617));
#22708=CARTESIAN_POINT('Ctrl Pts',(4.86843309564754,-5.05189013463151,0.517831691158166));
#22709=CARTESIAN_POINT('Ctrl Pts',(5.0497304775803,-4.87067346811471,0.529577494975458));
#22710=CARTESIAN_POINT('Ctrl Pts',(5.34566795837694,-4.54054057475343,0.549755745055887));
#22711=CARTESIAN_POINT('Ctrl Pts',(5.46499738837264,-4.39618922258884,0.558223296853779));
#22712=CARTESIAN_POINT('Ctrl Pts',(5.70953561679692,-4.07500749496314,0.57640095972916));
#22713=CARTESIAN_POINT('Ctrl Pts',(5.83261775805606,-3.89680046723166,0.586087800144649));
#22714=CARTESIAN_POINT('Ctrl Pts',(6.05218242189192,-3.5451325863076,0.604664271504848));
#22715=CARTESIAN_POINT('Ctrl Pts',(6.14993486925177,-3.37271053492856,0.613544313471033));
#22716=CARTESIAN_POINT('Ctrl Pts',(6.29096259082812,-3.09738414210479,0.627555224997623));
#22717=CARTESIAN_POINT('Ctrl Pts',(6.33930794442124,-2.99719415308173,0.632625771398413));
#22718=CARTESIAN_POINT('Ctrl Pts',(6.41744039454165,-2.82491767512174,0.641285071597625));
#22719=CARTESIAN_POINT('Ctrl Pts',(6.44844618251633,-2.75340567747632,0.644861937113561));
#22720=CARTESIAN_POINT('Ctrl Pts',(6.63094349624851,-2.31249147471794,0.66678915431235));
#22721=CARTESIAN_POINT('Ctrl Pts',(6.75184801516868,-1.93121408346769,0.685163578727264));
#22722=CARTESIAN_POINT('Ctrl Pts',(6.88379637084582,-1.34584247504007,0.712424849648115));
#22723=CARTESIAN_POINT('Ctrl Pts',(6.9195147439769,-1.14815585810827,0.721484840716629));
#22724=CARTESIAN_POINT('Ctrl Pts',(6.98320203995558,-0.68206527646686,0.742626730668839));
#22725=CARTESIAN_POINT('Ctrl Pts',(7.00426442178689,-0.413041210143523,
0.754658315309748));
#22726=CARTESIAN_POINT('Ctrl Pts',(7.01246849324306,-0.0122125706970769,
0.772675701945629));
#22727=CARTESIAN_POINT('Ctrl Pts',(7.01146764743179,0.119097956915563,0.778594530890423));
#22728=CARTESIAN_POINT('Ctrl Pts',(7.00129066234927,0.403986015878096,0.791548813195998));
#22729=CARTESIAN_POINT('Ctrl Pts',(6.99074586380984,0.557446758404484,0.798594980744528));
#22730=CARTESIAN_POINT('Ctrl Pts',(6.93347914745049,1.11970085952642,0.824560061699123));
#22731=CARTESIAN_POINT('Ctrl Pts',(6.85585374680587,1.52451456157718,0.843495300485487));
#22732=CARTESIAN_POINT('Ctrl Pts',(6.68689510407699,2.11785316136084,0.871511712397881));
#22733=CARTESIAN_POINT('Ctrl Pts',(6.62194192000074,2.31295377337637,0.880779799361355));
#22734=CARTESIAN_POINT('Ctrl Pts',(6.41650278036058,2.85002486111788,0.906611143946151));
#22735=CARTESIAN_POINT('Ctrl Pts',(6.25742302352168,3.18414795801925,0.923033593896662));
#22736=CARTESIAN_POINT('Ctrl Pts',(6.01338813118964,3.60706274953789,0.945171474088692));
#22737=CARTESIAN_POINT('Ctrl Pts',(5.95141153384286,3.708428012476,0.950595039809579));
#22738=CARTESIAN_POINT('Ctrl Pts',(5.78917250790118,3.95922666655062,0.964283414428022));
#22739=CARTESIAN_POINT('Ctrl Pts',(5.68567649769621,4.10646764394342,0.972566799975525));
#22740=CARTESIAN_POINT('Ctrl Pts',(5.42543518029854,4.44797801056314,0.992313632627998));
#22741=CARTESIAN_POINT('Ctrl Pts',(5.263754551808,4.63818350970906,1.00375063794982));
#22742=CARTESIAN_POINT('Ctrl Pts',(4.96365066537529,4.95528166754589,1.0236213095988));
#22743=CARTESIAN_POINT('Ctrl Pts',(4.82963075185957,5.08599180451281,1.03208537602857));
#22744=CARTESIAN_POINT('Ctrl Pts',(4.52989208273937,5.35578390390235,1.0502451856365));
#22745=CARTESIAN_POINT('Ctrl Pts',(4.3626420268057,5.49287709725563,1.05991780976532));
#22746=CARTESIAN_POINT('Ctrl Pts',(4.02960451979685,5.7410443712721,1.07852773008465));
#22747=CARTESIAN_POINT('Ctrl Pts',(3.86488519773559,5.85320113806293,1.0874554928949));
#22748=CARTESIAN_POINT('Ctrl Pts',(3.60089399270991,6.01694385573736,1.10152611333106));
#22749=CARTESIAN_POINT('Ctrl Pts',(3.50478513799313,6.07342829086807,1.10660761948416));
#22750=CARTESIAN_POINT('Ctrl Pts',(3.33888889818418,6.16567819833357,1.11529721067078));
#22751=CARTESIAN_POINT('Ctrl Pts',(3.26977229165828,6.2026087886183,1.1188935011329));
#22752=CARTESIAN_POINT('Ctrl Pts',(2.84252173647579,6.42177231072161,1.14095893728608));
#22753=CARTESIAN_POINT('Ctrl Pts',(2.46987885139551,6.57410063911161,1.15944994906116));
#22754=CARTESIAN_POINT('Ctrl Pts',(1.89218828862413,6.75415167548213,1.18693426548889));
#22755=CARTESIAN_POINT('Ctrl Pts',(1.69559462082048,6.80616647034856,1.1961026518323));
#22756=CARTESIAN_POINT('Ctrl Pts',(1.22384362942314,6.90927070632869,1.2177994944551));
#22757=CARTESIAN_POINT('Ctrl Pts',(0.947344419517943,6.95257882587064,1.23027198563359));
#22758=CARTESIAN_POINT('Ctrl Pts',(0.548737309762689,6.99078751274997,1.24828400048376));
#22759=CARTESIAN_POINT('Ctrl Pts',(0.428197077049147,6.99920492306276,1.25373700365624));
#22760=CARTESIAN_POINT('Ctrl Pts',(0.133839260142499,7.01212735035969,1.26713460178215));
#22761=CARTESIAN_POINT('Ctrl Pts',(-0.0400437255557122,7.0132901082745,
1.27510979342304));
#22762=CARTESIAN_POINT('Ctrl Pts',(-0.588842850094366,6.99654828430897,
1.30035270897044));
#22763=CARTESIAN_POINT('Ctrl Pts',(-0.962382024109751,6.95501645697339,
1.31760840753119));
#22764=CARTESIAN_POINT('Ctrl Pts',(-1.52562683409449,6.84612769934643,1.34367692070361));
#22765=CARTESIAN_POINT('Ctrl Pts',(-1.71876625190528,6.80020925915605,1.35263330246511));
#22766=CARTESIAN_POINT('Ctrl Pts',(-2.16000731735223,6.67530296431773,1.37324820797228));
#22767=CARTESIAN_POINT('Ctrl Pts',(-2.40617696132,6.59057004050047,1.38486160845223));
#22768=CARTESIAN_POINT('Ctrl Pts',(-2.76869089556182,6.44276560460703,1.40244212312232));
#22769=CARTESIAN_POINT('Ctrl Pts',(-2.88889593140564,6.38976975176113,1.40835606004339));
#22770=CARTESIAN_POINT('Ctrl Pts',(-3.1193879371304,6.28031658599071,1.41993058842503));
#22771=CARTESIAN_POINT('Ctrl Pts',(-3.22980763527441,6.22425089625768,1.42558774449429));
#22772=CARTESIAN_POINT('Ctrl Pts',(-3.51253867514311,6.07114389917868,1.44033016396364));
#22773=CARTESIAN_POINT('Ctrl Pts',(-3.6823338936865,5.96968450062091,1.44943719768248));
#22774=CARTESIAN_POINT('Ctrl Pts',(-4.05289941509658,5.72642434443336,1.46981380593275));
#22775=CARTESIAN_POINT('Ctrl Pts',(-4.25096605565736,5.58096945780786,1.4810564867486));
#22776=CARTESIAN_POINT('Ctrl Pts',(-4.59321746301029,5.3008185832543,1.50115837571214));
#22777=CARTESIAN_POINT('Ctrl Pts',(-4.74013059600811,5.1698634318345,1.51003964146286));
#22778=CARTESIAN_POINT('Ctrl Pts',(-5.06321648100504,4.8565068317316,1.53027673730393));
#22779=CARTESIAN_POINT('Ctrl Pts',(-5.23539368083716,4.67038250404488,1.54159104914307));
#22780=CARTESIAN_POINT('Ctrl Pts',(-5.48939864600899,4.36406113378797,1.55945237351226));
#22781=CARTESIAN_POINT('Ctrl Pts',(-5.57821398391441,4.24994763216309,1.56595770228343));
#22782=CARTESIAN_POINT('Ctrl Pts',(-5.73751506703633,4.03166692716497,1.57821810049252));
#22783=CARTESIAN_POINT('Ctrl Pts',(-5.80884984573459,3.92819040919106,1.58396099058554));
#22784=CARTESIAN_POINT('Ctrl Pts',(-5.98915441136919,3.65098509479588,1.59912627575862));
#22785=CARTESIAN_POINT('Ctrl Pts',(-6.09335180602451,3.47429508306388,1.60857163925835));
#22786=CARTESIAN_POINT('Ctrl Pts',(-6.29312264193406,3.0988312280876,1.6281169753501));
#22787=CARTESIAN_POINT('Ctrl Pts',(-6.38736856202891,2.89959869798888,1.63820181520507));
#22788=CARTESIAN_POINT('Ctrl Pts',(-6.53856613128265,2.53666513588663,1.65608648002703));
#22789=CARTESIAN_POINT('Ctrl Pts',(-6.59912728896108,2.3746657192263,1.66390616530035));
#22790=CARTESIAN_POINT('Ctrl Pts',(-6.76468036029949,1.87636918106151,1.68755680402165));
#22791=CARTESIAN_POINT('Ctrl Pts',(-6.85038059533619,1.53425718069475,1.70323109943137));
#22792=CARTESIAN_POINT('Ctrl Pts',(-6.92785816130958,1.08328913852958,1.72383606851373));
#22793=CARTESIAN_POINT('Ctrl Pts',(-6.94335881845196,0.979031222269562,
1.72859848252526));
#22794=CARTESIAN_POINT('Ctrl Pts',(-6.99295834142992,0.584458581263378,
1.74668492580571));
#22795=CARTESIAN_POINT('Ctrl Pts',(-7.01124254080886,0.292460787846147,
1.76016286206212));
#22796=CARTESIAN_POINT('Ctrl Pts',(-7.01124999771819,0.000178876124116781,
1.77360028780278));
#22797=CARTESIAN_POINT('Ctrl Pts',(-7.01124999779487,0.000175845004380833,
1.77353435691035));
#22798=CARTESIAN_POINT('Ctrl Pts',(-7.01125469776653,-0.187220302170659,
1.78204174915585));
#22799=CARTESIAN_POINT('Ctrl Pts',(-7.00374199053544,-0.374635673529691,
1.79054914140135));
#22800=CARTESIAN_POINT('Ctrl Pts',(-6.98873332011083,-0.561456269777726,
1.79905653364685));
#22801=CARTESIAN_POINT('Ctrl Pts',(-6.97372411902929,-0.748283471383788,
1.80756422668558));
#22802=CARTESIAN_POINT('Ctrl Pts',(-6.95121844661908,-0.934515547269003,
1.81607191972432));
#22803=CARTESIAN_POINT('Ctrl Pts',(-6.92128973059513,-1.11954232955185,
1.82457961276305));
#22804=CARTESIAN_POINT('Ctrl Pts',(-6.89136184031077,-1.30456400690681,
1.83308707107274));
#22805=CARTESIAN_POINT('Ctrl Pts',(-6.85401136725828,-1.48838015211063,
1.84159452938244));
#22806=CARTESIAN_POINT('Ctrl Pts',(-6.80936316069837,-1.67038914873869,
1.85010198769213));
#22807=CARTESIAN_POINT('Ctrl Pts',(-6.76470558146594,-1.85243635318854,
1.85861123191052));
#22808=CARTESIAN_POINT('Ctrl Pts',(-6.71274728206629,-2.03267535073124,
1.86712047612892));
#22809=CARTESIAN_POINT('Ctrl Pts',(-6.65366367649957,-2.2105171889244,1.87562972034732));
#22810=CARTESIAN_POINT('Ctrl Pts',(-6.62788311018922,-2.28811677443237,
1.87934264769356));
#22811=CARTESIAN_POINT('Ctrl Pts',(-6.60074657699216,-2.36526015197544,
1.8830555750398));
#22812=CARTESIAN_POINT('Ctrl Pts',(-6.5722715952584,-2.44189939200199,1.88676850238605));
#22813=CARTESIAN_POINT('',(-7.01124999783523,-0.000174228519746755,1.22646564308963));
#22814=CARTESIAN_POINT('Ctrl Pts',(-6.57174751820247,-2.44170444323764,
1.33970341751688));
#22815=CARTESIAN_POINT('Ctrl Pts',(-6.75170954457185,-1.95778367933175,
1.31626836550204));
#22816=CARTESIAN_POINT('Ctrl Pts',(-6.95635145461453,-1.14674394506303,
1.27852244232832));
#22817=CARTESIAN_POINT('Ctrl Pts',(-7.01140638052565,-0.315405155950845,
1.24077651915461));
#22818=CARTESIAN_POINT('Ctrl Pts',(-7.01110477910546,-0.000174332979431822,
1.22646564799572));
#22819=CARTESIAN_POINT('Ctrl Pts',(-7.01124999783522,-0.000174228519746755,
1.22646564308963));
#22820=CARTESIAN_POINT('Ctrl Pts',(-7.01125465583345,0.187271490041512,
1.21795614517059));
#22821=CARTESIAN_POINT('Ctrl Pts',(-7.00373793128268,0.37473528203682,1.20944664725154));
#22822=CARTESIAN_POINT('Ctrl Pts',(-6.98872154284581,0.561602848161269,
1.2009371493325));
#22823=CARTESIAN_POINT('Ctrl Pts',(-6.9737043785875,0.748480068795355,1.19242721177039));
#22824=CARTESIAN_POINT('Ctrl Pts',(-6.95118679760751,0.934760693715983,
1.18391727420828));
#22825=CARTESIAN_POINT('Ctrl Pts',(-6.92124250286083,1.11983426411806,1.17540733664616));
#22826=CARTESIAN_POINT('Ctrl Pts',(-6.891298882398,1.30490366704444,1.16689759071032));
#22827=CARTESIAN_POINT('Ctrl Pts',(-6.8539289340877,1.48876576509718,1.15838784477448));
#22828=CARTESIAN_POINT('Ctrl Pts',(-6.80925778001219,1.6708186759321,1.14987809883864));
#22829=CARTESIAN_POINT('Ctrl Pts',(-6.76457640959323,1.85291322247357,1.14136640671428));
#22830=CARTESIAN_POINT('Ctrl Pts',(-6.71259057104574,2.03319745495257,1.13285471458992));
#22831=CARTESIAN_POINT('Ctrl Pts',(-6.65347595510241,2.21108215075199,1.12434302246556));
#22832=CARTESIAN_POINT('Ctrl Pts',(-6.62358007377258,2.30104331638169,1.12003842649373));
#22833=CARTESIAN_POINT('Ctrl Pts',(-6.59186172858171,2.39039101146068,1.1157338305219));
#22834=CARTESIAN_POINT('Ctrl Pts',(-6.5583484482587,2.47905066380715,1.11142923455007));
#22835=CARTESIAN_POINT('Ctrl Pts',(-6.49192007391006,2.65478746184447,1.10289687633624));
#22836=CARTESIAN_POINT('Ctrl Pts',(-6.41841290841537,2.82788232028147,1.09436451812241));
#22837=CARTESIAN_POINT('Ctrl Pts',(-6.3380624199563,2.99776438754578,1.08583215990858));
#22838=CARTESIAN_POINT('Ctrl Pts',(-6.25772697742553,3.1676146437601,1.07730139941061));
#22839=CARTESIAN_POINT('Ctrl Pts',(-6.1705508999817,3.33425303289975,1.06877063891265));
#22840=CARTESIAN_POINT('Ctrl Pts',(-6.07681697087871,3.49713054731168,1.06023987841468));
#22841=CARTESIAN_POINT('Ctrl Pts',(-5.97904454197702,3.66702559332035,1.05134157251577));
#22842=CARTESIAN_POINT('Ctrl Pts',(-5.87413681319125,3.83282819629963,1.04244326661686));
#22843=CARTESIAN_POINT('Ctrl Pts',(-5.76246730796888,3.99394505308847,1.03354496071795));
#22844=CARTESIAN_POINT('Ctrl Pts',(-5.6554136261984,4.14840219588844,1.02501446346088));
#22845=CARTESIAN_POINT('Ctrl Pts',(-5.54214610708143,4.29855290334076,1.01648396620381));
#22846=CARTESIAN_POINT('Ctrl Pts',(-5.42303765706886,4.44390471685804,1.00795346894674));
#22847=CARTESIAN_POINT('Ctrl Pts',(-5.30392798815565,4.58925801783836,0.999422884392513));
#22848=CARTESIAN_POINT('Ctrl Pts',(-5.17897746534402,4.72981209213407,0.990892299838288));
#22849=CARTESIAN_POINT('Ctrl Pts',(-5.04859908113031,4.86510779741931,0.982361715284064));
#22850=CARTESIAN_POINT('Ctrl Pts',(-4.91819489804679,5.00043027459859,0.973829442724257));
#22851=CARTESIAN_POINT('Ctrl Pts',(-4.78236092142949,5.13049208493782,0.96529717016445));
#22852=CARTESIAN_POINT('Ctrl Pts',(-4.64154738344617,5.25487054547722,0.956764897604643));
#22853=CARTESIAN_POINT('Ctrl Pts',(-4.62336758104229,5.27092848896965,0.955663334279022));
#22854=CARTESIAN_POINT('Ctrl Pts',(-4.60510482600696,5.28689175381491,0.954561770953402));
#22855=CARTESIAN_POINT('Ctrl Pts',(-4.58676012916224,5.30275947785939,0.953460207627781));
#22856=CARTESIAN_POINT('Ctrl Pts',(-4.44466795782465,5.42566580783316,0.944927849413946));
#22857=CARTESIAN_POINT('Ctrl Pts',(-4.29760892848704,5.54287832971843,0.93639549120011));
#22858=CARTESIAN_POINT('Ctrl Pts',(-4.14606191555579,5.65400717676214,0.927863132986275));
#22859=CARTESIAN_POINT('Ctrl Pts',(-3.99454328036692,5.76511521451553,0.919332372488281));
#22860=CARTESIAN_POINT('Ctrl Pts',(-3.8385385853446,5.87014166996735,0.910801611990286));
#22861=CARTESIAN_POINT('Ctrl Pts',(-3.67855791096258,5.96873841428778,0.902270851492292));
#22862=CARTESIAN_POINT('Ctrl Pts',(-3.51168451451707,6.07158317142346,0.893372545593392));
#22863=CARTESIAN_POINT('Ctrl Pts',(-3.34048522943482,6.16743169515204,0.884474239694491));
#22864=CARTESIAN_POINT('Ctrl Pts',(-3.1655710211493,6.25594011101128,0.875575933795591));
#22865=CARTESIAN_POINT('Ctrl Pts',(-2.9978868359848,6.34079005967487,0.867045436538524));
#22866=CARTESIAN_POINT('Ctrl Pts',(-2.82678895492625,6.41889435489977,0.858514939281457));
#22867=CARTESIAN_POINT('Ctrl Pts',(-2.65283978343348,6.48999750739032,0.849984442024389));
#22868=CARTESIAN_POINT('Ctrl Pts',(-2.47888883182517,6.56110138751773,0.84145385747015));
#22869=CARTESIAN_POINT('Ctrl Pts',(-2.30208681593066,6.62520386896563,0.832923272915911));
#22870=CARTESIAN_POINT('Ctrl Pts',(-2.1230155277549,6.68209784659067,0.824392688361672));
#22871=CARTESIAN_POINT('Ctrl Pts',(-1.94390880550797,6.73900308221955,0.815860415801817));
#22872=CARTESIAN_POINT('Ctrl Pts',(-1.76253220605297,6.78869687341039,0.807328143241962));
#22873=CARTESIAN_POINT('Ctrl Pts',(-1.57948290834741,6.83102190779231,0.798795870682106));
#22874=CARTESIAN_POINT('Ctrl Pts',(-1.5558502370159,6.83648630257109,0.797694307356568));
#22875=CARTESIAN_POINT('Ctrl Pts',(-1.53218970172665,6.84182794236975,0.79659274403103));
#22876=CARTESIAN_POINT('Ctrl Pts',(-1.50850260187556,6.84704655034816,0.795491180705493));
#22877=CARTESIAN_POINT('Ctrl Pts',(-1.32502988061606,6.8874682234532,0.786958822491666));
#22878=CARTESIAN_POINT('Ctrl Pts',(-1.13990061171332,6.92051799186226,0.77842646427784));
#22879=CARTESIAN_POINT('Ctrl Pts',(-0.95372153551622,6.94608103862837,0.769894106064014));
#22880=CARTESIAN_POINT('Ctrl Pts',(-0.767577322044346,6.9716392986188,0.761363345566032));
#22881=CARTESIAN_POINT('Ctrl Pts',(-0.580383996592522,6.98971359307129,
0.752832585068051));
#22882=CARTESIAN_POINT('Ctrl Pts',(-0.392755867337207,7.00024066666084,
0.744301824570069));
#22883=CARTESIAN_POINT('Ctrl Pts',(-0.197043833252064,7.0112212962357,0.735403518671163));
#22884=CARTESIAN_POINT('Ctrl Pts',(-0.00085904929266481,7.01398991619409,
0.726505212772258));
#22885=CARTESIAN_POINT('Ctrl Pts',(0.19509748762768,7.00853504898287,0.717606906873352));
#22886=CARTESIAN_POINT('Ctrl Pts',(0.382954223471156,7.00330565697144,0.709076409616276));
#22887=CARTESIAN_POINT('Ctrl Pts',(0.570600875278154,6.99051894899005,0.7005459123592));
#22888=CARTESIAN_POINT('Ctrl Pts',(0.757421232792699,6.97021804813987,0.692015415102123));
#22889=CARTESIAN_POINT('Ctrl Pts',(0.944243502139027,6.94991693953981,0.683484830547945));
#22890=CARTESIAN_POINT('Ctrl Pts',(1.13023915645784,6.92210152068343,0.674954245993767));
#22891=CARTESIAN_POINT('Ctrl Pts',(1.31479797593136,6.88686669284275,0.666423661439589));
#22892=CARTESIAN_POINT('Ctrl Pts',(1.49939331533318,6.85162489284332,0.657891388879727));
#22893=CARTESIAN_POINT('Ctrl Pts',(1.68255095165807,6.80896080995481,0.649359116319865));
#22894=CARTESIAN_POINT('Ctrl Pts',(1.86367084333698,6.75902045789149,0.640826843760003));
#22895=CARTESIAN_POINT('Ctrl Pts',(1.88705441773763,6.752572883706,0.639725280434402));
#22896=CARTESIAN_POINT('Ctrl Pts',(1.91040404455407,6.74600409587929,0.638623717108802));
#22897=CARTESIAN_POINT('Ctrl Pts',(1.93371844932792,6.7393144696793,0.637522153783201));
#22898=CARTESIAN_POINT('Ctrl Pts',(2.11430439336691,6.68749875856379,0.628989795569389));
#22899=CARTESIAN_POINT('Ctrl Pts',(2.2928368916444,6.62841170029351,0.620457437355577));
#22900=CARTESIAN_POINT('Ctrl Pts',(2.46872772896921,6.56224123015289,0.611925079141765));
#22901=CARTESIAN_POINT('Ctrl Pts',(2.64458563007975,6.49608315067921,0.603394318643801));
#22902=CARTESIAN_POINT('Ctrl Pts',(2.81780257113077,6.42284441402677,0.594863558145838));
#22903=CARTESIAN_POINT('Ctrl Pts',(2.98780823326861,6.34276190028542,0.586332797647874));
#22904=CARTESIAN_POINT('Ctrl Pts',(3.16513854123012,6.25922905411132,0.577434491748961));
#22905=CARTESIAN_POINT('Ctrl Pts',(3.33897439771579,6.16824977232899,0.568536185850047));
#22906=CARTESIAN_POINT('Ctrl Pts',(3.50869390715765,6.07014774353761,0.559637879951134));
#22907=CARTESIAN_POINT('Ctrl Pts',(3.67139811470115,5.97610073087889,0.55110738269408));
#22908=CARTESIAN_POINT('Ctrl Pts',(3.83031914624211,5.87550812891856,0.542576885437027));
#22909=CARTESIAN_POINT('Ctrl Pts',(3.98493566267762,5.76870126864099,0.534046388179973));
#22910=CARTESIAN_POINT('Ctrl Pts',(4.13955376138723,5.66189331535127,0.525515803625745));
#22911=CARTESIAN_POINT('Ctrl Pts',(4.28986700705451,5.54887115323685,0.516985219071517));
#22912=CARTESIAN_POINT('Ctrl Pts',(4.43538398265685,5.43000879270845,0.508454634517289));
#22913=CARTESIAN_POINT('Ctrl Pts',(4.58092975270658,5.31112291206515,0.499922361957472));
#22914=CARTESIAN_POINT('Ctrl Pts',(4.72167712078367,5.18639471921427,0.491390089397654));
#22915=CARTESIAN_POINT('Ctrl Pts',(4.85716795756154,5.05623832453905,0.482857816837836));
#22916=CARTESIAN_POINT('Ctrl Pts',(4.87466056995861,5.03943441796354,0.481756253512194));
#22917=CARTESIAN_POINT('Ctrl Pts',(4.89206561392294,5.02254008487155,0.480654690186552));
#22918=CARTESIAN_POINT('Ctrl Pts',(4.90938214742827,5.00555626209641,0.47955312686091));
#22919=CARTESIAN_POINT('Ctrl Pts',(5.04351049343434,4.87400498729954,0.471020768647081));
#22920=CARTESIAN_POINT('Ctrl Pts',(5.17237084479945,4.73703731504642,0.462488410433252));
#22921=CARTESIAN_POINT('Ctrl Pts',(5.29553543293831,4.5950985888221,0.453956052219423));
#22922=CARTESIAN_POINT('Ctrl Pts',(5.41867695804973,4.45318644115244,0.445425291721419));
#22923=CARTESIAN_POINT('Ctrl Pts',(5.53612464792779,4.30630532815229,0.436894531223415));
#22924=CARTESIAN_POINT('Ctrl Pts',(5.64748977655617,4.154935112152,0.428363770725412));
#22925=CARTESIAN_POINT('Ctrl Pts',(5.7636530402227,3.99704315325006,0.419465464826512));
#22926=CARTESIAN_POINT('Ctrl Pts',(5.87319777382074,3.83426696932088,0.410567158927613));
#22927=CARTESIAN_POINT('Ctrl Pts',(5.97573123079891,3.66718731724391,0.401668853028713));
#22928=CARTESIAN_POINT('Ctrl Pts',(6.07402649997131,3.50701384940077,0.393138355771637));
#22929=CARTESIAN_POINT('Ctrl Pts',(6.16587828585823,3.34288580406798,0.384607858514561));
#22930=CARTESIAN_POINT('Ctrl Pts',(6.25098590644932,3.17534277832678,0.376077361257485));
#22931=CARTESIAN_POINT('Ctrl Pts',(6.33609439799203,3.00779803802854,0.367546776703286));
#22932=CARTESIAN_POINT('Ctrl Pts',(6.41445845063592,2.8368385217534,0.359016192149087));
#22933=CARTESIAN_POINT('Ctrl Pts',(6.48582401665194,2.66302710979834,0.350485607594888));
#22934=CARTESIAN_POINT('Ctrl Pts',(6.55720370426484,2.48918130458011,0.341953335035072));
#22935=CARTESIAN_POINT('Ctrl Pts',(6.62158202404142,2.31248276000431,0.333421062475256));
#22936=CARTESIAN_POINT('Ctrl Pts',(6.67875329391682,2.13351376876158,0.32488878991544));
#22937=CARTESIAN_POINT('Ctrl Pts',(6.68613441937098,2.11040788743961,0.323787226589833));
#22938=CARTESIAN_POINT('Ctrl Pts',(6.69339548359188,2.08726418435723,0.322685663264226));
#22939=CARTESIAN_POINT('Ctrl Pts',(6.70053610427249,2.06408393187896,0.32158409993862));
#22940=CARTESIAN_POINT('Ctrl Pts',(6.75584507480538,1.88453708873849,0.313051741724777));
#22941=CARTESIAN_POINT('Ctrl Pts',(6.80394253568359,1.70273563755189,0.304519383510934));
#22942=CARTESIAN_POINT('Ctrl Pts',(6.84466437466792,1.51927487988572,0.295987025297092));
#22943=CARTESIAN_POINT('Ctrl Pts',(6.88537858833604,1.3358484759306,0.287456264799144));
#22944=CARTESIAN_POINT('Ctrl Pts',(6.91871987002713,1.15076368414967,0.278925504301196));
#22945=CARTESIAN_POINT('Ctrl Pts',(6.94457487631809,0.964627570470402,0.270394743803248));
#22946=CARTESIAN_POINT('Ctrl Pts',(6.97154383823544,0.770471835029124,0.261496437904338));
#22947=CARTESIAN_POINT('Ctrl Pts',(6.9903670753975,0.575172525106002,0.252598132005428));
#22948=CARTESIAN_POINT('Ctrl Pts',(7.00097575007869,0.3794273439146,0.243699826106518));
#22949=CARTESIAN_POINT('Ctrl Pts',(7.01114591856887,0.191773227478618,0.235169328849452));
#22950=CARTESIAN_POINT('Ctrl Pts',(7.01376694603514,0.00370968489178242,
0.226638831592386));
#22951=CARTESIAN_POINT('Ctrl Pts',(7.00883135452383,-0.18414561179569,0.218108334335321));
#22952=CARTESIAN_POINT('Ctrl Pts',(7.00389571250398,-0.372002830906788,
0.209577749781118));
#22953=CARTESIAN_POINT('Ctrl Pts',(6.99140330825087,-0.559651494072332,
0.201047165226916));
#22954=CARTESIAN_POINT('Ctrl Pts',(6.97139875862046,-0.746475659887957,
0.192516580672714));
#22955=CARTESIAN_POINT('Ctrl Pts',(6.95139025055174,-0.933336793890739,
0.183984308112868));
#22956=CARTESIAN_POINT('Ctrl Pts',(6.92386666175923,-1.11937280054723,0.175452035553022));
#22957=CARTESIAN_POINT('Ctrl Pts',(6.88892438331984,-1.30397369735794,0.166919762993175));
#22958=CARTESIAN_POINT('Ctrl Pts',(6.88441314294721,-1.32780668867135,0.16581819966756));
#22959=CARTESIAN_POINT('Ctrl Pts',(6.87977831627972,-1.35161577155493,0.164716636341944));
#22960=CARTESIAN_POINT('Ctrl Pts',(6.87502017297057,-1.37539964510236,0.163615073016328));
#22961=CARTESIAN_POINT('Ctrl Pts',(6.83816511234691,-1.559621944538,0.155082714802508));
#22962=CARTESIAN_POINT('Ctrl Pts',(6.79389498193691,-1.74239308271298,0.146550356588688));
#22963=CARTESIAN_POINT('Ctrl Pts',(6.74234892197997,-1.92311143119049,0.138017998374868));
#22964=CARTESIAN_POINT('Ctrl Pts',(6.69081251421497,-2.10379593948338,0.129487237876939));
#22965=CARTESIAN_POINT('Ctrl Pts',(6.63200297973483,-2.28242813106,0.12095647737901));
#22966=CARTESIAN_POINT('Ctrl Pts',(6.56610970461094,-2.45842020604981,0.112425716881081));
#22967=CARTESIAN_POINT('Ctrl Pts',(6.49737743638276,-2.64199484976712,0.103527410982161));
#22968=CARTESIAN_POINT('Ctrl Pts',(6.42093760606955,-2.82269650182234,0.0946291050832411));
#22969=CARTESIAN_POINT('Ctrl Pts',(6.3370618935737,-2.99987885080649,0.0857307991843212));
#22970=CARTESIAN_POINT('Ctrl Pts',(6.25665315695463,-3.16973742379592,0.0772003019272322));
#22971=CARTESIAN_POINT('Ctrl Pts',(6.16941103836503,-3.33636148742264,0.0686698046701432));
#22972=CARTESIAN_POINT('Ctrl Pts',(6.07562306814898,-3.49920432331065,0.0601393074130542));
#22973=CARTESIAN_POINT('Ctrl Pts',(5.9818341381507,-3.6620488256561,0.0516087228588453));
#22974=CARTESIAN_POINT('Ctrl Pts',(5.88149937818162,-3.82111175940824,0.0430781383046364));
#22975=CARTESIAN_POINT('Ctrl Pts',(5.77495130476384,-3.97587273313753,0.0345475537504275));
#22976=CARTESIAN_POINT('Ctrl Pts',(5.66838214794392,-4.13066433048805,0.0260152811906182));
#22977=CARTESIAN_POINT('Ctrl Pts',(5.55559739641577,-4.28115201614751,0.0174830086308088));
#22978=CARTESIAN_POINT('Ctrl Pts',(5.43697225766915,-4.42684529115667,0.00895073607099953));
#22979=CARTESIAN_POINT('Ctrl Pts',(5.42165709967018,-4.44565509445578,0.00784917274534623));
#22980=CARTESIAN_POINT('Ctrl Pts',(5.40624464856188,-4.46438502763424,0.00674760941969292));
#22981=CARTESIAN_POINT('Ctrl Pts',(5.39073576089718,-4.48303407511969,0.00564604609403962));
#22982=CARTESIAN_POINT('Ctrl Pts',(5.27060886308617,-4.62748364945361,-0.00288631211978283));
#22983=CARTESIAN_POINT('Ctrl Pts',(5.14465240415034,-4.76712642172868,-0.0114186703336053));
#22984=CARTESIAN_POINT('Ctrl Pts',(5.01327520578717,-4.9014995943629,-0.0199510285474277));
#22985=CARTESIAN_POINT('Ctrl Pts',(4.88192260829423,-5.03584760511953,-0.028481789045362));
#22986=CARTESIAN_POINT('Ctrl Pts',(4.74515151086828,-5.16492776673308,-0.0370125495432962));
#22987=CARTESIAN_POINT('Ctrl Pts',(4.60340833500619,-5.28831336663171,-0.0455433100412305));
#22988=CARTESIAN_POINT('Ctrl Pts',(4.45555819453976,-5.41701500017134,-0.0544416159401489));
#22989=CARTESIAN_POINT('Ctrl Pts',(4.30229829444563,-5.53952025612765,-0.0633399218390673));
#22990=CARTESIAN_POINT('Ctrl Pts',(4.14417528276514,-5.65539015349237,-0.0722382277379857));
#22991=CARTESIAN_POINT('Ctrl Pts',(3.99258823543917,-5.76647060553293,-0.0807687249950581));
#22992=CARTESIAN_POINT('Ctrl Pts',(3.83653228743178,-5.87145301799739,-0.0892992222521305));
#22993=CARTESIAN_POINT('Ctrl Pts',(3.67652060358513,-5.96999353550019,-0.0978297195092029));
#22994=CARTESIAN_POINT('Ctrl Pts',(3.51650728225407,-6.06853506142036,-0.106360304063377));
#22995=CARTESIAN_POINT('Ctrl Pts',(3.35253840642575,-6.16063440295548,-0.114890888617551));
#22996=CARTESIAN_POINT('Ctrl Pts',(3.18515416446187,-6.24599227594073,-0.123421473171726));
#22997=CARTESIAN_POINT('Ctrl Pts',(3.01773680102362,-6.33136703927699,-0.131953745731499));
#22998=CARTESIAN_POINT('Ctrl Pts',(2.84690299468735,-6.4099975316115,-0.140486018291272));
#22999=CARTESIAN_POINT('Ctrl Pts',(2.67321624127837,-6.48163108251816,-0.149018290851045));
#23000=CARTESIAN_POINT('Ctrl Pts',(2.65079232591689,-6.49087936801516,-0.15011985417678));
#23001=CARTESIAN_POINT('Ctrl Pts',(2.62832088499811,-6.50001109234066,-0.151221417502516));
#23002=CARTESIAN_POINT('Ctrl Pts',(2.60580315531013,-6.50902577028819,-0.152322980828251));
#23003=CARTESIAN_POINT('Ctrl Pts',(2.43138800243462,-6.57885059073544,-0.16085533904209));
#23004=CARTESIAN_POINT('Ctrl Pts',(2.25413532275062,-6.64167272808602,-0.169387697255928));
#23005=CARTESIAN_POINT('Ctrl Pts',(2.07462498107822,-6.69727987696395,-0.177920055469766));
#23006=CARTESIAN_POINT('Ctrl Pts',(1.89514825338543,-6.75287661319627,-0.186450815967772));
#23007=CARTESIAN_POINT('Ctrl Pts',(1.71341499952775,-6.80126096661933,-0.194981576465778));
#23008=CARTESIAN_POINT('Ctrl Pts',(1.53002096621149,-6.84227026691092,-0.203512336963784));
#23009=CARTESIAN_POINT('Ctrl Pts',(1.33872545289098,-6.88504644129532,-0.21241064286268));
#23010=CARTESIAN_POINT('Ctrl Pts',(1.1456232205715,-6.91979788136369,-0.221308948761577));
#23011=CARTESIAN_POINT('Ctrl Pts',(0.951403993087149,-6.94639885152284,
-0.230207254660473));
#23012=CARTESIAN_POINT('Ctrl Pts',(0.765212755547516,-6.97190027904801,
-0.238737751917524));
#23013=CARTESIAN_POINT('Ctrl Pts',(0.577995331319964,-6.98991143949831,
-0.247268249174574));
#23014=CARTESIAN_POINT('Ctrl Pts',(0.390366706047602,-7.00037430408614,
-0.255798746431625));
#23015=CARTESIAN_POINT('Ctrl Pts',(0.202736160669771,-7.01083727574615,
-0.264329330985879));
#23016=CARTESIAN_POINT('Ctrl Pts',(0.0146947115222116,-7.01375178338187,
-0.272859915540134));
#23017=CARTESIAN_POINT('Ctrl Pts',(-0.173140114982729,-7.00911185979249,
-0.281390500094389));
#23018=CARTESIAN_POINT('Ctrl Pts',(-0.361012109659622,-7.00447101806945,
-0.289922772654215));
#23019=CARTESIAN_POINT('Ctrl Pts',(-0.548677094163707,-6.99227276804658,
-0.298455045214041));
#23020=CARTESIAN_POINT('Ctrl Pts',(-0.735519241624514,-6.97256323081405,
-0.306987317773867));
#23021=CARTESIAN_POINT('Ctrl Pts',(-0.759641590725308,-6.97001862113043,
-0.308088881099424));
#23022=CARTESIAN_POINT('Ctrl Pts',(-0.783750231116449,-6.96734888248705,
-0.309190444424982));
#23023=CARTESIAN_POINT('Ctrl Pts',(-0.807843844180328,-6.96455417711141,
-0.310292007750539));
#23024=CARTESIAN_POINT('Ctrl Pts',(-0.994465287139578,-6.94290728054736,
-0.318824365964374));
#23025=CARTESIAN_POINT('Ctrl Pts',(-1.18024759914043,-6.91375139016416,
-0.327356724178208));
#23026=CARTESIAN_POINT('Ctrl Pts',(-1.36457977895502,-6.87717591670935,
-0.335889082392043));
#23027=CARTESIAN_POINT('Ctrl Pts',(-1.54887744188274,-6.8406072921481,-0.344419842890039));
#23028=CARTESIAN_POINT('Ctrl Pts',(-1.73172521451693,-6.79662191666365,
-0.352950603388035));
#23029=CARTESIAN_POINT('Ctrl Pts',(-1.91252176355406,-6.74536041041782,
-0.361481363886031));
#23030=CARTESIAN_POINT('Ctrl Pts',(-2.10110788072095,-6.6918903166881,-0.370379669784931));
#23031=CARTESIAN_POINT('Ctrl Pts',(-2.28746176066021,-6.63050329733387,
-0.37927797568383));
#23032=CARTESIAN_POINT('Ctrl Pts',(-2.47091701666132,-6.56141719899547,
-0.38817628158273));
#23033=CARTESIAN_POINT('Ctrl Pts',(-2.64678920805253,-6.49518675254061,
-0.39670677883978));
#23034=CARTESIAN_POINT('Ctrl Pts',(-2.81999727924531,-6.42188102350908,
-0.405237276096829));
#23035=CARTESIAN_POINT('Ctrl Pts',(-2.98997280427668,-6.34174181059004,
-0.413767773353879));
#23036=CARTESIAN_POINT('Ctrl Pts',(-3.15995006876101,-6.2616017775624,-0.422298357908195));
#23037=CARTESIAN_POINT('Ctrl Pts',(-3.32669444560058,-6.17462825432024,
-0.430828942462511));
#23038=CARTESIAN_POINT('Ctrl Pts',(-3.4896600638369,-6.08111003036139,-0.439359527016827));
#23039=CARTESIAN_POINT('Ctrl Pts',(-3.65265792920186,-5.98757330130783,
-0.447891799576629));
#23040=CARTESIAN_POINT('Ctrl Pts',(-3.81187527764207,-5.88748943813292,
-0.456424072136431));
#23041=CARTESIAN_POINT('Ctrl Pts',(-3.96679253468986,-5.78119222559056,
-0.464956344696233));
#23042=CARTESIAN_POINT('Ctrl Pts',(-3.98679320481144,-5.76746867068508,
-0.466057908021765));
#23043=CARTESIAN_POINT('Ctrl Pts',(-4.00672223952132,-5.75364160948471,
-0.467159471347298));
#23044=CARTESIAN_POINT('Ctrl Pts',(-4.02657855652151,-5.73971181250951,
-0.468261034672831));
#23045=CARTESIAN_POINT('Ctrl Pts',(-4.18037925551463,-5.63181604756988,
-0.476793392886621));
#23046=CARTESIAN_POINT('Ctrl Pts',(-4.32986662685901,-5.51771670837547,
-0.485325751100411));
#23047=CARTESIAN_POINT('Ctrl Pts',(-4.47454595206147,-5.39778334924535,
-0.493858109314201));
#23048=CARTESIAN_POINT('Ctrl Pts',(-4.61919818552228,-5.2778724480827,-0.502388869812187));
#23049=CARTESIAN_POINT('Ctrl Pts',(-4.75904393408753,-5.15212990229196,
-0.510919630310174));
#23050=CARTESIAN_POINT('Ctrl Pts',(-4.89362136437337,-5.02096569443056,
-0.51945039080816));
#23051=CARTESIAN_POINT('Ctrl Pts',(-5.03399702514309,-4.88415031380712,
-0.528348696707074));
#23052=CARTESIAN_POINT('Ctrl Pts',(-5.16864007484259,-4.74143597016446,
-0.537247002605987));
#23053=CARTESIAN_POINT('Ctrl Pts',(-5.29706824614347,-4.593331531492,-0.5461453085049));
#23054=CARTESIAN_POINT('Ctrl Pts',(-5.42018787986454,-4.45134894264784,
-0.554675805761967));
#23055=CARTESIAN_POINT('Ctrl Pts',(-5.53759587132219,-4.30441314245886,
-0.563206303019034));
#23056=CARTESIAN_POINT('Ctrl Pts',(-5.64890750104157,-4.15300741718291,
-0.571736800276102));
#23057=CARTESIAN_POINT('Ctrl Pts',(-5.76022026987218,-4.00160014249149,
-0.580267384830293));
#23058=CARTESIAN_POINT('Ctrl Pts',(-5.86543637366439,-3.84572309974774,
-0.588797969384485));
#23059=CARTESIAN_POINT('Ctrl Pts',(-5.96421330176928,-3.68589015754653,
-0.597328553938677));
#23060=CARTESIAN_POINT('Ctrl Pts',(-6.06300977554652,-3.52602558809817,
-0.605860826498497));
#23061=CARTESIAN_POINT('Ctrl Pts',(-6.15536436876196,-3.36220381657647,
-0.614393099058317));
#23062=CARTESIAN_POINT('Ctrl Pts',(-6.24097911952844,-3.19496575758021,
-0.622925371618137));
#23063=CARTESIAN_POINT('Ctrl Pts',(-6.25203245484078,-3.17337440414494,
-0.624026934943799));
#23064=CARTESIAN_POINT('Ctrl Pts',(-6.26297351185236,-3.15172614053068,
-0.625128498269461));
#23065=CARTESIAN_POINT('Ctrl Pts',(-6.27380170571591,-3.13002215964299,
-0.626230061595122));
#23066=CARTESIAN_POINT('Ctrl Pts',(-6.35745714771697,-2.9623435848758,-0.634740415959077));
#23067=CARTESIAN_POINT('Ctrl Pts',(-6.43440197266013,-2.79127817175156,
-0.643250770323033));
#23068=CARTESIAN_POINT('Ctrl Pts',(-6.50437781620031,-2.61738338548661,
-0.651761124686988));
#23069=CARTESIAN_POINT('Ctrl Pts',(-6.5277917422228,-2.55919816819849,-0.654608690324241));
#23070=CARTESIAN_POINT('Ctrl Pts',(-6.55042583092581,-2.50069636654977,
-0.657456255961495));
#23071=CARTESIAN_POINT('Ctrl Pts',(-6.5722715952584,-2.44189939200198,-0.660303821598748));
#23072=CARTESIAN_POINT('Origin',(0.,0.,0.));
#23073=CARTESIAN_POINT('',(-6.57261910096697,-2.44202878201564,-2.66029322980694));
#23074=CARTESIAN_POINT('',(-6.57227163721606,-2.44189927907465,-2.11302806574593));
#23075=CARTESIAN_POINT('',(-6.57227159525839,-2.441899392002,0.));
#23076=CARTESIAN_POINT('Ctrl Pts',(-6.57227163721606,-2.44189927907466,
-2.11302806574593));
#23077=CARTESIAN_POINT('Ctrl Pts',(-6.51953748579793,-2.5838310821789,-2.10622305876647));
#23078=CARTESIAN_POINT('Ctrl Pts',(-6.46220633364772,-2.72405292621106,
-2.09944006788617));
#23079=CARTESIAN_POINT('Ctrl Pts',(-6.33650509248318,-3.00512819872079,
-2.08564570072172));
#23080=CARTESIAN_POINT('Ctrl Pts',(-6.26788868974173,-3.1457372854464,-2.07863975024577));
#23081=CARTESIAN_POINT('Ctrl Pts',(-6.15383678120463,-3.36087845473853,
-2.06767142613725));
#23082=CARTESIAN_POINT('Ctrl Pts',(-6.11161603784971,-3.43705691998926,
-2.06373707023924));
#23083=CARTESIAN_POINT('Ctrl Pts',(-5.99986890027327,-3.63010861102319,
-2.05360831065317));
#23084=CARTESIAN_POINT('Ctrl Pts',(-5.92834201533009,-3.74578101905171,
-2.04738680115132));
#23085=CARTESIAN_POINT('Ctrl Pts',(-5.69016811754324,-4.10702550372183,
-2.02752645117635));
#23086=CARTESIAN_POINT('Ctrl Pts',(-5.51127520696392,-4.34413621110689,
-2.01384649718659));
#23087=CARTESIAN_POINT('Ctrl Pts',(-5.19460340716075,-4.71269729482426,
-1.99160728170246));
#23088=CARTESIAN_POINT('Ctrl Pts',(-5.06554858082755,-4.85114826985282,
-1.98299428255651));
#23089=CARTESIAN_POINT('Ctrl Pts',(-4.71483135622538,-5.19812482824586,
-1.96065680487294));
#23090=CARTESIAN_POINT('Ctrl Pts',(-4.48492016006575,-5.39774311405849,
-1.94704021335579));
#23091=CARTESIAN_POINT('Ctrl Pts',(-4.07276902366969,-5.71102252482692,
-1.92384579853699));
#23092=CARTESIAN_POINT('Ctrl Pts',(-3.89695293238659,-5.8324078513493,-1.91428098375394));
#23093=CARTESIAN_POINT('Ctrl Pts',(-3.62003185496311,-6.00547831241529,
-1.89948619697423));
#23094=CARTESIAN_POINT('Ctrl Pts',(-3.52275654162347,-6.0630508716118,-1.89433181645506));
#23095=CARTESIAN_POINT('Ctrl Pts',(-3.18463566105164,-6.25228339227409,
-1.87658940572744));
#23096=CARTESIAN_POINT('Ctrl Pts',(-2.93747413220861,-6.37214232036376,
-1.86393092679018));
#23097=CARTESIAN_POINT('Ctrl Pts',(-2.48580379030894,-6.55929853983847,
-1.84149219324628));
#23098=CARTESIAN_POINT('Ctrl Pts',(-2.28401871681013,-6.6322604385465,-1.83169692937167));
#23099=CARTESIAN_POINT('Ctrl Pts',(-1.87862206162202,-6.75814461970629,
-1.81243081495137));
#23100=CARTESIAN_POINT('Ctrl Pts',(-1.67533986993288,-6.81138588901042,
-1.80296694735822));
#23101=CARTESIAN_POINT('Ctrl Pts',(-1.18806296773287,-6.91587015740234,
-1.78059141505088));
#23102=CARTESIAN_POINT('Ctrl Pts',(-0.902695260293384,-6.95887151122777,
-1.76773609250292));
#23103=CARTESIAN_POINT('Ctrl Pts',(-0.50632953486355,-6.9938020064444,-1.74980433031526));
#23104=CARTESIAN_POINT('Ctrl Pts',(-0.39695619116797,-7.00086149172748,
-1.7448451267552));
#23105=CARTESIAN_POINT('Ctrl Pts',(-0.0704598280006472,-7.01425911832889,
-1.72995996183026));
#23106=CARTESIAN_POINT('Ctrl Pts',(0.146836526019976,-7.0130758563541,-1.71996890697031));
#23107=CARTESIAN_POINT('Ctrl Pts',(0.569885949331282,-6.99109961083581,
-1.70048068945671));
#23108=CARTESIAN_POINT('Ctrl Pts',(0.775475263538958,-6.97128991803752,
-1.69099278094508));
#23109=CARTESIAN_POINT('Ctrl Pts',(1.06527357053363,-6.93038628930513,-1.67761158148982));
#23110=CARTESIAN_POINT('Ctrl Pts',(1.15042649250193,-6.91676087008585,-1.67367830779049));
#23111=CARTESIAN_POINT('Ctrl Pts',(1.42088198533952,-6.8683522326076,-1.66117676076989));
#23112=CARTESIAN_POINT('Ctrl Pts',(1.60504366515428,-6.827664634724,-1.652652527281));
#23113=CARTESIAN_POINT('Ctrl Pts',(2.17672919603003,-6.67694812038725,-1.62603700615829));
#23114=CARTESIAN_POINT('Ctrl Pts',(2.55654114230817,-6.54093839122033,-1.60816388687753));
#23115=CARTESIAN_POINT('Ctrl Pts',(3.01940679865851,-6.32867748826894,-1.58511560681427));
#23116=CARTESIAN_POINT('Ctrl Pts',(3.11521786188344,-6.28206917467245,-1.58026433345328));
#23117=CARTESIAN_POINT('Ctrl Pts',(3.45492929911434,-6.1071297303324,-1.56278674522321));
#23118=CARTESIAN_POINT('Ctrl Pts',(3.69227790865397,-5.9666283192268,-1.55007586514755));
#23119=CARTESIAN_POINT('Ctrl Pts',(4.10506250509221,-5.68819143019162,-1.52721245076718));
#23120=CARTESIAN_POINT('Ctrl Pts',(4.28336906056868,-5.55516082737718,-1.51705058499257));
#23121=CARTESIAN_POINT('Ctrl Pts',(4.61560006042116,-5.28176968717741,-1.4975148638704));
#23122=CARTESIAN_POINT('Ctrl Pts',(4.770190878907,-5.14258065267075,-1.48814172755728));
#23123=CARTESIAN_POINT('Ctrl Pts',(5.1281382503437,-4.79024651914989,-1.46558351981212));
#23124=CARTESIAN_POINT('Ctrl Pts',(5.32469539334947,-4.57076365934437,-1.4524621633358));
#23125=CARTESIAN_POINT('Ctrl Pts',(5.57533038512504,-4.25271092174228,-1.43421715648585));
#23126=CARTESIAN_POINT('Ctrl Pts',(5.64171980018662,-4.16423540730412,-1.429213607102));
#23127=CARTESIAN_POINT('Ctrl Pts',(5.81936632704178,-3.91543988374907,-1.4152905826453));
#23128=CARTESIAN_POINT('Ctrl Pts',(5.9260651735649,-3.75199201605711,-1.40632367816575));
#23129=CARTESIAN_POINT('Ctrl Pts',(6.13693332561609,-3.39748833767617,-1.38734957803417));
#23130=CARTESIAN_POINT('Ctrl Pts',(6.23931191876503,-3.20559911688762,-1.37735167651129));
#23131=CARTESIAN_POINT('Ctrl Pts',(6.41306114104572,-2.83996606376113,-1.35883085801239));
#23132=CARTESIAN_POINT('Ctrl Pts',(6.48669087267177,-2.66750886342719,-1.35030100584811));
#23133=CARTESIAN_POINT('Ctrl Pts',(6.64787543344751,-2.24368692236273,-1.32977722671881));
#23134=CARTESIAN_POINT('Ctrl Pts',(6.72820443306059,-1.98988603124351,-1.31785105648502));
#23135=CARTESIAN_POINT('Ctrl Pts',(6.83598640412604,-1.56713457381781,-1.29830478262318));
#23136=CARTESIAN_POINT('Ctrl Pts',(6.87202848356104,-1.40065869672694,-1.29068356264488));
#23137=CARTESIAN_POINT('Ctrl Pts',(6.922376645178,-1.11883289029985,-1.2777962314217));
#23138=CARTESIAN_POINT('Ctrl Pts',(6.93994123689945,-1.00414181979542,-1.27255440448487));
#23139=CARTESIAN_POINT('Ctrl Pts',(6.97569617344906,-0.724451852747487,
-1.25972304350627));
#23140=CARTESIAN_POINT('Ctrl Pts',(6.99088876476121,-0.559142896839073,
-1.252108629037));
#23141=CARTESIAN_POINT('Ctrl Pts',(7.01345372084819,-0.157673539843914,
-1.23362207052769));
#23142=CARTESIAN_POINT('Ctrl Pts',(7.0147853281581,0.0786263206280219,-1.22274933931911));
#23143=CARTESIAN_POINT('Ctrl Pts',(6.99556447043618,0.506633699858591,-1.20313059071173));
#23144=CARTESIAN_POINT('Ctrl Pts',(6.97903946981141,0.698290572471308,-1.19437160873707));
#23145=CARTESIAN_POINT('Ctrl Pts',(6.906028430232,1.26943908542235,-1.16828904011256));
#23146=CARTESIAN_POINT('Ctrl Pts',(6.8262697841316,1.64521970948371,-1.15118534066737));
#23147=CARTESIAN_POINT('Ctrl Pts',(6.69383214117339,2.08717518292637,-1.130484971321));
#23148=CARTESIAN_POINT('Ctrl Pts',(6.67024108955778,2.16138212353261,-1.12698714340597));
#23149=CARTESIAN_POINT('Ctrl Pts',(6.60997288537854,2.34056563741783,-1.11847035518716));
#23150=CARTESIAN_POINT('Ctrl Pts',(6.57202555391534,2.4450907777513,-1.11344109812216));
#23151=CARTESIAN_POINT('Ctrl Pts',(6.45966058649541,2.73305427449377,-1.09936460835701));
#23152=CARTESIAN_POINT('Ctrl Pts',(6.37993814708852,2.9143075243136,-1.0902676665805));
#23153=CARTESIAN_POINT('Ctrl Pts',(6.19717111788147,3.28627105452563,-1.07120305700744));
#23154=CARTESIAN_POINT('Ctrl Pts',(6.09273529955224,3.47607323663455,-1.06124494652088));
#23155=CARTESIAN_POINT('Ctrl Pts',(5.88192895315215,3.82041774221988,-1.04277387146757));
#23156=CARTESIAN_POINT('Ctrl Pts',(5.77781639586997,3.97611860963083,-1.03425424626747));
#23157=CARTESIAN_POINT('Ctrl Pts',(5.51633433584106,4.33517044357127,-1.01415058180392));
#23158=CARTESIAN_POINT('Ctrl Pts',(5.35376855983176,4.53440314263139,-1.00262587369899));
#23159=CARTESIAN_POINT('Ctrl Pts',(5.06243592471743,4.85387882066213,-0.983253652586092));
#23160=CARTESIAN_POINT('Ctrl Pts',(4.93941696602262,4.97901159816298,-0.975404346216908));
#23161=CARTESIAN_POINT('Ctrl Pts',(4.72637753451685,5.18003742826861,-0.962221554904486));
#23162=CARTESIAN_POINT('Ctrl Pts',(4.6389071789761,5.25851426109885,-0.956914085935074));
#23163=CARTESIAN_POINT('Ctrl Pts',(4.44114884533163,5.42716351144375,-0.945088750833864));
#23164=CARTESIAN_POINT('Ctrl Pts',(4.33000280149616,5.51624707609266,-0.938562475106899));
#23165=CARTESIAN_POINT('Ctrl Pts',(4.01632625589052,5.75233377439716,-0.920525766494181));
#23166=CARTESIAN_POINT('Ctrl Pts',(3.80851901656226,5.89197798147266,-0.908999622644175));
#23167=CARTESIAN_POINT('Ctrl Pts',(3.42547694329479,6.12063019898576,-0.888561787861463));
#23168=CARTESIAN_POINT('Ctrl Pts',(3.25312430962182,6.21395126374646,-0.879632547332947));
#23169=CARTESIAN_POINT('Ctrl Pts',(2.85668838537808,6.40758322178479,-0.859638089324845));
#23170=CARTESIAN_POINT('Ctrl Pts',(2.63078947535102,6.50359442553203,-0.848617999075666));
#23171=CARTESIAN_POINT('Ctrl Pts',(2.21532642632959,6.6549772720127,-0.828796816384092));
#23172=CARTESIAN_POINT('Ctrl Pts',(2.02757430087945,6.7145614495574,-0.819993903164605));
#23173=CARTESIAN_POINT('Ctrl Pts',(1.71829410496459,6.79855622026545,-0.805580649543301));
#23174=CARTESIAN_POINT('Ctrl Pts',(1.59818849064993,6.82778840026634,-0.800003364071787));
#23175=CARTESIAN_POINT('Ctrl Pts',(1.34873321047896,6.88155960884435,-0.788400046508771));
#23176=CARTESIAN_POINT('Ctrl Pts',(1.21933840783383,6.90566123529639,-0.782374836239947));
#23177=CARTESIAN_POINT('Ctrl Pts',(0.832617388102664,6.96648502223349,-0.764400539666374));
#23178=CARTESIAN_POINT('Ctrl Pts',(0.573843077236756,6.99255822311188,-0.752423249359184));
#23179=CARTESIAN_POINT('Ctrl Pts',(0.11605306322733,7.01309542224427,-0.731422272237092));
#23180=CARTESIAN_POINT('Ctrl Pts',(-0.0824039055175498,7.01357163845523,
-0.722377798841256));
#23181=CARTESIAN_POINT('Ctrl Pts',(-0.655101838414206,6.99063180179189,
-0.696396248055746));
#23182=CARTESIAN_POINT('Ctrl Pts',(-1.02778326705308,6.94562860512029,-0.679662612450395));
#23183=CARTESIAN_POINT('Ctrl Pts',(-1.56570433335402,6.83641054771974,-0.655050768707296));
#23184=CARTESIAN_POINT('Ctrl Pts',(-1.73497665737009,6.79542446991993,-0.647230708071769));
#23185=CARTESIAN_POINT('Ctrl Pts',(-2.01876329756693,6.71541521806983,-0.633856319975324));
#23186=CARTESIAN_POINT('Ctrl Pts',(-2.13411374301414,6.67965301808382,-0.628340561556277));
#23187=CARTESIAN_POINT('Ctrl Pts',(-2.51340711941884,6.55123215530529,-0.609983091602798));
#23188=CARTESIAN_POINT('Ctrl Pts',(-2.7727283881231,6.44576110261613,-0.597083850232413));
#23189=CARTESIAN_POINT('Ctrl Pts',(-3.20844135660255,6.23737552779624,-0.574937859495651));
#23190=CARTESIAN_POINT('Ctrl Pts',(-3.38792802955432,6.14173387660556,-0.565663596643418));
#23191=CARTESIAN_POINT('Ctrl Pts',(-3.90916097761288,5.83417755729144,-0.538216858581451));
#23192=CARTESIAN_POINT('Ctrl Pts',(-4.23711154293978,5.60054074252687,-0.520292896684572));
#23193=CARTESIAN_POINT('Ctrl Pts',(-4.60289977383775,5.28933610627461,-0.498745982025865));
#23194=CARTESIAN_POINT('Ctrl Pts',(-4.66170747694175,5.23758017311961,-0.495227118306987));
#23195=CARTESIAN_POINT('Ctrl Pts',(-4.80205278176163,5.10982745900633,-0.486677628279994));
#23196=CARTESIAN_POINT('Ctrl Pts',(-4.88266817310611,5.03285195838024,-0.48163682753406));
#23197=CARTESIAN_POINT('Ctrl Pts',(-5.10211786256593,4.81307322170992,-0.467493951432141));
#23198=CARTESIAN_POINT('Ctrl Pts',(-5.23675217016614,4.66623035799095,-0.458341175817069));
#23199=CARTESIAN_POINT('Ctrl Pts',(-5.50411364112357,4.34845753317505,-0.439237595113581));
#23200=CARTESIAN_POINT('Ctrl Pts',(-5.63555286791056,4.17670863639256,-0.429296446644721));
#23201=CARTESIAN_POINT('Ctrl Pts',(-5.86558794953502,3.84545494795492,-0.410846564889966));
#23202=CARTESIAN_POINT('Ctrl Pts',(-5.9661322944301,3.68753478099821,-0.402331288097689));
#23203=CARTESIAN_POINT('Ctrl Pts',(-6.18591950332344,3.30975650239894,-0.382549926611484));
#23204=CARTESIAN_POINT('Ctrl Pts',(-6.2999600098488,3.08716606843899,-0.371336894420973));
#23205=CARTESIAN_POINT('Ctrl Pts',(-6.47511748331437,2.69494806530593,-0.35208947617182));
#23206=CARTESIAN_POINT('Ctrl Pts',(-6.54203221130213,2.52818223171317,-0.344053311846169));
#23207=CARTESIAN_POINT('Ctrl Pts',(-6.64241059628119,2.24724281384611,-0.330628628174148));
#23208=CARTESIAN_POINT('Ctrl Pts',(-6.67950624280283,2.13445890569617,-0.325267530957115));
#23209=CARTESIAN_POINT('Ctrl Pts',(-6.76622730642944,1.84634295529001,-0.311579604140177));
#23210=CARTESIAN_POINT('Ctrl Pts',(-6.81191448793027,1.66992033273699,-0.3032162317978));
#23211=CARTESIAN_POINT('Ctrl Pts',(-6.89944374467669,1.26799910238903,-0.284299975755273));
#23212=CARTESIAN_POINT('Ctrl Pts',(-6.93720115188294,1.04181915943751,-0.273752348830883));
#23213=CARTESIAN_POINT('Ctrl Pts',(-6.97413171097342,0.72595239414745,-0.259194191658068));
#23214=CARTESIAN_POINT('Ctrl Pts',(-6.98277083377061,0.637519914007879,
-0.25513616674583));
#23215=CARTESIAN_POINT('Ctrl Pts',(-7.00407233685088,0.366288335271892,
-0.242740651524406));
#23216=CARTESIAN_POINT('Ctrl Pts',(-7.0112523177922,0.183136087572746,-0.234442732772776));
#23217=CARTESIAN_POINT('Ctrl Pts',(-7.01124871528832,-0.101579106034701,
-0.221607777351206));
#23218=CARTESIAN_POINT('Ctrl Pts',(-7.00904376688205,-0.203057910238692,
-0.21704532616958));
#23219=CARTESIAN_POINT('Ctrl Pts',(-6.99269606217985,-0.579173637994724,
-0.200147900057931));
#23220=CARTESIAN_POINT('Ctrl Pts',(-6.96460424313232,-0.852951423398579,
-0.187881817746726));
#23221=CARTESIAN_POINT('Ctrl Pts',(-6.90275168889596,-1.23365491144146,
-0.170504260987112));
#23222=CARTESIAN_POINT('Ctrl Pts',(-6.88241021161708,-1.34250316286391,
-0.165495514278024));
#23223=CARTESIAN_POINT('Ctrl Pts',(-6.81424568765894,-1.66478500130876,
-0.15049327476538));
#23224=CARTESIAN_POINT('Ctrl Pts',(-6.75900633229958,-1.87650875306416,
-0.140433011724079));
#23225=CARTESIAN_POINT('Ctrl Pts',(-6.65659239076678,-2.2052646011545,-0.124592045835341));
#23226=CARTESIAN_POINT('Ctrl Pts',(-6.61601241605238,-2.32417276872652,
-0.118814850930105));
#23227=CARTESIAN_POINT('Ctrl Pts',(-6.57227163891168,-2.44189927451098,
-0.113051811211838));
#23228=CARTESIAN_POINT('',(-7.01138978795984,7.81656089707349E-5,-0.773534355761736));
#23229=CARTESIAN_POINT('Ctrl Pts',(-6.5722715952584,-2.44189939200198,-0.660303821598748));
#23230=CARTESIAN_POINT('Ctrl Pts',(-6.63754513530709,-2.26621834855315,
-0.668812138672701));
#23231=CARTESIAN_POINT('Ctrl Pts',(-6.69577709547641,-2.08790084462448,
-0.677320455746654));
#23232=CARTESIAN_POINT('Ctrl Pts',(-6.74677372834014,-1.9075300315013,-0.685828772820607));
#23233=CARTESIAN_POINT('Ctrl Pts',(-6.79777217374385,-1.7271528075762,-0.694337392300112));
#23234=CARTESIAN_POINT('Ctrl Pts',(-6.84153469067179,-1.54472242525412,
-0.702846011779617));
#23235=CARTESIAN_POINT('Ctrl Pts',(-6.87791759594143,-1.36083654637111,
-0.711354631259122));
#23236=CARTESIAN_POINT('Ctrl Pts',(-6.9142994945855,-1.17695575515848,-0.719863015326035));
#23237=CARTESIAN_POINT('Ctrl Pts',(-6.94330213173949,-0.991619851606324,
-0.728371399392948));
#23238=CARTESIAN_POINT('Ctrl Pts',(-6.96483300486484,-0.805436389074502,
-0.736879783459861));
#23239=CARTESIAN_POINT('Ctrl Pts',(-6.98636838000213,-0.619213996390389,
-0.745389946592879));
#23240=CARTESIAN_POINT('Ctrl Pts',(-7.00042883457153,-0.432143997917336,
-0.753900109725898));
#23241=CARTESIAN_POINT('Ctrl Pts',(-7.00697367561977,-0.244839685654932,
-0.762410272858916));
#23242=CARTESIAN_POINT('Ctrl Pts',(-7.00982537777381,-0.163227908256182,
-0.766118300350915));
#23243=CARTESIAN_POINT('Ctrl Pts',(-7.01125090971808,-0.0815716875323698,
-0.769826327842913));
#23244=CARTESIAN_POINT('Ctrl Pts',(-7.0112499995644,7.81546515054621E-5,
-0.773534355334912));
#23245=CARTESIAN_POINT('Ctrl Pts',(-7.01176597774635,7.81950970159262E-5,
-0.773534356910375));
#23246=CARTESIAN_POINT('Ctrl Pts',(-7.01181069762049,0.078362201253698,
-0.777089267446053));
#23247=CARTESIAN_POINT('Ctrl Pts',(-6.99150694704885,1.31618785766362,-0.833300520289124));
#23248=CARTESIAN_POINT('Ctrl Pts',(-6.30415497350669,3.69183680131228,-0.942168115439734));
#23249=CARTESIAN_POINT('Ctrl Pts',(-3.78576056174483,6.24820341111258,-1.10013714236197));
#23250=CARTESIAN_POINT('Ctrl Pts',(-0.35395787806857,7.29703657096924,-1.25810616928429));
#23251=CARTESIAN_POINT('Ctrl Pts',(3.16324588907938,6.58527936709808,-1.41607519620657));
#23252=CARTESIAN_POINT('Ctrl Pts',(5.91723842982768,4.28466081062169,-1.57404422312886));
#23253=CARTESIAN_POINT('Ctrl Pts',(7.24355099965782,0.950261970649094,-1.73201325005114));
#23254=CARTESIAN_POINT('Ctrl Pts',(6.82217792133075,-2.6134110482692,-1.88998227697345));
#23255=CARTESIAN_POINT('Ctrl Pts',(4.75478586103601,-5.5465340811355,-2.04795130389573));
#23256=CARTESIAN_POINT('Ctrl Pts',(1.54018423325358,-7.14141872635569,-2.20592033081802));
#23257=CARTESIAN_POINT('Ctrl Pts',(-2.04602489478722,-7.0132596577781,-2.36388935774031));
#23258=CARTESIAN_POINT('Ctrl Pts',(-5.01110659443209,-5.26800938017539,
-2.51534699073651));
#23259=CARTESIAN_POINT('Ctrl Pts',(-6.21784576943405,-3.39432725900993,
-2.61414828142529));
#23260=CARTESIAN_POINT('Ctrl Pts',(-6.5726191009646,-2.44202878202201,-2.66029322980663));
#23261=CARTESIAN_POINT('Origin',(0.,0.,0.));
#23262=CARTESIAN_POINT('',(-6.57227158383948,-2.44189942273553,-4.66062920490781));
#23263=CARTESIAN_POINT('',(-6.57227159525839,-2.44189939200201,-4.11323059144668));
#23264=CARTESIAN_POINT('',(-6.57227159525839,-2.441899392002,0.));
#23265=CARTESIAN_POINT('',(-7.01124999966544,-6.84931509963988E-5,-2.22646564448509));
#23266=CARTESIAN_POINT('Ctrl Pts',(-6.57227159525839,-2.44189939200201,
-4.11323059144668));
#23267=CARTESIAN_POINT('Ctrl Pts',(-6.57127504206402,-2.44458157386175,
-4.11310064298898));
#23268=CARTESIAN_POINT('Ctrl Pts',(-6.57027684974964,-2.447263138134,-4.11297069453128));
#23269=CARTESIAN_POINT('Ctrl Pts',(-6.5692770191055,-2.44994408278074,-4.11284074607358));
#23270=CARTESIAN_POINT('Ctrl Pts',(-6.50362858156447,-2.62597372162417,
-4.10430838785975));
#23271=CARTESIAN_POINT('Ctrl Pts',(-6.43088970711211,-2.79939283689036,
-4.09577602964593));
#23272=CARTESIAN_POINT('Ctrl Pts',(-6.35129333024236,-2.96962953846418,
-4.08724367143211));
#23273=CARTESIAN_POINT('Ctrl Pts',(-6.27171185809064,-3.13983436258157,
-4.07871291093415));
#23274=CARTESIAN_POINT('Ctrl Pts',(-6.1852755756442,-3.30685768517568,-4.07018215043618));
#23275=CARTESIAN_POINT('Ctrl Pts',(-6.09226482886828,-3.47014925002291,
-4.06165138993822));
#23276=CARTESIAN_POINT('Ctrl Pts',(-5.99524674039942,-3.64047618571277,
-4.05275308403931));
#23277=CARTESIAN_POINT('Ctrl Pts',(-5.89107527475381,-3.80674235923873,
-4.0438547781404));
#23278=CARTESIAN_POINT('Ctrl Pts',(-5.78012132077499,-3.96835281692825,
-4.03495647224149));
#23279=CARTESIAN_POINT('Ctrl Pts',(-5.67375361316515,-4.12328315779282,
-4.02642597498441));
#23280=CARTESIAN_POINT('Ctrl Pts',(-5.56115303293323,-4.27393466016442,
-4.01789547772733));
#23281=CARTESIAN_POINT('Ctrl Pts',(-5.44269029911535,-4.41981321668865,
-4.00936498047026));
#23282=CARTESIAN_POINT('Ctrl Pts',(-5.32422635300546,-4.56569326606555,
-4.00083439591608));
#23283=CARTESIAN_POINT('Ctrl Pts',(-5.19990032883057,-4.70680003650741,
-3.9923038113619));
#23284=CARTESIAN_POINT('Ctrl Pts',(-5.07012317901512,-4.84267255883707,
-3.98377322680771));
#23285=CARTESIAN_POINT('Ctrl Pts',(-4.94032034929951,-4.97857196720032,
-3.9752409542479));
#23286=CARTESIAN_POINT('Ctrl Pts',(-4.8050644516411,-5.10923483821213,-3.96670868168809));
#23287=CARTESIAN_POINT('Ctrl Pts',(-4.66480383944429,-5.23423649656813,
-3.95817640912828));
#23288=CARTESIAN_POINT('Ctrl Pts',(-4.64669542280057,-5.25037489832764,
-3.95707484580262));
#23289=CARTESIAN_POINT('Ctrl Pts',(-4.6285036344999,-5.26641899021432,-3.95597328247695));
#23290=CARTESIAN_POINT('Ctrl Pts',(-4.61022948153129,-5.28236790560064,
-3.95487171915129));
#23291=CARTESIAN_POINT('Ctrl Pts',(-4.4686837205656,-5.40590311781067,-3.94633936093745));
#23292=CARTESIAN_POINT('Ctrl Pts',(-4.32214590192658,-5.52376660284747,
-3.9378070027236));
#23293=CARTESIAN_POINT('Ctrl Pts',(-4.17109316649515,-5.63556637428018,
-3.92927464450976));
#23294=CARTESIAN_POINT('Ctrl Pts',(-4.02006871625134,-5.74734521078907,
-3.92074388401179));
#23295=CARTESIAN_POINT('Ctrl Pts',(-3.86453128223555,-5.85306241768264,
-3.91221312351381));
#23296=CARTESIAN_POINT('Ctrl Pts',(-3.70498939617103,-5.95236760766338,
-3.90368236301584));
#23297=CARTESIAN_POINT('Ctrl Pts',(-3.53857369311297,-6.05595133364036,
-3.89478405711694));
#23298=CARTESIAN_POINT('Ctrl Pts',(-3.36780111999451,-6.15255807762932,
-3.88588575121803));
#23299=CARTESIAN_POINT('Ctrl Pts',(-3.19328111137226,-6.24184125929627,
-3.87698744531913));
#23300=CARTESIAN_POINT('Ctrl Pts',(-3.02597483175353,-6.32743394906945,
-3.86845694806207));
#23301=CARTESIAN_POINT('Ctrl Pts',(-2.85522497701526,-6.40629618935039,
-3.859926450805));
#23302=CARTESIAN_POINT('Ctrl Pts',(-2.68159281415117,-6.47816999943602,
-3.85139595354794));
#23303=CARTESIAN_POINT('Ctrl Pts',(-2.50795887441577,-6.550044545045,-3.84286536899371));
#23304=CARTESIAN_POINT('Ctrl Pts',(-2.33144285156541,-6.61493040351321,
-3.83433478443948));
#23305=CARTESIAN_POINT('Ctrl Pts',(-2.15262561350206,-6.67261789184686,
-3.82580419988525));
#23306=CARTESIAN_POINT('Ctrl Pts',(-1.9737729916391,-6.73031679520152,-3.81727192732544));
#23307=CARTESIAN_POINT('Ctrl Pts',(-1.79261853660246,-6.78081439051791,
-3.80873965476564));
#23308=CARTESIAN_POINT('Ctrl Pts',(-1.60975872389551,-6.82395071885358,
-3.80020738220584));
#23309=CARTESIAN_POINT('Ctrl Pts',(-1.58615051611798,-6.82951985614533,
-3.79910581888022));
#23310=CARTESIAN_POINT('Ctrl Pts',(-1.56251390031448,-6.83496636322321,
-3.79800425555461));
#23311=CARTESIAN_POINT('Ctrl Pts',(-1.5388501746405,-6.84028995748783,-3.796902692229));
#23312=CARTESIAN_POINT('Ctrl Pts',(-1.35555850231488,-6.88152482088126,
-3.78837033401517));
#23313=CARTESIAN_POINT('Ctrl Pts',(-1.17057760880854,-6.91539519781984,
-3.77983797580134));
#23314=CARTESIAN_POINT('Ctrl Pts',(-0.984513719362953,-6.94178358196841,
-3.77130561758751));
#23315=CARTESIAN_POINT('Ctrl Pts',(-0.798484671074311,-6.96816702479367,
-3.76277485708957));
#23316=CARTESIAN_POINT('Ctrl Pts',(-0.611373334375636,-6.9870712278236,
-3.75424409659162));
#23317=CARTESIAN_POINT('Ctrl Pts',(-0.423793730905451,-6.99843021227941,
-3.74571333609368));
#23318=CARTESIAN_POINT('Ctrl Pts',(-0.228132313324107,-7.01027859536474,
-3.73681503019477));
#23319=CARTESIAN_POINT('Ctrl Pts',(-0.0319617353477988,-7.01391714592579,
-3.72791672429585));
#23320=CARTESIAN_POINT('Ctrl Pts',(0.164017063898131,-7.00933127803575,
-3.71901841839694));
#23321=CARTESIAN_POINT('Ctrl Pts',(0.351895141860959,-7.00493496553517,
-3.71048792113986));
#23322=CARTESIAN_POINT('Ctrl Pts',(0.539596649861354,-6.9929804797751,-3.70195742388278));
#23323=CARTESIAN_POINT('Ctrl Pts',(0.726505192477673,-6.97350821092246,
-3.6934269266257));
#23324=CARTESIAN_POINT('Ctrl Pts',(0.913415647828903,-6.9540357427997,-3.68489634207148));
#23325=CARTESIAN_POINT('Ctrl Pts',(1.09953281758467,-6.92704537277569,-3.67636575751727));
#23326=CARTESIAN_POINT('Ctrl Pts',(1.28424606709855,-6.89262929524299,-3.66783517296306));
#23327=CARTESIAN_POINT('Ctrl Pts',(1.46899586709716,-6.85820640756366,-3.65930290040324));
#23328=CARTESIAN_POINT('Ctrl Pts',(1.65234089137479,-6.81635493464919,-3.65077062784342));
#23329=CARTESIAN_POINT('Ctrl Pts',(1.83368045678168,-6.76721822796612,-3.6422383552836));
#23330=CARTESIAN_POINT('Ctrl Pts',(1.85709239226987,-6.76087440882006,-3.64113679195797));
#23331=CARTESIAN_POINT('Ctrl Pts',(1.88047091801492,-6.75440922668806,-3.64003522863234));
#23332=CARTESIAN_POINT('Ctrl Pts',(1.90381475790691,-6.74782305118294,-3.63893366530671));
#23333=CARTESIAN_POINT('Ctrl Pts',(2.08462869697889,-6.6968086361591,-3.63040130709289));
#23334=CARTESIAN_POINT('Ctrl Pts',(2.26342145439287,-6.6385138397135,-3.62186894887907));
#23335=CARTESIAN_POINT('Ctrl Pts',(2.43960398736454,-6.57312398691331,-3.61333659066524));
#23336=CARTESIAN_POINT('Ctrl Pts',(2.61575352950025,-6.50774637860677,-3.6048058301673));
#23337=CARTESIAN_POINT('Ctrl Pts',(2.78929353586459,-6.43527647171821,-3.59627506966935));
#23338=CARTESIAN_POINT('Ctrl Pts',(2.95965264279496,-6.35594861499814,-3.5877443091714));
#23339=CARTESIAN_POINT('Ctrl Pts',(3.13735162361824,-6.27320294002925,-3.57884600327249));
#23340=CARTESIAN_POINT('Ctrl Pts',(3.31158920764571,-6.18299540694012,-3.56994769737357));
#23341=CARTESIAN_POINT('Ctrl Pts',(3.48174207006567,-6.08564694342638,-3.56104939147466));
#23342=CARTESIAN_POINT('Ctrl Pts',(3.64486171808,-5.99232234766433,-3.55251889421759));
#23343=CARTESIAN_POINT('Ctrl Pts',(3.80422725291596,-5.89243545091744,-3.54398839696053));
#23344=CARTESIAN_POINT('Ctrl Pts',(3.95931587134899,-5.78631526909691,-3.53545789970347));
#23345=CARTESIAN_POINT('Ctrl Pts',(4.11440607688664,-5.68019400129191,-3.52692731514927));
#23346=CARTESIAN_POINT('Ctrl Pts',(4.26521902786838,-5.56783949640685,-3.51839673059508));
#23347=CARTESIAN_POINT('Ctrl Pts',(4.41126165359899,-5.44962358204556,-3.50986614604088));
#23348=CARTESIAN_POINT('Ctrl Pts',(4.5573331777919,-5.3313842754854,-3.50133387348104));
#23349=CARTESIAN_POINT('Ctrl Pts',(4.69863225422026,-5.20728143622244,-3.49280160092121));
#23350=CARTESIAN_POINT('Ctrl Pts',(4.83469892173909,-5.07772713904901,-3.48426932836137));
#23351=CARTESIAN_POINT('Ctrl Pts',(4.85226587705268,-5.0610009665732,-3.48316776503572));
#23352=CARTESIAN_POINT('Ctrl Pts',(4.86974566578001,-5.04418398015829,-3.48206620171007));
#23353=CARTESIAN_POINT('Ctrl Pts',(4.8871373417498,-5.02727711245111,-3.48096463838442));
#23354=CARTESIAN_POINT('Ctrl Pts',(5.02184771732065,-4.89632190706907,-3.47243228017058));
#23355=CARTESIAN_POINT('Ctrl Pts',(5.15131416840792,-4.75992699719581,-3.46389992195674));
#23356=CARTESIAN_POINT('Ctrl Pts',(5.27510695580997,-4.61853582504946,-3.4553675637429));
#23357=CARTESIAN_POINT('Ctrl Pts',(5.39887656255142,-4.47717112892681,-3.44683680324492));
#23358=CARTESIAN_POINT('Ctrl Pts',(5.51697442431981,-4.33081226770075,-3.43830604274694));
#23359=CARTESIAN_POINT('Ctrl Pts',(5.62900969102896,-4.17993737522491,-3.42977528224896));
#23360=CARTESIAN_POINT('Ctrl Pts',(5.74587196548612,-4.02256208072073,-3.42087697635006));
#23361=CARTESIAN_POINT('Ctrl Pts',(5.85613743345589,-3.86027326013519,-3.41197867045116));
#23362=CARTESIAN_POINT('Ctrl Pts',(5.95941077695181,-3.69364992305045,-3.40308036455226));
#23363=CARTESIAN_POINT('Ctrl Pts',(6.05841534966832,-3.53391390856453,-3.39454986729517));
#23364=CARTESIAN_POINT('Ctrl Pts',(6.15099403854922,-3.37019478261854,-3.38601937003809));
#23365=CARTESIAN_POINT('Ctrl Pts',(6.2368437717621,-3.20303080365024,-3.37748887278101));
#23366=CARTESIAN_POINT('Ctrl Pts',(6.32269438352104,-3.03586511400389,-3.3689582882268));
#23367=CARTESIAN_POINT('Ctrl Pts',(6.40181576510515,-2.86525477455143,-3.3604277036726));
#23368=CARTESIAN_POINT('Ctrl Pts',(6.47395137525816,-2.69176153351164,-3.3518971191184));
#23369=CARTESIAN_POINT('Ctrl Pts',(6.54610125938249,-2.51823396216619,-3.34336484655852));
#23370=CARTESIAN_POINT('Ctrl Pts',(6.61126249463669,-2.34182263278763,-3.33483257399864));
#23371=CARTESIAN_POINT('Ctrl Pts',(6.66922681887129,-2.16310892026914,-3.32630030143876));
#23372=CARTESIAN_POINT('Ctrl Pts',(6.67671033200553,-2.1400359968363,-3.32519873811322));
#23373=CARTESIAN_POINT('Ctrl Pts',(6.68407395280301,-2.11692471961782,-3.32409717478768));
#23374=CARTESIAN_POINT('Ctrl Pts',(6.69131729331829,-2.09377635927041,-3.32299561146213));
#23375=CARTESIAN_POINT('Ctrl Pts',(6.74742189893471,-1.91447654239467,-3.3144632532483));
#23376=CARTESIAN_POINT('Ctrl Pts',(6.79632506358751,-1.73289016106787,-3.30593089503446));
#23377=CARTESIAN_POINT('Ctrl Pts',(6.83786003685788,-1.54961178326768,-3.29739853682063));
#23378=CARTESIAN_POINT('Ctrl Pts',(6.87938723254975,-1.36636772502653,-3.28886777632266));
#23379=CARTESIAN_POINT('Ctrl Pts',(6.91354892267587,-1.1814326008848,-3.28033701582468));
#23380=CARTESIAN_POINT('Ctrl Pts',(6.94022907296669,-0.995412968193562,
-3.27180625532671));
#23381=CARTESIAN_POINT('Ctrl Pts',(6.96805872997944,-0.80137873229134,-3.26290794942781));
#23382=CARTESIAN_POINT('Ctrl Pts',(6.98774781336841,-0.606164811914298,
-3.2540096435289));
#23383=CARTESIAN_POINT('Ctrl Pts',(6.99922439220387,-0.410468598163639,
-3.24511133762999));
#23384=CARTESIAN_POINT('Ctrl Pts',(7.01022659030634,-0.222861425115102,
-3.23658084037295));
#23385=CARTESIAN_POINT('Ctrl Pts',(7.01368153715842,-0.0348113541834391,
-3.2280503431159));
#23386=CARTESIAN_POINT('Ctrl Pts',(7.00957901588756,0.153063981814104,-3.21951984585885));
#23387=CARTESIAN_POINT('Ctrl Pts',(7.0054764526334,0.340941240440978,-3.21098926130463));
#23388=CARTESIAN_POINT('Ctrl Pts',(6.99381627662711,0.528643454725836,-3.20245867675042));
#23389=CARTESIAN_POINT('Ctrl Pts',(6.97464037296792,0.715554491472127,-3.1939280921962));
#23390=CARTESIAN_POINT('Ctrl Pts',(6.9554606748404,0.902502513594548,-3.18539581963638));
#23391=CARTESIAN_POINT('Ctrl Pts',(6.92876231094879,1.08865874120466,-3.17686354707656));
#23392=CARTESIAN_POINT('Ctrl Pts',(6.89463896652825,1.27341277036565,-3.16833127451674));
#23393=CARTESIAN_POINT('Ctrl Pts',(6.89023345504253,1.29726553190831,-3.1672297111911));
#23394=CARTESIAN_POINT('Ctrl Pts',(6.88570425245799,1.32109493328478,-3.16612814786547));
#23395=CARTESIAN_POINT('Ctrl Pts',(6.88105162265645,1.34489967240575,-3.16502658453984));
#23396=CARTESIAN_POINT('Ctrl Pts',(6.84501383601325,1.52928358991725,-3.15649422632601));
#23397=CARTESIAN_POINT('Ctrl Pts',(6.80155461748795,1.71224924167072,-3.14796186811218));
#23398=CARTESIAN_POINT('Ctrl Pts',(6.75081043810302,1.89319438814383,-3.13942950989834));
#23399=CARTESIAN_POINT('Ctrl Pts',(6.70007576075442,2.07410565196526,-3.13089874940032));
#23400=CARTESIAN_POINT('Ctrl Pts',(6.64205892744768,2.25299687105402,-3.1223679889023));
#23401=CARTESIAN_POINT('Ctrl Pts',(6.57694671586432,2.42927941150901,-3.11383722840428));
#23402=CARTESIAN_POINT('Ctrl Pts',(6.50902916307913,2.61315703531129,-3.10493892250538));
#23403=CARTESIAN_POINT('Ctrl Pts',(6.43339138405314,2.79419587395531,-3.09604061660649));
#23404=CARTESIAN_POINT('Ctrl Pts',(6.35030219002736,2.97174841765478,-3.0871423107076));
#23405=CARTESIAN_POINT('Ctrl Pts',(6.27064746138764,3.14196188347907,-3.07861181345052));
#23406=CARTESIAN_POINT('Ctrl Pts',(6.18414507491995,3.30897117355236,-3.07008131619344));
#23407=CARTESIAN_POINT('Ctrl Pts',(6.09108013378454,3.47222829985521,-3.06155081893637));
#23408=CARTESIAN_POINT('Ctrl Pts',(5.99801424026553,3.63548709685601,-3.05302023438212));
#23409=CARTESIAN_POINT('Ctrl Pts',(5.89838581222268,3.79499338913906,-3.04448964982788));
#23410=CARTESIAN_POINT('Ctrl Pts',(5.79252505529564,3.95022531588672,-3.03595906527364));
#23411=CARTESIAN_POINT('Ctrl Pts',(5.68664335097022,4.10548795944676,-3.02742679271377));
#23412=CARTESIAN_POINT('Ctrl Pts',(5.57452702786904,4.25647429593832,-3.0188945201539));
#23413=CARTESIAN_POINT('Ctrl Pts',(5.45654911473421,4.40269216741227,-3.01036224759404));
#23414=CARTESIAN_POINT('Ctrl Pts',(5.44131751712455,4.42156969899809,-3.00926068426854));
#23415=CARTESIAN_POINT('Ctrl Pts',(5.42598827318772,4.44036779268315,-3.00815912094305));
#23416=CARTESIAN_POINT('Ctrl Pts',(5.41056223496481,4.4590854291068,-3.00705755761755));
#23417=CARTESIAN_POINT('Ctrl Pts',(5.2910770624906,4.60406627150271,-2.99852519940372));
#23418=CARTESIAN_POINT('Ctrl Pts',(5.16574107102182,4.74426620958732,-2.98999284118989));
#23419=CARTESIAN_POINT('Ctrl Pts',(5.03496102601622,4.87922063745817,-2.98146048297606));
#23420=CARTESIAN_POINT('Ctrl Pts',(4.90420547006126,5.01414979460965,-2.97292972247809));
#23421=CARTESIAN_POINT('Ctrl Pts',(4.76800810780415,5.14383518209711,-2.96439896198012));
#23422=CARTESIAN_POINT('Ctrl Pts',(4.62681346414701,5.26784811194172,-2.95586820148215));
#23423=CARTESIAN_POINT('Ctrl Pts',(4.47953548924109,5.39720410375976,-2.94696989558324));
#23424=CARTESIAN_POINT('Ctrl Pts',(4.32682033080478,5.52038776784499,-2.93807158968433));
#23425=CARTESIAN_POINT('Ctrl Pts',(4.16921268489638,5.63695770346019,-2.92917328378543));
#23426=CARTESIAN_POINT('Ctrl Pts',(4.01811970086244,5.7487092578929,-2.92064278652837));
#23427=CARTESIAN_POINT('Ctrl Pts',(3.86253081906203,5.85438264950738,-2.91211228927132));
#23428=CARTESIAN_POINT('Ctrl Pts',(3.70295767450657,5.95363175073105,-2.90358179201426));
#23429=CARTESIAN_POINT('Ctrl Pts',(3.54338289695334,6.05288186762413,-2.89505120746004));
#23430=CARTESIAN_POINT('Ctrl Pts',(3.37982403670182,6.14570740390164,-2.88652062290582));
#23431=CARTESIAN_POINT('Ctrl Pts',(3.21281994966298,6.23180668294096,-2.8779900383516));
#23432=CARTESIAN_POINT('Ctrl Pts',(3.0457828163744,6.31792299903804,-2.86945776579182));
#23433=CARTESIAN_POINT('Ctrl Pts',(2.87529936711953,6.39731026024745,-2.86092549323204));
#23434=CARTESIAN_POINT('Ctrl Pts',(2.70193197174684,6.4697132998729,-2.85239322067226));
#23435=CARTESIAN_POINT('Ctrl Pts',(2.67954928726617,6.47906093059604,-2.85129165734659));
#23436=CARTESIAN_POINT('Ctrl Pts',(2.65711856081897,6.48829221204009,-2.85019009402093));
#23437=CARTESIAN_POINT('Ctrl Pts',(2.63464102702961,6.49740665351896,-2.84908853069526));
#23438=CARTESIAN_POINT('Ctrl Pts',(2.46053721875456,6.5680042104681,-2.84055617248142));
#23439=CARTESIAN_POINT('Ctrl Pts',(2.28356485901358,6.6316117358416,-2.83202381426759));
#23440=CARTESIAN_POINT('Ctrl Pts',(2.1043028654829,6.68801435501005,-2.82349145605375));
#23441=CARTESIAN_POINT('Ctrl Pts',(1.92507443942696,6.74440641257837,-2.81496069555571));
#23442=CARTESIAN_POINT('Ctrl Pts',(1.74355752694815,6.79359616454269,-2.80642993505767));
#23443=CARTESIAN_POINT('Ctrl Pts',(1.56034714755351,6.83541830041305,-2.79789917455963));
#23444=CARTESIAN_POINT('Ctrl Pts',(1.36924320083274,6.8790423311668,-2.78900086866074));
#23445=CARTESIAN_POINT('Ctrl Pts',(1.17629696815757,6.91464971818105,-2.78010256276186));
#23446=CARTESIAN_POINT('Ctrl Pts',(0.982197609021416,6.94211166860147,-2.77120425686297));
#23447=CARTESIAN_POINT('Ctrl Pts',(0.796121285109166,6.96843848804298,-2.76267375960589));
#23448=CARTESIAN_POINT('Ctrl Pts',(0.608985569910114,6.98727966455462,-2.75414326234881));
#23449=CARTESIAN_POINT('Ctrl Pts',(0.421405185699195,6.99857444283947,-2.74561276509173));
#23450=CARTESIAN_POINT('Ctrl Pts',(0.233822881879344,7.00986933670975,-2.73708218053757));
#23451=CARTESIAN_POINT('Ctrl Pts',(0.045796205574106,7.01361766287508,-2.72855159598342));
#23452=CARTESIAN_POINT('Ctrl Pts',(-0.142057349336477,7.00981071584672,
-2.72002101142927));
#23453=CARTESIAN_POINT('Ctrl Pts',(-0.329948076126833,7.00600301551147,
-2.71148873886946));
#23454=CARTESIAN_POINT('Ctrl Pts',(-0.517665307197656,6.99463706321847,
-2.70295646630965));
#23455=CARTESIAN_POINT('Ctrl Pts',(-0.704593017214773,6.97575624879426,
-2.69442419374983));
#23456=CARTESIAN_POINT('Ctrl Pts',(-0.728726412913724,6.97331863178405,
-2.69332263042421));
#23457=CARTESIAN_POINT('Ctrl Pts',(-0.752846654907111,6.9707558262547,-2.69222106709859));
#23458=CARTESIAN_POINT('Ctrl Pts',(-0.776952423870934,6.96806798858486,
-2.69111950377297));
#23459=CARTESIAN_POINT('Ctrl Pts',(-0.963668022544028,6.94724885518932,
-2.68258714555912));
#23460=CARTESIAN_POINT('Ctrl Pts',(-1.14957779623874,6.91891708077707,-2.67405478734527));
#23461=CARTESIAN_POINT('Ctrl Pts',(-1.3340703532533,6.88315936580511,-2.66552242913141));
#23462=CARTESIAN_POINT('Ctrl Pts',(-1.51852836334871,6.8474083465986,-2.65699166863345));
#23463=CARTESIAN_POINT('Ctrl Pts',(-1.70156938609551,6.80423422002569,-2.64846090813548));
#23464=CARTESIAN_POINT('Ctrl Pts',(-1.88259147053926,6.75377493832544,-2.63993014763752));
#23465=CARTESIAN_POINT('Ctrl Pts',(-2.0714128402427,6.7011416327585,-2.63103184173861));
#23466=CARTESIAN_POINT('Ctrl Pts',(-2.25803710131995,6.64058158081811,-2.62213353583971));
#23467=CARTESIAN_POINT('Ctrl Pts',(-2.44179690759758,6.57230967199103,-2.61323522994081));
#23468=CARTESIAN_POINT('Ctrl Pts',(-2.61796106077668,6.50685976078319,-2.60470473268375));
#23469=CARTESIAN_POINT('Ctrl Pts',(-2.79149249444014,6.43432282284169,-2.59617423542669));
#23470=CARTESIAN_POINT('Ctrl Pts',(-2.96182171598655,6.35493813386177,-2.58764373816963));
#23471=CARTESIAN_POINT('Ctrl Pts',(-3.13215268060353,6.27555263249561,-2.57911315361541));
#23472=CARTESIAN_POINT('Ctrl Pts',(-3.2992810916516,6.18931937224999,-2.57058256906118));
#23473=CARTESIAN_POINT('Ctrl Pts',(-3.46265980293689,6.09652471918429,-2.56205198450695));
#23474=CARTESIAN_POINT('Ctrl Pts',(-3.62607084309448,6.00371170420065,-2.55351971194713));
#23475=CARTESIAN_POINT('Ctrl Pts',(-3.78573043597567,5.90433485521893,-2.54498743938731));
#23476=CARTESIAN_POINT('Ctrl Pts',(-3.94111753209282,5.79872564972086,-2.53645516682749));
#23477=CARTESIAN_POINT('Ctrl Pts',(-3.96117886102417,5.78509092030885,-2.53535360350189));
#23478=CARTESIAN_POINT('Ctrl Pts',(-3.98116901423432,5.77135236796101,-2.53425204017628));
#23479=CARTESIAN_POINT('Ctrl Pts',(-4.00108690601917,5.75751075839046,-2.53315047685068));
#23480=CARTESIAN_POINT('Ctrl Pts',(-4.15536454364832,5.6502980649691,-2.52461811863684));
#23481=CARTESIAN_POINT('Ctrl Pts',(-4.30535640504065,5.5368627313533,-2.516085760423));
#23482=CARTESIAN_POINT('Ctrl Pts',(-4.45056613782287,5.41757211445907,-2.50755340220916));
#23483=CARTESIAN_POINT('Ctrl Pts',(-4.59574867954287,5.29830383517625,-2.49902264171111));
#23484=CARTESIAN_POINT('Ctrl Pts',(-4.73615064335071,5.17318265482241,-2.49049188121306));
#23485=CARTESIAN_POINT('Ctrl Pts',(-4.87130838238491,5.04261650397951,-2.48196112071501));
#23486=CARTESIAN_POINT('Ctrl Pts',(-5.01228935433964,4.90642494749334,-2.47306281481613));
#23487=CARTESIAN_POINT('Ctrl Pts',(-5.14756392982854,4.76430906541191,-2.46416450891724));
#23488=CARTESIAN_POINT('Ctrl Pts',(-5.27664758975097,4.61677558216503,-2.45526620301836));
#23489=CARTESIAN_POINT('Ctrl Pts',(-5.40039561768075,4.47534034848493,-2.44673570576127));
#23490=CARTESIAN_POINT('Ctrl Pts',(-5.51845402392328,4.32892662456899,-2.43820520850419));
#23491=CARTESIAN_POINT('Ctrl Pts',(-5.63043594971143,4.17801598593126,-2.4296747112471));
#23492=CARTESIAN_POINT('Ctrl Pts',(-5.74241902147132,4.02710380294318,-2.42114412669281));
#23493=CARTESIAN_POINT('Ctrl Pts',(-5.84832530878325,3.87169486092134,-2.41261354213852));
#23494=CARTESIAN_POINT('Ctrl Pts',(-5.94781002567736,3.71230150458605,-2.40408295758424));
#23495=CARTESIAN_POINT('Ctrl Pts',(-6.04731442829802,3.55287660798887,-2.39555068502439));
#23496=CARTESIAN_POINT('Ctrl Pts',(-6.14039456142936,3.3894659824808,-2.38701841246455));
#23497=CARTESIAN_POINT('Ctrl Pts',(-6.22675006749305,3.22260921606627,-2.37848613990471));
#23498=CARTESIAN_POINT('Ctrl Pts',(-6.23789903838709,3.20106708960527,-2.37738457657927));
#23499=CARTESIAN_POINT('Ctrl Pts',(-6.24893598444566,3.1794675556402,-2.37628301325383));
#23500=CARTESIAN_POINT('Ctrl Pts',(-6.25986031553744,3.1578118044715,-2.37518144992838));
#23501=CARTESIAN_POINT('Ctrl Pts',(-6.34428116655006,2.99046087674696,-2.3666688085047));
#23502=CARTESIAN_POINT('Ctrl Pts',(-6.42200273866975,2.81969184675183,-2.35815616708101));
#23503=CARTESIAN_POINT('Ctrl Pts',(-6.49276411959083,2.64606134657796,-2.34964352565732));
#23504=CARTESIAN_POINT('Ctrl Pts',(-6.56351169396974,2.47246472416044,-2.34113254516988));
#23505=CARTESIAN_POINT('Ctrl Pts',(-6.62730167060251,2.296008031561,-2.33262156468244));
#23506=CARTESIAN_POINT('Ctrl Pts',(-6.68392119685633,2.11726805027485,-2.324110584195));
#23507=CARTESIAN_POINT('Ctrl Pts',(-6.74054189011732,1.93852438490915,-2.31559942828442));
#23508=CARTESIAN_POINT('Ctrl Pts',(-6.78999174023709,1.75749762994793,-2.30708827237384));
#23509=CARTESIAN_POINT('Ctrl Pts',(-6.83210744490193,1.57478075420538,-2.29857711646326));
#23510=CARTESIAN_POINT('Ctrl Pts',(-6.87422073043193,1.39207437375816,-2.29006644943524));
#23511=CARTESIAN_POINT('Ctrl Pts',(-6.90900064431342,1.20767836785345,-2.28155578240723));
#23512=CARTESIAN_POINT('Ctrl Pts',(-6.9363347135591,1.02219729209926,-2.27304511537921));
#23513=CARTESIAN_POINT('Ctrl Pts',(-6.96367525103699,0.836672324794936,
-2.26453243441869));
#23514=CARTESIAN_POINT('Ctrl Pts',(-6.98356637669238,0.650062080119472,
-2.25601975345816));
#23515=CARTESIAN_POINT('Ctrl Pts',(-6.99594720559743,0.462978680927659,
-2.24750707249764));
#23516=CARTESIAN_POINT('Ctrl Pts',(-7.00614807812903,0.30883602032161,-2.24049326316012));
#23517=CARTESIAN_POINT('Ctrl Pts',(-7.01125150840371,0.154372366967734,
-2.2334794538226));
#23518=CARTESIAN_POINT('Ctrl Pts',(-7.01124999966544,-6.84931509963988E-5,
-2.22646564448509));
#23519=CARTESIAN_POINT('Ctrl Pts',(-7.01124999951636,-8.23516846733779E-5,
-2.22677279634694));
#23520=CARTESIAN_POINT('Ctrl Pts',(-7.01124880883069,-0.101454836867331,
-2.22219948827291));
#23521=CARTESIAN_POINT('Ctrl Pts',(-7.00904910995193,-0.202813406512794,
-2.21760633059935));
#23522=CARTESIAN_POINT('Ctrl Pts',(-6.99729784000022,-0.473502170309707,
-2.20525735769209));
#23523=CARTESIAN_POINT('Ctrl Pts',(-6.98379961971893,-0.642591040978516,
-2.19746942105447));
#23524=CARTESIAN_POINT('Ctrl Pts',(-6.93583102485646,-1.054493625703,-2.17839760819467));
#23525=CARTESIAN_POINT('Ctrl Pts',(-6.89472871351082,-1.29631268506705,
-2.16711896464435));
#23526=CARTESIAN_POINT('Ctrl Pts',(-6.8029333810765,-1.70528906870794,-2.14795172209859));
#23527=CARTESIAN_POINT('Ctrl Pts',(-6.75851063828571,-1.87361912106811,
-2.14003340177884));
#23528=CARTESIAN_POINT('Ctrl Pts',(-6.66672192903047,-2.17541791283756,
-2.12575233329747));
#23529=CARTESIAN_POINT('Ctrl Pts',(-6.62149981133014,-2.3094036699173,-2.1193806486438));
#23530=CARTESIAN_POINT('Ctrl Pts',(-6.57227163721606,-2.44189927907466,
-2.11302806574593));
#23531=CARTESIAN_POINT('',(-7.01074934648484,9.37578675265012E-5,-2.77353775949927));
#23532=CARTESIAN_POINT('Ctrl Pts',(-6.5726191009646,-2.44202878202201,-2.66029322980663));
#23533=CARTESIAN_POINT('Ctrl Pts',(-6.62268024518726,-2.30765241502215,
-2.66680462373271));
#23534=CARTESIAN_POINT('Ctrl Pts',(-6.88878358359034,-1.51975160196419,
-2.70455166610063));
#23535=CARTESIAN_POINT('Ctrl Pts',(-7.01041463086307,-0.688046937181739,
-2.74229870846854));
#23536=CARTESIAN_POINT('Ctrl Pts',(-7.01074344146299,9.39112607581394E-5,
-2.77353435691037));
#23537=CARTESIAN_POINT('Ctrl Pts',(-7.01124999953497,8.07525321924046E-5,
-2.77382624556319));
#23538=CARTESIAN_POINT('Ctrl Pts',(-7.01124590840154,0.355288923246704,
-2.78984771974093));
#23539=CARTESIAN_POINT('Ctrl Pts',(-6.98424833394108,0.709982097587371,
-2.80566510602609));
#23540=CARTESIAN_POINT('Ctrl Pts',(-6.91597066131533,1.15593282800845,-2.82595038395769));
#23541=CARTESIAN_POINT('Ctrl Pts',(-6.89950613365193,1.25045820016344,-2.83027522025353));
#23542=CARTESIAN_POINT('Ctrl Pts',(-6.86186625834546,1.44308137055211,-2.83916825388826));
#23543=CARTESIAN_POINT('Ctrl Pts',(-6.8405143033683,1.54112161527904,-2.84374089258977));
#23544=CARTESIAN_POINT('Ctrl Pts',(-6.7310378686837,1.99655729969631,-2.86517247507147));
#23545=CARTESIAN_POINT('Ctrl Pts',(-6.61695979443096,2.34711706640564,-2.88217334921628));
#23546=CARTESIAN_POINT('Ctrl Pts',(-6.40928460343441,2.84761270848719,-2.90695326912895));
#23547=CARTESIAN_POINT('Ctrl Pts',(-6.33673573359343,3.00559624128286,-2.91486072610223));
#23548=CARTESIAN_POINT('Ctrl Pts',(-6.12058121892723,3.43359319367885,-2.93656920662926));
#23549=CARTESIAN_POINT('Ctrl Pts',(-5.96507201325998,3.69716048636172,-2.9502531876902));
#23550=CARTESIAN_POINT('Ctrl Pts',(-5.7085545283741,4.07338018707437,-2.97065443723908));
#23551=CARTESIAN_POINT('Ctrl Pts',(-5.62031524539495,4.19429099361423,-2.97736005047625));
#23552=CARTESIAN_POINT('Ctrl Pts',(-5.47329443792854,4.38276916253252,-2.98813117667118));
#23553=CARTESIAN_POINT('Ctrl Pts',(-5.41697090112093,4.45219536837568,-2.99217187593043));
#23554=CARTESIAN_POINT('Ctrl Pts',(-5.26723793930212,4.62971217807466,-3.00272606466486));
#23555=CARTESIAN_POINT('Ctrl Pts',(-5.17182587978082,4.7360581267113,-3.00926771045137));
#23556=CARTESIAN_POINT('Ctrl Pts',(-4.89653443268444,5.02465044725512,-3.02758473970247));
#23557=CARTESIAN_POINT('Ctrl Pts',(-4.70982173006713,5.20007134358355,-3.03938128910531));
#23558=CARTESIAN_POINT('Ctrl Pts',(-4.36289807132683,5.49196762218392,-3.06015693190967));
#23559=CARTESIAN_POINT('Ctrl Pts',(-4.20656074624372,5.6126140457021,-3.06915550734746));
#23560=CARTESIAN_POINT('Ctrl Pts',(-3.84119904084998,5.8707143072342,-3.08943122255127));
#23561=CARTESIAN_POINT('Ctrl Pts',(-3.62949137987601,6.00390634861941,-3.10065985685495));
#23562=CARTESIAN_POINT('Ctrl Pts',(-3.24022587235689,6.2206772305833,-3.12063134823794));
#23563=CARTESIAN_POINT('Ctrl Pts',(-3.06542261854953,6.30865060212891,-3.12937715772036));
#23564=CARTESIAN_POINT('Ctrl Pts',(-2.77487028879792,6.43994628684181,-3.14371708307237));
#23565=CARTESIAN_POINT('Ctrl Pts',(-2.66125173902792,6.48772318041217,-3.14927856377225));
#23566=CARTESIAN_POINT('Ctrl Pts',(-2.42324549258326,6.58050068012467,-3.16089431094035));
#23567=CARTESIAN_POINT('Ctrl Pts',(-2.29872442284727,6.62502628419134,-3.16694829616124));
#23568=CARTESIAN_POINT('Ctrl Pts',(-1.92645407201859,6.74638100654683,-3.18492674927493));
#23569=CARTESIAN_POINT('Ctrl Pts',(-1.67561647432196,6.81301640353276,-3.19687864983173));
#23570=CARTESIAN_POINT('Ctrl Pts',(-1.22755398574876,6.90579702552752,-3.21784800100911));
#23571=CARTESIAN_POINT('Ctrl Pts',(-1.03182343738932,6.93774196356555,-3.22688605427261));
#23572=CARTESIAN_POINT('Ctrl Pts',(-0.604916001749064,6.98894868852491,
-3.2463764626622));
#23573=CARTESIAN_POINT('Ctrl Pts',(-0.373602768797742,7.00512314699171,
-3.25679624392579));
#23574=CARTESIAN_POINT('Ctrl Pts',(0.0669087924883373,7.01404117675433,
-3.27655401677683));
#23575=CARTESIAN_POINT('Ctrl Pts',(0.275812978775597,7.00893550892242,-3.2858884782659));
#23576=CARTESIAN_POINT('Ctrl Pts',(0.610720721519649,6.98575243248526,-3.30098156573496));
#23577=CARTESIAN_POINT('Ctrl Pts',(0.737003415781903,6.97356023232605,-3.30670325664519));
#23578=CARTESIAN_POINT('Ctrl Pts',(1.01995213739006,6.93847056754246,-3.31966396866203));
#23579=CARTESIAN_POINT('Ctrl Pts',(1.17631346404718,6.91367932067892,-3.32691880099318));
#23580=CARTESIAN_POINT('Ctrl Pts',(1.57308583746265,6.83692003012535,-3.34548993018733));
#23581=CARTESIAN_POINT('Ctrl Pts',(1.81185013991261,6.77755670113293,-3.3568147244724));
#23582=CARTESIAN_POINT('Ctrl Pts',(2.23331267827011,6.64890120151752,-3.37700054401989));
#23583=CARTESIAN_POINT('Ctrl Pts',(2.417173939016,6.58428770560722,-3.38587769400206));
#23584=CARTESIAN_POINT('Ctrl Pts',(2.82317849638355,6.42230565229147,-3.40568503922625));
#23585=CARTESIAN_POINT('Ctrl Pts',(3.0434445300554,6.32090139619768,-3.41657212340553));
#23586=CARTESIAN_POINT('Ctrl Pts',(3.43282994590629,6.11655782431705,-3.43628437358597));
#23587=CARTESIAN_POINT('Ctrl Pts',(3.60368684859317,6.01747800099115,-3.44511064157775));
#23588=CARTESIAN_POINT('Ctrl Pts',(3.87445847834976,5.84478475332479,-3.45955387390316));
#23589=CARTESIAN_POINT('Ctrl Pts',(3.97700284751861,5.77549870053841,-3.46513761179685));
#23590=CARTESIAN_POINT('Ctrl Pts',(4.18458889671162,5.62708810785398,-3.47674063443582));
#23591=CARTESIAN_POINT('Ctrl Pts',(4.28934664858187,5.54764900331619,-3.48275894099708));
#23592=CARTESIAN_POINT('Ctrl Pts',(4.59451236575126,5.30242438790547,-3.5007335426723));
#23593=CARTESIAN_POINT('Ctrl Pts',(4.78799873685138,5.12838351370287,-3.51271826026345));
#23594=CARTESIAN_POINT('Ctrl Pts',(5.1112759687563,4.80331652796788,-3.53372849666487));
#23595=CARTESIAN_POINT('Ctrl Pts',(5.24514957391362,4.65675847143009,-3.54277485582992));
#23596=CARTESIAN_POINT('Ctrl Pts',(5.613603857019,4.21731528101331,-3.5687707326019));
#23597=CARTESIAN_POINT('Ctrl Pts',(5.83113005358908,3.911038544606,-3.58551637652729));
#23598=CARTESIAN_POINT('Ctrl Pts',(6.11214632647117,3.43941097107539,-3.61013305077131));
#23599=CARTESIAN_POINT('Ctrl Pts',(6.19558667963229,3.28672857628575,-3.61794562952778));
#23600=CARTESIAN_POINT('Ctrl Pts',(6.32720452154977,3.02302822755733,-3.63131428558462));
#23601=CARTESIAN_POINT('Ctrl Pts',(6.37834442382916,2.91357825372106,-3.63683195242053));
#23602=CARTESIAN_POINT('Ctrl Pts',(6.53842567600284,2.54653112494688,-3.65518917141804));
#23603=CARTESIAN_POINT('Ctrl Pts',(6.63478458503777,2.28373934758444,-3.66808616614431));
#23604=CARTESIAN_POINT('Ctrl Pts',(6.77363529379773,1.8212109716682,-3.69022936149848));
#23605=CARTESIAN_POINT('Ctrl Pts',(6.82358617795048,1.62407453630684,-3.69950305917718));
#23606=CARTESIAN_POINT('Ctrl Pts',(6.9465810154549,1.03156856503938,-3.72694663545437));
#23607=CARTESIAN_POINT('Ctrl Pts',(6.99428024190498,0.631798167362091,-3.74486810024395));
#23608=CARTESIAN_POINT('Ctrl Pts',(7.01004353802653,0.151838302369994,-3.76641314522748));
#23609=CARTESIAN_POINT('Ctrl Pts',(7.01130258281483,0.0734932960740408,
-3.76993271995863));
#23610=CARTESIAN_POINT('Ctrl Pts',(7.01117112255727,-0.116314552547843,
-3.77848332036554));
#23611=CARTESIAN_POINT('Ctrl Pts',(7.00843618512526,-0.227753304968802,
-3.78352451643272));
#23612=CARTESIAN_POINT('Ctrl Pts',(6.99425056386765,-0.520729752687469,
-3.79688132570966));
#23613=CARTESIAN_POINT('Ctrl Pts',(6.97839108675056,-0.701966537763913,
-3.80523424939673));
#23614=CARTESIAN_POINT('Ctrl Pts',(6.92723979238907,-1.10517522002605,-3.82392767453972));
#23615=CARTESIAN_POINT('Ctrl Pts',(6.88828713330589,-1.32648597921271,-3.83426151654963));
#23616=CARTESIAN_POINT('Ctrl Pts',(6.79705512902356,-1.73017226468217,-3.85320338147652));
#23617=CARTESIAN_POINT('Ctrl Pts',(6.74787020651669,-1.91303522731362,-3.8618206509253));
#23618=CARTESIAN_POINT('Ctrl Pts',(6.60002304218254,-2.38554959743193,-3.88423786293243));
#23619=CARTESIAN_POINT('Ctrl Pts',(6.48970196677333,-2.67112758261271,-3.89792798567451));
#23620=CARTESIAN_POINT('Ctrl Pts',(6.27058880968273,-3.14382724641097,-3.92127111415586));
#23621=CARTESIAN_POINT('Ctrl Pts',(6.17115064055129,-3.33479102023564,-3.93091041485874));
#23622=CARTESIAN_POINT('Ctrl Pts',(6.00518975336127,-3.62058231883819,-3.94588798894772));
#23623=CARTESIAN_POINT('Ctrl Pts',(5.94484009525226,-3.71884332088699,-3.95114871237711));
#23624=CARTESIAN_POINT('Ctrl Pts',(5.72524171716036,-4.05737695954606,-3.96963228348334));
#23625=CARTESIAN_POINT('Ctrl Pts',(5.55362604195964,-4.28928186450089,-3.98292821331062));
#23626=CARTESIAN_POINT('Ctrl Pts',(5.23607603510089,-4.66726260484389,-4.00556885570729));
#23627=CARTESIAN_POINT('Ctrl Pts',(5.09707575743117,-4.8186775336576,-4.01494398407426));
#23628=CARTESIAN_POINT('Ctrl Pts',(4.66061568935461,-5.25406965953527,-4.04290743849807));
#23629=CARTESIAN_POINT('Ctrl Pts',(4.3446403335694,-5.51821441551957,-4.06123111974664));
#23630=CARTESIAN_POINT('Ctrl Pts',(3.88101915321531,-5.8411487479271,-4.08658577877555));
#23631=CARTESIAN_POINT('Ctrl Pts',(3.75182812168114,-5.92495679019439,-4.09351132361659));
#23632=CARTESIAN_POINT('Ctrl Pts',(3.50762965018205,-6.07218023984643,-4.10645361136492));
#23633=CARTESIAN_POINT('Ctrl Pts',(3.39339663625125,-6.13674970732486,-4.11245308486267));
#23634=CARTESIAN_POINT('Ctrl Pts',(3.03898543253231,-6.3241554297724,-4.13084726117303));
#23635=CARTESIAN_POINT('Ctrl Pts',(2.79347267554831,-6.4363720950731,-4.14328214501769));
#23636=CARTESIAN_POINT('Ctrl Pts',(2.35495418029332,-6.60697696924434,-4.16485208389484));
#23637=CARTESIAN_POINT('Ctrl Pts',(2.16475852466024,-6.67171464216146,-4.17401121538921));
#23638=CARTESIAN_POINT('Ctrl Pts',(1.58879316350656,-6.84053089277647,-4.20122486106248));
#23639=CARTESIAN_POINT('Ctrl Pts',(1.19664427648142,-6.91991130224887,-4.21903446986866));
#23640=CARTESIAN_POINT('Ctrl Pts',(0.722474742964915,-6.97436207109186,
-4.24044874187128));
#23641=CARTESIAN_POINT('Ctrl Pts',(0.644934006514725,-6.98195932946982,
-4.24394859196465));
#23642=CARTESIAN_POINT('Ctrl Pts',(0.456435757829557,-6.99726096939189,
-4.25246852491921));
#23643=CARTESIAN_POINT('Ctrl Pts',(0.345392108645162,-7.00362040021651,
-4.25749889277586));
#23644=CARTESIAN_POINT('Ctrl Pts',(0.0363132898915868,-7.01395237971942,
-4.27158177342206));
#23645=CARTESIAN_POINT('Ctrl Pts',(-0.161806438995436,-7.01217967974589,
-4.28068409025098));
#23646=CARTESIAN_POINT('Ctrl Pts',(-0.575782563090936,-6.99092029973489,
-4.29975245772036));
#23647=CARTESIAN_POINT('Ctrl Pts',(-0.791353721284571,-6.96981009452171,
-4.30970894112332));
#23648=CARTESIAN_POINT('Ctrl Pts',(-1.19088429473961,-6.91190793591781,
-4.32817799076764));
#23649=CARTESIAN_POINT('Ctrl Pts',(-1.37501749591971,-6.8776453216945,-4.33669720632862));
#23650=CARTESIAN_POINT('Ctrl Pts',(-1.79533658134681,-6.78187774416473,
-4.35620866809789));
#23651=CARTESIAN_POINT('Ctrl Pts',(-2.03012599702565,-6.71533243912823,
-4.36715313937824));
#23652=CARTESIAN_POINT('Ctrl Pts',(-2.43481472181455,-6.57746399831273,
-4.38631128582253));
#23653=CARTESIAN_POINT('Ctrl Pts',(-2.60626245536179,-6.51143231088565,
-4.39452635026103));
#23654=CARTESIAN_POINT('Ctrl Pts',(-2.88499622565634,-6.39130589228717,
-4.40818236147793));
#23655=CARTESIAN_POINT('Ctrl Pts',(-2.99383735568591,-6.3410513144667,-4.41359454885594));
#23656=CARTESIAN_POINT('Ctrl Pts',(-3.43256220124429,-6.12466663274223,
-4.435845953407));
#23657=CARTESIAN_POINT('Ctrl Pts',(-3.75036053482541,-5.93538707445485,
-4.45291872314849));
#23658=CARTESIAN_POINT('Ctrl Pts',(-4.21994097535676,-5.60287325244001,
-4.47930874630594));
#23659=CARTESIAN_POINT('Ctrl Pts',(-4.38278519575835,-5.47643008206499,
-4.48871313522633));
#23660=CARTESIAN_POINT('Ctrl Pts',(-4.71158148882153,-5.19705921583717,
-4.50828449058583));
#23661=CARTESIAN_POINT('Ctrl Pts',(-4.87620253288263,-5.04292332122871,
-4.51842816277566));
#23662=CARTESIAN_POINT('Ctrl Pts',(-5.2269186453325,-4.68128650424208,-4.54102913560914));
#23663=CARTESIAN_POINT('Ctrl Pts',(-5.40864681169705,-4.4700848913034,-4.55344650508219));
#23664=CARTESIAN_POINT('Ctrl Pts',(-5.60648153205455,-4.21038060508412,
-4.56817596372438));
#23665=CARTESIAN_POINT('Ctrl Pts',(-5.63523327615461,-4.17182045272179,
-4.57035015071541));
#23666=CARTESIAN_POINT('Ctrl Pts',(-5.73152086507164,-4.03987337155385,
-4.57775287863013));
#23667=CARTESIAN_POINT('Ctrl Pts',(-5.79714901358844,-3.94511985899341,
-4.58301117054901));
#23668=CARTESIAN_POINT('Ctrl Pts',(-6.01867157118361,-3.60781592309585,
-4.60149561129016));
#23669=CARTESIAN_POINT('Ctrl Pts',(-6.16191836365588,-3.35730634733075,
-4.61479498720285));
#23670=CARTESIAN_POINT('Ctrl Pts',(-6.38014051035421,-2.91438625547387,
-4.63743992604504));
#23671=CARTESIAN_POINT('Ctrl Pts',(-6.46280109794801,-2.72617756743884,
-4.64681593004686));
#23672=CARTESIAN_POINT('Ctrl Pts',(-6.54902910051275,-2.5037846095666,-4.65763515361273));
#23673=CARTESIAN_POINT('Ctrl Pts',(-6.56076062700498,-2.47288068830357,
-4.6591330043543));
#23674=CARTESIAN_POINT('Ctrl Pts',(-6.57227158383948,-2.44189942273553,
-4.6606292049078));
#23675=CARTESIAN_POINT('Origin',(0.,0.,0.));
#23676=CARTESIAN_POINT('',(-6.5722714983487,-2.44189965283043,-6.66023848729892));
#23677=CARTESIAN_POINT('',(-6.57227174271038,-2.44189899514102,-6.11302261786463));
#23678=CARTESIAN_POINT('',(-6.57227159525839,-2.441899392002,0.));
#23679=CARTESIAN_POINT('',(-7.0112499978881,0.00017208778304258,-4.22646564308965));
#23680=CARTESIAN_POINT('Ctrl Pts',(-6.57227174271038,-2.44189899514102,
-6.11302261786463));
#23681=CARTESIAN_POINT('Ctrl Pts',(-6.51134619784151,-2.60587761905121,
-6.105001908522));
#23682=CARTESIAN_POINT('Ctrl Pts',(-6.44427743276589,-2.76759301087802,
-6.09701124066779));
#23683=CARTESIAN_POINT('Ctrl Pts',(-6.28674107852913,-3.11053720106985,
-6.07986803322655));
#23684=CARTESIAN_POINT('Ctrl Pts',(-6.19437377980903,-3.29063676100689,
-6.07074150759056));
#23685=CARTESIAN_POINT('Ctrl Pts',(-5.95799008587052,-3.70621667689436,
-6.04925757833389));
#23686=CARTESIAN_POINT('Ctrl Pts',(-5.80760812360777,-3.93768648618198,
-6.03695396159107));
#23687=CARTESIAN_POINT('Ctrl Pts',(-5.56958851842973,-4.26063780837813,
-6.01891451978956));
#23688=CARTESIAN_POINT('Ctrl Pts',(-5.49249818474332,-4.35956580711916,
-6.01325719512312));
#23689=CARTESIAN_POINT('Ctrl Pts',(-5.30648224427145,-4.58550440909404,
-5.99995194459492));
#23690=CARTESIAN_POINT('Ctrl Pts',(-5.1955815240398,-4.71078931039558,-5.99228093501358));
#23691=CARTESIAN_POINT('Ctrl Pts',(-4.81412592909629,-5.11184836173482,
-5.96683880431027));
#23692=CARTESIAN_POINT('Ctrl Pts',(-4.5252675167531,-5.36924260197459,-5.94907212635811));
#23693=CARTESIAN_POINT('Ctrl Pts',(-4.05674090527729,-5.72193647333492,
-5.92242814067287));
#23694=CARTESIAN_POINT('Ctrl Pts',(-3.89171492337875,-5.83543147044556,
-5.91339449686395));
#23695=CARTESIAN_POINT('Ctrl Pts',(-3.49561843034168,-6.08355763852672,
-5.89238727747053));
#23696=CARTESIAN_POINT('Ctrl Pts',(-3.26125702234848,-6.21234447314634,
-5.88046267125955));
#23697=CARTESIAN_POINT('Ctrl Pts',(-2.89939337099132,-6.38506380215797,
-5.86244632528071));
#23698=CARTESIAN_POINT('Ctrl Pts',(-2.77704432500597,-6.4392193469182,-5.85641724528001));
#23699=CARTESIAN_POINT('Ctrl Pts',(-2.51462695486597,-6.54650266054002,
-5.84353642877551));
#23700=CARTESIAN_POINT('Ctrl Pts',(-2.37425336995916,-6.59870940216665,
-5.83667800574024));
#23701=CARTESIAN_POINT('Ctrl Pts',(-1.83443645159856,-6.7800175360291,-5.81052087636864));
#23702=CARTESIAN_POINT('Ctrl Pts',(-1.4253481344753,-6.87765879366356,-5.79119796203726));
#23703=CARTESIAN_POINT('Ctrl Pts',(-0.804366687127787,-6.96805541337416,
-5.76270493355499));
#23704=CARTESIAN_POINT('Ctrl Pts',(-0.597516053346675,-6.98883240744239,
-5.75333740374891));
#23705=CARTESIAN_POINT('Ctrl Pts',(-0.0324883748679699,-7.0203145014224,
-5.72792049107774));
#23706=CARTESIAN_POINT('Ctrl Pts',(0.326064777081194,-7.01281295085359,
-5.71199564948401));
#23707=CARTESIAN_POINT('Ctrl Pts',(0.795427355416544,-6.96690778708516,
-5.69062793359969));
#23708=CARTESIAN_POINT('Ctrl Pts',(0.908101270318745,-6.95311872462858,
-5.68545118332169));
#23709=CARTESIAN_POINT('Ctrl Pts',(1.18023373432557,-6.91308745378104,-5.67285514064947));
#23710=CARTESIAN_POINT('Ctrl Pts',(1.33921736221832,-6.88405594359876,-5.66542121935758));
#23711=CARTESIAN_POINT('Ctrl Pts',(1.7730509725222,-6.78923628398118,-5.64499243357249));
#23712=CARTESIAN_POINT('Ctrl Pts',(2.0451523321977,-6.71228688025453,-5.63202805724349));
#23713=CARTESIAN_POINT('Ctrl Pts',(2.48942172737593,-6.55711645661793,-5.61061408389849));
#23714=CARTESIAN_POINT('Ctrl Pts',(2.66440775694261,-6.48798347592862,-5.60210950660562));
#23715=CARTESIAN_POINT('Ctrl Pts',(3.03746506549949,-6.32295570218357,-5.58374371965392));
#23716=CARTESIAN_POINT('Ctrl Pts',(3.23423170374685,-6.22460511456047,-5.57390738015286));
#23717=CARTESIAN_POINT('Ctrl Pts',(3.58928652142074,-6.02574911621908,-5.55567139031329));
#23718=CARTESIAN_POINT('Ctrl Pts',(3.7487942857898,-5.92783012312946,-5.54728236116348));
#23719=CARTESIAN_POINT('Ctrl Pts',(3.99483419768763,-5.7628842387067,-5.5338715206011));
#23720=CARTESIAN_POINT('Ctrl Pts',(4.08404295284515,-5.70001117422567,-5.5288998898695));
#23721=CARTESIAN_POINT('Ctrl Pts',(4.23125463770712,-5.59102788116846,-5.52051892836126));
#23722=CARTESIAN_POINT('Ctrl Pts',(4.29006077082934,-5.54603345388105,-5.51712243361233));
#23723=CARTESIAN_POINT('Ctrl Pts',(4.67617982355893,-5.24078520970028,-5.49451277806392));
#23724=CARTESIAN_POINT('Ctrl Pts',(4.98036689096504,-4.95262008893787,-5.47526240477633));
#23725=CARTESIAN_POINT('Ctrl Pts',(5.39424980759214,-4.48360195891624,-5.44685950732038));
#23726=CARTESIAN_POINT('Ctrl Pts',(5.52447759238921,-4.32212525020034,-5.43751154359048));
#23727=CARTESIAN_POINT('Ctrl Pts',(5.8607718425196,-3.86505605412114,-5.41202401306825));
#23728=CARTESIAN_POINT('Ctrl Pts',(6.05151775956992,-3.55899284298793,-5.39601181822503));
#23729=CARTESIAN_POINT('Ctrl Pts',(6.27069321898006,-3.1383251110126,-5.37451772065111));
#23730=CARTESIAN_POINT('Ctrl Pts',(6.32099542095487,-3.03573614658974,-5.36930627359539));
#23731=CARTESIAN_POINT('Ctrl Pts',(6.43741146221111,-2.78285913337723,-5.35655646586825));
#23732=CARTESIAN_POINT('Ctrl Pts',(6.50079729942602,-2.63138847996865,-5.34900287562634));
#23733=CARTESIAN_POINT('Ctrl Pts',(6.65686626467081,-2.21827505774401,-5.32868784701643));
#23734=CARTESIAN_POINT('Ctrl Pts',(6.73943138833716,-1.95312089102667,-5.31595676936915));
#23735=CARTESIAN_POINT('Ctrl Pts',(6.85117915692958,-1.50141863815789,-5.29478165095512));
#23736=CARTESIAN_POINT('Ctrl Pts',(6.8889452941563,-1.31732608523719,-5.28628660733263));
#23737=CARTESIAN_POINT('Ctrl Pts',(6.9546279799784,-0.915822948130322,-5.26796901957214));
#23738=CARTESIAN_POINT('Ctrl Pts',(6.97983819041424,-0.698170157146178,
-5.2581709353385));
#23739=CARTESIAN_POINT('Ctrl Pts',(7.00781143127827,-0.290269127143199,
-5.23984979167635));
#23740=CARTESIAN_POINT('Ctrl Pts',(7.01310174712942,-0.100396500618003,
-5.2313370143895));
#23741=CARTESIAN_POINT('Ctrl Pts',(7.00928089057375,0.199051880567814,-5.21777728906797));
#23742=CARTESIAN_POINT('Ctrl Pts',(7.00531266557363,0.30859991953487,-5.21278300268002));
#23743=CARTESIAN_POINT('Ctrl Pts',(6.98158728758654,0.705837637291974,-5.19457236717849));
#23744=CARTESIAN_POINT('Ctrl Pts',(6.94665710998975,0.992332074562671,-5.18126963967956));
#23745=CARTESIAN_POINT('Ctrl Pts',(6.85597364790044,1.48234554062127,-5.15840232062872));
#23746=CARTESIAN_POINT('Ctrl Pts',(6.80850316320757,1.68701206812089,-5.14881242820551));
#23747=CARTESIAN_POINT('Ctrl Pts',(6.69411925160376,2.09580625252878,-5.12954641415351));
#23748=CARTESIAN_POINT('Ctrl Pts',(6.62687127628842,2.29961202115196,-5.11988312154751));
#23749=CARTESIAN_POINT('Ctrl Pts',(6.45251862516887,2.756439942648,-5.09793245849722));
#23750=CARTESIAN_POINT('Ctrl Pts',(6.3396799790906,3.00689437778745,-5.08568917062978));
#23751=CARTESIAN_POINT('Ctrl Pts',(6.16007886246485,3.35019700701687,-5.0682400307183));
#23752=CARTESIAN_POINT('Ctrl Pts',(6.10529438365007,3.44902476145725,-5.06313182744073));
#23753=CARTESIAN_POINT('Ctrl Pts',(5.93912073600712,3.73241578671817,-5.04817582179967));
#23754=CARTESIAN_POINT('Ctrl Pts',(5.82158146460825,3.91321737801238,-5.03826343675899));
#23755=CARTESIAN_POINT('Ctrl Pts',(5.51996940853453,4.33342785555409,-5.01446796623745));
#23756=CARTESIAN_POINT('Ctrl Pts',(5.32839521754225,4.56693208006331,-5.00061537900585));
#23757=CARTESIAN_POINT('Ctrl Pts',(4.99328129453979,4.92549613841691,-4.97828631747505));
#23758=CARTESIAN_POINT('Ctrl Pts',(4.8586533818069,5.05834549469446,-4.96973889305962));
#23759=CARTESIAN_POINT('Ctrl Pts',(4.55335442338125,5.33616345512455,-4.95115805038667));
#23760=CARTESIAN_POINT('Ctrl Pts',(4.3807770225186,5.47872889107436,-4.94115133866499));
#23761=CARTESIAN_POINT('Ctrl Pts',(4.05716400257742,5.72098198394382,-4.92303450322575));
#23762=CARTESIAN_POINT('Ctrl Pts',(3.90852624558663,5.82354151113776,-4.91493682758702));
#23763=CARTESIAN_POINT('Ctrl Pts',(3.66342411535084,5.97904641016079,-4.90179339501776));
#23764=CARTESIAN_POINT('Ctrl Pts',(3.56938370746226,6.03565832098991,-4.8967922520089));
#23765=CARTESIAN_POINT('Ctrl Pts',(3.40871001119445,6.12731442169353,-4.88832709939066));
#23766=CARTESIAN_POINT('Ctrl Pts',(3.34276994090111,6.16353591655151,-4.88487562078499));
#23767=CARTESIAN_POINT('Ctrl Pts',(2.91068531912496,6.39191026605421,-4.86242337175407));
#23768=CARTESIAN_POINT('Ctrl Pts',(2.5287247133862,6.55241707554525,-4.84338993644098));
#23769=CARTESIAN_POINT('Ctrl Pts',(1.93856019464885,6.74107389614773,-4.81525394774652));
#23770=CARTESIAN_POINT('Ctrl Pts',(1.73959909928719,6.79513720893601,-4.8059618347278));
#23771=CARTESIAN_POINT('Ctrl Pts',(1.17827430318887,6.92139124222625,-4.78011706316965));
#23772=CARTESIAN_POINT('Ctrl Pts',(0.812172143355865,6.97383358486175,-4.76370414853906));
#23773=CARTESIAN_POINT('Ctrl Pts',(0.324072299708876,7.00478128660869,-4.74152719440797));
#23774=CARTESIAN_POINT('Ctrl Pts',(0.204318291362056,7.00929645774514,-4.73605580997046));
#23775=CARTESIAN_POINT('Ctrl Pts',(-0.0989748059805782,7.01295244028332,
-4.72215425318536));
#23776=CARTESIAN_POINT('Ctrl Pts',(-0.282474672911588,7.00796016287849,
-4.7137048124347));
#23777=CARTESIAN_POINT('Ctrl Pts',(-0.708992712108262,6.97957554126962,
-4.6940471780958));
#23778=CARTESIAN_POINT('Ctrl Pts',(-0.951410426440865,6.95068100315977,
-4.68286401330344));
#23779=CARTESIAN_POINT('Ctrl Pts',(-1.37627961892231,6.87739157466336,-4.66324151956071));
#23780=CARTESIAN_POINT('Ctrl Pts',(-1.55938259890341,6.83820063129862,-4.65477559786249));
#23781=CARTESIAN_POINT('Ctrl Pts',(-1.9502396885087,6.73802515195734,-4.63660628141201));
#23782=CARTESIAN_POINT('Ctrl Pts',(-2.15718274362952,6.67465213721348,-4.62692608644044));
#23783=CARTESIAN_POINT('Ctrl Pts',(-2.54788460171998,6.53493380206192,-4.60833400214877));
#23784=CARTESIAN_POINT('Ctrl Pts',(-2.73197552733957,6.46013804580409,-4.59943167485397));
#23785=CARTESIAN_POINT('Ctrl Pts',(-3.01391716052841,6.33137633869536,-4.58539291192272));
#23786=CARTESIAN_POINT('Ctrl Pts',(-3.11407640382979,6.2827183849206,-4.58031727872298));
#23787=CARTESIAN_POINT('Ctrl Pts',(-3.28247985232057,6.1958903767336,-4.57164390928719));
#23788=CARTESIAN_POINT('Ctrl Pts',(-3.35132310281836,6.15892562923275,-4.56805801760813));
#23789=CARTESIAN_POINT('Ctrl Pts',(-3.77103344811813,5.92444492914084,-4.54596606919803));
#23790=CARTESIAN_POINT('Ctrl Pts',(-4.10497246511925,5.69815351094268,-4.52743742372748));
#23791=CARTESIAN_POINT('Ctrl Pts',(-4.57561920977808,5.31626968473013,-4.49990856148787));
#23792=CARTESIAN_POINT('Ctrl Pts',(-4.72794437893988,5.18126994390225,-4.49073226988463));
#23793=CARTESIAN_POINT('Ctrl Pts',(-5.0756926188213,4.8449516462406,-4.46899584952018));
#23794=CARTESIAN_POINT('Ctrl Pts',(-5.26533000746845,4.63815811979918,-4.45649208908233));
#23795=CARTESIAN_POINT('Ctrl Pts',(-5.51787367553666,4.32725653558499,-4.43847376052746));
#23796=CARTESIAN_POINT('Ctrl Pts',(-5.5912572939989,4.23201140327411,-4.43304720976354));
#23797=CARTESIAN_POINT('Ctrl Pts',(-5.7159541582044,4.06125792598364,-4.4234323640533));
#23798=CARTESIAN_POINT('Ctrl Pts',(-5.76830919154459,3.98654696326831,-4.41926401880285));
#23799=CARTESIAN_POINT('Ctrl Pts',(-5.91832603620198,3.76332701830764,-4.4069400660947));
#23800=CARTESIAN_POINT('Ctrl Pts',(-6.01181602556229,3.61210202038548,-4.39875774161554));
#23801=CARTESIAN_POINT('Ctrl Pts',(-6.22424303243211,3.2373532685571,-4.37894546442074));
#23802=CARTESIAN_POINT('Ctrl Pts',(-6.33702003603994,3.01062081028342,-4.36734276624509));
#23803=CARTESIAN_POINT('Ctrl Pts',(-6.50676703027325,2.61731678805357,-4.34784642969746));
#23804=CARTESIAN_POINT('Ctrl Pts',(-6.57017874608918,2.45379641593338,-4.33991294832414));
#23805=CARTESIAN_POINT('Ctrl Pts',(-6.74448595619915,1.948915497106,-4.31584706652881));
#23806=CARTESIAN_POINT('Ctrl Pts',(-6.83536941741902,1.60127606293307,-4.29988137936741));
#23807=CARTESIAN_POINT('Ctrl Pts',(-6.91800407317094,1.14452974964774,-4.27897974113059));
#23808=CARTESIAN_POINT('Ctrl Pts',(-6.93442260486219,1.04043817544725,-4.27421844970426));
#23809=CARTESIAN_POINT('Ctrl Pts',(-6.99027522850461,0.625817670587475,
-4.25519105535893));
#23810=CARTESIAN_POINT('Ctrl Pts',(-7.01124210805982,0.313172090659878,
-4.2407473831395));
#23811=CARTESIAN_POINT('Ctrl Pts',(-7.01124999777253,0.000176733446466751,
-4.22636455703907));
#23812=CARTESIAN_POINT('Ctrl Pts',(-7.0112499978881,0.00017208778304258,
-4.22646564308965));
#23813=CARTESIAN_POINT('Ctrl Pts',(-7.01125459996624,-0.187327104922663,
-4.2179538597749));
#23814=CARTESIAN_POINT('Ctrl Pts',(-7.00373353003433,-0.374843190662422,
-4.20944207646015));
#23815=CARTESIAN_POINT('Ctrl Pts',(-6.98870878823683,-0.561761547029809,
-4.2009302931454));
#23816=CARTESIAN_POINT('Ctrl Pts',(-6.97368319756446,-0.748690463997657,
-4.19241802892795));
#23817=CARTESIAN_POINT('Ctrl Pts',(-6.9511531095221,-0.93502127618761,-4.1839057647105));
#23818=CARTESIAN_POINT('Ctrl Pts',(-6.9211925057364,-1.12014323237624,-4.17539350049304));
#23819=CARTESIAN_POINT('Ctrl Pts',(-6.89123239521493,-1.30526214076115,
-4.16688137641948));
#23820=CARTESIAN_POINT('Ctrl Pts',(-6.85384206526541,-1.48917192862319,
-4.15836925234591));
#23821=CARTESIAN_POINT('Ctrl Pts',(-6.80914691169823,-1.67127044412639,
-4.14985712827235));
#23822=CARTESIAN_POINT('Ctrl Pts',(-6.76444180092798,-1.85340952760519,
-4.14134310786459));
#23823=CARTESIAN_POINT('Ctrl Pts',(-6.71242868925155,-2.03373623281141,
-4.13282908745683));
#23824=CARTESIAN_POINT('Ctrl Pts',(-6.65328352886334,-2.21166110583331,
-4.12431506704907));
#23825=CARTESIAN_POINT('Ctrl Pts',(-6.62761633303324,-2.28887507446445,
-4.12062024184827));
#23826=CARTESIAN_POINT('Ctrl Pts',(-6.60060659762498,-2.36563690067436,
-4.11692541664747));
#23827=CARTESIAN_POINT('Ctrl Pts',(-6.57227159525839,-2.44189939200201,
-4.11323059144668));
#23828=CARTESIAN_POINT('Ctrl Pts',(-6.57227158383948,-2.44189942273553,
-4.6606292049078));
#23829=CARTESIAN_POINT('Ctrl Pts',(-6.70390621728781,-2.08761023588097,
-4.67773914757001));
#23830=CARTESIAN_POINT('Ctrl Pts',(-6.80669705592026,-1.72320489332983,
-4.69459415246904));
#23831=CARTESIAN_POINT('Ctrl Pts',(-6.8942421135184,-1.27781271705034,-4.71496363186487));
#23832=CARTESIAN_POINT('Ctrl Pts',(-6.90766216320481,-1.20315543525653,
-4.7183718645118));
#23833=CARTESIAN_POINT('Ctrl Pts',(-6.93758375007867,-1.01964549419006,
-4.72675020208282));
#23834=CARTESIAN_POINT('Ctrl Pts',(-6.95273764935542,-0.910595489399886,
-4.73173114360371));
#23835=CARTESIAN_POINT('Ctrl Pts',(-6.99590754101394,-0.535308904302658,
-4.74893736830413));
#23836=CARTESIAN_POINT('Ctrl Pts',(-7.01124315989833,-0.267853137209664,
-4.76127380578758));
#23837=CARTESIAN_POINT('Ctrl Pts',(-7.01125616410567,0.241211380042968,
-4.78468215521764));
#23838=CARTESIAN_POINT('Ctrl Pts',(-6.99879608154224,0.482443869538131,
-4.79574490275203));
#23839=CARTESIAN_POINT('Ctrl Pts',(-6.95454963225591,0.909499595056456,
-4.81528242823844));
#23840=CARTESIAN_POINT('Ctrl Pts',(-6.92767134590944,1.09559177564294,-4.82378164659587));
#23841=CARTESIAN_POINT('Ctrl Pts',(-6.85328797825378,1.49605893575086,-4.84212032646349));
#23842=CARTESIAN_POINT('Ctrl Pts',(-6.80312743939344,1.7097386383162,-4.85193514871219));
#23843=CARTESIAN_POINT('Ctrl Pts',(-6.69135122731386,2.10215003965919,-4.87021889566688));
#23844=CARTESIAN_POINT('Ctrl Pts',(-6.63236935521845,2.28142305464891,-4.87867739602326));
#23845=CARTESIAN_POINT('Ctrl Pts',(-6.52787863739525,2.56054559408591,-4.89217164560283));
#23846=CARTESIAN_POINT('Ctrl Pts',(-6.48713477867009,2.66208091752975,-4.89715582769753));
#23847=CARTESIAN_POINT('Ctrl Pts',(-6.38618840884508,2.89754642513058,-4.90887903910264));
#23848=CARTESIAN_POINT('Ctrl Pts',(-6.32412098437491,3.03062221629724,-4.91562892313301));
#23849=CARTESIAN_POINT('Ctrl Pts',(-6.11679971881715,3.44097761944665,-4.93677868961053));
#23850=CARTESIAN_POINT('Ctrl Pts',(-5.95713126674611,3.71054690471241,-4.95115154162357));
#23851=CARTESIAN_POINT('Ctrl Pts',(-5.67263970273283,4.12489429513226,-4.97401646496258));
#23852=CARTESIAN_POINT('Ctrl Pts',(-5.5589918147202,4.27682191451809,-4.98258951225769));
#23853=CARTESIAN_POINT('Ctrl Pts',(-5.29671652139686,4.59929346983292,-5.00129800651448));
#23854=CARTESIAN_POINT('Ctrl Pts',(-5.14571502500059,4.76763293840727,-5.01140565108458));
#23855=CARTESIAN_POINT('Ctrl Pts',(-4.85820073886254,5.05855778491549,-5.02973830064952));
#23856=CARTESIAN_POINT('Ctrl Pts',(-4.72450834552819,5.18364163316081,-5.0379498830824));
#23857=CARTESIAN_POINT('Ctrl Pts',(-4.4997412231803,5.37800924921345,-5.05141469837085));
#23858=CARTESIAN_POINT('Ctrl Pts',(-4.41159619883565,5.45054792240292,-5.05662136292772));
#23859=CARTESIAN_POINT('Ctrl Pts',(-4.19274521403411,5.62186287422926,-5.06934998955121));
#23860=CARTESIAN_POINT('Ctrl Pts',(-4.06027139790908,5.71827337155505,-5.0768870993764));
#23861=CARTESIAN_POINT('Ctrl Pts',(-3.69404964851037,5.96565104395998,-5.09721749249556));
#23862=CARTESIAN_POINT('Ctrl Pts',(-3.45449158594315,6.10749433473452,-5.1099803871655));
#23863=CARTESIAN_POINT('Ctrl Pts',(-3.04006933351791,6.32067268306784,-5.13118804424986));
#23864=CARTESIAN_POINT('Ctrl Pts',(-2.86961096598136,6.39986399361892,-5.13968434669682));
#23865=CARTESIAN_POINT('Ctrl Pts',(-2.49392285582217,6.55636948057832,-5.15800827483852));
#23866=CARTESIAN_POINT('Ctrl Pts',(-2.28783068562546,6.63109820841612,-5.16781138680754));
#23867=CARTESIAN_POINT('Ctrl Pts',(-1.89759290916194,6.7522351463715,-5.18612128988212));
#23868=CARTESIAN_POINT('Ctrl Pts',(-1.71440687784977,6.80105475186465,-5.19461775716185));
#23869=CARTESIAN_POINT('Ctrl Pts',(-1.4225672291869,6.86628928141453,-5.20815778505994));
#23870=CARTESIAN_POINT('Ctrl Pts',(-1.31512015945449,6.8876762543057,-5.21314901403829));
#23871=CARTESIAN_POINT('Ctrl Pts',(-1.06205205194053,6.9319109140208,-5.22490524125236));
#23872=CARTESIAN_POINT('Ctrl Pts',(-0.916123168975142,6.95270173267984,
-5.23168125048848));
#23873=CARTESIAN_POINT('Ctrl Pts',(-0.459758082269938,7.00310306459452,
-5.25280287560086));
#23874=CARTESIAN_POINT('Ctrl Pts',(-0.147925049822086,7.01661981552651,
-5.26712116522719));
#23875=CARTESIAN_POINT('Ctrl Pts',(0.353314907659504,7.00490833466094,-5.28993009385463));
#23876=CARTESIAN_POINT('Ctrl Pts',(0.542600648481804,6.99279331011027,-5.29850063154806));
#23877=CARTESIAN_POINT('Ctrl Pts',(0.955717812126998,6.94947542758775,-5.31719664334724));
#23878=CARTESIAN_POINT('Ctrl Pts',(1.17900327353281,6.91509632353111,-5.32729442246173));
#23879=CARTESIAN_POINT('Ctrl Pts',(1.57946014632695,6.83347540813823,-5.34561190263004));
#23880=CARTESIAN_POINT('Ctrl Pts',(1.75717955787997,6.78994837413825,-5.35381828449975));
#23881=CARTESIAN_POINT('Ctrl Pts',(2.04231668194139,6.70816699631933,-5.36725884042856));
#23882=CARTESIAN_POINT('Ctrl Pts',(2.15086121074734,6.67415590566567,-5.37244650716258));
#23883=CARTESIAN_POINT('Ctrl Pts',(2.41225178430267,6.58521333907708,-5.38509096611195));
#23884=CARTESIAN_POINT('Ctrl Pts',(2.56411081606651,6.52758214676201,-5.39256257809965));
#23885=CARTESIAN_POINT('Ctrl Pts',(2.9728435641803,6.35600012754387,-5.41295498145386));
#23886=CARTESIAN_POINT('Ctrl Pts',(3.22509093691513,6.23179982166028,-5.42584530572912));
#23887=CARTESIAN_POINT('Ctrl Pts',(3.63257878684362,5.99977841309522,-5.44718338554033));
#23888=CARTESIAN_POINT('Ctrl Pts',(3.79214334581374,5.90022203051291,-5.45568484932166));
#23889=CARTESIAN_POINT('Ctrl Pts',(4.12897764336816,5.67074790180028,-5.47403487931341));
#23890=CARTESIAN_POINT('Ctrl Pts',(4.30453298717051,5.53866722424426,-5.48385870964967));
#23891=CARTESIAN_POINT('Ctrl Pts',(4.61835709735215,5.27861227506268,-5.50212242281259));
#23892=CARTESIAN_POINT('Ctrl Pts',(4.75822823513098,5.15288582155602,-5.51055180079543));
#23893=CARTESIAN_POINT('Ctrl Pts',(4.97114535632935,4.94543045900397,-5.52401103294801));
#23894=CARTESIAN_POINT('Ctrl Pts',(5.04761981505703,4.86735061284432,-5.52898990317804));
#23895=CARTESIAN_POINT('Ctrl Pts',(5.28531488702843,4.61303702173026,-5.54491845710866));
#23896=CARTESIAN_POINT('Ctrl Pts',(5.43937069638893,4.43033969889257,-5.55592567941762));
#23897=CARTESIAN_POINT('Ctrl Pts',(5.71800133490058,4.06341341139405,-5.57710026901083));
#23898=CARTESIAN_POINT('Ctrl Pts',(5.84373613370387,3.88041467470019,-5.58726057644863));
#23899=CARTESIAN_POINT('Ctrl Pts',(6.06056948761918,3.53032340841884,-5.60599358800878));
#23900=CARTESIAN_POINT('Ctrl Pts',(6.15395836412213,3.36488987640865,-5.61457712308354));
#23901=CARTESIAN_POINT('Ctrl Pts',(6.34396198930457,2.9938730092555,-5.63333773553946));
#23902=CARTESIAN_POINT('Ctrl Pts',(6.43753861109095,2.78697444509421,-5.64348656152049));
#23903=CARTESIAN_POINT('Ctrl Pts',(6.58824561808943,2.40545848224129,-5.66187265736131));
#23904=CARTESIAN_POINT('Ctrl Pts',(6.64886531533272,2.2324424354922,-5.67009605360231));
#23905=CARTESIAN_POINT('Ctrl Pts',(6.73660825648486,1.94657141526927,-5.68364913403675));
#23906=CARTESIAN_POINT('Ctrl Pts',(6.76783262889296,1.83506721414836,-5.68893221611056));
#23907=CARTESIAN_POINT('Ctrl Pts',(6.83792256297493,1.55857601904308,-5.70199859010682));
#23908=CARTESIAN_POINT('Ctrl Pts',(6.87359451254463,1.39285399253202,-5.70979829890135));
#23909=CARTESIAN_POINT('Ctrl Pts',(6.94999793375986,0.962651139356424,-5.72989698975842));
#23910=CARTESIAN_POINT('Ctrl Pts',(6.98166120249297,0.696834938462023,-5.74216638201182));
#23911=CARTESIAN_POINT('Ctrl Pts',(7.00955502099417,0.242725585568709,-5.76287175551013));
#23912=CARTESIAN_POINT('Ctrl Pts',(7.01353913261123,0.0552054826433945,
-5.77135111488268));
#23913=CARTESIAN_POINT('Ctrl Pts',(7.00589901430265,-0.349762775455823,
-5.78958902682646));
#23914=CARTESIAN_POINT('Ctrl Pts',(6.99167393646226,-0.566966754980128,
-5.79932379705014));
#23915=CARTESIAN_POINT('Ctrl Pts',(6.94564379190608,-0.976474418599964,
-5.81778888747249));
#23916=CARTESIAN_POINT('Ctrl Pts',(6.91587835810513,-1.16880055450405,-5.82650937513558));
#23917=CARTESIAN_POINT('Ctrl Pts',(6.85672868373382,-1.46802792137355,-5.84032251187271));
#23918=CARTESIAN_POINT('Ctrl Pts',(6.83274382423929,-1.57589505695686,-5.84535822128053));
#23919=CARTESIAN_POINT('Ctrl Pts',(6.735689642359,-1.96835720429491,-5.86386222842968));
#23920=CARTESIAN_POINT('Ctrl Pts',(6.64730156138577,-2.24885022792779,-5.87741782164038));
#23921=CARTESIAN_POINT('Ctrl Pts',(6.46662001669965,-2.71732296584495,-5.90045136230478));
#23922=CARTESIAN_POINT('Ctrl Pts',(6.38303640796235,-2.90824118798729,-5.90996020281285));
#23923=CARTESIAN_POINT('Ctrl Pts',(6.19318611573004,-3.29412236647469,-5.92947115545108));
#23924=CARTESIAN_POINT('Ctrl Pts',(6.08591182043921,-3.48833424810144,-5.93945405321215));
#23925=CARTESIAN_POINT('Ctrl Pts',(5.82510822334941,-3.91173334406615,-5.96176801844721));
#23926=CARTESIAN_POINT('Ctrl Pts',(5.66690089155583,-4.13760505953238,-5.97405882283894));
#23927=CARTESIAN_POINT('Ctrl Pts',(5.42947375803411,-4.43732532204864,-5.99129752003615));
#23928=CARTESIAN_POINT('Ctrl Pts',(5.36122825266725,-4.51954341314763,-5.99613485629221));
#23929=CARTESIAN_POINT('Ctrl Pts',(5.02288070966675,-4.90871178621462,-6.01963184827458));
#23930=CARTESIAN_POINT('Ctrl Pts',(4.72815728289039,-5.19319881463183,-6.0385459037528));
#23931=CARTESIAN_POINT('Ctrl Pts',(4.27894856406941,-5.5566885261447,-6.06498223518058));
#23932=CARTESIAN_POINT('Ctrl Pts',(4.14376853386443,-5.65821276367141,-6.07267733515801));
#23933=CARTESIAN_POINT('Ctrl Pts',(3.78012610677635,-5.9112916003396,-6.0927513643439));
#23934=CARTESIAN_POINT('Ctrl Pts',(3.54621572088584,-6.05450896422114,-6.10504501523413));
#23935=CARTESIAN_POINT('Ctrl Pts',(3.08610916948512,-6.30038761924725,-6.12841946046126));
#23936=CARTESIAN_POINT('Ctrl Pts',(2.86166855482467,-6.40545111666512,-6.13948895318468));
#23937=CARTESIAN_POINT('Ctrl Pts',(2.5316105293928,-6.53913907747908,-6.15560895566176));
#23938=CARTESIAN_POINT('Ctrl Pts',(2.43014745855055,-6.57752037678161,-6.16054952415093));
#23939=CARTESIAN_POINT('Ctrl Pts',(2.05568743160319,-6.70932311625542,-6.17871129988722));
#23940=CARTESIAN_POINT('Ctrl Pts',(1.77788575318046,-6.7882243442581,-6.19202222402473));
#23941=CARTESIAN_POINT('Ctrl Pts',(1.28922590751124,-6.89494920809898,-6.21497704368261));
#23942=CARTESIAN_POINT('Ctrl Pts',(1.08049549130856,-6.93072576545548,-6.22464480964778));
#23943=CARTESIAN_POINT('Ctrl Pts',(0.659355031407631,-6.98341910910548,
-6.24390958938615));
#23944=CARTESIAN_POINT('Ctrl Pts',(0.447150726398731,-7.00021068726772,
-6.25349601558817));
#23945=CARTESIAN_POINT('Ctrl Pts',(-0.0479150094512006,-7.01677872881925,
-6.27573545400535));
#23946=CARTESIAN_POINT('Ctrl Pts',(-0.330650687769794,-7.0091474322944,
-6.28833750190172));
#23947=CARTESIAN_POINT('Ctrl Pts',(-0.722904410143011,-6.97476855196262,
-6.30607670790614));
#23948=CARTESIAN_POINT('Ctrl Pts',(-0.833409285102849,-6.96242887557347,
-6.311105588362));
#23949=CARTESIAN_POINT('Ctrl Pts',(-1.38274308358209,-6.88782073617079,
-6.33635129730869));
#23950=CARTESIAN_POINT('Ctrl Pts',(-1.81526823350533,-6.786667836431,-6.35686880016417));
#23951=CARTESIAN_POINT('Ctrl Pts',(-2.4082933198585,-6.58718793621379,-6.3854507255645));
#23952=CARTESIAN_POINT('Ctrl Pts',(-2.57890510103155,-6.52228269564939,
-6.39374013815183));
#23953=CARTESIAN_POINT('Ctrl Pts',(-2.82933461806604,-6.41564811689309,
-6.40604262781619));
#23954=CARTESIAN_POINT('Ctrl Pts',(-2.9111952322872,-6.37891978400674,-6.41008673270239));
#23955=CARTESIAN_POINT('Ctrl Pts',(-3.20607472588871,-6.2397575338227,-6.42475624235216));
#23956=CARTESIAN_POINT('Ctrl Pts',(-3.41458332433729,-6.1281408589003,-6.4353201318437));
#23957=CARTESIAN_POINT('Ctrl Pts',(-3.7586230823732,-5.92095334177488,-6.45332838543319));
#23958=CARTESIAN_POINT('Ctrl Pts',(-3.89712972844991,-5.8307216173014,-6.46075112571011));
#23959=CARTESIAN_POINT('Ctrl Pts',(-4.12700081411852,-5.66911693031274,
-6.47348647246354));
#23960=CARTESIAN_POINT('Ctrl Pts',(-4.2200202129524,-5.60021883402846,-6.47876782501162));
#23961=CARTESIAN_POINT('Ctrl Pts',(-4.44482669160317,-5.42492547707781,
-6.49182656067331));
#23962=CARTESIAN_POINT('Ctrl Pts',(-4.57454684955087,-5.31599675076628,
-6.49962033275064));
#23963=CARTESIAN_POINT('Ctrl Pts',(-4.89883956243725,-5.02301353446546,
-6.51972395108936));
#23964=CARTESIAN_POINT('Ctrl Pts',(-5.0870445420839,-4.83231574338115,-6.53200418158846));
#23965=CARTESIAN_POINT('Ctrl Pts',(-5.38135978233284,-4.49780184072536,
-6.55228135748184));
#23966=CARTESIAN_POINT('Ctrl Pts',(-5.49371302340107,-4.35985928930604,
-6.5603275647837));
#23967=CARTESIAN_POINT('Ctrl Pts',(-5.72660556133383,-4.05060716273615,
-6.57776759697057));
#23968=CARTESIAN_POINT('Ctrl Pts',(-5.84496164891105,-3.87786716922929,
-6.58713843404064));
#23969=CARTESIAN_POINT('Ctrl Pts',(-6.06481104935635,-3.52401262702012,
-6.60580253501089));
#23970=CARTESIAN_POINT('Ctrl Pts',(-6.16634450597322,-3.34317087659181,
-6.61508683885542));
#23971=CARTESIAN_POINT('Ctrl Pts',(-6.3069702654834,-3.06443449918892,-6.62921800477762));
#23972=CARTESIAN_POINT('Ctrl Pts',(-6.35211616926502,-2.9697225814325,-6.63399490891892));
#23973=CARTESIAN_POINT('Ctrl Pts',(-6.45898223987877,-2.73193097941898,
-6.64591800053814));
#23974=CARTESIAN_POINT('Ctrl Pts',(-6.5180611244172,-2.58780462279585,-6.65307815376513));
#23975=CARTESIAN_POINT('Ctrl Pts',(-6.5722714983487,-2.44189965283043,-6.66023848729892));
#23976=CARTESIAN_POINT('Origin',(0.,0.,0.));
#23977=CARTESIAN_POINT('',(-6.57227159525839,-2.44189939200199,-8.66029439624775));
#23978=CARTESIAN_POINT('',(-6.57227165853301,-2.44189922170096,-8.11305756739085));
#23979=CARTESIAN_POINT('',(-6.57227159525839,-2.441899392002,0.));
#23980=CARTESIAN_POINT('Ctrl Pts',(-6.57227165853301,-2.44189922170096,
-8.11305756739085));
#23981=CARTESIAN_POINT('Ctrl Pts',(-6.51817519271005,-2.58749764197787,
-8.10608231724909));
#23982=CARTESIAN_POINT('Ctrl Pts',(-6.45923882215988,-2.73130286006209,
-8.0991275279903));
#23983=CARTESIAN_POINT('Ctrl Pts',(-6.33712037052739,-3.00314237969816,
-8.08577404493706));
#23984=CARTESIAN_POINT('Ctrl Pts',(-6.27473543286156,-3.13139800508645,
-8.0793815528912));
#23985=CARTESIAN_POINT('Ctrl Pts',(-6.16355711632633,-3.34328277427315,
-8.06859486435757));
#23986=CARTESIAN_POINT('Ctrl Pts',(-6.11686483163985,-3.4279644824695,-8.06422004891531));
#23987=CARTESIAN_POINT('Ctrl Pts',(-5.99274121333451,-3.64246061971337,
-8.05294144285684));
#23988=CARTESIAN_POINT('Ctrl Pts',(-5.9128377489431,-3.77078446643113,-8.04601158176694));
#23989=CARTESIAN_POINT('Ctrl Pts',(-5.68078292142082,-4.11792658014196,
-8.02682113598621));
#23990=CARTESIAN_POINT('Ctrl Pts',(-5.52020798851787,-4.3308105001367,-8.01454987363125));
#23991=CARTESIAN_POINT('Ctrl Pts',(-5.22641443800212,-4.67734054736446,
-7.99376276196743));
#23992=CARTESIAN_POINT('Ctrl Pts',(-5.09920929828207,-4.81570229432193,
-7.98521238398094));
#23993=CARTESIAN_POINT('Ctrl Pts',(-4.77036319129291,-5.14573188995945,
-7.96412293838842));
#23994=CARTESIAN_POINT('Ctrl Pts',(-4.56258523254715,-5.33082923970444,
-7.95166344456971));
#23995=CARTESIAN_POINT('Ctrl Pts',(-4.21575006671975,-5.60463457235991,
-7.93186652732066));
#23996=CARTESIAN_POINT('Ctrl Pts',(-4.08361626691444,-5.70162738977248,
-7.92453006375508));
#23997=CARTESIAN_POINT('Ctrl Pts',(-3.85386888447544,-5.85818687811532,
-7.91201145782549));
#23998=CARTESIAN_POINT('Ctrl Pts',(-3.75797669565571,-5.92015791706546,
-7.90685140890572));
#23999=CARTESIAN_POINT('Ctrl Pts',(-3.35368857734603,-6.16764986481274,
-7.88527471484278));
#24000=CARTESIAN_POINT('Ctrl Pts',(-3.03275446176226,-6.3316294580092,-7.86864324095011));
#24001=CARTESIAN_POINT('Ctrl Pts',(-2.50925959838254,-6.5501341291496,-7.84262266007155));
#24002=CARTESIAN_POINT('Ctrl Pts',(-2.31441160311268,-6.62149090484725,
-7.83315618534303));
#24003=CARTESIAN_POINT('Ctrl Pts',(-1.71783496608031,-6.81041146448286,
-7.80476754391258));
#24004=CARTESIAN_POINT('Ctrl Pts',(-1.30847988470247,-6.90076408149348,
-7.78612330577171));
#24005=CARTESIAN_POINT('Ctrl Pts',(-0.820128773837127,-6.96351132196717,
-7.76402426653175));
#24006=CARTESIAN_POINT('Ctrl Pts',(-0.746597344149629,-6.97177835629235,
-7.76069878717101));
#24007=CARTESIAN_POINT('Ctrl Pts',(-0.564354023764458,-6.98935144802316,
-7.75244684525943));
#24008=CARTESIAN_POINT('Ctrl Pts',(-0.455531393873775,-6.99728661804769,
-7.74750901691098));
#24009=CARTESIAN_POINT('Ctrl Pts',(-0.166941845043998,-7.01156909937355,
-7.73434570204032));
#24010=CARTESIAN_POINT('Ctrl Pts',(0.0129573714319099,-7.01354416492444,
-7.72608435581353));
#24011=CARTESIAN_POINT('Ctrl Pts',(0.416039609820819,-7.00245970656703,
-7.7075377941428));
#24012=CARTESIAN_POINT('Ctrl Pts',(0.638928484736241,-6.98564975975726,
-7.69725933870154));
#24013=CARTESIAN_POINT('Ctrl Pts',(1.04818172256356,-6.93503090250718,-7.67838699514727));
#24014=CARTESIAN_POINT('Ctrl Pts',(1.2347160983123,-6.90426073555607,-7.66978424118245));
#24015=CARTESIAN_POINT('Ctrl Pts',(1.71374568405082,-6.80520480935842,-7.64763715745567));
#24016=CARTESIAN_POINT('Ctrl Pts',(2.00350447835029,-6.72560106154017,-7.63419616636894));
#24017=CARTESIAN_POINT('Ctrl Pts',(2.48964951866254,-6.55782793963812,-7.61115532333263));
#24018=CARTESIAN_POINT('Ctrl Pts',(2.68872121877613,-6.47875280894356,-7.60156725238652));
#24019=CARTESIAN_POINT('Ctrl Pts',(2.98525083369218,-6.34494110385861,-7.58683255586316));
#24020=CARTESIAN_POINT('Ctrl Pts',(3.08553692081057,-6.29678181487987,-7.5817617336861));
#24021=CARTESIAN_POINT('Ctrl Pts',(3.436369340257,-6.11791110360568,-7.56373508888826));
#24022=CARTESIAN_POINT('Ctrl Pts',(3.68011604037794,-5.97446370742416,-7.55070040509004));
#24023=CARTESIAN_POINT('Ctrl Pts',(4.09098900750442,-5.6979531826868,-7.52797353176129));
#24024=CARTESIAN_POINT('Ctrl Pts',(4.26194496183058,-5.57123763934641,-7.51826070876749));
#24025=CARTESIAN_POINT('Ctrl Pts',(4.59106903748204,-5.30325776469124,-7.49899969670924));
#24026=CARTESIAN_POINT('Ctrl Pts',(4.74912157020259,-5.16219953346053,-7.48946075461461));
#24027=CARTESIAN_POINT('Ctrl Pts',(5.10716828169107,-4.81226847836516,-7.46698482479571));
#24028=CARTESIAN_POINT('Ctrl Pts',(5.3011061557193,-4.59775672716515,-7.45410331544837));
#24029=CARTESIAN_POINT('Ctrl Pts',(5.5487896495945,-4.28722406604433,-7.43619722595163));
#24030=CARTESIAN_POINT('Ctrl Pts',(5.61435203948097,-4.20100079446446,-7.43129396117637));
#24031=CARTESIAN_POINT('Ctrl Pts',(5.78460655947834,-3.96598551284471,-7.41807084366292));
#24032=CARTESIAN_POINT('Ctrl Pts',(5.88554790328168,-3.81458239403292,-7.40971370741527));
#24033=CARTESIAN_POINT('Ctrl Pts',(6.09609552605055,-3.47049107377572,-7.39115883803676));
#24034=CARTESIAN_POINT('Ctrl Pts',(6.2026871626226,-3.27618103792163,-7.38096856961922));
#24035=CARTESIAN_POINT('Ctrl Pts',(6.38262817790572,-2.90778483295969,-7.36220684332091));
#24036=CARTESIAN_POINT('Ctrl Pts',(6.45849151211225,-2.7351497354249,-7.35362712588235));
#24037=CARTESIAN_POINT('Ctrl Pts',(6.63357967465798,-2.28866405948016,-7.33191541296364));
#24038=CARTESIAN_POINT('Ctrl Pts',(6.72287263719483,-2.01130527664654,-7.31887668513947));
#24039=CARTESIAN_POINT('Ctrl Pts',(6.84884588211138,-1.51630923499633,-7.29599354187019));
#24040=CARTESIAN_POINT('Ctrl Pts',(6.892988858788,-1.30099417499752,-7.28615915682875));
#24041=CARTESIAN_POINT('Ctrl Pts',(6.94396998395295,-0.975205561409179,
-7.27122696245657));
#24042=CARTESIAN_POINT('Ctrl Pts',(6.9584252124808,-0.866061645879403,-7.26621024907983));
#24043=CARTESIAN_POINT('Ctrl Pts',(7.00082706162474,-0.475440040128734,
-7.24822800460087));
#24044=CARTESIAN_POINT('Ctrl Pts',(7.01430697306611,-0.192666848376906,
-7.23518066190373));
#24045=CARTESIAN_POINT('Ctrl Pts',(7.00791699459066,0.30428356830222,-7.21237153645258));
#24046=CARTESIAN_POINT('Ctrl Pts',(6.99535385784562,0.51818499952154,-7.2025902543283));
#24047=CARTESIAN_POINT('Ctrl Pts',(6.95064379059364,0.94457130352698,-7.18313239595964));
#24048=CARTESIAN_POINT('Ctrl Pts',(6.91848372796387,1.15682708978907,-7.1734662618088));
#24049=CARTESIAN_POINT('Ctrl Pts',(6.82117084362721,1.64625709416158,-7.15106490792058));
#24050=CARTESIAN_POINT('Ctrl Pts',(6.74877593285378,1.92160227799906,-7.13838069462069));
#24051=CARTESIAN_POINT('Ctrl Pts',(6.64385062179033,2.2404234805491,-7.12325361596668));
#24052=CARTESIAN_POINT('Ctrl Pts',(6.62731134533452,2.2888846063367,-7.12094161123295));
#24053=CARTESIAN_POINT('Ctrl Pts',(6.57400369553663,2.43965584654816,-7.11370212319582));
#24054=CARTESIAN_POINT('Ctrl Pts',(6.53538634295797,2.54129294053583,-7.10874992640004));
#24055=CARTESIAN_POINT('Ctrl Pts',(6.39065146904711,2.89707380426187,-7.09117661951697));
#24056=CARTESIAN_POINT('Ctrl Pts',(6.27194272407044,3.1458221597177,-7.07847472992205));
#24057=CARTESIAN_POINT('Ctrl Pts',(6.03249746006562,3.57982230837531,-7.05571703294241));
#24058=CARTESIAN_POINT('Ctrl Pts',(5.9170501266622,3.76758191939754,-7.04565040359384));
#24059=CARTESIAN_POINT('Ctrl Pts',(5.67503961797406,4.12254368379534,-7.02614580139638));
#24060=CARTESIAN_POINT('Ctrl Pts',(5.54943852748492,4.29012528818939,-7.01671079925425));
#24061=CARTESIAN_POINT('Ctrl Pts',(5.23107653002378,4.67747461441378,-6.99419410083532));
#24062=CARTESIAN_POINT('Ctrl Pts',(5.0317095340301,4.89130119970314,-6.98117314653623));
#24063=CARTESIAN_POINT('Ctrl Pts',(4.73946237932808,5.1679101678667,-6.96304180099587));
#24064=CARTESIAN_POINT('Ctrl Pts',(4.65755588733432,5.24184815195318,-6.95805014302439));
#24065=CARTESIAN_POINT('Ctrl Pts',(4.43672915741739,5.43192745495537,-6.94477961869521));
#24066=CARTESIAN_POINT('Ctrl Pts',(4.29499849107725,5.54467205903683,-6.93646401459017));
#24067=CARTESIAN_POINT('Ctrl Pts',(3.96849114943427,5.78436549426352,-6.9178345626302));
#24068=CARTESIAN_POINT('Ctrl Pts',(3.78166660262041,5.908198131128,-6.9075274383583));
#24069=CARTESIAN_POINT('Ctrl Pts',(3.42676215032734,6.11969767484504,-6.88861911683933));
#24070=CARTESIAN_POINT('Ctrl Pts',(3.26043690729395,6.20990750729763,-6.88000885666077));
#24071=CARTESIAN_POINT('Ctrl Pts',(2.81861347951256,6.42688945506487,-6.85772241496385));
#24072=CARTESIAN_POINT('Ctrl Pts',(2.53818201931679,6.54271542689402,-6.84415289199739));
#24073=CARTESIAN_POINT('Ctrl Pts',(2.05757120596388,6.70565436760548,-6.82141645457886));
#24074=CARTESIAN_POINT('Ctrl Pts',(1.86123291250805,6.76278122571477,-6.81226151026225));
#24075=CARTESIAN_POINT('Ctrl Pts',(1.55943660990965,6.83645222220464,-6.79820135841265));
#24076=CARTESIAN_POINT('Ctrl Pts',(1.45563287447383,6.85930417364746,-6.79336227335932));
#24077=CARTESIAN_POINT('Ctrl Pts',(1.08090125771741,6.93291022512691,-6.77589587002869));
#24078=CARTESIAN_POINT('Ctrl Pts',(0.807554912700613,6.97003919652783,-6.76318318159885));
#24079=CARTESIAN_POINT('Ctrl Pts',(0.310520245701929,7.00791478987115,-6.74029328680237));
#24080=CARTESIAN_POINT('Ctrl Pts',(0.0876223906700351,7.01424388409346,
-6.73010713012611));
#24081=CARTESIAN_POINT('Ctrl Pts',(-0.342739865064623,7.00594352479632,
-6.71056247626169));
#24082=CARTESIAN_POINT('Ctrl Pts',(-0.550001215201553,6.99272591980853,
-6.70120413859114));
#24083=CARTESIAN_POINT('Ctrl Pts',(-1.04945901861334,6.93852819869003,-6.67863951195789));
#24084=CARTESIAN_POINT('Ctrl Pts',(-1.34024571486383,6.88827097736807,-6.66549759879253));
#24085=CARTESIAN_POINT('Ctrl Pts',(-1.73467865652842,6.79417182040374,-6.64722756787435));
#24086=CARTESIAN_POINT('Ctrl Pts',(-1.84172999618833,6.76593756488301,-6.64221972285008));
#24087=CARTESIAN_POINT('Ctrl Pts',(-2.12226240203206,6.68479698662707,-6.62891983133171));
#24088=CARTESIAN_POINT('Ctrl Pts',(-2.2944342593525,6.62767520792402,-6.62059083729334));
#24089=CARTESIAN_POINT('Ctrl Pts',(-2.67408710196292,6.48514825080581,-6.60193933390689));
#24090=CARTESIAN_POINT('Ctrl Pts',(-2.88007950768366,6.39632964823763,-6.59162353032621));
#24091=CARTESIAN_POINT('Ctrl Pts',(-3.25139434267168,6.21464813663892,-6.5727043152711));
#24092=CARTESIAN_POINT('Ctrl Pts',(-3.41789282565394,6.12465728644501,-6.56409178119931));
#24093=CARTESIAN_POINT('Ctrl Pts',(-3.84189576222056,5.87280710540862,-6.54176298274265));
#24094=CARTESIAN_POINT('Ctrl Pts',(-4.09287151809201,5.70073961859469,-6.52815439597193));
#24095=CARTESIAN_POINT('Ctrl Pts',(-4.50262227913299,5.37877003992366,-6.50480700081698));
#24096=CARTESIAN_POINT('Ctrl Pts',(-4.66702908684039,5.2367558254219,-6.49508142677324));
#24097=CARTESIAN_POINT('Ctrl Pts',(-4.90846581330569,5.00778953466546,-6.48000090135578));
#24098=CARTESIAN_POINT('Ctrl Pts',(-4.9903714161686,4.92617345323335,-6.47472556069264));
#24099=CARTESIAN_POINT('Ctrl Pts',(-5.25826271359213,4.64568858880247,-6.45695840972673));
#24100=CARTESIAN_POINT('Ctrl Pts',(-5.43467776796553,4.43802062151827,-6.44440223021673));
#24101=CARTESIAN_POINT('Ctrl Pts',(-5.72651142781564,4.05090913540504,-6.42215566534128));
#24102=CARTESIAN_POINT('Ctrl Pts',(-5.84667166910733,3.87546519868902,-6.41244980528081));
#24103=CARTESIAN_POINT('Ctrl Pts',(-6.07033880171417,3.514755915509,-6.39318884680505));
#24104=CARTESIAN_POINT('Ctrl Pts',(-6.17378039797205,3.32970866586246,-6.38364319269721));
#24105=CARTESIAN_POINT('Ctrl Pts',(-6.3984520465339,2.88121212588124,-6.36112372107576));
#24106=CARTESIAN_POINT('Ctrl Pts',(-6.51203712877862,2.61437218374742,-6.34820587646107));
#24107=CARTESIAN_POINT('Ctrl Pts',(-6.64484320577531,2.23949640543405,-6.3302760460809));
#24108=CARTESIAN_POINT('Ctrl Pts',(-6.67854312086716,2.13690123503765,-6.3253871362613));
#24109=CARTESIAN_POINT('Ctrl Pts',(-6.76984834968026,1.83563500788081,-6.31104229493326));
#24110=CARTESIAN_POINT('Ctrl Pts',(-6.82104814237988,1.63514627549764,-6.30153036791633));
#24111=CARTESIAN_POINT('Ctrl Pts',(-6.90610487471028,1.22768153889449,-6.28238133669502));
#24112=CARTESIAN_POINT('Ctrl Pts',(-6.93969300269204,1.02085688592325,-6.27275397964097));
#24113=CARTESIAN_POINT('Ctrl Pts',(-6.97400667889152,0.726875324778639,
-6.25921896890452));
#24114=CARTESIAN_POINT('Ctrl Pts',(-6.98244783564724,0.640733382814972,
-6.25527035484034));
#24115=CARTESIAN_POINT('Ctrl Pts',(-7.00392758728411,0.369967034499953,
-6.24290898893682));
#24116=CARTESIAN_POINT('Ctrl Pts',(-7.01125277045169,0.184968370858522,
-6.23453801484205));
#24117=CARTESIAN_POINT('Ctrl Pts',(-7.01124677665848,-0.215320004964521,
-6.21651180210464));
#24118=CARTESIAN_POINT('Ctrl Pts',(-7.00133432271619,-0.430421342449451,
-6.20687998953804));
#24119=CARTESIAN_POINT('Ctrl Pts',(-6.96294211853579,-0.846158790037305,
-6.18817303064746));
#24120=CARTESIAN_POINT('Ctrl Pts',(-6.93563167370119,-1.04668951243584,
-6.17910730173908));
#24121=CARTESIAN_POINT('Ctrl Pts',(-6.87975920415703,-1.35614245711543,
-6.16486257391386));
#24122=CARTESIAN_POINT('Ctrl Pts',(-6.85718273817151,-1.46603312094027,
-6.15974794181732));
#24123=CARTESIAN_POINT('Ctrl Pts',(-6.81409091533509,-1.65291580623209,
-6.15096724362044));
#24124=CARTESIAN_POINT('Ctrl Pts',(-6.79488156059996,-1.73018789276738,
-6.14731269945627));
#24125=CARTESIAN_POINT('Ctrl Pts',(-6.71706876478634,-2.02188583155679,
-6.13343855391773));
#24126=CARTESIAN_POINT('Ctrl Pts',(-6.64962111007924,-2.23371632153885,
-6.12320548606609));
#24127=CARTESIAN_POINT('Ctrl Pts',(-6.57227174271038,-2.44189899514102,
-6.11302261786463));
#24128=CARTESIAN_POINT('',(-7.01124999933522,9.65497915988582E-5,-6.77353435691037));
#24129=CARTESIAN_POINT('Ctrl Pts',(-6.5722714983487,-2.44189965283043,-6.66023848729892));
#24130=CARTESIAN_POINT('Ctrl Pts',(-6.66318645252301,-2.19720582956012,
-6.67224691572112));
#24131=CARTESIAN_POINT('Ctrl Pts',(-6.74040831275645,-1.94750920134252,
-6.6842496182875));
#24132=CARTESIAN_POINT('Ctrl Pts',(-6.84556497205163,-1.52516452324806,
-6.70410727531474));
#24133=CARTESIAN_POINT('Ctrl Pts',(-6.88129720898833,-1.35485666965225,
-6.71200071435652));
#24134=CARTESIAN_POINT('Ctrl Pts',(-6.97760540239254,-0.792446624908524,
-6.73777021356879));
#24135=CARTESIAN_POINT('Ctrl Pts',(-7.011256159715,-0.396526017179738,-6.75540657027142));
#24136=CARTESIAN_POINT('Ctrl Pts',(-7.01124999915429,0.000108899215703687,
-6.77325998610253));
#24137=CARTESIAN_POINT('Ctrl Pts',(-7.01124999933522,9.65497915988582E-5,
-6.77353435691037));
#24138=CARTESIAN_POINT('Ctrl Pts',(-7.01124863601993,0.0990977407168242,
-6.77803027512839));
#24139=CARTESIAN_POINT('Ctrl Pts',(-7.00915014456632,0.198092936793512,
-6.78252619334641));
#24140=CARTESIAN_POINT('Ctrl Pts',(-7.00495668404128,0.296999018862735,
-6.78702211156443));
#24141=CARTESIAN_POINT('Ctrl Pts',(-6.99699833034792,0.484703083043638,
-6.79555446977832));
#24142=CARTESIAN_POINT('Ctrl Pts',(-6.98148974930442,0.672118710222703,
-6.80408682799221));
#24143=CARTESIAN_POINT('Ctrl Pts',(-6.95847548566115,0.858630000613053,
-6.8126191862061));
#24144=CARTESIAN_POINT('Ctrl Pts',(-6.93546553152443,1.04510636606995,-6.82114994670415));
#24145=CARTESIAN_POINT('Ctrl Pts',(-6.90495273703956,1.23067842912626,-6.8296807072022));
#24146=CARTESIAN_POINT('Ctrl Pts',(-6.86703342573335,1.41473619179017,-6.83821146770025));
#24147=CARTESIAN_POINT('Ctrl Pts',(-6.82748037163525,1.60672403104786,-6.84710977359913));
#24148=CARTESIAN_POINT('Ctrl Pts',(-6.77986849624805,1.79706384305653,-6.856008079498));
#24149=CARTESIAN_POINT('Ctrl Pts',(-6.72436639184499,1.985075109593,-6.86490638539687));
#24150=CARTESIAN_POINT('Ctrl Pts',(-6.67115844925952,2.16531499027655,-6.873436882654));
#24151=CARTESIAN_POINT('Ctrl Pts',(-6.61069953595977,2.34341464114204,-6.88196737991113));
#24152=CARTESIAN_POINT('Ctrl Pts',(-6.54318928729106,2.5187894936218,-6.89049787716825));
#24153=CARTESIAN_POINT('Ctrl Pts',(-6.47567834775357,2.69416614080698,-6.89902846172256));
#24154=CARTESIAN_POINT('Ctrl Pts',(-6.4011160415954,2.86681764949735,-6.90755904627686));
#24155=CARTESIAN_POINT('Ctrl Pts',(-6.31975051686545,3.03617851370417,-6.91608963083117));
#24156=CARTESIAN_POINT('Ctrl Pts',(-6.23836889177823,3.20557289051269,-6.92462190339104));
#24157=CARTESIAN_POINT('Ctrl Pts',(-6.1501814927871,3.37167504694702,-6.93315417595092));
#24158=CARTESIAN_POINT('Ctrl Pts',(-6.05548326369799,3.53394241684462,-6.9416864485108));
#24159=CARTESIAN_POINT('Ctrl Pts',(-6.0432572013677,3.55489202696535,-6.9427880118361));
#24160=CARTESIAN_POINT('Ctrl Pts',(-6.03092267699221,3.57577775305031,-6.94388957516141));
#24161=CARTESIAN_POINT('Ctrl Pts',(-6.01848037998311,3.59659845941388,-6.94499113848672));
#24162=CARTESIAN_POINT('Ctrl Pts',(-5.92210631537392,3.75786901089051,-6.95352349670053));
#24163=CARTESIAN_POINT('Ctrl Pts',(-5.81923020290197,3.91529086095874,-6.96205585491435));
#24164=CARTESIAN_POINT('Ctrl Pts',(-5.71018447586611,4.06834362045263,-6.97058821312816));
#24165=CARTESIAN_POINT('Ctrl Pts',(-5.60115916804912,4.22136772024681,-6.9791189736261));
#24166=CARTESIAN_POINT('Ctrl Pts',(-5.48596672866419,4.37002411305193,-6.98764973412403));
#24167=CARTESIAN_POINT('Ctrl Pts',(-5.36498231317679,4.51382225412125,-6.99618049462197));
#24168=CARTESIAN_POINT('Ctrl Pts',(-5.23878531839894,4.66381589738911,-7.00507880052089));
#24169=CARTESIAN_POINT('Ctrl Pts',(-5.10628640973121,4.80852309802423,-7.01397710641981));
#24170=CARTESIAN_POINT('Ctrl Pts',(-4.9679578714695,4.94742570937697,-7.02287541231873));
#24171=CARTESIAN_POINT('Ctrl Pts',(-4.83534709930489,5.08058682550413,-7.03140590957577));
#24172=CARTESIAN_POINT('Ctrl Pts',(-4.69737917042236,5.2084133346288,-7.03993640683282));
#24173=CARTESIAN_POINT('Ctrl Pts',(-4.55450798055408,5.33048624588501,-7.04846690408987));
#24174=CARTESIAN_POINT('Ctrl Pts',(-4.41163532860805,5.45256040637898,-7.05699748864408));
#24175=CARTESIAN_POINT('Ctrl Pts',(-4.26385955013853,5.56888065504471,-7.06552807319829));
#24176=CARTESIAN_POINT('Ctrl Pts',(-4.11166812443973,5.67906786338799,-7.0740586577525));
#24177=CARTESIAN_POINT('Ctrl Pts',(-3.95944658357395,5.7892768752341,-7.08259093031231));
#24178=CARTESIAN_POINT('Ctrl Pts',(-3.80280789877975,5.8933502442502,-7.09112320287213));
#24179=CARTESIAN_POINT('Ctrl Pts',(-3.64226977693333,5.9909512962916,-7.09965547543194));
#24180=CARTESIAN_POINT('Ctrl Pts',(-3.62154342224158,6.00355212903856,-7.10075703875763));
#24181=CARTESIAN_POINT('Ctrl Pts',(-3.60075210863097,6.01604514006157,-7.10185860208332));
#24182=CARTESIAN_POINT('Ctrl Pts',(-3.579896983104,6.02842965894626,-7.10296016540901));
#24183=CARTESIAN_POINT('Ctrl Pts',(-3.41835983181976,6.12435619259727,-7.11149252362288));
#24184=CARTESIAN_POINT('Ctrl Pts',(-3.25293759185572,6.21380235473948,-7.12002488183674));
#24185=CARTESIAN_POINT('Ctrl Pts',(-3.08417037731232,6.29646882357161,-7.12855724005061));
#24186=CARTESIAN_POINT('Ctrl Pts',(-2.91543476505835,6.37911981279959,-7.13708800054863));
#24187=CARTESIAN_POINT('Ctrl Pts',(-2.74335570288113,6.45499350767575,-7.14561876104664));
#24188=CARTESIAN_POINT('Ctrl Pts',(-2.5684966626596,6.52383717273864,-7.15414952154466));
#24189=CARTESIAN_POINT('Ctrl Pts',(-2.38610387019533,6.5956469476201,-7.16304782744355));
#24190=CARTESIAN_POINT('Ctrl Pts',(-2.20068656367054,6.65980734938466,-7.17194613334243));
#24191=CARTESIAN_POINT('Ctrl Pts',(-2.01290676914844,6.71608761863754,-7.18084443924132));
#24192=CARTESIAN_POINT('Ctrl Pts',(-1.8328887926581,6.77004156087621,-7.18937493649842));
#24193=CARTESIAN_POINT('Ctrl Pts',(-1.65070001986582,6.81675362467153,-7.19790543375552));
#24194=CARTESIAN_POINT('Ctrl Pts',(-1.46693909333062,6.85607148875786,-7.20643593101262));
#24195=CARTESIAN_POINT('Ctrl Pts',(-1.28317628627086,6.89538975520507,-7.21496651556689));
#24196=CARTESIAN_POINT('Ctrl Pts',(-1.09784159320205,6.92731360988333,-7.22349710012117));
#24197=CARTESIAN_POINT('Ctrl Pts',(-0.911544208239695,6.95174177590945,
-7.23202768467544));
#24198=CARTESIAN_POINT('Ctrl Pts',(-0.725209959329071,6.97617477570524,
-7.24055995723531));
#24199=CARTESIAN_POINT('Ctrl Pts',(-0.53791294157442,6.99310908564372,-7.24909222979517));
#24200=CARTESIAN_POINT('Ctrl Pts',(-0.350268715347124,7.00249515455377,
-7.25762450235504));
#24201=CARTESIAN_POINT('Ctrl Pts',(-0.326042813468306,7.00370694768493,
-7.25872606568046));
#24202=CARTESIAN_POINT('Ctrl Pts',(-0.301811128741185,7.00479299605895,
-7.25982762900588));
#24203=CARTESIAN_POINT('Ctrl Pts',(-0.277574989016474,7.00575325628676,
-7.2609291923313));
#24204=CARTESIAN_POINT('Ctrl Pts',(-0.0898495799762465,7.01319112577006,
-7.26946155054498));
#24205=CARTESIAN_POINT('Ctrl Pts',(0.0982065849262575,7.01308050338434,
-7.27799390875866));
#24206=CARTESIAN_POINT('Ctrl Pts',(0.285976026660581,7.00541535347301,-7.28652626697234));
#24207=CARTESIAN_POINT('Ctrl Pts',(0.473710307867381,6.99775163888957,-7.29505702747016));
#24208=CARTESIAN_POINT('Ctrl Pts',(0.661157667450691,6.98253623230385,-7.30358778796797));
#24209=CARTESIAN_POINT('Ctrl Pts',(0.847702268630839,6.95981518621423,-7.31211854846579));
#24210=CARTESIAN_POINT('Ctrl Pts',(1.04228409114593,6.93611521028568,-7.32101685436477));
#24211=CARTESIAN_POINT('Ctrl Pts',(1.23588328914722,6.90424853101664,-7.32991516026376));
#24212=CARTESIAN_POINT('Ctrl Pts',(1.42780782494883,6.86432745267261,-7.33881346616274));
#24213=CARTESIAN_POINT('Ctrl Pts',(1.6117992211513,6.82605649939534,-7.34734396341966));
#24214=CARTESIAN_POINT('Ctrl Pts',(1.79425129499713,6.78038367833687,-7.35587446067657));
#24215=CARTESIAN_POINT('Ctrl Pts',(1.97456509440875,6.72746008910068,-7.36440495793349));
#24216=CARTESIAN_POINT('Ctrl Pts',(2.15488073906813,6.67453595826904,-7.37293554248756));
#24217=CARTESIAN_POINT('Ctrl Pts',(2.33305777288524,6.6143610002643,-7.38146612704163));
#24218=CARTESIAN_POINT('Ctrl Pts',(2.50851227005532,6.54713622536464,-7.38999671159569));
#24219=CARTESIAN_POINT('Ctrl Pts',(2.68400148561692,6.4798981482351,-7.39852898415537));
#24220=CARTESIAN_POINT('Ctrl Pts',(2.85676680316711,6.40560757842274,-7.40706125671504));
#24221=CARTESIAN_POINT('Ctrl Pts',(3.02624332798783,6.32451404317432,-7.41559352927471));
#24222=CARTESIAN_POINT('Ctrl Pts',(3.04812367968835,6.31404442165151,-7.41669509260101));
#24223=CARTESIAN_POINT('Ctrl Pts',(3.06994924291153,6.30346147136764,-7.4177966559273));
#24224=CARTESIAN_POINT('Ctrl Pts',(3.09171882933523,6.29276578642762,-7.4188982192536));
#24225=CARTESIAN_POINT('Ctrl Pts',(3.2603391030037,6.20992042195642,-7.42743057746784));
#24226=CARTESIAN_POINT('Ctrl Pts',(3.42565599669263,6.12027970542203,-7.43596293568208));
#24227=CARTESIAN_POINT('Ctrl Pts',(3.58712364851388,6.02413234356388,-7.44449529389633));
#24228=CARTESIAN_POINT('Ctrl Pts',(3.74856106491592,5.92800298565736,-7.45302605439471));
#24229=CARTESIAN_POINT('Ctrl Pts',(3.90615041507801,5.82536957037538,-7.4615568148931));
#24230=CARTESIAN_POINT('Ctrl Pts',(4.0593720831585,5.71656582687311,-7.47008757539149));
#24231=CARTESIAN_POINT('Ctrl Pts',(4.21919526341856,5.60307430489335,-7.47898588129019));
#24232=CARTESIAN_POINT('Ctrl Pts',(4.37426576303269,5.48286916830926,-7.48788418718889));
#24233=CARTESIAN_POINT('Ctrl Pts',(4.52402850388267,5.3563786888678,-7.49678249308758));
#24234=CARTESIAN_POINT('Ctrl Pts',(4.66760084952214,5.23511665312112,-7.50531299034507));
#24235=CARTESIAN_POINT('Ctrl Pts',(4.80629515369704,5.10807864373767,-7.51384348760255));
#24236=CARTESIAN_POINT('Ctrl Pts',(4.93965666679844,4.97568272467746,-7.52237398486003));
#24237=CARTESIAN_POINT('Ctrl Pts',(5.07301954465978,4.84328545073876,-7.53090456941467));
#24238=CARTESIAN_POINT('Ctrl Pts',(5.20104930753212,4.70553037542654,-7.53943515396931));
#24239=CARTESIAN_POINT('Ctrl Pts',(5.32332818444906,4.56287229748437,-7.54796573852394));
#24240=CARTESIAN_POINT('Ctrl Pts',(5.44563125753062,4.42018599080453,-7.55649801108418));
#24241=CARTESIAN_POINT('Ctrl Pts',(5.56218097344032,4.27259497672405,-7.56503028364441));
#24242=CARTESIAN_POINT('Ctrl Pts',(5.67259939792121,4.12058765629418,-7.57356255620464));
#24243=CARTESIAN_POINT('Ctrl Pts',(5.68685502393588,4.10096267503106,-7.57466411952838));
#24244=CARTESIAN_POINT('Ctrl Pts',(5.70100850922188,4.08126412436716,-7.57576568285213));
#24245=CARTESIAN_POINT('Ctrl Pts',(5.71505909169771,4.06149309255886,-7.57686724617588));
#24246=CARTESIAN_POINT('Ctrl Pts',(5.82389042277079,3.90835298522979,-7.58539960438884));
#24247=CARTESIAN_POINT('Ctrl Pts',(5.92658126006258,3.75081021222637,-7.59393196260179));
#24248=CARTESIAN_POINT('Ctrl Pts',(6.02278906149478,3.58937856504978,-7.60246432081475));
#24249=CARTESIAN_POINT('Ctrl Pts',(6.11897884765776,3.4279771465505,-7.61099508131185));
#24250=CARTESIAN_POINT('Ctrl Pts',(6.20868786402269,3.26268856984488,-7.61952584180895));
#24251=CARTESIAN_POINT('Ctrl Pts',(6.29161808584625,3.09405372034042,-7.62805660230605));
#24252=CARTESIAN_POINT('Ctrl Pts',(6.37812133281203,2.91815328606017,-7.63695490820539));
#24253=CARTESIAN_POINT('Ctrl Pts',(6.45724854463107,2.73861215130986,-7.64585321410474));
#24254=CARTESIAN_POINT('Ctrl Pts',(6.52871552906318,2.5560712241777,-7.65475152000408));
#24255=CARTESIAN_POINT('Ctrl Pts',(6.59722844843272,2.38107556818878,-7.66328201726028));
#24256=CARTESIAN_POINT('Ctrl Pts',(6.65870155525924,2.20332342905852,-7.67181251451649));
#24257=CARTESIAN_POINT('Ctrl Pts',(6.71293402198145,2.02339896684367,-7.68034301177269));
#24258=CARTESIAN_POINT('Ctrl Pts',(6.76716704369365,1.84347266336501,-7.68887359632606));
#24259=CARTESIAN_POINT('Ctrl Pts',(6.8141591920312,1.66137428627281,-7.69740418087943));
#24260=CARTESIAN_POINT('Ctrl Pts',(6.85375964843389,1.47770269134199,-7.7059347654328));
#24261=CARTESIAN_POINT('Ctrl Pts',(6.89336794085206,1.29399475204569,-7.71446703799178));
#24262=CARTESIAN_POINT('Ctrl Pts',(6.92558155650885,1.10871327247536,-7.72299931055076));
#24263=CARTESIAN_POINT('Ctrl Pts',(6.95030070758579,0.9224676886658,-7.73153158310974));
#24264=CARTESIAN_POINT('Ctrl Pts',(6.9534920859875,0.898422359126289,-7.73263314643922));
#24265=CARTESIAN_POINT('Ctrl Pts',(6.95655861538205,0.874360969981249,-7.73373470976869));
#24266=CARTESIAN_POINT('Ctrl Pts',(6.95950014379962,0.85028484106981,-7.73483627309817));
#24267=CARTESIAN_POINT('Ctrl Pts',(6.98228428474481,0.663798825413119,-7.74336863131337));
#24268=CARTESIAN_POINT('Ctrl Pts',(6.99757236394241,0.476365082341321,-7.75190098952856));
#24269=CARTESIAN_POINT('Ctrl Pts',(7.00530780586358,0.288598523223641,-7.76043334774376));
#24270=CARTESIAN_POINT('Ctrl Pts',(7.01304179929443,0.100867124093482,-7.7689641082431));
#24271=CARTESIAN_POINT('Ctrl Pts',(7.01322596520084,-0.0871966611166099,
-7.77749486874244));
#24272=CARTESIAN_POINT('Ctrl Pts',(7.00585577577047,-0.274975292714809,
-7.78602562924178));
#24273=CARTESIAN_POINT('Ctrl Pts',(6.99816804381687,-0.470844313447413,
-7.79492393514001));
#24274=CARTESIAN_POINT('Ctrl Pts',(6.98226057294049,-0.666402711573646,
-7.80382224103823));
#24275=CARTESIAN_POINT('Ctrl Pts',(6.95818862517891,-0.860951577576125,
-7.81272054693645));
#24276=CARTESIAN_POINT('Ctrl Pts',(6.93511168371009,-1.04745882817475,-7.82125104419488));
#24277=CARTESIAN_POINT('Ctrl Pts',(6.90453168732619,-1.23303800175695,-7.82978154145329));
#24278=CARTESIAN_POINT('Ctrl Pts',(6.8665501851245,-1.41707978521563,-7.83831203871172));
#24279=CARTESIAN_POINT('Ctrl Pts',(6.82856829423773,-1.60112345207257,-7.84684262326729));
#24280=CARTESIAN_POINT('Ctrl Pts',(6.78318481119027,-1.78362939835818,-7.85537320782286));
#24281=CARTESIAN_POINT('Ctrl Pts',(6.730552258532,-1.96399920001761,-7.86390379237844));
#24282=CARTESIAN_POINT('Ctrl Pts',(6.67790929110769,-2.14440469269313,-7.87243606493959));
#24283=CARTESIAN_POINT('Ctrl Pts',(6.61801447579919,-2.32267290304711,-7.88096833750074));
#24284=CARTESIAN_POINT('Ctrl Pts',(6.55107024750312,-2.49822040156176,-7.88950061006189));
#24285=CARTESIAN_POINT('Ctrl Pts',(6.54242737940247,-2.52088454922139,-7.89060217338141));
#24286=CARTESIAN_POINT('Ctrl Pts',(6.53366707692705,-2.54350337191474,-7.89170373670093));
#24287=CARTESIAN_POINT('Ctrl Pts',(6.52478983488515,-2.56607563666377,-7.89280530002046));
#24288=CARTESIAN_POINT('Ctrl Pts',(6.45602954875569,-2.74091320168762,-7.90133765823293));
#24289=CARTESIAN_POINT('Ctrl Pts',(6.38022624302496,-2.91301489321258,-7.90987001644539));
#24290=CARTESIAN_POINT('Ctrl Pts',(6.29762295895764,-3.08181304256271,-7.91840237465786));
#24291=CARTESIAN_POINT('Ctrl Pts',(6.21503514266295,-3.25057958383062,-7.92693313515447));
#24292=CARTESIAN_POINT('Ctrl Pts',(6.12565002355203,-3.41604354269852,-7.93546389565108));
#24293=CARTESIAN_POINT('Ctrl Pts',(6.02975766319005,-3.57765972189934,-7.9439946561477));
#24294=CARTESIAN_POINT('Ctrl Pts',(5.92973380760608,-3.74623908846612,-7.95289296204728));
#24295=CARTESIAN_POINT('Ctrl Pts',(5.82262972442264,-3.9106314547288,-7.96179126794687));
#24296=CARTESIAN_POINT('Ctrl Pts',(5.7088267966233,-4.07024853892925,-7.97068957384646));
#24297=CARTESIAN_POINT('Ctrl Pts',(5.59972787664448,-4.22326790172758,-7.97922007110219));
#24298=CARTESIAN_POINT('Ctrl Pts',(5.48447295676529,-4.37189854886369,-7.98775056835792));
#24299=CARTESIAN_POINT('Ctrl Pts',(5.36344146151282,-4.5156530260224,-7.99628106561365));
#24300=CARTESIAN_POINT('Ctrl Pts',(5.24240872767983,-4.65940897429815,-8.00481165016655));
#24301=CARTESIAN_POINT('Ctrl Pts',(5.11559949989041,-4.7982884209006,-8.01334223471946));
#24302=CARTESIAN_POINT('Ctrl Pts',(4.98343284197084,-4.93183775808434,-8.02187281927236));
#24303=CARTESIAN_POINT('Ctrl Pts',(4.85124003132286,-5.06541352159678,-8.03040509183089));
#24304=CARTESIAN_POINT('Ctrl Pts',(4.71368788915149,-5.19365685236146,-8.03893736438941));
#24305=CARTESIAN_POINT('Ctrl Pts',(4.57123223064792,-5.31615109416443,-8.04746963694793));
#24306=CARTESIAN_POINT('Ctrl Pts',(4.55284042134847,-5.33196577474073,-8.04857120027954));
#24307=CARTESIAN_POINT('Ctrl Pts',(4.53436692624702,-5.34768468154511,-8.04967276361114));
#24308=CARTESIAN_POINT('Ctrl Pts',(4.51581276754526,-5.36330696594696,-8.05077432694275));
#24309=CARTESIAN_POINT('Ctrl Pts',(4.37209817225324,-5.48431219805896,-8.05930668515607));
#24310=CARTESIAN_POINT('Ctrl Pts',(4.22349290199429,-5.59955805283533,-8.0678390433694));
#24311=CARTESIAN_POINT('Ctrl Pts',(4.0704809751167,-5.70866106838662,-8.07637140158272));
#24312=CARTESIAN_POINT('Ctrl Pts',(3.9174977002926,-5.81774365399168,-8.08490216208018));
#24313=CARTESIAN_POINT('Ctrl Pts',(3.76010966460322,-5.92068551831789,-8.09343292257763));
#24314=CARTESIAN_POINT('Ctrl Pts',(3.59883153447204,-6.01714534883358,-8.10196368307508));
#24315=CARTESIAN_POINT('Ctrl Pts',(3.4306047817481,-6.11776112384758,-8.11086198897425));
#24316=CARTESIAN_POINT('Ctrl Pts',(3.25814559259368,-6.21132373813366,-8.11976029487341));
#24317=CARTESIAN_POINT('Ctrl Pts',(3.08206945287029,-6.29749747520266,-8.12865860077257));
#24318=CARTESIAN_POINT('Ctrl Pts',(2.91327136434961,-6.380109248273,-8.1371890980291));
#24319=CARTESIAN_POINT('Ctrl Pts',(2.74114961801278,-6.45593055312099,-8.14571959528563));
#24320=CARTESIAN_POINT('Ctrl Pts',(2.56626996827503,-6.52471340462013,-8.15425009254217));
#24321=CARTESIAN_POINT('Ctrl Pts',(2.39138852890024,-6.593496960011,-8.16278067709584));
#24322=CARTESIAN_POINT('Ctrl Pts',(2.21374941565735,-6.65524180913895,-8.17131126164952));
#24323=CARTESIAN_POINT('Ctrl Pts',(2.03393712414705,-6.70974860464358,-8.17984184620319));
#24324=CARTESIAN_POINT('Ctrl Pts',(1.85408925193832,-6.76426618578381,-8.18837411876248));
#24325=CARTESIAN_POINT('Ctrl Pts',(1.67206763570726,-6.81154276489854,-8.19690639132176));
#24326=CARTESIAN_POINT('Ctrl Pts',(1.48847149426284,-6.8514289876833,-8.20543866388105));
#24327=CARTESIAN_POINT('Ctrl Pts',(1.4647682223418,-6.85657851848025,-8.20654022720904));
#24328=CARTESIAN_POINT('Ctrl Pts',(1.44103872191223,-6.86160493449024,-8.20764179053704));
#24329=CARTESIAN_POINT('Ctrl Pts',(1.41728429593782,-6.86650797618324,-8.20874335386504));
#24330=CARTESIAN_POINT('Ctrl Pts',(1.23329008826146,-6.90448537342617,-8.21727571208572));
#24331=CARTESIAN_POINT('Ctrl Pts',(1.04773754642442,-6.93506948156557,-8.2258080703064));
#24332=CARTESIAN_POINT('Ctrl Pts',(0.861234884474282,-6.95815356515395,
-8.23434042852708));
#24333=CARTESIAN_POINT('Ctrl Pts',(0.674767145841206,-6.98123332616182,
-8.24287118903195));
#24334=CARTESIAN_POINT('Ctrl Pts',(0.487349945684015,-6.99681582772935,
-8.25140194953683));
#24335=CARTESIAN_POINT('Ctrl Pts',(0.299598379294797,-7.00484599214172,
-8.2599327100417));
#24336=CARTESIAN_POINT('Ctrl Pts',(0.103757590055591,-7.0132221339044,-8.26883101593717));
#24337=CARTESIAN_POINT('Ctrl Pts',(-0.0924466645823951,-7.01338070381287,
-8.27772932183264));
#24338=CARTESIAN_POINT('Ctrl Pts',(-0.288313297052236,-7.00531955054464,
-8.28662762772811));
#24339=CARTESIAN_POINT('Ctrl Pts',(-0.476083844840867,-6.99759160247151,
-8.29515812499206));
#24340=CARTESIAN_POINT('Ctrl Pts',(-0.663543793791819,-6.98230980183732,
-8.30368862225601));
#24341=CARTESIAN_POINT('Ctrl Pts',(-0.850077561831749,-6.95952546524332,
-8.31221911951996));
#24342=CARTESIAN_POINT('Ctrl Pts',(-1.03661323877084,-6.93674089548509,
-8.32074970408102));
#24343=CARTESIAN_POINT('Ctrl Pts',(-1.22222241253063,-6.90645367665657,
-8.32928028864208));
#24344=CARTESIAN_POINT('Ctrl Pts',(-1.40629617974004,-6.86876681925865,
-8.33781087320314));
#24345=CARTESIAN_POINT('Ctrl Pts',(-1.59040637089355,-6.8310725045027,-8.34634314576972));
#24346=CARTESIAN_POINT('Ctrl Pts',(-1.77298024911097,-6.78597568907706,
-8.3548754183363));
#24347=CARTESIAN_POINT('Ctrl Pts',(-1.95341976830739,-6.73363035600306,
-8.36340769090288));
#24348=CARTESIAN_POINT('Ctrl Pts',(-1.97671550220829,-6.72687228573289,
-8.3645092541977));
#24349=CARTESIAN_POINT('Ctrl Pts',(-1.99997567905117,-6.71999346415156,
-8.36561081749251));
#24350=CARTESIAN_POINT('Ctrl Pts',(-2.02319902948267,-6.71299428344762,
-8.36671238078733));
#24351=CARTESIAN_POINT('Ctrl Pts',(-2.20307970019863,-6.65878086048782,
-8.37524473897966));
#24352=CARTESIAN_POINT('Ctrl Pts',(-2.38081037766226,-6.59732405037942,
-8.38377709717198));
#24353=CARTESIAN_POINT('Ctrl Pts',(-2.5558053987975,-6.52881959667883,-8.39230945536431));
#24354=CARTESIAN_POINT('Ctrl Pts',(-2.73076765146093,-6.46032797069327,
-8.40084021584067));
#24355=CARTESIAN_POINT('Ctrl Pts',(-2.90299498527226,-6.3847914462397,-8.40937097631704));
#24356=CARTESIAN_POINT('Ctrl Pts',(-3.07192028301177,-6.3024544692779,-8.4179017367934));
#24357=CARTESIAN_POINT('Ctrl Pts',(-3.24812368004017,-6.2165700266523,-8.42680004270309));
#24358=CARTESIAN_POINT('Ctrl Pts',(-3.4207338764258,-6.12328629325861,-8.43569834861277));
#24359=CARTESIAN_POINT('Ctrl Pts',(-3.58913333758728,-6.02293520200239,
-8.44459665452246));
#24360=CARTESIAN_POINT('Ctrl Pts',(-3.7505720600242,-5.92673209151845,-8.45312715175804));
#24361=CARTESIAN_POINT('Ctrl Pts',(-3.90814086663486,-5.82403429775449,
-8.46165764899363));
#24362=CARTESIAN_POINT('Ctrl Pts',(-4.06132287207676,-5.71518005764002,
-8.47018814622922));
#24363=CARTESIAN_POINT('Ctrl Pts',(-4.21450644511474,-5.60632470355998,
-8.4787187307621));
#24364=CARTESIAN_POINT('Ctrl Pts',(-4.36330287973525,-5.49131295711294,
-8.48724931529497));
#24365=CARTESIAN_POINT('Ctrl Pts',(-4.50722577778393,-5.37052533283105,
-8.49577989982785));
#24366=CARTESIAN_POINT('Ctrl Pts',(-4.65117715485464,-5.24971380746421,
-8.50431217236666));
#24367=CARTESIAN_POINT('Ctrl Pts',(-4.79025283551472,-5.12312431901584,
-8.51284444490546));
#24368=CARTESIAN_POINT('Ctrl Pts',(-4.92400023980192,-4.99117703562303,
-8.52137671744426));
#24369=CARTESIAN_POINT('Ctrl Pts',(-4.94126776702301,-4.97414191393317,
-8.52247828086605));
#24370=CARTESIAN_POINT('Ctrl Pts',(-4.95844653061949,-4.95701753861724,
-8.52357984428784));
#24371=CARTESIAN_POINT('Ctrl Pts',(-4.9755356011107,-4.93980485895749,-8.52468140770962));
#24372=CARTESIAN_POINT('Ctrl Pts',(-5.10790102723548,-4.80648200332974,
-8.53321369808804));
#24373=CARTESIAN_POINT('Ctrl Pts',(-5.23492695661218,-4.66781339360536,
-8.54174598846645));
#24374=CARTESIAN_POINT('Ctrl Pts',(-5.35619159273083,-4.52425001347843,
-8.55027827884486));
#24375=CARTESIAN_POINT('Ctrl Pts',(-5.47743312604602,-4.38071398441329,
-8.55880894368895));
#24376=CARTESIAN_POINT('Ctrl Pts',(-5.59291535928422,-4.2322852796589,-8.56733960853305));
#24377=CARTESIAN_POINT('Ctrl Pts',(-5.70225599664267,-4.07944887346964,
-8.57587027337714));
#24378=CARTESIAN_POINT('Ctrl Pts',(-5.81159359130132,-3.92661672036792,
-8.58440070083235));
#24379=CARTESIAN_POINT('Ctrl Pts',(-5.91478975087791,-3.76937735782259,
-8.59293112828756));
#24380=CARTESIAN_POINT('Ctrl Pts',(-6.01150434705256,-3.60824639511609,
-8.60146155574276));
#24381=CARTESIAN_POINT('Ctrl Pts',(-6.10821283211414,-3.44712561380484,
-8.60999144418516));
#24382=CARTESIAN_POINT('Ctrl Pts',(-6.19844041559358,-3.28211398657138,
-8.61852133262755));
#24383=CARTESIAN_POINT('Ctrl Pts',(-6.2818917023905,-3.11375387626213,-8.62705122106994));
#24384=CARTESIAN_POINT('Ctrl Pts',(-6.36535301325014,-2.94537354274997,
-8.63558213411172));
#24385=CARTESIAN_POINT('Ctrl Pts',(-6.44203626553885,-2.77364419685501,
-8.64411304715349));
#24386=CARTESIAN_POINT('Ctrl Pts',(-6.51169282550364,-2.59913122192483,
-8.65264396019526));
#24387=CARTESIAN_POINT('Ctrl Pts',(-6.53251525701584,-2.54696406824526,
-8.65519410554609));
#24388=CARTESIAN_POINT('Ctrl Pts',(-6.55271011457438,-2.49454831123339,
-8.65774425089692));
#24389=CARTESIAN_POINT('Ctrl Pts',(-6.57227159525839,-2.441899392002,-8.66029439624775));
#24390=CARTESIAN_POINT('Origin',(0.,0.,0.));
#24391=CARTESIAN_POINT('',(-6.57172397189,-2.44169584043396,-10.6602982140525));
#24392=CARTESIAN_POINT('',(-6.57227159525839,-2.44189939200199,-10.1135674911542));
#24393=CARTESIAN_POINT('',(-6.57227159525839,-2.441899392002,0.));
#24394=CARTESIAN_POINT('',(-7.01124021554704,-0.000177496958404323,-10.7735343566727));
#24395=CARTESIAN_POINT('Ctrl Pts',(-6.57172397189039,-2.44169584043291,
-10.6602982140526));
#24396=CARTESIAN_POINT('Ctrl Pts',(-6.766036100056,-1.91888078236536,-10.6856147375756));
#24397=CARTESIAN_POINT('Ctrl Pts',(-6.96373099417918,-1.10522974870895,
-10.7233601182964));
#24398=CARTESIAN_POINT('Ctrl Pts',(-7.01150624902316,-0.273937984959162,
-10.7611054990171));
#24399=CARTESIAN_POINT('Ctrl Pts',(-7.01123043334559,-0.000177506793261869,
-10.7735343562149));
#24400=CARTESIAN_POINT('',(5.31037376991254,-4.57794244025905,-12.));
#24401=CARTESIAN_POINT('Ctrl Pts',(-7.01124999775337,-0.0001774919695956,
-10.7735343569104));
#24402=CARTESIAN_POINT('Ctrl Pts',(-7.01125473885781,0.187104606374703,
-10.7820370306241));
#24403=CARTESIAN_POINT('Ctrl Pts',(-7.00375121472552,0.374409186281723,
-10.7905397043379));
#24404=CARTESIAN_POINT('Ctrl Pts',(-6.98876009213104,0.561122925156835,
-10.7990423780516));
#24405=CARTESIAN_POINT('Ctrl Pts',(-6.97376854100906,0.747842001322058,
-10.8075452948179));
#24406=CARTESIAN_POINT('Ctrl Pts',(-6.95128898438519,0.933969893314279,
-10.8160482115841));
#24407=CARTESIAN_POINT('Ctrl Pts',(-6.92139408241581,1.11889700973748,-10.8245511283503));
#24408=CARTESIAN_POINT('Ctrl Pts',(-6.89150055657391,1.30381561356252,-10.8330536537088));
#24409=CARTESIAN_POINT('Ctrl Pts',(-6.8541924186819,1.48753324643887,-10.8415561790672));
#24410=CARTESIAN_POINT('Ctrl Pts',(-6.80959376620514,1.66944880177863,-10.8500587044256));
#24411=CARTESIAN_POINT('Ctrl Pts',(-6.76498431048066,1.85140842299707,-10.8585632893729));
#24412=CARTESIAN_POINT('Ctrl Pts',(-6.71308088446669,2.03156479294153,-10.8670678743202));
#24413=CARTESIAN_POINT('Ctrl Pts',(-6.65405819721535,2.20932932596551,-10.8755724592675));
#24414=CARTESIAN_POINT('Ctrl Pts',(-6.61092696152564,2.33923198421757,-10.8817872433597));
#24415=CARTESIAN_POINT('Ctrl Pts',(-6.56399505794186,2.46785764044409,-10.8880020274518));
#24416=CARTESIAN_POINT('Ctrl Pts',(-6.51334730152521,2.59498236838215,-10.894216811544));
#24417=CARTESIAN_POINT('Ctrl Pts',(-6.44381562976938,2.7695052985259,-10.9027487655356));
#24418=CARTESIAN_POINT('Ctrl Pts',(-6.36725376840712,2.94126144775786,-10.9112807195273));
#24419=CARTESIAN_POINT('Ctrl Pts',(-6.2839072441766,3.10968427803931,-10.919812673519));
#24420=CARTESIAN_POINT('Ctrl Pts',(-6.2005763275957,3.27807556909886,-10.9283430297986));
#24421=CARTESIAN_POINT('Ctrl Pts',(-6.11046341929546,3.44313451271079,-10.9368733860782));
#24422=CARTESIAN_POINT('Ctrl Pts',(-6.01386096649161,3.6043172499391,-10.9454037423578));
#24423=CARTESIAN_POINT('Ctrl Pts',(-5.91308936073532,3.77245628553556,-10.9543022503668));
#24424=CARTESIAN_POINT('Ctrl Pts',(-5.80525579364537,3.93637679919713,-10.9632007583758));
#24425=CARTESIAN_POINT('Ctrl Pts',(-5.69074430248391,4.09549213724638,-10.9720992663849));
#24426=CARTESIAN_POINT('Ctrl Pts',(-5.58097371801334,4.24801991833405,-10.9806293659859));
#24427=CARTESIAN_POINT('Ctrl Pts',(-5.46506721216166,4.39613212525469,-10.9891594655869));
#24428=CARTESIAN_POINT('Ctrl Pts',(-5.34340634120211,4.53934304005559,-10.9976895651879));
#24429=CARTESIAN_POINT('Ctrl Pts',(-5.22174416957121,4.68255548591846,-11.0062197559839));
#24430=CARTESIAN_POINT('Ctrl Pts',(-5.09432771051767,4.82086630382314,-11.0147499467799));
#24431=CARTESIAN_POINT('Ctrl Pts',(-4.96157800818184,4.95382379896846,-11.0232801375758));
#24432=CARTESIAN_POINT('Ctrl Pts',(-4.82880191749833,5.08680772376708,-11.0318120240263));
#24433=CARTESIAN_POINT('Ctrl Pts',(-4.6906906830514,5.21443598453826,-11.0403439104769));
#24434=CARTESIAN_POINT('Ctrl Pts',(-4.54770193502134,5.3362940017116,-11.0488757969274));
#24435=CARTESIAN_POINT('Ctrl Pts',(-4.52921056939334,5.35205273225019,-11.049979144107));
#24436=CARTESIAN_POINT('Ctrl Pts',(-4.51063768039098,5.3677150163051,-11.0510824912866));
#24437=CARTESIAN_POINT('Ctrl Pts',(-4.49198429904447,5.38328000568779,-11.0521858384662));
#24438=CARTESIAN_POINT('Ctrl Pts',(-4.34773747733382,5.50364425529522,-11.0607180354414));
#24439=CARTESIAN_POINT('Ctrl Pts',(-4.19862571394932,5.61822778014426,-11.0692502324165));
#24440=CARTESIAN_POINT('Ctrl Pts',(-4.04513469379083,5.72664927087296,-11.0777824293916));
#24441=CARTESIAN_POINT('Ctrl Pts',(-3.89167247929069,5.83505041414148,-11.0863130251294));
#24442=CARTESIAN_POINT('Ctrl Pts',(-3.7338328979712,5.93729165461563,-11.0948436208673));
#24443=CARTESIAN_POINT('Ctrl Pts',(-3.57213209683775,6.03303396685628,-11.1033742166051));
#24444=CARTESIAN_POINT('Ctrl Pts',(-3.40345965995557,6.13290415305923,-11.1122726040037));
#24445=CARTESIAN_POINT('Ctrl Pts',(-3.23058596600869,6.2257023943694,-11.1211709914023));
#24446=CARTESIAN_POINT('Ctrl Pts',(-3.05412800691252,6.31109567982396,-11.1300693788009));
#24447=CARTESIAN_POINT('Ctrl Pts',(-2.88496881527845,6.39295687334823,-11.1385997053836));
#24448=CARTESIAN_POINT('Ctrl Pts',(-2.71251619643036,6.46801322098118,-11.1471300319662));
#24449=CARTESIAN_POINT('Ctrl Pts',(-2.53733697359699,6.53601925065385,-11.1556603585489));
#24450=CARTESIAN_POINT('Ctrl Pts',(-2.36215598521096,6.60402596572873,-11.1641907711049));
#24451=CARTESIAN_POINT('Ctrl Pts',(-2.18424862435887,6.66498211312519,-11.1727211836608));
#24452=CARTESIAN_POINT('Ctrl Pts',(-2.00420024027551,6.71869094090356,-11.1812515962168));
#24453=CARTESIAN_POINT('Ctrl Pts',(-1.82411624572041,6.77241039136374,-11.1897836959416));
#24454=CARTESIAN_POINT('Ctrl Pts',(-1.64189067569975,6.81887957279563,-11.1983157956663));
#24455=CARTESIAN_POINT('Ctrl Pts',(-1.4581233812625,6.85795179098801,-11.2068478953911));
#24456=CARTESIAN_POINT('Ctrl Pts',(-1.4343811627069,6.86299981189193,-11.2079502187236));
#24457=CARTESIAN_POINT('Ctrl Pts',(-1.41061322557452,6.86792443286042,-11.2090525420561));
#24458=CARTESIAN_POINT('Ctrl Pts',(-1.38682087669682,6.87272539961098,-11.2101548653885));
#24459=CARTESIAN_POINT('Ctrl Pts',(-1.20261507129361,6.90989558198963,-11.2186893046874));
#24460=CARTESIAN_POINT('Ctrl Pts',(-1.01688339423534,6.93966194091266,-11.2272237439862));
#24461=CARTESIAN_POINT('Ctrl Pts',(-0.830234829243166,6.96192047432399,
-11.235758183285));
#24462=CARTESIAN_POINT('Ctrl Pts',(-0.643620942919284,6.98417487217555,
-11.244291036914));
#24463=CARTESIAN_POINT('Ctrl Pts',(-0.456090812032652,6.99892419212788,
-11.252823890543));
#24464=CARTESIAN_POINT('Ctrl Pts',(-0.268260064727012,7.00611612094552,
-11.2613567441721));
#24465=CARTESIAN_POINT('Ctrl Pts',(-0.0724077147546187,7.01361519221033,
-11.270254006517));
#24466=CARTESIAN_POINT('Ctrl Pts',(0.123771141487748,7.01289715947273,-11.2791512688619));
#24467=CARTESIAN_POINT('Ctrl Pts',(0.319575848457633,7.00396300958126,-11.2880485312068));
#24468=CARTESIAN_POINT('Ctrl Pts',(0.507355008166848,6.99539504824214,-11.296581116928));
#24469=CARTESIAN_POINT('Ctrl Pts',(0.69478975221258,6.97927107636034,-11.3051137026492));
#24470=CARTESIAN_POINT('Ctrl Pts',(0.881264443551761,6.95564515649206,-11.3136462883704));
#24471=CARTESIAN_POINT('Ctrl Pts',(1.06774081813107,6.93201902336107,-11.3221789511122));
#24472=CARTESIAN_POINT('Ctrl Pts',(1.25325681983915,6.90089084851375,-11.330711613854));
#24473=CARTESIAN_POINT('Ctrl Pts',(1.43720371639759,6.86236635863118,-11.3392442765958));
#24474=CARTESIAN_POINT('Ctrl Pts',(1.62118643860935,6.82383436568634,-11.3477786011662));
#24475=CARTESIAN_POINT('Ctrl Pts',(1.80359914631097,6.77790324421311,-11.3563129257366));
#24476=CARTESIAN_POINT('Ctrl Pts',(1.98384418620484,6.72472964567062,-11.3648472503071));
#24477=CARTESIAN_POINT('Ctrl Pts',(2.00691175934491,6.71792454371485,-11.3659394643083));
#24478=CARTESIAN_POINT('Ctrl Pts',(2.02994384797711,6.71100088741002,-11.3670316783096));
#24479=CARTESIAN_POINT('Ctrl Pts',(2.05293921673861,6.70395906423038,-11.3681238923108));
#24480=CARTESIAN_POINT('Ctrl Pts',(2.23244130289167,6.64899051973013,-11.37664972609));
#24481=CARTESIAN_POINT('Ctrl Pts',(2.40976571285594,6.58679883635617,-11.3851755598692));
#24482=CARTESIAN_POINT('Ctrl Pts',(2.58432844263528,6.51758184168686,-11.3937013936483));
#24483=CARTESIAN_POINT('Ctrl Pts',(2.75885790085022,6.44837803974031,-11.4022256024081));
#24484=CARTESIAN_POINT('Ctrl Pts',(2.9306264441014,6.37215171169286,-11.4107498111678));
#24485=CARTESIAN_POINT('Ctrl Pts',(3.09906881065696,6.28914931205432,-11.4192740199276));
#24486=CARTESIAN_POINT('Ctrl Pts',(3.27496811012105,6.2024724014361,-11.4281755948697));
#24487=CARTESIAN_POINT('Ctrl Pts',(3.44723970573288,6.10840595515281,-11.4370771698118));
#24488=CARTESIAN_POINT('Ctrl Pts',(3.61526631523908,6.00728524646514,-11.445978744754));
#24489=CARTESIAN_POINT('Ctrl Pts',(3.77616550589435,5.91045391579584,-11.4545027291869));
#24490=CARTESIAN_POINT('Ctrl Pts',(3.93317212461599,5.80715459675497,-11.4630267136198));
#24491=CARTESIAN_POINT('Ctrl Pts',(4.08577157516053,5.69772737133941,-11.4715506980527));
#24492=CARTESIAN_POINT('Ctrl Pts',(4.23837330556009,5.58829851106731,-11.480074809835));
#24493=CARTESIAN_POINT('Ctrl Pts',(4.38656748876948,5.47274174310529,-11.4885989216173));
#24494=CARTESIAN_POINT('Ctrl Pts',(4.52987021406729,5.3514392836139,-11.4971230333996));
#24495=CARTESIAN_POINT('Ctrl Pts',(4.67320287130983,5.23011148742004,-11.5056489256313));
#24496=CARTESIAN_POINT('Ctrl Pts',(4.81164179646588,5.10303580186513,-11.514174817863));
#24497=CARTESIAN_POINT('Ctrl Pts',(4.94473708522744,4.97063393547306,-11.5227007100946));
#24498=CARTESIAN_POINT('Ctrl Pts',(4.96238869057907,4.95307429444356,-11.5238314464741));
#24499=CARTESIAN_POINT('Ctrl Pts',(4.97994635858858,4.93542102467172,-11.5249621828536));
#24500=CARTESIAN_POINT('Ctrl Pts',(4.99740908835378,4.9176751586638,-11.5260929192331));
#24501=CARTESIAN_POINT('Ctrl Pts',(5.12940952880526,4.78353449676653,-11.534640133909));
#24502=CARTESIAN_POINT('Ctrl Pts',(5.25602657606199,4.64405509543233,-11.5431873485848));
#24503=CARTESIAN_POINT('Ctrl Pts',(5.37683936972328,4.49969165106831,-11.5517345632607));
#24504=CARTESIAN_POINT('Ctrl Pts',(5.49763025943708,4.35535438049936,-11.5602802282849));
#24505=CARTESIAN_POINT('Ctrl Pts',(5.61261880087413,4.20613506705435,-11.5688258933091));
#24506=CARTESIAN_POINT('Ctrl Pts',(5.72142380932097,4.05252219693306,-11.5773715583333));
#24507=CARTESIAN_POINT('Ctrl Pts',(5.83462397684529,3.89270416208481,-11.5862624239852));
#24508=CARTESIAN_POINT('Ctrl Pts',(5.94113043624094,3.72813050389469,-11.595153289637));
#24509=CARTESIAN_POINT('Ctrl Pts',(6.04056253881339,3.55938629221167,-11.6040441552888));
#24510=CARTESIAN_POINT('Ctrl Pts',(6.13612965882716,3.39720126431498,-11.6125894279201));
#24511=CARTESIAN_POINT('Ctrl Pts',(6.22516184564189,3.23116406529217,-11.6211347005513));
#24512=CARTESIAN_POINT('Ctrl Pts',(6.30736689750766,3.06182125257576,-11.6296799731825));
#24513=CARTESIAN_POINT('Ctrl Pts',(6.38957175909986,2.89247883182385,-11.6382252260346));
#24514=CARTESIAN_POINT('Ctrl Pts',(6.46494938717006,2.71983108719843,-11.6467704788867));
#24515=CARTESIAN_POINT('Ctrl Pts',(6.53325460348441,2.54444706145555,-11.6553157317389));
#24516=CARTESIAN_POINT('Ctrl Pts',(6.60157144856407,2.36903317709009,-11.6638624393956));
#24517=CARTESIAN_POINT('Ctrl Pts',(6.66281336753809,2.19088236457828,-11.6724091470523));
#24518=CARTESIAN_POINT('Ctrl Pts',(6.71678386931552,2.01058225780566,-11.680955854709));
#24519=CARTESIAN_POINT('Ctrl Pts',(6.72332195472672,1.98874037272202,-11.6819912185245));
#24520=CARTESIAN_POINT('Ctrl Pts',(6.72975338948023,1.96686696498067,-11.6830265823399));
#24521=CARTESIAN_POINT('Ctrl Pts',(6.73607787396623,1.94496309434462,-11.6840619461554));
#24522=CARTESIAN_POINT('Ctrl Pts',(6.78803206725332,1.76502780771706,-11.6925672230537));
#24523=CARTESIAN_POINT('Ctrl Pts',(6.832782121241,1.58297591034739,-11.701072499952));
#24524=CARTESIAN_POINT('Ctrl Pts',(6.87017476756959,1.39940173844046,-11.7095777768503));
#24525=CARTESIAN_POINT('Ctrl Pts',(6.90756022416318,1.21586286357125,-11.7180814183819));
#24526=CARTESIAN_POINT('Ctrl Pts',(6.93759103410159,1.03080260171472,-11.7265850599135));
#24527=CARTESIAN_POINT('Ctrl Pts',(6.96016488598172,0.844826208428179,-11.7350887014451));
#24528=CARTESIAN_POINT('Ctrl Pts',(6.9838223879921,0.649922081236072,-11.7440005574145));
#24529=CARTESIAN_POINT('Ctrl Pts',(6.99928929715512,0.454012056972497,-11.7529124133839));
#24530=CARTESIAN_POINT('Ctrl Pts',(7.00650878861348,0.257800615945896,-11.7618242693533));
#24531=CARTESIAN_POINT('Ctrl Pts',(7.01339764590694,0.0705751549320466,
-11.7703279852101));
#24532=CARTESIAN_POINT('Ctrl Pts',(7.01277762320226,-0.116924398607505,
-11.778831701067));
#24533=CARTESIAN_POINT('Ctrl Pts',(7.00465270090815,-0.304084037989905,
-11.7873354169239));
#24534=CARTESIAN_POINT('Ctrl Pts',(6.99652748248866,-0.491250498695174,
-11.7958394427118));
#24535=CARTESIAN_POINT('Ctrl Pts',(6.9808968355076,-0.678076711090961,-11.8043434684998));
#24536=CARTESIAN_POINT('Ctrl Pts',(6.95781679305076,-0.863951408842418,
-11.8128474942878));
#24537=CARTESIAN_POINT('Ctrl Pts',(6.93473092359782,-1.04987303419992,-11.8213536670789));
#24538=CARTESIAN_POINT('Ctrl Pts',(6.90419194189063,-1.23484235776442,-11.8298598398701));
#24539=CARTESIAN_POINT('Ctrl Pts',(6.86630752895882,-1.41825508293234,-11.8383660126613));
#24540=CARTESIAN_POINT('Ctrl Pts',(6.86086658322036,-1.44459675245163,-11.8395876661334));
#24541=CARTESIAN_POINT('Ctrl Pts',(6.85527421229141,-1.47090633170256,-11.8408093196056));
#24542=CARTESIAN_POINT('Ctrl Pts',(6.84953082152621,-1.49718204887129,-11.8420309730777));
#24543=CARTESIAN_POINT('Ctrl Pts',(6.80917135818051,-1.68182451658929,-11.850615671655));
#24544=CARTESIAN_POINT('Ctrl Pts',(6.76133572224075,-1.86486078725442,-11.8592003702323));
#24545=CARTESIAN_POINT('Ctrl Pts',(6.70617623540106,-2.04568493718903,-11.8677850688095));
#24546=CARTESIAN_POINT('Ctrl Pts',(6.65102750995593,-2.22647380905754,-11.8763680925466));
#24547=CARTESIAN_POINT('Ctrl Pts',(6.58855787255442,-2.40505113644434,-11.8849511162836));
#24548=CARTESIAN_POINT('Ctrl Pts',(6.51896962033777,-2.58082576932524,-11.8935341400206));
#24549=CARTESIAN_POINT('Ctrl Pts',(6.44703718968831,-2.7625216186516,-11.9024062950189));
#24550=CARTESIAN_POINT('Ctrl Pts',(6.36749828660038,-2.94122233992901,-11.9112784500172));
#24551=CARTESIAN_POINT('Ctrl Pts',(6.28063099339152,-3.1162960204945,-11.9201506050155));
#24552=CARTESIAN_POINT('Ctrl Pts',(6.19660794304912,-3.28563737018311,-11.9287322644471));
#24553=CARTESIAN_POINT('Ctrl Pts',(6.10572894942552,-3.45158515555319,-11.9373139238787));
#24554=CARTESIAN_POINT('Ctrl Pts',(6.00829329235825,-3.6135907731096,-11.9458955833104));
#24555=CARTESIAN_POINT('Ctrl Pts',(5.90591023089262,-3.78382240698266,-11.954912986092));
#24556=CARTESIAN_POINT('Ctrl Pts',(5.79628751298796,-3.94970081146458,-11.9639303888736));
#24557=CARTESIAN_POINT('Ctrl Pts',(5.67982548128847,-4.11062149371676,-11.9729477916552));
#24558=CARTESIAN_POINT('Ctrl Pts',(5.56336344958899,-4.27154217596894,-11.9819651944368));
#24559=CARTESIAN_POINT('Ctrl Pts',(5.44006233029551,-4.42750482809971,-11.9909825972184));
#24560=CARTESIAN_POINT('Ctrl Pts',(5.31037376991253,-4.57794244025905,-12.));
#24561=CARTESIAN_POINT('',(-5.30612006659788,-4.5828720690575,-12.));
#24562=CARTESIAN_POINT('Origin',(0.,0.,-12.));
#24563=CARTESIAN_POINT('Ctrl Pts',(-5.30612006659788,-4.5828720690575,-12.));
#24564=CARTESIAN_POINT('Ctrl Pts',(-5.03347260351227,-4.89854751301181,
-11.9809094032564));
#24565=CARTESIAN_POINT('Ctrl Pts',(-4.73319340804265,-5.18926879016435,
-11.961640649704));
#24566=CARTESIAN_POINT('Ctrl Pts',(-4.26928721805366,-5.56444336543857,
-11.934434282125));
#24567=CARTESIAN_POINT('Ctrl Pts',(-4.12544111385343,-5.67191152130197,
-11.9262961500531));
#24568=CARTESIAN_POINT('Ctrl Pts',(-3.6470612840599,-6.00147544434351,-11.9000812266326));
#24569=CARTESIAN_POINT('Ctrl Pts',(-3.29755039688922,-6.20039684214918,
-11.8822436608555));
#24570=CARTESIAN_POINT('Ctrl Pts',(-2.84327523265843,-6.4096145726469,-11.8596945470418));
#24571=CARTESIAN_POINT('Ctrl Pts',(-2.75274343167674,-6.44901360156294,
-11.8552267223847));
#24572=CARTESIAN_POINT('Ctrl Pts',(-2.51138791433897,-6.54804188864338,
-11.8433498403589));
#24573=CARTESIAN_POINT('Ctrl Pts',(-2.35927765702271,-6.60437201916886,
-11.8359092031642));
#24574=CARTESIAN_POINT('Ctrl Pts',(-1.98152840657345,-6.72954456640903,
-11.8176136683002));
#24575=CARTESIAN_POINT('Ctrl Pts',(-1.75410314623136,-6.79237427609974,
-11.8067576240749));
#24576=CARTESIAN_POINT('Ctrl Pts',(-1.36036524116173,-6.88005218881468,
-11.7882865299175));
#24577=CARTESIAN_POINT('Ctrl Pts',(-1.19553075121103,-6.91060193019187,
-11.7806467369069));
#24578=CARTESIAN_POINT('Ctrl Pts',(-0.615042517245142,-6.99679430867117,
-11.7540249259773));
#24579=CARTESIAN_POINT('Ctrl Pts',(-0.195638850546006,-7.02104953336165,
-11.7353431450287));
#24580=CARTESIAN_POINT('Ctrl Pts',(0.297165582144061,-7.00533824086339,
-11.7132142035408));
#24581=CARTESIAN_POINT('Ctrl Pts',(0.370874232377533,-7.00182286714805,
-11.7098979420791));
#24582=CARTESIAN_POINT('Ctrl Pts',(0.553165261822067,-6.9902423168726,-11.7016656930351));
#24583=CARTESIAN_POINT('Ctrl Pts',(0.661639547676978,-6.9808102898942,-11.6967383421722));
#24584=CARTESIAN_POINT('Ctrl Pts',(0.948828547277942,-6.94908445857838,
-11.6835757905944));
#24585=CARTESIAN_POINT('Ctrl Pts',(1.12697637330927,-6.92242540608268,-11.6753043121028));
#24586=CARTESIAN_POINT('Ctrl Pts',(1.52354478053644,-6.84736524831524,-11.6567404154643));
#24587=CARTESIAN_POINT('Ctrl Pts',(1.74107898270743,-6.79531050024874,-11.6464547558566));
#24588=CARTESIAN_POINT('Ctrl Pts',(2.13731763355941,-6.68021304921843,-11.6275709920011));
#24589=CARTESIAN_POINT('Ctrl Pts',(2.31667464301831,-6.62015054629303,-11.6189639974111));
#24590=CARTESIAN_POINT('Ctrl Pts',(2.77281340618289,-6.44658950593237,-11.5968674463903));
#24591=CARTESIAN_POINT('Ctrl Pts',(3.0451553181144,-6.32250287310991,-11.583479759843));
#24592=CARTESIAN_POINT('Ctrl Pts',(3.50228552551207,-6.07781315501453,-11.5602494497656));
#24593=CARTESIAN_POINT('Ctrl Pts',(3.69085097825893,-5.96518509499422,-11.550418783469));
#24594=CARTESIAN_POINT('Ctrl Pts',(3.96923164540474,-5.7806513947774,-11.5352842242218));
#24595=CARTESIAN_POINT('Ctrl Pts',(4.06307942085906,-5.71507787643148,-11.5300621540794));
#24596=CARTESIAN_POINT('Ctrl Pts',(4.37525483738569,-5.48537694098302,-11.5123111649174));
#24597=CARTESIAN_POINT('Ctrl Pts',(4.58558599868548,-5.31080185230311,-11.4997152980757));
#24598=CARTESIAN_POINT('Ctrl Pts',(4.94119644040959,-4.97873084231838,-11.4773866669656));
#24599=CARTESIAN_POINT('Ctrl Pts',(5.09046426918637,-4.82600857499741,-11.4676387417521));
#24600=CARTESIAN_POINT('Ctrl Pts',(5.37585245043567,-4.5060182196124,-11.4481798621427));
#24601=CARTESIAN_POINT('Ctrl Pts',(5.51169357637629,-4.33880463449659,-11.4384803286146));
#24602=CARTESIAN_POINT('Ctrl Pts',(5.80865010291946,-3.93676839718646,-11.4160439734009));
#24603=CARTESIAN_POINT('Ctrl Pts',(5.96358892251378,-3.69785969844857,-11.4033576605807));
#24604=CARTESIAN_POINT('Ctrl Pts',(6.15712521063663,-3.35548416189856,-11.3856306398269));
#24605=CARTESIAN_POINT('Ctrl Pts',(6.20845391045076,-3.25953441426689,-11.3807057284765));
#24606=CARTESIAN_POINT('Ctrl Pts',(6.34113915322826,-2.99698876308996,-11.3673035355086));
#24607=CARTESIAN_POINT('Ctrl Pts',(6.41815438112904,-2.82829993380119,-11.3587863707568));
#24608=CARTESIAN_POINT('Ctrl Pts',(6.57190190074028,-2.45281454952298,-11.3401230891118));
#24609=CARTESIAN_POINT('Ctrl Pts',(6.64574844918732,-2.24504401544025,-11.3299850128475));
#24610=CARTESIAN_POINT('Ctrl Pts',(6.76428428973349,-1.85404916061724,-11.3112895403224));
#24611=CARTESIAN_POINT('Ctrl Pts',(6.81160939606699,-1.67183111176069,-11.3027242322513));
#24612=CARTESIAN_POINT('Ctrl Pts',(6.90028627141531,-1.26349571513071,-11.2838083175218));
#24613=CARTESIAN_POINT('Ctrl Pts',(6.93796908099293,-1.03680230611507,-11.2734934561395));
#24614=CARTESIAN_POINT('Ctrl Pts',(6.98695277138019,-0.614941517490937,
-11.2544572438967));
#24615=CARTESIAN_POINT('Ctrl Pts',(7.00135391097328,-0.420362762101538,
-11.2457372445639));
#24616=CARTESIAN_POINT('Ctrl Pts',(7.01158185917485,-0.102432630642884,
-11.2314306546495));
#24617=CARTESIAN_POINT('Ctrl Pts',(7.01229959221733,0.0206550579174754,
-11.2258765123003));
#24618=CARTESIAN_POINT('Ctrl Pts',(7.0071533386387,0.271698113049057,-11.2144586100377));
#24619=CARTESIAN_POINT('Ctrl Pts',(7.00102386176057,0.399602346535745,-11.2085975989526));
#24620=CARTESIAN_POINT('Ctrl Pts',(6.97170942873689,0.788303666061847,-11.1907023277934));
#24621=CARTESIAN_POINT('Ctrl Pts',(6.93741857339419,1.04803609012085,-11.1786367683149));
#24622=CARTESIAN_POINT('Ctrl Pts',(6.85166451550499,1.50062109112961,-11.1575252467956));
#24623=CARTESIAN_POINT('Ctrl Pts',(6.80634892865225,1.69433951177183,-11.1484578660865));
#24624=CARTESIAN_POINT('Ctrl Pts',(6.69065690626181,2.10860529922559,-11.1289594846385));
#24625=CARTESIAN_POINT('Ctrl Pts',(6.61747176167516,2.32812710568623,-11.1185603431471));
#24626=CARTESIAN_POINT('Ctrl Pts',(6.45743457771486,2.73919845193073,-11.0987783253905));
#24627=CARTESIAN_POINT('Ctrl Pts',(6.37255542273968,2.9312465304788,-11.0893993783134));
#24628=CARTESIAN_POINT('Ctrl Pts',(6.22263804584527,3.23304210756713,-11.0742494700491));
#24629=CARTESIAN_POINT('Ctrl Pts',(6.16300002990119,3.34532743459506,-11.0685157621435));
#24630=CARTESIAN_POINT('Ctrl Pts',(6.0227182027061,3.59295041541811,-11.0555788379607));
#24631=CARTESIAN_POINT('Ctrl Pts',(5.94049956697817,3.72731687383393,-11.0483604982724));
#24632=CARTESIAN_POINT('Ctrl Pts',(5.71821977316415,4.0645170075794,-11.0298017335497));
#24633=CARTESIAN_POINT('Ctrl Pts',(5.57186124643667,4.26294491431963,-11.0184522234398));
#24634=CARTESIAN_POINT('Ctrl Pts',(5.2915524413866,4.60381313895361,-10.9982358323555));
#24635=CARTESIAN_POINT('Ctrl Pts',(5.16151752863195,4.74914320674079,-10.9893526475353));
#24636=CARTESIAN_POINT('Ctrl Pts',(4.8851564413371,5.0332333106444,-10.971393227088));
#24637=CARTESIAN_POINT('Ctrl Pts',(4.73856164040789,5.17148200532207,-10.9623288878831));
#24638=CARTESIAN_POINT('Ctrl Pts',(4.41542054660129,5.45093351673867,-10.9431587770593));
#24639=CARTESIAN_POINT('Ctrl Pts',(4.23758849946023,5.59030034277817,-10.9330718027781));
#24640=CARTESIAN_POINT('Ctrl Pts',(3.94625283975758,5.79671807991351,-10.9170256210937));
#24641=CARTESIAN_POINT('Ctrl Pts',(3.83705426030064,5.86957119018013,-10.9111087588167));
#24642=CARTESIAN_POINT('Ctrl Pts',(3.60534262314025,6.01492950884022,-10.8986788063955));
#24643=CARTESIAN_POINT('Ctrl Pts',(3.48253608698529,6.08685583711557,-10.8921630678228));
#24644=CARTESIAN_POINT('Ctrl Pts',(3.08960177350754,6.30120648873547,-10.8716076955209));
#24645=CARTESIAN_POINT('Ctrl Pts',(2.81230846483226,6.42975632135445,-10.8575366136582));
#24646=CARTESIAN_POINT('Ctrl Pts',(2.44718246039113,6.57087077794948,-10.8396404812248));
#24647=CARTESIAN_POINT('Ctrl Pts',(2.36627894206668,6.60043702284669,-10.8357120186529));
#24648=CARTESIAN_POINT('Ctrl Pts',(2.1062307121032,6.69007584689251,-10.8231972306517));
#24649=CARTESIAN_POINT('Ctrl Pts',(1.92519316392614,6.74440178678913,-10.8146552479193));
#24650=CARTESIAN_POINT('Ctrl Pts',(1.35311364546076,6.89115700034329,-10.7880694490012));
#24651=CARTESIAN_POINT('Ctrl Pts',(0.956195485671111,6.95734453454538,-10.7702412035067));
#24652=CARTESIAN_POINT('Ctrl Pts',(0.44937464068031,6.99764875429134,-10.7472274565676));
#24653=CARTESIAN_POINT('Ctrl Pts',(0.342766797865227,7.00368016451697,-10.7423651910949));
#24654=CARTESIAN_POINT('Ctrl Pts',(-0.039320008195268,7.01655207627336,
-10.724877655996));
#24655=CARTESIAN_POINT('Ctrl Pts',(-0.315011029876103,7.00958749346482,
-10.71216852385));
#24656=CARTESIAN_POINT('Ctrl Pts',(-0.810675321235539,6.96775900726511,
-10.6893281019996));
#24657=CARTESIAN_POINT('Ctrl Pts',(-1.03076777960181,6.93861515305332,-10.6791871536366));
#24658=CARTESIAN_POINT('Ctrl Pts',(-1.45398296333813,6.86199017205336,-10.6596591086824));
#24659=CARTESIAN_POINT('Ctrl Pts',(-1.65710424665962,6.81578923852454,-10.6502732128743));
#24660=CARTESIAN_POINT('Ctrl Pts',(-2.14130607810876,6.68272681845155,-10.6277204005744));
#24661=CARTESIAN_POINT('Ctrl Pts',(-2.41956113953147,6.58708973449629,-10.6146166352803));
#24662=CARTESIAN_POINT('Ctrl Pts',(-2.79304087099005,6.43185533820519,-10.5963930743974));
#24663=CARTESIAN_POINT('Ctrl Pts',(-2.89407372683863,6.387031971596,-10.5913932342474));
#24664=CARTESIAN_POINT('Ctrl Pts',(-3.15784811867006,6.26246381801166,-10.5781075853874));
#24665=CARTESIAN_POINT('Ctrl Pts',(-3.31862810849199,6.17876719680774,-10.5697849256581));
#24666=CARTESIAN_POINT('Ctrl Pts',(-3.67060749139187,5.9778332146982,-10.5511439421458));
#24667=CARTESIAN_POINT('Ctrl Pts',(-3.85979395696704,5.85746030153534,-10.5408323331279));
#24668=CARTESIAN_POINT('Ctrl Pts',(-4.19743532854404,5.61915870521632,-10.521918377674));
#24669=CARTESIAN_POINT('Ctrl Pts',(-4.34750389885634,5.50387312271211,-10.5133069374932));
#24670=CARTESIAN_POINT('Ctrl Pts',(-4.7257601169692,5.18815511995088,-10.4909989556166));
#24671=CARTESIAN_POINT('Ctrl Pts',(-4.94591634291057,4.97872241369126,-10.4774095892723));
#24672=CARTESIAN_POINT('Ctrl Pts',(-5.29023740070518,4.60572096020231,-10.4546664246096));
#24673=CARTESIAN_POINT('Ctrl Pts',(-5.42205176708675,4.44978988892693,-10.4455247372652));
#24674=CARTESIAN_POINT('Ctrl Pts',(-5.61189601397819,4.20423011722575,-10.4314767152607));
#24675=CARTESIAN_POINT('Ctrl Pts',(-5.67499471690442,4.11866021873803,-10.4266362406227));
#24676=CARTESIAN_POINT('Ctrl Pts',(-5.89460916821788,3.80620180057507,-10.4091685497005));
#24677=CARTESIAN_POINT('Ctrl Pts',(-6.03966144402538,3.57156529511606,-10.3964560552845));
#24678=CARTESIAN_POINT('Ctrl Pts',(-6.27631161660821,3.13291851302716,-10.3735691741923));
#24679=CARTESIAN_POINT('Ctrl Pts',(-6.3726930321161,2.93190242993521,-10.3633857936126));
#24680=CARTESIAN_POINT('Ctrl Pts',(-6.54008166079987,2.53536257424353,-10.3438421304199));
#24681=CARTESIAN_POINT('Ctrl Pts',(-6.61228777266003,2.34059474568933,-10.3344820717728));
#24682=CARTESIAN_POINT('Ctrl Pts',(-6.7658330343885,1.86225927027523,-10.3119181647198));
#24683=CARTESIAN_POINT('Ctrl Pts',(-6.83813304456533,1.57621081751037,-10.2987786156168));
#24684=CARTESIAN_POINT('Ctrl Pts',(-6.912525049042,1.17765687240146,-10.28051146429));
#24685=CARTESIAN_POINT('Ctrl Pts',(-6.93025477348721,1.06838512787543,-10.2755041151218));
#24686=CARTESIAN_POINT('Ctrl Pts',(-6.97212850224025,0.765039264511157,
-10.2615578922025));
#24687=CARTESIAN_POINT('Ctrl Pts',(-6.99075163635057,0.570307879520168,
-10.2525712455192));
#24688=CARTESIAN_POINT('Ctrl Pts',(-7.01283237363221,0.158123628128352,
-10.2335834381316));
#24689=CARTESIAN_POINT('Ctrl Pts',(-7.01436481487391,-0.0592325604935013,
-10.2235916143769));
#24690=CARTESIAN_POINT('Ctrl Pts',(-6.99841766858817,-0.463571089965065,
-10.2050784079148));
#24691=CARTESIAN_POINT('Ctrl Pts',(-6.98352685073223,-0.650463154832566,
-10.1965501317857));
#24692=CARTESIAN_POINT('Ctrl Pts',(-6.92956514944857,-1.0995011646996,-10.176079382904));
#24693=CARTESIAN_POINT('Ctrl Pts',(-6.88308868415413,-1.36046633352886,
-10.1642035884737));
#24694=CARTESIAN_POINT('Ctrl Pts',(-6.78251461914111,-1.78446933768445,
-10.1446799121039));
#24695=CARTESIAN_POINT('Ctrl Pts',(-6.73700313116651,-1.94926231142541,
-10.1370307867779));
#24696=CARTESIAN_POINT('Ctrl Pts',(-6.65051118328972,-2.22302242034616,
-10.1241073063752));
#24697=CARTESIAN_POINT('Ctrl Pts',(-6.612758016824,-2.33292923210549,-10.1188574485144));
#24698=CARTESIAN_POINT('Ctrl Pts',(-6.5722843992401,-2.44186493044116,-10.11356916409));
#24699=CARTESIAN_POINT('Ctrl Pts',(-6.57227799727717,-2.44188216123224,
-10.1135683276261));
#24700=CARTESIAN_POINT('Ctrl Pts',(-6.57227159525839,-2.44189939200199,
-10.1135674911542));
#24701=CARTESIAN_POINT('Origin',(0.,0.,0.));
#24702=CARTESIAN_POINT('',(-7.01125010206304,-6.30148839881794E-5,-8.22678883376454));
#24703=CARTESIAN_POINT('Ctrl Pts',(-6.57227159525839,-2.44189939200199,
-10.1135674911542));
#24704=CARTESIAN_POINT('Ctrl Pts',(-6.55563335767533,-2.48668052287923,
-10.111393580184));
#24705=CARTESIAN_POINT('Ctrl Pts',(-6.53853794377912,-2.53129023612478,
-10.1092142556917));
#24706=CARTESIAN_POINT('Ctrl Pts',(-6.41893712906644,-2.83408518985237,
-10.0943340971301));
#24707=CARTESIAN_POINT('Ctrl Pts',(-6.3016220842915,-3.08615476115843,-10.0815210439367));
#24708=CARTESIAN_POINT('Ctrl Pts',(-6.06202586012092,-3.52998740057746,
-10.0583555983445));
#24709=CARTESIAN_POINT('Ctrl Pts',(-5.94478479856127,-3.72404414589833,
-10.0479961152748));
#24710=CARTESIAN_POINT('Ctrl Pts',(-5.70373976967903,-4.08254476599991,
-10.0283774784473));
#24711=CARTESIAN_POINT('Ctrl Pts',(-5.58169100795926,-4.24788728897974,
-10.0191146389423));
#24712=CARTESIAN_POINT('Ctrl Pts',(-5.27144447599857,-4.63168439768932,
-9.99694473763417));
#24713=CARTESIAN_POINT('Ctrl Pts',(-5.07669470879712,-4.84435717107434,
-9.98409851500608));
#24714=CARTESIAN_POINT('Ctrl Pts',(-4.78639664337701,-5.12458273860975,
-9.96593391436084));
#24715=CARTESIAN_POINT('Ctrl Pts',(-4.7014129183229,-5.20265868213545,-9.96071963443434));
#24716=CARTESIAN_POINT('Ctrl Pts',(-4.4549021696597,-5.41815774778652,-9.94581838120971));
#24717=CARTESIAN_POINT('Ctrl Pts',(-4.2890166544668,-5.5503982846688,-9.93606963252502));
#24718=CARTESIAN_POINT('Ctrl Pts',(-3.86676039241555,-5.8567633677391,-9.91207036463691));
#24719=CARTESIAN_POINT('Ctrl Pts',(-3.60434923938149,-6.02180911091854,
-9.89785023588188));
#24720=CARTESIAN_POINT('Ctrl Pts',(-3.1651642018583,-6.25901484236853,-9.87514223515454));
#24721=CARTESIAN_POINT('Ctrl Pts',(-2.99485896822553,-6.34226714362656,
-9.86657638642382));
#24722=CARTESIAN_POINT('Ctrl Pts',(-2.61507429412999,-6.50920912463532,
-9.84790366541906));
#24723=CARTESIAN_POINT('Ctrl Pts',(-2.40450649183683,-6.58989879715603,
-9.83782428806167));
#24724=CARTESIAN_POINT('Ctrl Pts',(-2.01692711283363,-6.71736453849948,
-9.81953794502612));
#24725=CARTESIAN_POINT('Ctrl Pts',(-1.84127461696467,-6.76762052275582,
-9.81134411052068));
#24726=CARTESIAN_POINT('Ctrl Pts',(-1.55412979117488,-6.83776770478043,
-9.7979524202195));
#24727=CARTESIAN_POINT('Ctrl Pts',(-1.44376664335993,-6.86191836181938,
-9.79280089508966));
#24728=CARTESIAN_POINT('Ctrl Pts',(-1.25334026162923,-6.89879169823925,
-9.78391936223826));
#24729=CARTESIAN_POINT('Ctrl Pts',(-1.17354982764886,-6.91281197550355,
-9.7802005893264));
#24730=CARTESIAN_POINT('Ctrl Pts',(-0.705750967202534,-6.98667787123912,
-9.75843382213963));
#24731=CARTESIAN_POINT('Ctrl Pts',(-0.313500584881129,-7.01523200327381,
-9.74037191885143));
#24732=CARTESIAN_POINT('Ctrl Pts',(0.280420151652584,-7.00853306035149,
-9.71338916156268));
#24733=CARTESIAN_POINT('Ctrl Pts',(0.481574664993027,-6.99758949172561,
-9.70430441878386));
#24734=CARTESIAN_POINT('Ctrl Pts',(0.95260313791147,-6.9515544839368,-9.68303561153323));
#24735=CARTESIAN_POINT('Ctrl Pts',(1.22145652174268,-6.90938533445735,-9.67090314030905));
#24736=CARTESIAN_POINT('Ctrl Pts',(1.61327646506455,-6.82433990681331,-9.65288084223265));
#24737=CARTESIAN_POINT('Ctrl Pts',(1.73859288307059,-6.79349470790795,-9.64706217086139));
#24738=CARTESIAN_POINT('Ctrl Pts',(2.01545571210786,-6.71718527644208,-9.63400956044661));
#24739=CARTESIAN_POINT('Ctrl Pts',(2.16645881854833,-6.67001460852423,-9.62676075780371));
#24740=CARTESIAN_POINT('Ctrl Pts',(2.69208767817669,-6.48608318937639,-9.60117141413292));
#24741=CARTESIAN_POINT('Ctrl Pts',(3.05652837817457,-6.32251978427163,-9.58282128894232));
#24742=CARTESIAN_POINT('Ctrl Pts',(3.5805204509342,-6.03139919028621,-9.55558821791589));
#24743=CARTESIAN_POINT('Ctrl Pts',(3.75168865020004,-5.92644386509312,-9.54653277069493));
#24744=CARTESIAN_POINT('Ctrl Pts',(4.14136661308595,-5.66384856685306,-9.52541413758718));
#24745=CARTESIAN_POINT('Ctrl Pts',(4.35576251628872,-5.50067543964145,-9.51340103279229));
#24746=CARTESIAN_POINT('Ctrl Pts',(4.66028882435961,-5.23991246658184,-9.49538413119836));
#24747=CARTESIAN_POINT('Ctrl Pts',(4.75789932949773,-5.15144328518606,-9.48944655333741));
#24748=CARTESIAN_POINT('Ctrl Pts',(4.96341591729386,-4.9543467014069,-9.47650705728897));
#24749=CARTESIAN_POINT('Ctrl Pts',(5.0703737113548,-4.84482798698939,-9.46949514487592));
#24750=CARTESIAN_POINT('Ctrl Pts',(5.45231069957782,-4.42723400922561,-9.4434963473546));
#24751=CARTESIAN_POINT('Ctrl Pts',(5.70351170441368,-4.09854357678903,-9.42449176193967));
#24752=CARTESIAN_POINT('Ctrl Pts',(6.03445099074402,-3.57567158865056,-9.39639098283425));
#24753=CARTESIAN_POINT('Ctrl Pts',(6.1368564923759,-3.39691334474483,-9.38710600788273));
#24754=CARTESIAN_POINT('Ctrl Pts',(6.37386387744646,-2.93739410744932,-9.36388012990598));
#24755=CARTESIAN_POINT('Ctrl Pts',(6.49791627700228,-2.65169869899579,-9.35001900094283));
#24756=CARTESIAN_POINT('Ctrl Pts',(6.63853016122665,-2.25808803434898,-9.33116932537813));
#24757=CARTESIAN_POINT('Ctrl Pts',(6.67217196427409,-2.15665603610392,-9.32632901535657));
#24758=CARTESIAN_POINT('Ctrl Pts',(6.76615056285521,-1.8500190400043,-9.31171019861519));
#24759=CARTESIAN_POINT('Ctrl Pts',(6.81942950598095,-1.64278532518974,-9.30187078375111));
#24760=CARTESIAN_POINT('Ctrl Pts',(6.9222311681217,-1.15058339330296,-9.27873901870707));
#24761=CARTESIAN_POINT('Ctrl Pts',(6.96376700641256,-0.864337889488257,
-9.26547632847848));
#24762=CARTESIAN_POINT('Ctrl Pts',(7.00300674771778,-0.388600837142123,
-9.24375578175975));
#24763=CARTESIAN_POINT('Ctrl Pts',(7.01091952486046,-0.200307405732222,
-9.23523773149981));
#24764=CARTESIAN_POINT('Ctrl Pts',(7.01161579047083,0.209153460630078,-9.21680406891329));
#24765=CARTESIAN_POINT('Ctrl Pts',(7.00153522190699,0.430123696089627,-9.20691390519347));
#24766=CARTESIAN_POINT('Ctrl Pts',(6.96403781339354,0.832693826912152,-9.18879542482949));
#24767=CARTESIAN_POINT('Ctrl Pts',(6.93989847695447,1.014400966877,-9.18057828843107));
#24768=CARTESIAN_POINT('Ctrl Pts',(6.89017627245457,1.30187235700103,-9.16737181638197));
#24769=CARTESIAN_POINT('Ctrl Pts',(6.86920351563081,1.40834760948636,-9.16242929894401));
#24770=CARTESIAN_POINT('Ctrl Pts',(6.78347668282857,1.79589911175014,-9.14427005405975));
#24771=CARTESIAN_POINT('Ctrl Pts',(6.70386803052358,2.07339406830289,-9.13096379629836));
#24772=CARTESIAN_POINT('Ctrl Pts',(6.53588682206941,2.54666731055961,-9.10791621983581));
#24773=CARTESIAN_POINT('Ctrl Pts',(6.45519931774765,2.74476499860548,-9.0981521436679));
#24774=CARTESIAN_POINT('Ctrl Pts',(6.27548975344534,3.13401577183411,-9.07869431602202));
#24775=CARTESIAN_POINT('Ctrl Pts',(6.17646680089845,3.32491899544151,-9.06901150243526));
#24776=CARTESIAN_POINT('Ctrl Pts',(5.93134215313975,3.74862480713826,-9.04703752610336));
#24777=CARTESIAN_POINT('Ctrl Pts',(5.78001485511577,3.97799374004855,-9.03479021895633));
#24778=CARTESIAN_POINT('Ctrl Pts',(5.54821455374222,4.28807877898038,-9.01735324692611));
#24779=CARTESIAN_POINT('Ctrl Pts',(5.47863802335601,4.37662307020571,-9.01226206298247));
#24780=CARTESIAN_POINT('Ctrl Pts',(5.37570018846381,4.50132036251301,-9.00490030870556));
#24781=CARTESIAN_POINT('Ctrl Pts',(5.34404473071823,4.53885705819345,-9.00265923001823));
#24782=CARTESIAN_POINT('Ctrl Pts',(5.12694212953571,4.79087496069243,-8.98744851412553));
#24783=CARTESIAN_POINT('Ctrl Pts',(4.92902658467874,4.99426822366104,-8.97436853820447));
#24784=CARTESIAN_POINT('Ctrl Pts',(4.55674781695201,5.33310535803238,-8.95125703918073));
#24785=CARTESIAN_POINT('Ctrl Pts',(4.38728197398616,5.47336483820739,-8.94121047947184));
#24786=CARTESIAN_POINT('Ctrl Pts',(4.04390378753554,5.73135369943985,-8.92171158334063));
#24787=CARTESIAN_POINT('Ctrl Pts',(3.87073839523873,5.84969736142594,-8.91226270498881));
#24788=CARTESIAN_POINT('Ctrl Pts',(3.43350890392148,6.12057893841721,-8.88916505283293));
#24789=CARTESIAN_POINT('Ctrl Pts',(3.16430536709535,6.26399541566597,-8.87558698468384));
#24790=CARTESIAN_POINT('Ctrl Pts',(2.789634337494,6.43326475561664,-8.85704322678649));
#24791=CARTESIAN_POINT('Ctrl Pts',(2.69165471315347,6.47487063609521,-8.8522208972402));
#24792=CARTESIAN_POINT('Ctrl Pts',(2.38880518474176,6.5954094766982,-8.83736128479388));
#24793=CARTESIAN_POINT('Ctrl Pts',(2.18114659618961,6.66696440665183,-8.82725894919786));
#24794=CARTESIAN_POINT('Ctrl Pts',(1.70104760554312,6.80756055696294,-8.80424551429163));
#24795=CARTESIAN_POINT('Ctrl Pts',(1.42711977915363,6.87020937909845,-8.79136282604805));
#24796=CARTESIAN_POINT('Ctrl Pts',(0.964729005599117,6.94710477029025,-8.77003258608758));
#24797=CARTESIAN_POINT('Ctrl Pts',(0.778118931541352,6.97047338331969,-8.7615314565525));
#24798=CARTESIAN_POINT('Ctrl Pts',(0.372032776105765,7.00481382531203,-8.74318308313487));
#24799=CARTESIAN_POINT('Ctrl Pts',(0.152523207717786,7.01302805488468,-8.73336056114841));
#24800=CARTESIAN_POINT('Ctrl Pts',(-0.255093735997572,7.00913207491632,
-8.71509397123718));
#24801=CARTESIAN_POINT('Ctrl Pts',(-0.443026827528892,6.99976648781566,
-8.70666039633668));
#24802=CARTESIAN_POINT('Ctrl Pts',(-0.739205899390721,6.97302995026178,
-8.69319613520645));
#24803=CARTESIAN_POINT('Ctrl Pts',(-0.847811881451378,6.96065990185586,
-8.68821651691027));
#24804=CARTESIAN_POINT('Ctrl Pts',(-1.10115160496994,6.92578771184345,-8.67651474288063));
#24805=CARTESIAN_POINT('Ctrl Pts',(-1.24555854211707,6.90127914005917,-8.66978183452009));
#24806=CARTESIAN_POINT('Ctrl Pts',(-1.6965882160546,6.81011252961119,-8.64861386731157));
#24807=CARTESIAN_POINT('Ctrl Pts',(-1.99957181749221,6.72738896653651,-8.6342056381497));
#24808=CARTESIAN_POINT('Ctrl Pts',(-2.47522606033523,6.56253486470539,-8.61130446702736));
#24809=CARTESIAN_POINT('Ctrl Pts',(-2.6518612157142,6.4931688361686,-8.60272984697376));
#24810=CARTESIAN_POINT('Ctrl Pts',(-3.03244035341468,6.32558894609971,-8.58401350154332));
#24811=CARTESIAN_POINT('Ctrl Pts',(-3.23488275015577,6.22449228667035,-8.57389964625463));
#24812=CARTESIAN_POINT('Ctrl Pts',(-3.59172571577048,6.02417207540035,-8.55555795444338));
#24813=CARTESIAN_POINT('Ctrl Pts',(-3.74779294308549,5.92833781657103,-8.54734360653233));
#24814=CARTESIAN_POINT('Ctrl Pts',(-3.9949918017487,5.76287713868979,-8.53386417815342));
#24815=CARTESIAN_POINT('Ctrl Pts',(-4.0884820789298,5.69693126292727,-8.5286456931841));
#24816=CARTESIAN_POINT('Ctrl Pts',(-4.31251610888672,5.53054681420163,-8.51586474445184));
#24817=CARTESIAN_POINT('Ctrl Pts',(-4.44121611984323,5.42773822158121,-8.50828693144187));
#24818=CARTESIAN_POINT('Ctrl Pts',(-4.77596570287999,5.14044808101262,-8.48799427053341));
#24819=CARTESIAN_POINT('Ctrl Pts',(-4.97492530895604,4.94814884130974,-8.47530973672958));
#24820=CARTESIAN_POINT('Ctrl Pts',(-5.2802353770552,4.61597897585171,-8.4547785319961));
#24821=CARTESIAN_POINT('Ctrl Pts',(-5.39361110877686,4.48297981094963,-8.44687395943722));
#24822=CARTESIAN_POINT('Ctrl Pts',(-5.63059353851227,4.18295934452165,-8.42964890297838));
#24823=CARTESIAN_POINT('Ctrl Pts',(-5.75198548675074,4.01439861804166,-8.42035171723981));
#24824=CARTESIAN_POINT('Ctrl Pts',(-5.98243789605577,3.66243952240189,-8.40150402343384));
#24825=CARTESIAN_POINT('Ctrl Pts',(-6.09096905111159,3.47895390888411,-8.39196295792931));
#24826=CARTESIAN_POINT('Ctrl Pts',(-6.23954140183416,3.19944627405982,-8.37763249214173));
#24827=CARTESIAN_POINT('Ctrl Pts',(-6.28607848509906,3.10701624938916,-8.3729202728785));
#24828=CARTESIAN_POINT('Ctrl Pts',(-6.48211764129864,2.69520323707306,-8.35206011545531));
#24829=CARTESIAN_POINT('Ctrl Pts',(-6.60944788205276,2.36583402036228,-8.33577429286849));
#24830=CARTESIAN_POINT('Ctrl Pts',(-6.76653161101002,1.84605459556445,-8.31091754506932));
#24831=CARTESIAN_POINT('Ctrl Pts',(-6.81415978112026,1.66165451476764,-8.30224882221859));
#24832=CARTESIAN_POINT('Ctrl Pts',(-6.95861947812567,0.990607171095191,
-8.27116381837615));
#24833=CARTESIAN_POINT('Ctrl Pts',(-7.01125445605145,0.495969930371231,
-8.24920677116425));
#24834=CARTESIAN_POINT('Ctrl Pts',(-7.01124999971706,-6.29887116476713E-5,
-8.22678901229957));
#24835=CARTESIAN_POINT('Ctrl Pts',(-7.01124999971675,-6.30228819856011E-5,
-8.22678901075528));
#24836=CARTESIAN_POINT('Ctrl Pts',(-7.01124918132822,-0.0911081541651411,
-8.22267430843915));
#24837=CARTESIAN_POINT('Ctrl Pts',(-7.00947497633958,-0.182142925889114,
-8.21854073419977));
#24838=CARTESIAN_POINT('Ctrl Pts',(-6.99953685041428,-0.437072884344599,
-8.20690147196852));
#24839=CARTESIAN_POINT('Ctrl Pts',(-6.98739183713415,-0.600752281441517,
-8.19936374275353));
#24840=CARTESIAN_POINT('Ctrl Pts',(-6.94396893096349,-0.996949710207563,
-8.18103189759171));
#24841=CARTESIAN_POINT('Ctrl Pts',(-6.90674368593749,-1.22861973404632,
-8.17024318619145));
#24842=CARTESIAN_POINT('Ctrl Pts',(-6.82218699227048,-1.62635116379858,
-8.15164360482691));
#24843=CARTESIAN_POINT('Ctrl Pts',(-6.78020561589611,-1.7933394799414,-8.14380870973982));
#24844=CARTESIAN_POINT('Ctrl Pts',(-6.6846911651413,-2.12164026690506,-8.12832257698379));
#24845=CARTESIAN_POINT('Ctrl Pts',(-6.63136950661576,-2.28283978608511,
-8.12067770055383));
#24846=CARTESIAN_POINT('Ctrl Pts',(-6.57227165853301,-2.44189922170096,
-8.11305756739085));
#24847=CARTESIAN_POINT('',(-7.01083548104182,7.7386374966269E-5,-8.77353436264612));
#24848=CARTESIAN_POINT('Ctrl Pts',(-6.57227159525839,-2.441899392002,-8.66029439624775));
#24849=CARTESIAN_POINT('Ctrl Pts',(-6.62943398574475,-2.28804917338076,
-8.66774640904247));
#24850=CARTESIAN_POINT('Ctrl Pts',(-6.6811857121734,-2.13220727019073,-8.67519842183719));
#24851=CARTESIAN_POINT('Ctrl Pts',(-6.72740127611852,-1.97476546267625,
-8.68265043463192));
#24852=CARTESIAN_POINT('Ctrl Pts',(-6.78061673854497,-1.79347721523458,
-8.6912311436621));
#24853=CARTESIAN_POINT('Ctrl Pts',(-6.82650811549892,-1.61000928425161,
-8.69981185269229));
#24854=CARTESIAN_POINT('Ctrl Pts',(-6.86491797772433,-1.42496586682535,
-8.70839256172248));
#24855=CARTESIAN_POINT('Ctrl Pts',(-6.90331958581666,-1.23996221452462,
-8.71697142679098));
#24856=CARTESIAN_POINT('Ctrl Pts',(-6.93424282786693,-1.05338404397609,
-8.72555029185948));
#24857=CARTESIAN_POINT('Ctrl Pts',(-6.9575812067861,-0.865846587726097,
-8.73412915692798));
#24858=CARTESIAN_POINT('Ctrl Pts',(-6.98091698638194,-0.678330018551714,
-8.74270706652121));
#24859=CARTESIAN_POINT('Ctrl Pts',(-6.99666955104869,-0.489854673144777,
-8.75128497611443));
#24860=CARTESIAN_POINT('Ctrl Pts',(-7.004784073487,-0.301042598850843,-8.75986288570765));
#24861=CARTESIAN_POINT('Ctrl Pts',(-7.00909504842534,-0.200733045636199,
-8.76442004277522));
#24862=CARTESIAN_POINT('Ctrl Pts',(-7.01125110605494,-0.100328544295878,
-8.7689771998428));
#24863=CARTESIAN_POINT('Ctrl Pts',(-7.01124999957427,7.72645793954891E-5,
-8.77353435691037));
#24864=CARTESIAN_POINT('Ctrl Pts',(-7.01071564309632,7.7421586253174E-5,
-8.77353436430433));
#24865=CARTESIAN_POINT('Ctrl Pts',(-7.01090830760592,0.492725215260218,
-8.79589606338762));
#24866=CARTESIAN_POINT('Ctrl Pts',(-6.83913257993509,2.14530585228538,-8.87091410477835));
#24867=CARTESIAN_POINT('Ctrl Pts',(-5.55442723662985,4.7455628683187,-8.99858848847648));
#24868=CARTESIAN_POINT('Ctrl Pts',(-2.62474354776125,6.81782592049443,-9.1565575153988));
#24869=CARTESIAN_POINT('Ctrl Pts',(0.938224379280063,7.24511999742928,-9.31452654232106));
#24870=CARTESIAN_POINT('Ctrl Pts',(4.2748224808499,5.92434990752088,-9.47249556924337));
#24871=CARTESIAN_POINT('Ctrl Pts',(6.58001406404274,3.17418394776362,-9.63046459616565));
#24872=CARTESIAN_POINT('Ctrl Pts',(7.29761463056158,-0.341832161412208,
-9.78843362308794));
#24873=CARTESIAN_POINT('Ctrl Pts',(6.25448545643946,-3.77537311475419,-9.94640265001023));
#24874=CARTESIAN_POINT('Ctrl Pts',(3.70230695067219,-6.29801144386563,-10.1043716769325));
#24875=CARTESIAN_POINT('Ctrl Pts',(0.256855774125145,-7.30110003209896,
-10.2623407038548));
#24876=CARTESIAN_POINT('Ctrl Pts',(-3.25056889473619,-6.54261565608652,
-10.4203097307771));
#24877=CARTESIAN_POINT('Ctrl Pts',(-5.53729420238302,-4.5801091614773,-10.5529622341764));
#24878=CARTESIAN_POINT('Ctrl Pts',(-6.36188242840926,-3.00629425112275,
-10.6329583952682));
#24879=CARTESIAN_POINT('Ctrl Pts',(-6.57172397189039,-2.44169584043291,
-10.6602982140526));
#24880=CARTESIAN_POINT('Origin',(0.,0.,-16.4167025567876));
#24881=CARTESIAN_POINT('',(-8.12521368785635,8.95665403536892E-5,-9.41670255780532));
#24882=CARTESIAN_POINT('Ctrl Pts',(4.94675008185374,-6.44587862049698,-10.7083437636031));
#24883=CARTESIAN_POINT('Ctrl Pts',(5.11324386102303,-6.31810657199534,-10.7001223210038));
#24884=CARTESIAN_POINT('Ctrl Pts',(5.27479811987266,-6.18387000071871,-10.6919008784046));
#24885=CARTESIAN_POINT('Ctrl Pts',(5.43091827111027,-6.04357628354442,-10.6836794358054));
#24886=CARTESIAN_POINT('Ctrl Pts',(5.58704849341192,-5.90327351624432,-10.6754574628539));
#24887=CARTESIAN_POINT('Ctrl Pts',(5.73774368584835,-5.75691301674722,-10.6672354899024));
#24888=CARTESIAN_POINT('Ctrl Pts',(5.88254383657361,-5.60494117482867,-10.659013516951));
#24889=CARTESIAN_POINT('Ctrl Pts',(6.0273393179283,-5.45297423354623,-10.6507918091335));
#24890=CARTESIAN_POINT('Ctrl Pts',(6.16623993542932,-5.29539652637689,-10.6425701013159));
#24891=CARTESIAN_POINT('Ctrl Pts',(6.29882356643554,-5.13269025379637,-10.6343483934984));
#24892=CARTESIAN_POINT('Ctrl Pts',(6.43143852287547,-4.96994553872851,-10.6261247431443));
#24893=CARTESIAN_POINT('Ctrl Pts',(6.55773332306666,-4.80207006492447,-10.6179010927901));
#24894=CARTESIAN_POINT('Ctrl Pts',(6.67732631326922,-4.6295789083482,-10.6096774424359));
#24895=CARTESIAN_POINT('Ctrl Pts',(6.77479347290812,-4.48900024177382,-10.6029752449198));
#24896=CARTESIAN_POINT('Ctrl Pts',(6.86780994836343,-4.34535645822659,-10.5962730474036));
#24897=CARTESIAN_POINT('Ctrl Pts',(6.95619037540507,-4.19894070256081,-10.5895708498875));
#24898=CARTESIAN_POINT('Ctrl Pts',(7.06463232354457,-4.01928995505725,-10.5813473169199));
#24899=CARTESIAN_POINT('Ctrl Pts',(7.16612867057859,-3.83540684465529,-10.5731237839523));
#24900=CARTESIAN_POINT('Ctrl Pts',(7.26036397147166,-3.64784903254729,-10.5649002509847));
#24901=CARTESIAN_POINT('Ctrl Pts',(7.35458213776429,-3.46032532366962,-10.5566782132843));
#24902=CARTESIAN_POINT('Ctrl Pts',(7.44154176065796,-3.26912851007378,-10.5484561755839));
#24903=CARTESIAN_POINT('Ctrl Pts',(7.52097373826056,-3.07484009192265,-10.5402341378835));
#24904=CARTESIAN_POINT('Ctrl Pts',(7.60039694531601,-2.88057312628707,-10.5320130080261));
#24905=CARTESIAN_POINT('Ctrl Pts',(7.67229405491373,-2.68321551050786,-10.5237918781687));
#24906=CARTESIAN_POINT('Ctrl Pts',(7.73644411056134,-2.48336869728615,-10.5155707483114));
#24907=CARTESIAN_POINT('Ctrl Pts',(7.80059925389462,-2.28350603438582,-10.5073489664433));
#24908=CARTESIAN_POINT('Ctrl Pts',(7.85700602295709,-2.08115405960809,-10.4991271845752));
#24909=CARTESIAN_POINT('Ctrl Pts',(7.90549302236132,-1.87693037587877,-10.4909054027071));
#24910=CARTESIAN_POINT('Ctrl Pts',(7.95397988712744,-1.67270725923533,-10.4826836436692));
#24911=CARTESIAN_POINT('Ctrl Pts',(7.99454696072024,-1.46661273161586,-10.4744618846312));
#24912=CARTESIAN_POINT('Ctrl Pts',(8.02707363735951,-1.25927613449469,-10.4662401255933));
#24913=CARTESIAN_POINT('Ctrl Pts',(8.05960709533697,-1.05189631071383,-10.4580166524384));
#24914=CARTESIAN_POINT('Ctrl Pts',(8.08409676186509,-0.843274191539016,
-10.4497931792834));
#24915=CARTESIAN_POINT('Ctrl Pts',(8.10047357116718,-0.634046910978997,
-10.4415697061285));
#24916=CARTESIAN_POINT('Ctrl Pts',(8.1070904883195,-0.549510322933475,-10.4382470784074));
#24917=CARTESIAN_POINT('Ctrl Pts',(8.11238357345324,-0.464875002095556,
-10.4349244506863));
#24918=CARTESIAN_POINT('Ctrl Pts',(8.11635067845989,-0.380183148973766,
-10.4316018229652));
#24919=CARTESIAN_POINT('Ctrl Pts',(8.12616931096018,-0.170569796118993,
-10.4233782794809));
#24920=CARTESIAN_POINT('Ctrl Pts',(8.12786496895076,0.039458169528622,-10.4151547359967));
#24921=CARTESIAN_POINT('Ctrl Pts',(8.12142579447583,0.249260159918624,-10.4069311925124));
#24922=CARTESIAN_POINT('Ctrl Pts',(8.11498779070991,0.459024006120668,-10.3987091441541));
#24923=CARTESIAN_POINT('Ctrl Pts',(8.10041791543133,0.668561664416116,-10.3904870957957));
#24924=CARTESIAN_POINT('Ctrl Pts',(8.07775641410193,0.877233650138387,-10.3822650474373));
#24925=CARTESIAN_POINT('Ctrl Pts',(8.0550974146648,1.08588259789764,-10.3740439068158));
#24926=CARTESIAN_POINT('Ctrl Pts',(8.02434860452279,1.29366577079501,-10.3658227661942));
#24927=CARTESIAN_POINT('Ctrl Pts',(7.98560206685205,1.49994906326457,-10.3576016255727));
#24928=CARTESIAN_POINT('Ctrl Pts',(7.94685245586464,1.70624871781239,-10.3493798328627));
#24929=CARTESIAN_POINT('Ctrl Pts',(7.90010390166676,1.91104796386036,-10.3411580401528));
#24930=CARTESIAN_POINT('Ctrl Pts',(7.84549975958371,2.11372209262994,-10.3329362474428));
#24931=CARTESIAN_POINT('Ctrl Pts',(7.7908957689595,2.31639565922995,-10.3247144775382));
#24932=CARTESIAN_POINT('Ctrl Pts',(7.72843631336478,2.51694383626728,-10.3164927076335));
#24933=CARTESIAN_POINT('Ctrl Pts',(7.658314999941,2.71475577615717,-10.3082709377288));
#24934=CARTESIAN_POINT('Ctrl Pts',(7.58817906754253,2.91260895611515,-10.3000474537398));
#24935=CARTESIAN_POINT('Ctrl Pts',(7.5103781848199,3.10772448128915,-10.2918239697508));
#24936=CARTESIAN_POINT('Ctrl Pts',(7.42515499169712,3.29950919255808,-10.2836004857617));
#24937=CARTESIAN_POINT('Ctrl Pts',(7.39072196440478,3.37699664586041,-10.2802779225221));
#24938=CARTESIAN_POINT('Ctrl Pts',(7.35507784413455,3.45394059557975,-10.2769553592825));
#24939=CARTESIAN_POINT('Ctrl Pts',(7.31824083470829,3.53030291160804,-10.2736327960429));
#24940=CARTESIAN_POINT('Ctrl Pts',(7.22706710013741,3.71930407215873,-10.2654092593437));
#24941=CARTESIAN_POINT('Ctrl Pts',(7.12855291764284,3.90480206002756,-10.2571857226446));
#24942=CARTESIAN_POINT('Ctrl Pts',(7.02299287655094,4.08622792051726,-10.2489621859455));
#24943=CARTESIAN_POINT('Ctrl Pts',(6.91745202847966,4.26762079399552,-10.2407401444571));
#24944=CARTESIAN_POINT('Ctrl Pts',(6.80486802695956,4.44494276304557,-10.2325181029687));
#24945=CARTESIAN_POINT('Ctrl Pts',(6.68558075375882,4.61765065238479,-10.2242960614803));
#24946=CARTESIAN_POINT('Ctrl Pts',(6.5663066511169,4.79033947297213,-10.2160749277911));
#24947=CARTESIAN_POINT('Ctrl Pts',(6.44033092194771,4.95841498834916,-10.2078537941018));
#24948=CARTESIAN_POINT('Ctrl Pts',(6.3080364709158,5.12136343604866,-10.1996326604125));
#24949=CARTESIAN_POINT('Ctrl Pts',(6.17573152713792,5.28432480777221,-10.1914108746758));
#24950=CARTESIAN_POINT('Ctrl Pts',(6.03710704397904,5.44215806865236,-10.183189088939));
#24951=CARTESIAN_POINT('Ctrl Pts',(5.89258653862695,5.59438213275536,-10.1749673032022));
#24952=CARTESIAN_POINT('Ctrl Pts',(5.7480664343292,5.74660577442613,-10.1667455402815));
#24953=CARTESIAN_POINT('Ctrl Pts',(5.59765054558968,5.89322003842304,-10.1585237773607));
#24954=CARTESIAN_POINT('Ctrl Pts',(5.44179997913404,6.0337799553511,-10.15030201444));
#24955=CARTESIAN_POINT('Ctrl Pts',(5.2859169201942,6.17436917689437,-10.1420785374061));
#24956=CARTESIAN_POINT('Ctrl Pts',(5.12459713908876,6.30890133221201,-10.1338550603722));
#24957=CARTESIAN_POINT('Ctrl Pts',(4.95833643774039,6.43697035356509,-10.1256315833383));
#24958=CARTESIAN_POINT('Ctrl Pts',(4.89116064434143,6.48871522201236,-10.1223089785991));
#24959=CARTESIAN_POINT('Ctrl Pts',(4.82317863122845,6.53940546242915,-10.1189863738598));
#24960=CARTESIAN_POINT('Ctrl Pts',(4.75442456323024,6.58901621147292,-10.1156637691206));
#24961=CARTESIAN_POINT('Ctrl Pts',(4.58425631376351,6.71180420882794,-10.1074402290653));
#24962=CARTESIAN_POINT('Ctrl Pts',(4.40930119041436,6.82801646716751,-10.0992166890101));
#24963=CARTESIAN_POINT('Ctrl Pts',(4.23008915387307,6.93729293837196,-10.0909931489548));
#24964=CARTESIAN_POINT('Ctrl Pts',(4.05090970095194,7.04654954136275,-10.0827711040709));
#24965=CARTESIAN_POINT('Ctrl Pts',(3.86747513129313,7.14887272063463,-10.074549059187));
#24966=CARTESIAN_POINT('Ctrl Pts',(3.6803429591141,7.24394666364954,-10.0663270143031));
#24967=CARTESIAN_POINT('Ctrl Pts',(3.49323144762652,7.33901010984084,-10.0581058771901));
#24968=CARTESIAN_POINT('Ctrl Pts',(3.30242341149901,7.42682578413742,-10.049884740077));
#24969=CARTESIAN_POINT('Ctrl Pts',(3.10850019267276,7.50712422400571,-10.041663602964));
#24970=CARTESIAN_POINT('Ctrl Pts',(2.91456159272127,7.5874290327883,-10.033441813787));
#24971=CARTESIAN_POINT('Ctrl Pts',(2.71750758786926,7.6602153005277,-10.02522002461));
#24972=CARTESIAN_POINT('Ctrl Pts',(2.51793967416545,7.72526163697797,-10.016998235433));
#24973=CARTESIAN_POINT('Ctrl Pts',(2.31837231420016,7.79030779294501,-10.0087764690689));
#24974=CARTESIAN_POINT('Ctrl Pts',(2.11629134058487,7.84761397174942,-10.0005547027048));
#24975=CARTESIAN_POINT('Ctrl Pts',(1.91231410721149,7.89700844104018,-9.99233293634071));
#24976=CARTESIAN_POINT('Ctrl Pts',(1.70829434812204,7.94641320822127,-9.9841094558809));
#24977=CARTESIAN_POINT('Ctrl Pts',(1.50237782620332,7.98790290132602,-9.97588597542108));
#24978=CARTESIAN_POINT('Ctrl Pts',(1.29519388187691,8.02135651687722,-9.96766249496127));
#24979=CARTESIAN_POINT('Ctrl Pts',(1.21148405675715,8.03487299044624,-9.96433991070695));
#24980=CARTESIAN_POINT('Ctrl Pts',(1.1275674387783,8.04707819603545,-9.96101732645263));
#24981=CARTESIAN_POINT('Ctrl Pts',(1.04348590916681,8.05796653752486,-9.95769474219831));
#24982=CARTESIAN_POINT('Ctrl Pts',(0.835380510040261,8.08491565062911,-9.9494712033834));
#24983=CARTESIAN_POINT('Ctrl Pts',(0.62619676826291,8.10380302437128,-9.9412476645685));
#24984=CARTESIAN_POINT('Ctrl Pts',(0.416572149134518,8.11456438800417,-9.93302412575359));
#24985=CARTESIAN_POINT('Ctrl Pts',(0.206985643462719,8.12532379503116,-9.92480208212323));
#24986=CARTESIAN_POINT('Ctrl Pts',(-0.0030412851703448,8.12796012566084,
-9.91658003849286));
#24987=CARTESIAN_POINT('Ctrl Pts',(-0.212868004803957,8.12246112794828,
-9.9083579948625));
#24988=CARTESIAN_POINT('Ctrl Pts',(-0.422671557875082,8.11696273736942,
-9.90013685901207));
#24989=CARTESIAN_POINT('Ctrl Pts',(-0.632274651359207,8.103330819407,-9.89191572316165));
#24990=CARTESIAN_POINT('Ctrl Pts',(-0.841037769756865,8.08160522621233,
-9.88369458731123));
#24991=CARTESIAN_POINT('Ctrl Pts',(-1.04981744621454,8.05987790985084,-9.87547279940089));
#24992=CARTESIAN_POINT('Ctrl Pts',(-1.25775672083429,8.03005566347492,-9.86725101149056));
#24993=CARTESIAN_POINT('Ctrl Pts',(-1.46422124509005,7.99223020864182,-9.85902922358022));
#24994=CARTESIAN_POINT('Ctrl Pts',(-1.67068519647114,7.95440485876257,-9.85080745848278));
#24995=CARTESIAN_POINT('Ctrl Pts',(-1.87567411605584,7.90857640064783,-9.84258569338535));
#24996=CARTESIAN_POINT('Ctrl Pts',(-2.07856335525882,7.85488777390709,-9.83436392828791));
#24997=CARTESIAN_POINT('Ctrl Pts',(-2.28149489355781,7.80118795396367,-9.82614044908659));
#24998=CARTESIAN_POINT('Ctrl Pts',(-2.4823255918076,7.73962476716973,-9.81791696988528));
#24999=CARTESIAN_POINT('Ctrl Pts',(-2.68044441560244,7.67039146962954,-9.80969349068397));
#25000=CARTESIAN_POINT('Ctrl Pts',(-2.76049179746798,7.64241863948722,-9.80637089888132));
#25001=CARTESIAN_POINT('Ctrl Pts',(-2.84009665958289,7.61319425858774,-9.80304830707867));
#25002=CARTESIAN_POINT('Ctrl Pts',(-2.91921950827893,7.58273334787553,-9.79972571527603));
#25003=CARTESIAN_POINT('Ctrl Pts',(-3.1150515197089,7.5073414539654,-9.79150217622762));
#25004=CARTESIAN_POINT('Ctrl Pts',(-3.30799316668953,7.42434691148092,-9.78327863717921));
#25005=CARTESIAN_POINT('Ctrl Pts',(-3.49745328333352,7.33399673393707,-9.7750550981308));
#25006=CARTESIAN_POINT('Ctrl Pts',(-3.68687895281885,7.24366298363371,-9.76683305426544));
#25007=CARTESIAN_POINT('Ctrl Pts',(-3.87282408928764,7.14597639442396,-9.75861101040008));
#25008=CARTESIAN_POINT('Ctrl Pts',(-4.05471951110016,7.04123123102797,-9.75038896653472));
#25009=CARTESIAN_POINT('Ctrl Pts',(-4.23659485020781,6.93649763233317,-9.74216783044855));
#25010=CARTESIAN_POINT('Ctrl Pts',(-4.41442111183242,6.82470716246459,-9.73394669436239));
#25011=CARTESIAN_POINT('Ctrl Pts',(-4.58765490561207,6.706199372932,-9.72572555827623));
#25012=CARTESIAN_POINT('Ctrl Pts',(-4.76090243942555,6.58768218395718,-9.71750377013087));
#25013=CARTESIAN_POINT('Ctrl Pts',(-4.92955653265772,6.46244677510975,-9.70928198198552));
#25014=CARTESIAN_POINT('Ctrl Pts',(-5.09310303634507,6.33087584964929,-9.70106019384016));
#25015=CARTESIAN_POINT('Ctrl Pts',(-5.25664908622561,6.1993052892702,-9.69283842850852));
#25016=CARTESIAN_POINT('Ctrl Pts',(-5.41508734680205,6.0613994344153,-9.68461666317688));
#25017=CARTESIAN_POINT('Ctrl Pts',(-5.56793658648711,5.91758140893374,-9.67639489784523));
#25018=CARTESIAN_POINT('Ctrl Pts',(-5.72081769269233,5.77373339978974,-9.66817141841249));
#25019=CARTESIAN_POINT('Ctrl Pts',(-5.86810723539858,5.62397095980253,-9.65994793897975));
#25020=CARTESIAN_POINT('Ctrl Pts',(-6.00935991315134,5.46875497683977,-9.651724459547));
#25021=CARTESIAN_POINT('Ctrl Pts',(-6.06643122883918,5.40604196846076,-9.64840186914924));
#25022=CARTESIAN_POINT('Ctrl Pts',(-6.12251748081821,5.34243910080151,-9.64507927875149));
#25023=CARTESIAN_POINT('Ctrl Pts',(-6.17759109212944,5.27797838769192,-9.64175668835373));
#25024=CARTESIAN_POINT('Ctrl Pts',(-6.31390040065081,5.11843564078345,-9.63353314918797));
#25025=CARTESIAN_POINT('Ctrl Pts',(-6.44404800923583,4.95358366325013,-9.6253096100222));
#25026=CARTESIAN_POINT('Ctrl Pts',(-6.56763168481993,4.7839211547693,-9.61708607085644));
#25027=CARTESIAN_POINT('Ctrl Pts',(-6.69119289076534,4.61428949385187,-9.6088640268716));
#25028=CARTESIAN_POINT('Ctrl Pts',(-6.80819237210817,4.43984928594032,-9.60064198288675));
#25029=CARTESIAN_POINT('Ctrl Pts',(-6.91826972669666,4.2611303137985,-9.59241993890191));
#25030=CARTESIAN_POINT('Ctrl Pts',(-7.02833492789097,4.08243107361812,-9.58419880269453));
#25031=CARTESIAN_POINT('Ctrl Pts',(-7.13147937352829,3.89945426337947,-9.57597766648715));
#25032=CARTESIAN_POINT('Ctrl Pts',(-7.22738690476808,3.71275720877178,-9.56775653027977));
#25033=CARTESIAN_POINT('Ctrl Pts',(-7.32330204293134,3.52604534625292,-9.55953474201146));
#25034=CARTESIAN_POINT('Ctrl Pts',(-7.41197898266931,3.33561291092459,-9.55131295374316));
#25035=CARTESIAN_POINT('Ctrl Pts',(-7.49314782575478,3.14204125114334,-9.54309116547485));
#25036=CARTESIAN_POINT('Ctrl Pts',(-7.57431644362136,2.94847012846468,-9.53486940001951));
#25037=CARTESIAN_POINT('Ctrl Pts',(-7.64797689494447,2.7517600717876,-9.52664763456417));
#25038=CARTESIAN_POINT('Ctrl Pts',(-7.71390747417866,2.55251230012914,-9.51842586910882));
#25039=CARTESIAN_POINT('Ctrl Pts',(-7.77985179884272,2.35322298862219,-9.51020238955205));
#25040=CARTESIAN_POINT('Ctrl Pts',(-7.83806293933497,2.15139518525295,-9.50197890999527));
#25041=CARTESIAN_POINT('Ctrl Pts',(-7.88836876716378,1.94764620907776,-9.49375543043849));
#25042=CARTESIAN_POINT('Ctrl Pts',(-7.90869418083824,1.86532409243151,-9.49043284076948));
#25043=CARTESIAN_POINT('Ctrl Pts',(-7.9277296580035,1.7826885076049,-9.48711025110047));
#25044=CARTESIAN_POINT('Ctrl Pts',(-7.94546619198763,1.69978073717808,-9.48378766143146));
#25045=CARTESIAN_POINT('Ctrl Pts',(-7.9902909041595,1.49025180951269,-9.47539063607622));
#25046=CARTESIAN_POINT('Ctrl Pts',(-8.02682757236947,1.27892832382411,-9.46699361072099));
#25047=CARTESIAN_POINT('Ctrl Pts',(-8.05495717630292,1.06646727583459,-9.45859658536576));
#25048=CARTESIAN_POINT('Ctrl Pts',(-8.08307984587844,0.85405860259438,-9.45020162999983));
#25049=CARTESIAN_POINT('Ctrl Pts',(-8.10279955479153,0.64051319213268,-9.44180667463391));
#25050=CARTESIAN_POINT('Ctrl Pts',(-8.11404888660069,0.426495285265938,
-9.43341171926798));
#25051=CARTESIAN_POINT('Ctrl Pts',(-8.12151237281116,0.284502878624238,
-9.42784199880156));
#25052=CARTESIAN_POINT('Ctrl Pts',(-8.12524843182286,0.142302641431262,
-9.42227227833514));
#25053=CARTESIAN_POINT('Ctrl Pts',(-8.12524999950632,8.95685591188772E-5,
-9.41670255786871));
#25054=CARTESIAN_POINT('Ctrl Pts',(-8.12463074038876,8.95341310840764E-5,
-9.41670255678762));
#25055=CARTESIAN_POINT('Ctrl Pts',(-8.124328237486,-0.773372194525053,-9.38640791602813));
#25056=CARTESIAN_POINT('Ctrl Pts',(-7.8241694511866,-2.89144900506152,-9.30345693296121));
#25057=CARTESIAN_POINT('Ctrl Pts',(-6.00817426353592,-5.96502784783864,
-9.16784960758686));
#25058=CARTESIAN_POINT('Ctrl Pts',(-2.44310026360785,-8.10623070945008,
-9.00988058066457));
#25059=CARTESIAN_POINT('Ctrl Pts',(1.58509684317598,-8.28596807580914,-8.85671523469708));
#25060=CARTESIAN_POINT('Ctrl Pts',(3.97770688061432,-7.18910576064169,-8.75620623103704));
#25061=CARTESIAN_POINT('Ctrl Pts',(4.94707560569883,-6.44630337359169,-8.70835356968441));
#25062=CARTESIAN_POINT('',(-8.12524999771476,0.000192707558782804,-9.58329744321239));
#25063=CARTESIAN_POINT('Ctrl Pts',(-8.12524999771476,0.000192707558782804,
-9.58329744321239));
#25064=CARTESIAN_POINT('Ctrl Pts',(-8.12525496787522,-0.20936729363032,
-9.57508874610108));
#25065=CARTESIAN_POINT('Ctrl Pts',(-8.11714838747745,-0.418942865113511,
-9.56688004898976));
#25066=CARTESIAN_POINT('Ctrl Pts',(-8.10095270917323,-0.62789550582793,
-9.55867135187845));
#25067=CARTESIAN_POINT('Ctrl Pts',(-8.08475586360825,-0.836863206252313,
-9.55046206314696));
#25068=CARTESIAN_POINT('Ctrl Pts',(-8.06046877518818,-1.04520759010267,
-9.54225277441548));
#25069=CARTESIAN_POINT('Ctrl Pts',(-8.02816588827779,-1.25229390831103,
-9.53404348568399));
#25070=CARTESIAN_POINT('Ctrl Pts',(-7.99586328014076,-1.45937843936803,
-9.52583426779852));
#25071=CARTESIAN_POINT('Ctrl Pts',(-7.9555450600785,-1.66520463367737,-9.51762504991305));
#25072=CARTESIAN_POINT('Ctrl Pts',(-7.90733713346637,-1.86914606711297,
-9.50941583202759));
#25073=CARTESIAN_POINT('Ctrl Pts',(-7.85911838623119,-2.07313327670053,
-9.5012047715229));
#25074=CARTESIAN_POINT('Ctrl Pts',(-7.80300646254863,-2.27523459131867,
-9.49299371101821));
#25075=CARTESIAN_POINT('Ctrl Pts',(-7.73917793735757,-2.47483583625619,
-9.48478265051352));
#25076=CARTESIAN_POINT('Ctrl Pts',(-7.70734013857672,-2.57439734505975,
-9.4806869567568));
#25077=CARTESIAN_POINT('Ctrl Pts',(-7.67358320372099,-2.67333705226453,
-9.47659126300008));
#25078=CARTESIAN_POINT('Ctrl Pts',(-7.63793365164408,-2.77158025241609,
-9.47249556924336));
#25079=CARTESIAN_POINT('Ctrl Pts',(-7.56635468679208,-2.96883789412297,
-9.46427202918809));
#25080=CARTESIAN_POINT('Ctrl Pts',(-7.48711843473188,-3.16335319052398,
-9.45604848913282));
#25081=CARTESIAN_POINT('Ctrl Pts',(-7.40046039517722,-3.35453029527434,
-9.44782494907755));
#25082=CARTESIAN_POINT('Ctrl Pts',(-7.31381811144289,-3.54567264096337,
-9.43960290419365));
#25083=CARTESIAN_POINT('Ctrl Pts',(-7.2197568551662,-3.73347773788535,-9.43138085930975));
#25084=CARTESIAN_POINT('Ctrl Pts',(-7.11855979482363,-3.91737080323277,
-9.42315881442585));
#25085=CARTESIAN_POINT('Ctrl Pts',(-7.01737390733895,-4.10124356550934,
-9.41493767731277));
#25086=CARTESIAN_POINT('Ctrl Pts',(-6.9090539308259,-4.28120490022198,-9.4067165401997));
#25087=CARTESIAN_POINT('Ctrl Pts',(-6.7939288123268,-4.45670493251862,-9.39849540308663));
#25088=CARTESIAN_POINT('Ctrl Pts',(-6.67879456261701,-4.6322188846947,-9.39027361390964));
#25089=CARTESIAN_POINT('Ctrl Pts',(-6.5568542520048,-4.80327057935863,-9.38205182473265));
#25090=CARTESIAN_POINT('Ctrl Pts',(-6.42848053838611,-4.96933854049922,
-9.37383003555567));
#25091=CARTESIAN_POINT('Ctrl Pts',(-6.30010718096393,-5.13540604085369,
-9.36560826919155));
#25092=CARTESIAN_POINT('Ctrl Pts',(-6.16530063875436,-5.2964896036532,-9.35738650282743));
#25093=CARTESIAN_POINT('Ctrl Pts',(-6.02447462116785,-5.45209987999161,
-9.34916473646332));
#25094=CARTESIAN_POINT('Ctrl Pts',(-5.88361924379905,-5.60774259837384,
-9.3409412560035));
#25095=CARTESIAN_POINT('Ctrl Pts',(-5.7367420819481,-5.75790953201645,-9.33271777554369));
#25096=CARTESIAN_POINT('Ctrl Pts',(-5.5842952989107,-5.90214652283929,-9.32449429508388));
#25097=CARTESIAN_POINT('Ctrl Pts',(-5.52270127149018,-5.9604234965529,-9.32117171082961));
#25098=CARTESIAN_POINT('Ctrl Pts',(-5.46019844734465,-6.01773285695843,
-9.31784912657534));
#25099=CARTESIAN_POINT('Ctrl Pts',(-5.39681829916226,-6.07404641144002,
-9.31452654232107));
#25100=CARTESIAN_POINT('Ctrl Pts',(-5.239949708696,-6.21342487881518,-9.30630300350617));
#25101=CARTESIAN_POINT('Ctrl Pts',(-5.07765336222313,-6.34674579477515,
-9.29807946469126));
#25102=CARTESIAN_POINT('Ctrl Pts',(-4.91042006300688,-6.4735973281723,-9.28985592587636));
#25103=CARTESIAN_POINT('Ctrl Pts',(-4.74321716975749,-6.60042579772068,
-9.28163388224602));
#25104=CARTESIAN_POINT('Ctrl Pts',(-4.57107935018773,-6.72078705420987,
-9.27341183861569));
#25105=CARTESIAN_POINT('Ctrl Pts',(-4.39452929623703,-6.83431048658272,
-9.26518979498536));
#25106=CARTESIAN_POINT('Ctrl Pts',(-4.21799873483613,-6.94782138505308,
-9.25696865913495));
#25107=CARTESIAN_POINT('Ctrl Pts',(-4.03705715960278,-7.05449580718584,
-9.24874752328454));
#25108=CARTESIAN_POINT('Ctrl Pts',(-3.85225565845309,-7.15400684263135,
-9.24052638743413));
#25109=CARTESIAN_POINT('Ctrl Pts',(-3.66743949975987,-7.25352577080135,
-9.23230459952378));
#25110=CARTESIAN_POINT('Ctrl Pts',(-3.47876306186508,-7.34588003487075,
-9.22408281161343));
#25111=CARTESIAN_POINT('Ctrl Pts',(-3.28680234819714,-7.43078851040626,
-9.21586102370307));
#25112=CARTESIAN_POINT('Ctrl Pts',(-3.09484216716088,-7.51569675034699,
-9.20763925860564));
#25113=CARTESIAN_POINT('Ctrl Pts',(-2.89959799939557,-7.59315912624164,
-9.19941749350821));
#25114=CARTESIAN_POINT('Ctrl Pts',(-2.70166665009423,-7.66294231181918,
-9.19119572841078));
#25115=CARTESIAN_POINT('Ctrl Pts',(-2.50369403533593,-7.73274004605235,
-9.18297224920947));
#25116=CARTESIAN_POINT('Ctrl Pts',(-2.30303339805748,-7.79485529357421,
-9.17474877000816));
#25117=CARTESIAN_POINT('Ctrl Pts',(-2.10029860215858,-7.84910398353027,
-9.16652529080685));
#25118=CARTESIAN_POINT('Ctrl Pts',(-2.01838619568401,-7.87102247424959,
-9.16320269900416));
#25119=CARTESIAN_POINT('Ctrl Pts',(-1.93613535735116,-7.89165735018837,
-9.15988010720147));
#25120=CARTESIAN_POINT('Ctrl Pts',(-1.85358718734212,-7.91099880555048,
-9.15655751539878));
#25121=CARTESIAN_POINT('Ctrl Pts',(-1.64927737748347,-7.95886963136031,
-9.14833397635037));
#25122=CARTESIAN_POINT('Ctrl Pts',(-1.44307892078272,-7.99882923191098,
-9.14011043730195));
#25123=CARTESIAN_POINT('Ctrl Pts',(-1.23561950582139,-8.03074915554792,
-9.13188689825353));
#25124=CARTESIAN_POINT('Ctrl Pts',(-1.02819781060594,-8.06266327558512,
-9.12366485438817));
#25125=CARTESIAN_POINT('Ctrl Pts',(-0.819515906075216,-8.08654059137286,
-9.11544281052281));
#25126=CARTESIAN_POINT('Ctrl Pts',(-0.610209895465547,-8.10230408254195,
-9.10722076665745));
#25127=CARTESIAN_POINT('Ctrl Pts',(-0.400926993910222,-8.11806583329578,
-9.09899963057137));
#25128=CARTESIAN_POINT('Ctrl Pts',(-0.191020417832148,-8.12571552578341,
-9.09077849448529));
#25129=CARTESIAN_POINT('Ctrl Pts',(0.01886956737902,-8.12522808922475,-9.0825573583992));
#25130=CARTESIAN_POINT('Ctrl Pts',(0.228776200010718,-8.12474061400507,
-9.07433557025385));
#25131=CARTESIAN_POINT('Ctrl Pts',(0.438665944197674,-8.11611471821314,
-9.0661137821085));
#25132=CARTESIAN_POINT('Ctrl Pts',(0.647898425864787,-8.09937745708038,
-9.05789199396315));
#25133=CARTESIAN_POINT('Ctrl Pts',(0.857130326957093,-8.0826402423899,-9.04967022863148));
#25134=CARTESIAN_POINT('Ctrl Pts',(1.0657046753998,-8.05779173358663,-9.04144846329982));
#25135=CARTESIAN_POINT('Ctrl Pts',(1.27298556404421,-8.02491092263553,-9.03322669796815));
#25136=CARTESIAN_POINT('Ctrl Pts',(1.48030966730031,-7.99202325658319,-9.0250032185354));
#25137=CARTESIAN_POINT('Ctrl Pts',(1.6863394807022,-7.95109998922567,-9.01677973910264));
#25138=CARTESIAN_POINT('Ctrl Pts',(1.8904475494082,-7.90227154844963,-9.00855625966988));
#25139=CARTESIAN_POINT('Ctrl Pts',(1.97291477204086,-7.88254304912174,-9.00523366927209));
#25140=CARTESIAN_POINT('Ctrl Pts',(2.05506840269879,-7.86152464277297,-9.00191107887428));
#25141=CARTESIAN_POINT('Ctrl Pts',(2.13686763041419,-7.83922727649786,-8.99858848847649));
#25142=CARTESIAN_POINT('Ctrl Pts',(2.33932188973639,-7.78404097584268,-8.99036502968837));
#25143=CARTESIAN_POINT('Ctrl Pts',(2.53967004483497,-7.72099870846218,-8.98214157090025));
#25144=CARTESIAN_POINT('Ctrl Pts',(2.73729898511362,-7.6502863886652,-8.97391811211213));
#25145=CARTESIAN_POINT('Ctrl Pts',(2.93550376974204,-7.57936802976403,-8.96567069209509));
#25146=CARTESIAN_POINT('Ctrl Pts',(3.13097317892045,-7.50073492507245,-8.95742327207806));
#25147=CARTESIAN_POINT('Ctrl Pts',(3.32310566778239,-7.4146244870022,-8.94917585206102));
#25148=CARTESIAN_POINT('Ctrl Pts',(3.5146335017164,-7.32878504474859,-8.94095438727511));
#25149=CARTESIAN_POINT('Ctrl Pts',(3.70284512438198,-7.23551540107621,-8.93273292248921));
#25150=CARTESIAN_POINT('Ctrl Pts',(3.88716557477536,-7.13509855270278,-8.9245114577033));
#25151=CARTESIAN_POINT('Ctrl Pts',(4.07235887690803,-7.03420617912002,-8.9162510600707));
#25152=CARTESIAN_POINT('Ctrl Pts',(4.25362378264773,-6.92609885551256,-8.9079906624381));
#25153=CARTESIAN_POINT('Ctrl Pts',(4.43040241461211,-6.81111018902933,-8.89973026480549));
#25154=CARTESIAN_POINT('Ctrl Pts',(4.60718104657649,-6.6961215225461,-8.89146986717289));
#25155=CARTESIAN_POINT('Ctrl Pts',(4.77947315318472,-6.57425168013767,-8.88320946954029));
#25156=CARTESIAN_POINT('Ctrl Pts',(4.94675008185375,-6.44587862049697,-8.87494907190769));
#25157=CARTESIAN_POINT('Ctrl Pts',(4.94701442880054,-6.44622255101802,-10.8749380057189));
#25158=CARTESIAN_POINT('Ctrl Pts',(5.88239992671177,-5.72708597335159,-10.8287079320199));
#25159=CARTESIAN_POINT('Ctrl Pts',(7.54661450291582,-3.74878751104997,-10.7298215160133));
#25160=CARTESIAN_POINT('Ctrl Pts',(8.46533576428991,0.133483448085083,-10.5782787576994));
#25161=CARTESIAN_POINT('Ctrl Pts',(7.38054169264561,4.14816882234201,-10.4203097307771));
#25162=CARTESIAN_POINT('Ctrl Pts',(4.51501107248497,7.16201092752528,-10.2623407038548));
#25163=CARTESIAN_POINT('Ctrl Pts',(0.560121710166043,8.44783839312321,-10.1043716769325));
#25164=CARTESIAN_POINT('Ctrl Pts',(-3.52991045919384,7.69541743414669,-9.94640265001023));
#25165=CARTESIAN_POINT('Ctrl Pts',(-6.76826471849102,5.08628620969646,-9.78843362308794));
#25166=CARTESIAN_POINT('Ctrl Pts',(-7.99827042167485,2.14691493907655,-9.66739855694933));
#25167=CARTESIAN_POINT('Ctrl Pts',(-8.1253377544992,0.401556537849047,-9.59901983311814));
#25168=CARTESIAN_POINT('Ctrl Pts',(-8.1249788462242,0.000192915105033694,
-9.58329745159439));
#25169=CARTESIAN_POINT('Ctrl Pts',(5.30944861964463,-4.57791378026326,-11.9996110935251));
#25170=CARTESIAN_POINT('Ctrl Pts',(6.06687727096382,-3.6994534565604,-11.9469459372515));
#25171=CARTESIAN_POINT('Ctrl Pts',(7.13654022615018,-1.56045331767952,-11.8416244386703));
#25172=CARTESIAN_POINT('Ctrl Pts',(7.01811917762224,2.02657116595001,-11.6836465977818));
#25173=CARTESIAN_POINT('Ctrl Pts',(5.20670544824235,5.12353011424085,-11.5256775708595));
#25174=CARTESIAN_POINT('Ctrl Pts',(2.1389031829018,6.98475869103201,-11.3677085439372));
#25175=CARTESIAN_POINT('Ctrl Pts',(-1.44489008506026,7.16051286830259,-11.209739517015));
#25176=CARTESIAN_POINT('Ctrl Pts',(-4.68010501547651,5.60873401464311,-11.0517704900927));
#25177=CARTESIAN_POINT('Ctrl Pts',(-6.7861098885743,2.70364896469204,-10.8938014631704));
#25178=CARTESIAN_POINT('Ctrl Pts',(-7.25480791088177,-0.85372703166743,
-10.7358324362481));
#25179=CARTESIAN_POINT('Ctrl Pts',(-5.97309921761341,-4.20513633432643,
-10.5778634093258));
#25180=CARTESIAN_POINT('Ctrl Pts',(-3.2502353630771,-6.54194433684208,-10.4198943824035));
#25181=CARTESIAN_POINT('Ctrl Pts',(0.256829418882314,-7.30035088692297,
-10.2619253554812));
#25182=CARTESIAN_POINT('Ctrl Pts',(3.70192706745187,-6.29736522276595,-10.1039563285589));
#25183=CARTESIAN_POINT('Ctrl Pts',(6.25384370141796,-3.77498573442189,-9.94598730163663));
#25184=CARTESIAN_POINT('Ctrl Pts',(7.29686584301275,-0.341797086983226,
-9.78801827471434));
#25185=CARTESIAN_POINT('Ctrl Pts',(6.57933890745369,3.1738582537474,-9.63004924779205));
#25186=CARTESIAN_POINT('Ctrl Pts',(4.27438385343404,5.92374202677216,-9.47208022086977));
#25187=CARTESIAN_POINT('Ctrl Pts',(0.938128110736348,7.24437659620591,-9.31411119394746));
#25188=CARTESIAN_POINT('Ctrl Pts',(-2.62447423026687,6.81712636270503,-9.15614216702519));
#25189=CARTESIAN_POINT('Ctrl Pts',(-5.55385731259764,4.74507593956608,-8.99817314010289));
#25190=CARTESIAN_POINT('Ctrl Pts',(-7.14323510016274,1.52815871821299,-8.8402041131806));
#25191=CARTESIAN_POINT('Ctrl Pts',(-7.00913092711596,-2.05746455634189,
-8.68223508625831));
#25192=CARTESIAN_POINT('Ctrl Pts',(-5.18390074123243,-5.14667366916295,
-8.52426605933603));
#25193=CARTESIAN_POINT('Ctrl Pts',(-2.10792642022479,-6.99412059972256,
-8.36629703241372));
#25194=CARTESIAN_POINT('Ctrl Pts',(1.47663723085556,-7.15406312813223,-8.20832800549144));
#25195=CARTESIAN_POINT('Ctrl Pts',(4.70492566621234,-5.58791116879607,-8.05035897856915));
#25196=CARTESIAN_POINT('Ctrl Pts',(6.7980345379359,-2.67353757689276,-7.89238995164686));
#25197=CARTESIAN_POINT('Ctrl Pts',(7.25094961548956,0.885893011560273,-7.73442092472457));
#25198=CARTESIAN_POINT('Ctrl Pts',(5.95439394599882,4.23158002289299,-7.57645189780228));
#25199=CARTESIAN_POINT('Ctrl Pts',(3.22119361930529,6.55629380223107,-7.41848287087999));
#25200=CARTESIAN_POINT('Ctrl Pts',(-0.289199255448484,7.29913971266049,
-7.2605138439577));
#25201=CARTESIAN_POINT('Ctrl Pts',(-3.72981566445424,6.28088782445941,-7.10254481703542));
#25202=CARTESIAN_POINT('Ctrl Pts',(-6.27052189027239,3.74721656404909,-6.94457579011312));
#25203=CARTESIAN_POINT('Ctrl Pts',(-7.29830978161512,0.309436723489391,
-6.78660676319084));
#25204=CARTESIAN_POINT('Ctrl Pts',(-6.56520011570507,-3.20300237199563,
-6.62863773626853));
#25205=CARTESIAN_POINT('Ctrl Pts',(-4.2480737126944,-5.94263800729771,-6.47066870934626));
#25206=CARTESIAN_POINT('Ctrl Pts',(-0.905994567535462,-7.24846539605864,
-6.31269968242396));
#25207=CARTESIAN_POINT('Ctrl Pts',(2.65467815183388,-6.80542141710856,-6.15473065550168));
#25208=CARTESIAN_POINT('Ctrl Pts',(5.57484417681311,-4.72040137684464,-5.99676162857937));
#25209=CARTESIAN_POINT('Ctrl Pts',(7.14994130409419,-1.49646787545602,-5.8387926016571));
#25210=CARTESIAN_POINT('Ctrl Pts',(6.99993843512708,2.08852547475353,-5.68082357473479));
#25211=CARTESIAN_POINT('Ctrl Pts',(5.16102746823472,5.16961045209313,-5.52285454781251));
#25212=CARTESIAN_POINT('Ctrl Pts',(2.07689110893385,7.00339918010501,-5.36488552089022));
#25213=CARTESIAN_POINT('Ctrl Pts',(-1.50834654502773,7.14744481995956,-5.20691649396793));
#25214=CARTESIAN_POINT('Ctrl Pts',(-4.7296583276429,5.56699280204512,-5.04894746704564));
#25215=CARTESIAN_POINT('Ctrl Pts',(-6.80982318103781,2.64336622458256,-4.89097844012335));
#25216=CARTESIAN_POINT('Ctrl Pts',(-7.2469499388148,-0.918037765332133,
-4.73300941320106));
#25217=CARTESIAN_POINT('Ctrl Pts',(-5.93557097038376,-4.25794246201161,
-4.57504038627877));
#25218=CARTESIAN_POINT('Ctrl Pts',(-3.19208885267558,-6.57051333693862,
-4.41707135935648));
#25219=CARTESIAN_POINT('Ctrl Pts',(0.321563569035109,-7.29778552886649,
-4.2591023324342));
#25220=CARTESIAN_POINT('Ctrl Pts',(3.75763083470845,-6.26428665246988,-4.1011333055119));
#25221=CARTESIAN_POINT('Ctrl Pts',(6.28707682012798,-3.71937384677495,-3.94316427858961));
#25222=CARTESIAN_POINT('Ctrl Pts',(7.29961018521532,-0.277070204396804,
-3.78519525166732));
#25223=CARTESIAN_POINT('Ctrl Pts',(6.55093223855146,3.23208347048326,-3.62722622474503));
#25224=CARTESIAN_POINT('Ctrl Pts',(4.22168003267289,5.96141715165068,-3.46925719782274));
#25225=CARTESIAN_POINT('Ctrl Pts',(0.87384321207103,7.25241165371776,-3.31128817090045));
#25226=CARTESIAN_POINT('Ctrl Pts',(-2.68482987385822,6.79358265591156,-3.15331914397816));
#25227=CARTESIAN_POINT('Ctrl Pts',(-5.59572141748757,4.69563399043567,-2.99535011705587));
#25228=CARTESIAN_POINT('Ctrl Pts',(-7.15650691328321,1.46474760774455,-2.83738109013358));
#25229=CARTESIAN_POINT('Ctrl Pts',(-6.99060829739456,-2.11954532545598,
-2.67941206321129));
#25230=CARTESIAN_POINT('Ctrl Pts',(-5.13805270983225,-5.19244558038399,
-2.521443036289));
#25231=CARTESIAN_POINT('Ctrl Pts',(-2.04581495797315,-7.01254004708689,
-2.36347400936671));
#25232=CARTESIAN_POINT('Ctrl Pts',(1.54002619931572,-7.14068596562577,-2.20550498244442));
#25233=CARTESIAN_POINT('Ctrl Pts',(4.75429798593852,-5.54596496699761,-2.04753595552213));
#25234=CARTESIAN_POINT('Ctrl Pts',(6.82147791699478,-2.61314289357019,-1.88956692859984));
#25235=CARTESIAN_POINT('Ctrl Pts',(7.24280775942499,0.95016446696199,-1.73159790167755));
#25236=CARTESIAN_POINT('Ctrl Pts',(5.9166312787675,4.2842211737227,-1.57362887475526));
#25237=CARTESIAN_POINT('Ctrl Pts',(3.16292131738634,6.5846036702513,-1.41565984783297));
#25238=CARTESIAN_POINT('Ctrl Pts',(-0.353921559454153,7.29628784273328,
-1.25769082091068));
#25239=CARTESIAN_POINT('Ctrl Pts',(-3.78537211558607,6.24756230067434,-1.09972179398839));
#25240=CARTESIAN_POINT('Ctrl Pts',(-6.30350812203686,3.69145799240344,-0.9417527670661));
#25241=CARTESIAN_POINT('Ctrl Pts',(-7.3007670505948,0.24469823704531,-0.783783740143811));
#25242=CARTESIAN_POINT('Ctrl Pts',(-6.53653554504556,-3.26110101386324,
-0.625814713221519));
#25243=CARTESIAN_POINT('Ctrl Pts',(-4.19520333829513,-5.98007907176997,
-0.46784568629923));
#25244=CARTESIAN_POINT('Ctrl Pts',(-0.841674673510988,-7.2562153012596,
-0.309876659376941));
#25245=CARTESIAN_POINT('Ctrl Pts',(2.71492880187119,-6.78161030692815,-0.151907632454651));
#25246=CARTESIAN_POINT('Ctrl Pts',(5.61648862490336,-4.67077426992517,0.00606139446763901));
#25247=CARTESIAN_POINT('Ctrl Pts',(7.16293179820857,-1.43299853749978,0.164030421389929));
#25248=CARTESIAN_POINT('Ctrl Pts',(6.98114069759885,2.15052349780071,0.32199944831222));
#25249=CARTESIAN_POINT('Ctrl Pts',(5.1149769176862,5.21517860535967,0.479968475234509));
#25250=CARTESIAN_POINT('Ctrl Pts',(2.01469857847539,7.0215430207436,0.637937502156801));
#25251=CARTESIAN_POINT('Ctrl Pts',(-1.57167557080576,7.13378669812858,0.795906529079091));
#25252=CARTESIAN_POINT('Ctrl Pts',(-4.77884415657439,5.52482807709332,0.953875556001379));
#25253=CARTESIAN_POINT('Ctrl Pts',(-6.83299851663795,2.58286817818632,1.11184458292367));
#25254=CARTESIAN_POINT('Ctrl Pts',(-7.23852315876716,-0.982272484728826,
1.26981360984596));
#25255=CARTESIAN_POINT('Ctrl Pts',(-5.89757524357886,-4.31041564127981,
1.42778263676825));
#25256=CARTESIAN_POINT('Ctrl Pts',(-3.13369158698168,-6.59856452510272,
1.58575166369054));
#25257=CARTESIAN_POINT('Ctrl Pts',(0.386272590423321,-7.29464668370932,
1.74372069061283));
#25258=CARTESIAN_POINT('Ctrl Pts',(3.81303896158782,-6.23071509793838,1.90168971753512));
#25259=CARTESIAN_POINT('Ctrl Pts',(6.31981547289674,-3.66346954986648,2.05965874445741));
#25260=CARTESIAN_POINT('Ctrl Pts',(7.30178035500521,-0.212321457991736,
2.2176277713797));
#25261=CARTESIAN_POINT('Ctrl Pts',(6.52201031828136,3.29005443153991,2.37559679830199));
#25262=CARTESIAN_POINT('Ctrl Pts',(4.16864415019414,5.99862340069086,2.53356582522428));
#25263=CARTESIAN_POINT('Ctrl Pts',(0.809489584411698,7.25987626388997,2.69153485214657));
#25264=CARTESIAN_POINT('Ctrl Pts',(-2.74497434401292,6.76950460558043,2.84950387906886));
#25265=CARTESIAN_POINT('Ctrl Pts',(-5.63714539069788,4.6458227041502,3.00747290599115));
#25266=CARTESIAN_POINT('Ctrl Pts',(-7.16921583253243,1.40122128902973,3.16544193291344));
#25267=CARTESIAN_POINT('Ctrl Pts',(-6.97153582190914,-2.18145938263847,
3.32341095983573));
#25268=CARTESIAN_POINT('Ctrl Pts',(-5.09180054555483,-5.23780908000201,
3.48137998675802));
#25269=CARTESIAN_POINT('Ctrl Pts',(-1.9835425823075,-7.03040792404231,3.63934901368031));
#25270=CARTESIAN_POINT('Ctrl Pts',(1.60329403715025,-7.12674715313392,3.7973180406026));
#25271=CARTESIAN_POINT('Ctrl Pts',(4.80329635687901,-5.50358254796425,3.95528706752489));
#25272=CARTESIAN_POINT('Ctrl Pts',(6.8443847534283,-2.55254267374754,4.11325609444718));
#25273=CARTESIAN_POINT('Ctrl Pts',(7.23409622109297,1.01436118726632,4.27122512136948));
#25274=CARTESIAN_POINT('Ctrl Pts',(5.87840323953227,4.33652534959965,4.42919414829176));
#25275=CARTESIAN_POINT('Ctrl Pts',(3.1044002362298,6.61239562696911,4.58716317521405));
#25276=CARTESIAN_POINT('Ctrl Pts',(-0.418616025797768,7.29286208406613,
4.74513220213634));
#25277=CARTESIAN_POINT('Ctrl Pts',(-3.84063082867778,6.21374537554234,4.90310122905863));
#25278=CARTESIAN_POINT('Ctrl Pts',(-6.33599855204275,3.6354090695238,5.06107025598092));
#25279=CARTESIAN_POINT('Ctrl Pts',(-7.30265007852114,0.179940503887283,
5.21903928290322));
#25280=CARTESIAN_POINT('Ctrl Pts',(-6.50735684388029,-3.31894315417848,
5.37700830982549));
#25281=CARTESIAN_POINT('Ctrl Pts',(-4.14200299062497,-6.01704977376103,
5.53497733674779));
#25282=CARTESIAN_POINT('Ctrl Pts',(-0.777288577654901,-7.26339446962033,
5.69294636367007));
#25283=CARTESIAN_POINT('Ctrl Pts',(2.77496590947331,-6.75726578991273,5.85091539059238));
#25284=CARTESIAN_POINT('Ctrl Pts',(5.65769130868017,-4.62077978375391,6.00888441751465));
#25285=CARTESIAN_POINT('Ctrl Pts',(7.17535889268669,-1.3694164871965,6.16685344443696));
#25286=CARTESIAN_POINT('Ctrl Pts',(6.96179385919402,2.2123523716516,6.32482247135923));
#25287=CARTESIAN_POINT('Ctrl Pts',(5.0685240491741,5.26033655930945,6.48279149828153));
#25288=CARTESIAN_POINT('Ctrl Pts',(1.95234758211533,7.03913458266513,6.64076052520383));
#25289=CARTESIAN_POINT('Ctrl Pts',(-1.63488097660941,7.11956746906613,6.7987295521261));
#25290=CARTESIAN_POINT('Ctrl Pts',(-4.82765410602868,5.48222879737866,6.95669857904841));
#25291=CARTESIAN_POINT('Ctrl Pts',(-6.85563640346892,2.52216697656922,7.11466760597069));
#25292=CARTESIAN_POINT('Ctrl Pts',(-7.22952703345286,-1.04642994358814,
7.27263663289298));
#25293=CARTESIAN_POINT('Ctrl Pts',(-5.85911564362261,-4.36254978526544,
7.43060565981527));
#25294=CARTESIAN_POINT('Ctrl Pts',(-3.07504784111029,-6.6260967038787,7.58857468673756));
#25295=CARTESIAN_POINT('Ctrl Pts',(0.450951229581866,-7.29093407889477,
7.74654371365985));
#25296=CARTESIAN_POINT('Ctrl Pts',(3.86814717429503,-6.19665346717748,7.90451274058214));
#25297=CARTESIAN_POINT('Ctrl Pts',(6.3520570412528,-3.60727710314822,8.06248176750443));
#25298=CARTESIAN_POINT('Ctrl Pts',(7.30337620404243,-0.147556011471691,
8.22045079442672));
#25299=CARTESIAN_POINT('Ctrl Pts',(6.49257540998184,3.34776661372899,8.37841982134901));
#25300=CARTESIAN_POINT('Ctrl Pts',(4.11528038346205,6.03535782862288,8.5363888482713));
#25301=CARTESIAN_POINT('Ctrl Pts',(0.745072286421063,7.26676984931728,8.69435787519359));
#25302=CARTESIAN_POINT('Ctrl Pts',(-2.8049029084755,6.74489410049378,8.85232690211588));
#25303=CARTESIAN_POINT('Ctrl Pts',(-5.67812597489344,4.59564600135665,9.01029592903816));
#25304=CARTESIAN_POINT('Ctrl Pts',(-7.18136085776966,1.3375847570525,9.16826495596046));
#25305=CARTESIAN_POINT('Ctrl Pts',(-6.95191500122292,-2.24320185668345,
9.32623398288275));
#25306=CARTESIAN_POINT('Ctrl Pts',(-5.04514788584998,-5.28276060163157,
9.48420300980505));
#25307=CARTESIAN_POINT('Ctrl Pts',(-1.92111419208628,-7.04772282243763,
9.64217203672733));
#25308=CARTESIAN_POINT('Ctrl Pts',(1.66643576956794,-7.11224779210674,9.80014106364964));
#25309=CARTESIAN_POINT('Ctrl Pts',(4.8519169221348,-5.46076723551842,9.95811009057189));
#25310=CARTESIAN_POINT('Ctrl Pts',(6.86675325118528,-2.49174170282171,10.1160791174942));
#25311=CARTESIAN_POINT('Ctrl Pts',(7.22481567467034,1.07847815974748,10.2740481444165));
#25312=CARTESIAN_POINT('Ctrl Pts',(5.83971285652996,4.38848836535715,10.4320171713388));
#25313=CARTESIAN_POINT('Ctrl Pts',(3.04563493721469,6.63966762466851,10.5899861982611));
#25314=CARTESIAN_POINT('Ctrl Pts',(-0.483277485164237,7.28886243758024,
10.7479552251834));
#25315=CARTESIAN_POINT('Ctrl Pts',(-3.89558761425688,6.17944023049411,10.9059242521057));
#25316=CARTESIAN_POINT('Ctrl Pts',(-6.36799032002207,3.57907319090321,11.063893279028));
#25317=CARTESIAN_POINT('Ctrl Pts',(-7.30395930917253,0.115170585126009,
11.2218623059502));
#25318=CARTESIAN_POINT('Ctrl Pts',(-6.47766515763742,-3.37652806502809,
11.3798313328725));
#25319=CARTESIAN_POINT('Ctrl Pts',(-4.08847908705193,-6.05353978254256,
11.5378003597948));
#25320=CARTESIAN_POINT('Ctrl Pts',(-0.712837007271165,-7.27001675403624,
11.6957693867171));
#25321=CARTESIAN_POINT('Ctrl Pts',(2.83477632842898,-6.73236177450462,11.8537384136394));
#25322=CARTESIAN_POINT('Ctrl Pts',(5.69846535245322,-4.57047627984927,12.0117074405617));
#25323=CARTESIAN_POINT('Ctrl Pts',(7.18718979160324,-1.3056206783609,12.169676467484));
#25324=CARTESIAN_POINT('Ctrl Pts',(6.94196157239741,2.27379792622975,12.3276454944063));
#25325=CARTESIAN_POINT('Ctrl Pts',(5.02154850583196,5.30552096540472,12.4856145213286));
#25326=CARTESIAN_POINT('Ctrl Pts',(2.93392826290545,6.47182695586933,12.5909272059434));
#25327=CARTESIAN_POINT('Ctrl Pts',(1.81369530454163,6.7718570992692,12.6435835482508));
#25328=CARTESIAN_POINT('Ctrl Pts',(5.59099055985781,-4.82066492452619,-12.214237887564));
#25329=CARTESIAN_POINT('Ctrl Pts',(6.38858306760391,-3.89562284786681,-12.1615727312903));
#25330=CARTESIAN_POINT('Ctrl Pts',(7.51496659875801,-1.64319883160089,-12.0562512327092));
#25331=CARTESIAN_POINT('Ctrl Pts',(7.39026608617398,2.13403331859815,-11.8982733918206));
#25332=CARTESIAN_POINT('Ctrl Pts',(5.48279926871797,5.39521343061514,-11.7403043648983));
#25333=CARTESIAN_POINT('Ctrl Pts',(2.25232191904217,7.35513660683255,-11.582335337976));
#25334=CARTESIAN_POINT('Ctrl Pts',(-1.52150767515003,7.54021042830991,-11.4243663110537));
#25335=CARTESIAN_POINT('Ctrl Pts',(-4.92827501218454,5.90614603795184,-11.2663972841314));
#25336=CARTESIAN_POINT('Ctrl Pts',(-7.14595413632915,2.8470142422763,-11.1084282572091));
#25337=CARTESIAN_POINT('Ctrl Pts',(-7.63950561518693,-0.898997262557083,
-10.9504592302869));
#25338=CARTESIAN_POINT('Ctrl Pts',(-6.28983228413006,-4.42812036284623,
-10.7924902033646));
#25339=CARTESIAN_POINT('Ctrl Pts',(-3.42258425197763,-6.88884131867677,
-10.6345211764423));
#25340=CARTESIAN_POINT('Ctrl Pts',(0.270448206458184,-7.68746357981854,
-10.47655214952));
#25341=CARTESIAN_POINT('Ctrl Pts',(3.89822762590192,-6.63129300888081,-10.3185831225977));
#25342=CARTESIAN_POINT('Ctrl Pts',(6.58546368978599,-3.97516034464673,-10.1606140956754));
#25343=CARTESIAN_POINT('Ctrl Pts',(7.68379373592351,-0.359921420020828,
-10.0026450687531));
#25344=CARTESIAN_POINT('Ctrl Pts',(6.92821879574774,3.34215712519999,-9.84467604183086));
#25345=CARTESIAN_POINT('Ctrl Pts',(4.50103984156416,6.23785784990473,-9.68670701490859));
#25346=CARTESIAN_POINT('Ctrl Pts',(0.987873842805025,7.6285211634938,-9.52873798798628));
#25347=CARTESIAN_POINT('Ctrl Pts',(-2.76364114189211,7.17861530823001,-9.37076896106401));
#25348=CARTESIAN_POINT('Ctrl Pts',(-5.84835941168012,4.99669112264581,-9.2127999341417));
#25349=CARTESIAN_POINT('Ctrl Pts',(-7.52201647909117,1.60919175973965,-9.05483090721943));
#25350=CARTESIAN_POINT('Ctrl Pts',(-7.38080121941844,-2.16656488004954,
-8.89686188029712));
#25351=CARTESIAN_POINT('Ctrl Pts',(-5.45878530592322,-5.41958420927045,
-8.73889285337486));
#25352=CARTESIAN_POINT('Ctrl Pts',(-2.21970256435789,-7.36499494559062,
-8.58092382645254));
#25353=CARTESIAN_POINT('Ctrl Pts',(1.5549382637402,-7.53341868043001,-8.42295479953027));
#25354=CARTESIAN_POINT('Ctrl Pts',(4.95441181732098,-5.88421902765374,-8.26498577260798));
#25355=CARTESIAN_POINT('Ctrl Pts',(7.15851110914994,-2.81530615034617,-8.10701674568568));
#25356=CARTESIAN_POINT('Ctrl Pts',(7.63544272755767,0.932868894587585,-7.94904771876339));
#25357=CARTESIAN_POINT('Ctrl Pts',(6.27013513579911,4.45596626997045,-7.7910786918411));
#25358=CARTESIAN_POINT('Ctrl Pts',(3.39200252364726,6.90395168724349,-7.63310966491881));
#25359=CARTESIAN_POINT('Ctrl Pts',(-0.304534504985681,7.68618818111842,
-7.47514063799653));
#25360=CARTESIAN_POINT('Ctrl Pts',(-3.92759506002511,6.61394187037614,-7.31717161107423));
#25361=CARTESIAN_POINT('Ctrl Pts',(-6.60302626607604,3.94591866993969,-7.15920258415194));
#25362=CARTESIAN_POINT('Ctrl Pts',(-7.6853142416621,0.325845096890364,-7.00123355722965));
#25363=CARTESIAN_POINT('Ctrl Pts',(-6.91333027212556,-3.37284665657586,
-6.84326453030737));
#25364=CARTESIAN_POINT('Ctrl Pts',(-4.47333456385235,-6.25775581978934,
-6.68529550338507));
#25365=CARTESIAN_POINT('Ctrl Pts',(-0.954036367473559,-7.63282677844849,
-6.52732647646279));
#25366=CARTESIAN_POINT('Ctrl Pts',(2.79544667433989,-7.16628968931519,-6.36935744954049));
#25367=CARTESIAN_POINT('Ctrl Pts',(5.87045913768095,-4.9707081520726,-6.2113884226182));
#25368=CARTESIAN_POINT('Ctrl Pts',(7.52907829013018,-1.57582045974579,-6.05341939569592));
#25369=CARTESIAN_POINT('Ctrl Pts',(7.37112128095155,2.19927285295983,-5.89545036877362));
#25370=CARTESIAN_POINT('Ctrl Pts',(5.43469914132034,5.44373725152078,-5.73748134185133));
#25371=CARTESIAN_POINT('Ctrl Pts',(2.1870215564265,7.37476553742481,-5.57951231492904));
#25372=CARTESIAN_POINT('Ctrl Pts',(-1.58832901462538,7.5264494259619,-5.42154328800675));
#25373=CARTESIAN_POINT('Ctrl Pts',(-4.98045596737956,5.86219143130419,-5.26357426108446));
#25374=CARTESIAN_POINT('Ctrl Pts',(-7.17092486376328,2.78353491419177,-5.10560523416217));
#25375=CARTESIAN_POINT('Ctrl Pts',(-7.63123096167894,-0.966718174948357,
-4.94763620723988));
#25376=CARTESIAN_POINT('Ctrl Pts',(-6.25031404202623,-4.48372661926579,
-4.78966718031759));
#25377=CARTESIAN_POINT('Ctrl Pts',(-3.36135443057194,-6.91892523534814,
-4.6316981533953));
#25378=CARTESIAN_POINT('Ctrl Pts',(0.338614987668868,-7.6847621895794,-4.47372912647301));
#25379=CARTESIAN_POINT('Ctrl Pts',(3.95688517383029,-6.59646039489246,-4.31576009955072));
#25380=CARTESIAN_POINT('Ctrl Pts',(6.62045904736319,-3.91659954839013,-4.15779107262843));
#25381=CARTESIAN_POINT('Ctrl Pts',(7.68668360122721,-0.291762291750758,
-3.99982204570614));
#25382=CARTESIAN_POINT('Ctrl Pts',(6.8983058181399,3.40346982646831,-3.84185301878385));
#25383=CARTESIAN_POINT('Ctrl Pts',(4.44554131705566,6.27753075807789,-3.68388399186156));
#25384=CARTESIAN_POINT('Ctrl Pts',(0.920180135354985,7.63698229268348,-3.52591496493927));
#25385=CARTESIAN_POINT('Ctrl Pts',(-2.82719723928136,7.15382315901524,-3.36794593801698));
#25386=CARTESIAN_POINT('Ctrl Pts',(-5.89244342717854,4.9446274356885,-3.20997691109469));
#25387=CARTESIAN_POINT('Ctrl Pts',(-7.53599205116739,1.54241817449251,-3.0520078841724));
#25388=CARTESIAN_POINT('Ctrl Pts',(-7.36129639785696,-2.23193758048048,
-2.89403885725011));
#25389=CARTESIAN_POINT('Ctrl Pts',(-5.41050610988806,-5.46778324873317,
-2.73606983032782));
#25390=CARTESIAN_POINT('Ctrl Pts',(-2.15429754323705,-7.38439111338679,
-2.57810080340553));
#25391=CARTESIAN_POINT('Ctrl Pts',(1.62168853286391,-7.51933217264942,-2.42013177648324));
#25392=CARTESIAN_POINT('Ctrl Pts',(5.00640218266438,-5.84004856192791,-2.26216274956095));
#25393=CARTESIAN_POINT('Ctrl Pts',(7.18319761059275,-2.751708943082,-2.10419372263866));
#25394=CARTESIAN_POINT('Ctrl Pts',(7.62686913665253,1.00054844592363,-1.94622469571637));
#25395=CARTESIAN_POINT('Ctrl Pts',(6.23037004320095,4.51139880137492,-1.78825566879408));
#25396=CARTESIAN_POINT('Ctrl Pts',(3.33064024042927,6.93376273094893,-1.63028664187179));
#25397=CARTESIAN_POINT('Ctrl Pts',(-0.372688811888484,7.68318508626183,
-1.4723176149495));
#25398=CARTESIAN_POINT('Ctrl Pts',(-3.98609748015743,6.57884920779809,-1.31434858802721));
#25399=CARTESIAN_POINT('Ctrl Pts',(-6.63776164513556,3.88720341153253,-1.15637956110492));
#25400=CARTESIAN_POINT('Ctrl Pts',(-7.68790181122962,0.257673749449668,
-0.998410534182634));
#25401=CARTESIAN_POINT('Ctrl Pts',(-6.88314571711041,-3.43402607114267,
-0.840441507260343));
#25402=CARTESIAN_POINT('Ctrl Pts',(-4.41766065393471,-6.29718225613171,
-0.682472480338053));
#25403=CARTESIAN_POINT('Ctrl Pts',(-0.886305808979903,-7.64098763467338,
-0.524503453415764));
#25404=CARTESIAN_POINT('Ctrl Pts',(2.85889221072524,-7.14121595722447,-0.366534426493473));
#25405=CARTESIAN_POINT('Ctrl Pts',(5.91431184872925,-4.91844948904059,-0.208565399571184));
#25406=CARTESIAN_POINT('Ctrl Pts',(7.54275762581348,-1.50898555940589,-0.050596372648894));
#25407=CARTESIAN_POINT('Ctrl Pts',(7.35132676355511,2.26455841958236,0.107372654273397));
#25408=CARTESIAN_POINT('Ctrl Pts',(5.38620668723756,5.49172172844002,0.265341681195686));
#25409=CARTESIAN_POINT('Ctrl Pts',(2.1215311683285,7.39387148401118,0.423310708117978));
#25410=CARTESIAN_POINT('Ctrl Pts',(-1.6550161625111,7.51206706054266,0.581279735040268));
#25411=CARTESIAN_POINT('Ctrl Pts',(-5.0322499529579,5.81779085488797,0.739248761962557));
#25412=CARTESIAN_POINT('Ctrl Pts',(-7.1953291083175,2.71982886286287,0.897217788884847));
#25413=CARTESIAN_POINT('Ctrl Pts',(-7.62235733824431,-1.03435904229439,
1.05518681580714));
#25414=CARTESIAN_POINT('Ctrl Pts',(-6.21030353150069,-4.53898227215012,
1.21315584272943));
#25415=CARTESIAN_POINT('Ctrl Pts',(-3.29986055717648,-6.9484638822875,1.37112486965172));
#25416=CARTESIAN_POINT('Ctrl Pts',(0.40675530762235,-7.68145690217578,1.52909389657401));
#25417=CARTESIAN_POINT('Ctrl Pts',(4.01523140458121,-6.56110865539718,1.6870629234963));
#25418=CARTESIAN_POINT('Ctrl Pts',(6.65493371915781,-3.8577308374068,1.84503195041859));
#25419=CARTESIAN_POINT('Ctrl Pts',(7.68896884771471,-0.223580140298352,
2.00300097734088));
#25420=CARTESIAN_POINT('Ctrl Pts',(6.8678502671426,3.46451478974651,2.16097000426317));
#25421=CARTESIAN_POINT('Ctrl Pts',(4.38969312272992,6.31670992752719,2.31893903118546));
#25422=CARTESIAN_POINT('Ctrl Pts',(0.852414054446948,7.64484272565788,2.47690805810775));
#25423=CARTESIAN_POINT('Ctrl Pts',(-2.89053096542732,7.12846833184862,2.63487708503004));
#25424=CARTESIAN_POINT('Ctrl Pts',(-5.93606397231646,4.89217482688728,2.79284611195233));
#25425=CARTESIAN_POINT('Ctrl Pts',(-7.54937488103139,1.47552327189886,2.95081513887462));
#25426=CARTESIAN_POINT('Ctrl Pts',(-7.3412125740871,-2.29713472881507,3.10878416579691));
#25427=CARTESIAN_POINT('Ctrl Pts',(-5.36180135118839,-5.51555221991937,
3.2667531927192));
#25428=CARTESIAN_POINT('Ctrl Pts',(-2.08872307601302,-7.40320646287767,
3.42472221964149));
#25429=CARTESIAN_POINT('Ctrl Pts',(1.68831124821834,-7.50465423250149,3.58269124656378));
#25430=CARTESIAN_POINT('Ctrl Pts',(5.05799876999421,-5.79541874785593,3.74066027348607));
#25431=CARTESIAN_POINT('Ctrl Pts',(7.20731911838588,-2.68789530041857,3.89862930040836));
#25432=CARTESIAN_POINT('Ctrl Pts',(7.6176956551735,1.06814929921513,4.05659832733065));
#25433=CARTESIAN_POINT('Ctrl Pts',(6.19011490150972,4.56647648919493,4.21456735425294));
#25434=CARTESIAN_POINT('Ctrl Pts',(3.26901598605976,6.96302840028308,4.37253638117523));
#25435=CARTESIAN_POINT('Ctrl Pts',(-0.440813804993028,7.67957767130397,
4.53050540809751));
#25436=CARTESIAN_POINT('Ctrl Pts',(-4.04428637421744,6.54323908653675,4.68847443501981));
#25437=CARTESIAN_POINT('Ctrl Pts',(-6.67197493176133,3.82818240555635,4.84644346194209));
#25438=CARTESIAN_POINT('Ctrl Pts',(-7.68988468970048,0.189482134707461,
5.0044124888644));
#25439=CARTESIAN_POINT('Ctrl Pts',(-6.85241976900343,-3.49493538275516,
5.16238151578668));
#25440=CARTESIAN_POINT('Ctrl Pts',(-4.36163927338976,-6.33611338827574,
5.32035054270897));
#25441=CARTESIAN_POINT('Ctrl Pts',(-0.818505538197435,-7.6485474898312,
5.47831956963126));
#25442=CARTESIAN_POINT('Ctrl Pts',(2.92211288124885,-7.1155805335547,5.63628859655355));
#25443=CARTESIAN_POINT('Ctrl Pts',(5.95769937021023,-4.86580396588883,5.79425762347584));
#25444=CARTESIAN_POINT('Ctrl Pts',(7.5558436867006,-1.44203196996787,5.95222665039812));
#25445=CARTESIAN_POINT('Ctrl Pts',(7.33095402833655,2.32966586760398,6.11019567732041));
#25446=CARTESIAN_POINT('Ctrl Pts',(5.33729058164263,5.5392742545727,6.26816470424272));
#25447=CARTESIAN_POINT('Ctrl Pts',(2.05587391142296,7.41239586642492,6.42613373116499));
#25448=CARTESIAN_POINT('Ctrl Pts',(-1.7215731352771,7.49709383429043,6.58410275808729));
#25449=CARTESIAN_POINT('Ctrl Pts',(-5.08364812745316,5.77293268075287,6.74207178500957));
#25450=CARTESIAN_POINT('Ctrl Pts',(-7.21916740502853,2.65590888368507,6.90004081193188));
#25451=CARTESIAN_POINT('Ctrl Pts',(-7.61288417910656,-1.10191855224044,
7.05800983885415));
#25452=CARTESIAN_POINT('Ctrl Pts',(-6.16980455021368,-4.59388091186788,
7.21597886577645));
#25453=CARTESIAN_POINT('Ctrl Pts',(-3.2381071336009,-6.97745599854215,7.37394789269874));
#25454=CARTESIAN_POINT('Ctrl Pts',(0.474863634280211,-7.67754743059828,
7.53191691962102));
#25455=CARTESIAN_POINT('Ctrl Pts',(4.07326181773498,-6.52524085260257,7.68988594654333));
#25456=CARTESIAN_POINT('Ctrl Pts',(6.68888494784978,-3.79855869701265,7.84785497346561));
#25457=CARTESIAN_POINT('Ctrl Pts',(7.69064931918003,-0.155380403180869,
8.00582400038789));
#25458=CARTESIAN_POINT('Ctrl Pts',(6.83685452611142,3.52528725199694,8.1637930273102));
#25459=CARTESIAN_POINT('Ctrl Pts',(4.3334996575679,6.35539225680518,8.32176205423247));
#25460=CARTESIAN_POINT('Ctrl Pts',(0.784580926987224,7.65210185439399,8.47973108115477));
#25461=CARTESIAN_POINT('Ctrl Pts',(-2.95363733713913,7.10255281566796,8.63770010807706));
#25462=CARTESIAN_POINT('Ctrl Pts',(-5.97921761703337,4.83933742478764,8.79566913499935));
#25463=CARTESIAN_POINT('Ctrl Pts',(-7.5621639155084,1.40851231180965,8.95363816192163));
#25464=CARTESIAN_POINT('Ctrl Pts',(-7.32055132824183,-2.36215119554395,
9.11160718884394));
#25465=CARTESIAN_POINT('Ctrl Pts',(-5.3126748601556,-5.56288736733038,9.26957621576621));
#25466=CARTESIAN_POINT('Ctrl Pts',(-2.02298432131397,-7.4214395112426,9.42754524268851));
#25467=CARTESIAN_POINT('Ctrl Pts',(1.75480117121603,-7.48938601984247,9.5855142696108));
#25468=CARTESIAN_POINT('Ctrl Pts',(5.10919751789325,-5.75033308551119,9.74348329653307));
#25469=CARTESIAN_POINT('Ctrl Pts',(7.23087374123971,-2.62387026150611,9.90145232345539));
#25470=CARTESIAN_POINT('Ctrl Pts',(7.60792299304672,1.13566617592857,10.0594213503777));
#25471=CARTESIAN_POINT('Ctrl Pts',(6.14937289953934,4.62119492633867,10.2173903773));
#25472=CARTESIAN_POINT('Ctrl Pts',(3.20713456379208,6.99174653894661,10.3753594042223));
#25473=CARTESIAN_POINT('Ctrl Pts',(-0.508904040873067,7.67536593721493,
10.5333284311446));
#25474=CARTESIAN_POINT('Ctrl Pts',(-4.10215733057928,6.50711485672321,10.6912974580669));
#25475=CARTESIAN_POINT('Ctrl Pts',(-6.70566311401509,3.7688592275556,10.8492664849892));
#25476=CARTESIAN_POINT('Ctrl Pts',(-7.69126334438516,0.121277688201066,
11.0072355119115));
#25477=CARTESIAN_POINT('Ctrl Pts',(-6.82115363397089,-3.55557382490135,
11.1652045388337));
#25478=CARTESIAN_POINT('Ctrl Pts',(-4.30527717987661,-6.37453833768985,
11.323173565756));
#25479=CARTESIAN_POINT('Ctrl Pts',(-0.750636320996575,-7.65552093138916,
11.4811425926783));
#25480=CARTESIAN_POINT('Ctrl Pts',(2.98509484260074,-7.08935594320191,11.6391116196006));
#25481=CARTESIAN_POINT('Ctrl Pts',(6.00063552237091,-4.81283303884795,11.7970806465229));
#25482=CARTESIAN_POINT('Ctrl Pts',(7.56830193781019,-1.37485328711205,11.9550496734452));
#25483=CARTESIAN_POINT('Ctrl Pts',(7.31007010305476,2.39436967024001,12.1130187003675));
#25484=CARTESIAN_POINT('Ctrl Pts',(5.28782408555519,5.58685463551785,12.2709877272898));
#25485=CARTESIAN_POINT('Ctrl Pts',(3.08950446577676,6.81500585228764,12.3763004119046));
#25486=CARTESIAN_POINT('Ctrl Pts',(1.90986937676202,7.13094557024913,12.4289567542121));
#25487=CARTESIAN_POINT('Ctrl Pts',(5.87253250007098,-5.06341606878912,-12.4288646816028));
#25488=CARTESIAN_POINT('Ctrl Pts',(6.71028886424398,-4.09179223917321,-12.376199525329));
#25489=CARTESIAN_POINT('Ctrl Pts',(7.89339297136583,-1.72594434552226,-12.270878026748));
#25490=CARTESIAN_POINT('Ctrl Pts',(7.76241299472572,2.24149547124628,-12.1129001858595));
#25491=CARTESIAN_POINT('Ctrl Pts',(5.75889308919358,5.66689674698945,-11.9549311589372));
#25492=CARTESIAN_POINT('Ctrl Pts',(2.36574065518254,7.72551452263309,-11.7969621320149));
#25493=CARTESIAN_POINT('Ctrl Pts',(-1.59812526523981,7.91990798831724,-11.6389931050926));
#25494=CARTESIAN_POINT('Ctrl Pts',(-5.17644500889257,6.20355806126057,-11.4810240781703));
#25495=CARTESIAN_POINT('Ctrl Pts',(-7.505798384084,2.99037951986057,-11.323055051248));
#25496=CARTESIAN_POINT('Ctrl Pts',(-8.02420331949211,-0.944267493446741,
-11.1650860243257));
#25497=CARTESIAN_POINT('Ctrl Pts',(-6.60656535064672,-4.65110439136602,
-11.0071169974035));
#25498=CARTESIAN_POINT('Ctrl Pts',(-3.59493314087816,-7.23573830051147,
-10.8491479704812));
#25499=CARTESIAN_POINT('Ctrl Pts',(0.28406699403406,-8.07457627271411,-10.6911789435589));
#25500=CARTESIAN_POINT('Ctrl Pts',(4.09452818435197,-6.96522079499565,-10.5332099166366));
#25501=CARTESIAN_POINT('Ctrl Pts',(6.91708367815401,-4.17533495487158,-10.3752408897143));
#25502=CARTESIAN_POINT('Ctrl Pts',(8.07072162883429,-0.378045753058428,
-10.217271862792));
#25503=CARTESIAN_POINT('Ctrl Pts',(7.27709868404176,3.51045599665256,-10.0593028358697));
#25504=CARTESIAN_POINT('Ctrl Pts',(4.7276958296943,6.5519736730373,-9.90133380894741));
#25505=CARTESIAN_POINT('Ctrl Pts',(1.0376195748737,8.01266573078172,-9.7433647820251));
#25506=CARTESIAN_POINT('Ctrl Pts',(-2.90280805351734,7.54010425375498,-9.58539575510284));
#25507=CARTESIAN_POINT('Ctrl Pts',(-6.1428615107626,5.24830630572554,-9.42742672818051));
#25508=CARTESIAN_POINT('Ctrl Pts',(-7.90079785801961,1.69022480126632,-9.26945770125828));
#25509=CARTESIAN_POINT('Ctrl Pts',(-7.75247151172096,-2.27566520375718,
-9.11148867433593));
#25510=CARTESIAN_POINT('Ctrl Pts',(-5.733669870614,-5.69249474937794,-8.95351964741368));
#25511=CARTESIAN_POINT('Ctrl Pts',(-2.33147870849099,-7.7358692914587,-8.79555062049136));
#25512=CARTESIAN_POINT('Ctrl Pts',(1.63323929662484,-7.91277423272776,-8.63758159356908));
#25513=CARTESIAN_POINT('Ctrl Pts',(5.20389796842962,-6.18052688651141,-8.47961256664679));
#25514=CARTESIAN_POINT('Ctrl Pts',(7.518987680364,-2.95707472379959,-8.3216435397245));
#25515=CARTESIAN_POINT('Ctrl Pts',(8.01993583962579,0.9798447776149,-8.16367451280222));
#25516=CARTESIAN_POINT('Ctrl Pts',(6.5858763255994,4.68035251704791,-8.00570548587992));
#25517=CARTESIAN_POINT('Ctrl Pts',(3.56281142798924,7.2516095722559,-7.84773645895763));
#25518=CARTESIAN_POINT('Ctrl Pts',(-0.319869754522884,8.07323664957635,
-7.68976743203535));
#25519=CARTESIAN_POINT('Ctrl Pts',(-4.12537445559599,6.94699591629286,-7.53179840511305));
#25520=CARTESIAN_POINT('Ctrl Pts',(-6.9355306418797,4.1446207758303,-7.37382937819076));
#25521=CARTESIAN_POINT('Ctrl Pts',(-8.07231870170907,0.342253470291336,
-7.21586035126847));
#25522=CARTESIAN_POINT('Ctrl Pts',(-7.26146042854604,-3.5426909411561,-7.05789132434619));
#25523=CARTESIAN_POINT('Ctrl Pts',(-4.69859541501031,-6.57287363228098,
-6.8999222974239));
#25524=CARTESIAN_POINT('Ctrl Pts',(-1.00207816741164,-8.01718816083833,
-6.7419532705016));
#25525=CARTESIAN_POINT('Ctrl Pts',(2.93621519684588,-7.52715796152183,-6.58398424357932));
#25526=CARTESIAN_POINT('Ctrl Pts',(6.16607409854881,-5.22101492730056,-6.42601521665703));
#25527=CARTESIAN_POINT('Ctrl Pts',(7.90821527616617,-1.65517304403557,-6.26804618973472));
#25528=CARTESIAN_POINT('Ctrl Pts',(7.74230412677602,2.31002023116615,-6.11007716281246));
#25529=CARTESIAN_POINT('Ctrl Pts',(5.70837081440596,5.7178640509484,-5.95210813589015));
#25530=CARTESIAN_POINT('Ctrl Pts',(2.29715200391916,7.74613189474464,-5.79413910896788));
#25531=CARTESIAN_POINT('Ctrl Pts',(-1.66831148422301,7.90545403196422,-5.63617008204558));
#25532=CARTESIAN_POINT('Ctrl Pts',(-5.23125360711624,6.15739006056327,-5.4782010551233));
#25533=CARTESIAN_POINT('Ctrl Pts',(-7.53202654648873,2.92370360380095,-5.32023202820099));
#25534=CARTESIAN_POINT('Ctrl Pts',(-8.0155119845431,-1.01539858456457,-5.16226300127872));
#25535=CARTESIAN_POINT('Ctrl Pts',(-6.56505711366871,-4.70951077651998,
-5.00429397435641));
#25536=CARTESIAN_POINT('Ctrl Pts',(-3.5306200084683,-7.26733713375767,-4.84632494743412));
#25537=CARTESIAN_POINT('Ctrl Pts',(0.355666406302637,-8.07173885029227,
-4.68835592051184));
#25538=CARTESIAN_POINT('Ctrl Pts',(4.15613951295213,-6.92863413731507,-4.53038689358954));
#25539=CARTESIAN_POINT('Ctrl Pts',(6.95384127459843,-4.11382525000531,-4.37241786666726));
#25540=CARTESIAN_POINT('Ctrl Pts',(8.07375701723909,-0.30645437910471,-4.21444883974496));
#25541=CARTESIAN_POINT('Ctrl Pts',(7.24567939772833,3.57485618245337,-4.05647981282269));
#25542=CARTESIAN_POINT('Ctrl Pts',(4.66940260143842,6.59364436450509,-3.89851078590038));
#25543=CARTESIAN_POINT('Ctrl Pts',(0.966517058638944,8.0215529316492,-3.7405417589781));
#25544=CARTESIAN_POINT('Ctrl Pts',(-2.9695646047045,7.51406366211892,-3.5825727320558));
#25545=CARTESIAN_POINT('Ctrl Pts',(-6.18916543686952,5.19362088094133,-3.42460370513352));
#25546=CARTESIAN_POINT('Ctrl Pts',(-7.91547718905155,1.62008874124048,-3.26663467821122));
#25547=CARTESIAN_POINT('Ctrl Pts',(-7.73198449831937,-2.344329835505,-3.10866565128894));
#25548=CARTESIAN_POINT('Ctrl Pts',(-5.68295950994386,-5.74312091708233,
-2.95069662436664));
#25549=CARTESIAN_POINT('Ctrl Pts',(-2.26278012850095,-7.75624217968669,
-2.79272759744436));
#25550=CARTESIAN_POINT('Ctrl Pts',(1.70335086641213,-7.89797837967305,-2.63475857052206));
#25551=CARTESIAN_POINT('Ctrl Pts',(5.25850637939024,-6.13413215685821,-2.47678954359978));
#25552=CARTESIAN_POINT('Ctrl Pts',(7.54491730419073,-2.89027499259379,-2.31882051667748));
#25553=CARTESIAN_POINT('Ctrl Pts',(8.01093051388007,1.05093242488527,-2.1608514897552));
#25554=CARTESIAN_POINT('Ctrl Pts',(6.5441088076344,4.73857642902715,-2.0028824628329));
#25555=CARTESIAN_POINT('Ctrl Pts',(3.49835916347221,7.28292179164652,-1.84491343591062));
#25556=CARTESIAN_POINT('Ctrl Pts',(-0.391456064322818,8.07008232979038,
-1.68694440898833));
#25557=CARTESIAN_POINT('Ctrl Pts',(-4.18682284472876,6.91013611492184,-1.52897538206604));
#25558=CARTESIAN_POINT('Ctrl Pts',(-6.97201516823428,4.08294883066162,-1.37100635514375));
#25559=CARTESIAN_POINT('Ctrl Pts',(-8.07503657186441,0.270649261854018,
-1.21303732822146));
#25560=CARTESIAN_POINT('Ctrl Pts',(-7.22975588917528,-3.60695112842209,
-1.05506830129917));
#25561=CARTESIAN_POINT('Ctrl Pts',(-4.64011796957429,-6.61428544049345,
-0.897099274376876));
#25562=CARTESIAN_POINT('Ctrl Pts',(-0.93093694444881,-8.02575996808715,
-0.739130247454587));
#25563=CARTESIAN_POINT('Ctrl Pts',(3.00285561957928,-7.5008216075208,-0.581161220532296));
#25564=CARTESIAN_POINT('Ctrl Pts',(6.21213507255517,-5.166124708156,-0.423192193610008));
#25565=CARTESIAN_POINT('Ctrl Pts',(7.92258345341839,-1.58497258131202,-0.265223166687717));
#25566=CARTESIAN_POINT('Ctrl Pts',(7.72151282951138,2.378593341364,-0.107254139765427));
#25567=CARTESIAN_POINT('Ctrl Pts',(5.65743645678892,5.76826485152039,0.0507148871568628));
#25568=CARTESIAN_POINT('Ctrl Pts',(2.22836375818162,7.76619994727875,0.208683914079155));
#25569=CARTESIAN_POINT('Ctrl Pts',(-1.73835675421644,7.89034742295674,0.366652941001444));
#25570=CARTESIAN_POINT('Ctrl Pts',(-5.28565574934141,6.11075363268263,0.524621967923734));
#25571=CARTESIAN_POINT('Ctrl Pts',(-7.55765969999705,2.85678954753941,0.682590994846022));
#25572=CARTESIAN_POINT('Ctrl Pts',(-8.00619151772145,-1.08644559985997,
0.840560021768314));
#25573=CARTESIAN_POINT('Ctrl Pts',(-6.52303181942251,-4.76754890302042,
0.998529048690603));
#25574=CARTESIAN_POINT('Ctrl Pts',(-3.46602952737128,-7.29836323947227,
1.15649807561289));
#25575=CARTESIAN_POINT('Ctrl Pts',(0.42723802482138,-8.06826712064225,1.31446710253518));
#25576=CARTESIAN_POINT('Ctrl Pts',(4.21742384757461,-6.89150221285597,1.47243612945747));
#25577=CARTESIAN_POINT('Ctrl Pts',(6.99005196541889,-4.05199212494712,1.63040515637976));
#25578=CARTESIAN_POINT('Ctrl Pts',(8.07615734042419,-0.234838822604965,
1.78837418330205));
#25579=CARTESIAN_POINT('Ctrl Pts',(7.21369021600383,3.6389751479531,1.94634321022434));
#25580=CARTESIAN_POINT('Ctrl Pts',(4.61074209526571,6.63479645436352,2.10431223714663));
#25581=CARTESIAN_POINT('Ctrl Pts',(0.895338524482194,8.0298091874258,2.26228126406892));
#25582=CARTESIAN_POINT('Ctrl Pts',(-3.03608758684171,7.48743205811683,2.42025029099121));
#25583=CARTESIAN_POINT('Ctrl Pts',(-6.23498255393503,5.13852694962435,2.5782193179135));
#25584=CARTESIAN_POINT('Ctrl Pts',(-7.92953392953035,1.54982525476801,2.73618834483579));
#25585=CARTESIAN_POINT('Ctrl Pts',(-7.71088932626506,-2.41281007499168,
2.89415737175808));
#25586=CARTESIAN_POINT('Ctrl Pts',(-5.63180215682195,-5.79329535983672,
3.05212639868037));
#25587=CARTESIAN_POINT('Ctrl Pts',(-2.19390356971854,-7.77600500171303,
3.21009542560265));
#25588=CARTESIAN_POINT('Ctrl Pts',(1.77332845928644,-7.88256131186905,3.36806445252495));
#25589=CARTESIAN_POINT('Ctrl Pts',(5.31270118310939,-6.08725494774761,3.52603347944724));
#25590=CARTESIAN_POINT('Ctrl Pts',(7.57025348334349,-2.82324792708962,3.68400250636953));
#25591=CARTESIAN_POINT('Ctrl Pts',(8.00129508925402,1.12193741116395,3.84197153329182));
#25592=CARTESIAN_POINT('Ctrl Pts',(6.50182656348719,4.79642762879022,3.99994056021411));
#25593=CARTESIAN_POINT('Ctrl Pts',(3.43363173588971,7.31366117359706,4.15790958713639));
#25594=CARTESIAN_POINT('Ctrl Pts',(-0.463011584188287,8.06629325854182,
4.3158786140587));
#25595=CARTESIAN_POINT('Ctrl Pts',(-4.24794191975708,6.87273279753116,4.47384764098098));
#25596=CARTESIAN_POINT('Ctrl Pts',(-7.00795131147991,4.02095574158889,4.63181666790327));
#25597=CARTESIAN_POINT('Ctrl Pts',(-8.07711930087982,0.199023765527639,
4.78978569482556));
#25598=CARTESIAN_POINT('Ctrl Pts',(-7.19748269412656,-3.67092761133184,
4.94775472174785));
#25599=CARTESIAN_POINT('Ctrl Pts',(-4.58127555615453,-6.65517700279045,
5.10572374867013));
#25600=CARTESIAN_POINT('Ctrl Pts',(-0.859722498739969,-8.03370051004207,
5.26369277559244));
#25601=CARTESIAN_POINT('Ctrl Pts',(3.06925985302439,-7.47389527719666,5.42166180251471));
#25602=CARTESIAN_POINT('Ctrl Pts',(6.25770743174028,-5.11082814802378,5.57963082943701));
#25603=CARTESIAN_POINT('Ctrl Pts',(7.93632848071451,-1.51464745273923,5.7375998563593));
#25604=CARTESIAN_POINT('Ctrl Pts',(7.7001141974791,2.44697936355635,5.89556888328158));
#25605=CARTESIAN_POINT('Ctrl Pts',(5.60605711411115,5.81821194983595,6.05353791020388));
#25606=CARTESIAN_POINT('Ctrl Pts',(2.15940024073058,7.78565715018472,6.21150693712617));
#25607=CARTESIAN_POINT('Ctrl Pts',(-1.8082652939448,7.8746201995147,6.36947596404845));
#25608=CARTESIAN_POINT('Ctrl Pts',(-5.33964214887762,6.06363656412707,6.52744499097075));
#25609=CARTESIAN_POINT('Ctrl Pts',(-7.58269840658814,2.78965079080092,6.68541401789304));
#25610=CARTESIAN_POINT('Ctrl Pts',(-7.99624132476026,-1.15740716089275,
6.84338304481532));
#25611=CARTESIAN_POINT('Ctrl Pts',(-6.48049345680476,-4.82521203847034,
7.00135207173762));
#25612=CARTESIAN_POINT('Ctrl Pts',(-3.40116642609152,-7.3288152932056,7.15932109865991));
#25613=CARTESIAN_POINT('Ctrl Pts',(0.498776038978558,-8.0641607823018,7.3172901255822));
#25614=CARTESIAN_POINT('Ctrl Pts',(4.27837646117492,-6.85382823802765,7.47525915250449));
#25615=CARTESIAN_POINT('Ctrl Pts',(7.02571285444676,-3.98984029087707,7.63322817942678));
#25616=CARTESIAN_POINT('Ctrl Pts',(8.07792243431764,-0.163204794890052,
7.79119720634906));
#25617=CARTESIAN_POINT('Ctrl Pts',(7.18113364224099,3.70280789026489,7.94916623327137));
#25618=CARTESIAN_POINT('Ctrl Pts',(4.55171893167374,6.67542668498747,8.10713526019364));
#25619=CARTESIAN_POINT('Ctrl Pts',(0.824089567553389,8.03743385947071,8.26510428711594));
#25620=CARTESIAN_POINT('Ctrl Pts',(-3.10237176580277,7.46021153084213,8.42307331403823));
#25621=CARTESIAN_POINT('Ctrl Pts',(-6.28030925917329,5.08302884821862,8.58104234096052));
#25622=CARTESIAN_POINT('Ctrl Pts',(-7.94296697324716,1.4794398665668,8.73901136788281));
#25623=CARTESIAN_POINT('Ctrl Pts',(-7.68918765526074,-2.48110053440443,
8.89698039480511));
#25624=CARTESIAN_POINT('Ctrl Pts',(-5.5802018344612,-5.84301413302921,9.05494942172739));
#25625=CARTESIAN_POINT('Ctrl Pts',(-2.12485445054169,-7.79515620004759,
9.21291844864968));
#25626=CARTESIAN_POINT('Ctrl Pts',(1.84316657286411,-7.86652424757819,9.37088747557198));
#25627=CARTESIAN_POINT('Ctrl Pts',(5.36647811365167,-6.03989893550398,9.52885650249425));
#25628=CARTESIAN_POINT('Ctrl Pts',(7.59499423129414,-2.75599882019051,9.68682552941656));
#25629=CARTESIAN_POINT('Ctrl Pts',(7.99103031142311,1.19285419210965,9.84479455633884));
#25630=CARTESIAN_POINT('Ctrl Pts',(6.45903294254871,4.85390148732021,10.0027635832611));
#25631=CARTESIAN_POINT('Ctrl Pts',(3.36863419036948,7.34382545322469,10.1607326101834));
#25632=CARTESIAN_POINT('Ctrl Pts',(-0.534530596581897,8.06186943684965,
10.3187016371057));
#25633=CARTESIAN_POINT('Ctrl Pts',(-4.30872704690166,6.8347894829523,10.476670664028));
#25634=CARTESIAN_POINT('Ctrl Pts',(-7.0433359080081,3.958645264208,10.6346396909503));
#25635=CARTESIAN_POINT('Ctrl Pts',(-8.0785673795978,0.127384791276112,10.7926087178726));
#25636=CARTESIAN_POINT('Ctrl Pts',(-7.16464211030434,-3.7346195847746,10.9505777447949));
#25637=CARTESIAN_POINT('Ctrl Pts',(-4.5220752727013,-6.69553689283714,11.1085467717172));
#25638=CARTESIAN_POINT('Ctrl Pts',(-0.788435634721984,-8.04102510874207,
11.2665157986394));
#25639=CARTESIAN_POINT('Ctrl Pts',(3.1354133567725,-7.44635011189922,11.4244848255617));
#25640=CARTESIAN_POINT('Ctrl Pts',(6.30280569228859,-5.05518979784663,11.582453852484));
#25641=CARTESIAN_POINT('Ctrl Pts',(7.94941408401714,-1.4440858958632,11.7404228794063));
#25642=CARTESIAN_POINT('Ctrl Pts',(7.67817863371211,2.51494141425027,11.8983919063286));
#25643=CARTESIAN_POINT('Ctrl Pts',(5.5540996652784,5.86818830563099,12.0563609332509));
#25644=CARTESIAN_POINT('Ctrl Pts',(3.24508066864809,7.15818474870596,12.1616736178657));
#25645=CARTESIAN_POINT('Ctrl Pts',(2.00604344898242,7.49003404122904,12.2143299601732));
#25646=CARTESIAN_POINT('Ctrl Pts',(6.15407444028416,-5.30616721305205,-12.6434914756415));
#25647=CARTESIAN_POINT('Ctrl Pts',(7.03199466088407,-4.28796163047964,-12.5908263193679));
#25648=CARTESIAN_POINT('Ctrl Pts',(8.27181934397364,-1.80868985944361,-12.4855048207869));
#25649=CARTESIAN_POINT('Ctrl Pts',(8.13455990327747,2.3489576238944,-12.3275269798982));
#25650=CARTESIAN_POINT('Ctrl Pts',(6.0349869096692,5.93858006336376,-12.169557952976));
#25651=CARTESIAN_POINT('Ctrl Pts',(2.47915939132291,8.09589243843362,-12.0115889260537));
#25652=CARTESIAN_POINT('Ctrl Pts',(-1.67474285532958,8.29960554832456,-11.8536198991314));
#25653=CARTESIAN_POINT('Ctrl Pts',(-5.42461500560061,6.5009700845693,-11.6956508722091));
#25654=CARTESIAN_POINT('Ctrl Pts',(-7.86564263183886,3.13374479744483,-11.5376818452868));
#25655=CARTESIAN_POINT('Ctrl Pts',(-8.40890102379728,-0.989537724336396,
-11.3797128183645));
#25656=CARTESIAN_POINT('Ctrl Pts',(-6.92329841716338,-4.87408841988581,
-11.2217437914422));
#25657=CARTESIAN_POINT('Ctrl Pts',(-3.76728202977869,-7.58263528234616,
-11.0637747645199));
#25658=CARTESIAN_POINT('Ctrl Pts',(0.297685781609928,-8.46168896560967,
-10.9058057375976));
#25659=CARTESIAN_POINT('Ctrl Pts',(4.29082874280202,-7.29914858111052,-10.7478367106754));
#25660=CARTESIAN_POINT('Ctrl Pts',(7.24870366652204,-4.37550956509642,-10.5898676837531));
#25661=CARTESIAN_POINT('Ctrl Pts',(8.45764952174504,-0.396170086096032,
-10.4318986568308));
#25662=CARTESIAN_POINT('Ctrl Pts',(7.62597857233582,3.67875486810516,-10.2739296299085));
#25663=CARTESIAN_POINT('Ctrl Pts',(4.95435181782442,6.86608949616986,-10.1159606029862));
#25664=CARTESIAN_POINT('Ctrl Pts',(1.08736530694238,8.39681029806963,-9.95799157606393));
#25665=CARTESIAN_POINT('Ctrl Pts',(-3.04197496514258,7.90159319927995,-9.80002254914166));
#25666=CARTESIAN_POINT('Ctrl Pts',(-6.43736360984507,5.49992148880527,-9.64205352221935));
#25667=CARTESIAN_POINT('Ctrl Pts',(-8.27957923694806,1.77125784279299,-9.48408449529707));
#25668=CARTESIAN_POINT('Ctrl Pts',(-8.12414180402343,-2.38476552746483,
-9.32611546837478));
#25669=CARTESIAN_POINT('Ctrl Pts',(-6.0085544353048,-5.96540528948545,-9.16814644145249));
#25670=CARTESIAN_POINT('Ctrl Pts',(-2.44325485262408,-8.10674363732677,
-9.0101774145302));
#25671=CARTESIAN_POINT('Ctrl Pts',(1.71154032950948,-8.29212978502554,-8.85220838760791));
#25672=CARTESIAN_POINT('Ctrl Pts',(5.45338411953825,-6.47683474536908,-8.69423936068563));
#25673=CARTESIAN_POINT('Ctrl Pts',(7.87946425157805,-3.098843297253,-8.53627033376333));
#25674=CARTESIAN_POINT('Ctrl Pts',(8.4044289516939,1.02682066064222,-8.37830130684105));
#25675=CARTESIAN_POINT('Ctrl Pts',(6.90161751539969,4.90473876412536,-8.22033227991874));
#25676=CARTESIAN_POINT('Ctrl Pts',(3.73362033233122,7.59926745726833,-8.06236325299647));
#25677=CARTESIAN_POINT('Ctrl Pts',(-0.335205004060077,8.46028511803427,
-7.90439422607416));
#25678=CARTESIAN_POINT('Ctrl Pts',(-4.32315385116687,7.28004996220959,-7.7464251991519));
#25679=CARTESIAN_POINT('Ctrl Pts',(-7.26803501768335,4.34332288172089,-7.58845617222958));
#25680=CARTESIAN_POINT('Ctrl Pts',(-8.45932316175605,0.35866184369231,-7.43048714530731));
#25681=CARTESIAN_POINT('Ctrl Pts',(-7.60959058496652,-3.71253522573633,
-7.272518118385));
#25682=CARTESIAN_POINT('Ctrl Pts',(-4.92385626616827,-6.88799144477263,
-7.11454909146273));
#25683=CARTESIAN_POINT('Ctrl Pts',(-1.05011996734974,-8.40154954322816,
-6.95658006454043));
#25684=CARTESIAN_POINT('Ctrl Pts',(3.07698371935187,-7.88802623372847,-6.79861103761815));
#25685=CARTESIAN_POINT('Ctrl Pts',(6.46168905941665,-5.47132170252852,-6.64064201069584));
#25686=CARTESIAN_POINT('Ctrl Pts',(8.28735226220217,-1.73452562832534,-6.48267298377357));
#25687=CARTESIAN_POINT('Ctrl Pts',(8.11348697260047,2.42076760937246,-6.32470395685127));
#25688=CARTESIAN_POINT('Ctrl Pts',(5.9820424874916,5.99199085037602,-6.16673492992898));
#25689=CARTESIAN_POINT('Ctrl Pts',(2.40728245141181,8.11749825206445,-6.0087659030067));
#25690=CARTESIAN_POINT('Ctrl Pts',(-1.74829395382065,8.28445863796655,-5.8507968760844));
#25691=CARTESIAN_POINT('Ctrl Pts',(-5.48205124685291,6.45258868982236,-5.69282784916212));
#25692=CARTESIAN_POINT('Ctrl Pts',(-7.89312822921419,3.06387229341016,-5.53485882223982));
#25693=CARTESIAN_POINT('Ctrl Pts',(-8.39979300740726,-1.0640789941808,-5.37688979531754));
#25694=CARTESIAN_POINT('Ctrl Pts',(-6.87980018531119,-4.93529493377415,
-5.21892076839524));
#25695=CARTESIAN_POINT('Ctrl Pts',(-3.69988558636464,-7.61574903216721,
-5.06095174147296));
#25696=CARTESIAN_POINT('Ctrl Pts',(0.372717824936398,-8.45871551100516,
-4.90298271455066));
#25697=CARTESIAN_POINT('Ctrl Pts',(4.35539385207399,-7.26080787973768,-4.74501368762838));
#25698=CARTESIAN_POINT('Ctrl Pts',(7.28722350183364,-4.31105095162049,-4.58704466070608));
#25699=CARTESIAN_POINT('Ctrl Pts',(8.46083043325097,-0.321146466458664,
-4.4290756337838));
#25700=CARTESIAN_POINT('Ctrl Pts',(7.59305297731676,3.74624253843844,-4.2711066068615));
#25701=CARTESIAN_POINT('Ctrl Pts',(4.8932638858212,6.9097579709323,-4.11313757993922));
#25702=CARTESIAN_POINT('Ctrl Pts',(1.0128539819229,8.40612357061492,-3.95516855301692));
#25703=CARTESIAN_POINT('Ctrl Pts',(-3.11193197012765,7.8743041652226,-3.79719952609464));
#25704=CARTESIAN_POINT('Ctrl Pts',(-6.48588744656048,5.44261432619416,-3.63923049917234));
#25705=CARTESIAN_POINT('Ctrl Pts',(-8.29496232693573,1.69775930798845,-3.48126147225005));
#25706=CARTESIAN_POINT('Ctrl Pts',(-8.10267259878177,-2.45672209052951,
-3.32329244532776));
#25707=CARTESIAN_POINT('Ctrl Pts',(-5.95541290999965,-6.01845858543149,
-3.16532341840547));
#25708=CARTESIAN_POINT('Ctrl Pts',(-2.37126271376485,-8.12809324598661,
-3.00735439148318));
#25709=CARTESIAN_POINT('Ctrl Pts',(1.78501319996033,-8.27662458669668,-2.84938536456089));
#25710=CARTESIAN_POINT('Ctrl Pts',(5.5106105761161,-6.42821575178852,-2.6914163376386));
#25711=CARTESIAN_POINT('Ctrl Pts',(7.90663699778871,-3.02884104210559,-2.53344731071631));
#25712=CARTESIAN_POINT('Ctrl Pts',(8.39499189110759,1.10131640384692,-2.37547828379402));
#25713=CARTESIAN_POINT('Ctrl Pts',(6.85784757206785,4.96575405667938,-2.21750925687173));
#25714=CARTESIAN_POINT('Ctrl Pts',(3.66607808651513,7.63208085234415,-2.05954022994944));
#25715=CARTESIAN_POINT('Ctrl Pts',(-0.410223316757149,8.45697957331891,
-1.90157120302715));
#25716=CARTESIAN_POINT('Ctrl Pts',(-4.3875482093001,7.24142302204562,-1.74360217610486));
#25717=CARTESIAN_POINT('Ctrl Pts',(-7.30626869133298,4.2786942497907,-1.58563314918257));
#25718=CARTESIAN_POINT('Ctrl Pts',(-8.46217133249921,0.283624774258379,
-1.42766412226028));
#25719=CARTESIAN_POINT('Ctrl Pts',(-7.57636606124012,-3.77987618570152,
-1.26969509533799));
#25720=CARTESIAN_POINT('Ctrl Pts',(-4.86257528521387,-6.93138862485518,
-1.1117260684157));
#25721=CARTESIAN_POINT('Ctrl Pts',(-0.975568079917719,-8.41053230150091,
-0.953757041493409));
#25722=CARTESIAN_POINT('Ctrl Pts',(3.14681902843333,-7.86042725781713,-0.795788014571121));
#25723=CARTESIAN_POINT('Ctrl Pts',(6.50995829638106,-5.41379992727141,-0.63781898764883));
#25724=CARTESIAN_POINT('Ctrl Pts',(8.30240928102332,-1.66095960321813,-0.479849960726541));
#25725=CARTESIAN_POINT('Ctrl Pts',(8.09169889546763,2.49262826314565,-0.321880933804249));
#25726=CARTESIAN_POINT('Ctrl Pts',(5.92866622634028,6.04480797460074,-0.16391190688196));
#25727=CARTESIAN_POINT('Ctrl Pts',(2.33519634803474,8.13852841054634,-0.00594287995966794));
#25728=CARTESIAN_POINT('Ctrl Pts',(-1.82169734592179,8.2686277853708,0.152026146962621));
#25729=CARTESIAN_POINT('Ctrl Pts',(-5.53906154572492,6.40371641047728,0.309995173884911));
#25730=CARTESIAN_POINT('Ctrl Pts',(-7.91999029167661,2.99375023221594,0.4679642008072));
#25731=CARTESIAN_POINT('Ctrl Pts',(-8.39002569719858,-1.13853215742554,
0.625933227729491));
#25732=CARTESIAN_POINT('Ctrl Pts',(-6.83576010734434,-4.99611553389072,
0.783902254651781));
#25733=CARTESIAN_POINT('Ctrl Pts',(-3.63219849756608,-7.64826259665706,
0.941871281574071));
#25734=CARTESIAN_POINT('Ctrl Pts',(0.447720742020407,-8.4550773391087,1.09984030849636));
#25735=CARTESIAN_POINT('Ctrl Pts',(4.41961629056801,-7.22189577031478,1.25780933541865));
#25736=CARTESIAN_POINT('Ctrl Pts',(7.32517021167997,-4.24625341248742,1.41577836234094));
#25737=CARTESIAN_POINT('Ctrl Pts',(8.46334583313366,-0.246097504911587,
1.57374738926323));
#25738=CARTESIAN_POINT('Ctrl Pts',(7.55953016486508,3.8134355061597,1.73171641618552));
#25739=CARTESIAN_POINT('Ctrl Pts',(4.83179106780148,6.95288298119983,1.88968544310781));
#25740=CARTESIAN_POINT('Ctrl Pts',(0.938262994517446,8.41477564919374,2.0476544700301));
#25741=CARTESIAN_POINT('Ctrl Pts',(-3.18164420825611,7.84639578438501,2.20562349695239));
#25742=CARTESIAN_POINT('Ctrl Pts',(-6.53390113555359,5.38487907236143,2.36359252387468));
#25743=CARTESIAN_POINT('Ctrl Pts',(-8.30969297802931,1.62412723763715,2.52156155079697));
#25744=CARTESIAN_POINT('Ctrl Pts',(-8.08056607844303,-2.52848542116828,
2.67953057771926));
#25745=CARTESIAN_POINT('Ctrl Pts',(-5.90180296245549,-6.07103849975408,
2.83749960464155));
#25746=CARTESIAN_POINT('Ctrl Pts',(-2.29908406342406,-8.14880354054839,
2.99546863156383));
#25747=CARTESIAN_POINT('Ctrl Pts',(1.85834567035452,-8.26046839123662,3.15343765848613));
#25748=CARTESIAN_POINT('Ctrl Pts',(5.56740359622459,-6.3790911476393,3.31140668540842));
#25749=CARTESIAN_POINT('Ctrl Pts',(7.93318784830107,-2.95860055376065,3.46937571233071));
#25750=CARTESIAN_POINT('Ctrl Pts',(8.38489452333455,1.17572552311275,3.627344739253));
#25751=CARTESIAN_POINT('Ctrl Pts',(6.81353822546464,5.02637876838552,3.78531376617529));
#25752=CARTESIAN_POINT('Ctrl Pts',(3.59824748571965,7.66429394691102,3.94328279309757));
#25753=CARTESIAN_POINT('Ctrl Pts',(-0.485209363383541,8.45300884577968,
4.10125182001987));
#25754=CARTESIAN_POINT('Ctrl Pts',(-4.45159746529674,7.20222650852556,4.25922084694216));
#25755=CARTESIAN_POINT('Ctrl Pts',(-7.34392769119849,4.21372907762145,4.41718987386444));
#25756=CARTESIAN_POINT('Ctrl Pts',(-8.46435391205914,0.208565396347819,
4.57515890078674));
#25757=CARTESIAN_POINT('Ctrl Pts',(-7.54254561924968,-3.84691983990853,
4.73312792770903));
#25758=CARTESIAN_POINT('Ctrl Pts',(-4.80091183891932,-6.97424061730516,
4.89109695463132));
#25759=CARTESIAN_POINT('Ctrl Pts',(-0.900939459282501,-8.41885353025294,
5.04906598155361));
#25760=CARTESIAN_POINT('Ctrl Pts',(3.21640682479993,-7.83221002083862,5.2070350084759));
#25761=CARTESIAN_POINT('Ctrl Pts',(6.55771549327035,-5.35585233015872,5.36500403539819));
#25762=CARTESIAN_POINT('Ctrl Pts',(8.31681327472841,-1.58726293551058,5.52297306232048));
#25763=CARTESIAN_POINT('Ctrl Pts',(8.06927436662165,2.56429285950871,5.68094208924277));
#25764=CARTESIAN_POINT('Ctrl Pts',(5.87482364657965,6.0971496450992,5.83891111616505));
#25765=CARTESIAN_POINT('Ctrl Pts',(2.26292657003822,8.15891843394451,5.99688014308736));
#25766=CARTESIAN_POINT('Ctrl Pts',(-1.89495745261251,8.25214656473898,6.15484917000963));
#25767=CARTESIAN_POINT('Ctrl Pts',(-5.5956361703021,6.35434044750129,6.31281819693194));
#25768=CARTESIAN_POINT('Ctrl Pts',(-7.94622940814776,2.92339269791678,6.47078722385421));
#25769=CARTESIAN_POINT('Ctrl Pts',(-8.37959847041395,-1.21289576954504,
6.62875625077651));
#25770=CARTESIAN_POINT('Ctrl Pts',(-6.79118236339584,-5.05654316507279,
6.78672527769879));
#25771=CARTESIAN_POINT('Ctrl Pts',(-3.56422571858213,-7.68017458786904,
6.9446943046211));
#25772=CARTESIAN_POINT('Ctrl Pts',(0.522688443676895,-8.45077413400531,
7.10266333154337));
#25773=CARTESIAN_POINT('Ctrl Pts',(4.48349110461487,-7.18241562345274,7.26063235846567));
#25774=CARTESIAN_POINT('Ctrl Pts',(7.36254076104373,-4.18112188474151,7.41860138538795));
#25775=CARTESIAN_POINT('Ctrl Pts',(8.46519554945526,-0.171029186599225,
7.57657041231025));
#25776=CARTESIAN_POINT('Ctrl Pts',(7.52541275837057,3.88032852853282,7.73453943923254));
#25777=CARTESIAN_POINT('Ctrl Pts',(4.76993820577959,6.99546111316978,7.89250846615483));
#25778=CARTESIAN_POINT('Ctrl Pts',(0.863598208119548,8.4227658645474,8.05047749307711));
#25779=CARTESIAN_POINT('Ctrl Pts',(-3.2511061944664,7.81787024601633,8.20844651999941));
#25780=CARTESIAN_POINT('Ctrl Pts',(-6.58140090131321,5.32672027164962,8.36641554692169));
#25781=CARTESIAN_POINT('Ctrl Pts',(-8.3237700309859,1.55036742132396,8.524384573844));
#25782=CARTESIAN_POINT('Ctrl Pts',(-8.05782398227964,-2.60004987326493,
8.68235360076627));
#25783=CARTESIAN_POINT('Ctrl Pts',(-5.84772880876681,-6.12314089872802,
8.84032262768858));
#25784=CARTESIAN_POINT('Ctrl Pts',(-2.22672457976938,-8.16887288885258,
8.99829165461085));
#25785=CARTESIAN_POINT('Ctrl Pts',(1.9315319745122,-8.24366247531389,9.15626068153316));
#25786=CARTESIAN_POINT('Ctrl Pts',(5.62375870941011,-6.32946478549677,9.31422970845543));
#25787=CARTESIAN_POINT('Ctrl Pts',(7.95911472134858,-2.8881273788749,9.47219873537773));
#25788=CARTESIAN_POINT('Ctrl Pts',(8.37413762979948,1.25004220829073,9.63016776230001));
#25789=CARTESIAN_POINT('Ctrl Pts',(6.76869298555811,5.08660804830173,9.78813678922231));
#25790=CARTESIAN_POINT('Ctrl Pts',(3.53013381694687,7.69590436750279,9.94610581614459));
#25791=CARTESIAN_POINT('Ctrl Pts',(-0.560157152290724,8.44837293648434,
10.1040748430669));
#25792=CARTESIAN_POINT('Ctrl Pts',(-4.51529676322405,7.16246410918141,10.2620438699892));
#25793=CARTESIAN_POINT('Ctrl Pts',(-7.38100870200111,4.14843130086038,10.4200128969115));
#25794=CARTESIAN_POINT('Ctrl Pts',(-8.46587141481043,0.133491894351164,
10.5779819238338));
#25795=CARTESIAN_POINT('Ctrl Pts',(-7.50813058663781,-3.91366534464785,
10.7359509507561));
#25796=CARTESIAN_POINT('Ctrl Pts',(-4.73887336552598,-7.01653544798443,
10.8939199776784));
#25797=CARTESIAN_POINT('Ctrl Pts',(-0.82623494844739,-8.42652928609498,
11.0518890046007));
#25798=CARTESIAN_POINT('Ctrl Pts',(3.28573187094426,-7.80334428059651,11.2098580315229));
#25799=CARTESIAN_POINT('Ctrl Pts',(6.60497586220628,-5.2975465568453,11.3678270584453));
#25800=CARTESIAN_POINT('Ctrl Pts',(8.3305262302241,-1.51331850461435,11.5257960853675));
#25801=CARTESIAN_POINT('Ctrl Pts',(8.04628716436945,2.63551315826054,11.6837651122898));
#25802=CARTESIAN_POINT('Ctrl Pts',(5.82037524500162,6.14952197574412,11.8417341392121));
#25803=CARTESIAN_POINT('Ctrl Pts',(3.4006568715194,7.50136364512427,11.947046823827));
#25804=CARTESIAN_POINT('Ctrl Pts',(2.10221752120281,7.84912251220897,11.9997031661344));
#25805=CARTESIAN_POINT('Ctrl Pts',(2.10208451021619,7.84862588447234,12.));
#25806=CARTESIAN_POINT('Ctrl Pts',(2.2993955749037,7.78116612976009,12.));
#25807=CARTESIAN_POINT('Ctrl Pts',(2.49365425396881,7.70609002735957,12.));
#25808=CARTESIAN_POINT('Ctrl Pts',(2.68449722322631,7.62371149358249,12.));
#25809=CARTESIAN_POINT('Ctrl Pts',(2.87766974768538,7.54032739306849,12.));
#25810=CARTESIAN_POINT('Ctrl Pts',(3.06734326822009,7.44946115104765,12.));
#25811=CARTESIAN_POINT('Ctrl Pts',(3.25311885290036,7.35138992462918,12.));
#25812=CARTESIAN_POINT('Ctrl Pts',(3.43857588515895,7.25348686254041,12.));
#25813=CARTESIAN_POINT('Ctrl Pts',(3.62014888805913,7.1484030613508,12.));
#25814=CARTESIAN_POINT('Ctrl Pts',(3.79741044071271,7.03637241507993,12.));
#25815=CARTESIAN_POINT('Ctrl Pts',(3.97212170910349,6.92595356781374,12.));
#25816=CARTESIAN_POINT('Ctrl Pts',(4.14264513227527,6.80878584951957,12.));
#25817=CARTESIAN_POINT('Ctrl Pts',(4.30853456648212,6.68505947211609,12.));
#25818=CARTESIAN_POINT('Ctrl Pts',(4.45106252434089,6.57875693398944,12.));
#25819=CARTESIAN_POINT('Ctrl Pts',(4.59016935875685,6.46761224470133,12.));
#25820=CARTESIAN_POINT('Ctrl Pts',(4.72554610344008,6.35172956521935,12.));
#25821=CARTESIAN_POINT('Ctrl Pts',(4.74477333824113,6.33527102580781,12.));
#25822=CARTESIAN_POINT('Ctrl Pts',(4.76392528681677,6.31871689013953,12.));
#25823=CARTESIAN_POINT('Ctrl Pts',(4.78300101992008,6.30206743516809,12.));
#25824=CARTESIAN_POINT('Ctrl Pts',(4.80076087393577,6.28656649016472,12.));
#25825=CARTESIAN_POINT('Ctrl Pts',(4.81844738030779,6.27098927657102,12.));
#25826=CARTESIAN_POINT('Ctrl Pts',(4.83605920680848,6.25533688423888,12.));
#25827=CARTESIAN_POINT('Ctrl Pts',(4.98998560005503,6.11853583766523,12.));
#25828=CARTESIAN_POINT('Ctrl Pts',(5.13823022848562,5.97597793333321,12.));
#25829=CARTESIAN_POINT('Ctrl Pts',(5.28041162851553,5.82790909187815,12.));
#25830=CARTESIAN_POINT('Ctrl Pts',(5.32007318404608,5.78660523232639,12.));
#25831=CARTESIAN_POINT('Ctrl Pts',(5.35926272429222,5.74487232374225,12.));
#25832=CARTESIAN_POINT('Ctrl Pts',(5.39797144463401,5.70271520266631,12.));
#25833=CARTESIAN_POINT('Ctrl Pts',(5.537130358362,5.55115919350284,12.));
#25834=CARTESIAN_POINT('Ctrl Pts',(5.67007843940407,5.39412278727632,12.));
#25835=CARTESIAN_POINT('Ctrl Pts',(5.79659171893264,5.23204542006403,12.));
#25836=CARTESIAN_POINT('Ctrl Pts',(5.92308395052344,5.06999501756527,12.));
#25837=CARTESIAN_POINT('Ctrl Pts',(6.04314381607103,4.90290466616952,12.));
#25838=CARTESIAN_POINT('Ctrl Pts',(6.15650094748101,4.73119033909099,12.));
#25839=CARTESIAN_POINT('Ctrl Pts',(6.2685847071828,4.56140492608495,12.));
#25840=CARTESIAN_POINT('Ctrl Pts',(6.37411567049303,4.38709818588679,12.));
#25841=CARTESIAN_POINT('Ctrl Pts',(6.47278349045617,4.20865935363704,12.));
#25842=CARTESIAN_POINT('Ctrl Pts',(6.513215075432,4.13553961903878,12.));
#25843=CARTESIAN_POINT('Ctrl Pts',(6.5524936416175,4.06172594633208,12.));
#25844=CARTESIAN_POINT('Ctrl Pts',(6.59059530005883,3.98724486707222,12.));
#25845=CARTESIAN_POINT('Ctrl Pts',(6.60144172391569,3.9660422898612,12.));
#25846=CARTESIAN_POINT('Ctrl Pts',(6.61219276480136,3.94478562751987,12.));
#25847=CARTESIAN_POINT('Ctrl Pts',(6.62284784887895,3.92347549186304,12.));
#25848=CARTESIAN_POINT('Ctrl Pts',(6.63395017824082,3.90127086700178,12.));
#25849=CARTESIAN_POINT('Ctrl Pts',(6.64494485731741,3.87901508077576,12.));
#25850=CARTESIAN_POINT('Ctrl Pts',(6.65582886903515,3.85671429060614,12.));
#25851=CARTESIAN_POINT('Ctrl Pts',(6.74450049831353,3.6750306017405,12.));
#25852=CARTESIAN_POINT('Ctrl Pts',(6.82588701041696,3.4902491840288,12.));
#25853=CARTESIAN_POINT('Ctrl Pts',(6.89978215802754,3.3027870592376,12.));
#25854=CARTESIAN_POINT('Ctrl Pts',(6.97319794282983,3.11654101389823,12.));
#25855=CARTESIAN_POINT('Ctrl Pts',(7.03921944722408,2.92764827349166,12.));
#25856=CARTESIAN_POINT('Ctrl Pts',(7.09759598956962,2.73650163287192,12.));
#25857=CARTESIAN_POINT('Ctrl Pts',(7.13572390237701,2.6116565811758,12.));
#25858=CARTESIAN_POINT('Ctrl Pts',(7.17058956880297,2.48584973539685,12.));
#25859=CARTESIAN_POINT('Ctrl Pts',(7.20211123195996,2.35918876245082,12.));
#25860=CARTESIAN_POINT('Ctrl Pts',(7.25235994792851,2.15727837396125,12.));
#25861=CARTESIAN_POINT('Ctrl Pts',(7.29411388123278,1.95319690708858,12.));
#25862=CARTESIAN_POINT('Ctrl Pts',(7.32732391013097,1.74748626497986,12.));
#25863=CARTESIAN_POINT('Ctrl Pts',(7.36053393902917,1.54177562287114,12.));
#25864=CARTESIAN_POINT('Ctrl Pts',(7.38520001023308,1.33443494496339,12.));
#25865=CARTESIAN_POINT('Ctrl Pts',(7.40121439147182,1.12601971526756,12.));
#25866=CARTESIAN_POINT('Ctrl Pts',(7.40333855631591,1.09837529383825,12.));
#25867=CARTESIAN_POINT('Ctrl Pts',(7.40531048989455,1.07071006825862,12.));
#25868=CARTESIAN_POINT('Ctrl Pts',(7.40712860673866,1.04304720983276,12.));
#25869=CARTESIAN_POINT('Ctrl Pts',(7.42012496900755,0.845306052184669,12.));
#25870=CARTESIAN_POINT('Ctrl Pts',(7.42528630994362,0.647440157454434,12.));
#25871=CARTESIAN_POINT('Ctrl Pts',(7.42264771266255,0.449916696084704,12.));
#25872=CARTESIAN_POINT('Ctrl Pts',(7.42001587668523,0.252899380964936,12.));
#25873=CARTESIAN_POINT('Ctrl Pts',(7.40962392243267,0.0562220340153437,
12.));
#25874=CARTESIAN_POINT('Ctrl Pts',(7.39145489568746,-0.139648191421885,
12.));
#25875=CARTESIAN_POINT('Ctrl Pts',(7.37321585338488,-0.336273215847537,
12.));
#25876=CARTESIAN_POINT('Ctrl Pts',(7.34713964605262,-0.532085602194281,
12.));
#25877=CARTESIAN_POINT('Ctrl Pts',(7.31315786408237,-0.726598445503667,
12.));
#25878=CARTESIAN_POINT('Ctrl Pts',(7.27917608211211,-0.921111288813166,
12.));
#25879=CARTESIAN_POINT('Ctrl Pts',(7.23728866332716,-1.11432529315272,12.));
#25880=CARTESIAN_POINT('Ctrl Pts',(7.18737683938923,-1.30572860229433,12.));
#25881=CARTESIAN_POINT('Ctrl Pts',(7.16523608896148,-1.39063459378882,12.));
#25882=CARTESIAN_POINT('Ctrl Pts',(7.14151561885176,-1.47518388140826,12.));
#25883=CARTESIAN_POINT('Ctrl Pts',(7.11622968392941,-1.55933456450703,12.));
#25884=CARTESIAN_POINT('Ctrl Pts',(7.10233271500884,-1.60558317786698,12.));
#25885=CARTESIAN_POINT('Ctrl Pts',(7.08796315084845,-1.65171049254164,12.));
#25886=CARTESIAN_POINT('Ctrl Pts',(7.07312223633881,-1.69771223079685,12.));
#25887=CARTESIAN_POINT('Ctrl Pts',(7.06252436973796,-1.73056197769887,12.));
#25888=CARTESIAN_POINT('Ctrl Pts',(7.05168654638728,-1.7633460344081,12.));
#25889=CARTESIAN_POINT('Ctrl Pts',(7.04061734109932,-1.79603977805719,12.));
#25890=CARTESIAN_POINT('Ctrl Pts',(6.97824817218232,-1.98025188426835,12.));
#25891=CARTESIAN_POINT('Ctrl Pts',(6.90848807259781,-2.16175440386442,12.));
#25892=CARTESIAN_POINT('Ctrl Pts',(6.83157468295091,-2.34012772594946,12.));
#25893=CARTESIAN_POINT('Ctrl Pts',(6.75497532969541,-2.51777275202981,12.));
#25894=CARTESIAN_POINT('Ctrl Pts',(6.67128054581601,-2.69231466539617,12.));
#25895=CARTESIAN_POINT('Ctrl Pts',(6.58068264439258,-2.86331016587819,12.));
#25896=CARTESIAN_POINT('Ctrl Pts',(6.51303849241552,-2.9909825008911,12.));
#25897=CARTESIAN_POINT('Ctrl Pts',(6.44154513262403,-3.11667726450743,12.));
#25898=CARTESIAN_POINT('Ctrl Pts',(6.36626922705372,-3.24019647327262,12.));
#25899=CARTESIAN_POINT('Ctrl Pts',(6.35043403973881,-3.26618021658287,12.));
#25900=CARTESIAN_POINT('Ctrl Pts',(6.33443045294555,-3.29206910662706,12.));
#25901=CARTESIAN_POINT('Ctrl Pts',(6.31826810629452,-3.31784702529636,12.));
#25902=CARTESIAN_POINT('Ctrl Pts',(6.21663338793026,-3.47994796029905,12.));
#25903=CARTESIAN_POINT('Ctrl Pts',(6.10865101626227,-3.63778508614921,12.));
#25904=CARTESIAN_POINT('Ctrl Pts',(5.99452112172698,-3.79093554697371,12.));
#25905=CARTESIAN_POINT('Ctrl Pts',(5.88191571077627,-3.94204030921547,12.));
#25906=CARTESIAN_POINT('Ctrl Pts',(5.76332545224429,-4.08858324137673,12.));
#25907=CARTESIAN_POINT('Ctrl Pts',(5.63890846560756,-4.23012100294325,12.));
#25908=CARTESIAN_POINT('Ctrl Pts',(5.58859724884651,-4.2873554465232,12.));
#25909=CARTESIAN_POINT('Ctrl Pts',(5.53733289223766,-4.34377097889626,12.));
#25910=CARTESIAN_POINT('Ctrl Pts',(5.48512449108001,-4.39933625912035,12.));
#25911=CARTESIAN_POINT('Ctrl Pts',(5.4281364310843,-4.45998851915656,12.));
#25912=CARTESIAN_POINT('Ctrl Pts',(5.37002354987676,-4.5196277380235,12.));
#25913=CARTESIAN_POINT('Ctrl Pts',(5.31081700063339,-4.57822770314263,12.));
#25914=CARTESIAN_POINT('Ctrl Pts',(5.31037376991254,-4.57794244025905,-12.));
#25915=CARTESIAN_POINT('Ctrl Pts',(5.44267363655215,-4.44683792433415,-12.));
#25916=CARTESIAN_POINT('Ctrl Pts',(5.56937771169702,-4.31060781960146,-12.));
#25917=CARTESIAN_POINT('Ctrl Pts',(5.6903584571106,-4.16972393460644,-12.));
#25918=CARTESIAN_POINT('Ctrl Pts',(5.8143418732599,-4.02534339469196,-12.));
#25919=CARTESIAN_POINT('Ctrl Pts',(5.93231481872001,-3.87607486581971,-12.));
#25920=CARTESIAN_POINT('Ctrl Pts',(6.04411419453926,-3.72237753023135,-12.));
#25921=CARTESIAN_POINT('Ctrl Pts',(6.15675534768411,-3.56752295265345,-12.));
#25922=CARTESIAN_POINT('Ctrl Pts',(6.26313006821541,-3.40817211459952,-12.));
#25923=CARTESIAN_POINT('Ctrl Pts',(6.36303861860623,-3.24475251660394,-12.));
#25924=CARTESIAN_POINT('Ctrl Pts',(6.45945119635235,-3.08705125244431,-12.));
#25925=CARTESIAN_POINT('Ctrl Pts',(6.54984238090044,-2.92556030592911,-12.));
#25926=CARTESIAN_POINT('Ctrl Pts',(6.63399797028678,-2.76063397584875,-12.));
#25927=CARTESIAN_POINT('Ctrl Pts',(6.67607576497995,-2.67817081080857,-12.));
#25928=CARTESIAN_POINT('Ctrl Pts',(6.71659409382163,-2.59484838741849,-12.));
#25929=CARTESIAN_POINT('Ctrl Pts',(6.7555225444137,-2.51070882516395,-12.));
#25930=CARTESIAN_POINT('Ctrl Pts',(6.77498676970973,-2.46863904403668,-12.));
#25931=CARTESIAN_POINT('Ctrl Pts',(6.79405348565133,-2.42636495809896,-12.));
#25932=CARTESIAN_POINT('Ctrl Pts',(6.81271864440367,-2.38389172142662,-12.));
#25933=CARTESIAN_POINT('Ctrl Pts',(6.82488864469961,-2.35619845025061,-12.));
#25934=CARTESIAN_POINT('Ctrl Pts',(6.83688874062191,-2.32841859568406,-12.));
#25935=CARTESIAN_POINT('Ctrl Pts',(6.84871511036648,-2.30055985767388,-12.));
#25936=CARTESIAN_POINT('Ctrl Pts',(6.85502687237034,-2.28569158212981,-12.));
#25937=CARTESIAN_POINT('Ctrl Pts',(6.86128851596274,-2.27080232980739,-12.));
#25938=CARTESIAN_POINT('Ctrl Pts',(6.86749846779438,-2.25589588159315,-12.));
#25939=CARTESIAN_POINT('Ctrl Pts',(6.9429142099725,-2.0748669644943,-12.));
#25940=CARTESIAN_POINT('Ctrl Pts',(7.01079261617851,-1.8911080179053,-12.));
#25941=CARTESIAN_POINT('Ctrl Pts',(7.07095894577038,-1.70508173509055,-12.));
#25942=CARTESIAN_POINT('Ctrl Pts',(7.08700753589636,-1.65546163052699,-12.));
#25943=CARTESIAN_POINT('Ctrl Pts',(7.10250722151628,-1.60568000149234,-12.));
#25944=CARTESIAN_POINT('Ctrl Pts',(7.11745423244714,-1.55574520184558,-12.));
#25945=CARTESIAN_POINT('Ctrl Pts',(7.17289725401069,-1.37052180257242,-12.));
#25946=CARTESIAN_POINT('Ctrl Pts',(7.22073965069804,-1.18319304603741,-12.));
#25947=CARTESIAN_POINT('Ctrl Pts',(7.26105716846878,-0.994238416058683,
-12.));
#25948=CARTESIAN_POINT('Ctrl Pts',(7.30180998831209,-0.803243671841799,
-12.));
#25949=CARTESIAN_POINT('Ctrl Pts',(7.33487473704459,-0.6105871243123,-12.));
#25950=CARTESIAN_POINT('Ctrl Pts',(7.36028116535095,-0.416741430078175,
-12.));
#25951=CARTESIAN_POINT('Ctrl Pts',(7.38577396141591,-0.222236768045678,
-12.));
#25952=CARTESIAN_POINT('Ctrl Pts',(7.40355641032544,-0.0265341668316033,
-12.));
#25953=CARTESIAN_POINT('Ctrl Pts',(7.41360781144787,0.169901389152281,-12.));
#25954=CARTESIAN_POINT('Ctrl Pts',(7.4166886322644,0.230110184185977,-12.));
#25955=CARTESIAN_POINT('Ctrl Pts',(7.41904278312292,0.29038788552009,-12.));
#25956=CARTESIAN_POINT('Ctrl Pts',(7.42066868798675,0.350721181107772,-12.));
#25957=CARTESIAN_POINT('Ctrl Pts',(7.4216482379621,0.387069850406059,-12.));
#25958=CARTESIAN_POINT('Ctrl Pts',(7.42236347434099,0.423440379102023,-12.));
#25959=CARTESIAN_POINT('Ctrl Pts',(7.42281390769938,0.459825068682672,-12.));
#25960=CARTESIAN_POINT('Ctrl Pts',(7.42316672971766,0.488324999634255,-12.));
#25961=CARTESIAN_POINT('Ctrl Pts',(7.42335696411711,0.51682607170187,-12.));
#25962=CARTESIAN_POINT('Ctrl Pts',(7.4233848049328,0.545317083559071,-12.));
#25963=CARTESIAN_POINT('Ctrl Pts',(7.42357977148935,0.744836901380488,-12.));
#25964=CARTESIAN_POINT('Ctrl Pts',(7.41581674804868,0.944011512545434,-12.));
#25965=CARTESIAN_POINT('Ctrl Pts',(7.40017828941996,1.14234330858621,-12.));
#25966=CARTESIAN_POINT('Ctrl Pts',(7.38439461942376,1.34251672035145,-12.));
#25967=CARTESIAN_POINT('Ctrl Pts',(7.3605887283379,1.54183228746579,-12.));
#25968=CARTESIAN_POINT('Ctrl Pts',(7.32879500122438,1.73979431536829,-12.));
#25969=CARTESIAN_POINT('Ctrl Pts',(7.30959003369515,1.85937307077222,-12.));
#25970=CARTESIAN_POINT('Ctrl Pts',(7.28746951960363,1.97845821396004,-12.));
#25971=CARTESIAN_POINT('Ctrl Pts',(7.2624318954249,2.09694161440503,-12.));
#25972=CARTESIAN_POINT('Ctrl Pts',(7.22127493906698,2.29170514733619,-12.));
#25973=CARTESIAN_POINT('Ctrl Pts',(7.17223845228515,2.48484324886949,-12.));
#25974=CARTESIAN_POINT('Ctrl Pts',(7.11556674531464,2.67596142272514,-12.));
#25975=CARTESIAN_POINT('Ctrl Pts',(7.05858971676105,2.86810925505617,-12.));
#25976=CARTESIAN_POINT('Ctrl Pts',(6.99389478787003,3.05821599278081,-12.));
#25977=CARTESIAN_POINT('Ctrl Pts',(6.92167928825846,3.24586879408122,-12.));
#25978=CARTESIAN_POINT('Ctrl Pts',(6.91269241961899,3.26922127497781,-12.));
#25979=CARTESIAN_POINT('Ctrl Pts',(6.90358902068414,3.29253573016435,-12.));
#25980=CARTESIAN_POINT('Ctrl Pts',(6.89436941920698,3.31581134317188,-12.));
#25981=CARTESIAN_POINT('Ctrl Pts',(6.88279319264489,3.3450364425663,-12.));
#25982=CARTESIAN_POINT('Ctrl Pts',(6.87103714791754,3.37419161400014,-12.));
#25983=CARTESIAN_POINT('Ctrl Pts',(6.85910773788451,3.40326238116243,-12.));
#25984=CARTESIAN_POINT('Ctrl Pts',(6.78106408142094,3.59344688813005,-12.));
#25985=CARTESIAN_POINT('Ctrl Pts',(6.69553789775985,3.78018911471325,-12.));
#25986=CARTESIAN_POINT('Ctrl Pts',(6.60286394971234,3.96308083941159,-12.));
#25987=CARTESIAN_POINT('Ctrl Pts',(6.51036026948687,4.14563654113595,-12.));
#25988=CARTESIAN_POINT('Ctrl Pts',(6.41073477459907,4.3243565276691,-12.));
#25989=CARTESIAN_POINT('Ctrl Pts',(6.3042667134665,4.49882949555396,-12.));
#25990=CARTESIAN_POINT('Ctrl Pts',(6.19750469508528,4.67378418155275,-12.));
#25991=CARTESIAN_POINT('Ctrl Pts',(6.08386202640003,4.84446903588274,-12.));
#25992=CARTESIAN_POINT('Ctrl Pts',(5.96357023683373,5.01045404774627,-12.));
#25993=CARTESIAN_POINT('Ctrl Pts',(5.84327844726742,5.1764390596098,-12.));
#25994=CARTESIAN_POINT('Ctrl Pts',(5.71633726955937,5.33772491039946,-12.));
#25995=CARTESIAN_POINT('Ctrl Pts',(5.58293216084948,5.49385617917443,-12.));
#25996=CARTESIAN_POINT('Ctrl Pts',(5.48072058003189,5.61347996233291,-12.));
#25997=CARTESIAN_POINT('Ctrl Pts',(5.37471348653155,5.730077391454,-12.));
#25998=CARTESIAN_POINT('Ctrl Pts',(5.26507849878159,5.84352819875606,-12.));
#25999=CARTESIAN_POINT('Ctrl Pts',(5.24734949409338,5.86187425721622,-12.));
#26000=CARTESIAN_POINT('Ctrl Pts',(5.22953248942995,5.88013086702314,-12.));
#26001=CARTESIAN_POINT('Ctrl Pts',(5.21162852093184,5.89829754282688,-12.));
#26002=CARTESIAN_POINT('Ctrl Pts',(5.06686638504291,6.04518379274567,-12.));
#26003=CARTESIAN_POINT('Ctrl Pts',(4.91642028337385,6.18619531935667,-12.));
#26004=CARTESIAN_POINT('Ctrl Pts',(4.7607493602725,6.32112569282487,-12.));
#26005=CARTESIAN_POINT('Ctrl Pts',(4.60343491120369,6.45748061988455,-12.));
#26006=CARTESIAN_POINT('Ctrl Pts',(4.44078428868537,6.58762579275016,-12.));
#26007=CARTESIAN_POINT('Ctrl Pts',(4.27322757175171,6.71131806402962,-12.));
#26008=CARTESIAN_POINT('Ctrl Pts',(4.19032886513755,6.77251483068203,-12.));
#26009=CARTESIAN_POINT('Ctrl Pts',(4.10622862770558,6.83213156416253,-12.));
#26010=CARTESIAN_POINT('Ctrl Pts',(4.0209755701235,6.89013557221799,-12.));
#26011=CARTESIAN_POINT('Ctrl Pts',(3.98093099022267,6.91738088401116,-12.));
#26012=CARTESIAN_POINT('Ctrl Pts',(3.94063203236017,6.94427034483953,-12.));
#26013=CARTESIAN_POINT('Ctrl Pts',(3.90008359516906,6.97080038552624,-12.));
#26014=CARTESIAN_POINT('Ctrl Pts',(3.87285102989615,6.98861811451265,-12.));
#26015=CARTESIAN_POINT('Ctrl Pts',(3.84550593396186,7.00627372305823,-12.));
#26016=CARTESIAN_POINT('Ctrl Pts',(3.81804976883042,7.0237660991706,-12.));
#26017=CARTESIAN_POINT('Ctrl Pts',(3.79110003457158,7.04093582719077,-12.));
#26018=CARTESIAN_POINT('Ctrl Pts',(3.76405158817414,7.05794299142264,-12.));
#26019=CARTESIAN_POINT('Ctrl Pts',(3.73690799396172,7.07478559879379,-12.));
#26020=CARTESIAN_POINT('Ctrl Pts',(3.55729426387553,7.18623596570672,-12.));
#26021=CARTESIAN_POINT('Ctrl Pts',(3.37348978795351,7.29050138644909,-12.));
#26022=CARTESIAN_POINT('Ctrl Pts',(3.18594346175011,7.38734226264639,-12.));
#26023=CARTESIAN_POINT('Ctrl Pts',(2.99823564615633,7.4842665250362,-12.));
#26024=CARTESIAN_POINT('Ctrl Pts',(2.80677898323789,7.57375390615019,-12.));
#26025=CARTESIAN_POINT('Ctrl Pts',(2.61198894494858,7.65552549589783,-12.));
#26026=CARTESIAN_POINT('Ctrl Pts',(2.53306554533635,7.68865702516523,-12.));
#26027=CARTESIAN_POINT('Ctrl Pts',(2.45359457631988,7.72052141836669,-12.));
#26028=CARTESIAN_POINT('Ctrl Pts',(2.37360237640535,7.75109805319065,-12.));
#26029=CARTESIAN_POINT('Ctrl Pts',(2.2838343803519,7.78541143921003,-12.));
#26030=CARTESIAN_POINT('Ctrl Pts',(2.19340997675606,7.81810312229487,-12.));
#26031=CARTESIAN_POINT('Ctrl Pts',(2.10237422929003,7.84917075545908,-12.));
#26032=CARTESIAN_POINT('Ctrl Pts',(-2.10221711401193,7.84912099186632,-11.9997040748415));
#26033=CARTESIAN_POINT('Ctrl Pts',(-3.40065621282619,7.50136219214109,-11.9470477325341));
#26034=CARTESIAN_POINT('Ctrl Pts',(-5.82037411761894,6.1495207846071,-11.8417350479192));
#26035=CARTESIAN_POINT('Ctrl Pts',(-8.04628560583682,2.63551264777254,-11.6837660209969));
#26036=CARTESIAN_POINT('Ctrl Pts',(-8.33052461663556,-1.51331821149076,
-11.5257969940746));
#26037=CARTESIAN_POINT('Ctrl Pts',(-6.60497458284972,-5.29754553073239,
-11.3678279671523));
#26038=CARTESIAN_POINT('Ctrl Pts',(-3.28573123451154,-7.80334276912094,
-11.20985894023));
#26039=CARTESIAN_POINT('Ctrl Pts',(0.826234788409155,-8.42652765391102,
-11.0518899133078));
#26040=CARTESIAN_POINT('Ctrl Pts',(4.7388724476258,-7.01653408891042,-10.8939208863855));
#26041=CARTESIAN_POINT('Ctrl Pts',(7.50812913234392,-3.91366458658699,-10.7359518594632));
#26042=CARTESIAN_POINT('Ctrl Pts',(8.46586977500607,0.133491868494349,-10.5779828325409));
#26043=CARTESIAN_POINT('Ctrl Pts',(7.38100727233018,4.14843049732635,-10.4200138056186));
#26044=CARTESIAN_POINT('Ctrl Pts',(4.51529588862971,7.16246272184166,-10.2620447786963));
#26045=CARTESIAN_POINT('Ctrl Pts',(0.560157043790593,8.44837130006937,-10.104075751774));
#26046=CARTESIAN_POINT('Ctrl Pts',(-3.53013313317451,7.69590287683787,-9.94610672485177));
#26047=CARTESIAN_POINT('Ctrl Pts',(-6.76869167449018,5.08660706304677,-9.78813769792948));
#26048=CARTESIAN_POINT('Ctrl Pts',(-8.37413600776358,1.25004196616275,-9.63016867100719));
#26049=CARTESIAN_POINT('Ctrl Pts',(-7.95911317970092,-2.88812681945649,
-9.4721996440849));
#26050=CARTESIAN_POINT('Ctrl Pts',(-5.62375762011129,-6.32946355950556,
-9.31423061716261));
#26051=CARTESIAN_POINT('Ctrl Pts',(-1.93153160038241,-8.2436608785505,-9.15626159024033));
#26052=CARTESIAN_POINT('Ctrl Pts',(2.22672414846207,-8.16887130657559,-8.99829256331803));
#26053=CARTESIAN_POINT('Ctrl Pts',(5.84772767608588,-6.12313971270086,-8.84032353639575));
#26054=CARTESIAN_POINT('Ctrl Pts',(8.05782242151238,-2.60004936964598,-8.68235450947345));
#26055=CARTESIAN_POINT('Ctrl Pts',(8.32376841870599,1.55036712102419,-8.52438548255116));
#26056=CARTESIAN_POINT('Ctrl Pts',(6.581399626523,5.32671923988587,-8.36641645562887));
#26057=CARTESIAN_POINT('Ctrl Pts',(3.25110556474056,7.81786873172712,-8.20844742870658));
#26058=CARTESIAN_POINT('Ctrl Pts',(-0.863598040844137,8.4227642330924,-8.05047840178429));
#26059=CARTESIAN_POINT('Ctrl Pts',(-4.76993728186221,6.99545975817784,-7.89250937486201));
#26060=CARTESIAN_POINT('Ctrl Pts',(-7.52541130072914,3.88032777692923,-7.7345403479397));
#26061=CARTESIAN_POINT('Ctrl Pts',(-8.46519390978181,-0.171029153471515,
-7.57657132101743));
#26062=CARTESIAN_POINT('Ctrl Pts',(-7.36253933495,-4.1811210748754,-7.41860229409512));
#26063=CARTESIAN_POINT('Ctrl Pts',(-4.48349023618117,-7.18241423224846,
-7.26063326717284));
#26064=CARTESIAN_POINT('Ctrl Pts',(-0.52268834243429,-8.45077249712525,
-7.10266424025055));
#26065=CARTESIAN_POINT('Ctrl Pts',(3.56422502820635,-7.68017310025088,-6.94469521332826));
#26066=CARTESIAN_POINT('Ctrl Pts',(6.79118104797183,-5.05654218564124,-6.78672618640598));
#26067=CARTESIAN_POINT('Ctrl Pts',(8.37959684732031,-1.21289553461213,-6.62875715948368));
#26068=CARTESIAN_POINT('Ctrl Pts',(7.94622786899591,2.92339213166767,-6.4707881325614));
#26069=CARTESIAN_POINT('Ctrl Pts',(5.59563508645045,6.35433921669177,-6.3128191056391));
#26070=CARTESIAN_POINT('Ctrl Pts',(1.89495708556707,8.25214496633223,-6.15485007871682));
#26071=CARTESIAN_POINT('Ctrl Pts',(-2.26292613171868,8.15891685359569,-5.99688105179451));
#26072=CARTESIAN_POINT('Ctrl Pts',(-5.87482250865055,6.09714846410646,-5.83891202487224));
#26073=CARTESIAN_POINT('Ctrl Pts',(-8.06927280363647,2.56429236281581,-5.68094299794993));
#26074=CARTESIAN_POINT('Ctrl Pts',(-8.31681166379602,-1.58726262806428,
-5.52297397102766));
#26075=CARTESIAN_POINT('Ctrl Pts',(-6.5577142230679,-5.35585129275224,-5.36500494410535));
#26076=CARTESIAN_POINT('Ctrl Pts',(-3.21640620179515,-7.83220850377189,
-5.20703591718308));
#26077=CARTESIAN_POINT('Ctrl Pts',(0.900939284774293,-8.41885189955573,
-5.04906689026078));
#26078=CARTESIAN_POINT('Ctrl Pts',(4.8009109090025,-6.97423926642352,-4.89109786333849));
#26079=CARTESIAN_POINT('Ctrl Pts',(7.54254415828974,-3.84691909477602,-4.7331288364162));
#26080=CARTESIAN_POINT('Ctrl Pts',(8.46435227254872,0.208565355949563,-4.57515980949391));
#26081=CARTESIAN_POINT('Ctrl Pts',(7.34392626871001,4.21372826143952,-4.41719078257162));
#26082=CARTESIAN_POINT('Ctrl Pts',(4.45159660304068,7.20222511348401,-4.25922175564932));
#26083=CARTESIAN_POINT('Ctrl Pts',(0.485209269400489,8.45300720846675,-4.10125272872704));
#26084=CARTESIAN_POINT('Ctrl Pts',(-3.59824678875397,7.66429246236889,-3.94328370180475));
#26085=CARTESIAN_POINT('Ctrl Pts',(-6.8135369057104,5.02637779479667,-3.78531467488246));
#26086=CARTESIAN_POINT('Ctrl Pts',(-8.3848928992151,1.17572529537953,-3.62734564796017));
#26087=CARTESIAN_POINT('Ctrl Pts',(-7.93318631167529,-2.95859998069199,
-3.46937662103788));
#26088=CARTESIAN_POINT('Ctrl Pts',(-5.56740251784145,-6.37908991203571,
-3.31140759411559));
#26089=CARTESIAN_POINT('Ctrl Pts',(-1.85834531040058,-8.26046679121798,
-3.1534385671933));
#26090=CARTESIAN_POINT('Ctrl Pts',(2.29908361810098,-8.14880196215876,-2.99546954027101));
#26091=CARTESIAN_POINT('Ctrl Pts',(5.90180181930062,-6.07103732381897,-2.83750051334872));
#26092=CARTESIAN_POINT('Ctrl Pts',(8.08056451327072,-2.52848493141107,-2.67953148642643));
#26093=CARTESIAN_POINT('Ctrl Pts',(8.30969136847607,1.62412692305045,-2.52156245950414));
#26094=CARTESIAN_POINT('Ctrl Pts',(6.53389986996386,5.38487802933261,-2.36359343258185));
#26095=CARTESIAN_POINT('Ctrl Pts',(3.1816435919847,7.84639426457055,-2.20562440565956));
#26096=CARTESIAN_POINT('Ctrl Pts',(-0.938262812779821,8.4147740192864,-2.04765537873727));
#26097=CARTESIAN_POINT('Ctrl Pts',(-4.83179013190352,6.95288163445507,-1.88968635181498));
#26098=CARTESIAN_POINT('Ctrl Pts',(-7.55952870061531,3.81343476751294,-1.73171732489269));
#26099=CARTESIAN_POINT('Ctrl Pts',(-8.46334419381849,-0.246097457243576,
-1.5737482979704));
#26100=CARTESIAN_POINT('Ctrl Pts',(-7.32516879282469,-4.24625259000572,
-1.41577927104811));
#26101=CARTESIAN_POINT('Ctrl Pts',(-4.41961543450651,-7.22189437146341,
-1.25781024412582));
#26102=CARTESIAN_POINT('Ctrl Pts',(-0.447720655298665,-8.45507570139511,
-1.09984121720353));
#26103=CARTESIAN_POINT('Ctrl Pts',(3.6321977940243,-7.64826111522011,-0.941872190281239));
#26104=CARTESIAN_POINT('Ctrl Pts',(6.83575878328587,-4.99611456616368,-0.78390316335895));
#26105=CARTESIAN_POINT('Ctrl Pts',(8.39002407208524,-1.1385319368965,-0.625934136436659));
#26106=CARTESIAN_POINT('Ctrl Pts',(7.91998875760714,2.99374965233894,-0.46796510951437));
#26107=CARTESIAN_POINT('Ctrl Pts',(5.53906047283149,6.4037151701039,-0.309996082592078));
#26108=CARTESIAN_POINT('Ctrl Pts',(1.82169699306643,8.26862618377173,-0.152027055669789));
#26109=CARTESIAN_POINT('Ctrl Pts',(-2.33519589571696,8.13852683414694,0.00594197125250266));
#26110=CARTESIAN_POINT('Ctrl Pts',(-5.92866507798216,6.0448068037463,0.163910998174792));
#26111=CARTESIAN_POINT('Ctrl Pts',(-8.09169732813897,2.49262778033376,0.321880025097081));
#26112=CARTESIAN_POINT('Ctrl Pts',(-8.30240767288088,-1.66095928149717,
0.479849052019373));
#26113=CARTESIAN_POINT('Ctrl Pts',(-6.50995703542896,-5.41379887864077,
0.637818078941659));
#26114=CARTESIAN_POINT('Ctrl Pts',(-3.1468184189074,-7.86042573528484,0.795787105863953));
#26115=CARTESIAN_POINT('Ctrl Pts',(0.975567890954294,-8.4105306724155,0.953756132786241));
#26116=CARTESIAN_POINT('Ctrl Pts',(4.86257434335317,-6.93138728227376,1.11172515970853));
#26117=CARTESIAN_POINT('Ctrl Pts',(7.57636459372931,-3.77987545355504,1.26969418663082));
#26118=CARTESIAN_POINT('Ctrl Pts',(8.46216969341154,0.28362471932149,1.42766321355311));
#26119=CARTESIAN_POINT('Ctrl Pts',(7.30626727613884,4.27869342102536,1.5856322404754));
#26120=CARTESIAN_POINT('Ctrl Pts',(4.38754735945002,7.2414216194119,1.74360126739769));
#26121=CARTESIAN_POINT('Ctrl Pts',(0.410223237298467,8.45697793523688,1.90157029431998));
#26122=CARTESIAN_POINT('Ctrl Pts',(-3.66607737641103,7.63207937404152,2.05953932124227));
#26123=CARTESIAN_POINT('Ctrl Pts',(-6.85784624373112,4.96575309483324,2.21750834816456));
#26124=CARTESIAN_POINT('Ctrl Pts',(-8.39499026503231,1.10131619052641,2.37547737508686));
#26125=CARTESIAN_POINT('Ctrl Pts',(-7.90663546630572,-3.02884045543163,
2.53344640200914));
#26126=CARTESIAN_POINT('Ctrl Pts',(-5.51060950873351,-6.42821450666971,
2.69141542893143));
#26127=CARTESIAN_POINT('Ctrl Pts',(-1.78501285421056,-8.27662298354866,
2.84938445585372));
#26128=CARTESIAN_POINT('Ctrl Pts',(2.37126225446112,-8.12809167160846,3.00735348277601));
#26129=CARTESIAN_POINT('Ctrl Pts',(5.9554117564608,-6.01845741968086,3.1653225096983));
#26130=CARTESIAN_POINT('Ctrl Pts',(8.10267102932754,-2.45672161467252,3.32329153662059));
#26131=CARTESIAN_POINT('Ctrl Pts',(8.29496072023576,1.69775897913956,3.48126056354288));
#26132=CARTESIAN_POINT('Ctrl Pts',(6.48588619027077,5.4426132719823,3.63922959046517));
#26133=CARTESIAN_POINT('Ctrl Pts',(3.11193136735919,7.87430264000241,3.79719861738746));
#26134=CARTESIAN_POINT('Ctrl Pts',(-1.01285378573731,8.40612194238345,3.95516764430975));
#26135=CARTESIAN_POINT('Ctrl Pts',(-4.89326293801619,6.9097566325407,4.11313667123204));
#26136=CARTESIAN_POINT('Ctrl Pts',(-7.59305150657372,3.74624181280671,4.27110569815433));
#26137=CARTESIAN_POINT('Ctrl Pts',(-8.46082879442303,-0.321146404253918,
4.42907472507662));
#26138=CARTESIAN_POINT('Ctrl Pts',(-7.2872220903285,-4.31105011658773,4.58704375199891));
#26139=CARTESIAN_POINT('Ctrl Pts',(-4.35539300845213,-7.26080647334918,
4.7450127789212));
#26140=CARTESIAN_POINT('Ctrl Pts',(-0.37271775274243,-8.45871387258687,
4.90298180584349));
#26141=CARTESIAN_POINT('Ctrl Pts',(3.69988486971213,-7.61574755702801,5.06095083276578));
#26142=CARTESIAN_POINT('Ctrl Pts',(6.87979885272231,-4.93529397782784,5.21891985968807));
#26143=CARTESIAN_POINT('Ctrl Pts',(8.39979138040202,-1.06407878807301,5.37688888661037));
#26144=CARTESIAN_POINT('Ctrl Pts',(7.8931267003478,3.06387169995084,5.53485791353265));
#26145=CARTESIAN_POINT('Ctrl Pts',(5.4820501850021,6.45258743998261,5.69282694045494));
#26146=CARTESIAN_POINT('Ctrl Pts',(1.74829361518324,8.28445703330112,5.85079596737723));
#26147=CARTESIAN_POINT('Ctrl Pts',(-2.40728198513118,8.11749667973851,6.00876499429952));
#26148=CARTESIAN_POINT('Ctrl Pts',(-5.98204132879465,5.99198968975211,6.1667340212218));
#26149=CARTESIAN_POINT('Ctrl Pts',(-8.11348540105156,2.42076714047972,6.32470304814411));
#26150=CARTESIAN_POINT('Ctrl Pts',(-8.28735065697621,-1.73452529235496,
6.48267207506639));
#26151=CARTESIAN_POINT('Ctrl Pts',(-6.46168780781411,-5.47132064275613,
6.64064110198868));
#26152=CARTESIAN_POINT('Ctrl Pts',(-3.07698312335276,-7.88802470585037,
6.79861012891098));
#26153=CARTESIAN_POINT('Ctrl Pts',(1.0501197639459,-8.40154791588267,6.95657915583325));
#26154=CARTESIAN_POINT('Ctrl Pts',(4.9238553124377,-6.88799011059706,7.11454818275556));
#26155=CARTESIAN_POINT('Ctrl Pts',(7.60958911102027,-3.71253450663348,7.27251720967785));
#26156=CARTESIAN_POINT('Ctrl Pts',(8.45932152322004,0.358661774221112,7.43048623660013));
#26157=CARTESIAN_POINT('Ctrl Pts',(7.2680336098949,4.34332204043724,7.58845526352242));
#26158=CARTESIAN_POINT('Ctrl Pts',(4.32315301378977,7.28004855209397,7.74642429044472));
#26159=CARTESIAN_POINT('Ctrl Pts',(0.335204939132236,8.46028347931194,7.90439331736699));
#26160=CARTESIAN_POINT('Ctrl Pts',(-3.73361960914439,7.59926598532158,8.0623623442893));
#26161=CARTESIAN_POINT('Ctrl Pts',(-6.9016161785849,4.90473781409765,8.22033137121157));
#26162=CARTESIAN_POINT('Ctrl Pts',(-8.40442732379069,1.02682046175124,8.37830039813387));
#26163=CARTESIAN_POINT('Ctrl Pts',(-7.87946272535832,-3.0988426970199,8.53626942505616));
#26164=CARTESIAN_POINT('Ctrl Pts',(-5.45338306324019,-6.47683349083296,
8.69423845197845));
#26165=CARTESIAN_POINT('Ctrl Pts',(-1.71153999799109,-8.29212817887424,
8.85220747890073));
#26166=CARTESIAN_POINT('Ctrl Pts',(2.44325437937582,-8.10674206708394,9.01017650582304));
#26167=CARTESIAN_POINT('Ctrl Pts',(6.00855327147267,-5.96540413401097,9.16814553274532));
#26168=CARTESIAN_POINT('Ctrl Pts',(8.12414023041075,-2.38476506554547,9.32611455966761));
#26169=CARTESIAN_POINT('Ctrl Pts',(8.2795776332277,1.77125749970778,9.48408358658991));
#26170=CARTESIAN_POINT('Ctrl Pts',(6.43736236295422,5.49992042349329,9.64205261351219));
#26171=CARTESIAN_POINT('Ctrl Pts',(3.04197437592444,7.90159166877402,9.80002164043448));
#26172=CARTESIAN_POINT('Ctrl Pts',(-1.08736509632437,8.39680867164209,9.95799066735678));
#26173=CARTESIAN_POINT('Ctrl Pts',(-4.95435085818707,6.86608816623656,10.1159596942791));
#26174=CARTESIAN_POINT('Ctrl Pts',(-7.62597709521529,3.67875415554537,10.2739287212014));
#26175=CARTESIAN_POINT('Ctrl Pts',(-8.45764788353322,-0.396170009359619,
10.4318977481237));
#26176=CARTESIAN_POINT('Ctrl Pts',(-7.24870226247802,-4.37550871757833,
10.589866775046));
#26177=CARTESIAN_POINT('Ctrl Pts',(-4.29082791168611,-7.29914716729561,
10.7478358019683));
#26178=CARTESIAN_POINT('Ctrl Pts',(-0.297685723949315,-8.46168732661545,
10.9058048288906));
#26179=CARTESIAN_POINT('Ctrl Pts',(3.76728130007181,-7.58263381362094,11.0637738558128));
#26180=CARTESIAN_POINT('Ctrl Pts',(6.92329707614913,-4.87408747579489,11.2217428827352));
#26181=CARTESIAN_POINT('Ctrl Pts',(8.40889939502786,-0.989537532666886,
11.3797119096574));
#26182=CARTESIAN_POINT('Ctrl Pts',(7.86564110829628,3.13374419045154,11.5376809365797));
#26183=CARTESIAN_POINT('Ctrl Pts',(5.42461395487494,6.50096882535833,11.695649963502));
#26184=CARTESIAN_POINT('Ctrl Pts',(1.67474253093863,8.29960394072526,11.8536189904243));
#26185=CARTESIAN_POINT('Ctrl Pts',(-2.4791589111201,8.09589087029261,12.0115880173466));
#26186=CARTESIAN_POINT('Ctrl Pts',(-6.03498574071721,5.93857891308519,12.1695570442689));
#26187=CARTESIAN_POINT('Ctrl Pts',(-8.1345583276468,2.34895716891092,12.3275260711912));
#26188=CARTESIAN_POINT('Ctrl Pts',(-8.27181774175635,-1.80868950910794,
12.4855039120797));
#26189=CARTESIAN_POINT('Ctrl Pts',(-7.03199329881568,-4.28796079991923,
12.5908254106607));
#26190=CARTESIAN_POINT('Ctrl Pts',(-6.15407324826529,-5.30616618526941,
12.6434905669344));
#26191=CARTESIAN_POINT('Ctrl Pts',(-2.00604317752182,7.49003302766729,-12.214330565978));
#26192=CARTESIAN_POINT('Ctrl Pts',(-3.24508022951926,7.15818378005051,-12.1616742236706));
#26193=CARTESIAN_POINT('Ctrl Pts',(-5.55409891368994,5.86818751153965,-12.0563615390557));
#26194=CARTESIAN_POINT('Ctrl Pts',(-7.67817759469036,2.51494107392495,-11.8983925121334));
#26195=CARTESIAN_POINT('Ctrl Pts',(-7.94941300829144,-1.44408570044746,
-11.7404234852111));
#26196=CARTESIAN_POINT('Ctrl Pts',(-6.30280483938424,-5.05518911377136,
-11.5824544582888));
#26197=CARTESIAN_POINT('Ctrl Pts',(-3.13541293248401,-7.44634910424883,
-11.4244854313665));
#26198=CARTESIAN_POINT('Ctrl Pts',(0.78843552802984,-8.04102402061944,-11.2665164044443));
#26199=CARTESIAN_POINT('Ctrl Pts',(4.52207466076785,-6.69553598678779,-11.108547377522));
#26200=CARTESIAN_POINT('Ctrl Pts',(7.16464114077509,-3.73461907940069,-10.9505783505997));
#26201=CARTESIAN_POINT('Ctrl Pts',(8.07856628639489,0.12738477403824,-10.7926093236774));
#26202=CARTESIAN_POINT('Ctrl Pts',(7.04333495489414,3.95864472851865,-10.6346402967551));
#26203=CARTESIAN_POINT('Ctrl Pts',(4.30872646383876,6.83478855805914,-10.4766712698328));
#26204=CARTESIAN_POINT('Ctrl Pts',(0.534530524248469,8.06186834590634,-10.3187022429105));
#26205=CARTESIAN_POINT('Ctrl Pts',(-3.36863373452123,7.34382445944808,-10.1607332159882));
#26206=CARTESIAN_POINT('Ctrl Pts',(-6.45903206850345,4.85390083048357,-10.0027641890659));
#26207=CARTESIAN_POINT('Ctrl Pts',(-7.99102923006582,1.19285403069102,-9.84479516214361));
#26208=CARTESIAN_POINT('Ctrl Pts',(-7.59499320352905,-2.75599844724488,
-9.68682613522134));
#26209=CARTESIAN_POINT('Ctrl Pts',(-5.36647738745246,-6.0398981181765,-9.52885710829904));
#26210=CARTESIAN_POINT('Ctrl Pts',(-1.84316632344425,-7.86652318306926,
-9.37088808137676));
#26211=CARTESIAN_POINT('Ctrl Pts',(2.12485416300348,-7.79515514519626,-9.21291905445446));
#26212=CARTESIAN_POINT('Ctrl Pts',(5.5802010793406,-5.84301334234443,-9.05495002753217));
#26213=CARTESIAN_POINT('Ctrl Pts',(7.68918661474923,-2.48110019865847,-8.89698100060988));
#26214=CARTESIAN_POINT('Ctrl Pts',(7.9429658983939,1.47943966636695,-8.73901197368759));
#26215=CARTESIAN_POINT('Ctrl Pts',(6.28030840931315,5.08302816037614,-8.5810429467653));
#26216=CARTESIAN_POINT('Ctrl Pts',(3.10237134598554,7.46021052131602,-8.42307391984302));
#26217=CARTESIAN_POINT('Ctrl Pts',(-0.824089456036443,8.03743277183402,
-8.26510489292072));
#26218=CARTESIAN_POINT('Ctrl Pts',(-4.55171831572882,6.67542578165953,-8.10713586599843));
#26219=CARTESIAN_POINT('Ctrl Pts',(-7.18113267048003,3.70280738919583,-7.94916683907614));
#26220=CARTESIAN_POINT('Ctrl Pts',(-8.07792134120202,-0.163204772804889,
-7.79119781215386));
#26221=CARTESIAN_POINT('Ctrl Pts',(-7.0257119037176,-3.98983975096633,-7.63322878523156));
#26222=CARTESIAN_POINT('Ctrl Pts',(-4.27837588221913,-6.85382731055814,
-7.47525975830927));
#26223=CARTESIAN_POINT('Ctrl Pts',(-0.498775971483477,-8.06415969104843,
-7.31729073138698));
#26224=CARTESIAN_POINT('Ctrl Pts',(3.401165965841,-7.32881430146016,-7.15932170446469));
#26225=CARTESIAN_POINT('Ctrl Pts',(6.48049257985542,-4.82521138551596,-7.0013526775424));
#26226=CARTESIAN_POINT('Ctrl Pts',(7.99624024269784,-1.15740700427081,-6.84338365062012));
#26227=CARTESIAN_POINT('Ctrl Pts',(7.5826973804869,2.78965041330152,-6.68541462369781));
#26228=CARTESIAN_POINT('Ctrl Pts',(5.33964142630988,6.0636357435874,-6.52744559677554));
#26229=CARTESIAN_POINT('Ctrl Pts',(1.80826504924783,7.8746191339102,-6.36947656985323));
#26230=CARTESIAN_POINT('Ctrl Pts',(-2.15939994851756,7.78565609661882,-6.21150754293096));
#26231=CARTESIAN_POINT('Ctrl Pts',(-5.60605635549174,5.81821116250748,-6.05353851600865));
#26232=CARTESIAN_POINT('Ctrl Pts',(-7.70011315548899,2.44697903242775,-5.89556948908638));
#26233=CARTESIAN_POINT('Ctrl Pts',(-7.93632740675959,-1.51464724777502,
-5.73760046216408));
#26234=CARTESIAN_POINT('Ctrl Pts',(-6.25770658493865,-5.11082745641947,
-5.57963143524179));
#26235=CARTESIAN_POINT('Ctrl Pts',(-3.06925943768785,-7.47389426581884,
-5.4216624083195));
#26236=CARTESIAN_POINT('Ctrl Pts',(0.859722382401179,-8.0336994229106,-5.26369338139721));
#26237=CARTESIAN_POINT('Ctrl Pts',(4.58127493621,-6.65517610220269,-5.10572435447492));
#26238=CARTESIAN_POINT('Ctrl Pts',(7.19748172015326,-3.67092711457684,-4.94775532755263));
#26239=CARTESIAN_POINT('Ctrl Pts',(8.07711820787286,0.199023738595472,-4.78978630063034));
#26240=CARTESIAN_POINT('Ctrl Pts',(7.00795036315426,4.02095519746761,-4.63181727370805));
#26241=CARTESIAN_POINT('Ctrl Pts',(4.24794134491971,6.87273186750345,-4.47384824678576));
#26242=CARTESIAN_POINT('Ctrl Pts',(0.463011521532918,8.06629216699988,-4.31587921986347));
#26243=CARTESIAN_POINT('Ctrl Pts',(-3.43363127124591,7.31366018390231,-4.15791019294118));
#26244=CARTESIAN_POINT('Ctrl Pts',(-6.50182568365104,4.79642697973099,-3.99994116601889));
#26245=CARTESIAN_POINT('Ctrl Pts',(-8.00129400650773,1.12193725934179,-3.8419721390966));
#26246=CARTESIAN_POINT('Ctrl Pts',(-7.57025245892629,-2.82324754504386,
-3.68400311217431));
#26247=CARTESIAN_POINT('Ctrl Pts',(-5.31270046418729,-6.08725412401191,
-3.52603408525202));
#26248=CARTESIAN_POINT('Ctrl Pts',(-1.77332821931713,-7.88256024518995,
-3.36806505832973));
#26249=CARTESIAN_POINT('Ctrl Pts',(2.19390327283648,-7.77600394945329,-3.21009603140744));
#26250=CARTESIAN_POINT('Ctrl Pts',(5.6318013947187,-5.79329457587998,-3.05212700448515));
#26251=CARTESIAN_POINT('Ctrl Pts',(7.71088828281686,-2.41280974848687,-2.89415797756286));
#26252=CARTESIAN_POINT('Ctrl Pts',(7.92953285649486,1.54982504504355,-2.73618895064057));
#26253=CARTESIAN_POINT('Ctrl Pts',(6.23498171020852,5.13852625427182,-2.57821992371828));
#26254=CARTESIAN_POINT('Ctrl Pts',(3.0360871759941,7.48743104490719,-2.42025089679599));
#26255=CARTESIAN_POINT('Ctrl Pts',(-0.895338403323793,8.02980810082093,
-2.2622818698737));
#26256=CARTESIAN_POINT('Ctrl Pts',(-4.61074147133374,6.63479555653366,-2.10431284295141));
#26257=CARTESIAN_POINT('Ctrl Pts',(-7.21368923983733,3.63897465552193,-1.94634381602912));
#26258=CARTESIAN_POINT('Ctrl Pts',(-8.0761562475474,-0.234838790826315,
-1.78837478910683));
#26259=CARTESIAN_POINT('Ctrl Pts',(-6.99005101951537,-4.05199157662599,
-1.63040576218454));
#26260=CARTESIAN_POINT('Ctrl Pts',(-4.21742327686693,-6.8915012802884,-1.47243673526225));
#26261=CARTESIAN_POINT('Ctrl Pts',(-0.42723796700686,-8.06826602883319,
-1.31446770833996));
#26262=CARTESIAN_POINT('Ctrl Pts',(3.46602905834345,-7.29836225184764,-1.15649868141767));
#26263=CARTESIAN_POINT('Ctrl Pts',(6.52303093671688,-4.76754825786905,-0.998529654495381));
#26264=CARTESIAN_POINT('Ctrl Pts',(8.00619043431256,-1.08644545284059,-0.840560627573093));
#26265=CARTESIAN_POINT('Ctrl Pts',(7.55765867728407,2.85678916095475,-0.682591600650801));
#26266=CARTESIAN_POINT('Ctrl Pts',(5.28565503407912,6.11075280576706,-0.524622573728512));
#26267=CARTESIAN_POINT('Ctrl Pts',(1.7383565189795,7.89034635522403,-0.366653546806221));
#26268=CARTESIAN_POINT('Ctrl Pts',(-2.22836345663647,7.76619889634581,-0.20868451988393));
#26269=CARTESIAN_POINT('Ctrl Pts',(-5.65743569121687,5.76826407095074,-0.0507154929616409));
#26270=CARTESIAN_POINT('Ctrl Pts',(-7.7215117846256,2.37859301948939,0.107253533960649));
#26271=CARTESIAN_POINT('Ctrl Pts',(-7.92258238132345,-1.58497236683139,
0.265222560882939));
#26272=CARTESIAN_POINT('Ctrl Pts',(-6.21213423192041,-5.16612400906892,
0.423191587805229));
#26273=CARTESIAN_POINT('Ctrl Pts',(-3.00285521322863,-7.50082059249928,
0.581160614727519));
#26274=CARTESIAN_POINT('Ctrl Pts',(0.930936818473215,-8.0257588820302,0.739129641649809));
#26275=CARTESIAN_POINT('Ctrl Pts',(4.64011734166718,-6.61428454543915,0.897098668572098));
#26276=CARTESIAN_POINT('Ctrl Pts',(7.22975491083474,-3.60695064032443,1.05506769549439));
#26277=CARTESIAN_POINT('Ctrl Pts',(8.0750354791393,0.270649225229449,1.21303672241668));
#26278=CARTESIAN_POINT('Ctrl Pts',(6.97201422477151,4.08294827815141,1.37100574933897));
#26279=CARTESIAN_POINT('Ctrl Pts',(4.18682227816202,6.91013517983273,1.52897477626126));
#26280=CARTESIAN_POINT('Ctrl Pts',(0.391456011350326,8.07008123773568,1.68694380318355));
#26281=CARTESIAN_POINT('Ctrl Pts',(-3.4983586900695,7.28292080611145,1.84491283010584));
#26282=CARTESIAN_POINT('Ctrl Pts',(-6.54410792207659,4.73857578779637,2.00288185702813));
#26283=CARTESIAN_POINT('Ctrl Pts',(-8.01092942982988,1.05093228267159,2.16085088395042));
#26284=CARTESIAN_POINT('Ctrl Pts',(-7.54491628320208,-2.89027460147783,
2.31881991087271));
#26285=CARTESIAN_POINT('Ctrl Pts',(-5.25850566780182,-6.13413132677903,
2.476788937795));
#26286=CARTESIAN_POINT('Ctrl Pts',(-1.70335063591225,-7.89797731090771,
2.63475796471729));
#26287=CARTESIAN_POINT('Ctrl Pts',(2.26277982229849,-7.75624113010126,2.79272699163958));
#26288=CARTESIAN_POINT('Ctrl Pts',(5.68295874091796,-5.74312013991523,2.95069601856187));
#26289=CARTESIAN_POINT('Ctrl Pts',(7.73198345201655,-2.34432951826698,3.10866504548416));
#26290=CARTESIAN_POINT('Ctrl Pts',(7.91547611791824,1.62008852200791,3.26663407240645));
#26291=CARTESIAN_POINT('Ctrl Pts',(6.18916459934302,5.19362017813345,3.42460309932874));
#26292=CARTESIAN_POINT('Ctrl Pts',(2.96956420285885,7.51406264530547,3.58257212625103));
#26293=CARTESIAN_POINT('Ctrl Pts',(-0.966516927848558,8.02155184616155,
3.74054115317332));
#26294=CARTESIAN_POINT('Ctrl Pts',(-4.66940196956842,6.59364347224404,3.89851018009561));
#26295=CARTESIAN_POINT('Ctrl Pts',(-7.24567841723297,3.57485569869889,4.05647920701789));
#26296=CARTESIAN_POINT('Ctrl Pts',(-8.07375592468714,-0.306454337634883,
4.21444823394019));
#26297=CARTESIAN_POINT('Ctrl Pts',(-6.95384033359499,-4.11382469331681,
4.37241726086248));
#26298=CARTESIAN_POINT('Ctrl Pts',(-4.15613895053757,-6.92863319972275,
4.53038628778477));
#26299=CARTESIAN_POINT('Ctrl Pts',(-0.355666358173307,-8.07173775801342,
4.68835531470706));
#26300=CARTESIAN_POINT('Ctrl Pts',(3.53061953069998,-7.26733615033155,4.84632434162935));
#26301=CARTESIAN_POINT('Ctrl Pts',(6.56505622527614,-4.70951013922241,5.00429336855164));
#26302=CARTESIAN_POINT('Ctrl Pts',(8.01551089987296,-1.01539844715936,5.16226239547394));
#26303=CARTESIAN_POINT('Ctrl Pts',(7.53202552724446,2.92370320816144,5.32023142239622));
#26304=CARTESIAN_POINT('Ctrl Pts',(5.23125289921567,6.15738922733681,5.47820044931851));
#26305=CARTESIAN_POINT('Ctrl Pts',(1.66831125846471,7.90545296218727,5.6361694762408));
#26306=CARTESIAN_POINT('Ctrl Pts',(-2.29715169306541,7.74613084652733,5.79413850316309));
#26307=CARTESIAN_POINT('Ctrl Pts',(-5.70837004194135,5.71786327719911,5.95210753008538));
#26308=CARTESIAN_POINT('Ctrl Pts',(-7.74230307907673,2.31001991857098,6.11007655700767));
#26309=CARTESIAN_POINT('Ctrl Pts',(-7.90821420601554,-1.65517282005532,
6.26804558392996));
#26310=CARTESIAN_POINT('Ctrl Pts',(-6.1660732641471,-5.22101422078565,6.42601461085225));
#26311=CARTESIAN_POINT('Ctrl Pts',(-2.93621479951312,-7.52715694293644,
6.58398363777455));
#26312=CARTESIAN_POINT('Ctrl Pts',(1.00207803180911,-8.01718707594133,6.74195266469683));
#26313=CARTESIAN_POINT('Ctrl Pts',(4.69859477918996,-6.5728727428306,6.89992169161912));
#26314=CARTESIAN_POINT('Ctrl Pts',(7.26145944591522,-3.54269046175417,7.05789071854142));
#26315=CARTESIAN_POINT('Ctrl Pts',(8.07231760935175,0.342253423977237,7.2158597454637));
#26316=CARTESIAN_POINT('Ctrl Pts',(6.93552970335405,4.14462021497455,7.373828772386));
#26317=CARTESIAN_POINT('Ctrl Pts',(4.12537389734458,6.94699497621579,7.53179779930828));
#26318=CARTESIAN_POINT('Ctrl Pts',(0.319869711237644,8.07323555709481,7.68976682623056));
#26319=CARTESIAN_POINT('Ctrl Pts',(-3.56281094586469,7.25160859095806,7.84773585315286));
#26320=CARTESIAN_POINT('Ctrl Pts',(-6.58587543438956,4.68035188369609,8.00570488007515));
#26321=CARTESIAN_POINT('Ctrl Pts',(-8.01993475435698,0.979844645020895,
8.16367390699745));
#26322=CARTESIAN_POINT('Ctrl Pts',(-7.51898666288417,-2.9570743236442,8.32164293391973));
#26323=CARTESIAN_POINT('Ctrl Pts',(-5.20389726423089,-6.18052605015402,
8.47961196084203));
#26324=CARTESIAN_POINT('Ctrl Pts',(-1.63323907561256,-7.91277316196025,
8.6375809877643));
#26325=CARTESIAN_POINT('Ctrl Pts',(2.33147839299217,-7.73586824463014,8.79555001468662));
#26326=CARTESIAN_POINT('Ctrl Pts',(5.73366909472596,-5.6924939790616,8.95351904160888));
#26327=CARTESIAN_POINT('Ctrl Pts',(7.75247046264582,-2.27566489581091,9.1114880685312));
#26328=CARTESIAN_POINT('Ctrl Pts',(7.90079678887271,1.69022457254288,9.26945709545346));
#26329=CARTESIAN_POINT('Ctrl Pts',(6.142860679502,5.24830559551758,9.42742612237578));
#26330=CARTESIAN_POINT('Ctrl Pts',(2.90280766070521,7.54010323341772,9.58539514929804));
#26331=CARTESIAN_POINT('Ctrl Pts',(-1.03761943446175,8.01266464649669,9.74336417622037));
#26332=CARTESIAN_POINT('Ctrl Pts',(-4.7276951899361,6.55197278641507,9.90133320314262));
#26333=CARTESIAN_POINT('Ctrl Pts',(-7.27709769929478,3.51045552161269,10.0593022300649));
#26334=CARTESIAN_POINT('Ctrl Pts',(-8.07072053669306,-0.378045701900852,
10.2172712569872));
#26335=CARTESIAN_POINT('Ctrl Pts',(-6.91708274212466,-4.17533438985954,
10.3752402839095));
#26336=CARTESIAN_POINT('Ctrl Pts',(-4.09452763027467,-6.9652198524524,10.5332093108318));
#26337=CARTESIAN_POINT('Ctrl Pts',(-0.284066955593615,-8.0745751800513,
10.6911783377541));
#26338=CARTESIAN_POINT('Ctrl Pts',(3.59493265440695,-7.23573732136131,10.8491473646764));
#26339=CARTESIAN_POINT('Ctrl Pts',(6.60656445663723,-4.65110376197204,11.0071163915987));
#26340=CARTESIAN_POINT('Ctrl Pts',(8.02420223364584,-0.944267365667029,
11.1650854185209));
#26341=CARTESIAN_POINT('Ctrl Pts',(7.50579736838894,2.99037911519842,11.3230544454432));
#26342=CARTESIAN_POINT('Ctrl Pts',(5.17644430840876,6.20355722178662,11.4810234723655));
#26343=CARTESIAN_POINT('Ctrl Pts',(1.59812504897912,7.91990691658437,11.6389924992878));
#26344=CARTESIAN_POINT('Ctrl Pts',(-2.36574033504738,7.72551347720574,11.7969615262101));
#26345=CARTESIAN_POINT('Ctrl Pts',(-5.75889230989227,5.66689598013705,11.9549305531324));
#26346=CARTESIAN_POINT('Ctrl Pts',(-7.76241194430529,2.24149516792393,12.1128995800547));
#26347=CARTESIAN_POINT('Ctrl Pts',(-7.89339190322096,-1.72594411196516,
12.2708774209432));
#26348=CARTESIAN_POINT('Ctrl Pts',(-6.71028795619838,-4.09179168546631,
12.3761989195243));
#26349=CARTESIAN_POINT('Ctrl Pts',(-5.87253170539172,-5.06341538360071,
12.428864075798));
#26350=CARTESIAN_POINT('Ctrl Pts',(-1.90986924103173,7.13094506346825,-12.4289570571144));
#26351=CARTESIAN_POINT('Ctrl Pts',(-3.08950424621235,6.81500536795992,-12.3763007148069));
#26352=CARTESIAN_POINT('Ctrl Pts',(-5.28782370976095,5.58685423847219,-12.2709880301921));
#26353=CARTESIAN_POINT('Ctrl Pts',(-7.31006958354388,2.39436950007738,-12.1130190032698));
#26354=CARTESIAN_POINT('Ctrl Pts',(-7.56830139994735,-1.37485318940416,
-11.9550499763475));
#26355=CARTESIAN_POINT('Ctrl Pts',(-6.00063509591875,-4.81283269681031,
-11.7970809494252));
#26356=CARTESIAN_POINT('Ctrl Pts',(-2.98509463045649,-7.08935543937673,
-11.6391119225029));
#26357=CARTESIAN_POINT('Ctrl Pts',(0.750636267650531,-7.65552038732784,
-11.4811428955806));
#26358=CARTESIAN_POINT('Ctrl Pts',(4.30527687390991,-6.37453788466516,-11.3231738686583));
#26359=CARTESIAN_POINT('Ctrl Pts',(6.82115314920626,-3.55557357221439,-11.1652048417361));
#26360=CARTESIAN_POINT('Ctrl Pts',(7.69126279778371,0.121277679582131,-11.0072358148138));
#26361=CARTESIAN_POINT('Ctrl Pts',(6.70566263745811,3.76885895971093,-10.8492667878915));
#26362=CARTESIAN_POINT('Ctrl Pts',(4.10215703904782,6.50711439427663,-10.6912977609692));
#26363=CARTESIAN_POINT('Ctrl Pts',(0.508904004706356,7.67536539174329,-10.5333287340469));
#26364=CARTESIAN_POINT('Ctrl Pts',(-3.20713433586796,6.9917460420583,-10.3753597071246));
#26365=CARTESIAN_POINT('Ctrl Pts',(-6.14937246251668,4.62119459792037,-10.2173906802023));
#26366=CARTESIAN_POINT('Ctrl Pts',(-7.60792245236808,1.13566609521927,-10.05942165328));
#26367=CARTESIAN_POINT('Ctrl Pts',(-7.23087322735717,-2.62387007503327,
-9.90145262635776));
#26368=CARTESIAN_POINT('Ctrl Pts',(-5.10919715479364,-5.75033267684747,
-9.74348359943547));
#26369=CARTESIAN_POINT('Ctrl Pts',(-1.75480104650608,-7.48938548758801,
-9.58551457251319));
#26370=CARTESIAN_POINT('Ctrl Pts',(2.0229841775449,-7.42143898381695,-9.42754554559091));
#26371=CARTESIAN_POINT('Ctrl Pts',(5.3126744825953,-5.56288697198798,-9.2695765186686));
#26372=CARTESIAN_POINT('Ctrl Pts',(7.32055080798609,-2.36215102767096,-9.11160749174632));
#26373=CARTESIAN_POINT('Ctrl Pts',(7.56216337808177,1.40851221170973,-8.95363846482402));
#26374=CARTESIAN_POINT('Ctrl Pts',(5.97921719210332,4.8393370808664,-8.79566943790175));
#26375=CARTESIAN_POINT('Ctrl Pts',(2.95363712723051,7.10255231090489,-8.63770041097944));
#26376=CARTESIAN_POINT('Ctrl Pts',(-0.784580871228743,7.65210131057567,
-8.47973138405716));
#26377=CARTESIAN_POINT('Ctrl Pts',(-4.33349934959543,6.3553918051412,-8.32176235713486));
#26378=CARTESIAN_POINT('Ctrl Pts',(-6.83685404023092,3.52528700146243,-8.16379333021257));
#26379=CARTESIAN_POINT('Ctrl Pts',(-7.69064877262224,-0.155380392138265,
-8.00582430329029));
#26380=CARTESIAN_POINT('Ctrl Pts',(-6.68888447248521,-3.79855842705726,
-7.84785527636799));
#26381=CARTESIAN_POINT('Ctrl Pts',(-4.0732615282571,-6.52524038886781,-7.68988624944571));
#26382=CARTESIAN_POINT('Ctrl Pts',(-0.474863600532664,-7.67754688497162,
-7.53191722252343));
#26383=CARTESIAN_POINT('Ctrl Pts',(3.23810690347566,-6.97745550266942,-7.37394819560114));
#26384=CARTESIAN_POINT('Ctrl Pts',(6.16980411173903,-4.5938805853907,-7.21597916867884));
#26385=CARTESIAN_POINT('Ctrl Pts',(7.61288363807535,-1.10191847392946,-7.05801014175656));
#26386=CARTESIAN_POINT('Ctrl Pts',(7.21916689197791,2.65590869493537,-6.90004111483424));
#26387=CARTESIAN_POINT('Ctrl Pts',(5.08364776616928,5.77293227048303,-6.74207208791196));
#26388=CARTESIAN_POINT('Ctrl Pts',(1.72157301292862,7.49709330148819,-6.58410306098967));
#26389=CARTESIAN_POINT('Ctrl Pts',(-2.05587376531645,7.41239533964198,-6.42613403406738));
#26390=CARTESIAN_POINT('Ctrl Pts',(-5.33729020233292,5.53927386090847,-6.26816500714509));
#26391=CARTESIAN_POINT('Ctrl Pts',(-7.3309535073415,2.32966570203969,-6.11019598022282));
#26392=CARTESIAN_POINT('Ctrl Pts',(-7.55584314972316,-1.44203186748576,
-5.95222695330051));
#26393=CARTESIAN_POINT('Ctrl Pts',(-5.95769894680941,-4.8658036200867,-5.79425792637823));
#26394=CARTESIAN_POINT('Ctrl Pts',(-2.92211267358056,-7.11558002786579,
-5.63628889945594));
#26395=CARTESIAN_POINT('Ctrl Pts',(0.818505480028056,-7.64854694626547,
-5.47831987253366));
#26396=CARTESIAN_POINT('Ctrl Pts',(4.36163896341749,-6.33611293798186,-5.32035084561134));
#26397=CARTESIAN_POINT('Ctrl Pts',(6.85241928201679,-3.49493513437767,-5.16238181868907));
#26398=CARTESIAN_POINT('Ctrl Pts',(7.689884143197,0.189482121241377,-5.00441279176677));
#26399=CARTESIAN_POINT('Ctrl Pts',(6.67197445759853,3.82818213349571,-4.84644376484448));
#26400=CARTESIAN_POINT('Ctrl Pts',(4.04428608679874,6.5432386215229,-4.68847473792219));
#26401=CARTESIAN_POINT('Ctrl Pts',(0.440813773665348,7.679577125533,-4.5305057109999));
#26402=CARTESIAN_POINT('Ctrl Pts',(-3.26901575373787,6.96302790543571,-4.37253668407762));
#26403=CARTESIAN_POINT('Ctrl Pts',(-6.19011446159165,4.56647616466531,-4.21456765715532));
#26404=CARTESIAN_POINT('Ctrl Pts',(-7.61769511380036,1.06814922330403,-4.05659863023303));
#26405=CARTESIAN_POINT('Ctrl Pts',(-7.20731860617729,-2.68789510939572,
-3.89862960331074));
#26406=CARTESIAN_POINT('Ctrl Pts',(-5.05799841053314,-5.7954183359881,-3.74066057638846));
#26407=CARTESIAN_POINT('Ctrl Pts',(-1.68831112823367,-7.50465369916194,
-3.58269154946616));
#26408=CARTESIAN_POINT('Ctrl Pts',(2.088722927572,-7.4032059367478,-3.42472252254387));
#26409=CARTESIAN_POINT('Ctrl Pts',(5.36180097013677,-5.515551827941,-3.26675349562158));
#26410=CARTESIAN_POINT('Ctrl Pts',(7.34121205236302,-2.29713456556267,-3.10878446869929));
#26411=CARTESIAN_POINT('Ctrl Pts',(7.54937434451365,1.47552316703666,-2.950815441777));
#26412=CARTESIAN_POINT('Ctrl Pts',(5.93606355045319,4.89217447921103,-2.79284641485471));
#26413=CARTESIAN_POINT('Ctrl Pts',(2.89053076000349,7.12846782524383,-2.63487738793242));
#26414=CARTESIAN_POINT('Ctrl Pts',(-0.852413993867771,7.64484218235544,
-2.47690836101013));
#26415=CARTESIAN_POINT('Ctrl Pts',(-4.38969281076395,6.31670947861226,-2.31893933408784));
#26416=CARTESIAN_POINT('Ctrl Pts',(-6.86784977905936,3.46451454353091,-2.16097030716555));
#26417=CARTESIAN_POINT('Ctrl Pts',(-7.6889683012763,-0.223580124409053,
-2.00300128024326));
#26418=CARTESIAN_POINT('Ctrl Pts',(-6.65493324620604,-3.85773056324626,
-1.84503225332097));
#26419=CARTESIAN_POINT('Ctrl Pts',(-4.01523111922735,-6.56110818911341,
-1.68706322639868));
#26420=CARTESIAN_POINT('Ctrl Pts',(-0.406755278715055,-7.68145635627126,
-1.52909419947639));
#26421=CARTESIAN_POINT('Ctrl Pts',(3.2998603226626,-6.94846338847517,-1.3711251725541));
#26422=CARTESIAN_POINT('Ctrl Pts',(6.2103030901479,-4.5389819495744,-1.21315614563181));
#26423=CARTESIAN_POINT('Ctrl Pts',(7.62235679653987,-1.03435896878468,-1.05518711870952));
#26424=CARTESIAN_POINT('Ctrl Pts',(7.195328596961,2.71982866957056,-0.897218091787235));
#26425=CARTESIAN_POINT('Ctrl Pts',(5.03224959532673,5.81779044143021,-0.739249064864944));
#26426=CARTESIAN_POINT('Ctrl Pts',(1.65501604489259,7.51206652667632,-0.581280037942654));
#26427=CARTESIAN_POINT('Ctrl Pts',(-2.12153101755598,7.39387095854469,-0.423311011020362));
#26428=CARTESIAN_POINT('Ctrl Pts',(-5.38620630445157,5.49172133815517,-0.265341984098074));
#26429=CARTESIAN_POINT('Ctrl Pts',(-7.35132624111223,2.26455825864503,-0.107372957175783));
#26430=CARTESIAN_POINT('Ctrl Pts',(-7.54275708976602,-1.50898545216561,
0.0505960697465059));
#26431=CARTESIAN_POINT('Ctrl Pts',(-5.91431142841186,-4.91844913949706,
0.208565096668796));
#26432=CARTESIAN_POINT('Ctrl Pts',(-2.85889200754989,-7.14121544971374,
0.366534123591086));
#26433=CARTESIAN_POINT('Ctrl Pts',(0.88630574599214,-7.6409870916449,0.524503150513376));
#26434=CARTESIAN_POINT('Ctrl Pts',(4.41766033998119,-6.29718180860455,0.682472177435666));
#26435=CARTESIAN_POINT('Ctrl Pts',(6.88314522794016,-3.43402582709381,0.840441204357956));
#26436=CARTESIAN_POINT('Ctrl Pts',(7.68790126486706,0.257673731137408,0.998410231280246));
#26437=CARTESIAN_POINT('Ctrl Pts',(6.63776117340416,3.88720313527745,1.15637925820254));
#26438=CARTESIAN_POINT('Ctrl Pts',(3.98609719687402,6.57884874025357,1.31434828512483));
#26439=CARTESIAN_POINT('Ctrl Pts',(0.372688785402186,7.68318454023448,1.47231731204712));
#26440=CARTESIAN_POINT('Ctrl Pts',(-3.33064000372796,6.93376223818136,1.63028633896941));
#26441=CARTESIAN_POINT('Ctrl Pts',(-6.23036960042207,4.51139848075951,1.7882553658917));
#26442=CARTESIAN_POINT('Ctrl Pts',(-7.62686859462744,1.00054837481676,1.94622439281399));
#26443=CARTESIAN_POINT('Ctrl Pts',(-7.18319710009842,-2.75170874752403,
2.10419341973628));
#26444=CARTESIAN_POINT('Ctrl Pts',(-5.00640182687015,-5.84004814688836,
2.26216244665857));
#26445=CARTESIAN_POINT('Ctrl Pts',(-1.62168841761395,-7.51933163826675,
2.42013147358086));
#26446=CARTESIAN_POINT('Ctrl Pts',(2.15429739013586,-7.38439058859407,2.57810050050315));
#26447=CARTESIAN_POINT('Ctrl Pts',(5.41050572537514,-5.4677828601496,2.73606952742544));
#26448=CARTESIAN_POINT('Ctrl Pts',(7.36129587470557,-2.23193742186146,2.89403855434773));
#26449=CARTESIAN_POINT('Ctrl Pts',(7.53599151560073,1.54241806487627,3.05200758127002));
#26450=CARTESIAN_POINT('Ctrl Pts',(5.89244300841527,4.94462708428458,3.20997660819231));
#26451=CARTESIAN_POINT('Ctrl Pts',(2.8271970383585,7.15382265060854,3.3679456351146));
#26452=CARTESIAN_POINT('Ctrl Pts',(-0.920180069959813,7.63698174993965,
3.52591466203689));
#26453=CARTESIAN_POINT('Ctrl Pts',(-4.44554100112066,6.27753031194737,3.68388368895918));
#26454=CARTESIAN_POINT('Ctrl Pts',(-6.89830532789223,3.40346958459108,3.84185271588147));
#26455=CARTESIAN_POINT('Ctrl Pts',(-7.68668305495123,-0.291762271015844,
3.99982174280376));
#26456=CARTESIAN_POINT('Ctrl Pts',(-6.62045857686149,-3.91659927004588,
4.15779076972605));
#26457=CARTESIAN_POINT('Ctrl Pts',(-3.95688489262299,-6.59645992609632,
4.31575979664834));
#26458=CARTESIAN_POINT('Ctrl Pts',(-0.338614963604182,-7.68476164343996,
4.47372882357063));
#26459=CARTESIAN_POINT('Ctrl Pts',(3.3613541916878,-6.91892474363507,4.63169785049292));
#26460=CARTESIAN_POINT('Ctrl Pts',(6.25031359782997,-4.48372630061699,4.78966687741521));
#26461=CARTESIAN_POINT('Ctrl Pts',(7.63123041934389,-0.966718106245712,
4.94763590433751));
#26462=CARTESIAN_POINT('Ctrl Pts',(7.17092435414114,2.78353471637204,5.10560493125978));
#26463=CARTESIAN_POINT('Ctrl Pts',(4.98045561342925,5.862191014691,5.26357395818209));
#26464=CARTESIAN_POINT('Ctrl Pts',(1.58832890174619,7.52644889107342,5.42154298510437));
#26465=CARTESIAN_POINT('Ctrl Pts',(-2.18702140099965,7.37476501331616,5.57951201202667));
#26466=CARTESIAN_POINT('Ctrl Pts',(-5.43469875508803,5.44373686464613,5.73748103894893));
#26467=CARTESIAN_POINT('Ctrl Pts',(-7.37112075710193,2.19927269666223,5.89545006587125));
#26468=CARTESIAN_POINT('Ctrl Pts',(-7.52907775505485,-1.57582034775569,
6.05341909279352));
#26469=CARTESIAN_POINT('Ctrl Pts',(-5.8704587204801,-4.97070779881518,6.21138811971583));
#26470=CARTESIAN_POINT('Ctrl Pts',(-2.79544647567348,-7.16628918002251,
6.36935714663811));
#26471=CARTESIAN_POINT('Ctrl Pts',(0.954036299672317,-7.63282623599999,
6.5273261735604));
#26472=CARTESIAN_POINT('Ctrl Pts',(4.47333424594222,-6.25775537506413,6.68529520048269));
#26473=CARTESIAN_POINT('Ctrl Pts',(6.91332978081018,-3.37284641687486,6.84326422740498));
#26474=CARTESIAN_POINT('Ctrl Pts',(7.68531369548343,0.325845073733365,7.00123325432727));
#26475=CARTESIAN_POINT('Ctrl Pts',(6.60302579681321,3.94591838951186,7.15920228124957));
#26476=CARTESIAN_POINT('Ctrl Pts',(3.92759478089939,6.61394140033761,7.31717130817185));
#26477=CARTESIAN_POINT('Ctrl Pts',(0.304534483343064,7.68618763487766,7.47514033509413));
#26478=CARTESIAN_POINT('Ctrl Pts',(-3.39200228258501,6.90395119659456,7.63310936201643));
#26479=CARTESIAN_POINT('Ctrl Pts',(-6.27013469019421,4.45596595329453,7.79107838893872));
#26480=CARTESIAN_POINT('Ctrl Pts',(-7.63544218492327,0.932868828290557,
7.94904741586101));
#26481=CARTESIAN_POINT('Ctrl Pts',(-7.15851060041003,-2.81530595026851,
8.10701644278331));
#26482=CARTESIAN_POINT('Ctrl Pts',(-4.9544114652216,-5.88421860947506,8.26498546970558));
#26483=CARTESIAN_POINT('Ctrl Pts',(-1.55493815323402,-7.53341814504625,
8.42295449662788));
#26484=CARTESIAN_POINT('Ctrl Pts',(2.21970240660853,-7.36499442217634,8.58092352355018));
#26485=CARTESIAN_POINT('Ctrl Pts',(5.45878491797924,-5.41958382411224,8.73889255047245));
#26486=CARTESIAN_POINT('Ctrl Pts',(7.38080069488091,-2.16656472607635,8.89686157739476));
#26487=CARTESIAN_POINT('Ctrl Pts',(7.52201594451772,1.60919164537799,9.05483060431704));
#26488=CARTESIAN_POINT('Ctrl Pts',(5.84835899604979,4.99669076754189,9.21279963123934));
#26489=CARTESIAN_POINT('Ctrl Pts',(2.76364094548598,7.1786147980614,9.37076865816163));
#26490=CARTESIAN_POINT('Ctrl Pts',(-0.987873772599122,7.6285206213513,9.52873768508391));
#26491=CARTESIAN_POINT('Ctrl Pts',(-4.50103952168514,6.23785740659357,9.68670671200621));
#26492=CARTESIAN_POINT('Ctrl Pts',(-6.92821830337425,3.34215688767999,9.84467573892849));
#26493=CARTESIAN_POINT('Ctrl Pts',(-7.68379318985292,-0.359921394442083,
10.0026447658508));
#26494=CARTESIAN_POINT('Ctrl Pts',(-6.58546322177129,-3.97516006214074,
10.1606137927731));
#26495=CARTESIAN_POINT('Ctrl Pts',(-3.89822734886324,-6.6312925376092,10.3185828196954));
#26496=CARTESIAN_POINT('Ctrl Pts',(-0.270448187237914,-7.68746303348714,
10.4765518466177));
#26497=CARTESIAN_POINT('Ctrl Pts',(3.42258400874207,-6.88884082910166,10.63452087354));
#26498=CARTESIAN_POINT('Ctrl Pts',(6.28983183712536,-4.4281200481492,10.7924899004623));
#26499=CARTESIAN_POINT('Ctrl Pts',(7.63950507226382,-0.898997198667169,
10.9504589273846));
#26500=CARTESIAN_POINT('Ctrl Pts',(7.14595362848161,2.8470140399453,11.1084279543069));
#26501=CARTESIAN_POINT('Ctrl Pts',(4.92827466194258,5.90614561821491,11.2663969812292));
#26502=CARTESIAN_POINT('Ctrl Pts',(1.52150756701962,7.5402098924435,11.4243660081514));
#26503=CARTESIAN_POINT('Ctrl Pts',(-2.25232175897465,7.35513608411886,11.5823350350737));
#26504=CARTESIAN_POINT('Ctrl Pts',(-5.48279887906735,5.39521304718891,11.740304061996));
#26505=CARTESIAN_POINT('Ctrl Pts',(-7.39026556096377,2.13403316693694,11.8982730889183));
#26506=CARTESIAN_POINT('Ctrl Pts',(-7.51496606468558,-1.64319871482238,
12.0562509298068));
#26507=CARTESIAN_POINT('Ctrl Pts',(-6.38858261358109,-3.89562257101338,
12.1615724283879));
#26508=CARTESIAN_POINT('Ctrl Pts',(-5.59099016251816,-4.82066458193201,
12.2142375846616));
#26509=CARTESIAN_POINT('Ctrl Pts',(-1.81369530454162,6.77185709926922,-12.6435835482508));
#26510=CARTESIAN_POINT('Ctrl Pts',(-2.93392826290543,6.47182695586933,-12.5909272059434));
#26511=CARTESIAN_POINT('Ctrl Pts',(-5.02154850583196,5.30552096540475,-12.4856145213285));
#26512=CARTESIAN_POINT('Ctrl Pts',(-6.94196157239741,2.27379792622978,-12.3276454944063));
#26513=CARTESIAN_POINT('Ctrl Pts',(-7.18718979160325,-1.30562067836087,
-12.169676467484));
#26514=CARTESIAN_POINT('Ctrl Pts',(-5.69846535245324,-4.57047627984927,
-12.0117074405617));
#26515=CARTESIAN_POINT('Ctrl Pts',(-2.83477632842897,-6.73236177450464,
-11.8537384136394));
#26516=CARTESIAN_POINT('Ctrl Pts',(0.712837007271223,-7.27001675403625,
-11.6957693867171));
#26517=CARTESIAN_POINT('Ctrl Pts',(4.08847908705196,-6.05353978254254,-11.5378003597948));
#26518=CARTESIAN_POINT('Ctrl Pts',(6.47766515763744,-3.37652806502808,-11.3798313328725));
#26519=CARTESIAN_POINT('Ctrl Pts',(7.30395930917253,0.11517058512602,-11.2218623059502));
#26520=CARTESIAN_POINT('Ctrl Pts',(6.36799032002208,3.57907319090322,-11.0638932790279));
#26521=CARTESIAN_POINT('Ctrl Pts',(3.89558761425688,6.17944023049411,-10.9059242521056));
#26522=CARTESIAN_POINT('Ctrl Pts',(0.483277485164234,7.28886243758025,-10.7479552251834));
#26523=CARTESIAN_POINT('Ctrl Pts',(-3.04563493721468,6.63966762466852,-10.5899861982611));
#26524=CARTESIAN_POINT('Ctrl Pts',(-5.83971285652995,4.38848836535718,-10.4320171713388));
#26525=CARTESIAN_POINT('Ctrl Pts',(-7.22481567467033,1.07847815974754,-10.2740481444165));
#26526=CARTESIAN_POINT('Ctrl Pts',(-6.86675325118532,-2.49174170282166,
-10.1160791174942));
#26527=CARTESIAN_POINT('Ctrl Pts',(-4.85191692213481,-5.46076723551842,
-9.95811009057192));
#26528=CARTESIAN_POINT('Ctrl Pts',(-1.66643576956793,-7.11224779210676,
-9.80014106364962));
#26529=CARTESIAN_POINT('Ctrl Pts',(1.92111419208633,-7.04772282243761,-9.64217203672734));
#26530=CARTESIAN_POINT('Ctrl Pts',(5.04514788585,-5.28276060163156,-9.48420300980503));
#26531=CARTESIAN_POINT('Ctrl Pts',(6.95191500122294,-2.24320185668345,-9.32623398288276));
#26532=CARTESIAN_POINT('Ctrl Pts',(7.18136085776967,1.3375847570525,-9.16826495596046));
#26533=CARTESIAN_POINT('Ctrl Pts',(5.67812597489346,4.59564600135666,-9.01029592903816));
#26534=CARTESIAN_POINT('Ctrl Pts',(2.8049029084755,6.74489410049379,-8.85232690211588));
#26535=CARTESIAN_POINT('Ctrl Pts',(-0.745072286421055,7.26676984931728,
-8.6943578751936));
#26536=CARTESIAN_POINT('Ctrl Pts',(-4.11528038346203,6.0353578286229,-8.5363888482713));
#26537=CARTESIAN_POINT('Ctrl Pts',(-6.49257540998183,3.34776661372903,-8.37841982134901));
#26538=CARTESIAN_POINT('Ctrl Pts',(-7.30337620404243,-0.147556011471637,
-8.22045079442673));
#26539=CARTESIAN_POINT('Ctrl Pts',(-6.35205704125284,-3.60727710314818,
-8.06248176750443));
#26540=CARTESIAN_POINT('Ctrl Pts',(-3.86814717429505,-6.19665346717748,
-7.90451274058214));
#26541=CARTESIAN_POINT('Ctrl Pts',(-0.450951229581856,-7.29093407889479,
-7.74654371365985));
#26542=CARTESIAN_POINT('Ctrl Pts',(3.07504784111031,-6.62609670387868,-7.58857468673757));
#26543=CARTESIAN_POINT('Ctrl Pts',(5.85911564362261,-4.36254978526543,-7.43060565981527));
#26544=CARTESIAN_POINT('Ctrl Pts',(7.22952703345288,-1.04642994358814,-7.27263663289299));
#26545=CARTESIAN_POINT('Ctrl Pts',(6.85563640346892,2.52216697656922,-7.11466760597068));
#26546=CARTESIAN_POINT('Ctrl Pts',(4.82765410602869,5.48222879737866,-6.9566985790484));
#26547=CARTESIAN_POINT('Ctrl Pts',(1.6348809766094,7.11956746906614,-6.79872955212611));
#26548=CARTESIAN_POINT('Ctrl Pts',(-1.95234758211534,7.03913458266514,-6.64076052520382));
#26549=CARTESIAN_POINT('Ctrl Pts',(-5.06852404917411,5.26033655930947,-6.48279149828154));
#26550=CARTESIAN_POINT('Ctrl Pts',(-6.96179385919399,2.21235237165163,-6.32482247135924));
#26551=CARTESIAN_POINT('Ctrl Pts',(-7.17535889268673,-1.36941648719649,
-6.16685344443695));
#26552=CARTESIAN_POINT('Ctrl Pts',(-5.65769130868016,-4.62077978375393,
-6.00888441751466));
#26553=CARTESIAN_POINT('Ctrl Pts',(-2.77496590947326,-6.75726578991277,
-5.85091539059237));
#26554=CARTESIAN_POINT('Ctrl Pts',(0.777288577654942,-7.26339446962032,
-5.69294636367007));
#26555=CARTESIAN_POINT('Ctrl Pts',(4.14200299062499,-6.01704977376104,-5.53497733674778));
#26556=CARTESIAN_POINT('Ctrl Pts',(6.50735684388032,-3.31894315417848,-5.37700830982551));
#26557=CARTESIAN_POINT('Ctrl Pts',(7.30265007852113,0.17994050388728,-5.2190392829032));
#26558=CARTESIAN_POINT('Ctrl Pts',(6.33599855204277,3.6354090695238,-5.06107025598093));
#26559=CARTESIAN_POINT('Ctrl Pts',(3.84063082867778,6.21374537554234,-4.90310122905862));
#26560=CARTESIAN_POINT('Ctrl Pts',(0.418616025797775,7.29286208406613,-4.74513220213635));
#26561=CARTESIAN_POINT('Ctrl Pts',(-3.10440023622982,6.61239562696912,-4.58716317521405));
#26562=CARTESIAN_POINT('Ctrl Pts',(-5.87840323953228,4.33652534959964,-4.42919414829176));
#26563=CARTESIAN_POINT('Ctrl Pts',(-7.23409622109299,1.01436118726629,-4.27122512136947));
#26564=CARTESIAN_POINT('Ctrl Pts',(-6.84438475342828,-2.55254267374759,
-4.11325609444718));
#26565=CARTESIAN_POINT('Ctrl Pts',(-4.80329635687898,-5.50358254796429,
-3.95528706752489));
#26566=CARTESIAN_POINT('Ctrl Pts',(-1.60329403715022,-7.12674715313392,
-3.7973180406026));
#26567=CARTESIAN_POINT('Ctrl Pts',(1.98354258230751,-7.03040792404231,-3.63934901368031));
#26568=CARTESIAN_POINT('Ctrl Pts',(5.09180054555484,-5.23780908000201,-3.48137998675802));
#26569=CARTESIAN_POINT('Ctrl Pts',(6.97153582190916,-2.18145938263847,-3.32341095983573));
#26570=CARTESIAN_POINT('Ctrl Pts',(7.16921583253244,1.40122128902976,-3.16544193291344));
#26571=CARTESIAN_POINT('Ctrl Pts',(5.63714539069785,4.64582270415024,-3.00747290599115));
#26572=CARTESIAN_POINT('Ctrl Pts',(2.74497434401289,6.76950460558047,-2.84950387906886));
#26573=CARTESIAN_POINT('Ctrl Pts',(-0.809489584411743,7.25987626388997,
-2.69153485214657));
#26574=CARTESIAN_POINT('Ctrl Pts',(-4.16864415019417,5.99862340069084,-2.53356582522428));
#26575=CARTESIAN_POINT('Ctrl Pts',(-6.52201031828139,3.29005443153989,-2.37559679830199));
#26576=CARTESIAN_POINT('Ctrl Pts',(-7.30178035500522,-0.21232145799179,
-2.2176277713797));
#26577=CARTESIAN_POINT('Ctrl Pts',(-6.31981547289671,-3.66346954986654,
-2.05965874445741));
#26578=CARTESIAN_POINT('Ctrl Pts',(-3.81303896158777,-6.23071509793841,
-1.90168971753512));
#26579=CARTESIAN_POINT('Ctrl Pts',(-0.38627259042325,-7.29464668370934,
-1.74372069061283));
#26580=CARTESIAN_POINT('Ctrl Pts',(3.13369158698175,-6.5985645251027,-1.58575166369054));
#26581=CARTESIAN_POINT('Ctrl Pts',(5.89757524357891,-4.31041564127977,-1.42778263676825));
#26582=CARTESIAN_POINT('Ctrl Pts',(7.23852315876718,-0.982272484728769,
-1.26981360984596));
#26583=CARTESIAN_POINT('Ctrl Pts',(6.83299851663794,2.58286817818637,-1.11184458292367));
#26584=CARTESIAN_POINT('Ctrl Pts',(4.77884415657435,5.52482807709338,-0.953875556001376));
#26585=CARTESIAN_POINT('Ctrl Pts',(1.57167557080567,7.13378669812861,-0.795906529079087));
#26586=CARTESIAN_POINT('Ctrl Pts',(-2.0146985784755,7.02154302074358,-0.637937502156794));
#26587=CARTESIAN_POINT('Ctrl Pts',(-5.11497691768626,5.21517860535962,-0.479968475234507));
#26588=CARTESIAN_POINT('Ctrl Pts',(-6.98114069759888,2.15052349780065,-0.321999448312216));
#26589=CARTESIAN_POINT('Ctrl Pts',(-7.16293179820856,-1.43299853749984,
-0.164030421389927));
#26590=CARTESIAN_POINT('Ctrl Pts',(-5.61648862490333,-4.67077426992521,
-0.0060613944676359));
#26591=CARTESIAN_POINT('Ctrl Pts',(-2.71492880187113,-6.7816103069282,0.151907632454654));
#26592=CARTESIAN_POINT('Ctrl Pts',(0.841674673511063,-7.2562153012596,0.309876659376944));
#26593=CARTESIAN_POINT('Ctrl Pts',(4.1952033382952,-5.98007907176994,0.467845686299233));
#26594=CARTESIAN_POINT('Ctrl Pts',(6.53653554504559,-3.2611010138632,0.625814713221524));
#26595=CARTESIAN_POINT('Ctrl Pts',(7.30076705059481,0.244698237045366,0.783783740143812));
#26596=CARTESIAN_POINT('Ctrl Pts',(6.30350812203683,3.69145799240351,0.941752767066107));
#26597=CARTESIAN_POINT('Ctrl Pts',(3.78537211558601,6.24756230067438,1.09972179398839));
#26598=CARTESIAN_POINT('Ctrl Pts',(0.353921559454047,7.2962878427333,1.25769082091068));
#26599=CARTESIAN_POINT('Ctrl Pts',(-3.16292131738643,6.58460367025127,1.41565984783297));
#26600=CARTESIAN_POINT('Ctrl Pts',(-5.91663127876754,4.28422117372264,1.57362887475526));
#26601=CARTESIAN_POINT('Ctrl Pts',(-7.24280775942501,0.950164466961936,
1.73159790167755));
#26602=CARTESIAN_POINT('Ctrl Pts',(-6.82147791699476,-2.61314289357025,
1.88956692859984));
#26603=CARTESIAN_POINT('Ctrl Pts',(-4.75429798593847,-5.54596496699767,
2.04753595552213));
#26604=CARTESIAN_POINT('Ctrl Pts',(-1.54002619931564,-7.1406859656258,2.20550498244442));
#26605=CARTESIAN_POINT('Ctrl Pts',(2.04581495797322,-7.01254004708686,2.36347400936671));
#26606=CARTESIAN_POINT('Ctrl Pts',(5.1380527098323,-5.19244558038397,2.52144303628901));
#26607=CARTESIAN_POINT('Ctrl Pts',(6.99060829739458,-2.11954532545592,2.67941206321129));
#26608=CARTESIAN_POINT('Ctrl Pts',(7.15650691328321,1.46474760774462,2.83738109013358));
#26609=CARTESIAN_POINT('Ctrl Pts',(5.59572141748752,4.69563399043573,2.99535011705587));
#26610=CARTESIAN_POINT('Ctrl Pts',(2.68482987385815,6.79358265591159,3.15331914397817));
#26611=CARTESIAN_POINT('Ctrl Pts',(-0.873843212071065,7.25241165371776,
3.31128817090046));
#26612=CARTESIAN_POINT('Ctrl Pts',(-4.2216800326729,5.96141715165069,3.46925719782274));
#26613=CARTESIAN_POINT('Ctrl Pts',(-6.55093223855147,3.23208347048325,3.62722622474502));
#26614=CARTESIAN_POINT('Ctrl Pts',(-7.29961018521533,-0.277070204396807,
3.78519525166733));
#26615=CARTESIAN_POINT('Ctrl Pts',(-6.28707682012798,-3.71937384677498,
3.94316427858961));
#26616=CARTESIAN_POINT('Ctrl Pts',(-3.75763083470842,-6.26428665246989,
4.10113330551191));
#26617=CARTESIAN_POINT('Ctrl Pts',(-0.321563569035062,-7.29778552886652,
4.2591023324342));
#26618=CARTESIAN_POINT('Ctrl Pts',(3.19208885267565,-6.57051333693858,4.41707135935648));
#26619=CARTESIAN_POINT('Ctrl Pts',(5.93557097038379,-4.25794246201158,4.57504038627877));
#26620=CARTESIAN_POINT('Ctrl Pts',(7.24694993881483,-0.918037765332063,
4.73300941320106));
#26621=CARTESIAN_POINT('Ctrl Pts',(6.80982318103779,2.64336622458265,4.89097844012336));
#26622=CARTESIAN_POINT('Ctrl Pts',(4.72965832764282,5.5669928020452,5.04894746704564));
#26623=CARTESIAN_POINT('Ctrl Pts',(1.50834654502766,7.14744481995958,5.20691649396794));
#26624=CARTESIAN_POINT('Ctrl Pts',(-2.07689110893389,7.00339918010499,5.36488552089023));
#26625=CARTESIAN_POINT('Ctrl Pts',(-5.16102746823473,5.16961045209314,5.52285454781252));
#26626=CARTESIAN_POINT('Ctrl Pts',(-6.99993843512712,2.08852547475349,5.68082357473481));
#26627=CARTESIAN_POINT('Ctrl Pts',(-7.14994130409418,-1.49646787545607,
5.8387926016571));
#26628=CARTESIAN_POINT('Ctrl Pts',(-5.57484417681309,-4.72040137684468,
5.99676162857939));
#26629=CARTESIAN_POINT('Ctrl Pts',(-2.65467815183384,-6.80542141710859,
6.15473065550168));
#26630=CARTESIAN_POINT('Ctrl Pts',(0.905994567535526,-7.24846539605865,
6.31269968242397));
#26631=CARTESIAN_POINT('Ctrl Pts',(4.24807371269448,-5.94263800729767,6.47066870934625));
#26632=CARTESIAN_POINT('Ctrl Pts',(6.56520011570513,-3.20300237199555,6.62863773626855));
#26633=CARTESIAN_POINT('Ctrl Pts',(7.29830978161512,0.309436723489496,6.78660676319084));
#26634=CARTESIAN_POINT('Ctrl Pts',(6.27052189027236,3.74721656404915,6.94457579011314));
#26635=CARTESIAN_POINT('Ctrl Pts',(3.72981566445421,6.28088782445943,7.10254481703542));
#26636=CARTESIAN_POINT('Ctrl Pts',(0.289199255448475,7.2991397126605,7.2605138439577));
#26637=CARTESIAN_POINT('Ctrl Pts',(-3.22119361930532,6.55629380223107,7.41848287088));
#26638=CARTESIAN_POINT('Ctrl Pts',(-5.95439394599886,4.23158002289297,7.5764518978023));
#26639=CARTESIAN_POINT('Ctrl Pts',(-7.25094961548957,0.885893011560218,
7.73442092472457));
#26640=CARTESIAN_POINT('Ctrl Pts',(-6.79803453793589,-2.67353757689281,
7.89238995164688));
#26641=CARTESIAN_POINT('Ctrl Pts',(-4.7049256662123,-5.58791116879611,8.05035897856914));
#26642=CARTESIAN_POINT('Ctrl Pts',(-1.47663723085548,-7.15406312813226,
8.20832800549145));
#26643=CARTESIAN_POINT('Ctrl Pts',(2.10792642022488,-6.99412059972255,8.36629703241375));
#26644=CARTESIAN_POINT('Ctrl Pts',(5.18390074123251,-5.14667366916288,8.52426605933602));
#26645=CARTESIAN_POINT('Ctrl Pts',(7.009130927116,-2.05746455634179,8.68223508625831));
#26646=CARTESIAN_POINT('Ctrl Pts',(7.14323510016273,1.52815871821309,8.84020411318062));
#26647=CARTESIAN_POINT('Ctrl Pts',(5.55385731259759,4.74507593956618,8.9981731401029));
#26648=CARTESIAN_POINT('Ctrl Pts',(2.62447423026674,6.81712636270509,9.15614216702519));
#26649=CARTESIAN_POINT('Ctrl Pts',(-0.938128110736495,7.2443765962059,9.31411119394749));
#26650=CARTESIAN_POINT('Ctrl Pts',(-4.27438385343418,5.92374202677208,9.47208022086977));
#26651=CARTESIAN_POINT('Ctrl Pts',(-6.57933890745375,3.17385825374728,9.63004924779207));
#26652=CARTESIAN_POINT('Ctrl Pts',(-7.29686584301274,-0.34179708698331,
9.78801827471435));
#26653=CARTESIAN_POINT('Ctrl Pts',(-6.25384370141794,-3.77498573442195,
9.94598730163664));
#26654=CARTESIAN_POINT('Ctrl Pts',(-3.7019270674518,-6.297365222766,10.1039563285589));
#26655=CARTESIAN_POINT('Ctrl Pts',(-0.256829418882215,-7.30035088692299,
10.2619253554812));
#26656=CARTESIAN_POINT('Ctrl Pts',(3.25023536307719,-6.54194433684203,10.4198943824035));
#26657=CARTESIAN_POINT('Ctrl Pts',(5.97309921761348,-4.20513633432635,10.5778634093258));
#26658=CARTESIAN_POINT('Ctrl Pts',(7.25480791088178,-0.853727031667314,
10.7358324362481));
#26659=CARTESIAN_POINT('Ctrl Pts',(6.78610988857427,2.70364896469217,10.8938014631704));
#26660=CARTESIAN_POINT('Ctrl Pts',(4.6801050154764,5.6087340146432,11.0517704900927));
#26661=CARTESIAN_POINT('Ctrl Pts',(1.44489008506012,7.16051286830262,11.2097395170149));
#26662=CARTESIAN_POINT('Ctrl Pts',(-2.13890318290192,6.98475869103198,11.3677085439373));
#26663=CARTESIAN_POINT('Ctrl Pts',(-5.20670544824242,5.12353011424077,11.5256775708595));
#26664=CARTESIAN_POINT('Ctrl Pts',(-7.01811917762225,2.02657116594995,11.6836465977818));
#26665=CARTESIAN_POINT('Ctrl Pts',(-7.13654022615019,-1.5604533176796,11.8416244386703));
#26666=CARTESIAN_POINT('Ctrl Pts',(-6.06687727096378,-3.69945345656046,
11.9469459372515));
#26667=CARTESIAN_POINT('Ctrl Pts',(-5.3094486196446,-4.57791378026331,11.9996110935251));
#26668=CARTESIAN_POINT('Ctrl Pts',(-5.31037376991248,-4.57794244025911,
12.));
#26669=CARTESIAN_POINT('Ctrl Pts',(-5.44263380122459,-4.44687739974309,
12.));
#26670=CARTESIAN_POINT('Ctrl Pts',(-5.5693014092247,-4.3106898541843,12.));
#26671=CARTESIAN_POINT('Ctrl Pts',(-5.69024917409142,-4.1698511932344,12.));
#26672=CARTESIAN_POINT('Ctrl Pts',(-5.81418999782626,-4.02552723924421,
12.));
#26673=CARTESIAN_POINT('Ctrl Pts',(-5.93212486388003,-3.876318788248,12.));
#26674=CARTESIAN_POINT('Ctrl Pts',(-6.04389086929985,-3.72268453170137,
12.));
#26675=CARTESIAN_POINT('Ctrl Pts',(-6.15652040037929,-3.56786326733222,
12.));
#26676=CARTESIAN_POINT('Ctrl Pts',(-6.26288583253187,-3.40854703539605,
12.));
#26677=CARTESIAN_POINT('Ctrl Pts',(-6.36278756125166,-3.24516313822355,
12.));
#26678=CARTESIAN_POINT('Ctrl Pts',(-6.46266655647491,-3.08181642046033,
12.));
#26679=CARTESIAN_POINT('Ctrl Pts',(-6.55608521685512,-2.914403315385,12.));
#26680=CARTESIAN_POINT('Ctrl Pts',(-6.64280476241556,-2.74331712888927,
12.));
#26681=CARTESIAN_POINT('Ctrl Pts',(-6.71416600011118,-2.60253085121616,
12.));
#26682=CARTESIAN_POINT('Ctrl Pts',(-6.78099027006545,-2.45925655037198,
12.));
#26683=CARTESIAN_POINT('Ctrl Pts',(-6.84312140434658,-2.31370042357453,
12.));
#26684=CARTESIAN_POINT('Ctrl Pts',(-6.85476347855885,-2.28642625177913,
12.));
#26685=CARTESIAN_POINT('Ctrl Pts',(-6.86623701980134,-2.25908044570938,
12.));
#26686=CARTESIAN_POINT('Ctrl Pts',(-6.87753655261754,-2.23167620907008,
12.));
#26687=CARTESIAN_POINT('Ctrl Pts',(-6.95229594262949,-2.05036570285519,
12.));
#26688=CARTESIAN_POINT('Ctrl Pts',(-7.01950773615009,-1.86634543828863,
12.));
#26689=CARTESIAN_POINT('Ctrl Pts',(-7.07899546236369,-1.68007671471902,
12.));
#26690=CARTESIAN_POINT('Ctrl Pts',(-7.0921962818188,-1.63874214124503,12.));
#26691=CARTESIAN_POINT('Ctrl Pts',(-7.1050165991878,-1.59729670185842,12.));
#26692=CARTESIAN_POINT('Ctrl Pts',(-7.11745423244715,-1.55574520184557,
12.));
#26693=CARTESIAN_POINT('Ctrl Pts',(-7.17295666561696,-1.37032332097173,
12.));
#26694=CARTESIAN_POINT('Ctrl Pts',(-7.22084218410379,-1.18279157288797,
12.));
#26695=CARTESIAN_POINT('Ctrl Pts',(-7.26118675281216,-0.993630970717798,
12.));
#26696=CARTESIAN_POINT('Ctrl Pts',(-7.30190404530392,-0.80272280604871,
12.));
#26697=CARTESIAN_POINT('Ctrl Pts',(-7.33494057259123,-0.610154914422011,
12.));
#26698=CARTESIAN_POINT('Ctrl Pts',(-7.36032600263038,-0.416399269132085,
12.));
#26699=CARTESIAN_POINT('Ctrl Pts',(-7.38580045309683,-0.22196417069481,
12.));
#26700=CARTESIAN_POINT('Ctrl Pts',(-7.40357018172954,-0.0263322814024089,
12.));
#26701=CARTESIAN_POINT('Ctrl Pts',(-7.41361448974918,0.170031926235426,
12.));
#26702=CARTESIAN_POINT('Ctrl Pts',(-7.41789307147214,0.2536773409518,12.));
#26703=CARTESIAN_POINT('Ctrl Pts',(-7.42076922976018,0.337455728705427,
12.));
#26704=CARTESIAN_POINT('Ctrl Pts',(-7.42223849461264,0.421331393594551,
12.));
#26705=CARTESIAN_POINT('Ctrl Pts',(-7.42278385315547,0.452464181060878,
12.));
#26706=CARTESIAN_POINT('Ctrl Pts',(-7.42313532094487,0.483614843921272,
12.));
#26707=CARTESIAN_POINT('Ctrl Pts',(-7.42329265508154,0.514752665167828,
12.));
#26708=CARTESIAN_POINT('Ctrl Pts',(-7.42430042249123,0.714198774723802,
12.));
#26709=CARTESIAN_POINT('Ctrl Pts',(-7.41735325724622,0.913326000511656,
12.));
#26710=CARTESIAN_POINT('Ctrl Pts',(-7.40253605861267,1.11163646571176,12.));
#26711=CARTESIAN_POINT('Ctrl Pts',(-7.3875739546921,1.31188631470432,12.));
#26712=CARTESIAN_POINT('Ctrl Pts',(-7.36458728597274,1.51130404209091,12.));
#26713=CARTESIAN_POINT('Ctrl Pts',(-7.33361305290546,1.70939347351054,12.));
#26714=CARTESIAN_POINT('Ctrl Pts',(-7.31331709001647,1.83919219169224,12.));
#26715=CARTESIAN_POINT('Ctrl Pts',(-7.28959057761779,1.96842091312578,12.));
#26716=CARTESIAN_POINT('Ctrl Pts',(-7.26243189542493,2.09694161440494,12.));
#26717=CARTESIAN_POINT('Ctrl Pts',(-7.22127493916038,2.29170514689428,12.));
#26718=CARTESIAN_POINT('Ctrl Pts',(-7.17223845250762,2.48484324799321,12.));
#26719=CARTESIAN_POINT('Ctrl Pts',(-7.11556674570035,2.67596142142443,12.));
#26720=CARTESIAN_POINT('Ctrl Pts',(-7.05858971833812,2.86810924986448,12.));
#26721=CARTESIAN_POINT('Ctrl Pts',(-6.99389479095136,3.05821598378138,12.0000000000001));
#26722=CARTESIAN_POINT('Ctrl Pts',(-6.92167929314466,3.24586878138439,12.));
#26723=CARTESIAN_POINT('Ctrl Pts',(-6.91269242292701,3.26922126650541,12.));
#26724=CARTESIAN_POINT('Ctrl Pts',(-6.90358902237198,3.29253572590266,12.));
#26725=CARTESIAN_POINT('Ctrl Pts',(-6.89436941923266,3.31581134310704,12.));
#26726=CARTESIAN_POINT('Ctrl Pts',(-6.88573306865334,3.33761449310057,12.));
#26727=CARTESIAN_POINT('Ctrl Pts',(-6.87699606722048,3.35938015973985,12.));
#26728=CARTESIAN_POINT('Ctrl Pts',(-6.86816257821046,3.38109857716582,12.));
#26729=CARTESIAN_POINT('Ctrl Pts',(-6.7899490171883,3.57339799189585,12.));
#26730=CARTESIAN_POINT('Ctrl Pts',(-6.70409267881087,3.76220414798894,12.));
#26731=CARTESIAN_POINT('Ctrl Pts',(-6.61094013320699,3.94709682805149,12.));
#26732=CARTESIAN_POINT('Ctrl Pts',(-6.5188674146208,4.12984622678978,12.));
#26733=CARTESIAN_POINT('Ctrl Pts',(-6.41966627981606,4.30877300552798,12.));
#26734=CARTESIAN_POINT('Ctrl Pts',(-6.3136173503513,4.48346635617926,12.));
#26735=CARTESIAN_POINT('Ctrl Pts',(-6.20570281127415,4.66123290705839,12.));
#26736=CARTESIAN_POINT('Ctrl Pts',(-6.09069729335284,4.8346165151789,12.));
#26737=CARTESIAN_POINT('Ctrl Pts',(-5.96884373944417,5.00316848119551,12.));
#26738=CARTESIAN_POINT('Ctrl Pts',(-5.84699018553566,5.17172044721195,12.));
#26739=CARTESIAN_POINT('Ctrl Pts',(-5.71828830820229,5.33544150355174,12.));
#26740=CARTESIAN_POINT('Ctrl Pts',(-5.58293216084951,5.49385617917438,12.));
#26741=CARTESIAN_POINT('Ctrl Pts',(-5.48072057973372,5.61347996268186,12.));
#26742=CARTESIAN_POINT('Ctrl Pts',(-5.37471348591305,5.73007739213431,12.));
#26743=CARTESIAN_POINT('Ctrl Pts',(-5.265078497822,5.84352819974904,12.));
#26744=CARTESIAN_POINT('Ctrl Pts',(-5.24734949338018,5.86187425794772,12.));
#26745=CARTESIAN_POINT('Ctrl Pts',(-5.22953248896639,5.88013086749493,12.));
#26746=CARTESIAN_POINT('Ctrl Pts',(-5.21162852071991,5.89829754304194,12.));
#26747=CARTESIAN_POINT('Ctrl Pts',(-5.06686638441565,6.04518379337078,12.));
#26748=CARTESIAN_POINT('Ctrl Pts',(-4.91642028229973,6.18619532035819,12.));
#26749=CARTESIAN_POINT('Ctrl Pts',(-4.76074935872281,6.32112569416813,12.));
#26750=CARTESIAN_POINT('Ctrl Pts',(-4.60343491033637,6.45748062056515,12.));
#26751=CARTESIAN_POINT('Ctrl Pts',(-4.44078428855073,6.58762579282384,12.));
#26752=CARTESIAN_POINT('Ctrl Pts',(-4.27322757239386,6.7113180635556,12.));
#26753=CARTESIAN_POINT('Ctrl Pts',(-4.1903288657841,6.77251483021751,12.));
#26754=CARTESIAN_POINT('Ctrl Pts',(-4.10622862835614,6.83213156370766,12.));
#26755=CARTESIAN_POINT('Ctrl Pts',(-4.02097557077802,6.89013557177268,12.));
#26756=CARTESIAN_POINT('Ctrl Pts',(-3.95347972739972,6.93605802376314,12.));
#26757=CARTESIAN_POINT('Ctrl Pts',(-3.88526124287464,6.98096956683595,12.));
#26758=CARTESIAN_POINT('Ctrl Pts',(-3.81634342773284,7.02485291118474,12.));
#26759=CARTESIAN_POINT('Ctrl Pts',(-3.79116897753097,7.04088271515818,12.));
#26760=CARTESIAN_POINT('Ctrl Pts',(-3.76590910034549,7.05677028659542,12.));
#26761=CARTESIAN_POINT('Ctrl Pts',(-3.74056584986644,7.0725145443284,12.));
#26762=CARTESIAN_POINT('Ctrl Pts',(-3.56101544976198,7.18405855395118,12.));
#26763=CARTESIAN_POINT('Ctrl Pts',(-3.37727141976454,7.28841963306843,12.));
#26764=CARTESIAN_POINT('Ctrl Pts',(-3.18978287088803,7.38535844839708,12.));
#26765=CARTESIAN_POINT('Ctrl Pts',(-3.00212282400591,7.48238593481309,12.));
#26766=CARTESIAN_POINT('Ctrl Pts',(-2.8107108547889,7.57197802781875,12.));
#26767=CARTESIAN_POINT('Ctrl Pts',(-2.61596266530345,7.65385608862354,12.));
#26768=CARTESIAN_POINT('Ctrl Pts',(-2.53573323788768,7.68758697954293,12.));
#26769=CARTESIAN_POINT('Ctrl Pts',(-2.45493724389214,7.72000819012581,12.));
#26770=CARTESIAN_POINT('Ctrl Pts',(-2.37360237640543,7.75109805319064,12.));
#26771=CARTESIAN_POINT('Ctrl Pts',(-2.28382628244401,7.78541453459649,12.));
#26772=CARTESIAN_POINT('Ctrl Pts',(-2.19339366251994,7.81810902050074,12.));
#26773=CARTESIAN_POINT('Ctrl Pts',(-2.10234959246262,7.84917916318753,12.));
#26774=CARTESIAN_POINT('',(-5.31059994331846,-4.57805082698748,-12.0001612281326));
#26775=CARTESIAN_POINT('Ctrl Pts',(-5.31041659161217,-4.57789276698681,
-12.0001612281326));
#26776=CARTESIAN_POINT('Ctrl Pts',(-5.30898519516614,-4.57955320593178,
-12.0001074854218));
#26777=CARTESIAN_POINT('Ctrl Pts',(-5.30755301995135,-4.58121297353208,
-12.0000537427109));
#26778=CARTESIAN_POINT('Ctrl Pts',(-5.30612006659788,-4.5828720690575,-12.));
#26779=CARTESIAN_POINT('Ctrl Pts',(-2.10208451021625,7.84862588447231,-12.));
#26780=CARTESIAN_POINT('Ctrl Pts',(-2.29939557502752,7.78116612971775,-12.));
#26781=CARTESIAN_POINT('Ctrl Pts',(-2.4936542542127,7.70609002726533,-12.));
#26782=CARTESIAN_POINT('Ctrl Pts',(-2.68449722358562,7.62371149342739,-12.));
#26783=CARTESIAN_POINT('Ctrl Pts',(-2.87766974795956,7.54032739293898,-12.));
#26784=CARTESIAN_POINT('Ctrl Pts',(-3.06734326841189,7.44946115095014,-12.));
#26785=CARTESIAN_POINT('Ctrl Pts',(-3.25311885301286,7.35138992456979,-12.));
#26786=CARTESIAN_POINT('Ctrl Pts',(-3.43857588505528,7.2534868625914,-12.));
#26787=CARTESIAN_POINT('Ctrl Pts',(-3.62014888774859,7.14840306152861,-12.));
#26788=CARTESIAN_POINT('Ctrl Pts',(-3.79741044020532,7.03637241540061,-12.));
#26789=CARTESIAN_POINT('Ctrl Pts',(-3.97212170749682,6.92595356884738,-12.));
#26790=CARTESIAN_POINT('Ctrl Pts',(-4.14264512962284,6.80878585135145,-12.));
#26791=CARTESIAN_POINT('Ctrl Pts',(-4.30853456284606,6.68505947482801,-12.));
#26792=CARTESIAN_POINT('Ctrl Pts',(-4.45106252196752,6.5787569358854,-12.));
#26793=CARTESIAN_POINT('Ctrl Pts',(-4.59016935759093,6.46761224569854,-12.));
#26794=CARTESIAN_POINT('Ctrl Pts',(-4.72554610341853,6.35172956523783,-12.));
#26795=CARTESIAN_POINT('Ctrl Pts',(-4.74477333857637,6.335271025521,-12.));
#26796=CARTESIAN_POINT('Ctrl Pts',(-4.76392528750574,6.31871688954409,-12.));
#26797=CARTESIAN_POINT('Ctrl Pts',(-4.78300102096013,6.30206743426034,-12.));
#26798=CARTESIAN_POINT('Ctrl Pts',(-4.80076087470544,6.28656648948747,-12.));
#26799=CARTESIAN_POINT('Ctrl Pts',(-4.81844738080901,6.27098927612685,-12.));
#26800=CARTESIAN_POINT('Ctrl Pts',(-4.83605920704347,6.25533688403005,-12.));
#26801=CARTESIAN_POINT('Ctrl Pts',(-4.98998560019154,6.11853583753291,-12.));
#26802=CARTESIAN_POINT('Ctrl Pts',(-5.13823022853012,5.97597793328466,-12.));
#26803=CARTESIAN_POINT('Ctrl Pts',(-5.28041162847577,5.82790909191958,-12.));
#26804=CARTESIAN_POINT('Ctrl Pts',(-5.3200731840196,5.78660523235457,-12.));
#26805=CARTESIAN_POINT('Ctrl Pts',(-5.35926272427924,5.7448723237564,-12.));
#26806=CARTESIAN_POINT('Ctrl Pts',(-5.39797144463395,5.70271520266639,-12.));
#26807=CARTESIAN_POINT('Ctrl Pts',(-5.53713035840687,5.55115919345398,-12.));
#26808=CARTESIAN_POINT('Ctrl Pts',(-5.67007843949,5.39412278717484,-12.));
#26809=CARTESIAN_POINT('Ctrl Pts',(-5.79659171905523,5.23204541990698,-12.));
#26810=CARTESIAN_POINT('Ctrl Pts',(-5.92308395045967,5.06999501763838,-12.));
#26811=CARTESIAN_POINT('Ctrl Pts',(-6.04314381583919,4.90290466648765,-12.));
#26812=CARTESIAN_POINT('Ctrl Pts',(-6.156500947101,4.73119033966662,-12.));
#26813=CARTESIAN_POINT('Ctrl Pts',(-6.26858470722818,4.56140492604889,-12.));
#26814=CARTESIAN_POINT('Ctrl Pts',(-6.37411567091608,4.38709818520557,-12.));
#26815=CARTESIAN_POINT('Ctrl Pts',(-6.47278349120591,4.2086593522812,-12.));
#26816=CARTESIAN_POINT('Ctrl Pts',(-6.51321507587661,4.13553961820042,-12.));
#26817=CARTESIAN_POINT('Ctrl Pts',(-6.55249364177314,4.06172594602181,-12.));
#26818=CARTESIAN_POINT('Ctrl Pts',(-6.59059529994264,3.98724486729933,-12.));
#26819=CARTESIAN_POINT('Ctrl Pts',(-6.60144172394684,3.96604228980204,-12.));
#26820=CARTESIAN_POINT('Ctrl Pts',(-6.61219276497738,3.94478562717274,-12.));
#26821=CARTESIAN_POINT('Ctrl Pts',(-6.6228478491971,3.92347549122676,-12.));
#26822=CARTESIAN_POINT('Ctrl Pts',(-6.63395017846395,3.90127086655045,-12.));
#26823=CARTESIAN_POINT('Ctrl Pts',(-6.64494485744702,3.87901508051083,-12.));
#26824=CARTESIAN_POINT('Ctrl Pts',(-6.65582886907332,3.85671429052793,-12.));
#26825=CARTESIAN_POINT('Ctrl Pts',(-6.74450049838414,3.67503060159064,-12.));
#26826=CARTESIAN_POINT('Ctrl Pts',(-6.82588701051427,3.49024918380503,-12.));
#26827=CARTESIAN_POINT('Ctrl Pts',(-6.89978215814578,3.30278705893769,-12.));
#26828=CARTESIAN_POINT('Ctrl Pts',(-6.97319794291742,3.11654101365302,-12.));
#26829=CARTESIAN_POINT('Ctrl Pts',(-7.03921944728565,2.92764827330257,-12.));
#26830=CARTESIAN_POINT('Ctrl Pts',(-7.09759598960971,2.73650163274067,-12.));
#26831=CARTESIAN_POINT('Ctrl Pts',(-7.13572390240132,2.61165658108795,-12.));
#26832=CARTESIAN_POINT('Ctrl Pts',(-7.17058956881407,2.48584973535233,-12.));
#26833=CARTESIAN_POINT('Ctrl Pts',(-7.20211123196002,2.35918876245064,-12.));
#26834=CARTESIAN_POINT('Ctrl Pts',(-7.25068389468356,2.16401312439806,-12.));
#26835=CARTESIAN_POINT('Ctrl Pts',(-7.29131871208896,1.96680886809969,-12.));
#26836=CARTESIAN_POINT('Ctrl Pts',(-7.32397220360618,1.76806533469225,-12.));
#26837=CARTESIAN_POINT('Ctrl Pts',(-7.34491006029522,1.64062831564753,-12.));
#26838=CARTESIAN_POINT('Ctrl Pts',(-7.36256531297852,1.51255845860445,-12.));
#26839=CARTESIAN_POINT('Ctrl Pts',(-7.37691540720549,1.38398700277358,-12.));
#26840=CARTESIAN_POINT('Ctrl Pts',(-7.38319357342979,1.32773699084752,-12.));
#26841=CARTESIAN_POINT('Ctrl Pts',(-7.38883900049354,1.27139100187669,-12.));
#26842=CARTESIAN_POINT('Ctrl Pts',(-7.3938492823474,1.21496020175245,-12.));
#26843=CARTESIAN_POINT('Ctrl Pts',(-7.3971413694576,1.17788142751856,-12.));
#26844=CARTESIAN_POINT('Ctrl Pts',(-7.40015928907374,1.14076530742901,-12.));
#26845=CARTESIAN_POINT('Ctrl Pts',(-7.40290212229044,1.10361724454502,-12.));
#26846=CARTESIAN_POINT('Ctrl Pts',(-7.4050102017394,1.07506608530655,-12.));
#26847=CARTESIAN_POINT('Ctrl Pts',(-7.40695526086128,1.04650256796338,-12.));
#26848=CARTESIAN_POINT('Ctrl Pts',(-7.40873654184619,1.01794082405229,-12.));
#26849=CARTESIAN_POINT('Ctrl Pts',(-7.42105643069599,0.820398991336265,
-12.));
#26850=CARTESIAN_POINT('Ctrl Pts',(-7.42556039755354,0.622752454170974,
-12.));
#26851=CARTESIAN_POINT('Ctrl Pts',(-7.42228121331595,0.425466835953437,
-12.));
#26852=CARTESIAN_POINT('Ctrl Pts',(-7.41900759948271,0.228516350068992,
-12.));
#26853=CARTESIAN_POINT('Ctrl Pts',(-7.40797716007023,0.0319248474341827,
-12.));
#26854=CARTESIAN_POINT('Ctrl Pts',(-7.38917084323832,-0.163840412592323,
-12.));
#26855=CARTESIAN_POINT('Ctrl Pts',(-7.37064698047464,-0.356665453403957,
-12.));
#26856=CARTESIAN_POINT('Ctrl Pts',(-7.34457887203224,-0.548689509627672,
-12.));
#26857=CARTESIAN_POINT('Ctrl Pts',(-7.31090041837079,-0.739452309249457,
-12.));
#26858=CARTESIAN_POINT('Ctrl Pts',(-7.27732639532349,-0.929623588948032,
-12.));
#26859=CARTESIAN_POINT('Ctrl Pts',(-7.23618907077922,-1.11854204252748,
-12.));
#26860=CARTESIAN_POINT('Ctrl Pts',(-7.18737683938924,-1.30572860229432,
-12.));
#26861=CARTESIAN_POINT('Ctrl Pts',(-7.16523608895308,-1.39063459382108,
-12.));
#26862=CARTESIAN_POINT('Ctrl Pts',(-7.1415156188337,-1.4751838814727,-12.));
#26863=CARTESIAN_POINT('Ctrl Pts',(-7.11622968390057,-1.55933456460308,
-12.));
#26864=CARTESIAN_POINT('Ctrl Pts',(-7.10233271497777,-1.60558317796809,
-12.));
#26865=CARTESIAN_POINT('Ctrl Pts',(-7.0879631508151,-1.65171049264756,-12.));
#26866=CARTESIAN_POINT('Ctrl Pts',(-7.07312223630299,-1.69771223090791,
-12.));
#26867=CARTESIAN_POINT('Ctrl Pts',(-7.06252436985534,-1.73056197733326,
-12.));
#26868=CARTESIAN_POINT('Ctrl Pts',(-7.05168654666488,-1.76334603356747,
-12.));
#26869=CARTESIAN_POINT('Ctrl Pts',(-7.04061734154373,-1.79603977674457,
-12.));
#26870=CARTESIAN_POINT('Ctrl Pts',(-6.97824817291142,-1.98025188223161,
-12.));
#26871=CARTESIAN_POINT('Ctrl Pts',(-6.9084880736702,-2.16175440112574,-12.));
#26872=CARTESIAN_POINT('Ctrl Pts',(-6.8315746844225,-2.34012772253663,-12.));
#26873=CARTESIAN_POINT('Ctrl Pts',(-6.75497533051359,-2.51777275038292,
-12.));
#26874=CARTESIAN_POINT('Ctrl Pts',(-6.6712805458415,-2.692314665458,-12.));
#26875=CARTESIAN_POINT('Ctrl Pts',(-6.58068264349192,-2.86331016757811,
-12.));
#26876=CARTESIAN_POINT('Ctrl Pts',(-6.51303849165583,-2.99098250224288,
-12.));
#26877=CARTESIAN_POINT('Ctrl Pts',(-6.44154513202555,-3.11667726552047,
-12.));
#26878=CARTESIAN_POINT('Ctrl Pts',(-6.36626922663613,-3.24019647395781,
-12.));
#26879=CARTESIAN_POINT('Ctrl Pts',(-6.35043403970592,-3.26618021663031,
-12.));
#26880=CARTESIAN_POINT('Ctrl Pts',(-6.33443045330557,-3.29206910604144,
-12.));
#26881=CARTESIAN_POINT('Ctrl Pts',(-6.31826810705525,-3.31784702408304,
-12.));
#26882=CARTESIAN_POINT('Ctrl Pts',(-6.21663338877916,-3.47994795901695,
-12.));
#26883=CARTESIAN_POINT('Ctrl Pts',(-6.1086510172057,-3.63778508480432,-12.));
#26884=CARTESIAN_POINT('Ctrl Pts',(-5.99452112277152,-3.79093554557209,
-12.));
#26885=CARTESIAN_POINT('Ctrl Pts',(-5.88191571230597,-3.94204030724072,
-12.));
#26886=CARTESIAN_POINT('Ctrl Pts',(-5.76332545430664,-4.08858323886591,
-12.));
#26887=CARTESIAN_POINT('Ctrl Pts',(-5.63890846824723,-4.23012099994035,
-12.));
#26888=CARTESIAN_POINT('Ctrl Pts',(-5.58859725063955,-4.28735544455003,
-12.));
#26889=CARTESIAN_POINT('Ctrl Pts',(-5.53733289315066,-4.34377097792458,
-12.));
#26890=CARTESIAN_POINT('Ctrl Pts',(-5.48512449108,-4.39933625912037,-12.));
#26891=CARTESIAN_POINT('Ctrl Pts',(-5.42813643108429,-4.45998851915659,
-12.));
#26892=CARTESIAN_POINT('Ctrl Pts',(-5.37002354987675,-4.51962773802353,
-12.));
#26893=CARTESIAN_POINT('Ctrl Pts',(-5.31081700063333,-4.57822770314271,
-12.));
#26894=CARTESIAN_POINT('Origin',(2.22044604925031E-15,-4.16333634234434E-16,
12.));
#26895=CARTESIAN_POINT('',(15.1652636634099,-5.0941581860707,12.));
#26896=CARTESIAN_POINT('',(15.8449177974003,-2.20777027769627,12.));
#26897=CARTESIAN_POINT('Origin',(0.,0.,12.));
#26898=CARTESIAN_POINT('',(15.3516930915734,-2.13904623492406,11.9999999854331));
#26899=CARTESIAN_POINT('',(15.8449177974003,-2.20777027769627,12.));
#26900=CARTESIAN_POINT('',(15.4951571010802,0.387435137602754,11.9999999854331));
#26901=CARTESIAN_POINT('Origin',(2.22044604925031E-15,-4.16333634234434E-16,
12.));
#26902=CARTESIAN_POINT('',(15.9929910697025,0.399882795164268,12.));
#26903=CARTESIAN_POINT('',(15.4951570863814,0.387435139568728,12.));
#26904=CARTESIAN_POINT('',(15.6444542379842,3.34465561770867,12.));
#26905=CARTESIAN_POINT('Origin',(0.,0.,12.));
#26906=CARTESIAN_POINT('',(15.1574696145705,3.24054230899359,11.9999999854331));
#26907=CARTESIAN_POINT('',(15.6444542379842,3.34465561770867,12.));
#26908=CARTESIAN_POINT('',(14.4281741645111,5.66372579240368,11.9999999854331));
#26909=CARTESIAN_POINT('Origin',(2.22044604925031E-15,-4.16333634234434E-16,
12.));
#26910=CARTESIAN_POINT('',(14.8917277215788,5.8456920096609,12.));
#26911=CARTESIAN_POINT('',(14.4281741500264,5.66372578922383,12.));
#26912=CARTESIAN_POINT('',(13.5570386099129,8.4936666837582,12.));
#26913=CARTESIAN_POINT('Origin',(0.,0.,12.));
#26914=CARTESIAN_POINT('',(13.1350316016236,8.22927362513566,11.9999999854331));
#26915=CARTESIAN_POINT('',(13.5570386099129,8.4936666837582,12.));
#26916=CARTESIAN_POINT('',(11.6209404865298,10.2568875289503,11.9999999854331));
#26917=CARTESIAN_POINT('Origin',(2.22044604925031E-15,-4.16333634234434E-16,
12.));
#26918=CARTESIAN_POINT('',(11.9943022317386,10.5864244945667,12.));
#26919=CARTESIAN_POINT('',(11.6209404740062,10.2568875210082,12.));
#26920=CARTESIAN_POINT('',(9.83444404490535,12.6182161945767,12.));
#26921=CARTESIAN_POINT('Origin',(0.,0.,12.));
#26922=CARTESIAN_POINT('',(9.52831492510037,12.2254330909426,11.9999999854331));
#26923=CARTESIAN_POINT('',(9.83444404490536,12.6182161945767,12.));
#26924=CARTESIAN_POINT('',(7.41204987905737,13.6129172539676,11.9999999854331));
#26925=CARTESIAN_POINT('Origin',(2.22044604925031E-15,-4.16333634234434E-16,
12.));
#26926=CARTESIAN_POINT('',(7.65018687570268,14.0502779464422,12.));
#26927=CARTESIAN_POINT('',(7.41204987000543,13.6129172422212,12.));
#26928=CARTESIAN_POINT('',(4.92567038714607,15.2208226072918,12.));
#26929=CARTESIAN_POINT('Origin',(0.,0.,12.));
#26930=CARTESIAN_POINT('',(4.77234284565852,14.7470248978055,11.9999999854331));
#26931=CARTESIAN_POINT('',(4.92567038714608,15.2208226072918,12.));
#26932=CARTESIAN_POINT('',(2.30915666596483,15.3270282528948,11.9999999854331));
#26933=CARTESIAN_POINT('Origin',(2.22044604925031E-15,-4.16333634234434E-16,
12.));
#26934=CARTESIAN_POINT('',(2.38334607772337,15.8194605179587,12.));
#26935=CARTESIAN_POINT('',(2.30915666147631,15.3270282387607,12.));
#26936=CARTESIAN_POINT('',(-0.577211814455682,15.9875731781501,12.));
#26937=CARTESIAN_POINT('Origin',(0.,0.,12.));
#26938=CARTESIAN_POINT('',(-0.559244213248937,15.4899078590853,11.9999999854331));
#26939=CARTESIAN_POINT('',(-0.577211814455683,15.9875731781501,12.));
#26940=CARTESIAN_POINT('',(-3.0722549205659,15.1924734416771,11.9999999854331));
#26941=CARTESIAN_POINT('Origin',(2.22044604925031E-15,-4.16333634234434E-16,
12.));
#26942=CARTESIAN_POINT('',(-3.17096143167129,15.6805826806374,12.));
#26943=CARTESIAN_POINT('',(-3.07225491994961,15.1924734268603,12.));
#26944=CARTESIAN_POINT('',(-6.01047375249498,14.825986472273,12.));
#26945=CARTESIAN_POINT('Origin',(0.,0.,12.));
#26946=CARTESIAN_POINT('',(-5.823378166473,14.3644793258666,11.9999999854331));
#26947=CARTESIAN_POINT('',(-6.01047375249498,14.825986472273,12.));
#26948=CARTESIAN_POINT('',(-8.08310722202279,13.2254821163649,11.9999999854331));
#26949=CARTESIAN_POINT('Origin',(2.22044604925031E-15,-4.16333634234434E-16,
12.));
#26950=CARTESIAN_POINT('',(-8.34280419399984,13.6503951512779,12.));
#26951=CARTESIAN_POINT('',(-8.08310721637601,13.2254821026524,12.));
#26952=CARTESIAN_POINT('',(-10.7187838508382,11.8761669895831,12.));
#26953=CARTESIAN_POINT('Origin',(0.,0.,12.));
#26954=CARTESIAN_POINT('',(-10.3851267689119,11.5064825888119,11.9999999854331));
#26955=CARTESIAN_POINT('',(-10.7187838508382,11.8761669895831,12.));
#26956=CARTESIAN_POINT('',(-12.1190174985463,9.6633024604911,11.9999999854331));
#26957=CARTESIAN_POINT('Origin',(2.22044604925031E-15,-4.16333634234434E-16,
12.));
#26958=CARTESIAN_POINT('',(-12.5083816438555,9.97376850829778,12.));
#26959=CARTESIAN_POINT('',(-12.1190174885501,9.66330244953692,12.));
#26960=CARTESIAN_POINT('',(-14.1342504243686,7.49390649439194,12.));
#26961=CARTESIAN_POINT('Origin',(0.,0.,12.));
#26962=CARTESIAN_POINT('',(-13.6942758148726,7.26063423394962,11.9999999854331));
#26963=CARTESIAN_POINT('',(-14.1342504243686,7.49390649439194,12.));
#26964=CARTESIAN_POINT('',(-14.6931954070957,4.93558591272671,11.9999999854331));
#26965=CARTESIAN_POINT('Origin',(2.22044604925031E-15,-4.16333634234434E-16,
12.));
#26966=CARTESIAN_POINT('',(-15.1652636634099,5.09415818607069,12.));
#26967=CARTESIAN_POINT('',(-14.6931953939558,4.93558590585204,12.));
#26968=CARTESIAN_POINT('',(-15.8449177974003,2.20777027769626,12.));
#26969=CARTESIAN_POINT('Origin',(0.,0.,12.));
#26970=CARTESIAN_POINT('',(-15.3516930915734,2.13904623492405,11.9999999854331));
#26971=CARTESIAN_POINT('',(-15.8449177974003,2.20777027769626,12.));
#26972=CARTESIAN_POINT('',(-15.4951571010802,-0.387435137602753,11.9999999854331));
#26973=CARTESIAN_POINT('Origin',(2.22044604925031E-15,-4.16333634234434E-16,
12.));
#26974=CARTESIAN_POINT('',(-15.9929910697025,-0.399882795164266,12.));
#26975=CARTESIAN_POINT('',(-15.4951570863814,-0.387435139568727,12.));
#26976=CARTESIAN_POINT('',(-15.6444542379842,-3.34465561770867,12.));
#26977=CARTESIAN_POINT('Origin',(0.,0.,12.));
#26978=CARTESIAN_POINT('',(-15.1574696145705,-3.24054230899359,11.9999999854331));
#26979=CARTESIAN_POINT('',(-15.6444542379842,-3.34465561770867,12.));
#26980=CARTESIAN_POINT('',(-14.4281741645111,-5.66372579240368,11.9999999854331));
#26981=CARTESIAN_POINT('Origin',(2.22044604925031E-15,-4.16333634234434E-16,
12.));
#26982=CARTESIAN_POINT('',(-14.8917277215788,-5.8456920096609,12.));
#26983=CARTESIAN_POINT('',(-14.4281741500264,-5.66372578922383,12.));
#26984=CARTESIAN_POINT('',(-13.5570386099129,-8.4936666837582,12.));
#26985=CARTESIAN_POINT('Origin',(0.,0.,12.));
#26986=CARTESIAN_POINT('',(-13.1350316016236,-8.22927362513566,11.9999999854331));
#26987=CARTESIAN_POINT('',(-13.5570386099129,-8.4936666837582,12.));
#26988=CARTESIAN_POINT('',(-11.6209404865298,-10.2568875289503,11.9999999854331));
#26989=CARTESIAN_POINT('Origin',(2.22044604925031E-15,-4.16333634234434E-16,
12.));
#26990=CARTESIAN_POINT('',(-11.9943022317386,-10.5864244945667,12.));
#26991=CARTESIAN_POINT('',(-11.6209404740062,-10.2568875210082,12.));
#26992=CARTESIAN_POINT('',(-9.83444404490535,-12.6182161945767,12.));
#26993=CARTESIAN_POINT('Origin',(0.,0.,12.));
#26994=CARTESIAN_POINT('',(-9.52831492510037,-12.2254330909426,11.9999999854331));
#26995=CARTESIAN_POINT('',(-9.83444404490535,-12.6182161945767,12.));
#26996=CARTESIAN_POINT('',(-7.41204987905737,-13.6129172539676,11.9999999854331));
#26997=CARTESIAN_POINT('Origin',(2.22044604925031E-15,-4.16333634234434E-16,
12.));
#26998=CARTESIAN_POINT('',(-7.65018687570268,-14.0502779464422,12.));
#26999=CARTESIAN_POINT('',(-7.41204987000543,-13.6129172422212,12.));
#27000=CARTESIAN_POINT('',(-4.92567038714607,-15.2208226072918,12.));
#27001=CARTESIAN_POINT('Origin',(0.,0.,12.));
#27002=CARTESIAN_POINT('',(-4.77234284565852,-14.7470248978055,11.9999999854331));
#27003=CARTESIAN_POINT('',(-4.92567038714608,-15.2208226072918,12.));
#27004=CARTESIAN_POINT('',(-2.30915666596483,-15.3270282528948,11.9999999854331));
#27005=CARTESIAN_POINT('Origin',(2.22044604925031E-15,-4.16333634234434E-16,
12.));
#27006=CARTESIAN_POINT('',(-2.38334607772337,-15.8194605179587,12.));
#27007=CARTESIAN_POINT('',(-2.30915666147631,-15.3270282387607,12.));
#27008=CARTESIAN_POINT('',(0.577211814455688,-15.9875731781501,12.));
#27009=CARTESIAN_POINT('Origin',(0.,0.,12.));
#27010=CARTESIAN_POINT('',(0.559244213248943,-15.4899078590853,11.9999999854331));
#27011=CARTESIAN_POINT('',(0.577211814455689,-15.9875731781501,12.));
#27012=CARTESIAN_POINT('',(3.0722549205659,-15.1924734416771,11.9999999854331));
#27013=CARTESIAN_POINT('Origin',(2.22044604925031E-15,-4.16333634234434E-16,
12.));
#27014=CARTESIAN_POINT('',(3.1709614316713,-15.6805826806374,12.));
#27015=CARTESIAN_POINT('',(3.07225491994961,-15.1924734268603,12.));
#27016=CARTESIAN_POINT('',(6.01047375249498,-14.825986472273,12.));
#27017=CARTESIAN_POINT('Origin',(0.,0.,12.));
#27018=CARTESIAN_POINT('',(5.823378166473,-14.3644793258666,11.9999999854331));
#27019=CARTESIAN_POINT('',(6.01047375249497,-14.825986472273,12.));
#27020=CARTESIAN_POINT('',(8.0831072220228,-13.2254821163649,11.9999999854331));
#27021=CARTESIAN_POINT('Origin',(2.22044604925031E-15,-4.16333634234434E-16,
12.));
#27022=CARTESIAN_POINT('',(8.34280419399985,-13.6503951512779,12.));
#27023=CARTESIAN_POINT('',(8.08310721637602,-13.2254821026524,12.));
#27024=CARTESIAN_POINT('',(10.7187838508382,-11.8761669895831,12.));
#27025=CARTESIAN_POINT('Origin',(0.,0.,12.));
#27026=CARTESIAN_POINT('',(10.385126768912,-11.506482588812,11.9999999854331));
#27027=CARTESIAN_POINT('',(10.7187838508382,-11.8761669895831,12.));
#27028=CARTESIAN_POINT('',(12.1190174985463,-9.6633024604911,11.9999999854331));
#27029=CARTESIAN_POINT('Origin',(2.22044604925031E-15,-4.16333634234434E-16,
12.));
#27030=CARTESIAN_POINT('',(12.5083816438555,-9.97376850829778,12.));
#27031=CARTESIAN_POINT('',(12.1190174885501,-9.66330244953692,12.));
#27032=CARTESIAN_POINT('',(14.1342504243686,-7.49390649439194,12.));
#27033=CARTESIAN_POINT('Origin',(0.,0.,12.));
#27034=CARTESIAN_POINT('',(13.6942758148726,-7.26063423394962,11.9999999854331));
#27035=CARTESIAN_POINT('',(14.1342504243686,-7.49390649439194,12.));
#27036=CARTESIAN_POINT('',(14.6931954070957,-4.93558591272672,11.9999999854331));
#27037=CARTESIAN_POINT('Origin',(2.22044604925031E-15,-4.16333634234434E-16,
12.));
#27038=CARTESIAN_POINT('',(14.6931953939558,-4.93558590585205,12.));
#27039=CARTESIAN_POINT('Origin',(0.,-23.1141426487074,8.));
#27040=CARTESIAN_POINT('',(16.9018270974371,-10.6886774987574,8.00000000095189));
#27041=CARTESIAN_POINT('',(16.9029194185226,-10.6907051200357,8.00000000000001));
#27042=CARTESIAN_POINT('',(16.901826662391,-10.6886766938315,8.00000000000001));
#27043=CARTESIAN_POINT('',(15.9309316922789,-12.0882174594936,8.00000000066043));
#27044=CARTESIAN_POINT('Origin',(0.,0.,8.));
#27045=CARTESIAN_POINT('',(15.9332134908661,-12.0885304601968,8.00000000000001));
#27046=CARTESIAN_POINT('',(15.9332134908661,-12.0885304601968,8.00000000000001));
#27047=CARTESIAN_POINT('Origin',(-0.00247907756725008,0.00171979730317018,
8.));
#27048=CARTESIAN_POINT('Origin',(0.,-23.1141426487074,8.));
#27049=CARTESIAN_POINT('',(12.22677921905,-15.8248366763907,8.00000000093426));
#27050=CARTESIAN_POINT('',(12.2271131583396,-15.8271170588848,8.00000001165519));
#27051=CARTESIAN_POINT('',(12.2267790880642,-15.8248357882219,7.99999999999988));
#27052=CARTESIAN_POINT('',(10.8357650986362,-16.8079082773193,8.00000000066548));
#27053=CARTESIAN_POINT('Origin',(0.,0.,8.));
#27054=CARTESIAN_POINT('',(10.8378022221802,-16.8089828313771,8.));
#27055=CARTESIAN_POINT('',(10.8378022221802,-16.8089828313771,8.));
#27056=CARTESIAN_POINT('Origin',(-0.00174136557906213,0.00246397530291764,
8.));
#27057=CARTESIAN_POINT('Origin',(0.,-23.1141426487074,8.));
#27058=CARTESIAN_POINT('',(6.07700129997158,-19.0522870308522,8.00000000093426));
#27059=CARTESIAN_POINT('',(6.07653516349412,-19.0545441034233,8.00000001165519));
#27060=CARTESIAN_POINT('',(6.07700148065507,-19.0522861514548,7.99999999999989));
#27061=CARTESIAN_POINT('',(4.43364529035575,-19.5003173146329,8.00000000066041));
#27062=CARTESIAN_POINT('Origin',(0.,0.,8.));
#27063=CARTESIAN_POINT('',(4.43519205657354,-19.5020237989274,8.00000000000001));
#27064=CARTESIAN_POINT('',(4.43519205657354,-19.5020237989274,8.00000000000001));
#27065=CARTESIAN_POINT('Origin',(-0.000793619201507889,0.00291096152692738,
8.));
#27066=CARTESIAN_POINT('Origin',(0.,-23.1141426487074,8.));
#27067=CARTESIAN_POINT('',(-0.805752662867996,-19.9817503875941,8.00000000093425));
#27068=CARTESIAN_POINT('',(-0.806962652176574,-19.9837119139682,8.00000001165519));
#27069=CARTESIAN_POINT('',(-0.80575219231358,-19.981749623035,7.99999999999988));
#27070=CARTESIAN_POINT('',(-2.50323756031562,-19.8407002812071,8.00000000066041));
#27071=CARTESIAN_POINT('Origin',(0.,0.,8.));
#27072=CARTESIAN_POINT('',(-2.50236772751931,-19.8428328771094,8.));
#27073=CARTESIAN_POINT('',(-2.50236772751931,-19.8428328771094,8.));
#27074=CARTESIAN_POINT('Origin',(0.00024984937073258,0.00300684281118402,
8.00000000000001));
#27075=CARTESIAN_POINT('Origin',(0.,-23.1141426487074,8.));
#27076=CARTESIAN_POINT('',(-7.59132096296416,-18.5011197483583,8.00000000093426));
#27077=CARTESIAN_POINT('',(-7.59312886249445,-18.5025491395115,8.00000001165519));
#27078=CARTESIAN_POINT('',(-7.5913202592824,-18.5011191908384,7.99999999999989));
#27079=CARTESIAN_POINT('',(-9.13819300331897,-17.7880019835195,8.00000000066548));
#27080=CARTESIAN_POINT('Origin',(0.,0.,8.));
#27081=CARTESIAN_POINT('',(-9.13810503265895,-17.790303461288,8.));
#27082=CARTESIAN_POINT('',(-9.13810503265895,-17.790303461288,8.));
#27083=CARTESIAN_POINT('Origin',(0.00126318242769763,0.0027400545031897,
8.));
#27084=CARTESIAN_POINT('Origin',(0.,-23.1141426487074,8.));
#27085=CARTESIAN_POINT('',(-13.4612639189362,-14.7889810200223,8.00000000093431));
#27086=CARTESIAN_POINT('',(-13.4634504416559,-14.7897046298329,8.));
#27087=CARTESIAN_POINT('',(-13.461263067007,-14.7889807367977,8.));
#27088=CARTESIAN_POINT('',(-14.6709475311075,-13.5898081101815,8.00000000066043));
#27089=CARTESIAN_POINT('Origin',(0.,0.,8.));
#27090=CARTESIAN_POINT('',(-14.671652006793,-13.5920008911193,8.00000000000001));
#27091=CARTESIAN_POINT('',(-14.671652006793,-13.5920008911193,8.00000000000001));
#27092=CARTESIAN_POINT('Origin',(0.0021241570201247,0.00214277514138717,
8.));
#27093=CARTESIAN_POINT('Origin',(0.,-23.1141426487074,8.));
#27094=CARTESIAN_POINT('',(-17.7075797791827,-9.29307291856211,8.00000000093427));
#27095=CARTESIAN_POINT('',(-17.7098835054945,-9.29300580029393,8.00000001165519));
#27096=CARTESIAN_POINT('',(-17.7075788817646,-9.293072943795,7.99999999999989));
#27097=CARTESIAN_POINT('',(-18.4341692464304,-7.75248283619897,8.00000000066548));
#27098=CARTESIAN_POINT('Origin',(0.,0.,8.));
#27099=CARTESIAN_POINT('',(-18.4355812183855,-7.75430241691263,8.00000000000001));
#27100=CARTESIAN_POINT('',(-18.4355812183855,-7.75430241691263,8.00000000000001));
#27101=CARTESIAN_POINT('Origin',(0.00272892695798221,0.00128704551039749,
8.));
#27102=CARTESIAN_POINT('Origin',(0.,-23.1141426487074,8.));
#27103=CARTESIAN_POINT('',(-19.8181001820145,-2.67628307199986,8.00000000093425));
#27104=CARTESIAN_POINT('',(-19.8202420208341,-2.67543208062671,8.00000001165519));
#27105=CARTESIAN_POINT('',(-19.8180993473604,-2.67628340264097,7.99999999999988));
#27106=CARTESIAN_POINT('',(-19.9739581027431,-0.980093690383901,8.00000000066039));
#27107=CARTESIAN_POINT('Origin',(0.,0.,8.));
#27108=CARTESIAN_POINT('',(-19.9759072548391,-0.981320629910932,8.));
#27109=CARTESIAN_POINT('',(-19.9759072548391,-0.981320629910932,8.));
#27110=CARTESIAN_POINT('Origin',(0.0030045479955132,0.000276079177594091,
8.));
#27111=CARTESIAN_POINT('Origin',(0.,-23.1141426487074,8.));
#27112=CARTESIAN_POINT('',(-19.5382652188964,4.26330601082053,8.00000000093426));
#27113=CARTESIAN_POINT('',(-19.5399868328426,4.2648382331363,8.00000001165519));
#27114=CARTESIAN_POINT('',(-19.5382645476573,4.26330541464507,7.99999999999988));
#27115=CARTESIAN_POINT('',(-19.1045928215184,5.91050920446365,8.00000000066042));
#27116=CARTESIAN_POINT('Origin',(0.,0.,8.));
#27117=CARTESIAN_POINT('',(-19.1068440633666,5.91002290780806,8.00000000000001));
#27118=CARTESIAN_POINT('',(-19.1068440633666,5.91002290780806,8.00000000000001));
#27119=CARTESIAN_POINT('Origin',(0.00291777623414591,-0.000768186374036639,
8.00000000000001));
#27120=CARTESIAN_POINT('Origin',(0.,-23.1141426487074,8.));
#27121=CARTESIAN_POINT('',(-16.9018271162855,10.6886774690337,8.00000000093431));
#27122=CARTESIAN_POINT('',(-16.9029194185225,10.6907051200357,8.));
#27123=CARTESIAN_POINT('',(-16.9018266894279,10.6886766792289,8.));
#27124=CARTESIAN_POINT('',(-15.9309316922789,12.0882174594936,8.00000000066042));
#27125=CARTESIAN_POINT('Origin',(0.,0.,8.));
#27126=CARTESIAN_POINT('',(-15.9332134908661,12.0885304601968,7.99999999999999));
#27127=CARTESIAN_POINT('',(-15.9332134908661,12.0885304601968,7.99999999999999));
#27128=CARTESIAN_POINT('Origin',(0.00247907756889099,-0.00171979730426486,
8.));
#27129=CARTESIAN_POINT('Origin',(0.,-23.1141426487074,8.));
#27130=CARTESIAN_POINT('',(-12.22677921905,15.8248366763907,8.00000000093427));
#27131=CARTESIAN_POINT('',(-12.2271131583396,15.8271170588848,8.00000001165519));
#27132=CARTESIAN_POINT('',(-12.2267790880642,15.8248357882219,7.99999999999989));
#27133=CARTESIAN_POINT('',(-10.8357650986362,16.8079082773193,8.00000000066548));
#27134=CARTESIAN_POINT('Origin',(0.,0.,8.));
#27135=CARTESIAN_POINT('',(-10.8378022221802,16.8089828313771,8.00000000000001));
#27136=CARTESIAN_POINT('',(-10.8378022221802,16.8089828313771,8.00000000000001));
#27137=CARTESIAN_POINT('Origin',(0.00174136557906213,-0.00246397530291764,
8.00000000000001));
#27138=CARTESIAN_POINT('Origin',(0.,-23.1141426487074,8.));
#27139=CARTESIAN_POINT('',(-6.07700129997157,19.0522870308522,8.00000000093426));
#27140=CARTESIAN_POINT('',(-6.07653516349413,19.0545441034233,8.00000001165519));
#27141=CARTESIAN_POINT('',(-6.07700148065505,19.0522861514548,7.99999999999989));
#27142=CARTESIAN_POINT('',(-4.43364529035575,19.5003173146329,8.00000000066041));
#27143=CARTESIAN_POINT('Origin',(0.,0.,8.));
#27144=CARTESIAN_POINT('',(-4.43519205657354,19.5020237989274,8.00000000000001));
#27145=CARTESIAN_POINT('',(-4.43519205657354,19.5020237989274,8.00000000000001));
#27146=CARTESIAN_POINT('Origin',(0.000793619202019702,-0.00291096152836845,
8.00000000000001));
#27147=CARTESIAN_POINT('Origin',(0.,-23.1141426487074,8.));
#27148=CARTESIAN_POINT('',(0.805752662868007,19.9817503875941,8.00000000093425));
#27149=CARTESIAN_POINT('',(0.806962652176586,19.9837119139682,8.00000001165519));
#27150=CARTESIAN_POINT('',(0.805752192313582,19.981749623035,7.99999999999988));
#27151=CARTESIAN_POINT('',(2.50323756031564,19.8407002812071,8.00000000066041));
#27152=CARTESIAN_POINT('Origin',(0.,0.,8.));
#27153=CARTESIAN_POINT('',(2.50236772751932,19.8428328771094,8.00000000000001));
#27154=CARTESIAN_POINT('',(2.50236772751932,19.8428328771094,8.00000000000001));
#27155=CARTESIAN_POINT('Origin',(-0.00024984937056341,-0.00300684281156149,
8.00000000000001));
#27156=CARTESIAN_POINT('Origin',(0.,-23.1141426487074,8.));
#27157=CARTESIAN_POINT('',(7.59132096296184,18.5011197483593,8.00000000093431));
#27158=CARTESIAN_POINT('',(7.59312813310105,18.5025475539703,8.));
#27159=CARTESIAN_POINT('',(7.59132025928104,18.5011191908401,8.));
#27160=CARTESIAN_POINT('',(9.13819300331897,17.7880019835195,8.00000000066548));
#27161=CARTESIAN_POINT('Origin',(0.,0.,8.));
#27162=CARTESIAN_POINT('',(9.13810503265895,17.790303461288,8.));
#27163=CARTESIAN_POINT('',(9.13810503265895,17.790303461288,8.));
#27164=CARTESIAN_POINT('Origin',(-0.00126318241234658,-0.00274005446868619,
8.));
#27165=CARTESIAN_POINT('Origin',(0.,-23.1141426487074,8.));
#27166=CARTESIAN_POINT('',(13.461263918938,14.7889810200206,8.00000000093427));
#27167=CARTESIAN_POINT('',(13.4634516693485,14.789705870287,8.00000001165519));
#27168=CARTESIAN_POINT('',(13.4612630670076,14.7889807367957,7.99999999999988));
#27169=CARTESIAN_POINT('',(14.6709475311075,13.5898081101815,8.00000000066043));
#27170=CARTESIAN_POINT('Origin',(0.,0.,8.));
#27171=CARTESIAN_POINT('',(14.6716520067931,13.5920008911193,8.00000000000001));
#27172=CARTESIAN_POINT('',(14.6716520067931,13.5920008911193,8.00000000000001));
#27173=CARTESIAN_POINT('Origin',(-0.00212415699918145,-0.00214277512075034,
8.));
#27174=CARTESIAN_POINT('Origin',(0.,-23.1141426487074,8.));
#27175=CARTESIAN_POINT('',(17.7075797791828,9.2930729185621,8.00000000093426));
#27176=CARTESIAN_POINT('',(17.7098835054945,9.29300580029393,8.00000001165519));
#27177=CARTESIAN_POINT('',(17.7075788817646,9.29307294379499,7.99999999999988));
#27178=CARTESIAN_POINT('',(18.4341692464304,7.75248283619896,8.00000000066548));
#27179=CARTESIAN_POINT('Origin',(0.,0.,8.));
#27180=CARTESIAN_POINT('',(18.4355812183855,7.75430241691263,8.00000000000001));
#27181=CARTESIAN_POINT('',(18.4355812183855,7.75430241691263,8.00000000000001));
#27182=CARTESIAN_POINT('Origin',(-0.00272892695798221,-0.00128704551039749,
8.));
#27183=CARTESIAN_POINT('Origin',(0.,-23.1141426487074,8.));
#27184=CARTESIAN_POINT('',(19.8181001866742,2.67628303717104,8.00000000095184));
#27185=CARTESIAN_POINT('',(19.8202402830185,2.67543191952935,8.));
#27186=CARTESIAN_POINT('',(19.8180993360536,2.6762833741219,8.));
#27187=CARTESIAN_POINT('',(19.9739581027431,0.9800936903839,8.00000000066039));
#27188=CARTESIAN_POINT('Origin',(0.,0.,8.));
#27189=CARTESIAN_POINT('',(19.9759072548391,0.981320629910934,8.));
#27190=CARTESIAN_POINT('',(19.9759072548391,0.981320629910934,8.));
#27191=CARTESIAN_POINT('Origin',(-0.00300454799559757,-0.000276079177270461,
8.));
#27192=CARTESIAN_POINT('Origin',(0.,-23.1141426487074,8.));
#27193=CARTESIAN_POINT('',(19.5382652113567,-4.26330604517097,8.00000000095186));
#27194=CARTESIAN_POINT('',(19.5399851447315,-4.26483779015038,8.00000000000001));
#27195=CARTESIAN_POINT('',(19.5382645272615,-4.26330543759598,8.00000000000001));
#27196=CARTESIAN_POINT('',(19.1045928261591,-5.91050918942428,8.00000000066548));
#27197=CARTESIAN_POINT('Origin',(0.,0.,8.));
#27198=CARTESIAN_POINT('',(19.1068440633666,-5.91002290780807,8.00000000000001));
#27199=CARTESIAN_POINT('',(19.1068440633666,-5.91002290780807,8.00000000000001));
#27200=CARTESIAN_POINT('Origin',(-0.0029177762343191,0.000768186373893975,
8.));
#27201=CARTESIAN_POINT('Origin',(0.,0.,10.));
#27202=CARTESIAN_POINT('',(14.8535887419165,9.11368652088976,10.5713323675468));
#27203=CARTESIAN_POINT('Origin',(84.1567763450378,-127.862145793829,15.4574255506428));
#27204=CARTESIAN_POINT('',(16.2804344971325,6.21577136145369,10.5713324655957));
#27205=CARTESIAN_POINT('Origin',(59.1130480768744,-141.197517255051,15.4574255505854));
#27206=CARTESIAN_POINT('',(16.2815542228302,6.21606770943294,10.5701811473657));
#27207=CARTESIAN_POINT('',(16.2815542228691,6.21606770944323,10.5701811473257));
#27208=CARTESIAN_POINT('Ctrl Pts',(18.4341692463042,7.75248283719143,8.0000000013502));
#27209=CARTESIAN_POINT('Ctrl Pts',(18.0976291578699,7.40188904813054,8.44613531208677));
#27210=CARTESIAN_POINT('Ctrl Pts',(17.5769004256285,6.91371871607935,9.11066173754706));
#27211=CARTESIAN_POINT('Ctrl Pts',(16.8162268218363,6.45382336227621,9.98587039279228));
#27212=CARTESIAN_POINT('Ctrl Pts',(16.6537681950271,6.36537822880674,10.169193466808));
#27213=CARTESIAN_POINT('Ctrl Pts',(16.3647226969178,6.23920570500999,10.4842294831125));
#27214=CARTESIAN_POINT('Ctrl Pts',(16.2893139084681,6.2181207143498,10.5621995723545));
#27215=CARTESIAN_POINT('Ctrl Pts',(16.2815542228302,6.21606770943295,10.5701811473657));
#27216=CARTESIAN_POINT('',(14.8546432677704,9.11416913747482,10.5701811473657));
#27217=CARTESIAN_POINT('Ctrl Pts',(14.8546432677704,9.11416913747483,10.5701811473657));
#27218=CARTESIAN_POINT('Ctrl Pts',(14.8597660838235,9.11651393900879,10.5645884462914));
#27219=CARTESIAN_POINT('Ctrl Pts',(14.9084174072453,9.13819358907152,10.5117975421207));
#27220=CARTESIAN_POINT('Ctrl Pts',(15.1198127387954,9.20461324531954,10.2967812590607));
#27221=CARTESIAN_POINT('Ctrl Pts',(15.2446732178268,9.23447867692749,10.1745830867788));
#27222=CARTESIAN_POINT('Ctrl Pts',(15.660664811749,9.3162344169338,9.77607160548408));
#27223=CARTESIAN_POINT('Ctrl Pts',(16.0628737176647,9.3664847623405,9.40557671670551));
#27224=CARTESIAN_POINT('Ctrl Pts',(16.9608851316969,9.36432155355651,8.62456347338103));
#27225=CARTESIAN_POINT('Ctrl Pts',(17.3352154811581,9.33918367920404,8.30828898496766));
#27226=CARTESIAN_POINT('Ctrl Pts',(17.7075797799539,9.2930729176553,8.00000000200136));
#27227=CARTESIAN_POINT('',(14.8535890570749,9.11368666787079,10.5713320220547));
#27228=CARTESIAN_POINT('Origin',(0.,0.,10.));
#27229=CARTESIAN_POINT('',(10.8407433628677,13.644290522247,10.5713323675468));
#27230=CARTESIAN_POINT('Origin',(122.81293115029,-91.3678021723692,15.4574255506302));
#27231=CARTESIAN_POINT('',(13.1726851506206,11.4091510222243,10.5713324600808));
#27232=CARTESIAN_POINT('Origin',(103.840490158678,-112.464411861885,15.4574255506843));
#27233=CARTESIAN_POINT('',(13.1736359892169,11.4098124657167,10.5701811473657));
#27234=CARTESIAN_POINT('',(13.1736359892499,11.4098124657397,10.5701811473257));
#27235=CARTESIAN_POINT('Ctrl Pts',(14.6709475306549,13.5898081110632,8.00000000133987));
#27236=CARTESIAN_POINT('Ctrl Pts',(14.3604369828165,12.8867251148482,8.70558327641035));
#27237=CARTESIAN_POINT('Ctrl Pts',(14.0026935284487,12.3256974886778,9.34347607836948));
#27238=CARTESIAN_POINT('Ctrl Pts',(13.5537520758817,11.7645428250857,10.0506526867367));
#27239=CARTESIAN_POINT('Ctrl Pts',(13.4343328006559,11.6419837068836,10.2211211362091));
#27240=CARTESIAN_POINT('Ctrl Pts',(13.2466269841097,11.4634026012673,10.4799221943139));
#27241=CARTESIAN_POINT('Ctrl Pts',(13.1815445130367,11.415313000214,10.560601969236));
#27242=CARTESIAN_POINT('Ctrl Pts',(13.1736359892169,11.4098124657167,10.5701811473657));
#27243=CARTESIAN_POINT('',(10.8415692284374,13.6451047025743,10.5701811473657));
#27244=CARTESIAN_POINT('Ctrl Pts',(10.8415692284374,13.6451047025743,10.5701811473657));
#27245=CARTESIAN_POINT('Ctrl Pts',(10.8455842606271,13.6490632866647,10.5645840842365));
#27246=CARTESIAN_POINT('Ctrl Pts',(10.883887975225,13.6860750821818,10.5117924805975));
#27247=CARTESIAN_POINT('Ctrl Pts',(11.0598138704061,13.8207873220949,10.29678118048));
#27248=CARTESIAN_POINT('Ctrl Pts',(11.1669292473831,13.8915559581339,10.1745837097664));
#27249=CARTESIAN_POINT('Ctrl Pts',(11.5298621847818,14.110652648375,9.77608272381361));
#27250=CARTESIAN_POINT('Ctrl Pts',(11.8906295678059,14.2954387244256,9.40558508351274));
#27251=CARTESIAN_POINT('Ctrl Pts',(12.7352323400834,14.6005479099196,8.62456348537514));
#27252=CARTESIAN_POINT('Ctrl Pts',(13.0955850513573,14.7049548519353,8.30828904986755));
#27253=CARTESIAN_POINT('Ctrl Pts',(13.4612639199729,14.7889810194323,8.00000000200137));
#27254=CARTESIAN_POINT('',(10.8407436087492,13.6442907681545,10.5713320220547));
#27255=CARTESIAN_POINT('Origin',(0.,0.,10.));
#27256=CARTESIAN_POINT('',(5.52034434192461,16.5291917183393,10.5713323675469));
#27257=CARTESIAN_POINT('Origin',(146.656033934188,-43.8531531648588,15.4574255506454));
#27258=CARTESIAN_POINT('',(8.47611556230388,15.2264186862092,10.5713324655952));
#27259=CARTESIAN_POINT('Origin',(136.043236604389,-70.1664386002706,15.4574255506333));
#27260=CARTESIAN_POINT('',(8.47678283314335,15.2273654477372,10.5701811473657));
#27261=CARTESIAN_POINT('',(8.47678283315298,15.2273654477509,10.5701811473491));
#27262=CARTESIAN_POINT('Ctrl Pts',(9.13819300258433,17.7880019841986,8.0000000013502));
#27263=CARTESIAN_POINT('Ctrl Pts',(9.1057333419349,17.3029234088212,8.44630493034894));
#27264=CARTESIAN_POINT('Ctrl Pts',(9.02059000744949,16.5943080601136,9.11078948273925));
#27265=CARTESIAN_POINT('Ctrl Pts',(8.73353860606274,15.7531796317961,9.98586915522852));
#27266=CARTESIAN_POINT('Ctrl Pts',(8.66593979429594,15.5809995444073,10.1691927873516));
#27267=CARTESIAN_POINT('Ctrl Pts',(8.52562343281535,15.2985565384195,10.4842223372029));
#27268=CARTESIAN_POINT('Ctrl Pts',(8.48141008850886,15.2339297120029,10.5621950204523));
#27269=CARTESIAN_POINT('Ctrl Pts',(8.47678283314336,15.2273654477372,10.5701811473657));
#27270=CARTESIAN_POINT('',(5.52084193563401,16.5302392602455,10.5701811473657));
#27271=CARTESIAN_POINT('Ctrl Pts',(5.52084193563401,16.5302392602455,10.5701811473657));
#27272=CARTESIAN_POINT('Ctrl Pts',(5.52567641619241,16.540418080074,10.5589950747589));
#27273=CARTESIAN_POINT('Ctrl Pts',(5.5781171184741,16.6458555011213,10.4424799720176));
#27274=CARTESIAN_POINT('Ctrl Pts',(5.81421816143414,16.9698353195168,10.0598387239416));
#27275=CARTESIAN_POINT('Ctrl Pts',(5.98506360658063,17.1780723224927,9.80772177835393));
#27276=CARTESIAN_POINT('Ctrl Pts',(6.56710234337044,17.7566384813563,9.06700837109431));
#27277=CARTESIAN_POINT('Ctrl Pts',(7.02051088852432,18.1312684084711,8.55884949994453));
#27278=CARTESIAN_POINT('Ctrl Pts',(7.59132096413546,18.5011197481603,8.00000000200138));
#27279=CARTESIAN_POINT('',(5.52034448887238,16.5291920335133,10.5713320220547));
#27280=CARTESIAN_POINT('Origin',(0.,0.,10.));
#27281=CARTESIAN_POINT('',(-0.465889678260082,17.4204284483111,10.5713323675468));
#27282=CARTESIAN_POINT('Origin',(152.810254612387,8.95083331849518,15.457425550625));
#27283=CARTESIAN_POINT('',(2.757201345432,17.2071555398934,10.571332465597));
#27284=CARTESIAN_POINT('Origin',(151.837160932365,-19.4053572977299,15.4574255506596));
#27285=CARTESIAN_POINT('',(2.75750456340205,17.2082734247813,10.5701811473657));
#27286=CARTESIAN_POINT('',(2.75750456341259,17.2082734248201,10.5701811473257));
#27287=CARTESIAN_POINT('Ctrl Pts',(2.50323755940219,19.8407002815916,8.00000000133983));
#27288=CARTESIAN_POINT('Ctrl Pts',(2.71730857582917,19.1025054196079,8.70559254922064));
#27289=CARTESIAN_POINT('Ctrl Pts',(2.80390036182858,18.4427875325087,9.34347542918631));
#27290=CARTESIAN_POINT('Ctrl Pts',(2.82069736000104,17.7243294684306,10.0506659154585));
#27291=CARTESIAN_POINT('Ctrl Pts',(2.80799094009269,17.5536854982717,10.2211322370019));
#27292=CARTESIAN_POINT('Ctrl Pts',(2.77898047459641,17.2962388867833,10.479925433458));
#27293=CARTESIAN_POINT('Ctrl Pts',(2.76002529911824,17.2175636893543,10.5606090686878));
#27294=CARTESIAN_POINT('Ctrl Pts',(2.75750456340205,17.2082734247813,10.5701811473657));
#27295=CARTESIAN_POINT('',(-0.465780373556083,17.4215830027821,10.5701811473657));
#27296=CARTESIAN_POINT('Ctrl Pts',(-0.465780373556084,17.4215830027821,
10.5701811473657));
#27297=CARTESIAN_POINT('Ctrl Pts',(-0.465251399100026,17.4271731252073,
10.5646071593077));
#27298=CARTESIAN_POINT('Ctrl Pts',(-0.459705523523858,17.4801431215775,
10.5118192507908));
#27299=CARTESIAN_POINT('Ctrl Pts',(-0.411525259581317,17.6964481226821,
10.2967816258166));
#27300=CARTESIAN_POINT('Ctrl Pts',(-0.374958897313839,17.8195161996499,
10.1745804540546));
#27301=CARTESIAN_POINT('Ctrl Pts',(-0.237752210713215,18.2206987157159,
9.77602389544655));
#27302=CARTESIAN_POINT('Ctrl Pts',(-0.0801626929279727,18.5941348378397,
9.40554077366254));
#27303=CARTESIAN_POINT('Ctrl Pts',(0.370700233274875,19.3707182726362,8.62456342312436));
#27304=CARTESIAN_POINT('Ctrl Pts',(0.579637618643333,19.6823290959358,8.30828870776132));
#27305=CARTESIAN_POINT('Ctrl Pts',(0.805752664038896,19.9817503878085,8.00000000200133));
#27306=CARTESIAN_POINT('',(-0.465889647970186,17.4204287947368,10.5713320220547));
#27307=CARTESIAN_POINT('Origin',(0.,0.,10.));
#27308=CARTESIAN_POINT('',(-6.39593052744725,16.2105044092744,10.5713323675468));
#27309=CARTESIAN_POINT('Origin',(140.533303344984,60.6752172033596,15.4574255506187));
#27310=CARTESIAN_POINT('',(-3.29427204554907,17.1124554876038,10.571332460081));
#27311=CARTESIAN_POINT('Origin',(149.317282773282,33.6962964878064,15.4574255506284));
#27312=CARTESIAN_POINT('',(-3.29436945311861,17.1136096597291,10.5701811473657));
#27313=CARTESIAN_POINT('',(-3.29436945312001,17.1136096597458,10.5701811473491));
#27314=CARTESIAN_POINT('Ctrl Pts',(-4.4336452913456,19.5003173146818,8.00000000133982));
#27315=CARTESIAN_POINT('Ctrl Pts',(-3.98000666779979,18.8798574375332,8.70559279101266));
#27316=CARTESIAN_POINT('Ctrl Pts',(-3.67299983374732,18.289541876818,9.34347541242857));
#27317=CARTESIAN_POINT('Ctrl Pts',(-3.41148864538283,17.6201571111346,10.0506658403939));
#27318=CARTESIAN_POINT('Ctrl Pts',(-3.36506521136807,17.4554584510177,10.2211320704509));
#27319=CARTESIAN_POINT('Ctrl Pts',(-3.30427440668142,17.2036153133682,10.4799255162373));
#27320=CARTESIAN_POINT('Ctrl Pts',(-3.29517817846106,17.1232016110272,10.5606092524601));
#27321=CARTESIAN_POINT('Ctrl Pts',(-3.29436945311862,17.1136096597291,10.5701811473657));
#27322=CARTESIAN_POINT('',(-6.39622269550912,16.2116267200016,10.5701811473657));
#27323=CARTESIAN_POINT('Ctrl Pts',(-6.39622269550912,16.2116267200016,10.5701811473657));
#27324=CARTESIAN_POINT('Ctrl Pts',(-6.39764036742581,16.2170714320148,10.5645960857331));
#27325=CARTESIAN_POINT('Ctrl Pts',(-6.41054379697014,16.2687464183021,10.5118064054396));
#27326=CARTESIAN_POINT('Ctrl Pts',(-6.43924755267471,16.4884725819013,10.2967814029678));
#27327=CARTESIAN_POINT('Ctrl Pts',(-6.44697775603165,16.6166234337939,10.1745820042309));
#27328=CARTESIAN_POINT('Ctrl Pts',(-6.45525643928604,17.0405111803984,9.7760521316184));
#27329=CARTESIAN_POINT('Ctrl Pts',(-6.43489762059455,17.4453312682621,9.40556205383272));
#27330=CARTESIAN_POINT('Ctrl Pts',(-6.27683044794119,18.3293083104535,8.62456345283506));
#27331=CARTESIAN_POINT('Ctrl Pts',(-6.18707187916466,18.6935869635504,8.30828887166431));
#27332=CARTESIAN_POINT('Ctrl Pts',(-6.07700129894464,19.0522870314542,8.00000000200134));
#27333=CARTESIAN_POINT('',(-6.39593061746862,16.2105047451678,10.5713320220547));
#27334=CARTESIAN_POINT('Origin',(0.,0.,10.));
#27335=CARTESIAN_POINT('',(-11.554527761143,13.045354296914,10.5713323675469));
#27336=CARTESIAN_POINT('Origin',(111.305961646472,105.081274424751,15.4574255506739));
#27337=CARTESIAN_POINT('',(-8.94840760976408,14.9537407454735,10.5713324655966));
#27338=CARTESIAN_POINT('Origin',(128.787536624443,82.7336796129508,15.4574255506023));
#27339=CARTESIAN_POINT('',(-8.94889389387817,14.9547919997346,10.5701811473657));
#27340=CARTESIAN_POINT('',(-8.94889389389506,14.9547919997711,10.5701811473257));
#27341=CARTESIAN_POINT('Ctrl Pts',(-10.8357650995917,16.8079082770226,8.00000000135021));
#27342=CARTESIAN_POINT('Ctrl Pts',(-10.4319083043907,16.5372606075049,8.44630079324293));
#27343=CARTESIAN_POINT('Ctrl Pts',(-9.86079935971527,16.1092165464162,9.11078637104974));
#27344=CARTESIAN_POINT('Ctrl Pts',(-9.2758843950842,15.4400561032042,9.98586919170886));
#27345=CARTESIAN_POINT('Ctrl Pts',(-9.16057149290411,15.2954237764487,10.1691928081977));
#27346=CARTESIAN_POINT('Ctrl Pts',(-8.98612677762985,15.0326846060299,10.4842225127632));
#27347=CARTESIAN_POINT('Ctrl Pts',(-8.952265038833,14.9620813509935,10.5621951317299));
#27348=CARTESIAN_POINT('Ctrl Pts',(-8.94889389387818,14.9547919997346,10.5701811473657));
#27349=CARTESIAN_POINT('',(-11.5551861621905,13.0463089966602,10.5701811473657));
#27350=CARTESIAN_POINT('Ctrl Pts',(-11.5551861621905,13.0463089966602,10.5701811473657));
#27351=CARTESIAN_POINT('Ctrl Pts',(-11.558387142026,13.0509500533379,10.5645845413472));
#27352=CARTESIAN_POINT('Ctrl Pts',(-11.5881853135902,13.0950987474776,10.5117930110297));
#27353=CARTESIAN_POINT('Ctrl Pts',(-11.6903020291204,13.2917449279464,10.2967811885933));
#27354=CARTESIAN_POINT('Ctrl Pts',(-11.7413951816398,13.4095218883709,10.1745836443185));
#27355=CARTESIAN_POINT('Ctrl Pts',(-11.8941411179178,13.8049878581245,9.77608155874724));
#27356=CARTESIAN_POINT('Ctrl Pts',(-12.0134730293053,14.1923619596404,9.40558420693438));
#27357=CARTESIAN_POINT('Ctrl Pts',(-12.1672829307558,15.0771140530975,8.62456348411121));
#27358=CARTESIAN_POINT('Ctrl Pts',(-12.2075290668195,15.450122309667,8.30828904306058));
#27359=CARTESIAN_POINT('Ctrl Pts',(-12.2267792182909,15.8248366773076,8.00000000200137));
#27360=CARTESIAN_POINT('',(-11.5545279606177,13.0453545817615,10.5713320220547));
#27361=CARTESIAN_POINT('Origin',(0.,0.,10.));
#27362=CARTESIAN_POINT('',(-15.3194784201766,8.30674192742137,10.5713323675468));
#27363=CARTESIAN_POINT('Origin',(68.6534782678162,136.81297911302,15.4574255506294));
#27364=CARTESIAN_POINT('',(-13.5232331517002,10.991384178438,10.5713324655949));
#27365=CARTESIAN_POINT('Origin',(92.7241128561788,121.792159957727,15.4574255506777));
#27366=CARTESIAN_POINT('',(-13.5240496594282,10.9922057153483,10.5701811473657));
#27367=CARTESIAN_POINT('',(-13.5240496594565,10.9922057153769,10.5701811473257));
#27368=CARTESIAN_POINT('Ctrl Pts',(-15.9309316930687,12.0882174588948,8.00000000133986));
#27369=CARTESIAN_POINT('Ctrl Pts',(-15.1846105254595,11.9045133471794,8.70558326806036));
#27370=CARTESIAN_POINT('Ctrl Pts',(-14.5699846733765,11.6496262306723,9.3434760766814));
#27371=CARTESIAN_POINT('Ctrl Pts',(-13.9393973439685,11.3049486899113,10.0506526873813));
#27372=CARTESIAN_POINT('Ctrl Pts',(-13.7979632304026,11.2086258296407,10.2211211399706));
#27373=CARTESIAN_POINT('Ctrl Pts',(-13.5895004003257,11.0547819798244,10.4799221915463));
#27374=CARTESIAN_POINT('Ctrl Pts',(-13.5308399330947,10.9990389370527,10.5606019637361));
#27375=CARTESIAN_POINT('Ctrl Pts',(-13.5240496594282,10.9922057153483,10.5701811473657));
#27376=CARTESIAN_POINT('',(-15.3204236413265,8.30741386530727,10.5701811473657));
#27377=CARTESIAN_POINT('Ctrl Pts',(-15.3204236413265,8.30741386530727,10.5701811473657));
#27378=CARTESIAN_POINT('Ctrl Pts',(-15.3296093183982,8.31394314010386,10.5589938627884));
#27379=CARTESIAN_POINT('Ctrl Pts',(-15.4243397912466,8.38389819046196,10.4424768097922));
#27380=CARTESIAN_POINT('Ctrl Pts',(-15.7023973354593,8.67266944970296,10.059837781778));
#27381=CARTESIAN_POINT('Ctrl Pts',(-15.877803352698,8.87707981846489,9.80772094036177));
#27382=CARTESIAN_POINT('Ctrl Pts',(-16.3465096379412,9.55074263810651,9.06700787399611));
#27383=CARTESIAN_POINT('Ctrl Pts',(-16.6367153184879,10.0623165531715,8.5588483583004));
#27384=CARTESIAN_POINT('Ctrl Pts',(-16.9018271158858,10.688677470155,8.00000000200139));
#27385=CARTESIAN_POINT('',(-15.3194787050451,8.30674212686605,10.5713320220547));
#27386=CARTESIAN_POINT('Origin',(0.,0.,10.));
#27387=CARTESIAN_POINT('',(-17.2366738903149,2.56621388702747,10.5713323675469));
#27388=CARTESIAN_POINT('Origin',(17.7203721943182,152.043019376197,15.4574255505794));
#27389=CARTESIAN_POINT('',(-16.46695719617,5.70330446537958,10.571332460081));
#27390=CARTESIAN_POINT('Origin',(45.476792614545,146.160708349105,15.4574255506031));
#27391=CARTESIAN_POINT('',(-16.4680054423355,5.70379719401241,10.5701811473657));
#27392=CARTESIAN_POINT('',(-16.4680054423506,5.70379719401952,10.5701811473491));
#27393=CARTESIAN_POINT('Ctrl Pts',(-19.1045928220558,5.91050920363085,8.00000000133985));
#27394=CARTESIAN_POINT('Ctrl Pts',(-18.3404453742124,5.99314117727813,8.70558736914872));
#27395=CARTESIAN_POINT('Ctrl Pts',(-17.6757112795656,5.96384825561592,9.34347579792883));
#27396=CARTESIAN_POINT('Ctrl Pts',(-16.965266952437,5.85563210275787,10.0506513818862));
#27397=CARTESIAN_POINT('Ctrl Pts',(-16.7994199777579,5.81349051075214,10.2211182925806));
#27398=CARTESIAN_POINT('Ctrl Pts',(-16.5509086476868,5.74021758827718,10.4799236386272));
#27399=CARTESIAN_POINT('Ctrl Pts',(-16.4767204468357,5.70789456465678,10.5606051118207));
#27400=CARTESIAN_POINT('Ctrl Pts',(-16.4680054423355,5.7037971940124,10.5701811473657));
#27401=CARTESIAN_POINT('',(-17.2377919239465,2.56652201742732,10.5701811473657));
#27402=CARTESIAN_POINT('Ctrl Pts',(-17.2377919239465,2.56652201742732,10.5701811473657));
#27403=CARTESIAN_POINT('Ctrl Pts',(-17.2432165977388,2.56801679306029,10.5645954896389));
#27404=CARTESIAN_POINT('Ctrl Pts',(-17.2944202352089,2.58267975187223,10.5118057138876));
#27405=CARTESIAN_POINT('Ctrl Pts',(-17.499059900203,2.66768441718779,10.2967813913972));
#27406=CARTESIAN_POINT('Ctrl Pts',(-17.6139068024539,2.7250652631623,10.1745820882336));
#27407=CARTESIAN_POINT('Ctrl Pts',(-17.9851423528615,2.92983891430192,9.77605365105219));
#27408=CARTESIAN_POINT('Ctrl Pts',(-18.3255478232859,3.14988018146411,9.40556319816633));
#27409=CARTESIAN_POINT('Ctrl Pts',(-19.0120618406687,3.7287595937826,8.62456345423171));
#27410=CARTESIAN_POINT('Ctrl Pts',(-19.2826571305709,3.98863205185952,8.30828888039902));
#27411=CARTESIAN_POINT('Ctrl Pts',(-19.5382652189043,4.26330601201086,8.00000000200134));
#27412=CARTESIAN_POINT('',(-17.2366742262179,2.5662139770134,10.5713320220547));
#27413=CARTESIAN_POINT('Origin',(0.,0.,10.));
#27414=CARTESIAN_POINT('',(-17.0748721030675,-3.48383742142528,10.5713323675469));
#27415=CARTESIAN_POINT('Origin',(-35.3500722902058,148.93442758746,15.4574255506556));
#27416=CARTESIAN_POINT('',(-17.4245231720677,-0.272677940736843,10.5713324655957));
#27417=CARTESIAN_POINT('Origin',(-7.25569998124663,152.900118213319,15.4574255506581));
#27418=CARTESIAN_POINT('',(-17.4256767270215,-0.272573448002652,10.5701811473657));
#27419=CARTESIAN_POINT('',(-17.4256767270616,-0.272573447999024,10.5701811473257));
#27420=CARTESIAN_POINT('Ctrl Pts',(-19.9739581029631,-0.980093691350214,
8.00000000133979));
#27421=CARTESIAN_POINT('Ctrl Pts',(-19.2841435286873,-0.641084932274938,
8.70560031770914));
#27422=CARTESIAN_POINT('Ctrl Pts',(-18.6494933378834,-0.441236392474984,
9.34347484440447));
#27423=CARTESIAN_POINT('Ctrl Pts',(-17.9448526543321,-0.299930716980267,
10.0506796721615));
#27424=CARTESIAN_POINT('Ctrl Pts',(-17.774596174239,-0.282817401607676,
10.2211444100579));
#27425=CARTESIAN_POINT('Ctrl Pts',(-17.5160325453378,-0.266691128994518,
10.4799280527013));
#27426=CARTESIAN_POINT('Ctrl Pts',(-17.4352576748299,-0.271704780182462,
10.5606149575372));
#27427=CARTESIAN_POINT('Ctrl Pts',(-17.4256767270215,-0.272573448002655,
10.5701811473657));
#27428=CARTESIAN_POINT('',(-17.0760280978245,-3.48393026358523,10.5701811473657));
#27429=CARTESIAN_POINT('Ctrl Pts',(-17.0760280978245,-3.48393026358523,
10.5701811473657));
#27430=CARTESIAN_POINT('Ctrl Pts',(-17.0816242548471,-3.48437996814373,
10.5646080499549));
#27431=CARTESIAN_POINT('Ctrl Pts',(-17.134752365133,-3.48811668217437,10.5118202838587));
#27432=CARTESIAN_POINT('Ctrl Pts',(-17.3561386567893,-3.47822935651112,
10.2967816445881));
#27433=CARTESIAN_POINT('Ctrl Pts',(-17.483686879022,-3.46358907535537,10.1745803305061));
#27434=CARTESIAN_POINT('Ctrl Pts',(-17.9026024617299,-3.39813122398345,
9.77602162422452));
#27435=CARTESIAN_POINT('Ctrl Pts',(-18.2977298390231,-3.3077820989418,9.40553906114762));
#27436=CARTESIAN_POINT('Ctrl Pts',(-19.1408049443345,-2.99862155763995,
8.62456342110259));
#27437=CARTESIAN_POINT('Ctrl Pts',(-19.483963321225,-2.84696895217793,8.30828869477175));
#27438=CARTESIAN_POINT('Ctrl Pts',(-19.818100182429,-2.676283070884,8.00000000200132));
#27439=CARTESIAN_POINT('',(-17.07487244949,-3.48383745175174,10.5713320220547));
#27440=CARTESIAN_POINT('Origin',(0.,0.,10.));
#27441=CARTESIAN_POINT('',(-14.8535887419165,-9.11368652088975,10.5713323675468));
#27442=CARTESIAN_POINT('Origin',(-84.1567763447132,127.862145793152,15.4574255506348));
#27443=CARTESIAN_POINT('',(-16.2804344971332,-6.21577136145381,10.5713324655964));
#27444=CARTESIAN_POINT('Origin',(-59.1130480768611,141.19751725499,15.4574255506146));
#27445=CARTESIAN_POINT('',(-16.2815542228302,-6.21606770943294,10.5701811473657));
#27446=CARTESIAN_POINT('',(-16.2815542228464,-6.21606770943721,10.5701811473491));
#27447=CARTESIAN_POINT('Ctrl Pts',(-18.4341692463042,-7.75248283719144,
8.0000000013502));
#27448=CARTESIAN_POINT('Ctrl Pts',(-18.0976291590699,-7.40188904938079,
8.44613531049589));
#27449=CARTESIAN_POINT('Ctrl Pts',(-17.5769004278482,-6.91371871795296,
9.11066173479789));
#27450=CARTESIAN_POINT('Ctrl Pts',(-16.8162268240735,-6.45382336350305,
9.9858703902644));
#27451=CARTESIAN_POINT('Ctrl Pts',(-16.6537681965835,-6.36537822955351,
10.1691934650876));
#27452=CARTESIAN_POINT('Ctrl Pts',(-16.3647226973184,-6.23920570512901,
10.4842294826958));
#27453=CARTESIAN_POINT('Ctrl Pts',(-16.2893139085124,-6.2181207143615,10.562199572309));
#27454=CARTESIAN_POINT('Ctrl Pts',(-16.2815542228302,-6.21606770943295,
10.5701811473657));
#27455=CARTESIAN_POINT('',(-14.8546432677704,-9.11416913747482,10.5701811473657));
#27456=CARTESIAN_POINT('Ctrl Pts',(-14.8546432677704,-9.11416913747483,
10.5701811473657));
#27457=CARTESIAN_POINT('Ctrl Pts',(-14.8597660838178,-9.11651393900607,
10.5645884462977));
#27458=CARTESIAN_POINT('Ctrl Pts',(-14.9084174072385,-9.13819358906896,
10.5117975421278));
#27459=CARTESIAN_POINT('Ctrl Pts',(-15.1198127387867,-9.20461324531697,
10.2967812590694));
#27460=CARTESIAN_POINT('Ctrl Pts',(-15.2446732178137,-9.23447867692434,
10.1745830867917));
#27461=CARTESIAN_POINT('Ctrl Pts',(-15.6606648117142,-9.31623441692814,
9.77607160551689));
#27462=CARTESIAN_POINT('Ctrl Pts',(-16.0628737176155,-9.36648476233705,
9.40557671674966));
#27463=CARTESIAN_POINT('Ctrl Pts',(-16.9608851316586,-9.36432155355913,
8.62456347341339));
#27464=CARTESIAN_POINT('Ctrl Pts',(-17.3352154811392,-9.33918367920639,
8.30828898498332));
#27465=CARTESIAN_POINT('Ctrl Pts',(-17.7075797799539,-9.2930729176553,8.00000000200136));
#27466=CARTESIAN_POINT('',(-14.8535890570749,-9.11368666787078,10.5713320220547));
#27467=CARTESIAN_POINT('Origin',(0.,0.,10.));
#27468=CARTESIAN_POINT('',(-10.8407433628676,-13.644290522247,10.5713323675469));
#27469=CARTESIAN_POINT('Origin',(-122.812931151392,91.367802173297,15.4574255507475));
#27470=CARTESIAN_POINT('',(-13.1726851506205,-11.4091510222241,10.5713324600806));
#27471=CARTESIAN_POINT('Origin',(-103.840490158285,112.464411861506,15.4574255506242));
#27472=CARTESIAN_POINT('',(-13.1736359892169,-11.4098124657167,10.5701811473657));
#27473=CARTESIAN_POINT('',(-13.1736359892306,-11.4098124657263,10.5701811473491));
#27474=CARTESIAN_POINT('Ctrl Pts',(-14.6709475306549,-13.5898081110632,
8.00000000133986));
#27475=CARTESIAN_POINT('Ctrl Pts',(-14.3604369835261,-12.8867251164551,
8.70558327479781));
#27476=CARTESIAN_POINT('Ctrl Pts',(-14.0026935300856,-12.3256974912484,
9.34347607544347));
#27477=CARTESIAN_POINT('Ctrl Pts',(-13.5537520773979,-11.7645428267245,
10.0506526845183));
#27478=CARTESIAN_POINT('Ctrl Pts',(-13.4343328018142,-11.6419837080455,
10.2211211345728));
#27479=CARTESIAN_POINT('Ctrl Pts',(-13.24662698436,-11.4634026014367,10.4799221940139));
#27480=CARTESIAN_POINT('Ctrl Pts',(-13.18154451303,-11.4153130002093,10.5606019692441));
#27481=CARTESIAN_POINT('Ctrl Pts',(-13.1736359892169,-11.4098124657167,
10.5701811473657));
#27482=CARTESIAN_POINT('',(-10.8415692284374,-13.6451047025743,10.5701811473657));
#27483=CARTESIAN_POINT('Ctrl Pts',(-10.8415692284374,-13.6451047025743,
10.5701811473657));
#27484=CARTESIAN_POINT('Ctrl Pts',(-10.8495944627031,-13.6530171085486,
10.5589937544163));
#27485=CARTESIAN_POINT('Ctrl Pts',(-10.9349367082249,-13.7341609123916,
10.442476527063));
#27486=CARTESIAN_POINT('Ctrl Pts',(-11.2676049195369,-13.9578493996888,
10.0598376976806));
#27487=CARTESIAN_POINT('Ctrl Pts',(-11.4993688063476,-14.0950950751287,
9.8077208654343));
#27488=CARTESIAN_POINT('Ctrl Pts',(-12.2441871286723,-14.4397003276068,
9.06700782909466));
#27489=CARTESIAN_POINT('Ctrl Pts',(-12.7983827738291,-14.6366633254469,
8.55884825596709));
#27490=CARTESIAN_POINT('Ctrl Pts',(-13.461263919971,-14.788981019434,8.00000000200138));
#27491=CARTESIAN_POINT('',(-10.8407436087492,-13.6442907681545,10.5713320220547));
#27492=CARTESIAN_POINT('Origin',(0.,0.,10.));
#27493=CARTESIAN_POINT('',(-5.52034434192461,-16.5291917183394,10.5713323675469));
#27494=CARTESIAN_POINT('Origin',(-146.656033933765,43.8531531647029,15.4574255506582));
#27495=CARTESIAN_POINT('',(-8.47611556230396,-15.2264186862093,10.5713324655953));
#27496=CARTESIAN_POINT('Origin',(-136.043236604895,70.1664386006067,15.4574255506575));
#27497=CARTESIAN_POINT('',(-8.47678283314336,-15.2273654477372,10.5701811473657));
#27498=CARTESIAN_POINT('',(-8.47678283316653,-15.2273654477701,10.5701811473257));
#27499=CARTESIAN_POINT('Ctrl Pts',(-9.13819300258432,-17.7880019841986,
8.0000000013502));
#27500=CARTESIAN_POINT('Ctrl Pts',(-9.10573334157513,-17.3029234034518,
8.44630493528937));
#27501=CARTESIAN_POINT('Ctrl Pts',(-9.02059000590332,-16.5943080511345,
9.11078949135942));
#27502=CARTESIAN_POINT('Ctrl Pts',(-8.73353860313941,-15.7531796242835,
9.98586916321519));
#27503=CARTESIAN_POINT('Ctrl Pts',(-8.66593979204522,-15.5809995394391,
10.1691927927873));
#27504=CARTESIAN_POINT('Ctrl Pts',(-8.52562343208767,-15.2985565373186,
10.4842223385187));
#27505=CARTESIAN_POINT('Ctrl Pts',(-8.48141008842605,-15.2339297118854,
10.5621950205953));
#27506=CARTESIAN_POINT('Ctrl Pts',(-8.47678283314335,-15.2273654477372,
10.5701811473657));
#27507=CARTESIAN_POINT('',(-5.52084193563401,-16.5302392602455,10.5701811473657));
#27508=CARTESIAN_POINT('Ctrl Pts',(-5.52084193563401,-16.5302392602455,
10.5701811473657));
#27509=CARTESIAN_POINT('Ctrl Pts',(-5.5232591818717,-16.535328682705,10.5645880972756));
#27510=CARTESIAN_POINT('Ctrl Pts',(-5.54659294916294,-16.5832087508318,
10.5117971371651));
#27511=CARTESIAN_POINT('Ctrl Pts',(-5.66583723437205,-16.7699711064541,
10.2967812527268));
#27512=CARTESIAN_POINT('Ctrl Pts',(-5.74228875577475,-16.8731080724369,
10.1745831365675));
#27513=CARTESIAN_POINT('Ctrl Pts',(-6.00840470366951,-17.2031301364064,
9.77607249529175));
#27514=CARTESIAN_POINT('Ctrl Pts',(-6.28421432461988,-17.5001592694047,
9.40557738653905));
#27515=CARTESIAN_POINT('Ctrl Pts',(-6.97352197177043,-18.075733287063,8.62456347451042));
#27516=CARTESIAN_POINT('Ctrl Pts',(-7.27643393079308,-18.2970914797066,
8.30828899024054));
#27517=CARTESIAN_POINT('Ctrl Pts',(-7.59132096413778,-18.5011197481594,
8.00000000200135));
#27518=CARTESIAN_POINT('',(-5.52034448887238,-16.5291920335133,10.5713320220547));
#27519=CARTESIAN_POINT('Origin',(0.,0.,10.));
#27520=CARTESIAN_POINT('',(0.465889678260092,-17.4204284483111,10.5713323675468));
#27521=CARTESIAN_POINT('Origin',(-152.810254612452,-8.95083331846698,15.4574255505984));
#27522=CARTESIAN_POINT('',(-2.7572013454317,-17.207155539892,10.5713324655956));
#27523=CARTESIAN_POINT('Origin',(-151.837160932647,19.4053572978174,15.4574255506476));
#27524=CARTESIAN_POINT('',(-2.75750456340204,-17.2082734247813,10.5701811473657));
#27525=CARTESIAN_POINT('',(-2.75750456341258,-17.2082734248201,10.5701811473257));
#27526=CARTESIAN_POINT('Ctrl Pts',(-2.50323755940218,-19.8407002815916,
8.00000000133983));
#27527=CARTESIAN_POINT('Ctrl Pts',(-2.71730857598249,-19.1025054190797,
8.70559254972556));
#27528=CARTESIAN_POINT('Ctrl Pts',(-2.80390036195331,-18.4427875315623,
9.34347543010285));
#27529=CARTESIAN_POINT('Ctrl Pts',(-2.82069735996715,-17.7243294677321,
10.0506659161534));
#27530=CARTESIAN_POINT('Ctrl Pts',(-2.80799094004872,-17.5536854977597,
10.2211322375144));
#27531=CARTESIAN_POINT('Ctrl Pts',(-2.77898047457061,-17.2962388866928,
10.4799254335514));
#27532=CARTESIAN_POINT('Ctrl Pts',(-2.76002529911911,-17.2175636893571,
10.5606090686849));
#27533=CARTESIAN_POINT('Ctrl Pts',(-2.75750456340204,-17.2082734247813,
10.5701811473657));
#27534=CARTESIAN_POINT('',(0.46578037355609,-17.4215830027821,10.5701811473657));
#27535=CARTESIAN_POINT('Ctrl Pts',(0.465780373556093,-17.4215830027821,
10.5701811473657));
#27536=CARTESIAN_POINT('Ctrl Pts',(0.46525139910022,-17.4271731252052,10.5646071593099));
#27537=CARTESIAN_POINT('Ctrl Pts',(0.459705523525212,-17.4801431215649,
10.5118192508034));
#27538=CARTESIAN_POINT('Ctrl Pts',(0.41152525959577,-17.6964481226244,10.2967816258739));
#27539=CARTESIAN_POINT('Ctrl Pts',(0.374958897339234,-17.8195161995657,
10.1745804541382));
#27540=CARTESIAN_POINT('Ctrl Pts',(0.237752210792364,-18.2206987155065,
9.77602389565469));
#27541=CARTESIAN_POINT('Ctrl Pts',(0.0801626930635958,-18.5941348375598,
9.40554077394135));
#27542=CARTESIAN_POINT('Ctrl Pts',(-0.370700233139312,-19.370718272434,
8.6245634233295));
#27543=CARTESIAN_POINT('Ctrl Pts',(-0.579637618570482,-19.6823290958393,
8.30828870786065));
#27544=CARTESIAN_POINT('Ctrl Pts',(-0.805752664038882,-19.9817503878085,
8.00000000200133));
#27545=CARTESIAN_POINT('',(0.46588964797019,-17.4204287947368,10.5713320220547));
#27546=CARTESIAN_POINT('Origin',(0.,0.,10.));
#27547=CARTESIAN_POINT('',(6.39593052744725,-16.2105044092744,10.5713323675468));
#27548=CARTESIAN_POINT('Origin',(-140.533303345581,-60.6752172035179,15.4574255506022));
#27549=CARTESIAN_POINT('',(3.29427204554917,-17.1124554876035,10.5713324600807));
#27550=CARTESIAN_POINT('Origin',(-149.317282773139,-33.6962964878742,15.4574255506621));
#27551=CARTESIAN_POINT('',(3.29436945311861,-17.1136096597291,10.5701811473657));
#27552=CARTESIAN_POINT('',(3.29436945312199,-17.1136096597692,10.5701811473257));
#27553=CARTESIAN_POINT('Ctrl Pts',(4.43364529134561,-19.5003173146818,8.00000000133983));
#27554=CARTESIAN_POINT('Ctrl Pts',(3.98000666786252,-18.8798574376189,8.70559279091519));
#27555=CARTESIAN_POINT('Ctrl Pts',(3.67299983383264,-18.2895418769823,9.34347541225073));
#27556=CARTESIAN_POINT('Ctrl Pts',(3.41148864542289,-17.6201571112643,10.0506658402589));
#27557=CARTESIAN_POINT('Ctrl Pts',(3.36506521139396,-17.4554584511142,10.2211320703513));
#27558=CARTESIAN_POINT('Ctrl Pts',(3.30427440668273,-17.2036153133869,10.4799255162188));
#27559=CARTESIAN_POINT('Ctrl Pts',(3.29517817846112,-17.1232016110275,10.5606092524598));
#27560=CARTESIAN_POINT('Ctrl Pts',(3.29436945311862,-17.1136096597291,10.5701811473657));
#27561=CARTESIAN_POINT('',(6.39622269550912,-16.2116267200016,10.5701811473657));
#27562=CARTESIAN_POINT('Ctrl Pts',(6.39622269550912,-16.2116267200016,10.5701811473657));
#27563=CARTESIAN_POINT('Ctrl Pts',(6.39764036742772,-16.2170714320218,10.5645960857259));
#27564=CARTESIAN_POINT('Ctrl Pts',(6.41054379697892,-16.2687464183396,10.5118064054016));
#27565=CARTESIAN_POINT('Ctrl Pts',(6.43924755269189,-16.4884725820687,10.2967814028056));
#27566=CARTESIAN_POINT('Ctrl Pts',(6.44697775604531,-16.6166234340433,10.1745820039935));
#27567=CARTESIAN_POINT('Ctrl Pts',(6.45525643927773,-17.0405111810353,9.77605213102646));
#27568=CARTESIAN_POINT('Ctrl Pts',(6.43489762050362,-17.4453312691443,9.40556205303796));
#27569=CARTESIAN_POINT('Ctrl Pts',(6.27683044777478,-18.3293083111279,8.6245634522497));
#27570=CARTESIAN_POINT('Ctrl Pts',(6.18707187906349,-18.6935869638801,8.30828887138087));
#27571=CARTESIAN_POINT('Ctrl Pts',(6.07700129894464,-19.0522870314542,8.00000000200134));
#27572=CARTESIAN_POINT('',(6.39593061746862,-16.2105047451678,10.5713320220547));
#27573=CARTESIAN_POINT('Origin',(0.,0.,10.));
#27574=CARTESIAN_POINT('',(11.554527761143,-13.045354296914,10.5713323675468));
#27575=CARTESIAN_POINT('Origin',(-111.305961644556,-105.081274423327,15.4574255506698));
#27576=CARTESIAN_POINT('',(8.94840760976382,-14.953740745473,10.571332465596));
#27577=CARTESIAN_POINT('Origin',(-128.787536624077,-82.7336796127344,15.4574255505594));
#27578=CARTESIAN_POINT('',(8.94889389387819,-14.9547919997346,10.5701811473657));
#27579=CARTESIAN_POINT('',(8.94889389389507,-14.9547919997711,10.5701811473257));
#27580=CARTESIAN_POINT('Ctrl Pts',(10.8357650995917,-16.8079082770226,8.00000000135021));
#27581=CARTESIAN_POINT('Ctrl Pts',(10.4319083085344,-16.5372606102823,8.44630078866327));
#27582=CARTESIAN_POINT('Ctrl Pts',(9.86079936621396,-16.1092165518233,9.11078636305187));
#27583=CARTESIAN_POINT('Ctrl Pts',(9.27588439976794,-15.4400561090421,9.98586918429367));
#27584=CARTESIAN_POINT('Ctrl Pts',(9.16057149585408,-15.2954237805644,10.1691928031512));
#27585=CARTESIAN_POINT('Ctrl Pts',(8.98612677817748,-15.0326846071263,10.4842225115412));
#27586=CARTESIAN_POINT('Ctrl Pts',(8.95226503888915,-14.962081351115,10.5621951315968));
#27587=CARTESIAN_POINT('Ctrl Pts',(8.94889389387818,-14.9547919997346,10.5701811473657));
#27588=CARTESIAN_POINT('',(11.5551861621905,-13.0463089966602,10.5701811473657));
#27589=CARTESIAN_POINT('Ctrl Pts',(11.5551861621905,-13.0463089966602,10.5701811473657));
#27590=CARTESIAN_POINT('Ctrl Pts',(11.5583871420256,-13.0509500533373,10.564584541348));
#27591=CARTESIAN_POINT('Ctrl Pts',(11.5881853135926,-13.0950987474807,10.5117930110258));
#27592=CARTESIAN_POINT('Ctrl Pts',(11.6903020291314,-13.2917449279689,10.2967811885692));
#27593=CARTESIAN_POINT('Ctrl Pts',(11.7413951816546,-13.4095218884055,10.1745836442827));
#27594=CARTESIAN_POINT('Ctrl Pts',(11.8941411179495,-13.8049878582153,9.77608155865787));
#27595=CARTESIAN_POINT('Ctrl Pts',(12.0134730293381,-14.1923619597709,9.40558420681378));
#27596=CARTESIAN_POINT('Ctrl Pts',(12.1672829307671,-15.0771140532029,8.62456348402197));
#27597=CARTESIAN_POINT('Ctrl Pts',(12.2075290668222,-15.4501223097195,8.30828904301733));
#27598=CARTESIAN_POINT('Ctrl Pts',(12.2267792182909,-15.8248366773076,8.00000000200136));
#27599=CARTESIAN_POINT('',(11.5545279606177,-13.0453545817615,10.5713320220547));
#27600=CARTESIAN_POINT('Origin',(0.,0.,10.));
#27601=CARTESIAN_POINT('',(15.3194784201766,-8.30674192742138,10.5713323675468));
#27602=CARTESIAN_POINT('Origin',(-68.6534782675676,-136.812979112652,15.4574255506315));
#27603=CARTESIAN_POINT('',(13.5232331517007,-10.9913841784383,10.5713324655954));
#27604=CARTESIAN_POINT('Origin',(-92.7241128554327,-121.792159957011,15.4574255506737));
#27605=CARTESIAN_POINT('',(13.5240496594282,-10.9922057153483,10.5701811473657));
#27606=CARTESIAN_POINT('',(13.52404965944,-10.9922057153602,10.5701811473491));
#27607=CARTESIAN_POINT('Ctrl Pts',(15.9309316930687,-12.0882174588948,8.00000000133986));
#27608=CARTESIAN_POINT('Ctrl Pts',(15.1846105255028,-11.90451334719,8.70558326801943));
#27609=CARTESIAN_POINT('Ctrl Pts',(14.5699846734489,-11.6496262307027,9.34347607660589));
#27610=CARTESIAN_POINT('Ctrl Pts',(13.9393973440172,-11.304948689943,10.0506526873236));
#27611=CARTESIAN_POINT('Ctrl Pts',(13.7979632304376,-11.2086258296654,10.2211211399278));
#27612=CARTESIAN_POINT('Ctrl Pts',(13.5895004003317,-11.0547819798306,10.4799221915377));
#27613=CARTESIAN_POINT('Ctrl Pts',(13.5308399330952,-10.9990389370533,10.5606019637353));
#27614=CARTESIAN_POINT('Ctrl Pts',(13.5240496594282,-10.9922057153483,10.5701811473657));
#27615=CARTESIAN_POINT('',(15.3204236413265,-8.30741386530727,10.5701811473657));
#27616=CARTESIAN_POINT('Ctrl Pts',(15.3204236413265,-8.30741386530728,10.5701811473657));
#27617=CARTESIAN_POINT('Ctrl Pts',(15.3259880972987,-8.31136913848444,10.5634041670742));
#27618=CARTESIAN_POINT('Ctrl Pts',(15.3542103341916,-8.33285296379557,10.5283572769709));
#27619=CARTESIAN_POINT('Ctrl Pts',(15.4571749141827,-8.42277175408883,10.3949486774381));
#27620=CARTESIAN_POINT('Ctrl Pts',(15.5156233515662,-8.47953131429124,10.3164605964467));
#27621=CARTESIAN_POINT('Ctrl Pts',(15.7507362195951,-8.7230165051001,9.9932461136542));
#27622=CARTESIAN_POINT('Ctrl Pts',(15.9183553520326,-8.93678627005409,9.74293971143246));
#27623=CARTESIAN_POINT('Ctrl Pts',(16.3885040715423,-9.61540679748373,8.99849349761917));
#27624=CARTESIAN_POINT('Ctrl Pts',(16.6709049544784,-10.1431184734786,8.48676446374045));
#27625=CARTESIAN_POINT('Ctrl Pts',(16.9018270970315,-10.6886774998989,8.00000000203882));
#27626=CARTESIAN_POINT('',(15.3194787050451,-8.30674212686605,10.5713320220547));
#27627=CARTESIAN_POINT('Origin',(0.,0.,10.));
#27628=CARTESIAN_POINT('',(17.0748721030675,3.48383742142528,10.5713323675469));
#27629=CARTESIAN_POINT('Origin',(35.3500722903246,-148.93442758794,15.4574255506851));
#27630=CARTESIAN_POINT('',(17.4245231720676,0.272677940736963,10.5713324655955));
#27631=CARTESIAN_POINT('Origin',(7.25569998132668,-152.900118213192,15.4574255506867));
#27632=CARTESIAN_POINT('',(17.4256767270215,0.272573448002653,10.5701811473657));
#27633=CARTESIAN_POINT('',(17.4256767270616,0.272573447999023,10.5701811473257));
#27634=CARTESIAN_POINT('Ctrl Pts',(19.9739581029631,0.980093691350215,8.00000000133979));
#27635=CARTESIAN_POINT('Ctrl Pts',(19.2841435288454,0.641084932352634,8.70560031754744));
#27636=CARTESIAN_POINT('Ctrl Pts',(18.6494933381746,0.441236392566893,9.34347484411127));
#27637=CARTESIAN_POINT('Ctrl Pts',(17.9448526545539,0.299930717008343,10.0506796719394));
#27638=CARTESIAN_POINT('Ctrl Pts',(17.7745961744026,0.282817401622175,10.221144409894));
#27639=CARTESIAN_POINT('Ctrl Pts',(17.5160325453688,0.266691128991328,10.4799280526703));
#27640=CARTESIAN_POINT('Ctrl Pts',(17.4352576748297,0.271704780182212,10.5606149575373));
#27641=CARTESIAN_POINT('Ctrl Pts',(17.4256767270215,0.272573448002658,10.5701811473657));
#27642=CARTESIAN_POINT('',(17.0760280978245,3.48393026358524,10.5701811473657));
#27643=CARTESIAN_POINT('Ctrl Pts',(17.0760280978245,3.48393026358523,10.5701811473657));
#27644=CARTESIAN_POINT('Ctrl Pts',(17.082832989171,3.48447710146804,10.5634042963604));
#27645=CARTESIAN_POINT('Ctrl Pts',(17.118266172143,3.48616508036893,10.5283524025663));
#27646=CARTESIAN_POINT('Ctrl Pts',(17.2549505214738,3.48347943228899,10.3949314562896));
#27647=CARTESIAN_POINT('Ctrl Pts',(17.3362095820895,3.47757286967626,10.3164420312485));
#27648=CARTESIAN_POINT('Ctrl Pts',(17.6728162805958,3.44219121402148,9.99323475872722));
#27649=CARTESIAN_POINT('Ctrl Pts',(17.9386285191952,3.38617468577126,9.74292915184891));
#27650=CARTESIAN_POINT('Ctrl Pts',(18.734981412195,3.16851614964894,8.99849596508342));
#27651=CARTESIAN_POINT('Ctrl Pts',(19.2905272574431,2.94577048137857,8.48676235755947));
#27652=CARTESIAN_POINT('Ctrl Pts',(19.8181001870972,2.67628303603597,8.00000000203872));
#27653=CARTESIAN_POINT('',(17.07487244949,3.48383745175174,10.5713320220547));
#27654=CARTESIAN_POINT('Origin',(0.,0.,10.));
#27655=CARTESIAN_POINT('',(17.2366738903149,-2.5662138870275,10.5713323675469));
#27656=CARTESIAN_POINT('Origin',(-17.7203721942858,-152.043019376379,15.4574255506204));
#27657=CARTESIAN_POINT('',(16.4669571961699,-5.70330446537945,10.5713324600809));
#27658=CARTESIAN_POINT('Origin',(-45.4767926147669,-146.160708349767,15.4574255506576));
#27659=CARTESIAN_POINT('',(16.4680054423355,-5.70379719401242,10.5701811473657));
#27660=CARTESIAN_POINT('',(16.4680054423719,-5.70379719402953,10.5701811473257));
#27661=CARTESIAN_POINT('Ctrl Pts',(19.1045928267004,-5.91050918858286,8.0000000013502));
#27662=CARTESIAN_POINT('Ctrl Pts',(18.6214219412756,-5.96275677323712,8.44614350899531));
#27663=CARTESIAN_POINT('Ctrl Pts',(17.9087334712743,-6.00199692466679,9.11066791005939));
#27664=CARTESIAN_POINT('Ctrl Pts',(17.0304148875782,-5.86534666547789,9.98587033076591));
#27665=CARTESIAN_POINT('Ctrl Pts',(16.8491128872892,-5.82867319603526,10.1691934324495));
#27666=CARTESIAN_POINT('Ctrl Pts',(16.5465893477924,-5.7395321967925,10.4842291374935));
#27667=CARTESIAN_POINT('Ctrl Pts',(16.4752695527236,-5.70721242491232,10.5621993523733));
#27668=CARTESIAN_POINT('Ctrl Pts',(16.4680054423355,-5.70379719401242,10.5701811473657));
#27669=CARTESIAN_POINT('',(17.2377919239465,-2.56652201742733,10.5701811473657));
#27670=CARTESIAN_POINT('Ctrl Pts',(17.2377919239465,-2.56652201742733,10.5701811473657));
#27671=CARTESIAN_POINT('Ctrl Pts',(17.244373526362,-2.56833558618609,10.5634042277214));
#27672=CARTESIAN_POINT('Ctrl Pts',(17.2782442385717,-2.57886982391587,10.5283549849369));
#27673=CARTESIAN_POINT('Ctrl Pts',(17.4057597403456,-2.62814633108562,10.394940581853));
#27674=CARTESIAN_POINT('Ctrl Pts',(17.4800971046558,-2.66149073253721,10.3164518741183));
#27675=CARTESIAN_POINT('Ctrl Pts',(17.7843053281657,-2.80987217796775,9.99324083646631));
#27676=CARTESIAN_POINT('Ctrl Pts',(18.0149289146885,-2.95342222781332,9.74293477054091));
#27677=CARTESIAN_POINT('Ctrl Pts',(18.6888196107373,-3.4303196438136,8.99849465091812));
#27678=CARTESIAN_POINT('Ctrl Pts',(19.1346780195212,-3.8296291338376,8.48676348247822));
#27679=CARTESIAN_POINT('Ctrl Pts',(19.538265211366,-4.26330604638229,8.00000000203877));
#27680=CARTESIAN_POINT('',(17.2366742262179,-2.56621397701342,10.5713320220547));
#27681=CARTESIAN_POINT('Origin',(0.,0.,-10.));
#27682=CARTESIAN_POINT('',(15.8586462619277,-2.10689542799376,-12.));
#27683=CARTESIAN_POINT('',(17.2955741454208,-2.13341885727951,-10.5713324653939));
#27684=CARTESIAN_POINT('Origin',(23.5558393036297,151.248847158071,-15.457425550669));
#27685=CARTESIAN_POINT('',(15.9750644581313,0.856145527351446,-12.));
#27686=CARTESIAN_POINT('Origin',(0.,0.,-12.));
#27687=CARTESIAN_POINT('',(17.3922038024245,1.0952750368686,-10.5713323676496));
#27688=CARTESIAN_POINT('Origin',(-4.76307193196004,152.99805383595,-15.4574255506925));
#27689=CARTESIAN_POINT('',(17.3933450474474,1.09546964341861,-10.5701811473657));
#27690=CARTESIAN_POINT('',(17.3933450474559,1.09546964342005,-10.5701811473572));
#27691=CARTESIAN_POINT('',(19.9892823205607,0.590066302194425,-8.0000000006604));
#27692=CARTESIAN_POINT('Ctrl Pts',(19.9892823208559,0.590066301248343,-8.00000000133981));
#27693=CARTESIAN_POINT('Ctrl Pts',(19.2749998010589,0.873906210786177,-8.70559645872247));
#27694=CARTESIAN_POINT('Ctrl Pts',(18.6266223644309,1.02333760517501,-9.34347512881039));
#27695=CARTESIAN_POINT('Ctrl Pts',(17.9130663535317,1.10892131617197,-10.0506808566673));
#27696=CARTESIAN_POINT('Ctrl Pts',(17.7419904686334,1.11262517441619,-10.2211470622343));
#27697=CARTESIAN_POINT('Ctrl Pts',(17.4829623350634,1.10841935625201,-10.4799267635866));
#27698=CARTESIAN_POINT('Ctrl Pts',(17.4028311940924,1.09708783867808,-10.5606120436833));
#27699=CARTESIAN_POINT('Ctrl Pts',(17.3933450474474,1.09546964341861,-10.5701811473657));
#27700=CARTESIAN_POINT('',(19.966986344762,-1.11312273006808,-8.00000000095182));
#27701=CARTESIAN_POINT('Origin',(0.,0.,-8.));
#27702=CARTESIAN_POINT('',(17.2967344200949,-2.13342074610697,-10.5701811473657));
#27703=CARTESIAN_POINT('Ctrl Pts',(17.2967344200949,-2.13342074610697,-10.5701811473657));
#27704=CARTESIAN_POINT('Ctrl Pts',(17.3035611999971,-2.13343199258597,-10.5634043347187));
#27705=CARTESIAN_POINT('Ctrl Pts',(17.3390189242949,-2.13233598307216,-10.5283509622276));
#27706=CARTESIAN_POINT('Ctrl Pts',(17.4750744944769,-2.11893772957618,-10.3949263636951));
#27707=CARTESIAN_POINT('Ctrl Pts',(17.5556199162956,-2.10667499553378,-10.3164365320466));
#27708=CARTESIAN_POINT('Ctrl Pts',(17.8884105141753,-2.04499610289594,-9.99323129759905));
#27709=CARTESIAN_POINT('Ctrl Pts',(18.1490082042499,-1.96829604022225,-9.74292598155898));
#27710=CARTESIAN_POINT('Ctrl Pts',(18.925825438827,-1.68882439134058,-8.998496694386));
#27711=CARTESIAN_POINT('Ctrl Pts',(19.462184152493,-1.42317193372476,-8.48676171610473));
#27712=CARTESIAN_POINT('Ctrl Pts',(19.9669863450947,-1.11312272890333,-8.00000000203869));
#27713=CARTESIAN_POINT('',(17.2955750463447,-2.1334188914951,-10.5713320279724));
#27714=CARTESIAN_POINT('Origin',(0.,0.,-10.));
#27715=CARTESIAN_POINT('',(15.6228535442421,3.44414238100227,-12.));
#27716=CARTESIAN_POINT('',(16.9821956200472,3.91067679088529,-10.5713324653932));
#27717=CARTESIAN_POINT('Origin',(-29.594904012793,150.183997111332,-15.4574255505978));
#27718=CARTESIAN_POINT('',(14.7188311719128,6.26830746997787,-12.));
#27719=CARTESIAN_POINT('Origin',(0.,0.,-12.));
#27720=CARTESIAN_POINT('',(15.9687194472522,6.97770590713078,-10.5713323676496));
#27721=CARTESIAN_POINT('Origin',(-56.8042398485925,142.14207563998,-15.4574255506378));
#27722=CARTESIAN_POINT('',(15.9697253074185,6.97827910625622,-10.5701811473657));
#27723=CARTESIAN_POINT('',(15.969725307426,6.97827910626046,-10.5701811473572));
#27724=CARTESIAN_POINT('',(18.5819665360208,7.39121813950882,-8.00000000066548));
#27725=CARTESIAN_POINT('Ctrl Pts',(18.5819665366264,7.39121813871246,-8.0000000013502));
#27726=CARTESIAN_POINT('Ctrl Pts',(18.115084008858,7.40484396995126,-8.42878730500133));
#27727=CARTESIAN_POINT('Ctrl Pts',(17.6409432928525,7.38300231236836,-8.87475273362061));
#27728=CARTESIAN_POINT('Ctrl Pts',(16.796836385882,7.26187969081736,-9.69886565230376));
#27729=CARTESIAN_POINT('Ctrl Pts',(16.5173942721915,7.18523112291558,-9.98545215664171));
#27730=CARTESIAN_POINT('Ctrl Pts',(16.2441712341572,7.09655132569949,-10.2713413261852));
#27731=CARTESIAN_POINT('Ctrl Pts',(16.157205635271,7.0645803511292,-10.3638298171814));
#27732=CARTESIAN_POINT('Ctrl Pts',(16.0106083799487,7.00085283491759,-10.5236792308836));
#27733=CARTESIAN_POINT('Ctrl Pts',(15.9750505957941,6.98131421081911,-10.5640861067932));
#27734=CARTESIAN_POINT('Ctrl Pts',(15.9697253074185,6.97827910625623,-10.5701811473657));
#27735=CARTESIAN_POINT('',(19.1435401333719,5.78311828236397,-8.00000000093431));
#27736=CARTESIAN_POINT('Origin',(0.,0.,-8.));
#27737=CARTESIAN_POINT('',(16.9832865676143,3.91107185327861,-10.5701811473657));
#27738=CARTESIAN_POINT('Ctrl Pts',(16.9832865676143,3.91107185327861,-10.5701811473657));
#27739=CARTESIAN_POINT('Ctrl Pts',(16.9938807774509,3.91490807712278,-10.5589962499751));
#27740=CARTESIAN_POINT('Ctrl Pts',(17.1038574353568,3.95700002189838,-10.4424830400739));
#27741=CARTESIAN_POINT('Ctrl Pts',(17.4489770135646,4.16096284457778,-10.0598396416896));
#27742=CARTESIAN_POINT('Ctrl Pts',(17.6726303951008,4.31106257269274,-9.80772259382915));
#27743=CARTESIAN_POINT('Ctrl Pts',(18.3043191739733,4.83496893723644,-9.06700885143705));
#27744=CARTESIAN_POINT('Ctrl Pts',(18.7206809583787,5.25038372694467,-8.55885060615725));
#27745=CARTESIAN_POINT('Ctrl Pts',(19.1435401332864,5.78311828355128,-8.00000000200138));
#27746=CARTESIAN_POINT('',(16.9821964783418,3.91067706686746,-10.5713320279724));
#27747=CARTESIAN_POINT('Origin',(0.,0.,-10.));
#27748=CARTESIAN_POINT('',(13.5027141203588,8.57976578872144,-12.));
#27749=CARTESIAN_POINT('',(14.6205136742489,9.48308710459935,-10.5713324598778));
#27750=CARTESIAN_POINT('Origin',(-79.1760651305894,131.004740533131,-15.4574255506352));
#27751=CARTESIAN_POINT('',(11.6872896195489,10.9244190213593,-12.));
#27752=CARTESIAN_POINT('Origin',(0.,0.,-12.));
#27753=CARTESIAN_POINT('',(12.6191718535419,12.0185224650217,-10.5713323676496));
#27754=CARTESIAN_POINT('Origin',(-101.9939780973,114.141665326891,-15.4574255506697));
#27755=CARTESIAN_POINT('',(12.6199210072709,12.0194051204483,-10.5701811473657));
#27756=CARTESIAN_POINT('',(12.6199210072764,12.0194051204548,-10.5701811473572));
#27757=CARTESIAN_POINT('',(14.9333913461676,13.3008800022332,-8.00000000066548));
#27758=CARTESIAN_POINT('Ctrl Pts',(14.9333913470091,13.300880001692,-8.00000000135021));
#27759=CARTESIAN_POINT('Ctrl Pts',(14.4900047007427,13.1540007731545,-8.42878756921447));
#27760=CARTESIAN_POINT('Ctrl Pts',(14.05192955011,12.9713101258595,-8.87475254749765));
#27761=CARTESIAN_POINT('Ctrl Pts',(13.3001554516508,12.5687901368235,-9.69886534036099));
#27762=CARTESIAN_POINT('Ctrl Pts',(13.0637795260502,12.4011888222765,-9.9854532705251));
#27763=CARTESIAN_POINT('Ctrl Pts',(12.8373640975609,12.2244096937772,-10.2713421856512));
#27764=CARTESIAN_POINT('Ctrl Pts',(12.7665785152972,12.164623380239,-10.3638298315781));
#27765=CARTESIAN_POINT('Ctrl Pts',(12.6506190175245,12.0546010170489,-10.523677911962));
#27766=CARTESIAN_POINT('Ctrl Pts',(12.6238878102618,12.0240794086141,-10.564084976174));
#27767=CARTESIAN_POINT('Ctrl Pts',(12.6199210072709,12.0194051204483,-10.5701811473657));
#27768=CARTESIAN_POINT('',(16.0111004341151,11.9818299434094,-8.00000000095188));
#27769=CARTESIAN_POINT('Origin',(0.,0.,-8.));
#27770=CARTESIAN_POINT('',(14.6214037084642,9.48383146588572,-10.5701811473657));
#27771=CARTESIAN_POINT('Ctrl Pts',(14.6214037084642,9.48383146588573,-10.5701811473657));
#27772=CARTESIAN_POINT('Ctrl Pts',(14.6266406861662,9.48821113033898,-10.563404164166));
#27773=CARTESIAN_POINT('Ctrl Pts',(14.6530901817765,9.51184302828194,-10.5283573867385));
#27774=CARTESIAN_POINT('Ctrl Pts',(14.7486820596608,9.60956316447749,-10.3949490649912));
#27775=CARTESIAN_POINT('Ctrl Pts',(14.8024969463754,9.67073361738553,-10.3164610136522));
#27776=CARTESIAN_POINT('Ctrl Pts',(15.0177813930359,9.93191529884655,-9.99324636281345));
#27777=CARTESIAN_POINT('Ctrl Pts',(15.1681116736084,10.1581772795485,-9.74293994559928));
#27778=CARTESIAN_POINT('Ctrl Pts',(15.5835674700258,10.8715932850833,-8.99849344133071));
#27779=CARTESIAN_POINT('Ctrl Pts',(15.8236941965497,11.4198346996499,-8.48676450976364));
#27780=CARTESIAN_POINT('Ctrl Pts',(16.0111004336212,11.9818299445155,-8.00000000203881));
#27781=CARTESIAN_POINT('',(14.6205143845238,9.48308765551917,-10.5713320279724));
#27782=CARTESIAN_POINT('Origin',(0.,0.,-10.));
#27783=CARTESIAN_POINT('',(9.75394809472371,12.6805428184636,-12.));
#27784=CARTESIAN_POINT('',(10.4953820000271,13.9116971543318,-10.5713324653938));
#27785=CARTESIAN_POINT('Origin',(-119.207424280339,96.024378823486,-15.4574255505985));
#27786=CARTESIAN_POINT('',(7.24608845304286,14.2628844115113,-12.));
#27787=CARTESIAN_POINT('Origin',(0.,0.,-12.));
#27788=CARTESIAN_POINT('',(7.74756589515309,15.6097278391302,-10.5713323676496));
#27789=CARTESIAN_POINT('Origin',(-134.881737317318,72.3740856247486,-15.4574255506614));
#27790=CARTESIAN_POINT('',(7.74796798344852,15.610813489587,-10.5701811473657));
#27791=CARTESIAN_POINT('',(7.74796798345149,15.610813489595,-10.5701811473572));
#27792=CARTESIAN_POINT('',(9.48362876657315,17.6062594366159,-8.00000000066547));
#27793=CARTESIAN_POINT('Ctrl Pts',(9.48362876754896,17.6062594363951,-8.0000000013502));
#27794=CARTESIAN_POINT('Ctrl Pts',(9.10230391485961,17.3048011250946,-8.44623968757263));
#27795=CARTESIAN_POINT('Ctrl Pts',(8.56651432227087,16.8332645253691,-9.1107403480541));
#27796=CARTESIAN_POINT('Ctrl Pts',(8.0358763831978,16.1202369320469,-9.98586963003723));
#27797=CARTESIAN_POINT('Ctrl Pts',(7.93226696459376,15.9670031889161,-10.1691930478072));
#27798=CARTESIAN_POINT('Ctrl Pts',(7.77897326462272,15.6913850801188,-10.4842250863003));
#27799=CARTESIAN_POINT('Ctrl Pts',(7.75075624770121,15.6183433206485,-10.5621967716335));
#27800=CARTESIAN_POINT('Ctrl Pts',(7.74796798344853,15.610813489587,-10.5701811473657));
#27801=CARTESIAN_POINT('',(10.9474857635323,16.7353560273778,-8.00000000093431));
#27802=CARTESIAN_POINT('Origin',(0.,0.,-8.));
#27803=CARTESIAN_POINT('',(10.4959637731368,13.9127010372614,-10.5701811473657));
#27804=CARTESIAN_POINT('Ctrl Pts',(10.4959637731368,13.9127010372614,-10.5701811473657));
#27805=CARTESIAN_POINT('Ctrl Pts',(10.5016144966778,13.9224512473345,-10.5589943393125));
#27806=CARTESIAN_POINT('Ctrl Pts',(10.5588056026778,14.0253908150085,-10.4424780527323));
#27807=CARTESIAN_POINT('Ctrl Pts',(10.6920761194039,14.4034708467085,-10.0598381515106));
#27808=CARTESIAN_POINT('Ctrl Pts',(10.7669214225258,14.6622159512276,-9.80772126903106));
#27809=CARTESIAN_POINT('Ctrl Pts',(10.9140625720399,15.4695925301061,-9.06700806847332));
#27810=CARTESIAN_POINT('Ctrl Pts',(10.9659919501974,16.0554512351927,-8.55884880660357));
#27811=CARTESIAN_POINT('Ctrl Pts',(10.9474857627036,16.7353560282324,-8.0000000020014));
#27812=CARTESIAN_POINT('',(10.4953824801207,13.9116979174471,-10.5713320279724));
#27813=CARTESIAN_POINT('Origin',(0.,0.,-10.));
#27814=CARTESIAN_POINT('',(4.82871197592245,15.2518592394185,-12.));
#27815=CARTESIAN_POINT('',(5.10435236312686,16.6623512144409,-10.5713324653938));
#27816=CARTESIAN_POINT('Origin',(-144.86060874693,49.4620598581121,-15.4574255506524));
#27817=CARTESIAN_POINT('',(1.93090207822382,15.8810354438797,-12.));
#27818=CARTESIAN_POINT('Origin',(0.,0.,-12.));
#27819=CARTESIAN_POINT('',(1.94148914791391,17.3181696607923,-10.5713323676496));
#27820=CARTESIAN_POINT('Origin',(-151.50076837451,21.8771230683502,-15.4574255506003));
#27821=CARTESIAN_POINT('',(1.94149567299321,17.3193273608118,-10.5701811473657));
#27822=CARTESIAN_POINT('',(1.94149567299326,17.3193273608203,-10.5701811473572));
#27823=CARTESIAN_POINT('',(2.89000059425646,19.7880641422247,-8.00000000066547));
#27824=CARTESIAN_POINT('Ctrl Pts',(2.89000059524891,19.788064142351,-8.00000000135018));
#27825=CARTESIAN_POINT('Ctrl Pts',(2.64475964931276,19.39054597626,-8.42878617646645));
#27826=CARTESIAN_POINT('Ctrl Pts',(2.42659969707148,18.9690059600901,-8.87475353017283));
#27827=CARTESIAN_POINT('Ctrl Pts',(2.10944806509491,18.1774498969438,-9.69884249196947));
#27828=CARTESIAN_POINT('Ctrl Pts',(2.03610698480492,17.8971303337412,-9.98542034745814));
#27829=CARTESIAN_POINT('Ctrl Pts',(1.97628997602387,17.6161445060139,-10.2713376725187));
#27830=CARTESIAN_POINT('Ctrl Pts',(1.96049432139808,17.5248410224956,-10.3638297783296));
#27831=CARTESIAN_POINT('Ctrl Pts',(1.94238591343305,17.3660145389221,-10.5236848708594));
#27832=CARTESIAN_POINT('Ctrl Pts',(1.94152981246431,17.3254518932292,-10.5640909344681));
#27833=CARTESIAN_POINT('Ctrl Pts',(1.94149567299321,17.3193273608118,-10.5701811473657));
#27834=CARTESIAN_POINT('',(4.56344268684126,19.4703512230268,-8.00000000095185));
#27835=CARTESIAN_POINT('Origin',(0.,0.,-8.));
#27836=CARTESIAN_POINT('',(5.10455570284158,16.6634935339443,-10.5701811473657));
#27837=CARTESIAN_POINT('Ctrl Pts',(5.10455570284159,16.6634935339443,-10.5701811473657));
#27838=CARTESIAN_POINT('Ctrl Pts',(5.10575225003943,16.670214723682,-10.5634042571891));
#27839=CARTESIAN_POINT('Ctrl Pts',(5.11082706385406,16.7053218793388,-10.5283538728356));
#27840=CARTESIAN_POINT('Ctrl Pts',(5.12125055225597,16.8416316419825,-10.3949366521605));
#27841=CARTESIAN_POINT('Ctrl Pts',(5.1231583356211,16.923082645346,-10.3164476362452));
#27842=CARTESIAN_POINT('Ctrl Pts',(5.12019877873412,17.2615339859569,-9.99323823168558));
#27843=CARTESIAN_POINT('Ctrl Pts',(5.08991797344972,17.5314913857707,-9.74293234996718));
#27844=CARTESIAN_POINT('Ctrl Pts',(4.94959210998568,18.3450426232497,-8.99849520740764));
#27845=CARTESIAN_POINT('Ctrl Pts',(4.78112411324725,18.9193771867733,-8.48676299740456));
#27846=CARTESIAN_POINT('Ctrl Pts',(4.56344268575195,19.4703512235566,-8.00000000203874));
#27847=CARTESIAN_POINT('',(5.10435255326647,16.6623520957364,-10.5713320279724));
#27848=CARTESIAN_POINT('Origin',(0.,0.,-10.));
#27849=CARTESIAN_POINT('',(-0.678938071373979,15.9835763426303,-12.));
#27850=CARTESIAN_POINT('',(-0.902337501759209,17.4032798105771,-10.5713324598781));
#27851=CARTESIAN_POINT('Origin',(-153.041465883393,-3.06611350821765,-15.4574255506746));
#27852=CARTESIAN_POINT('',(-3.61717958430867,15.5836992225952,-12.));
#27853=CARTESIAN_POINT('Origin',(0.,0.,-12.));
#27854=CARTESIAN_POINT('',(-4.09875984389179,16.9377846323997,-10.5713323676496));
#27855=CARTESIAN_POINT('Origin',(-149.846570852488,-31.2585434020205,-15.4574255506772));
#27856=CARTESIAN_POINT('',(-4.09914966904954,16.9388747462736,-10.5701811473657));
#27857=CARTESIAN_POINT('',(-4.09914966905242,16.9388747462817,-10.5701811473572));
#27858=CARTESIAN_POINT('',(-4.05220430155577,19.5831362715489,-8.00000000066547));
#27859=CARTESIAN_POINT('Ctrl Pts',(-4.05220430066634,19.583136272007,-8.0000000013502));
#27860=CARTESIAN_POINT('Ctrl Pts',(-4.14669632796146,19.125713331242,-8.42878684330689));
#27861=CARTESIAN_POINT('Ctrl Pts',(-4.20752191859742,18.6549819182125,-8.87475305913646));
#27862=CARTESIAN_POINT('Ctrl Pts',(-4.23481731144313,17.80269093116,-9.69884177101634));
#27863=CARTESIAN_POINT('Ctrl Pts',(-4.2078615995899,17.5141886502129,-9.98542319365981));
#27864=CARTESIAN_POINT('Ctrl Pts',(-4.16796931937234,17.2296902080373,-10.2713398280482));
#27865=CARTESIAN_POINT('Ctrl Pts',(-4.15158517621766,17.1384926619022,-10.3638297967784));
#27866=CARTESIAN_POINT('Ctrl Pts',(-4.11428113814177,16.9830542376031,-10.5236815368733));
#27867=CARTESIAN_POINT('Ctrl Pts',(-4.10121326794226,16.9446443015203,-10.5640880820797));
#27868=CARTESIAN_POINT('Ctrl Pts',(-4.09914966904954,16.9388747462736,-10.5701811473657));
#27869=CARTESIAN_POINT('',(-2.37101889769494,19.8569346902003,-8.00000000095185));
#27870=CARTESIAN_POINT('Origin',(0.,0.,-8.));
#27871=CARTESIAN_POINT('',(-0.902537120435117,17.4044227834609,-10.5701811473657));
#27872=CARTESIAN_POINT('Ctrl Pts',(-0.902537120435117,17.4044227834609,
-10.5701811473657));
#27873=CARTESIAN_POINT('Ctrl Pts',(-0.903711515722634,17.4111478767131,
-10.5634042595987));
#27874=CARTESIAN_POINT('Ctrl Pts',(-0.910950040701272,17.445873597137,-10.5283537819086));
#27875=CARTESIAN_POINT('Ctrl Pts',(-0.947775684927258,17.5775281579718,
-10.3949363308107));
#27876=CARTESIAN_POINT('Ctrl Pts',(-0.973840771994048,17.65471959454,-10.3164472895697));
#27877=CARTESIAN_POINT('Ctrl Pts',(-1.0923787754393,17.9717474770875,-9.99323801735438));
#27878=CARTESIAN_POINT('Ctrl Pts',(-1.21316434486273,18.215067793567,-9.74293215129558));
#27879=CARTESIAN_POINT('Ctrl Pts',(-1.62327857933575,18.9315613697452,-8.99849525274451));
#27880=CARTESIAN_POINT('Ctrl Pts',(-1.97802108022651,19.4136399232311,-8.48676295744821));
#27881=CARTESIAN_POINT('Ctrl Pts',(-2.37101889889979,19.8569346903256,-8.00000000203875));
#27882=CARTESIAN_POINT('',(-0.902337623732298,17.403280701153,-10.5713320279724));
#27883=CARTESIAN_POINT('Origin',(0.,0.,-10.));
#27884=CARTESIAN_POINT('',(-6.10469816720394,14.7874382464574,-12.));
#27885=CARTESIAN_POINT('',(-6.80019214539383,16.045116011612,-10.5713324653945));
#27886=CARTESIAN_POINT('Origin',(-142.763263583003,-55.2244683342239,-15.4574255506132));
#27887=CARTESIAN_POINT('',(-8.72897600508841,13.4067388841599,-12.));
#27888=CARTESIAN_POINT('Origin',(0.,0.,-12.));
#27889=CARTESIAN_POINT('',(-9.64463790727134,14.5144528022616,-10.5713323676496));
#27890=CARTESIAN_POINT('Origin',(-130.118665385434,-80.6239682110755,-15.4574255506424));
#27891=CARTESIAN_POINT('',(-9.64537706399891,14.5153438461684,-10.5701811473657));
#27892=CARTESIAN_POINT('',(-9.64537706400437,14.515343846175,-10.5701811473572));
#27893=CARTESIAN_POINT('',(-10.5056535544358,17.0161931502252,-8.00000000066548));
#27894=CARTESIAN_POINT('Ctrl Pts',(-10.5056535537567,17.0161931509599,-8.0000000013502));
#27895=CARTESIAN_POINT('Ctrl Pts',(-10.4379990384668,16.5540372634017,-8.42878754157539));
#27896=CARTESIAN_POINT('Ctrl Pts',(-10.3341548985703,16.090893457156,-8.87475256715481));
#27897=CARTESIAN_POINT('Ctrl Pts',(-10.0682943444031,15.280643580727,-9.69886537601137));
#27898=CARTESIAN_POINT('Ctrl Pts',(-9.94428552962841,15.0187552442567,-9.98545315751203));
#27899=CARTESIAN_POINT('Ctrl Pts',(-9.80950865920445,14.7650822007685,-10.2713420955023));
#27900=CARTESIAN_POINT('Ctrl Pts',(-9.7629223749456,14.6849901507037,-10.3638298300135));
#27901=CARTESIAN_POINT('Ctrl Pts',(-9.6747075515577,14.5516870556448,-10.5236780502563));
#27902=CARTESIAN_POINT('Ctrl Pts',(-9.64929143497656,14.5200619743597,-10.5640850947464));
#27903=CARTESIAN_POINT('Ctrl Pts',(-9.64537706399891,14.5153438461684,-10.5701811473657));
#27904=CARTESIAN_POINT('',(-9.01950057931991,17.8484787924764,-8.00000000093431));
#27905=CARTESIAN_POINT('Origin',(0.,0.,-8.));
#27906=CARTESIAN_POINT('',(-6.80077064695807,16.0461217833684,-10.5701811473657));
#27907=CARTESIAN_POINT('Ctrl Pts',(-6.80077064695807,16.0461217833684,-10.5701811473657));
#27908=CARTESIAN_POINT('Ctrl Pts',(-6.80638919125232,16.055890517594,-10.5589943862035));
#27909=CARTESIAN_POINT('Ctrl Pts',(-6.86694184573586,16.156889202588,-10.4424781739493));
#27910=CARTESIAN_POINT('Ctrl Pts',(-7.12773354662917,16.4613449449585,-10.0598381867424));
#27911=CARTESIAN_POINT('Ctrl Pts',(-7.31439070989755,16.6555354459819,-9.80772129864558));
#27912=CARTESIAN_POINT('Ctrl Pts',(-7.9400287825512,17.1866517200601,-9.06700808049053));
#27913=CARTESIAN_POINT('Ctrl Pts',(-8.42143262084641,17.5245532010067,-8.55884884664401));
#27914=CARTESIAN_POINT('Ctrl Pts',(-9.01950058047432,17.848478792186,-8.00000000200139));
#27915=CARTESIAN_POINT('',(-6.80019256622393,16.0451168089422,-10.5713320279724));
#27916=CARTESIAN_POINT('Origin',(0.,0.,-10.));
#27917=CARTESIAN_POINT('',(-10.7941415683196,11.8077168584163,-12.));
#27918=CARTESIAN_POINT('',(-11.8778432569209,12.7516744235555,-10.5713324653938));
#27919=CARTESIAN_POINT('Origin',(-115.265704733187,-100.721937252455,-15.4574255506293));
#27920=CARTESIAN_POINT('',(-12.787929093689,9.61272797390185,-12.));
#27921=CARTESIAN_POINT('Origin',(0.,0.,-12.));
#27922=CARTESIAN_POINT('',(-14.0272302993381,10.3404637536615,-10.5713323676496));
#27923=CARTESIAN_POINT('Origin',(-94.6965285267638,-120.264952571911,-15.4574255506283));
#27924=CARTESIAN_POINT('',(-14.0282296344253,10.3410482545556,-10.5701811473657));
#27925=CARTESIAN_POINT('',(-14.0282296344327,10.3410482545599,-10.5701811473572));
#27926=CARTESIAN_POINT('',(-15.6919659417353,12.3968460027146,-8.00000000066548));
#27927=CARTESIAN_POINT('Ctrl Pts',(-15.6919659413484,12.3968460036373,-8.0000000013502));
#27928=CARTESIAN_POINT('Ctrl Pts',(-15.4612482665808,11.9688635895045,-8.44634716807826));
#27929=CARTESIAN_POINT('Ctrl Pts',(-15.0899124083607,11.3593769508001,-9.11082129036562));
#27930=CARTESIAN_POINT('Ctrl Pts',(-14.4799190402401,10.7130444208772,-9.98586884763384));
#27931=CARTESIAN_POINT('Ctrl Pts',(-14.347004802687,10.5843997718203,-10.1691926186395));
#27932=CARTESIAN_POINT('Ctrl Pts',(-14.1021964490745,10.3855767651888,-10.4842205569699));
#27933=CARTESIAN_POINT('Ctrl Pts',(-14.0351633980038,10.3451031649441,-10.5621938865181));
#27934=CARTESIAN_POINT('Ctrl Pts',(-14.0282296344253,10.3410482545556,-10.5701811473657));
#27935=CARTESIAN_POINT('',(-14.5800974363697,13.6872329069855,-8.00000000095188));
#27936=CARTESIAN_POINT('Origin',(0.,0.,-8.));
#27937=CARTESIAN_POINT('',(-11.8787308647727,12.7524216806657,-10.5701811473657));
#27938=CARTESIAN_POINT('Ctrl Pts',(-11.8787308647727,12.7524216806657,-10.5701811473657));
#27939=CARTESIAN_POINT('Ctrl Pts',(-11.8839533839592,12.7568185761942,-10.5634041641101));
#27940=CARTESIAN_POINT('Ctrl Pts',(-11.9118191664806,12.7787626049671,-10.5283573896283));
#27941=CARTESIAN_POINT('Ctrl Pts',(-12.0246540683064,12.8559332948898,-10.3949490753317));
#27942=CARTESIAN_POINT('Ctrl Pts',(-12.0942400622391,12.8983084727834,-10.3164610250703));
#27943=CARTESIAN_POINT('Ctrl Pts',(-12.3888375656887,13.0649685394825,-9.99324637132914));
#27944=CARTESIAN_POINT('Ctrl Pts',(-12.6377666955721,13.1737249856624,-9.74293995479456));
#27945=CARTESIAN_POINT('Ctrl Pts',(-13.4124874524261,13.4589856947628,-8.99849344275429));
#27946=CARTESIAN_POINT('Ctrl Pts',(-13.9940974085794,13.6002632407478,-8.4867645122222));
#27947=CARTESIAN_POINT('Ctrl Pts',(-14.5800974373733,13.687232906307,-8.00000000203881));
#27948=CARTESIAN_POINT('',(-11.8778439250753,12.7516750288689,-10.5713320279724));
#27949=CARTESIAN_POINT('Origin',(0.,0.,-10.));
#27950=CARTESIAN_POINT('',(-14.1816521917328,7.40381055390888,-12.));
#27951=CARTESIAN_POINT('',(-15.5228511760091,7.92019270597809,-10.571332459879));
#27952=CARTESIAN_POINT('Origin',(-73.8654007526338,-134.070854041611,-15.4574255505795));
#27953=CARTESIAN_POINT('',(-15.3044692038576,4.65928020123584,-12.));
#27954=CARTESIAN_POINT('Origin',(0.,0.,-12.));
#27955=CARTESIAN_POINT('',(-16.7179316974337,4.91926216737799,-10.5713323676496));
#27956=CARTESIAN_POINT('Origin',(-47.8525927545976,-145.400208728616,-15.4574255506014));
#27957=CARTESIAN_POINT('',(-16.7190706763204,4.91946962582534,-10.5701811473657));
#27958=CARTESIAN_POINT('',(-16.7190706763288,4.91946962582688,-10.5701811473572));
#27959=CARTESIAN_POINT('',(-18.9855956477114,6.28225626930338,-8.00000000066547));
#27960=CARTESIAN_POINT('Ctrl Pts',(-18.9855956476635,6.2822562703027,-8.00000000135019));
#27961=CARTESIAN_POINT('Ctrl Pts',(-18.6367017450793,5.97171227824352,-8.42878687911838));
#27962=CARTESIAN_POINT('Ctrl Pts',(-18.2594491909432,5.68367023000594,-8.87475303340393));
#27963=CARTESIAN_POINT('Ctrl Pts',(-17.5349912283894,5.23388632148025,-9.69884173367996));
#27964=CARTESIAN_POINT('Ctrl Pts',(-17.2716629153967,5.11297935279029,-9.98542334889029));
#27965=CARTESIAN_POINT('Ctrl Pts',(-17.0053339464139,5.00527782996971,-10.2713399444911));
#27966=CARTESIAN_POINT('Ctrl Pts',(-16.9181625924622,4.97386817752492,-10.363829798057));
#27967=CARTESIAN_POINT('Ctrl Pts',(-16.7648971338693,4.92845522395886,-10.5236813571024));
#27968=CARTESIAN_POINT('Ctrl Pts',(-16.7250992094526,4.92056730211027,-10.5640879281721));
#27969=CARTESIAN_POINT('Ctrl Pts',(-16.7190706763204,4.91946962582535,-10.5701811473657));
#27970=CARTESIAN_POINT('',(-18.3821193318641,7.87510474680894,-8.00000000095187));
#27971=CARTESIAN_POINT('Origin',(0.,0.,-8.));
#27972=CARTESIAN_POINT('',(-15.5239408288994,7.92059131757518,-10.5701811473657));
#27973=CARTESIAN_POINT('Ctrl Pts',(-15.5239408288994,7.92059131757521,-10.5701811473657));
#27974=CARTESIAN_POINT('Ctrl Pts',(-15.5303521795289,7.92293682684727,-10.563404205282));
#27975=CARTESIAN_POINT('Ctrl Pts',(-15.5640436349665,7.93402859460558,-10.5283558304942));
#27976=CARTESIAN_POINT('Ctrl Pts',(-15.6964698353132,7.96795801108948,-10.3949435685778));
#27977=CARTESIAN_POINT('Ctrl Pts',(-15.7763523057977,7.98397907252595,-10.3164550925782));
#27978=CARTESIAN_POINT('Ctrl Pts',(-16.1101805969897,8.03983262596674,-9.99324279225774));
#27979=CARTESIAN_POINT('Ctrl Pts',(-16.3812946407727,8.05689058530697,-9.74293659276605));
#27980=CARTESIAN_POINT('Ctrl Pts',(-17.2068565502871,8.05997362328367,-8.99849421884513));
#27981=CARTESIAN_POINT('Ctrl Pts',(-17.8017148435408,7.99380365638828,-8.48676384407007));
#27982=CARTESIAN_POINT('Ctrl Pts',(-18.382119332575,7.87510474582817,-8.00000000203878));
#27983=CARTESIAN_POINT('',(-15.5228520082561,7.92019304563385,-10.5713320279724));
#27984=CARTESIAN_POINT('Origin',(0.,0.,-10.));
#27985=CARTESIAN_POINT('',(-15.8586462619277,2.10689542799376,-12.));
#27986=CARTESIAN_POINT('',(-17.2955741454207,2.1334188572795,-10.5713324653938));
#27987=CARTESIAN_POINT('Origin',(-23.5558393036639,-151.248847157487,-15.4574255507057));
#27988=CARTESIAN_POINT('',(-15.9750644581313,-0.856145527351444,-12.));
#27989=CARTESIAN_POINT('Origin',(0.,0.,-12.));
#27990=CARTESIAN_POINT('',(-17.3922038024244,-1.09527503686864,-10.5713323676496));
#27991=CARTESIAN_POINT('Origin',(4.76307193199126,-152.998053835939,-15.4574255506736));
#27992=CARTESIAN_POINT('',(-17.3933450474474,-1.09546964341861,-10.5701811473657));
#27993=CARTESIAN_POINT('',(-17.3933450474559,-1.09546964342005,-10.5701811473572));
#27994=CARTESIAN_POINT('',(-19.9892823210147,-0.590066286421281,-8.00000000066547));
#27995=CARTESIAN_POINT('Ctrl Pts',(-19.9892823213114,-0.590066285465836,
-8.00000000135018));
#27996=CARTESIAN_POINT('Ctrl Pts',(-19.5552177612373,-0.762553143854976,
-8.42878612191519));
#27997=CARTESIAN_POINT('Ctrl Pts',(-19.1021987068298,-0.904199324209642,
-8.87475356581035));
#27998=CARTESIAN_POINT('Ctrl Pts',(-18.2675953127712,-1.07908057562433,
-9.69884256067525));
#27999=CARTESIAN_POINT('Ctrl Pts',(-17.9787991830665,-1.10263031045676,
-9.9854201300736));
#28000=CARTESIAN_POINT('Ctrl Pts',(-17.6916950067099,-1.11274582052662,
-10.2713374991643));
#28001=CARTESIAN_POINT('Ctrl Pts',(-17.5990355696582,-1.112446815737,-10.363829776856));
#28002=CARTESIAN_POINT('Ctrl Pts',(-17.4394772602174,-1.10270011330808,
-10.5236851384871));
#28003=CARTESIAN_POINT('Ctrl Pts',(-17.3993822358286,-1.09649949779314,
-10.5640911633362));
#28004=CARTESIAN_POINT('Ctrl Pts',(-17.3933450474474,-1.09546964341861,
-10.5701811473657));
#28005=CARTESIAN_POINT('',(-19.966986344762,1.11312273006808,-8.00000000095182));
#28006=CARTESIAN_POINT('Origin',(0.,0.,-8.));
#28007=CARTESIAN_POINT('',(-17.2967344200949,2.13342074610697,-10.5701811473657));
#28008=CARTESIAN_POINT('Ctrl Pts',(-17.2967344200949,2.13342074610697,-10.5701811473657));
#28009=CARTESIAN_POINT('Ctrl Pts',(-17.3035611999969,2.13343199258578,-10.563404334719));
#28010=CARTESIAN_POINT('Ctrl Pts',(-17.3390189242868,2.13233598307222,-10.5283509622356));
#28011=CARTESIAN_POINT('Ctrl Pts',(-17.4750744944391,2.11893772958056,-10.394926363732));
#28012=CARTESIAN_POINT('Ctrl Pts',(-17.5556199162392,2.10667499554252,-10.3164365321016));
#28013=CARTESIAN_POINT('Ctrl Pts',(-17.8884105140494,2.04499610292459,-9.99323129772077));
#28014=CARTESIAN_POINT('Ctrl Pts',(-18.1490082040659,1.96829604027826,-9.74292598173563));
#28015=CARTESIAN_POINT('Ctrl Pts',(-18.9258254386725,1.68882439141746,-8.99849669453326));
#28016=CARTESIAN_POINT('Ctrl Pts',(-19.4621841524218,1.42317193376853,-8.48676171617345));
#28017=CARTESIAN_POINT('Ctrl Pts',(-19.9669863450947,1.11312272890334,-8.00000000203869));
#28018=CARTESIAN_POINT('',(-17.2955750463446,2.1334188914951,-10.5713320279724));
#28019=CARTESIAN_POINT('Origin',(0.,0.,-10.));
#28020=CARTESIAN_POINT('',(-15.6228535442421,-3.44414238100227,-12.));
#28021=CARTESIAN_POINT('',(-16.9821956200471,-3.91067679088527,-10.5713324653932));
#28022=CARTESIAN_POINT('Origin',(29.5949040129132,-150.183997111823,-15.457425550639));
#28023=CARTESIAN_POINT('',(-14.7188311719128,-6.26830746997787,-12.));
#28024=CARTESIAN_POINT('Origin',(0.,0.,-12.));
#28025=CARTESIAN_POINT('',(-15.9687194472521,-6.9777059071309,-10.5713323676496));
#28026=CARTESIAN_POINT('Origin',(56.8042398484162,-142.14207563962,-15.4574255506568));
#28027=CARTESIAN_POINT('',(-15.9697253074185,-6.97827910625622,-10.5701811473657));
#28028=CARTESIAN_POINT('',(-15.969725307426,-6.97827910626046,-10.5701811473572));
#28029=CARTESIAN_POINT('',(-18.5819665360208,-7.39121813950882,-8.00000000066548));
#28030=CARTESIAN_POINT('Ctrl Pts',(-18.5819665366264,-7.39121813871246,
-8.0000000013502));
#28031=CARTESIAN_POINT('Ctrl Pts',(-18.1150840094864,-7.40484396993293,
-8.42878730442417));
#28032=CARTESIAN_POINT('Ctrl Pts',(-17.6409432941562,-7.3830023124265,-8.87475273239537));
#28033=CARTESIAN_POINT('Ctrl Pts',(-16.7968363871264,-7.26187969111102,
-9.69886565104633));
#28034=CARTESIAN_POINT('Ctrl Pts',(-16.5173942730729,-7.18523112316875,
-9.98545215573256));
#28035=CARTESIAN_POINT('Ctrl Pts',(-16.2441712345817,-7.09655132585296,
-10.2713413257348));
#28036=CARTESIAN_POINT('Ctrl Pts',(-16.157205635565,-7.06458035124848,-10.3638298168642));
#28037=CARTESIAN_POINT('Ctrl Pts',(-16.0106083799904,-7.00085283494231,
-10.5236792308355));
#28038=CARTESIAN_POINT('Ctrl Pts',(-15.9750505957893,-6.98131421081621,
-10.5640861067988));
#28039=CARTESIAN_POINT('Ctrl Pts',(-15.9697253074185,-6.97827910625622,
-10.5701811473657));
#28040=CARTESIAN_POINT('',(-19.1435401333719,-5.78311828236397,-8.00000000093431));
#28041=CARTESIAN_POINT('Origin',(0.,0.,-8.));
#28042=CARTESIAN_POINT('',(-16.9832865676143,-3.91107185327861,-10.5701811473657));
#28043=CARTESIAN_POINT('Ctrl Pts',(-16.9832865676143,-3.9110718532786,-10.5701811473657));
#28044=CARTESIAN_POINT('Ctrl Pts',(-16.9938807775104,-3.91490807714427,
-10.5589962499124));
#28045=CARTESIAN_POINT('Ctrl Pts',(-17.1038574351457,-3.95700002184885,
-10.4424830402896));
#28046=CARTESIAN_POINT('Ctrl Pts',(-17.4489770132551,-4.16096284432762,
-10.0598396420491));
#28047=CARTESIAN_POINT('Ctrl Pts',(-17.6726303942686,-4.31106257224221,
-9.8077225947347));
#28048=CARTESIAN_POINT('Ctrl Pts',(-18.304319171989,-4.83496893525044,-9.06700885386361));
#28049=CARTESIAN_POINT('Ctrl Pts',(-18.7206809573621,-5.25038372566414,
-8.55885060750064));
#28050=CARTESIAN_POINT('Ctrl Pts',(-19.1435401332864,-5.78311828355127,
-8.00000000200138));
#28051=CARTESIAN_POINT('',(-16.9821964783418,-3.91067706686746,-10.5713320279724));
#28052=CARTESIAN_POINT('Origin',(0.,0.,-10.));
#28053=CARTESIAN_POINT('',(-13.5027141203588,-8.57976578872145,-12.));
#28054=CARTESIAN_POINT('',(-14.6205136742495,-9.48308710459978,-10.5713324598787));
#28055=CARTESIAN_POINT('Origin',(79.1760651301776,-131.0047405326,-15.4574255506641));
#28056=CARTESIAN_POINT('',(-11.6872896195489,-10.9244190213593,-12.));
#28057=CARTESIAN_POINT('Origin',(0.,0.,-12.));
#28058=CARTESIAN_POINT('',(-12.6191718535418,-12.0185224650217,-10.5713323676496));
#28059=CARTESIAN_POINT('Origin',(101.993978097991,-114.141665327459,-15.4574255506783));
#28060=CARTESIAN_POINT('',(-12.6199210072709,-12.0194051204483,-10.5701811473657));
#28061=CARTESIAN_POINT('',(-12.6199210072764,-12.0194051204548,-10.5701811473572));
#28062=CARTESIAN_POINT('',(-14.9333913461659,-13.3008800022351,-8.00000000066548));
#28063=CARTESIAN_POINT('Ctrl Pts',(-14.9333913470074,-13.3008800016939,
-8.0000000013502));
#28064=CARTESIAN_POINT('Ctrl Pts',(-14.4718373134409,-13.1479825233628,
-8.44635677144831));
#28065=CARTESIAN_POINT('Ctrl Pts',(-13.8071322456388,-12.8881234815153,
-9.11082852198501));
#28066=CARTESIAN_POINT('Ctrl Pts',(-13.0647008722188,-12.3996358745634,
-9.9858687774913));
#28067=CARTESIAN_POINT('Ctrl Pts',(-12.914930261871,-12.2910798159437,-10.1691925801447));
#28068=CARTESIAN_POINT('Ctrl Pts',(-12.6766175616922,-12.0845161595089,
-10.4842201521152));
#28069=CARTESIAN_POINT('Ctrl Pts',(-12.6251185176542,-12.0255296144883,
-10.5621936286663));
#28070=CARTESIAN_POINT('Ctrl Pts',(-12.6199210072709,-12.0194051204483,
-10.5701811473657));
#28071=CARTESIAN_POINT('',(-16.0111004341151,-11.9818299434094,-8.00000000095188));
#28072=CARTESIAN_POINT('Origin',(0.,0.,-8.));
#28073=CARTESIAN_POINT('',(-14.6214037084642,-9.48383146588572,-10.5701811473657));
#28074=CARTESIAN_POINT('Ctrl Pts',(-14.6214037084642,-9.48383146588574,
-10.5701811473657));
#28075=CARTESIAN_POINT('Ctrl Pts',(-14.6266406861523,-9.48821113032728,
-10.5634041641841));
#28076=CARTESIAN_POINT('Ctrl Pts',(-14.6530901816378,-9.51184302815803,
-10.5283573869222));
#28077=CARTESIAN_POINT('Ctrl Pts',(-14.7486820590948,-9.60956316387482,
-10.3949490657943));
#28078=CARTESIAN_POINT('Ctrl Pts',(-14.802496945566,-9.67073361645766,-10.3164610148372));
#28079=CARTESIAN_POINT('Ctrl Pts',(-15.0177813913654,-9.93191529664271,
-9.99324636542056));
#28080=CARTESIAN_POINT('Ctrl Pts',(-15.1681116713633,-10.1581772761004,
-9.74293994937975));
#28081=CARTESIAN_POINT('Ctrl Pts',(-15.5835674685494,-10.8715932816978,
-8.9984934444827));
#28082=CARTESIAN_POINT('Ctrl Pts',(-15.8236941959833,-11.4198346979515,
-8.48676451123472));
#28083=CARTESIAN_POINT('Ctrl Pts',(-16.0111004336212,-11.9818299445155,
-8.00000000203882));
#28084=CARTESIAN_POINT('',(-14.6205143845238,-9.48308765551918,-10.5713320279724));
#28085=CARTESIAN_POINT('Origin',(0.,0.,-10.));
#28086=CARTESIAN_POINT('',(-9.75394809472372,-12.6805428184636,-12.));
#28087=CARTESIAN_POINT('',(-10.4953820000267,-13.9116971543312,-10.571332465393));
#28088=CARTESIAN_POINT('Origin',(119.207424280112,-96.0243788233682,-15.4574255506602));
#28089=CARTESIAN_POINT('',(-7.24608845304286,-14.2628844115113,-12.));
#28090=CARTESIAN_POINT('Origin',(0.,0.,-12.));
#28091=CARTESIAN_POINT('',(-7.7475658951531,-15.6097278391302,-10.5713323676496));
#28092=CARTESIAN_POINT('Origin',(134.881737317284,-72.3740856247587,-15.4574255506782));
#28093=CARTESIAN_POINT('',(-7.74796798344852,-15.610813489587,-10.5701811473657));
#28094=CARTESIAN_POINT('',(-7.74796798345149,-15.610813489595,-10.5701811473572));
#28095=CARTESIAN_POINT('',(-9.4836287665753,-17.6062594366147,-8.00000000066547));
#28096=CARTESIAN_POINT('Ctrl Pts',(-9.4836287675511,-17.606259436394,-8.0000000013502));
#28097=CARTESIAN_POINT('Ctrl Pts',(-9.117217467711,-17.3165911098976,-8.42878732671352));
#28098=CARTESIAN_POINT('Ctrl Pts',(-8.76804424999057,-16.9950876418137,
-8.87475271998277));
#28099=CARTESIAN_POINT('Ctrl Pts',(-8.19927701868966,-16.3597208566847,
-9.69886562696287));
#28100=CARTESIAN_POINT('Ctrl Pts',(-8.03448058174276,-16.1213826471877,
-9.9854522442967));
#28101=CARTESIAN_POINT('Ctrl Pts',(-7.88218185215363,-15.8778256257657,
-10.2713413953036));
#28102=CARTESIAN_POINT('Ctrl Pts',(-7.83611291692439,-15.7974340885403,
-10.363829818583));
#28103=CARTESIAN_POINT('Ctrl Pts',(-7.76477618887298,-15.6543851854117,
-10.5236791254642));
#28104=CARTESIAN_POINT('Ctrl Pts',(-7.75009649497616,-15.6165616292045,
-10.5640860164002));
#28105=CARTESIAN_POINT('Ctrl Pts',(-7.74796798344854,-15.610813489587,-10.5701811473657));
#28106=CARTESIAN_POINT('',(-10.9474857635323,-16.7353560273778,-8.00000000093432));
#28107=CARTESIAN_POINT('Origin',(0.,0.,-8.));
#28108=CARTESIAN_POINT('',(-10.4959637731368,-13.9127010372614,-10.5701811473657));
#28109=CARTESIAN_POINT('Ctrl Pts',(-10.4959637731368,-13.9127010372614,
-10.5701811473657));
#28110=CARTESIAN_POINT('Ctrl Pts',(-10.5016144965552,-13.9224512471231,
-10.5589943395551));
#28111=CARTESIAN_POINT('Ctrl Pts',(-10.5588056031706,-14.0253908156642,
-10.4424780519163));
#28112=CARTESIAN_POINT('Ctrl Pts',(-10.6920761196939,-14.403470848196,-10.0598381501417));
#28113=CARTESIAN_POINT('Ctrl Pts',(-10.7669214238514,-14.6622159545809,
-9.80772126558064));
#28114=CARTESIAN_POINT('Ctrl Pts',(-10.9140625729676,-15.4695925407666,
-9.06700805922446));
#28115=CARTESIAN_POINT('Ctrl Pts',(-10.9659919500273,-16.0554512414216,
-8.558848801484));
#28116=CARTESIAN_POINT('Ctrl Pts',(-10.9474857627035,-16.7353560282324,
-8.00000000200139));
#28117=CARTESIAN_POINT('',(-10.4953824801207,-13.9116979174471,-10.5713320279724));
#28118=CARTESIAN_POINT('Origin',(0.,0.,-10.));
#28119=CARTESIAN_POINT('',(-4.82871197592244,-15.2518592394185,-12.));
#28120=CARTESIAN_POINT('',(-5.10435236312695,-16.6623512144413,-10.5713324653942));
#28121=CARTESIAN_POINT('Origin',(144.860608746725,-49.4620598580445,-15.4574255505872));
#28122=CARTESIAN_POINT('',(-1.93090207822381,-15.8810354438797,-12.));
#28123=CARTESIAN_POINT('Origin',(0.,0.,-12.));
#28124=CARTESIAN_POINT('',(-1.94148914791405,-17.3181696607923,-10.5713323676496));
#28125=CARTESIAN_POINT('Origin',(151.500768374491,-21.8771230684231,-15.4574255506288));
#28126=CARTESIAN_POINT('',(-1.94149567299321,-17.3193273608118,-10.5701811473657));
#28127=CARTESIAN_POINT('',(-1.94149567299325,-17.3193273608203,-10.5701811473572));
#28128=CARTESIAN_POINT('',(-2.89000059425648,-19.7880641422247,-8.00000000066547));
#28129=CARTESIAN_POINT('Ctrl Pts',(-2.89000059524895,-19.788064142351,-8.00000000135019));
#28130=CARTESIAN_POINT('Ctrl Pts',(-2.64475964944046,-19.390545976467,-8.42878617624322));
#28131=CARTESIAN_POINT('Ctrl Pts',(-2.42659969730428,-18.969005960538,-8.87475352969895));
#28132=CARTESIAN_POINT('Ctrl Pts',(-2.10944806523733,-18.1774498974171,
-9.69884249148341));
#28133=CARTESIAN_POINT('Ctrl Pts',(-2.03610698489061,-17.897130334085,-9.98542034710692));
#28134=CARTESIAN_POINT('Ctrl Pts',(-1.97628997605455,-17.6161445061853,
-10.2713376723449));
#28135=CARTESIAN_POINT('Ctrl Pts',(-1.96049432141494,-17.5248410226167,
-10.3638297782074));
#28136=CARTESIAN_POINT('Ctrl Pts',(-1.94238591343281,-17.3660145389405,
-10.5236848708411));
#28137=CARTESIAN_POINT('Ctrl Pts',(-1.94152981246431,-17.3254518932265,
-10.5640909344707));
#28138=CARTESIAN_POINT('Ctrl Pts',(-1.9414956729932,-17.3193273608118,-10.5701811473657));
#28139=CARTESIAN_POINT('',(-4.56344268684126,-19.4703512230268,-8.00000000095185));
#28140=CARTESIAN_POINT('Origin',(0.,0.,-8.));
#28141=CARTESIAN_POINT('',(-5.10455570284158,-16.6634935339443,-10.5701811473657));
#28142=CARTESIAN_POINT('Ctrl Pts',(-5.10455570284158,-16.6634935339443,
-10.5701811473657));
#28143=CARTESIAN_POINT('Ctrl Pts',(-5.10575225004077,-16.6702147236891,
-10.5634042571818));
#28144=CARTESIAN_POINT('Ctrl Pts',(-5.11082706386516,-16.7053218794149,
-10.5283538727596));
#28145=CARTESIAN_POINT('Ctrl Pts',(-5.12125055227524,-16.841631642325,-10.3949366518273));
#28146=CARTESIAN_POINT('Ctrl Pts',(-5.123158335631,-16.9230826458571,-10.3164476357533));
#28147=CARTESIAN_POINT('Ctrl Pts',(-5.12019877867727,-17.2615339871035,
-9.99323823060328));
#28148=CARTESIAN_POINT('Ctrl Pts',(-5.08991797324345,-17.5314913874667,
-9.74293234839749));
#28149=CARTESIAN_POINT('Ctrl Pts',(-4.94959210955161,-18.3450426247206,
-8.99849520609888));
#28150=CARTESIAN_POINT('Ctrl Pts',(-4.7811241129742,-18.9193771874646,-8.48676299679378));
#28151=CARTESIAN_POINT('Ctrl Pts',(-4.56344268575194,-19.4703512235566,
-8.00000000203874));
#28152=CARTESIAN_POINT('',(-5.10435255326646,-16.6623520957364,-10.5713320279724));
#28153=CARTESIAN_POINT('Origin',(0.,0.,-10.));
#28154=CARTESIAN_POINT('',(0.678938071373981,-15.9835763426303,-12.));
#28155=CARTESIAN_POINT('',(0.902337501759208,-17.403279810577,-10.571332459878));
#28156=CARTESIAN_POINT('Origin',(153.041465883414,3.06611350829458,-15.4574255506013));
#28157=CARTESIAN_POINT('',(3.61717958430867,-15.5836992225952,-12.));
#28158=CARTESIAN_POINT('Origin',(0.,0.,-12.));
#28159=CARTESIAN_POINT('',(4.09875984389177,-16.9377846323997,-10.5713323676496));
#28160=CARTESIAN_POINT('Origin',(149.846570852324,31.2585434019396,-15.4574255506915));
#28161=CARTESIAN_POINT('',(4.09914966904954,-16.9388747462736,-10.5701811473657));
#28162=CARTESIAN_POINT('',(4.09914966905241,-16.9388747462817,-10.5701811473572));
#28163=CARTESIAN_POINT('',(4.05220430155578,-19.5831362715489,-8.00000000066547));
#28164=CARTESIAN_POINT('Ctrl Pts',(4.05220430066636,-19.583136272007,-8.00000000135019));
#28165=CARTESIAN_POINT('Ctrl Pts',(4.14669632797403,-19.1257133311813,-8.42878684336377));
#28166=CARTESIAN_POINT('Ctrl Pts',(4.20752191861409,-18.654981918085,-8.8747530592572));
#28167=CARTESIAN_POINT('Ctrl Pts',(4.23481731143593,-17.8026909310343,-9.6988417711401));
#28168=CARTESIAN_POINT('Ctrl Pts',(4.20786159958046,-17.5141886501232,-9.98542319374921));
#28169=CARTESIAN_POINT('Ctrl Pts',(4.16796931936474,-17.2296902079935,-10.2713398280925));
#28170=CARTESIAN_POINT('Ctrl Pts',(4.15158517621114,-17.1384926618717,-10.3638297968096));
#28171=CARTESIAN_POINT('Ctrl Pts',(4.11428113814045,-16.9830542376001,-10.5236815368766));
#28172=CARTESIAN_POINT('Ctrl Pts',(4.10121326794294,-16.9446443015219,-10.5640880820779));
#28173=CARTESIAN_POINT('Ctrl Pts',(4.09914966904953,-16.9388747462736,-10.5701811473657));
#28174=CARTESIAN_POINT('',(2.37101889769492,-19.8569346902003,-8.00000000095185));
#28175=CARTESIAN_POINT('Origin',(0.,0.,-8.));
#28176=CARTESIAN_POINT('',(0.902537120435117,-17.4044227834609,-10.5701811473657));
#28177=CARTESIAN_POINT('Ctrl Pts',(0.902537120435115,-17.4044227834609,
-10.5701811473657));
#28178=CARTESIAN_POINT('Ctrl Pts',(0.903711515723591,-17.4111478767184,
-10.5634042595934));
#28179=CARTESIAN_POINT('Ctrl Pts',(0.910950040711359,-17.4458735971854,
-10.5283537818598));
#28180=CARTESIAN_POINT('Ctrl Pts',(0.947775684990051,-17.5775281581801,
-10.3949363305994));
#28181=CARTESIAN_POINT('Ctrl Pts',(0.973840772098866,-17.6547195948464,
-10.316447289258));
#28182=CARTESIAN_POINT('Ctrl Pts',(1.09237877572117,-17.9717474777571,-9.99323801666938));
#28183=CARTESIAN_POINT('Ctrl Pts',(1.21316434535198,-18.2150677945305,-9.7429321503027));
#28184=CARTESIAN_POINT('Ctrl Pts',(1.62327857991182,-18.9315613705256,-8.99849525191663));
#28185=CARTESIAN_POINT('Ctrl Pts',(1.97802108053847,-19.413639923583,-8.48676295706184));
#28186=CARTESIAN_POINT('Ctrl Pts',(2.37101889889975,-19.8569346903256,-8.00000000203875));
#28187=CARTESIAN_POINT('',(0.902337623732299,-17.403280701153,-10.5713320279724));
#28188=CARTESIAN_POINT('Origin',(0.,0.,-10.));
#28189=CARTESIAN_POINT('',(6.10469816720395,-14.7874382464574,-12.));
#28190=CARTESIAN_POINT('',(6.80019214539348,-16.0451160116112,-10.5713324653937));
#28191=CARTESIAN_POINT('Origin',(142.763263582719,55.2244683340621,-15.4574255506391));
#28192=CARTESIAN_POINT('',(8.72897600508842,-13.4067388841598,-12.));
#28193=CARTESIAN_POINT('Origin',(0.,0.,-12.));
#28194=CARTESIAN_POINT('',(9.64463790727137,-14.5144528022616,-10.5713323676496));
#28195=CARTESIAN_POINT('Origin',(130.118665385375,80.6239682110759,-15.4574255506054));
#28196=CARTESIAN_POINT('',(9.64537706399892,-14.5153438461684,-10.5701811473657));
#28197=CARTESIAN_POINT('',(9.64537706400438,-14.515343846175,-10.5701811473572));
#28198=CARTESIAN_POINT('',(10.5056535544358,-17.0161931502252,-8.00000000066548));
#28199=CARTESIAN_POINT('Ctrl Pts',(10.5056535537567,-17.0161931509599,-8.0000000013502));
#28200=CARTESIAN_POINT('Ctrl Pts',(10.4379990385103,-16.5540372636988,-8.42878754129977));
#28201=CARTESIAN_POINT('Ctrl Pts',(10.3341548987057,-16.0908934577644,-8.87475256656962));
#28202=CARTESIAN_POINT('Ctrl Pts',(10.0682943446443,-15.2806435812879,-9.69886537541095));
#28203=CARTESIAN_POINT('Ctrl Pts',(9.9442855298204,-15.0187552446499,-9.9854531570782));
#28204=CARTESIAN_POINT('Ctrl Pts',(9.80950865931173,-14.7650822009551,-10.2713420952875));
#28205=CARTESIAN_POINT('Ctrl Pts',(9.76292237502594,-14.6849901508317,-10.3638298298625));
#28206=CARTESIAN_POINT('Ctrl Pts',(9.67470755157361,-14.5516870556634,-10.523678050232));
#28207=CARTESIAN_POINT('Ctrl Pts',(9.64929143497573,-14.5200619743586,-10.5640850947478));
#28208=CARTESIAN_POINT('Ctrl Pts',(9.64537706399891,-14.5153438461684,-10.5701811473657));
#28209=CARTESIAN_POINT('',(9.01950057931991,-17.8484787924764,-8.00000000093431));
#28210=CARTESIAN_POINT('Origin',(0.,0.,-8.));
#28211=CARTESIAN_POINT('',(6.80077064695808,-16.0461217833684,-10.5701811473657));
#28212=CARTESIAN_POINT('Ctrl Pts',(6.80077064695807,-16.0461217833684,-10.5701811473657));
#28213=CARTESIAN_POINT('Ctrl Pts',(6.80638919136614,-16.055890517792,-10.5589943859768));
#28214=CARTESIAN_POINT('Ctrl Pts',(6.86694184542916,-16.1568892018711,-10.4424781747251));
#28215=CARTESIAN_POINT('Ctrl Pts',(7.12773354554721,-16.4613449440162,-10.0598381880387));
#28216=CARTESIAN_POINT('Ctrl Pts',(7.31439070777692,-16.6555354433093,-9.80772130191037));
#28217=CARTESIAN_POINT('Ctrl Pts',(7.940028774259,-17.1866517142592,-9.06700808923736));
#28218=CARTESIAN_POINT('Ctrl Pts',(8.42143261566513,-17.524553198201,-8.55884885148502));
#28219=CARTESIAN_POINT('Ctrl Pts',(9.01950058047433,-17.848478792186,-8.00000000200139));
#28220=CARTESIAN_POINT('',(6.80019256622394,-16.0451168089422,-10.5713320279724));
#28221=CARTESIAN_POINT('Origin',(0.,0.,-10.));
#28222=CARTESIAN_POINT('',(10.7941415683196,-11.8077168584163,-12.));
#28223=CARTESIAN_POINT('',(11.8778432569201,-12.7516744235547,-10.5713324653927));
#28224=CARTESIAN_POINT('Origin',(115.265704733382,100.721937252619,-15.4574255506547));
#28225=CARTESIAN_POINT('',(12.787929093689,-9.61272797390185,-12.));
#28226=CARTESIAN_POINT('Origin',(0.,0.,-12.));
#28227=CARTESIAN_POINT('',(14.0272302993381,-10.3404637536614,-10.5713323676496));
#28228=CARTESIAN_POINT('Origin',(94.696528526693,120.26495257181,-15.45742555065));
#28229=CARTESIAN_POINT('',(14.0282296344253,-10.3410482545556,-10.5701811473657));
#28230=CARTESIAN_POINT('',(14.0282296344327,-10.3410482545599,-10.5701811473572));
#28231=CARTESIAN_POINT('',(15.6919659514913,-12.3968459903841,-8.00000000066043));
#28232=CARTESIAN_POINT('Ctrl Pts',(15.6919659511093,-12.3968459912986,-8.00000000133986));
#28233=CARTESIAN_POINT('Ctrl Pts',(15.3272491998243,-11.7202924653894,-8.70558356387746));
#28234=CARTESIAN_POINT('Ctrl Pts',(14.9265913761347,-11.1890623070545,-9.34347605757007));
#28235=CARTESIAN_POINT('Ctrl Pts',(14.435006267903,-10.664861021749,-10.0506525934817));
#28236=CARTESIAN_POINT('Ctrl Pts',(14.306339263984,-10.5520493954836,-10.2211209350345));
#28237=CARTESIAN_POINT('Ctrl Pts',(14.1052003455229,-10.3887460880048,-10.479922296626));
#28238=CARTESIAN_POINT('Ctrl Pts',(14.0365451533539,-10.3459112245296,-10.5606021910004));
#28239=CARTESIAN_POINT('Ctrl Pts',(14.0282296344253,-10.3410482545556,-10.5701811473657));
#28240=CARTESIAN_POINT('',(14.5800974363697,-13.6872329069855,-8.00000000095188));
#28241=CARTESIAN_POINT('Origin',(0.,0.,-8.));
#28242=CARTESIAN_POINT('',(11.8787308647727,-12.7524216806657,-10.5701811473657));
#28243=CARTESIAN_POINT('Ctrl Pts',(11.8787308647727,-12.7524216806657,-10.5701811473657));
#28244=CARTESIAN_POINT('Ctrl Pts',(11.8839533839603,-12.7568185761951,-10.5634041641087));
#28245=CARTESIAN_POINT('Ctrl Pts',(11.9118191664865,-12.7787626049719,-10.5283573896208));
#28246=CARTESIAN_POINT('Ctrl Pts',(12.0246540683316,-12.8559332949065,-10.3949490753023));
#28247=CARTESIAN_POINT('Ctrl Pts',(12.0942400622771,-12.8983084728067,-10.3164610250273));
#28248=CARTESIAN_POINT('Ctrl Pts',(12.3888375657762,-13.0649685395278,-9.99324637123619));
#28249=CARTESIAN_POINT('Ctrl Pts',(12.637766695706,-13.1737249857198,-9.74293995466056));
#28250=CARTESIAN_POINT('Ctrl Pts',(13.412487452553,-13.4589856947937,-8.99849344264267));
#28251=CARTESIAN_POINT('Ctrl Pts',(13.9940974086421,-13.6002632407572,-8.48676451217013));
#28252=CARTESIAN_POINT('Ctrl Pts',(14.5800974373733,-13.687232906307,-8.00000000203881));
#28253=CARTESIAN_POINT('',(11.8778439250753,-12.7516750288689,-10.5713320279724));
#28254=CARTESIAN_POINT('Origin',(0.,0.,-10.));
#28255=CARTESIAN_POINT('',(14.1816521917328,-7.40381055390889,-12.));
#28256=CARTESIAN_POINT('',(15.5228511760086,-7.92019270597788,-10.5713324598785));
#28257=CARTESIAN_POINT('Origin',(73.8654007527194,134.070854041584,-15.4574255507092));
#28258=CARTESIAN_POINT('',(15.3044692038576,-4.65928020123585,-12.));
#28259=CARTESIAN_POINT('Origin',(0.,0.,-12.));
#28260=CARTESIAN_POINT('',(16.7179316974337,-4.91926216737799,-10.5713323676496));
#28261=CARTESIAN_POINT('Origin',(47.8525927546613,145.400208728593,-15.4574255506749));
#28262=CARTESIAN_POINT('',(16.7190706763204,-4.91946962582535,-10.5701811473657));
#28263=CARTESIAN_POINT('',(16.7190706763288,-4.91946962582688,-10.5701811473572));
#28264=CARTESIAN_POINT('',(18.9855956526705,-6.28225625435353,-8.00000000066041));
#28265=CARTESIAN_POINT('Ctrl Pts',(18.9855956526243,-6.28225625534351,-8.00000000133983));
#28266=CARTESIAN_POINT('Ctrl Pts',(18.411474177151,-5.77123997637943,-8.70558959925413));
#28267=CARTESIAN_POINT('Ctrl Pts',(17.8532967549382,-5.40907168025849,-9.34347563383209));
#28268=CARTESIAN_POINT('Ctrl Pts',(17.2120575414615,-5.08460724071215,-10.0506668368878));
#28269=CARTESIAN_POINT('Ctrl Pts',(17.0525658199616,-5.02261030481196,-10.2211342731052));
#28270=CARTESIAN_POINT('Ctrl Pts',(16.807712775309,-4.93795899302286,-10.4799244165698));
#28271=CARTESIAN_POINT('Ctrl Pts',(16.728543360769,-4.92119441373731,-10.5606068211688));
#28272=CARTESIAN_POINT('Ctrl Pts',(16.7190706763204,-4.91946962582536,-10.5701811473657));
#28273=CARTESIAN_POINT('',(18.3821193180501,-7.87510477916341,-8.00000000093431));
#28274=CARTESIAN_POINT('Origin',(0.,0.,-8.));
#28275=CARTESIAN_POINT('',(15.5239408288994,-7.92059131757519,-10.5701811473657));
#28276=CARTESIAN_POINT('Ctrl Pts',(15.5239408288994,-7.92059131757522,-10.5701811473657));
#28277=CARTESIAN_POINT('Ctrl Pts',(15.5345224289455,-7.92446245837779,-10.5589961576797));
#28278=CARTESIAN_POINT('Ctrl Pts',(15.6458257921794,-7.96290977382766,-10.442482799353));
#28279=CARTESIAN_POINT('Ctrl Pts',(16.0413073392502,-8.02850372400974,-10.0598395697742));
#28280=CARTESIAN_POINT('Ctrl Pts',(16.3091180269029,-8.05728223823699,-9.80772253039812));
#28281=CARTESIAN_POINT('Ctrl Pts',(17.1297801903807,-8.06198840490791,-9.06700881562152));
#28282=CARTESIAN_POINT('Ctrl Pts',(17.7157553277321,-8.01139446553857,-8.55885052036936));
#28283=CARTESIAN_POINT('Ctrl Pts',(18.3821193187478,-7.87510477819889,-8.00000000200138));
#28284=CARTESIAN_POINT('',(15.5228520082561,-7.92019304563387,-10.5713320279724));
#28285=CARTESIAN_POINT('Origin',(0.,-19.9979895488606,-8.));
#28286=CARTESIAN_POINT('',(19.9690530659844,-1.11210632608748,-8.));
#28287=CARTESIAN_POINT('',(19.9669855232122,-1.11312313271343,-8.));
#28288=CARTESIAN_POINT('',(19.9913217286364,0.58899607364984,-8.));
#28289=CARTESIAN_POINT('',(19.9913217286364,0.58899607364984,-8.));
#28290=CARTESIAN_POINT('Origin',(-0.00301694686781318,3.94939979918296E-5,
-8.));
#28291=CARTESIAN_POINT('Origin',(0.,-19.9979895488606,-8.));
#28292=CARTESIAN_POINT('',(19.1451345752296,5.78478028355213,-8.));
#28293=CARTESIAN_POINT('',(19.1435395109765,5.78311763536045,-8.));
#28294=CARTESIAN_POINT('',(18.5842506056703,7.39091063456494,-8.00000000377262));
#28295=CARTESIAN_POINT('',(18.5842489954763,7.39090998578283,-8.));
#28296=CARTESIAN_POINT('Origin',(-0.00284851047704926,-0.000994744391011881,
-8.));
#28297=CARTESIAN_POINT('Origin',(0.,-19.9979895488606,-8.));
#28298=CARTESIAN_POINT('',(16.0120303026084,11.983937016731,-8.));
#28299=CARTESIAN_POINT('',(16.0111000635635,11.9818291068306,-8.));
#28300=CARTESIAN_POINT('',(14.9356428424434,13.3013722399403,-8.00000000377261));
#28301=CARTESIAN_POINT('',(14.9356415512525,13.3013710795657,-8.));
#28302=CARTESIAN_POINT('Origin',(-0.00233650163240506,-0.00190900190652155,
-8.));
#28303=CARTESIAN_POINT('Origin',(0.,-19.9979895488606,-8.));
#28304=CARTESIAN_POINT('',(10.9476388630933,16.7376540816183,-8.));
#28305=CARTESIAN_POINT('',(10.9474857026353,16.7353551316722,-8.));
#28306=CARTESIAN_POINT('',(9.48557530180814,17.6074905090519,-8.));
#28307=CARTESIAN_POINT('',(9.48557530180814,17.6074905090519,-8.));
#28308=CARTESIAN_POINT('Origin',(-0.00154267626085947,-0.00259300566760157,
-8.));
#28309=CARTESIAN_POINT('Origin',(0.,-19.9979895488606,-8.));
#28310=CARTESIAN_POINT('',(4.56280060674729,19.4725630427967,-8.));
#28311=CARTESIAN_POINT('',(4.56344294071614,19.4703503440143,-8.));
#28312=CARTESIAN_POINT('',(2.89140893620136,19.7898884520894,-8.00000000377262));
#28313=CARTESIAN_POINT('',(2.89140869296617,19.7898867332294,-8.));
#28314=CARTESIAN_POINT('Origin',(-0.000562781322250294,-0.0029642546098918,
-8.));
#28315=CARTESIAN_POINT('Origin',(0.,-19.9979895488606,-8.));
#28316=CARTESIAN_POINT('',(-2.37237874253754,19.8587935165906,-8.));
#28317=CARTESIAN_POINT('',(-2.37101835849106,19.8569339510296,-8.));
#28318=CARTESIAN_POINT('',(-4.05150484375975,19.5853322433773,-8.00000000377262));
#28319=CARTESIAN_POINT('',(-4.05150448444132,19.5853305449859,-8.));
#28320=CARTESIAN_POINT('Origin',(0.000484993332277583,-0.00297797073663508,
-8.));
#28321=CARTESIAN_POINT('Origin',(0.,-19.9979895488606,-8.));
#28322=CARTESIAN_POINT('',(-9.02141420289104,17.8497604077057,-8.));
#28323=CARTESIAN_POINT('',(-9.01949983406462,17.8484782918853,-8.));
#28324=CARTESIAN_POINT('',(-10.5057473457201,17.0184959173946,-8.00000000377262));
#28325=CARTESIAN_POINT('',(-10.5057464271872,17.018494444323,-8.));
#28326=CARTESIAN_POINT('Origin',(0.00147427065201211,-0.00263249966895751,
-8.));
#28327=CARTESIAN_POINT('Origin',(0.,-19.9979895488606,-8.));
#28328=CARTESIAN_POINT('',(-14.5823339684823,13.6877827592445,-8.));
#28329=CARTESIAN_POINT('',(-14.5800965481548,13.6872326873338,-8.));
#28330=CARTESIAN_POINT('',(-15.6928402991217,12.3989767391864,-8.));
#28331=CARTESIAN_POINT('',(-15.6928402991217,12.3989767391864,-8.));
#28332=CARTESIAN_POINT('Origin',(0.00228572915365266,-0.00196951024334036,
-8.));
#28333=CARTESIAN_POINT('Origin',(0.,-19.9979895488606,-8.));
#28334=CARTESIAN_POINT('',(-18.3844090451459,7.87485649985959,-8.));
#28335=CARTESIAN_POINT('',(-18.3821184221034,7.8751048441898,-8.));
#28336=CARTESIAN_POINT('',(-18.9871476862031,6.28396000343702,-8.00000000377262));
#28337=CARTESIAN_POINT('',(-18.9871460356938,6.28395946542021,-8.));
#28338=CARTESIAN_POINT('Origin',(0.00282149497524475,-0.00106896882248741,
-8.));
#28339=CARTESIAN_POINT('Origin',(0.,-19.9979895488606,-8.));
#28340=CARTESIAN_POINT('',(-19.9690530659844,1.11210632608748,-8.));
#28341=CARTESIAN_POINT('',(-19.9669855232122,1.11312313271343,-8.));
#28342=CARTESIAN_POINT('',(-19.9913234715256,-0.588996128437261,-8.00000000377262));
#28343=CARTESIAN_POINT('',(-19.9913217365416,-0.588996069500264,-8.));
#28344=CARTESIAN_POINT('Origin',(0.00301694686786202,-3.94939976390563E-5,
-8.));
#28345=CARTESIAN_POINT('Origin',(0.,-19.9979895488606,-8.));
#28346=CARTESIAN_POINT('',(-19.1451345752296,-5.78478028355213,-8.));
#28347=CARTESIAN_POINT('',(-19.1435395109765,-5.78311763536045,-8.));
#28348=CARTESIAN_POINT('',(-18.5842506056703,-7.39091063456494,-8.00000000377262));
#28349=CARTESIAN_POINT('',(-18.5842489954764,-7.39090998578282,-8.));
#28350=CARTESIAN_POINT('Origin',(0.00284851047831713,0.000994744391827895,
-8.));
#28351=CARTESIAN_POINT('Origin',(0.,-19.9979895488606,-8.));
#28352=CARTESIAN_POINT('',(-16.0120303026084,-11.983937016731,-8.));
#28353=CARTESIAN_POINT('',(-16.0111000635635,-11.9818291068306,-8.));
#28354=CARTESIAN_POINT('',(-14.9356415425294,-13.3013710776631,-8.));
#28355=CARTESIAN_POINT('',(-14.9356415425294,-13.3013710776631,-8.));
#28356=CARTESIAN_POINT('Origin',(0.0023365016822785,0.00190900194720678,
-8.));
#28357=CARTESIAN_POINT('Origin',(0.,-19.9979895488606,-8.));
#28358=CARTESIAN_POINT('',(-10.9476388630933,-16.7376540816183,-8.));
#28359=CARTESIAN_POINT('',(-10.9474857026353,-16.7353551316722,-8.));
#28360=CARTESIAN_POINT('',(-9.48557612580544,-17.6074920458319,-8.00000000377262));
#28361=CARTESIAN_POINT('',(-9.4855753093544,-17.6074905138232,-8.));
#28362=CARTESIAN_POINT('Origin',(0.00154267626200966,0.00259300566851861,
-8.));
#28363=CARTESIAN_POINT('Origin',(0.,-19.9979895488606,-8.));
#28364=CARTESIAN_POINT('',(-4.56280060674728,-19.4725630427967,-8.));
#28365=CARTESIAN_POINT('',(-4.56344294071613,-19.4703503440143,-8.));
#28366=CARTESIAN_POINT('',(-2.89140893620135,-19.7898884520893,-8.00000000377262));
#28367=CARTESIAN_POINT('',(-2.89140869296616,-19.7898867332294,-8.));
#28368=CARTESIAN_POINT('Origin',(0.000562781322135386,0.00296425461041583,
-8.));
#28369=CARTESIAN_POINT('Origin',(0.,-19.9979895488606,-8.));
#28370=CARTESIAN_POINT('',(2.37237874253754,-19.8587935165906,-8.));
#28371=CARTESIAN_POINT('',(2.37101835849106,-19.8569339510296,-8.));
#28372=CARTESIAN_POINT('',(4.05150484375973,-19.5853322433773,-8.00000000377262));
#28373=CARTESIAN_POINT('',(4.05150448444132,-19.585330544986,-8.));
#28374=CARTESIAN_POINT('Origin',(-0.000484993332055816,0.00297797073728345,
-8.));
#28375=CARTESIAN_POINT('Origin',(0.,-19.9979895488606,-8.));
#28376=CARTESIAN_POINT('',(9.02141420289106,-17.8497604077057,-8.));
#28377=CARTESIAN_POINT('',(9.01949983406462,-17.8484782918853,-8.));
#28378=CARTESIAN_POINT('',(10.5057473457202,-17.0184959173946,-8.00000000377261));
#28379=CARTESIAN_POINT('',(10.5057464271872,-17.018494444323,-8.));
#28380=CARTESIAN_POINT('Origin',(-0.00147427065151251,0.00263249966817813,
-8.));
#28381=CARTESIAN_POINT('Origin',(0.,-19.9979895488606,-8.));
#28382=CARTESIAN_POINT('',(14.5823339684823,-13.6877827592445,-8.));
#28383=CARTESIAN_POINT('',(14.5800965481548,-13.6872326873338,-8.));
#28384=CARTESIAN_POINT('',(15.6928402991217,-12.3989767391864,-8.));
#28385=CARTESIAN_POINT('',(15.6928402991217,-12.3989767391864,-8.));
#28386=CARTESIAN_POINT('Origin',(-0.00228572915365266,0.00196951024334036,
-8.));
#28387=CARTESIAN_POINT('Origin',(0.,-19.9979895488606,-8.));
#28388=CARTESIAN_POINT('',(18.3844090451459,-7.8748564998596,-8.));
#28389=CARTESIAN_POINT('',(18.3821184253814,-7.8751048747288,-8.));
#28390=CARTESIAN_POINT('',(18.9871460296846,-6.28395945881716,-8.));
#28391=CARTESIAN_POINT('',(18.9871460296846,-6.28395945881716,-8.));
#28392=CARTESIAN_POINT('Origin',(-0.00282149497482953,0.00106896882247964,
-8.));
#28393=CARTESIAN_POINT('Origin',(0.,24.1327223341711,-4.));
#28394=CARTESIAN_POINT('',(19.9913181983012,-0.588996262810959,-4.00000000280937));
#28395=CARTESIAN_POINT('',(19.9039912377183,-0.634233661918812,-3.99999999974498));
#28396=CARTESIAN_POINT('Origin',(19.1722717191265,1.97134495680374,-4.));
#28397=CARTESIAN_POINT('',(19.9690495720087,1.11210570270611,-3.99999999517897));
#28398=CARTESIAN_POINT('Origin',(-0.00301694691578147,-3.94939979864173E-5,
-4.));
#28399=CARTESIAN_POINT('',(19.8805681942686,1.15504449566104,-3.99999999942637));
#28400=CARTESIAN_POINT('Ctrl Pts',(19.8805681939836,1.15504449506584,-4.));
#28401=CARTESIAN_POINT('Ctrl Pts',(19.8953407698874,1.14797303633899,-4.));
#28402=CARTESIAN_POINT('Ctrl Pts',(19.9100944560528,1.14086163112927,-4.));
#28403=CARTESIAN_POINT('Ctrl Pts',(19.9395859598404,1.12654859964875,-4.));
#28404=CARTESIAN_POINT('Ctrl Pts',(19.9543240817709,1.11934667292683,-4.));
#28405=CARTESIAN_POINT('Ctrl Pts',(19.9690425803289,1.11210530225922,-4.));
#28406=CARTESIAN_POINT('Origin',(0.,0.,-4.));
#28407=CARTESIAN_POINT('Origin',(0.,24.1327223341711,-4.));
#28408=CARTESIAN_POINT('',(18.9871427769515,6.28395807361808,-4.00000000280937));
#28409=CARTESIAN_POINT('',(18.9205613829861,6.21155990717689,-3.99999999972963));
#28410=CARTESIAN_POINT('Origin',(17.7623944925155,8.36511986266225,-4.));
#28411=CARTESIAN_POINT('',(18.3844059803083,7.87485471676291,-3.99999999499105));
#28412=CARTESIAN_POINT('Origin',(-0.00282149497308426,-0.00106896882069996,
-4.));
#28413=CARTESIAN_POINT('',(18.2865666864733,7.88496026217301,-3.99999999944014));
#28414=CARTESIAN_POINT('Origin',(18.8467331574664,5.50254089697986,-4.00000000000001));
#28415=CARTESIAN_POINT('Origin',(0.,0.,-4.));
#28416=CARTESIAN_POINT('Origin',(0.,24.1327223341711,-4.));
#28417=CARTESIAN_POINT('',(15.6928377163185,12.3989743250248,-4.00000000280937));
#28418=CARTESIAN_POINT('',(15.6550192930803,12.3081879438969,-3.99999999974396));
#28419=CARTESIAN_POINT('Origin',(13.4170351668742,13.8335250454269,-4.));
#28420=CARTESIAN_POINT('',(14.582331698332,13.6877800354455,-3.99999999499104));
#28421=CARTESIAN_POINT('Origin',(-0.00228572913896219,-0.0019695102302042,
-4.));
#28422=CARTESIAN_POINT('',(14.4869365435604,13.6638131243706,-3.99999999943991));
#28423=CARTESIAN_POINT('Origin',(15.8280793362557,11.6165408927719,-4.00000000000001));
#28424=CARTESIAN_POINT('Origin',(0.,0.,-4.));
#28425=CARTESIAN_POINT('Origin',(0.,24.1327223341711,-4.));
#28426=CARTESIAN_POINT('',(10.505744825479,17.0184912834615,-4.00000000280937));
#28427=CARTESIAN_POINT('',(10.5012771500662,16.9202333832982,-3.99999999972948));
#28428=CARTESIAN_POINT('Origin',(8.22962456417494,17.8253797968202,-3.99999999999978));
#28429=CARTESIAN_POINT('',(9.02141299576732,17.8497570701434,-3.99999999517897));
#28430=CARTESIAN_POINT('Origin',(-0.00147427062574423,-0.0026324996252014,
-4.));
#28431=CARTESIAN_POINT('',(8.93996803521359,17.7946084824593,-3.99999999943877));
#28432=CARTESIAN_POINT('Ctrl Pts',(8.93996803557834,17.7946084819266,-4.));
#28433=CARTESIAN_POINT('Ctrl Pts',(8.95347996181212,17.803859942227,-4.));
#28434=CARTESIAN_POINT('Ctrl Pts',(8.96701623560628,17.8130763372781,-4.));
#28435=CARTESIAN_POINT('Ctrl Pts',(8.9941634619296,17.8314571197425,-4.));
#28436=CARTESIAN_POINT('Ctrl Pts',(9.00777496072053,17.8406216686514,-4.));
#28437=CARTESIAN_POINT('Ctrl Pts',(9.02140984672463,17.8497508149477,-4.));
#28438=CARTESIAN_POINT('Origin',(0.,0.,-4.));
#28439=CARTESIAN_POINT('Origin',(0.,24.1327223341711,-4.));
#28440=CARTESIAN_POINT('',(4.05150406040619,19.5853270269313,-4.00000000280937));
#28441=CARTESIAN_POINT('',(4.080889940232,19.4914713868594,-3.99999999974451));
#28442=CARTESIAN_POINT('Origin',(1.38702113800135,19.2224444775015,-4.));
#28443=CARTESIAN_POINT('',(2.37237875432575,19.858789970815,-3.99999999499105));
#28444=CARTESIAN_POINT('Origin',(-0.000484993334474715,-0.00297797075199169,
-4.));
#28445=CARTESIAN_POINT('',(2.31470740046591,19.7791114351774,-3.99999999944106));
#28446=CARTESIAN_POINT('Origin',(4.65787767890032,19.0736433944222,-4.00000000001511));
#28447=CARTESIAN_POINT('Origin',(0.,0.,-4.));
#28448=CARTESIAN_POINT('Origin',(0.,24.1327223341711,-4.));
#28449=CARTESIAN_POINT('',(-2.89140788818329,19.7898832823108,-4.00000000280937));
#28450=CARTESIAN_POINT('',(-2.83169367133746,19.7117383931695,-3.99999999974453));
#28451=CARTESIAN_POINT('Origin',(-5.27109455453329,18.5376028456143,-4.));
#28452=CARTESIAN_POINT('',(-4.56279938294332,19.4725597148893,-3.99999999499105));
#28453=CARTESIAN_POINT('Origin',(0.000562781319235484,-0.00296425459876293,
-4.));
#28454=CARTESIAN_POINT('',(-4.58974103670107,19.3779616247666,-3.99999999944051));
#28455=CARTESIAN_POINT('Origin',(-2.14638779193655,19.5161339587139,-4.));
#28456=CARTESIAN_POINT('Origin',(0.,0.,-4.));
#28457=CARTESIAN_POINT('Origin',(0.,24.1327223341711,-4.));
#28458=CARTESIAN_POINT('',(-9.4855733728222,17.6074875462724,-4.00000000280937));
#28459=CARTESIAN_POINT('',(-9.40271337253749,17.5544894759627,-3.99999999972949));
#28460=CARTESIAN_POINT('Origin',(-11.3224289626212,16.0397515114471,-4.));
#28461=CARTESIAN_POINT('',(-10.9476365748824,16.7376513729739,-3.99999999499105));
#28462=CARTESIAN_POINT('Origin',(0.00154267624008497,-0.00259300563156151,
-4.));
#28463=CARTESIAN_POINT('',(-10.9405989708154,16.6395436738711,-3.99999999943994));
#28464=CARTESIAN_POINT('Origin',(-8.69154686798984,17.6048190481095,-4.));
#28465=CARTESIAN_POINT('Origin',(0.,0.,-4.));
#28466=CARTESIAN_POINT('Origin',(0.,24.1327223341711,-4.));
#28467=CARTESIAN_POINT('',(-14.9356387165454,13.3013689533132,-4.00000000280937));
#28468=CARTESIAN_POINT('',(-14.8396644843238,13.2798899664757,-3.99999999974395));
#28469=CARTESIAN_POINT('Origin',(-15.9531968912017,10.8110539794297,-4.));
#28470=CARTESIAN_POINT('',(-16.0120272253659,11.9839352483846,-3.99999999517897));
#28471=CARTESIAN_POINT('Origin',(0.00233650163479426,-0.0019090019073964,
-4.));
#28472=CARTESIAN_POINT('',(-15.9718592319238,11.8941511756936,-3.99999999943859));
#28473=CARTESIAN_POINT('Ctrl Pts',(-15.9718592313356,11.8941511759604,-4.));
#28474=CARTESIAN_POINT('Ctrl Pts',(-15.9786238224323,11.9090643240662,-4.));
#28475=CARTESIAN_POINT('Ctrl Pts',(-15.9853496524799,11.9239953610795,-4.));
#28476=CARTESIAN_POINT('Ctrl Pts',(-15.9987371250949,11.9539219468768,-4.));
#28477=CARTESIAN_POINT('Ctrl Pts',(-16.0053988318356,11.9689180616204,-4.));
#28478=CARTESIAN_POINT('Ctrl Pts',(-16.0120216120262,11.9839310609795,-4.));
#28479=CARTESIAN_POINT('Origin',(0.,0.,-4.));
#28480=CARTESIAN_POINT('Origin',(0.,24.1327223341711,-4.));
#28481=CARTESIAN_POINT('',(-18.5842456045018,7.39090895728596,-4.00000000280937));
#28482=CARTESIAN_POINT('',(-18.4867130617665,7.40355047939383,-3.9999999997442));
#28483=CARTESIAN_POINT('Origin',(-18.6890790787513,4.70324601679737,-4.00000000001672));
#28484=CARTESIAN_POINT('',(-19.1451310812753,5.78477967944377,-3.99999999499105));
#28485=CARTESIAN_POINT('Origin',(0.00284851048307999,-0.000994744392314173,
-4.));
#28486=CARTESIAN_POINT('',(-19.0766775585171,5.71414847928127,-3.99999999944049));
#28487=CARTESIAN_POINT('Origin',(-17.9746451113272,7.899234737925,-4.00000000001512));
#28488=CARTESIAN_POINT('Origin',(0.,0.,-4.));
#28489=CARTESIAN_POINT('Origin',(0.,24.1327223341711,-4.));
#28490=CARTESIAN_POINT('',(-19.9913181983012,0.588996262810962,-4.00000000280937));
#28491=CARTESIAN_POINT('',(-19.9039912377183,0.634233661918836,-3.99999999974498));
#28492=CARTESIAN_POINT('Origin',(-19.1722692499955,-1.97135300847255,-4.));
#28493=CARTESIAN_POINT('',(-19.9690495761241,-1.11210569876088,-3.99999999499105));
#28494=CARTESIAN_POINT('Origin',(0.00301694687294463,3.94939983909548E-5,
-4.));
#28495=CARTESIAN_POINT('',(-19.8805670108458,-1.15506486493628,-3.99999999944111));
#28496=CARTESIAN_POINT('Origin',(-19.5927310596763,1.27500392343756,-4.00000000000001));
#28497=CARTESIAN_POINT('Origin',(0.,0.,-4.));
#28498=CARTESIAN_POINT('Origin',(0.,24.1327223341711,-4.));
#28499=CARTESIAN_POINT('',(-18.9871427769515,-6.28395807361808,-4.00000000280937));
#28500=CARTESIAN_POINT('',(-18.9205613829861,-6.21155990717691,-3.99999999972963));
#28501=CARTESIAN_POINT('Origin',(-17.7623922349505,-8.3651238873378,-3.9999999999849));
#28502=CARTESIAN_POINT('',(-18.3844059803083,-7.87485471676291,-3.99999999499105));
#28503=CARTESIAN_POINT('Origin',(0.00282149497308426,0.00106896882069996,
-3.99999999999969));
#28504=CARTESIAN_POINT('',(-18.2865666864733,-7.88496026217301,-3.99999999944013));
#28505=CARTESIAN_POINT('Origin',(-18.8467341402544,-5.50253621564204,-4.00000000000001));
#28506=CARTESIAN_POINT('Origin',(0.,0.,-4.));
#28507=CARTESIAN_POINT('Origin',(0.,24.1327223341711,-4.));
#28508=CARTESIAN_POINT('',(-15.6928377163185,-12.3989743250248,-4.00000000280937));
#28509=CARTESIAN_POINT('',(-15.6550192930802,-12.3081879438969,-3.99999999974395));
#28510=CARTESIAN_POINT('Origin',(-13.4170409317638,-13.8335212840106,-4.));
#28511=CARTESIAN_POINT('',(-14.5823316926435,-13.6877800358225,-3.99999999517897));
#28512=CARTESIAN_POINT('Origin',(0.00228572913896219,0.0019695102302042,
-4.));
#28513=CARTESIAN_POINT('',(-14.4869365434846,-13.6638131244428,-3.99999999943857));
#28514=CARTESIAN_POINT('Ctrl Pts',(-14.4869365436452,-13.6638131238172,
-4.));
#28515=CARTESIAN_POINT('Ctrl Pts',(-14.5027977864062,-13.6678853048282,
-4.));
#28516=CARTESIAN_POINT('Ctrl Pts',(-14.5186699155297,-13.6719162072235,
-4.));
#28517=CARTESIAN_POINT('Ctrl Pts',(-14.5504665592734,-13.6799035971688,
-4.));
#28518=CARTESIAN_POINT('Ctrl Pts',(-14.5663916423942,-13.6838600496388,
-4.));
#28519=CARTESIAN_POINT('Ctrl Pts',(-14.5823265941083,-13.6877752348972,
-4.));
#28520=CARTESIAN_POINT('Origin',(0.,0.,-4.));
#28521=CARTESIAN_POINT('Origin',(0.,24.1327223341711,-4.));
#28522=CARTESIAN_POINT('',(-10.505744825479,-17.0184912834615,-4.00000000280937));
#28523=CARTESIAN_POINT('',(-10.5012771500661,-16.9202333832982,-3.99999999972949));
#28524=CARTESIAN_POINT('Origin',(-8.22961578723204,-17.8253832975409,-4.));
#28525=CARTESIAN_POINT('',(-9.02141300124166,-17.8497570717348,-3.99999999499105));
#28526=CARTESIAN_POINT('Origin',(0.00147427062565764,0.00263249962513257,
-4.));
#28527=CARTESIAN_POINT('',(-8.93996803530948,-17.7946084824175,-3.99999999944011));
#28528=CARTESIAN_POINT('Origin',(-10.9004721713661,-16.3296227715457,-4.));
#28529=CARTESIAN_POINT('Origin',(0.,0.,-4.));
#28530=CARTESIAN_POINT('Origin',(0.,24.1327223341711,-4.));
#28531=CARTESIAN_POINT('',(-4.05150406040619,-19.5853270269313,-4.00000000280937));
#28532=CARTESIAN_POINT('',(-4.08088994023202,-19.4914713868594,-3.99999999974451));
#28533=CARTESIAN_POINT('Origin',(-1.38701078444917,-19.2224432491099,-4.00000000001672));
#28534=CARTESIAN_POINT('',(-2.37237875432574,-19.858789970815,-3.99999999499105));
#28535=CARTESIAN_POINT('Origin',(0.00048499333459795,0.0029779707527644,
-4.));
#28536=CARTESIAN_POINT('',(-2.31470740046595,-19.7791114351774,-3.99999999944107));
#28537=CARTESIAN_POINT('Origin',(-4.65788263325231,-19.073641819594,-3.99999999999017));
#28538=CARTESIAN_POINT('Origin',(0.,0.,-4.));
#28539=CARTESIAN_POINT('Origin',(0.,24.1327223341711,-4.));
#28540=CARTESIAN_POINT('',(2.89140788818329,-19.7898832823108,-4.00000000280937));
#28541=CARTESIAN_POINT('',(2.83169367133745,-19.7117383931695,-3.99999999974453));
#28542=CARTESIAN_POINT('Origin',(5.27108671270436,-18.5376067961811,-4.));
#28543=CARTESIAN_POINT('',(4.5627993829433,-19.4725597148893,-3.99999999499105));
#28544=CARTESIAN_POINT('Origin',(-0.000562781329067619,0.00296425464298977,
-4.));
#28545=CARTESIAN_POINT('',(4.58974103670108,-19.3779616247666,-3.99999999944051));
#28546=CARTESIAN_POINT('Origin',(2.14638847124274,-19.5161339346574,-4.00000000000001));
#28547=CARTESIAN_POINT('Origin',(0.,0.,-4.));
#28548=CARTESIAN_POINT('Origin',(0.,24.1327223341711,-4.));
#28549=CARTESIAN_POINT('',(9.48557337282221,-17.6074875462724,-4.00000000280937));
#28550=CARTESIAN_POINT('',(9.40271337253742,-17.5544894759628,-3.99999999972949));
#28551=CARTESIAN_POINT('Origin',(11.3224256916247,-16.0397541074757,-4.));
#28552=CARTESIAN_POINT('',(10.9476365748824,-16.7376513729739,-3.99999999499105));
#28553=CARTESIAN_POINT('Origin',(-0.00154267623871274,0.00259300562955644,
-4.));
#28554=CARTESIAN_POINT('',(10.9405989708155,-16.639543673871,-3.99999999943993));
#28555=CARTESIAN_POINT('Origin',(8.69154190830326,-17.6048210232288,-3.9999999999849));
#28556=CARTESIAN_POINT('Origin',(0.,0.,-4.));
#28557=CARTESIAN_POINT('Origin',(0.,24.1327223341711,-4.));
#28558=CARTESIAN_POINT('',(14.9356387165454,-13.3013689533132,-4.00000000280937));
#28559=CARTESIAN_POINT('',(14.8396644843238,-13.2798899664757,-3.99999999974396));
#28560=CARTESIAN_POINT('Origin',(15.9531974199694,-10.8110527965528,-4.));
#28561=CARTESIAN_POINT('',(16.0120272253659,-11.9839352483846,-3.99999999517897));
#28562=CARTESIAN_POINT('Origin',(-0.00233650165790245,0.00190900192542198,
-4.));
#28563=CARTESIAN_POINT('',(15.9718469875142,-11.8941676178388,-3.99999999942454));
#28564=CARTESIAN_POINT('Ctrl Pts',(15.9718469869114,-11.8941676181125,-4.));
#28565=CARTESIAN_POINT('Ctrl Pts',(15.978618029634,-11.9090802746427,-4.));
#28566=CARTESIAN_POINT('Ctrl Pts',(15.985348914733,-11.9240113943218,-4.));
#28567=CARTESIAN_POINT('Ctrl Pts',(15.9987405096734,-11.953932543778,-4.));
#28568=CARTESIAN_POINT('Ctrl Pts',(16.0054012593359,-11.9689229988458,-4.));
#28569=CARTESIAN_POINT('Ctrl Pts',(16.0120216120262,-11.9839310609795,-4.));
#28570=CARTESIAN_POINT('Origin',(0.,0.,-4.));
#28571=CARTESIAN_POINT('Origin',(0.,24.1327223341711,-4.));
#28572=CARTESIAN_POINT('',(18.5842456045018,-7.39090895728597,-4.00000000280937));
#28573=CARTESIAN_POINT('',(18.4867046535595,-7.40357147462304,-3.99999999972962));
#28574=CARTESIAN_POINT('Origin',(18.9837728420122,-5.00938144430632,-4.));
#28575=CARTESIAN_POINT('',(19.1451310787574,-5.78477967432897,-3.99999999517897));
#28576=CARTESIAN_POINT('Origin',(-0.0028485105206455,0.0009947444054903,
-4.));
#28577=CARTESIAN_POINT('',(19.0766716890448,-5.71416807437949,-3.9999999994254));
#28578=CARTESIAN_POINT('Ctrl Pts',(19.0766716885727,-5.71416807484213,-4.));
#28579=CARTESIAN_POINT('Ctrl Pts',(19.0881348030286,-5.72586557189522,-4.));
#28580=CARTESIAN_POINT('Ctrl Pts',(19.0995665001737,-5.73759414976848,-4.));
#28581=CARTESIAN_POINT('Ctrl Pts',(19.1223841117608,-5.76113066141302,-4.));
#28582=CARTESIAN_POINT('Ctrl Pts',(19.1337702092287,-5.77293898138808,-4.));
#28583=CARTESIAN_POINT('Ctrl Pts',(19.1451243717667,-5.78477765933064,-4.));
#28584=CARTESIAN_POINT('Origin',(0.,0.,-4.));
#28585=CARTESIAN_POINT('Origin',(0.,19.9140934904867,4.));
#28586=CARTESIAN_POINT('',(19.9099067849541,0.408327476897224,3.99999999942692));
#28587=CARTESIAN_POINT('',(19.9947464642997,0.458076119992405,3.99999999517722));
#28588=CARTESIAN_POINT('Ctrl Pts',(19.9099067846237,0.408327477467692,4.));
#28589=CARTESIAN_POINT('Ctrl Pts',(19.9240789959544,0.416536192806554,4.));
#28590=CARTESIAN_POINT('Ctrl Pts',(19.9382292433099,0.424783246564917,4.));
#28591=CARTESIAN_POINT('Ctrl Pts',(19.9665068467169,0.441366048207167,4.));
#28592=CARTESIAN_POINT('Ctrl Pts',(19.9806344826889,0.449702119578792,4.));
#28593=CARTESIAN_POINT('Ctrl Pts',(19.9947394627542,0.458075970644694,4.));
#28594=CARTESIAN_POINT('',(19.7928724810088,2.19392763772769,3.99999999974475));
#28595=CARTESIAN_POINT('Origin',(0.,0.,4.));
#28596=CARTESIAN_POINT('',(19.8834795218938,2.15568133214589,4.00000000280589));
#28597=CARTESIAN_POINT('Origin',(19.2673652038706,-0.46139871247229,4.));
#28598=CARTESIAN_POINT('Origin',(-0.00301074532259138,-0.000197334674881602,
4.));
#28599=CARTESIAN_POINT('Origin',(0.,19.9140934904867,4.));
#28600=CARTESIAN_POINT('',(18.5695436020587,7.19327254633851,3.99999999943895));
#28601=CARTESIAN_POINT('',(18.6322444467737,7.26905680119529,3.99999999517722));
#28602=CARTESIAN_POINT('Ctrl Pts',(18.5695436015635,7.19327254675251,4.));
#28603=CARTESIAN_POINT('Ctrl Pts',(18.5800475284678,7.20583555504045,4.));
#28604=CARTESIAN_POINT('Ctrl Pts',(18.5905188856696,7.21842615925354,4.));
#28605=CARTESIAN_POINT('Ctrl Pts',(18.6114169918593,7.24368668807207,4.));
#28606=CARTESIAN_POINT('Ctrl Pts',(18.6218439539793,7.25635714098723,4.));
#28607=CARTESIAN_POINT('Ctrl Pts',(18.632237918553,7.26905426618477,4.));
#28608=CARTESIAN_POINT('',(17.8488387931384,8.83119885770583,3.99999999972955));
#28609=CARTESIAN_POINT('Origin',(0.,0.,4.));
#28610=CARTESIAN_POINT('',(17.947072548527,8.82622835625882,4.00000000299381));
#28611=CARTESIAN_POINT('Origin',(18.5321522754301,6.48331038043728,4.));
#28612=CARTESIAN_POINT('Origin',(-0.00276168272250299,-0.00121516948046296,
4.));
#28613=CARTESIAN_POINT('Origin',(0.,19.9140934904867,4.));
#28614=CARTESIAN_POINT('',(14.9894054755396,13.1106385429418,3.99999999942451));
#28615=CARTESIAN_POINT('',(15.0224187663253,13.2032819523213,3.99999999517722));
#28616=CARTESIAN_POINT('Ctrl Pts',(14.9894054749172,13.1106385431674,4.));
#28617=CARTESIAN_POINT('Ctrl Pts',(14.9949856121388,13.1260364783791,4.));
#28618=CARTESIAN_POINT('Ctrl Pts',(15.0005242666941,13.1414496691744,4.));
#28619=CARTESIAN_POINT('Ctrl Pts',(15.0115269942644,13.1723292732651,4.));
#28620=CARTESIAN_POINT('Ctrl Pts',(15.0169910736063,13.1877961136521,4.));
#28621=CARTESIAN_POINT('Ctrl Pts',(15.0224134988291,13.2032773374076,4.));
#28622=CARTESIAN_POINT('',(13.7519742127091,14.4032747936281,3.99999999972944));
#28623=CARTESIAN_POINT('Origin',(0.,0.,4.));
#28624=CARTESIAN_POINT('',(13.8459837511274,14.4322019810711,4.00000000299381));
#28625=CARTESIAN_POINT('Origin',(15.1970464502794,12.4305473706751,4.));
#28626=CARTESIAN_POINT('Origin',(-0.00217952044569536,-0.0020864369252549,
4.));
#28627=CARTESIAN_POINT('Origin',(0.,19.9140934904867,4.));
#28628=CARTESIAN_POINT('',(9.60134920853995,17.4466390141573,3.99999999943866));
#28629=CARTESIAN_POINT('',(9.60066767536943,17.5449964403088,3.99999999517722));
#28630=CARTESIAN_POINT('Ctrl Pts',(9.60134920789419,17.4466390141562,4.));
#28631=CARTESIAN_POINT('Ctrl Pts',(9.60132034098192,17.4630146314442,4.));
#28632=CARTESIAN_POINT('Ctrl Pts',(9.60124878486742,17.4793904530073,4.));
#28633=CARTESIAN_POINT('Ctrl Pts',(9.60102051245635,17.5121741820761,4.));
#28634=CARTESIAN_POINT('Ctrl Pts',(9.6008636198518,17.5285826312153,4.));
#28635=CARTESIAN_POINT('Ctrl Pts',(9.6006643039356,17.5449903021187,4.));
#28636=CARTESIAN_POINT('',(7.99641856994512,18.2381032342188,3.99999999972954));
#28637=CARTESIAN_POINT('Origin',(0.,0.,4.));
#28638=CARTESIAN_POINT('',(8.07486496484469,18.2974390476607,4.00000000280589));
#28639=CARTESIAN_POINT('Origin',(10.0290598294463,16.8787298443224,3.99999999999999));
#28640=CARTESIAN_POINT('Origin',(-0.00133447584031332,-0.00270604931077445,
4.));
#28641=CARTESIAN_POINT('Origin',(0.,19.9140934904867,4.));
#28642=CARTESIAN_POINT('',(3.05519487166812,19.6783359004266,3.99999999942581));
#28643=CARTESIAN_POINT('',(3.02093437199968,19.7705254210252,3.99999999517722));
#28644=CARTESIAN_POINT('Ctrl Pts',(3.05519487104775,19.6783359001999,4.));
#28645=CARTESIAN_POINT('Ctrl Pts',(3.0495718701275,19.6937182385374,4.));
#28646=CARTESIAN_POINT('Ctrl Pts',(3.04390729298132,19.7090856016079,4.));
#28647=CARTESIAN_POINT('Ctrl Pts',(3.03248680703719,19.739813173271,4.));
#28648=CARTESIAN_POINT('Ctrl Pts',(3.02673062840326,19.755173713429,4.));
#28649=CARTESIAN_POINT('Ctrl Pts',(3.02093330327285,19.770518499915,4.));
#28650=CARTESIAN_POINT('',(1.27637679137333,19.873147254883,3.99999999973));
#28651=CARTESIAN_POINT('Origin',(0.,0.,4.));
#28652=CARTESIAN_POINT('',(1.32979829814077,19.9557349287161,4.0000000029938));
#28653=CARTESIAN_POINT('Origin',(3.6511832014166,19.2915843141947,4.));
#28654=CARTESIAN_POINT('Origin',(-0.000328473722452371,-0.00299927214920226,
4.));
#28655=CARTESIAN_POINT('Origin',(0.,19.9140934904867,4.));
#28656=CARTESIAN_POINT('',(-3.85944318620814,19.5365252234455,3.99999999942585));
#28657=CARTESIAN_POINT('',(-3.92316820087621,19.6114372540864,3.99999999517722));
#28658=CARTESIAN_POINT('Ctrl Pts',(-3.8594431867135,19.5365252230202,4.));
#28659=CARTESIAN_POINT('Ctrl Pts',(-3.86998814946638,19.5490567127974,4.));
#28660=CARTESIAN_POINT('Ctrl Pts',(-3.88056705909194,19.5615599106554,4.));
#28661=CARTESIAN_POINT('Ctrl Pts',(-3.90180825488829,19.5865283465661,4.));
#28662=CARTESIAN_POINT('Ctrl Pts',(-3.91247090803087,19.5989938039058,4.));
#28663=CARTESIAN_POINT('Ctrl Pts',(-3.92316683799181,19.611430384844,4.));
#28664=CARTESIAN_POINT('',(-5.59761479267543,19.1111964084047,3.99999999972973));
#28665=CARTESIAN_POINT('Origin',(0.,0.,4.));
#28666=CARTESIAN_POINT('',(-5.57566167259198,19.2070746593985,4.00000000299381));
#28667=CARTESIAN_POINT('Origin',(-3.16690114173538,19.3766326568612,4.));
#28668=CARTESIAN_POINT('Origin',(0.000717147159679521,-0.00293073854793047,
4.));
#28669=CARTESIAN_POINT('Origin',(0.,19.9140934904867,4.));
#28670=CARTESIAN_POINT('',(-10.3085579923323,17.0383318324703,3.99999999943867));
#28671=CARTESIAN_POINT('',(-10.3940787889303,17.0869203203164,3.99999999517722));
#28672=CARTESIAN_POINT('Ctrl Pts',(-10.3085579926542,17.0383318319105,4.));
#28673=CARTESIAN_POINT('Ctrl Pts',(-10.3227541267253,17.0464946409769,4.));
#28674=CARTESIAN_POINT('Ctrl Pts',(-10.3369717822929,17.0546205822697,4.));
#28675=CARTESIAN_POINT('Ctrl Pts',(-10.3654774608083,17.0708147570336,4.));
#28676=CARTESIAN_POINT('Ctrl Pts',(-10.379766040979,17.0788831086342,4.));
#28677=CARTESIAN_POINT('Ctrl Pts',(-10.3940751588187,17.086914331474,4.));
#28678=CARTESIAN_POINT('',(-11.7964514251346,16.0441532435407,3.99999999972946));
#28679=CARTESIAN_POINT('Origin',(0.,0.,4.));
#28680=CARTESIAN_POINT('',(-11.8086145576078,16.1417577199254,4.00000000299381));
#28681=CARTESIAN_POINT('Origin',(-9.60276988745231,17.1247213783635,4.));
#28682=CARTESIAN_POINT('Origin',(0.00167626948831101,-0.00250871457599722,
4.));
#28683=CARTESIAN_POINT('Origin',(0.,19.9140934904867,4.));
#28684=CARTESIAN_POINT('',(-15.5143414292227,12.4850442342554,3.9999999994245));
#28685=CARTESIAN_POINT('',(-15.611310074774,12.5014686198299,3.99999999517722));
#28686=CARTESIAN_POINT('Ctrl Pts',(-15.5143414293368,12.4850442336032,4.));
#28687=CARTESIAN_POINT('Ctrl Pts',(-15.5304744159661,12.4878657726368,4.));
#28688=CARTESIAN_POINT('Ctrl Pts',(-15.546615223024,12.4906438101088,4.));
#28689=CARTESIAN_POINT('Ctrl Pts',(-15.5789363001155,12.4961171945695,4.));
#28690=CARTESIAN_POINT('Ctrl Pts',(-15.5951169918514,12.4988124736256,4.));
#28691=CARTESIAN_POINT('Ctrl Pts',(-15.6113046152802,12.5014642337302,4.));
#28692=CARTESIAN_POINT('',(-16.5724619474212,11.0419484027528,3.99999999972945));
#28693=CARTESIAN_POINT('Origin',(0.,0.,4.));
#28694=CARTESIAN_POINT('',(-16.6172742483527,11.1295065685037,4.00000000280589));
#28695=CARTESIAN_POINT('Origin',(-14.8806548824468,12.8076250541992,4.));
#28696=CARTESIAN_POINT('Origin',(0.00243320901777366,-0.00178410266734153,
4.));
#28697=CARTESIAN_POINT('Origin',(0.,19.9140934904867,4.));
#28698=CARTESIAN_POINT('',(-18.8488487596698,6.42588670526778,3.99999999942508));
#28699=CARTESIAN_POINT('',(-18.9455869672014,6.40815530176509,3.99999999517722));
#28700=CARTESIAN_POINT('Ctrl Pts',(-18.8488487595541,6.42588670461663,4.));
#28701=CARTESIAN_POINT('Ctrl Pts',(-18.864973830457,6.42302026310499,4.));
#28702=CARTESIAN_POINT('Ctrl Pts',(-18.8810913724055,6.42011027220655,4.));
#28703=CARTESIAN_POINT('Ctrl Pts',(-18.913335263081,6.41419909595026,4.));
#28704=CARTESIAN_POINT('Ctrl Pts',(-18.9294619849968,6.41119770248451,4.));
#28705=CARTESIAN_POINT('Ctrl Pts',(-18.9455803368209,6.40815304743644,4.));
#28706=CARTESIAN_POINT('',(-19.3495889823633,4.70792159465315,3.99999999972972));
#28707=CARTESIAN_POINT('Origin',(0.,0.,4.));
#28708=CARTESIAN_POINT('',(-19.4216454237194,4.77487267832733,4.00000000299381));
#28709=CARTESIAN_POINT('Origin',(-18.3640870092082,6.94570038752625,4.));
#28710=CARTESIAN_POINT('Origin',(0.00289666758562568,-0.000844301606275355,
4.));
#28711=CARTESIAN_POINT('Origin',(0.,19.9140934904867,4.));
#28712=CARTESIAN_POINT('',(-19.9099067849541,-0.408327476897221,3.99999999942691));
#28713=CARTESIAN_POINT('',(-19.9947464642997,-0.458076119992403,3.99999999517722));
#28714=CARTESIAN_POINT('Ctrl Pts',(-19.9099067846237,-0.408327477467691,
4.));
#28715=CARTESIAN_POINT('Ctrl Pts',(-19.9240789959545,-0.416536192806615,
4.));
#28716=CARTESIAN_POINT('Ctrl Pts',(-19.9382292433101,-0.424783246565044,
4.));
#28717=CARTESIAN_POINT('Ctrl Pts',(-19.9665068467166,-0.441366048206973,
4.));
#28718=CARTESIAN_POINT('Ctrl Pts',(-19.9806344826885,-0.449702119578518,
4.));
#28719=CARTESIAN_POINT('Ctrl Pts',(-19.9947394627542,-0.458075970644692,
4.));
#28720=CARTESIAN_POINT('',(-19.7928699969466,-2.19395004769781,3.99999999973002));
#28721=CARTESIAN_POINT('Origin',(0.,0.,4.));
#28722=CARTESIAN_POINT('',(-19.8834795259929,-2.15568133042439,4.0000000029938));
#28723=CARTESIAN_POINT('Origin',(-19.6325516134049,0.245736990623587,4.));
#28724=CARTESIAN_POINT('Origin',(0.00301074532257362,0.000197334674880076,
4.));
#28725=CARTESIAN_POINT('Origin',(0.,19.9140934904867,4.));
#28726=CARTESIAN_POINT('',(-18.5695436020587,-7.19327254633852,3.99999999943895));
#28727=CARTESIAN_POINT('',(-18.6322444467737,-7.26905680119529,3.99999999517722));
#28728=CARTESIAN_POINT('Ctrl Pts',(-18.5695436015635,-7.19327254675251,
4.));
#28729=CARTESIAN_POINT('Ctrl Pts',(-18.5800475284678,-7.20583555504053,
4.));
#28730=CARTESIAN_POINT('Ctrl Pts',(-18.5905188856698,-7.2184261592537,4.));
#28731=CARTESIAN_POINT('Ctrl Pts',(-18.6114169918594,-7.24368668807219,
4.));
#28732=CARTESIAN_POINT('Ctrl Pts',(-18.6218439539793,-7.25635714098729,
4.));
#28733=CARTESIAN_POINT('Ctrl Pts',(-18.632237918553,-7.26905426618477,4.));
#28734=CARTESIAN_POINT('',(-17.8488387931384,-8.83119885770584,3.99999999972955));
#28735=CARTESIAN_POINT('Origin',(0.,0.,4.));
#28736=CARTESIAN_POINT('',(-17.947072548527,-8.82622835625882,4.00000000299381));
#28737=CARTESIAN_POINT('Origin',(-18.5321530186718,-6.48330768932856,4.0000000000151));
#28738=CARTESIAN_POINT('Origin',(0.00276168272122623,0.0012151694794782,
4.));
#28739=CARTESIAN_POINT('Origin',(0.,19.9140934904867,4.));
#28740=CARTESIAN_POINT('',(-14.9894054755396,-13.1106385429418,3.9999999994245));
#28741=CARTESIAN_POINT('',(-15.0224187663253,-13.2032819523213,3.99999999517722));
#28742=CARTESIAN_POINT('Ctrl Pts',(-14.9894054749172,-13.1106385431674,
4.));
#28743=CARTESIAN_POINT('Ctrl Pts',(-14.9949856121388,-13.1260364783793,
4.));
#28744=CARTESIAN_POINT('Ctrl Pts',(-15.0005242666942,-13.1414496691749,
4.));
#28745=CARTESIAN_POINT('Ctrl Pts',(-15.0115269942646,-13.1723292732657,
4.));
#28746=CARTESIAN_POINT('Ctrl Pts',(-15.0169910736066,-13.1877961136528,
4.));
#28747=CARTESIAN_POINT('Ctrl Pts',(-15.0224134988291,-13.2032773374076,
4.));
#28748=CARTESIAN_POINT('',(-13.751974212639,-14.403274793695,3.99999999972944));
#28749=CARTESIAN_POINT('Origin',(0.,0.,4.));
#28750=CARTESIAN_POINT('',(-13.8459837468808,-14.4322019797551,4.00000000280589));
#28751=CARTESIAN_POINT('Origin',(-15.1970434703156,-12.4305516593735,4.));
#28752=CARTESIAN_POINT('Origin',(0.00217952044569536,0.0020864369252549,
4.));
#28753=CARTESIAN_POINT('Origin',(0.,19.9140934904867,4.));
#28754=CARTESIAN_POINT('',(-9.60134920853987,-17.4466390141574,3.99999999943866));
#28755=CARTESIAN_POINT('',(-9.60066767536943,-17.5449964403088,3.99999999517722));
#28756=CARTESIAN_POINT('Ctrl Pts',(-9.60134920789411,-17.4466390141562,
4.));
#28757=CARTESIAN_POINT('Ctrl Pts',(-9.60132034098186,-17.4630146314438,
4.));
#28758=CARTESIAN_POINT('Ctrl Pts',(-9.60124878486737,-17.4793904530065,
4.));
#28759=CARTESIAN_POINT('Ctrl Pts',(-9.60102051245632,-17.5121741820764,
4.));
#28760=CARTESIAN_POINT('Ctrl Pts',(-9.60086361985177,-17.5285826312158,
4.));
#28761=CARTESIAN_POINT('Ctrl Pts',(-9.6006643039356,-17.5449903021187,4.));
#28762=CARTESIAN_POINT('',(-7.99641857003384,-18.2381032341799,3.99999999972955));
#28763=CARTESIAN_POINT('Origin',(0.,0.,4.));
#28764=CARTESIAN_POINT('',(-8.07486496838508,-18.2974390503498,4.0000000029938));
#28765=CARTESIAN_POINT('Origin',(-10.0290617346374,-16.8787286365668,4.00000000001511));
#28766=CARTESIAN_POINT('Origin',(0.00133447584018453,0.00270604930997509,
4.));
#28767=CARTESIAN_POINT('Origin',(0.,19.9140934904867,4.));
#28768=CARTESIAN_POINT('',(-3.05519487166813,-19.6783359004266,3.99999999942581));
#28769=CARTESIAN_POINT('',(-3.02093437199967,-19.7705254210252,3.99999999517722));
#28770=CARTESIAN_POINT('Ctrl Pts',(-3.05519487104776,-19.6783359001999,
4.));
#28771=CARTESIAN_POINT('Ctrl Pts',(-3.04957187012752,-19.6937182385374,
4.));
#28772=CARTESIAN_POINT('Ctrl Pts',(-3.04390729298135,-19.7090856016078,
4.));
#28773=CARTESIAN_POINT('Ctrl Pts',(-3.03248680703726,-19.7398131732708,
4.));
#28774=CARTESIAN_POINT('Ctrl Pts',(-3.02673062840331,-19.7551737134288,
4.));
#28775=CARTESIAN_POINT('Ctrl Pts',(-3.02093330327284,-19.770518499915,4.));
#28776=CARTESIAN_POINT('',(-1.27637679137335,-19.873147254883,3.99999999973));
#28777=CARTESIAN_POINT('Origin',(0.,0.,4.));
#28778=CARTESIAN_POINT('',(-1.32979829814076,-19.9557349287161,4.0000000029938));
#28779=CARTESIAN_POINT('Origin',(-3.65116939301718,-19.2915880101181,3.9999999999849));
#28780=CARTESIAN_POINT('Origin',(0.000328473722462364,0.00299927214920226,
4.));
#28781=CARTESIAN_POINT('Origin',(0.,19.9140934904867,4.));
#28782=CARTESIAN_POINT('',(3.85944318620815,-19.5365252234455,3.99999999942585));
#28783=CARTESIAN_POINT('',(3.92316820087621,-19.6114372540864,3.99999999517722));
#28784=CARTESIAN_POINT('Ctrl Pts',(3.85944318671351,-19.5365252230202,4.));
#28785=CARTESIAN_POINT('Ctrl Pts',(3.86998814946643,-19.5490567127974,4.));
#28786=CARTESIAN_POINT('Ctrl Pts',(3.88056705909203,-19.5615599106555,4.));
#28787=CARTESIAN_POINT('Ctrl Pts',(3.9018082548882,-19.5865283465659,4.));
#28788=CARTESIAN_POINT('Ctrl Pts',(3.91247090803083,-19.5989938039058,4.));
#28789=CARTESIAN_POINT('Ctrl Pts',(3.92316683799182,-19.6114303848441,4.));
#28790=CARTESIAN_POINT('',(5.59761479267544,-19.1111964084047,3.99999999972974));
#28791=CARTESIAN_POINT('Origin',(0.,0.,4.));
#28792=CARTESIAN_POINT('',(5.57566167259198,-19.2070746593985,4.00000000299381));
#28793=CARTESIAN_POINT('Origin',(3.16689861973229,-19.3766328787332,4.00000000000001));
#28794=CARTESIAN_POINT('Origin',(-0.000717147160155251,0.00293073854892079,
4.));
#28795=CARTESIAN_POINT('Origin',(0.,19.9140934904867,4.));
#28796=CARTESIAN_POINT('',(10.3085579923322,-17.0383318324703,3.99999999943867));
#28797=CARTESIAN_POINT('',(10.3940787889303,-17.0869203203164,3.99999999517722));
#28798=CARTESIAN_POINT('Ctrl Pts',(10.3085579926541,-17.0383318319105,4.));
#28799=CARTESIAN_POINT('Ctrl Pts',(10.3227541267254,-17.046494640977,4.));
#28800=CARTESIAN_POINT('Ctrl Pts',(10.336971782293,-17.0546205822698,4.));
#28801=CARTESIAN_POINT('Ctrl Pts',(10.3654774608076,-17.0708147570333,4.));
#28802=CARTESIAN_POINT('Ctrl Pts',(10.3797660409782,-17.0788831086338,4.));
#28803=CARTESIAN_POINT('Ctrl Pts',(10.3940751588187,-17.086914331474,4.));
#28804=CARTESIAN_POINT('',(11.7964514251347,-16.0441532435407,3.99999999972945));
#28805=CARTESIAN_POINT('Origin',(0.,0.,4.));
#28806=CARTESIAN_POINT('',(11.8086145576078,-16.1417577199254,4.0000000029938));
#28807=CARTESIAN_POINT('Origin',(9.60277970218749,-17.1247167460198,3.9999999999849));
#28808=CARTESIAN_POINT('Origin',(-0.00167626950157151,0.00250871459651858,
4.));
#28809=CARTESIAN_POINT('Origin',(0.,19.9140934904867,4.));
#28810=CARTESIAN_POINT('',(15.5143414292227,-12.4850442342554,3.9999999994245));
#28811=CARTESIAN_POINT('',(15.611310074774,-12.5014686198299,3.99999999517722));
#28812=CARTESIAN_POINT('Ctrl Pts',(15.5143414293368,-12.4850442336032,4.));
#28813=CARTESIAN_POINT('Ctrl Pts',(15.5304744159665,-12.4878657726369,4.));
#28814=CARTESIAN_POINT('Ctrl Pts',(15.5466152230249,-12.4906438101089,4.));
#28815=CARTESIAN_POINT('Ctrl Pts',(15.5789363001168,-12.4961171945697,4.));
#28816=CARTESIAN_POINT('Ctrl Pts',(15.5951169918525,-12.4988124736257,4.));
#28817=CARTESIAN_POINT('Ctrl Pts',(15.6113046152802,-12.5014642337302,4.));
#28818=CARTESIAN_POINT('',(16.5724493912922,-11.0419672478261,3.99999999974397));
#28819=CARTESIAN_POINT('Origin',(0.,0.,4.));
#28820=CARTESIAN_POINT('',(16.6172742483527,-11.1295065685037,4.00000000280589));
#28821=CARTESIAN_POINT('Origin',(14.4611068945492,-12.7381772024518,4.));
#28822=CARTESIAN_POINT('Origin',(-0.00243320901777366,0.00178410266734153,
4.));
#28823=CARTESIAN_POINT('Origin',(0.,19.9140934904867,4.));
#28824=CARTESIAN_POINT('',(18.8488421537318,-6.42590608228654,3.99999999943894));
#28825=CARTESIAN_POINT('',(18.9455869672014,-6.4081553017651,3.99999999517722));
#28826=CARTESIAN_POINT('Ctrl Pts',(18.8488421536186,-6.42590608165111,4.));
#28827=CARTESIAN_POINT('Ctrl Pts',(18.8649639745842,-6.42303405323124,4.));
#28828=CARTESIAN_POINT('Ctrl Pts',(18.881078584019,-6.4201199496557,4.));
#28829=CARTESIAN_POINT('Ctrl Pts',(18.9133246169989,-6.41420230587836,4.));
#28830=CARTESIAN_POINT('Ctrl Pts',(18.929456543401,-6.41119849796776,4.));
#28831=CARTESIAN_POINT('Ctrl Pts',(18.9455803368209,-6.40815304743646,4.));
#28832=CARTESIAN_POINT('',(19.3495836396352,-4.70794355337793,3.99999999974434));
#28833=CARTESIAN_POINT('Origin',(0.,0.,4.));
#28834=CARTESIAN_POINT('',(19.4216454204563,-4.77487267530771,4.00000000280589));
#28835=CARTESIAN_POINT('Origin',(17.9465883718404,-7.02371079670489,3.99999999998329));
#28836=CARTESIAN_POINT('Origin',(-0.00289666758440221,0.000844301606205411,
4.));
#28837=CARTESIAN_POINT('Origin',(0.,0.,-1.52655665885959E-15));
#28838=CARTESIAN_POINT('Ctrl Pts',(19.9039912380639,-0.634233661349708,
-3.99999999959214));
#28839=CARTESIAN_POINT('Ctrl Pts',(19.6812984735891,-0.667619141633003,
-3.37209215899804));
#28840=CARTESIAN_POINT('Ctrl Pts',(19.5117100620297,-0.663422606908006,
-2.72442970848406));
#28841=CARTESIAN_POINT('Ctrl Pts',(19.3267092023989,-0.612554982700328,
-1.65557386075461));
#28842=CARTESIAN_POINT('Ctrl Pts',(19.2773785775181,-0.58222314238337,-1.2405673563286));
#28843=CARTESIAN_POINT('Ctrl Pts',(19.2307632060366,-0.514706825018647,
-0.535449716754467));
#28844=CARTESIAN_POINT('Ctrl Pts',(19.2222233880155,-0.482364065768703,
-0.245612043957726));
#28845=CARTESIAN_POINT('Ctrl Pts',(19.2260726306592,-0.407801406965312,
0.339574192499094));
#28846=CARTESIAN_POINT('Ctrl Pts',(19.2389599748712,-0.365366877207829,
0.634888638796465));
#28847=CARTESIAN_POINT('Ctrl Pts',(19.2983007127951,-0.246059610097558,
1.3754102996081));
#28848=CARTESIAN_POINT('Ctrl Pts',(19.3587572800291,-0.16286451845944,1.81818944950897));
#28849=CARTESIAN_POINT('Ctrl Pts',(19.5571030357013,0.0653676913969697,
2.85334850598286));
#28850=CARTESIAN_POINT('Ctrl Pts',(19.7151513706548,0.22131331524976,3.43719532452554));
#28851=CARTESIAN_POINT('Ctrl Pts',(19.9099067854224,0.408327477794068,3.99999999896687));
#28852=CARTESIAN_POINT('Ctrl Pts',(19.7928724813984,2.19392763718696,3.99999999959177));
#28853=CARTESIAN_POINT('Ctrl Pts',(19.568248154273,2.20973759437162,3.37209584227646));
#28854=CARTESIAN_POINT('Ctrl Pts',(19.3995124415109,2.19224756440723,2.72443686861351));
#28855=CARTESIAN_POINT('Ctrl Pts',(19.2190722839147,2.12702120186606,1.65558298745174));
#28856=CARTESIAN_POINT('Ctrl Pts',(19.1722730539926,2.09291204321717,1.24057456625547));
#28857=CARTESIAN_POINT('Ctrl Pts',(19.1310981391587,2.02194588750386,0.535453312298503));
#28858=CARTESIAN_POINT('Ctrl Pts',(19.1251221278395,1.98903256836499,0.245613912296371));
#28859=CARTESIAN_POINT('Ctrl Pts',(19.1348096591669,1.91500135462234,-0.339575749237676));
#28860=CARTESIAN_POINT('Ctrl Pts',(19.1509867906522,1.87370858720253,-0.634891908540389));
#28861=CARTESIAN_POINT('Ctrl Pts',(19.2195059168057,1.75942465784691,-1.37541694661038));
#28862=CARTESIAN_POINT('Ctrl Pts',(19.2863040300092,1.68122936510914,-1.81819780767567));
#28863=CARTESIAN_POINT('Ctrl Pts',(19.5019456671156,1.46926376538599,-2.85335500863366));
#28864=CARTESIAN_POINT('Ctrl Pts',(19.6717414173474,1.32620060584982,-3.4371986138663));
#28865=CARTESIAN_POINT('Ctrl Pts',(19.8805681948062,1.15504449480289,-3.99999999896589));
#28866=CARTESIAN_POINT('Origin',(0.,0.,-1.52655665885959E-15));
#28867=CARTESIAN_POINT('Ctrl Pts',(18.9205613831265,6.21155990787279,-3.9999999995661));
#28868=CARTESIAN_POINT('Ctrl Pts',(18.722324530204,6.10368372785984,-3.37073547207111));
#28869=CARTESIAN_POINT('Ctrl Pts',(18.5614565921267,6.04926209466265,-2.72191645121725));
#28870=CARTESIAN_POINT('Ctrl Pts',(18.3705057444971,6.03370239487818,-1.65243153944395));
#28871=CARTESIAN_POINT('Ctrl Pts',(18.3139896008122,6.04528699644631,-1.23816612795984));
#28872=CARTESIAN_POINT('Ctrl Pts',(18.247326598681,6.09268509358316,-0.534322227019105));
#28873=CARTESIAN_POINT('Ctrl Pts',(18.2282992017452,6.12010477942619,-0.245020449800811));
#28874=CARTESIAN_POINT('Ctrl Pts',(18.2064590003793,6.19136501242513,0.339092780639954));
#28875=CARTESIAN_POINT('Ctrl Pts',(18.2040399950647,6.23557815835783,0.633871337552541));
#28876=CARTESIAN_POINT('Ctrl Pts',(18.2188652552579,6.36780451907379,1.37316141097512));
#28877=CARTESIAN_POINT('Ctrl Pts',(18.2470631112819,6.46654273341169,1.81522672164396));
#28878=CARTESIAN_POINT('Ctrl Pts',(18.3550861881491,6.74910453149341,2.85098957620195));
#28879=CARTESIAN_POINT('Ctrl Pts',(18.4502683407472,6.9503037778164,3.43595659389031));
#28880=CARTESIAN_POINT('Ctrl Pts',(18.5695436021889,7.1932725473206,3.99999999898836));
#28881=CARTESIAN_POINT('Ctrl Pts',(17.8488387937264,8.83119885730777,3.99999999956597));
#28882=CARTESIAN_POINT('Ctrl Pts',(17.6318350798684,8.76919556450322,3.37073606763092));
#28883=CARTESIAN_POINT('Ctrl Pts',(17.4789514598686,8.69525791381623,2.72191758661121));
#28884=CARTESIAN_POINT('Ctrl Pts',(17.3318496791326,8.57251654264658,1.65243297598597));
#28885=CARTESIAN_POINT('Ctrl Pts',(17.299659216222,8.52464104899507,1.23816724736839));
#28886=CARTESIAN_POINT('Ctrl Pts',(17.2853335211168,8.44410950932137,0.534322772007183));
#28887=CARTESIAN_POINT('Ctrl Pts',(17.290980930954,8.41121588890205,0.245020734146467));
#28888=CARTESIAN_POINT('Ctrl Pts',(17.3253503814398,8.34508143893279,-0.339093015441015));
#28889=CARTESIAN_POINT('Ctrl Pts',(17.3546144576286,8.31185087091933,-0.633871831961161));
#28890=CARTESIAN_POINT('Ctrl Pts',(17.4578673627717,8.22793150916394,-1.37316245063156));
#28891=CARTESIAN_POINT('Ctrl Pts',(17.5471861070962,8.17727058957665,-1.81522805453279));
#28892=CARTESIAN_POINT('Ctrl Pts',(17.8222838092634,8.05144781005231,-2.85099062303143));
#28893=CARTESIAN_POINT('Ctrl Pts',(18.0311947505155,7.97465658921816,-3.43595713130924));
#28894=CARTESIAN_POINT('Ctrl Pts',(18.2865666872494,7.88496026156532,-3.9999999989921));
#28895=CARTESIAN_POINT('Origin',(0.,0.,-1.52655665885959E-15));
#28896=CARTESIAN_POINT('Ctrl Pts',(15.6550192929788,12.3081879445576,-3.9999999995905));
#28897=CARTESIAN_POINT('Ctrl Pts',(15.5058897133034,12.1394742461233,-3.37210842589158));
#28898=CARTESIAN_POINT('Ctrl Pts',(15.3732799472876,12.0336838212003,-2.72446133399751));
#28899=CARTESIAN_POINT('Ctrl Pts',(15.1988603399475,11.9537342169491,-1.65561417383655));
#28900=CARTESIAN_POINT('Ctrl Pts',(15.1415712421423,11.9452603559541,-1.24059920501932));
#28901=CARTESIAN_POINT('Ctrl Pts',(15.0624597690905,11.9670172783189,-0.535465601249687));
#28902=CARTESIAN_POINT('Ctrl Pts',(15.0351273125387,11.9863044050078,-0.245620297792711));
#28903=CARTESIAN_POINT('Ctrl Pts',(14.9901468786545,12.0458983790383,0.339581070069207));
#28904=CARTESIAN_POINT('Ctrl Pts',(14.9727426549031,12.086689935466,0.634903084117227));
#28905=CARTESIAN_POINT('Ctrl Pts',(14.9415120504097,12.2162307198855,1.3754396605205));
#28906=CARTESIAN_POINT('Ctrl Pts',(14.9343491772112,12.318824241377,1.81822636537783));
#28907=CARTESIAN_POINT('Ctrl Pts',(14.9395904852342,12.6211525532081,2.85337722509545));
#28908=CARTESIAN_POINT('Ctrl Pts',(14.9604246816766,12.8421986625435,3.43720985077337));
#28909=CARTESIAN_POINT('Ctrl Pts',(14.9894054753209,13.110638543934,3.99999999896253));
#28910=CARTESIAN_POINT('Ctrl Pts',(13.7519742133981,14.4032747934551,3.99999999956581));
#28911=CARTESIAN_POINT('Ctrl Pts',(13.5692640754011,14.2707912447614,3.3707368720194));
#28912=CARTESIAN_POINT('Ctrl Pts',(13.4508888400675,14.1490232672934,2.72191911983545));
#28913=CARTESIAN_POINT('Ctrl Pts',(13.3546383747822,13.9833721569018,1.65243491602215));
#28914=CARTESIAN_POINT('Ctrl Pts',(13.3407635890821,13.9273739927272,1.23816875923414));
#28915=CARTESIAN_POINT('Ctrl Pts',(13.3548452424663,13.8467992629272,0.534323508198989));
#28916=CARTESIAN_POINT('Ctrl Pts',(13.3714023670614,13.8178208485285,0.245021118273289));
#28917=CARTESIAN_POINT('Ctrl Pts',(13.426318460135,13.7674297777744,-0.339093332539267));
#28918=CARTESIAN_POINT('Ctrl Pts',(13.4651832658699,13.7462121517018,-0.633872499721225));
#28919=CARTESIAN_POINT('Ctrl Pts',(13.5909115042562,13.7026683504298,-1.37316385456509));
#28920=CARTESIAN_POINT('Ctrl Pts',(13.6921708194976,13.6856115280933,-1.81522985428248));
#28921=CARTESIAN_POINT('Ctrl Pts',(13.9937119595891,13.6614659735749,-2.850992036466));
#28922=CARTESIAN_POINT('Ctrl Pts',(14.2162878528165,13.6607577213958,-3.43595785705526));
#28923=CARTESIAN_POINT('Ctrl Pts',(14.4869365444979,13.6638131240649,-3.99999999899171));
#28924=CARTESIAN_POINT('Origin',(0.,0.,-1.52655665885959E-15));
#28925=CARTESIAN_POINT('Ctrl Pts',(10.5012771497263,16.9202333839218,-3.99999999956587));
#28926=CARTESIAN_POINT('Ctrl Pts',(10.4187604568623,16.7101716410052,-3.37073654282549));
#28927=CARTESIAN_POINT('Ctrl Pts',(10.3305099036439,16.5650785907123,-2.72191849209908));
#28928=CARTESIAN_POINT('Ctrl Pts',(10.1942344309634,16.4304182339908,-1.652434121808));
#28929=CARTESIAN_POINT('Ctrl Pts',(10.143493957598,16.4029645969779,-1.23816814035234));
#28930=CARTESIAN_POINT('Ctrl Pts',(10.0619600213757,16.396423433878,-0.534323206889723));
#28931=CARTESIAN_POINT('Ctrl Pts',(10.0297590861831,16.4051975588644,-0.245020961051929));
#28932=CARTESIAN_POINT('Ctrl Pts',(9.96722322846384,16.4457475107094,0.339093202773109));
#28933=CARTESIAN_POINT('Ctrl Pts',(9.93695047231674,16.4780618942998,0.633872226446596));
#28934=CARTESIAN_POINT('Ctrl Pts',(9.86331380879727,16.5888828385059,1.37316327986747));
#28935=CARTESIAN_POINT('Ctrl Pts',(9.82144696476986,16.6826460743351,1.81522911749121));
#28936=CARTESIAN_POINT('Ctrl Pts',(9.72257053472987,16.968536856076,2.85099145780179));
#28937=CARTESIAN_POINT('Ctrl Pts',(9.66615620033031,17.1838459623933,3.43595756003759));
#28938=CARTESIAN_POINT('Ctrl Pts',(9.60134920800818,17.4466390149938,3.99999999898783));
#28939=CARTESIAN_POINT('Ctrl Pts',(7.9964185706515,18.2381032342919,3.99999999956596));
#28940=CARTESIAN_POINT('Ctrl Pts',(7.87003904657797,18.0511186748182,3.37073613064603));
#28941=CARTESIAN_POINT('Ctrl Pts',(7.80044962132109,17.8962074545261,2.72191770646729));
#28942=CARTESIAN_POINT('Ctrl Pts',(7.76665975518057,17.7076268932318,1.65243312773053));
#28943=CARTESIAN_POINT('Ctrl Pts',(7.77277420554943,17.6502604963407,1.23816736568045));
#28944=CARTESIAN_POINT('Ctrl Pts',(7.81356476628747,17.5793613666168,0.534322829701268));
#28945=CARTESIAN_POINT('Ctrl Pts',(7.83903454727416,17.5577934732534,0.245020764278644));
#28946=CARTESIAN_POINT('Ctrl Pts',(7.90787348487,17.5292237994333,-0.339093040194778));
#28947=CARTESIAN_POINT('Ctrl Pts',(7.95165126879749,17.5225782935396,-0.633871884162621));
#28948=CARTESIAN_POINT('Ctrl Pts',(8.08468991779793,17.5246620267298,-1.37316256028439));
#28949=CARTESIAN_POINT('Ctrl Pts',(8.18567626219244,17.5432664999848,-1.81522819503422));
#28950=CARTESIAN_POINT('Ctrl Pts',(8.47729064067002,17.6237100684105,-2.85099073335041));
#28951=CARTESIAN_POINT('Ctrl Pts',(8.68668612406968,17.699169946924,-3.43595718806009));
#28952=CARTESIAN_POINT('Ctrl Pts',(8.93996803620397,17.7946084824949,-3.99999999898803));
#28953=CARTESIAN_POINT('Origin',(0.,0.,-1.52655665885959E-15));
#28954=CARTESIAN_POINT('Ctrl Pts',(4.08088993973065,19.4914713872994,-3.99999999959139));
#28955=CARTESIAN_POINT('Ctrl Pts',(4.07509761685323,19.2663672599298,-3.37209958171796));
#28956=CARTESIAN_POINT('Ctrl Pts',(4.0415148849561,19.1000854490341,-2.72444413839122));
#28957=CARTESIAN_POINT('Ctrl Pts',(3.95929377670302,18.9267270968025,-1.65559225411347));
#28958=CARTESIAN_POINT('Ctrl Pts',(3.92085570624596,18.8834120879112,-1.24058188703958));
#28959=CARTESIAN_POINT('Ctrl Pts',(3.84626919931116,18.8492280764774,-0.535456963378757));
#28960=CARTESIAN_POINT('Ctrl Pts',(3.81293438334342,18.8464340988294,-0.245615809484055));
#28961=CARTESIAN_POINT('Ctrl Pts',(3.74017208754659,18.8631726846676,0.339577330001301));
#28962=CARTESIAN_POINT('Ctrl Pts',(3.70061976633521,18.8832332349204,0.634895228749923));
#28963=CARTESIAN_POINT('Ctrl Pts',(3.59342903056888,18.9623911496099,1.37542369557564));
#28964=CARTESIAN_POINT('Ctrl Pts',(3.52199606603956,19.0363769342805,1.81820629356909));
#28965=CARTESIAN_POINT('Ctrl Pts',(3.33167571846254,19.2713421302727,2.85336161046155));
#28966=CARTESIAN_POINT('Ctrl Pts',(3.20554674527637,19.4540672990726,3.4372019532105));
#28967=CARTESIAN_POINT('Ctrl Pts',(3.05519487086468,19.6783359010447,3.99999999896489));
#28968=CARTESIAN_POINT('Ctrl Pts',(1.27637679201105,19.8731472551927,3.99999999956669));
#28969=CARTESIAN_POINT('Ctrl Pts',(1.22157081634607,19.6542137025969,3.37073263858838));
#28970=CARTESIAN_POINT('Ctrl Pts',(1.20916011335533,19.4848433224629,2.72191105135517));
#28971=CARTESIAN_POINT('Ctrl Pts',(1.24190597611347,19.2960794163503,1.65242470708135));
#28972=CARTESIAN_POINT('Ctrl Pts',(1.26727187692808,19.2442644111506,1.23816080392278));
#28973=CARTESIAN_POINT('Ctrl Pts',(1.32985096795065,19.1915927623126,0.534319634829282));
#28974=CARTESIAN_POINT('Ctrl Pts',(1.36116119974462,19.180036875869,0.245019097176994));
#28975=CARTESIAN_POINT('Ctrl Pts',(1.4356196770548,19.176734501299,-0.339091664301467));
#28976=CARTESIAN_POINT('Ctrl Pts',(1.47903005465291,19.1854625584862,-0.633868986560752));
#28977=CARTESIAN_POINT('Ctrl Pts',(1.60333245432168,19.2329220526458,-1.37315646709438));
#28978=CARTESIAN_POINT('Ctrl Pts',(1.69186532339448,19.2849434365886,-1.81522038318764));
#28979=CARTESIAN_POINT('Ctrl Pts',(1.93838073553048,19.4602730828479,-2.85098459800567));
#28980=CARTESIAN_POINT('Ctrl Pts',(2.10934078988013,19.6028000727414,-3.43595403740795));
#28981=CARTESIAN_POINT('Ctrl Pts',(2.31470740137874,19.7791114355451,-3.99999999899377));
#28982=CARTESIAN_POINT('Origin',(0.,0.,-1.52655665885959E-15));
#28983=CARTESIAN_POINT('Ctrl Pts',(-2.83169367195905,19.7117383934115,-3.99999999959142));
#28984=CARTESIAN_POINT('Ctrl Pts',(-2.76014648784994,19.498228538721,-3.37209935132288));
#28985=CARTESIAN_POINT('Ctrl Pts',(-2.73483215303947,19.3304887480367,-2.72444369047209));
#28986=CARTESIAN_POINT('Ctrl Pts',(-2.7528026499327,19.1394639546639,-1.65559168315368));
#28987=CARTESIAN_POINT('Ctrl Pts',(-2.77410799980422,19.0856146013948,-1.24058143596684));
#28988=CARTESIAN_POINT('Ctrl Pts',(-2.83250474306813,19.0279820902425,-0.535456738414391));
#28989=CARTESIAN_POINT('Ctrl Pts',(-2.86287361435436,19.0139554414172,-0.245615692594552));
#28990=CARTESIAN_POINT('Ctrl Pts',(-2.93697271462192,19.0047984005021,0.339577232578708));
#28991=CARTESIAN_POINT('Ctrl Pts',(-2.98100083826584,19.0101214553002,0.634895024141513));
#28992=CARTESIAN_POINT('Ctrl Pts',(-3.10880075779996,19.0478441421203,1.37542327969907));
#28993=CARTESIAN_POINT('Ctrl Pts',(-3.201230406372,19.0929364953574,1.81820577067646));
#28994=CARTESIAN_POINT('Ctrl Pts',(-3.46043591760429,19.2486381220978,2.85336120366925));
#28995=CARTESIAN_POINT('Ctrl Pts',(-3.64145416795512,19.3772049873777,3.4372017474516));
#28996=CARTESIAN_POINT('Ctrl Pts',(-3.85944318717446,19.5365252237514,3.99999999896495));
#28997=CARTESIAN_POINT('Ctrl Pts',(-5.59761479218164,19.1111964089144,3.99999999956627));
#28998=CARTESIAN_POINT('Ctrl Pts',(-5.57423581313916,18.8867221808592,3.37073466341711));
#28999=CARTESIAN_POINT('Ctrl Pts',(-5.52796963846162,18.7233217839671,2.72191491022201));
#29000=CARTESIAN_POINT('Ctrl Pts',(-5.43263718388652,18.5571411928451,1.65242958953604));
#29001=CARTESIAN_POINT('Ctrl Pts',(-5.39107901246423,18.5171264390623,1.23816460840836));
#29002=CARTESIAN_POINT('Ctrl Pts',(-5.31425879573908,18.4890343760598,0.534321487023973));
#29003=CARTESIAN_POINT('Ctrl Pts',(-5.28088432901033,18.4888840935175,0.245020063602722));
#29004=CARTESIAN_POINT('Ctrl Pts',(-5.20978656133472,18.5112472302162,-0.339092462175414));
#29005=CARTESIAN_POINT('Ctrl Pts',(-5.17197924185572,18.5342962315364,-0.633870666713147));
#29006=CARTESIAN_POINT('Ctrl Pts',(-5.07140519543395,18.6214078210159,-1.37316000039744));
#29007=CARTESIAN_POINT('Ctrl Pts',(-5.00600388404419,18.7005722398839,-1.81522491330522));
#29008=CARTESIAN_POINT('Ctrl Pts',(-4.83432201949194,18.9496415943053,-2.85098815599153));
#29009=CARTESIAN_POINT('Ctrl Pts',(-4.72241993176988,19.142044415309,-3.43595586451284));
#29010=CARTESIAN_POINT('Ctrl Pts',(-4.58974103596834,19.377961625425,-3.99999999899278));
#29011=CARTESIAN_POINT('Origin',(0.,0.,-1.52655665885959E-15));
#29012=CARTESIAN_POINT('Ctrl Pts',(-9.40271337324756,17.5544894759802,-3.99999999956588));
#29013=CARTESIAN_POINT('Ctrl Pts',(-9.26205290644085,17.3779970458197,-3.37073651667098));
#29014=CARTESIAN_POINT('Ctrl Pts',(-9.18052390874618,17.2290232989812,-2.72191844225021));
#29015=CARTESIAN_POINT('Ctrl Pts',(-9.13204235463609,17.0436751051816,-1.65243405873456));
#29016=CARTESIAN_POINT('Ctrl Pts',(-9.13363704400476,16.9860057520412,-1.23816809120242));
#29017=CARTESIAN_POINT('Ctrl Pts',(-9.16873919747736,16.9121247155117,-0.53432318297038));
#29018=CARTESIAN_POINT('Ctrl Pts',(-9.19243827931884,16.8886249515421,-0.245020948588286));
#29019=CARTESIAN_POINT('Ctrl Pts',(-9.25882349418853,16.8547422874071,0.339093192415483));
#29020=CARTESIAN_POINT('Ctrl Pts',(-9.30194494783863,16.8446825032542,0.633872204674519));
#29021=CARTESIAN_POINT('Ctrl Pts',(-9.43473702863313,16.8363217519894,1.37316323412291));
#29022=CARTESIAN_POINT('Ctrl Pts',(-9.53687179234548,16.8469456166805,1.81522905885359));
#29023=CARTESIAN_POINT('Ctrl Pts',(-9.83389869109708,16.9042615007379,2.85099141175238));
#29024=CARTESIAN_POINT('Ctrl Pts',(-10.0485690253374,16.9630598055312,3.43595753639452));
#29025=CARTESIAN_POINT('Ctrl Pts',(-10.3085579933226,17.038331832428,3.99999999898785));
#29026=CARTESIAN_POINT('Ctrl Pts',(-11.7964514248447,16.0441532441892,3.99999999956582));
#29027=CARTESIAN_POINT('Ctrl Pts',(-11.6977078731037,15.841213326112,3.37073678762359));
#29028=CARTESIAN_POINT('Ctrl Pts',(-11.5983454761381,15.7034916683205,2.72191895896554));
#29029=CARTESIAN_POINT('Ctrl Pts',(-11.451924714039,15.5799384566389,1.65243471246575));
#29030=CARTESIAN_POINT('Ctrl Pts',(-11.3991866319024,15.5565504862445,1.23816860059909));
#29031=CARTESIAN_POINT('Ctrl Pts',(-11.3173907762762,15.5564265561475,0.534323430942822));
#29032=CARTESIAN_POINT('Ctrl Pts',(-11.2859775000167,15.5677000913793,0.245021077953252));
#29033=CARTESIAN_POINT('Ctrl Pts',(-11.2268159107147,15.6130315628994,-0.339093299295225));
#29034=CARTESIAN_POINT('Ctrl Pts',(-11.1991718272373,15.6476215182721,-0.633872429691263));
#29035=CARTESIAN_POINT('Ctrl Pts',(-11.1344570739679,15.7638783461568,-1.37316370731725));
#29036=CARTESIAN_POINT('Ctrl Pts',(-11.1000758830394,15.8606374078146,-1.81522966552197));
#29037=CARTESIAN_POINT('Ctrl Pts',(-11.0239350595913,16.1534046315372,-2.85099188822321));
#29038=CARTESIAN_POINT('Ctrl Pts',(-10.9845876486582,16.3724761407069,-3.43595778093828));
#29039=CARTESIAN_POINT('Ctrl Pts',(-10.9405989703516,16.6395436747412,-3.99999999899175));
#29040=CARTESIAN_POINT('Origin',(0.,0.,-1.52655665885959E-15));
#29041=CARTESIAN_POINT('Ctrl Pts',(-14.8396644849569,13.2798899662611,-3.9999999995905));
#29042=CARTESIAN_POINT('Ctrl Pts',(-14.6476178493579,13.1623228272291,-3.37210843277778));
#29043=CARTESIAN_POINT('Ctrl Pts',(-14.5204071762167,13.0500980157328,-2.72446134739535));
#29044=CARTESIAN_POINT('Ctrl Pts',(-14.4113845387682,12.8922113357405,-1.65561419092038));
#29045=CARTESIAN_POINT('Ctrl Pts',(-14.3930912670057,12.8372640574723,-1.24059921852505));
#29046=CARTESIAN_POINT('Ctrl Pts',(-14.4007800895362,12.7555764141237,-0.535465608026784));
#29047=CARTESIAN_POINT('Ctrl Pts',(-14.4150279702577,12.7253100241341,-0.245620301364524));
#29048=CARTESIAN_POINT('Ctrl Pts',(-14.4659058080358,12.6706645585323,0.339581072840045));
#29049=CARTESIAN_POINT('Ctrl Pts',(-14.503055437724,12.6464413644899,0.634903090053654));
#29050=CARTESIAN_POINT('Ctrl Pts',(-14.6252050701333,12.5931907021228,1.37543967266357));
#29051=CARTESIAN_POINT('Ctrl Pts',(-14.7249961464028,12.5683214715082,1.81822638064967));
#29052=CARTESIAN_POINT('Ctrl Pts',(-15.0236415549683,12.5209843938598,2.85337723697866));
#29053=CARTESIAN_POINT('Ctrl Pts',(-15.2449472948761,12.5031178193119,3.43720985678689));
#29054=CARTESIAN_POINT('Ctrl Pts',(-15.5143414301618,12.4850442338677,3.99999999896252));
#29055=CARTESIAN_POINT('Ctrl Pts',(-16.5724619473705,11.0419484034613,3.99999999956582));
#29056=CARTESIAN_POINT('Ctrl Pts',(-16.4102638255241,10.8850195504957,3.37073680996054));
#29057=CARTESIAN_POINT('Ctrl Pts',(-16.2697901329922,10.7895874722902,2.72191900128754));
#29058=CARTESIAN_POINT('Ctrl Pts',(-16.0899419309864,10.7235642814288,1.65243476610461));
#29059=CARTESIAN_POINT('Ctrl Pts',(-16.0323851836635,10.7196242645906,1.23816864245814));
#29060=CARTESIAN_POINT('Ctrl Pts',(-15.9554798306858,10.7474836393633,0.534323451403115));
#29061=CARTESIAN_POINT('Ctrl Pts',(-15.9298167816178,10.7688212711311,0.245021088648856));
#29062=CARTESIAN_POINT('Ctrl Pts',(-15.8897273477402,10.8316533775811,-0.339093308039497));
#29063=CARTESIAN_POINT('Ctrl Pts',(-15.875580867942,10.8736121380598,-0.633872448158881));
#29064=CARTESIAN_POINT('Ctrl Pts',(-15.8545310703183,11.0049915738749,-1.37316374602659));
#29065=CARTESIAN_POINT('Ctrl Pts',(-15.855316869219,11.1076744121152,-1.81522971507324));
#29066=CARTESIAN_POINT('Ctrl Pts',(-15.8839001931801,11.4088273039884,-2.85099192711218));
#29067=CARTESIAN_POINT('Ctrl Pts',(-15.9218525929265,11.6281447821453,-3.43595780101046));
#29068=CARTESIAN_POINT('Ctrl Pts',(-15.9718592317868,11.8941511766754,-3.9999999989877));
#29069=CARTESIAN_POINT('Origin',(0.,0.,-1.52655665885959E-15));
#29070=CARTESIAN_POINT('Ctrl Pts',(-18.4867130622875,7.40355047897599,-3.9999999995909));
#29071=CARTESIAN_POINT('Ctrl Pts',(-18.2660364568889,7.35875728365076,-3.37210452431144));
#29072=CARTESIAN_POINT('Ctrl Pts',(-18.1081135146886,7.29680957511262,-2.72445374790304));
#29073=CARTESIAN_POINT('Ctrl Pts',(-17.9516658028163,7.18573329947562,-1.65560450349881));
#29074=CARTESIAN_POINT('Ctrl Pts',(-17.9156830597558,7.14035694592513,-1.24059156465032));
#29075=CARTESIAN_POINT('Ctrl Pts',(-17.8949697327359,7.06096666507544,-0.535461790250346));
#29076=CARTESIAN_POINT('Ctrl Pts',(-17.8980066839884,7.02765276946775,-0.245618317617947));
#29077=CARTESIAN_POINT('Ctrl Pts',(-17.927126208346,6.95890199759269,0.339579419829294));
#29078=CARTESIAN_POINT('Ctrl Pts',(-17.953750427197,6.92343386222213,0.634899618176173));
#29079=CARTESIAN_POINT('Ctrl Pts',(-18.0503200716021,6.831617083009,1.37543261696681));
#29080=CARTESIAN_POINT('Ctrl Pts',(-18.1355867099821,6.77411698191067,1.81821751025154));
#29081=CARTESIAN_POINT('Ctrl Pts',(-18.4000312193516,6.62749077357112,2.85337033648387));
#29082=CARTESIAN_POINT('Ctrl Pts',(-18.601881004032,6.53500943299842,3.4372063667673));
#29083=CARTESIAN_POINT('Ctrl Pts',(-18.848848760419,6.42588670458299,3.99999999896357));
#29084=CARTESIAN_POINT('Ctrl Pts',(-19.3495889825578,4.70792159533567,3.99999999956624));
#29085=CARTESIAN_POINT('Ctrl Pts',(-19.1434991430015,4.61593129472241,3.3707347727776));
#29086=CARTESIAN_POINT('Ctrl Pts',(-18.9788571709899,4.5742988058017,2.72191511865313));
#29087=CARTESIAN_POINT('Ctrl Pts',(-18.7872743073193,4.57376884638241,1.65242985326193));
#29088=CARTESIAN_POINT('Ctrl Pts',(-18.7318414111458,4.58975190711804,1.23816481391789));
#29089=CARTESIAN_POINT('Ctrl Pts',(-18.6691028433861,4.64223414506052,0.534321587091021));
#29090=CARTESIAN_POINT('Ctrl Pts',(-18.6522854566278,4.6710621449107,0.245020115824628));
#29091=CARTESIAN_POINT('Ctrl Pts',(-18.6361036142338,4.74381619739426,-0.339092505248901));
#29092=CARTESIAN_POINT('Ctrl Pts',(-18.6371609770871,4.78808280322809,-0.633870757439877));
#29093=CARTESIAN_POINT('Ctrl Pts',(-18.6623148159461,4.91873829075295,-1.37316019119144));
#29094=CARTESIAN_POINT('Ctrl Pts',(-18.6981725716345,5.0149597044225,-1.81522515791414));
#29095=CARTESIAN_POINT('Ctrl Pts',(-18.8280320498957,5.28817521451328,-2.85098834810475));
#29096=CARTESIAN_POINT('Ctrl Pts',(-18.9387067316056,5.48128662831983,-3.43595596316373));
#29097=CARTESIAN_POINT('Ctrl Pts',(-19.0766775587209,5.71414848024506,-3.99999999899274));
#29098=CARTESIAN_POINT('Origin',(0.,0.,-1.52655665885959E-15));
#29099=CARTESIAN_POINT('Ctrl Pts',(-19.9039912380639,0.634233661349713,
-3.99999999959214));
#29100=CARTESIAN_POINT('Ctrl Pts',(-19.6812984735855,0.667619141633553,
-3.3720921589878));
#29101=CARTESIAN_POINT('Ctrl Pts',(-19.5117100620242,0.663422606907901,
-2.72442970846294));
#29102=CARTESIAN_POINT('Ctrl Pts',(-19.3267092023953,0.61255498269846,-1.65557386072678));
#29103=CARTESIAN_POINT('Ctrl Pts',(-19.2773785775159,0.582223142381439,
-1.24056735630538));
#29104=CARTESIAN_POINT('Ctrl Pts',(-19.2307632060359,0.514706825016789,
-0.535449716736964));
#29105=CARTESIAN_POINT('Ctrl Pts',(-19.2222233880153,0.48236406576677,-0.245612043941133));
#29106=CARTESIAN_POINT('Ctrl Pts',(-19.2260726306597,0.407801406963018,
0.339574192515873));
#29107=CARTESIAN_POINT('Ctrl Pts',(-19.2389599748721,0.365366877205189,
0.634888638814313));
#29108=CARTESIAN_POINT('Ctrl Pts',(-19.2983007127978,0.246059610093303,
1.3754102996325));
#29109=CARTESIAN_POINT('Ctrl Pts',(-19.3587572800335,0.162864518453664,
1.81818944953874));
#29110=CARTESIAN_POINT('Ctrl Pts',(-19.5571030357074,-0.0653676914030244,
2.85334850600551));
#29111=CARTESIAN_POINT('Ctrl Pts',(-19.7151513706586,-0.221313315253387,
3.43719532453647));
#29112=CARTESIAN_POINT('Ctrl Pts',(-19.9099067854224,-0.408327477794065,
3.99999999896687));
#29113=CARTESIAN_POINT('Ctrl Pts',(-19.7928699973623,-2.19395004712364,
3.99999999956673));
#29114=CARTESIAN_POINT('Ctrl Pts',(-19.5677455202026,-2.20990600018682,
3.37073247625875));
#29115=CARTESIAN_POINT('Ctrl Pts',(-19.3987931331181,-2.19271733132894,
2.7219107420094));
#29116=CARTESIAN_POINT('Ctrl Pts',(-19.2185832617589,-2.12769046720652,
1.6524243156881));
#29117=CARTESIAN_POINT('Ctrl Pts',(-19.1719602065399,-2.09371236649188,
1.23816049895436));
#29118=CARTESIAN_POINT('Ctrl Pts',(-19.1309555250841,-2.02293768065745,
0.534319486362197));
#29119=CARTESIAN_POINT('Ctrl Pts',(-19.1250121674529,-1.99009647260577,
0.245019019702941));
#29120=CARTESIAN_POINT('Ctrl Pts',(-19.1346895408446,-1.9161957526751,-0.339091600369012));
#29121=CARTESIAN_POINT('Ctrl Pts',(-19.1508231264452,-1.87496049495226,
-0.633868851915709));
#29122=CARTESIAN_POINT('Ctrl Pts',(-19.2191464649171,-1.76078779531645,
-1.37315618389887));
#29123=CARTESIAN_POINT('Ctrl Pts',(-19.2857510759732,-1.6826333610479,-1.8152200200743));
#29124=CARTESIAN_POINT('Ctrl Pts',(-19.5012240036822,-1.47030870183375,
-2.85098431280495));
#29125=CARTESIAN_POINT('Ctrl Pts',(-19.6712726215212,-1.32669540341637,
-3.43595389094347));
#29126=CARTESIAN_POINT('Ctrl Pts',(-19.8805670113664,-1.15506486410126,
-3.99999999899386));
#29127=CARTESIAN_POINT('Origin',(0.,0.,-1.52655665885959E-15));
#29128=CARTESIAN_POINT('Ctrl Pts',(-18.9205613831265,-6.2115599078728,-3.9999999995661));
#29129=CARTESIAN_POINT('Ctrl Pts',(-18.7223245302125,-6.10368372786451,
-3.37073547209815));
#29130=CARTESIAN_POINT('Ctrl Pts',(-18.5614565921404,-6.04926209466741,
-2.72191645127299));
#29131=CARTESIAN_POINT('Ctrl Pts',(-18.3705057445077,-6.03370239487686,
-1.65243153951694));
#29132=CARTESIAN_POINT('Ctrl Pts',(-18.3139896008193,-6.04528699644354,
-1.23816612802062));
#29133=CARTESIAN_POINT('Ctrl Pts',(-18.2473265986844,-6.09268509357922,
-0.534322227065162));
#29134=CARTESIAN_POINT('Ctrl Pts',(-18.2282992017476,-6.12010477942166,
-0.245020449844545));
#29135=CARTESIAN_POINT('Ctrl Pts',(-18.2064590003801,-6.19136501241902,
0.339092780595737));
#29136=CARTESIAN_POINT('Ctrl Pts',(-18.2040399950647,-6.23557815835044,
0.63387133750551));
#29137=CARTESIAN_POINT('Ctrl Pts',(-18.2188652552551,-6.3678045190608,1.37316141091046));
#29138=CARTESIAN_POINT('Ctrl Pts',(-18.2470631112762,-6.46654273339332,
1.81522672156502));
#29139=CARTESIAN_POINT('Ctrl Pts',(-18.3550861881394,-6.74910453147274,
2.85098957614178));
#29140=CARTESIAN_POINT('Ctrl Pts',(-18.4502683407411,-6.95030377780392,
3.43595659386126));
#29141=CARTESIAN_POINT('Ctrl Pts',(-18.5695436021889,-7.19327254732061,
3.99999999898836));
#29142=CARTESIAN_POINT('Ctrl Pts',(-17.8488387937264,-8.83119885730778,
3.99999999956597));
#29143=CARTESIAN_POINT('Ctrl Pts',(-17.6318350798565,-8.76919556449981,
3.37073606759622));
#29144=CARTESIAN_POINT('Ctrl Pts',(-17.4789514598517,-8.69525791380816,
2.72191758653968));
#29145=CARTESIAN_POINT('Ctrl Pts',(-17.3318496791241,-8.5725165426358,1.65243297589238));
#29146=CARTESIAN_POINT('Ctrl Pts',(-17.299659216218,-8.52464104898616,1.23816724729049));
#29147=CARTESIAN_POINT('Ctrl Pts',(-17.2853335211172,-8.44410950931466,
0.534322771948021));
#29148=CARTESIAN_POINT('Ctrl Pts',(-17.2909809309559,-8.41121588889571,
0.245020734090218));
#29149=CARTESIAN_POINT('Ctrl Pts',(-17.3253503814445,-8.34508143892643,
-0.339093015497721));
#29150=CARTESIAN_POINT('Ctrl Pts',(-17.3546144576353,-8.31185087091257,
-0.633871832021433));
#29151=CARTESIAN_POINT('Ctrl Pts',(-17.4578673627859,-8.22793150915451,
-1.37316245071452));
#29152=CARTESIAN_POINT('Ctrl Pts',(-17.547186107118,-8.17727058956495,-1.81522805463407));
#29153=CARTESIAN_POINT('Ctrl Pts',(-17.8222838092909,-8.05144781004217,
-2.85099062310861));
#29154=CARTESIAN_POINT('Ctrl Pts',(-18.0311947505324,-7.97465658921225,
-3.43595713134647));
#29155=CARTESIAN_POINT('Ctrl Pts',(-18.2865666872494,-7.88496026156533,
-3.9999999989921));
#29156=CARTESIAN_POINT('Origin',(0.,0.,-1.52655665885959E-15));
#29157=CARTESIAN_POINT('Ctrl Pts',(-15.6550192929788,-12.3081879445576,
-3.9999999995905));
#29158=CARTESIAN_POINT('Ctrl Pts',(-15.5058897133018,-12.1394742461215,
-3.37210842588511));
#29159=CARTESIAN_POINT('Ctrl Pts',(-15.3732799472849,-12.0336838211982,
-2.72446133398417));
#29160=CARTESIAN_POINT('Ctrl Pts',(-15.1988603399449,-11.9537342169486,
-1.65561417381906));
#29161=CARTESIAN_POINT('Ctrl Pts',(-15.1415712421405,-11.9452603559542,
-1.24059920500475));
#29162=CARTESIAN_POINT('Ctrl Pts',(-15.0624597690894,-11.9670172783195,
-0.535465601238678));
#29163=CARTESIAN_POINT('Ctrl Pts',(-15.0351273125377,-11.9863044050087,
-0.245620297782277));
#29164=CARTESIAN_POINT('Ctrl Pts',(-14.9901468786537,-12.0458983790397,
0.33958107008003));
#29165=CARTESIAN_POINT('Ctrl Pts',(-14.9727426549024,-12.0866899354678,
0.634903084128853));
#29166=CARTESIAN_POINT('Ctrl Pts',(-14.9415120504093,-12.2162307198888,
1.37543966053627));
#29167=CARTESIAN_POINT('Ctrl Pts',(-14.934349177211,-12.3188242413817,1.81822636539706));
#29168=CARTESIAN_POINT('Ctrl Pts',(-14.9395904852347,-12.6211525532137,
2.85337722511011));
#29169=CARTESIAN_POINT('Ctrl Pts',(-14.960424681677,-12.8421986625469,3.43720985078044));
#29170=CARTESIAN_POINT('Ctrl Pts',(-14.9894054753209,-13.110638543934,3.99999999896253));
#29171=CARTESIAN_POINT('Ctrl Pts',(-13.751974213328,-14.403274793522,3.9999999995658));
#29172=CARTESIAN_POINT('Ctrl Pts',(-13.5692640748007,-14.2707912447243,
3.37073687076865));
#29173=CARTESIAN_POINT('Ctrl Pts',(-13.4508888393199,-14.1490232670549,
2.72191911720231));
#29174=CARTESIAN_POINT('Ctrl Pts',(-13.3546383743594,-13.9833721567228,
1.6524349127806));
#29175=CARTESIAN_POINT('Ctrl Pts',(-13.3407635887915,-13.9273739926909,
1.23816875677089));
#29176=CARTESIAN_POINT('Ctrl Pts',(-13.3548452422531,-13.8467992630841,
0.534323507098637));
#29177=CARTESIAN_POINT('Ctrl Pts',(-13.3714023668365,-13.81782084875,0.245021117745642));
#29178=CARTESIAN_POINT('Ctrl Pts',(-13.4263184597996,-13.7674297780966,
-0.339093331911454));
#29179=CARTESIAN_POINT('Ctrl Pts',(-13.4651832654341,-13.746212152059,-0.633872498514063));
#29180=CARTESIAN_POINT('Ctrl Pts',(-13.5909115034643,-13.7026683508362,
-1.37316385195566));
#29181=CARTESIAN_POINT('Ctrl Pts',(-13.6921708184002,-13.6856115284966,
-1.81522985087203));
#29182=CARTESIAN_POINT('Ctrl Pts',(-13.9937119583052,-13.6614659738392,
-2.85099203376423));
#29183=CARTESIAN_POINT('Ctrl Pts',(-14.2162878519877,-13.6607577216152,
-3.43595785577492));
#29184=CARTESIAN_POINT('Ctrl Pts',(-14.4869365444277,-13.6638131241373,
-3.99999999898768));
#29185=CARTESIAN_POINT('Origin',(0.,0.,-1.52655665885959E-15));
#29186=CARTESIAN_POINT('Ctrl Pts',(-10.5012771497262,-16.9202333839219,
-3.99999999956588));
#29187=CARTESIAN_POINT('Ctrl Pts',(-10.4187604568685,-16.7101716410219,
-3.37073654287492));
#29188=CARTESIAN_POINT('Ctrl Pts',(-10.3305099036574,-16.5650785907353,
-2.72191849220108));
#29189=CARTESIAN_POINT('Ctrl Pts',(-10.1942344309796,-16.4304182340015,
-1.65243412194127));
#29190=CARTESIAN_POINT('Ctrl Pts',(-10.1434939576109,-16.4029645969824,
-1.23816814046302));
#29191=CARTESIAN_POINT('Ctrl Pts',(-10.0619600213849,-16.3964234338767,
-0.534323206973444));
#29192=CARTESIAN_POINT('Ctrl Pts',(-10.0297590861916,-16.405197558861,-0.245020961131435));
#29193=CARTESIAN_POINT('Ctrl Pts',(-9.96722322847196,-16.445747510702,0.339093202692876));
#29194=CARTESIAN_POINT('Ctrl Pts',(-9.93695047232516,-16.4780618942896,
0.633872226361229));
#29195=CARTESIAN_POINT('Ctrl Pts',(-9.86331380880832,-16.5888828384849,
1.37316327975098));
#29196=CARTESIAN_POINT('Ctrl Pts',(-9.82144696478302,-16.6826460743033,
1.81522911734934));
#29197=CARTESIAN_POINT('Ctrl Pts',(-9.72257053474009,-16.9685368560364,
2.85099145769367));
#29198=CARTESIAN_POINT('Ctrl Pts',(-9.66615620033608,-17.1838459623691,
3.43595755998537));
#29199=CARTESIAN_POINT('Ctrl Pts',(-9.6013492080081,-17.4466390149939,3.99999999898783));
#29200=CARTESIAN_POINT('Ctrl Pts',(-7.99641857074021,-18.238103234253,3.99999999956596));
#29201=CARTESIAN_POINT('Ctrl Pts',(-7.87003904712881,-18.0511186750576,
3.37073613189377));
#29202=CARTESIAN_POINT('Ctrl Pts',(-7.80044962194119,-17.8962074550045,
2.72191770909427));
#29203=CARTESIAN_POINT('Ctrl Pts',(-7.7666597555164,-17.7076268935435,1.6524331309639));
#29204=CARTESIAN_POINT('Ctrl Pts',(-7.77277420580999,-17.6502604964735,
1.23816736813676));
#29205=CARTESIAN_POINT('Ctrl Pts',(-7.81356476654144,-17.5793613665421,
0.534322830796256));
#29206=CARTESIAN_POINT('Ctrl Pts',(-7.83903454756133,-17.557793473122,0.245020764801146));
#29207=CARTESIAN_POINT('Ctrl Pts',(-7.90787348529572,-17.5292237992452,
-0.339093040828276));
#29208=CARTESIAN_POINT('Ctrl Pts',(-7.95165126932984,-17.5225782933531,
-0.633871885375969));
#29209=CARTESIAN_POINT('Ctrl Pts',(-8.08468991868255,-17.524662026619,-1.37316256290256));
#29210=CARTESIAN_POINT('Ctrl Pts',(-8.18567626336398,-17.5432664999818,
-1.81522819845542));
#29211=CARTESIAN_POINT('Ctrl Pts',(-8.47729064196968,-17.6237100686022,
-2.85099073606036));
#29212=CARTESIAN_POINT('Ctrl Pts',(-8.68668612492522,-17.699169947002,-3.43595718934435));
#29213=CARTESIAN_POINT('Ctrl Pts',(-8.93996803629468,-17.7946084824509,
-3.99999999899206));
#29214=CARTESIAN_POINT('Origin',(0.,0.,-1.52655665885959E-15));
#29215=CARTESIAN_POINT('Ctrl Pts',(-4.08088993973066,-19.4914713872994,
-3.99999999959139));
#29216=CARTESIAN_POINT('Ctrl Pts',(-4.075097616853,-19.2663672599189,-3.37209958168756));
#29217=CARTESIAN_POINT('Ctrl Pts',(-4.04151488495295,-19.100085449018,-2.72444413832849));
#29218=CARTESIAN_POINT('Ctrl Pts',(-3.95929377669572,-18.9267270967929,
-1.65559225403134));
#29219=CARTESIAN_POINT('Ctrl Pts',(-3.92085570623925,-18.8834120879058,
-1.24058188697122));
#29220=CARTESIAN_POINT('Ctrl Pts',(-3.84626919930535,-18.8492280764763,
-0.535456963326743));
#29221=CARTESIAN_POINT('Ctrl Pts',(-3.81293438333759,-18.8464340988296,
-0.245615809434569));
#29222=CARTESIAN_POINT('Ctrl Pts',(-3.74017208754007,-18.8631726846702,
0.33957733005154));
#29223=CARTESIAN_POINT('Ctrl Pts',(-3.70061976632791,-18.8832332349247,
0.634895228803465));
#29224=CARTESIAN_POINT('Ctrl Pts',(-3.59342903055762,-18.96239114962,1.37542369564931));
#29225=CARTESIAN_POINT('Ctrl Pts',(-3.52199606602467,-19.0363769342966,
1.81820629365906));
#29226=CARTESIAN_POINT('Ctrl Pts',(-3.33167571844776,-19.2713421302941,
2.85336161053001));
#29227=CARTESIAN_POINT('Ctrl Pts',(-3.20554674526758,-19.4540672990858,
3.43720195324353));
#29228=CARTESIAN_POINT('Ctrl Pts',(-3.05519487086468,-19.6783359010447,
3.99999999896488));
#29229=CARTESIAN_POINT('Ctrl Pts',(-1.27637679201104,-19.8731472551927,
3.99999999956669));
#29230=CARTESIAN_POINT('Ctrl Pts',(-1.22157081634586,-19.6542137025961,
3.37073263858597));
#29231=CARTESIAN_POINT('Ctrl Pts',(-1.20916011335527,-19.4848433224616,
2.72191105135018));
#29232=CARTESIAN_POINT('Ctrl Pts',(-1.2419059761139,-19.2960794163494,1.65242470707477));
#29233=CARTESIAN_POINT('Ctrl Pts',(-1.26727187692857,-19.2442644111501,
1.23816080391726));
#29234=CARTESIAN_POINT('Ctrl Pts',(-1.32985096795119,-19.1915927623124,
0.534319634824896));
#29235=CARTESIAN_POINT('Ctrl Pts',(-1.36116119974521,-19.1800368758689,
0.245019097172672));
#29236=CARTESIAN_POINT('Ctrl Pts',(-1.43561967705555,-19.1767345012991,
-0.3390916643061));
#29237=CARTESIAN_POINT('Ctrl Pts',(-1.47903005465377,-19.1854625584864,
-0.633868986565802));
#29238=CARTESIAN_POINT('Ctrl Pts',(-1.6033324543231,-19.2329220526464,-1.37315646710162));
#29239=CARTESIAN_POINT('Ctrl Pts',(-1.69186532339641,-19.2849434365897,
-1.81522038319652));
#29240=CARTESIAN_POINT('Ctrl Pts',(-1.93838073553248,-19.4602730828495,
-2.85098459801236));
#29241=CARTESIAN_POINT('Ctrl Pts',(-2.10934078988132,-19.6028000727424,
-3.43595403741119));
#29242=CARTESIAN_POINT('Ctrl Pts',(-2.31470740137875,-19.7791114355451,
-3.99999999899378));
#29243=CARTESIAN_POINT('Origin',(0.,0.,-1.52655665885959E-15));
#29244=CARTESIAN_POINT('Ctrl Pts',(2.83169367195904,-19.7117383934115,-3.99999999959142));
#29245=CARTESIAN_POINT('Ctrl Pts',(2.7601464878485,-19.4982285387167,-3.37209935131022));
#29246=CARTESIAN_POINT('Ctrl Pts',(2.7348321530384,-19.3304887480299,-2.724443690446));
#29247=CARTESIAN_POINT('Ctrl Pts',(2.75280264993414,-19.1394639546591,-1.65559168311938));
#29248=CARTESIAN_POINT('Ctrl Pts',(2.77410799980605,-19.0856146013918,-1.24058143593821));
#29249=CARTESIAN_POINT('Ctrl Pts',(2.83250474307015,-19.0279820902413,-0.535456738393028));
#29250=CARTESIAN_POINT('Ctrl Pts',(2.86287361435655,-19.0139554414165,-0.245615692574478));
#29251=CARTESIAN_POINT('Ctrl Pts',(2.93697271462468,-19.0047984005023,0.339577232598883));
#29252=CARTESIAN_POINT('Ctrl Pts',(2.98100083826909,-19.0101214553008,0.634895024162846));
#29253=CARTESIAN_POINT('Ctrl Pts',(3.10880075780547,-19.0478441421225,1.3754232797282));
#29254=CARTESIAN_POINT('Ctrl Pts',(3.20123040637967,-19.0929364953614,1.818205770712));
#29255=CARTESIAN_POINT('Ctrl Pts',(3.46043591761268,-19.2486381221038,2.85336120369635));
#29256=CARTESIAN_POINT('Ctrl Pts',(3.64145416796019,-19.3772049873814,3.43720174746467));
#29257=CARTESIAN_POINT('Ctrl Pts',(3.85944318717447,-19.5365252237514,3.99999999896495));
#29258=CARTESIAN_POINT('Ctrl Pts',(5.59761479218166,-19.1111964089144,3.99999999956627));
#29259=CARTESIAN_POINT('Ctrl Pts',(5.57423581314006,-18.8867221808677,3.37073466344091));
#29260=CARTESIAN_POINT('Ctrl Pts',(5.52796963846509,-18.7233217839794,2.72191491027107));
#29261=CARTESIAN_POINT('Ctrl Pts',(5.43263718389282,-18.5571411928521,1.65242958960015));
#29262=CARTESIAN_POINT('Ctrl Pts',(5.39107901246981,-18.5171264390661,1.2381646084617));
#29263=CARTESIAN_POINT('Ctrl Pts',(5.31425879574368,-18.4890343760603,0.534321487064496));
#29264=CARTESIAN_POINT('Ctrl Pts',(5.28088432901487,-18.488884093517,0.245020063641224));
#29265=CARTESIAN_POINT('Ctrl Pts',(5.20978656133964,-18.5112472302137,-0.339092462136402));
#29266=CARTESIAN_POINT('Ctrl Pts',(5.17197924186115,-18.5342962315327,-0.633870666671581));
#29267=CARTESIAN_POINT('Ctrl Pts',(5.07140519544207,-18.6214078210074,-1.37316000034045));
#29268=CARTESIAN_POINT('Ctrl Pts',(5.00600388405473,-18.7005722398706,-1.81522491323566));
#29269=CARTESIAN_POINT('Ctrl Pts',(4.83432201950212,-18.9496415942878,-2.8509881559385));
#29270=CARTESIAN_POINT('Ctrl Pts',(4.72241993177592,-19.1420444152983,-3.43595586448725));
#29271=CARTESIAN_POINT('Ctrl Pts',(4.58974103596836,-19.377961625425,-3.99999999899278));
#29272=CARTESIAN_POINT('Origin',(0.,0.,-1.52655665885959E-15));
#29273=CARTESIAN_POINT('Ctrl Pts',(9.40271337324749,-17.5544894759802,-3.99999999956588));
#29274=CARTESIAN_POINT('Ctrl Pts',(9.26205290644762,-17.3779970458287,-3.3707365167023));
#29275=CARTESIAN_POINT('Ctrl Pts',(9.18052390875412,-17.2290232989961,-2.72191844231462));
#29276=CARTESIAN_POINT('Ctrl Pts',(9.13204235463654,-17.0436751051941,-1.65243405881907));
#29277=CARTESIAN_POINT('Ctrl Pts',(9.13363704400285,-16.98600575205,-1.23816809127292));
#29278=CARTESIAN_POINT('Ctrl Pts',(9.16873919747339,-16.9121247155165,-0.534323183023807));
#29279=CARTESIAN_POINT('Ctrl Pts',(9.19243827931401,-16.8886249515458,-0.245020948638851));
#29280=CARTESIAN_POINT('Ctrl Pts',(9.25882349418162,-16.8547422874094,0.339093192364722));
#29281=CARTESIAN_POINT('Ctrl Pts',(9.30194494783013,-16.8446825032557,0.633872204620666));
#29282=CARTESIAN_POINT('Ctrl Pts',(9.43473702861777,-16.836321751989,1.37316323404884));
#29283=CARTESIAN_POINT('Ctrl Pts',(9.53687179232336,-16.8469456166778,1.8152290587629));
#29284=CARTESIAN_POINT('Ctrl Pts',(9.83389869107151,-16.9042615007311,2.8509914116832));
#29285=CARTESIAN_POINT('Ctrl Pts',(10.0485690253218,-16.9630598055269,3.43595753636118));
#29286=CARTESIAN_POINT('Ctrl Pts',(10.3085579933225,-17.0383318324281,3.99999999898785));
#29287=CARTESIAN_POINT('Ctrl Pts',(11.7964514248447,-16.0441532441892,3.99999999956582));
#29288=CARTESIAN_POINT('Ctrl Pts',(11.6977078731048,-15.8412133261142,3.37073678763047));
#29289=CARTESIAN_POINT('Ctrl Pts',(11.5983454761403,-15.7034916683235,2.72191895897971));
#29290=CARTESIAN_POINT('Ctrl Pts',(11.4519247140414,-15.5799384566402,1.65243471248429));
#29291=CARTESIAN_POINT('Ctrl Pts',(11.3991866319042,-15.556550486245,1.23816860061448));
#29292=CARTESIAN_POINT('Ctrl Pts',(11.3173907762775,-15.5564265561472,0.534323430954352));
#29293=CARTESIAN_POINT('Ctrl Pts',(11.2859775000178,-15.5677000913787,0.245021077964069));
#29294=CARTESIAN_POINT('Ctrl Pts',(11.2268159107157,-15.6130315628983,-0.3390932992844));
#29295=CARTESIAN_POINT('Ctrl Pts',(11.1991718272383,-15.6476215182706,-0.633872429679788));
#29296=CARTESIAN_POINT('Ctrl Pts',(11.1344570739692,-15.7638783461539,-1.37316370730182));
#29297=CARTESIAN_POINT('Ctrl Pts',(11.1000758830408,-15.8606374078102,-1.81522966550313));
#29298=CARTESIAN_POINT('Ctrl Pts',(11.0239350595923,-16.1534046315318,-2.85099188820882));
#29299=CARTESIAN_POINT('Ctrl Pts',(10.9845876486587,-16.3724761407036,-3.43595778093133));
#29300=CARTESIAN_POINT('Ctrl Pts',(10.9405989703516,-16.6395436747412,-3.99999999899174));
#29301=CARTESIAN_POINT('Origin',(0.,0.,-1.52655665885959E-15));
#29302=CARTESIAN_POINT('Ctrl Pts',(14.8396644849569,-13.2798899662611,-3.9999999995905));
#29303=CARTESIAN_POINT('Ctrl Pts',(14.6476178493517,-13.1623228272254,-3.37210843275759));
#29304=CARTESIAN_POINT('Ctrl Pts',(14.5204071762085,-13.0500980157257,-2.72446134735375));
#29305=CARTESIAN_POINT('Ctrl Pts',(14.4113845387651,-12.8922113357332,-1.65561419086607));
#29306=CARTESIAN_POINT('Ctrl Pts',(14.3930912670047,-12.8372640574668,-1.24059921848));
#29307=CARTESIAN_POINT('Ctrl Pts',(14.4007800895373,-12.7555764141202,-0.535465607992792));
#29308=CARTESIAN_POINT('Ctrl Pts',(14.4150279702596,-12.725310024131,-0.245620301332475));
#29309=CARTESIAN_POINT('Ctrl Pts',(14.4659058080392,-12.6706645585297,0.339581072872028));
#29310=CARTESIAN_POINT('Ctrl Pts',(14.5030554377286,-12.6464413644873,0.634903090087537));
#29311=CARTESIAN_POINT('Ctrl Pts',(14.6252050701422,-12.5931907021199,1.37543967270944));
#29312=CARTESIAN_POINT('Ctrl Pts',(14.7249961464161,-12.5683214715053,1.81822638070561));
#29313=CARTESIAN_POINT('Ctrl Pts',(15.0236415549845,-12.5209843938585,2.85337723702139));
#29314=CARTESIAN_POINT('Ctrl Pts',(15.244947294886,-12.5031178193113,3.43720985680749));
#29315=CARTESIAN_POINT('Ctrl Pts',(15.5143414301618,-12.4850442338677,3.99999999896253));
#29316=CARTESIAN_POINT('Ctrl Pts',(16.5724493912429,-11.0419672484927,3.99999999959052));
#29317=CARTESIAN_POINT('Ctrl Pts',(16.4105423432717,-10.8854741265665,3.37210815126127));
#29318=CARTESIAN_POINT('Ctrl Pts',(16.2700411426964,-10.7904141902987,2.72446080000339));
#29319=CARTESIAN_POINT('Ctrl Pts',(16.0898865008145,-10.7243958472827,1.65561349312514));
#29320=CARTESIAN_POINT('Ctrl Pts',(16.0321092007946,-10.720442960367,1.24059866719413));
#29321=CARTESIAN_POINT('Ctrl Pts',(15.9549486870048,-10.7483398201034,0.535465332991227));
#29322=CARTESIAN_POINT('Ctrl Pts',(15.9292137549567,-10.7697119622927,0.245620158427659));
#29323=CARTESIAN_POINT('Ctrl Pts',(15.8890476878997,-10.8326513267222,-0.339580953843327));
#29324=CARTESIAN_POINT('Ctrl Pts',(15.874897584762,-10.8746826391374,-0.634902840058553));
#29325=CARTESIAN_POINT('Ctrl Pts',(15.8539268865206,-11.0062743746583,-1.37543916459227));
#29326=CARTESIAN_POINT('Ctrl Pts',(15.8548354618282,-11.1091136012863,-1.81822574191787));
#29327=CARTESIAN_POINT('Ctrl Pts',(15.8837809457042,-11.4100987454289,-2.85337674009904));
#29328=CARTESIAN_POINT('Ctrl Pts',(15.9218939692831,-11.6288289263462,-3.43720960548705));
#29329=CARTESIAN_POINT('Ctrl Pts',(15.971846987374,-11.894167618845,-3.9999999989626));
#29330=CARTESIAN_POINT('Origin',(0.,0.,-1.52655665885959E-15));
#29331=CARTESIAN_POINT('Ctrl Pts',(18.4867046541144,-7.40357147418018,-3.99999999956608));
#29332=CARTESIAN_POINT('Ctrl Pts',(18.2655049621798,-7.35878522980345,-3.37073552377234));
#29333=CARTESIAN_POINT('Ctrl Pts',(18.1072914318695,-7.29707069450407,-2.72191654976098));
#29334=CARTESIAN_POINT('Ctrl Pts',(17.9510130074857,-7.186249267535,-1.65243166413342));
#29335=CARTESIAN_POINT('Ctrl Pts',(17.9151655629091,-7.14104706416568,-1.238166225129));
#29336=CARTESIAN_POINT('Ctrl Pts',(17.8945656455494,-7.0618878542373,-0.534322274341816));
#29337=CARTESIAN_POINT('Ctrl Pts',(17.897614847696,-7.0286525779651,-0.245020474504692));
#29338=CARTESIAN_POINT('Ctrl Pts',(17.9266894795329,-6.96002545649323,0.339092800984476));
#29339=CARTESIAN_POINT('Ctrl Pts',(17.9532560787444,-6.92460131329069,0.633871380422906));
#29340=CARTESIAN_POINT('Ctrl Pts',(18.0496063618674,-6.83283953621556,1.37316150113643));
#29341=CARTESIAN_POINT('Ctrl Pts',(18.1346748807368,-6.77532690925219,1.81522683723282));
#29342=CARTESIAN_POINT('Ctrl Pts',(18.3990525834921,-6.62830792441045,2.85098966698316));
#29343=CARTESIAN_POINT('Ctrl Pts',(18.6012947101893,-6.53536228497352,3.43595664050605));
#29344=CARTESIAN_POINT('Ctrl Pts',(18.8488421544629,-6.42590608161792,3.99999999898834));
#29345=CARTESIAN_POINT('Ctrl Pts',(19.3495836398166,-4.70794355402034,3.99999999959111));
#29346=CARTESIAN_POINT('Ctrl Pts',(19.1439151849879,-4.61626238501579,3.37210239330695));
#29347=CARTESIAN_POINT('Ctrl Pts',(18.9793742258157,-4.57498815790177,2.72444960464601));
#29348=CARTESIAN_POINT('Ctrl Pts',(18.7875058402052,-4.5745672552028,1.65559922198222));
#29349=CARTESIAN_POINT('Ctrl Pts',(18.7318618872307,-4.59061344990958,1.24058739192793));
#29350=CARTESIAN_POINT('Ctrl Pts',(18.6688970666432,-4.64321781147727,0.535459708945694));
#29351=CARTESIAN_POINT('Ctrl Pts',(18.65202412042,-4.67210262964909,0.245617236089079));
#29352=CARTESIAN_POINT('Ctrl Pts',(18.6358070632848,-4.74498326107249,-0.339578518865884));
#29353=CARTESIAN_POINT('Ctrl Pts',(18.6368857612635,-4.78931905828187,-0.634897725707169));
#29354=CARTESIAN_POINT('Ctrl Pts',(18.6621860721811,-4.92014654177133,-1.37542877063301));
#29355=CARTESIAN_POINT('Ctrl Pts',(18.6982122204778,-5.01647273909291,-1.81821267443061));
#29356=CARTESIAN_POINT('Ctrl Pts',(18.8283538957884,-5.28940758861785,-2.85336657449289));
#29357=CARTESIAN_POINT('Ctrl Pts',(18.9389788671592,-5.48191375800988,-3.43720446401169));
#29358=CARTESIAN_POINT('Ctrl Pts',(19.0766716892569,-5.71416807537147,-3.99999999896414));
#29359=CARTESIAN_POINT('Ctrl Pts',(16.7190336201597,-4.91959556137297,-10.5713320220547));
#29360=CARTESIAN_POINT('Ctrl Pts',(16.9459555615988,-4.14841111729778,-3.52377734068488));
#29361=CARTESIAN_POINT('Ctrl Pts',(17.1194334972985,-3.36150582706258,3.52377734068489));
#29362=CARTESIAN_POINT('Ctrl Pts',(17.2378112556832,-2.56639217442552,10.5713320220547));
#29363=CARTESIAN_POINT('Ctrl Pts',(16.7186664266411,-4.91948445047195,-10.5713320220547));
#29364=CARTESIAN_POINT('Ctrl Pts',(16.9455832429635,-4.14831694361546,-3.52377734068489));
#29365=CARTESIAN_POINT('Ctrl Pts',(17.1190572273169,-3.36142894566319,3.5237773406849));
#29366=CARTESIAN_POINT('Ctrl Pts',(17.2374322458488,-2.56633277528584,10.5713320220547));
#29367=CARTESIAN_POINT('Ctrl Pts',(16.718299233125,-4.91937333957171,-10.5713320220547));
#29368=CARTESIAN_POINT('Ctrl Pts',(16.9452109243307,-4.14822276993388,-3.52377734068487));
#29369=CARTESIAN_POINT('Ctrl Pts',(17.1186809573378,-3.36135206426426,3.52377734068488));
#29370=CARTESIAN_POINT('Ctrl Pts',(17.2370532360168,-2.56627337614658,10.5713320220547));
#29371=CARTESIAN_POINT('Ctrl Pts',(16.7179320396407,-4.91926222868205,-10.5713320220547));
#29372=CARTESIAN_POINT('Ctrl Pts',(16.9448386057302,-4.14812859626138,-3.52377734068488));
#29373=CARTESIAN_POINT('Ctrl Pts',(17.1183046873915,-3.36127518287299,3.52377734068489));
#29374=CARTESIAN_POINT('Ctrl Pts',(17.2366742262179,-2.56621397701342,10.5713320220547));
#29375=CARTESIAN_POINT('Ctrl Pts',(16.7190706763197,-4.91946962582517,-10.5701811473657));
#29376=CARTESIAN_POINT('Ctrl Pts',(16.9459620956421,-4.14836742740649,-3.52339371578857));
#29377=CARTESIAN_POINT('Ctrl Pts',(17.1194210550923,-3.3615482144642,3.52339371578857));
#29378=CARTESIAN_POINT('Ctrl Pts',(17.2377919239458,-2.56652201742717,10.5701811473657));
#29379=CARTESIAN_POINT('Ctrl Pts',(16.7179320396407,-4.91926222868205,-10.5713320220547));
#29380=CARTESIAN_POINT('Ctrl Pts',(16.9448386057302,-4.14812859626139,-3.52377734068488));
#29381=CARTESIAN_POINT('Ctrl Pts',(17.1183046873915,-3.36127518287299,3.52377734068489));
#29382=CARTESIAN_POINT('Ctrl Pts',(17.2366742262179,-2.56621397701342,10.5713320220547));
#29383=CARTESIAN_POINT('Ctrl Pts',(14.0281517405305,-10.341153921307,-10.5713320220547));
#29384=CARTESIAN_POINT('Ctrl Pts',(14.5051492284884,-9.69408946487939,-3.52377734068488));
#29385=CARTESIAN_POINT('Ctrl Pts',(14.9373026246845,-9.01397331881983,3.52377734068489));
#29386=CARTESIAN_POINT('Ctrl Pts',(15.3204862161389,-8.30729846463996,10.5713320220547));
#29387=CARTESIAN_POINT('Ctrl Pts',(14.027844693657,-10.3409239236334,-10.5713320220547));
#29388=CARTESIAN_POINT('Ctrl Pts',(14.5048315727105,-9.69387363009204,-3.52377734068488));
#29389=CARTESIAN_POINT('Ctrl Pts',(14.9369753415466,-9.01377238202311,3.52377734068489));
#29390=CARTESIAN_POINT('Ctrl Pts',(15.3201503790965,-8.30711301870881,10.5713320220547));
#29391=CARTESIAN_POINT('Ctrl Pts',(14.0275376467855,-10.3406939259613,-10.5713320220547));
#29392=CARTESIAN_POINT('Ctrl Pts',(14.5045139169348,-9.69365779530623,-3.52377734068489));
#29393=CARTESIAN_POINT('Ctrl Pts',(14.9366480584109,-9.0135714452277,3.5237773406849));
#29394=CARTESIAN_POINT('Ctrl Pts',(15.3198145420564,-8.30692757277894,10.5713320220547));
#29395=CARTESIAN_POINT('Ctrl Pts',(14.0272305999403,-10.34046392831,-10.5713320220547));
#29396=CARTESIAN_POINT('Ctrl Pts',(14.5041962611863,-9.69344196054,-3.52377734068488));
#29397=CARTESIAN_POINT('Ctrl Pts',(14.9363207753034,-9.01337050845065,3.52377734068489));
#29398=CARTESIAN_POINT('Ctrl Pts',(15.3194787050451,-8.30674212686605,10.5713320220547));
#29399=CARTESIAN_POINT('Ctrl Pts',(14.0282296344247,-10.3410482545552,-10.5701811473657));
#29400=CARTESIAN_POINT('Ctrl Pts',(14.5051703113035,-9.69405064458535,-3.52339371578857));
#29401=CARTESIAN_POINT('Ctrl Pts',(14.93727643549,-9.0140088944632,3.52339371578857));
#29402=CARTESIAN_POINT('Ctrl Pts',(15.3204236413258,-8.30741386530685,10.5701811473657));
#29403=CARTESIAN_POINT('Ctrl Pts',(14.0272305999403,-10.3404639283101,-10.5713320220547));
#29404=CARTESIAN_POINT('Ctrl Pts',(14.5041962611863,-9.69344196054,-3.52377734068488));
#29405=CARTESIAN_POINT('Ctrl Pts',(14.9363207753034,-9.01337050845065,3.52377734068488));
#29406=CARTESIAN_POINT('Ctrl Pts',(15.3194787050451,-8.30674212686606,10.5713320220547));
#29407=CARTESIAN_POINT('Ctrl Pts',(9.64526772752331,-14.5154164991539,-10.5713320220547));
#29408=CARTESIAN_POINT('Ctrl Pts',(10.314807825219,-14.0705175534734,-3.52377734068489));
#29409=CARTESIAN_POINT('Ctrl Pts',(10.9535126044255,-13.5792225962495,3.52377734068489));
#29410=CARTESIAN_POINT('Ctrl Pts',(11.5552844326327,-13.046221957351,10.5713320220547));
#29411=CARTESIAN_POINT('Ctrl Pts',(9.64505786167931,-14.5150953558215,-10.5713320220547));
#29412=CARTESIAN_POINT('Ctrl Pts',(10.3145831462736,-14.0702060904417,-3.5237773406849));
#29413=CARTESIAN_POINT('Ctrl Pts',(10.9532737833079,-13.5789218399987,3.5237773406849));
#29414=CARTESIAN_POINT('Ctrl Pts',(11.5550322752861,-13.0459328321446,10.5713320220547));
#29415=CARTESIAN_POINT('Ctrl Pts',(9.64484799583672,-14.5147742124913,-10.5713320220547));
#29416=CARTESIAN_POINT('Ctrl Pts',(10.3143584673295,-14.0698946274123,-3.52377734068489));
#29417=CARTESIAN_POINT('Ctrl Pts',(10.953034962192,-13.5786210837499,3.52377734068489));
#29418=CARTESIAN_POINT('Ctrl Pts',(11.5547801179413,-13.0456437069402,10.5713320220547));
#29419=CARTESIAN_POINT('Ctrl Pts',(9.64463813001165,-14.5144530691896,-10.5713320220547));
#29420=CARTESIAN_POINT('Ctrl Pts',(10.3141337884043,-14.0695831644105,-3.52377734068489));
#29421=CARTESIAN_POINT('Ctrl Pts',(10.9527961410962,-13.5783203275278,3.52377734068489));
#29422=CARTESIAN_POINT('Ctrl Pts',(11.5545279606177,-13.0453545817615,10.5713320220547));
#29423=CARTESIAN_POINT('Ctrl Pts',(9.64537706399844,-14.5153438461678,-10.5701811473657));
#29424=CARTESIAN_POINT('Ctrl Pts',(10.3148409139074,-14.070488285077,-3.52339371578857));
#29425=CARTESIAN_POINT('Ctrl Pts',(10.953475827046,-13.579247069187,3.52339371578857));
#29426=CARTESIAN_POINT('Ctrl Pts',(11.55518616219,-13.0463089966596,10.5701811473657));
#29427=CARTESIAN_POINT('Ctrl Pts',(9.64463813001167,-14.5144530691896,-10.5713320220547));
#29428=CARTESIAN_POINT('Ctrl Pts',(10.3141337884043,-14.0695831644105,-3.52377734068489));
#29429=CARTESIAN_POINT('Ctrl Pts',(10.9527961410962,-13.5783203275278,3.52377734068489));
#29430=CARTESIAN_POINT('Ctrl Pts',(11.5545279606177,-13.0453545817615,10.5713320220547));
#29431=CARTESIAN_POINT('Ctrl Pts',(4.09902207758572,-16.9389056224709,-10.5713320220547));
#29432=CARTESIAN_POINT('Ctrl Pts',(4.88034836787775,-16.7498335663957,-3.52377734068489));
#29433=CARTESIAN_POINT('Ctrl Pts',(5.64856730744365,-16.5066172205901,3.52377734068489));
#29434=CARTESIAN_POINT('Ctrl Pts',(6.39634480871554,-16.2115785402758,10.5713320220547));
#29435=CARTESIAN_POINT('Ctrl Pts',(4.09893470568933,-16.9385320681052,-10.5713320220547));
#29436=CARTESIAN_POINT('Ctrl Pts',(4.88024376536137,-16.749464042158,-3.5237773406849));
#29437=CARTESIAN_POINT('Ctrl Pts',(5.6484457536978,-16.5062529205276,3.5237773406849));
#29438=CARTESIAN_POINT('Ctrl Pts',(6.39620674496223,-16.211220608561,10.5713320220547));
#29439=CARTESIAN_POINT('Ctrl Pts',(4.09884733379351,-16.9381585137421,-10.5713320220547));
#29440=CARTESIAN_POINT('Ctrl Pts',(4.88013916284558,-16.749094517923,-3.52377734068488));
#29441=CARTESIAN_POINT('Ctrl Pts',(5.64832419995282,-16.5058886204677,3.52377734068488));
#29442=CARTESIAN_POINT('Ctrl Pts',(6.39606868120983,-16.2108626768487,10.5713320220547));
#29443=CARTESIAN_POINT('Ctrl Pts',(4.09875996190443,-16.9377849594116,-10.5713320220547));
#29444=CARTESIAN_POINT('Ctrl Pts',(4.88003456033808,-16.7487249937203,-3.52377734068489));
#29445=CARTESIAN_POINT('Ctrl Pts',(5.64820264621756,-16.5055243204397,3.52377734068489));
#29446=CARTESIAN_POINT('Ctrl Pts',(6.39593061746862,-16.2105047451678,10.5713320220547));
#29447=CARTESIAN_POINT('Ctrl Pts',(4.09914966904931,-16.9388747462729,-10.5701811473657));
#29448=CARTESIAN_POINT('Ctrl Pts',(4.88038947145514,-16.7498173800975,-3.52339371578857));
#29449=CARTESIAN_POINT('Ctrl Pts',(5.64852437777395,-16.5066276390243,3.52339371578857));
#29450=CARTESIAN_POINT('Ctrl Pts',(6.39622269550887,-16.2116267200009,10.5701811473657));
#29451=CARTESIAN_POINT('Ctrl Pts',(4.09875996190444,-16.9377849594116,-10.5713320220547));
#29452=CARTESIAN_POINT('Ctrl Pts',(4.88003456033808,-16.7487249937204,-3.52377734068489));
#29453=CARTESIAN_POINT('Ctrl Pts',(5.64820264621756,-16.5055243204397,3.52377734068489));
#29454=CARTESIAN_POINT('Ctrl Pts',(6.39593061746862,-16.2105047451678,10.5713320220547));
#29455=CARTESIAN_POINT('Ctrl Pts',(-1.94162613003165,-17.3193127360958,
-10.5713320220547));
#29456=CARTESIAN_POINT('Ctrl Pts',(-1.14275312890046,-17.4088724499949,
-3.52377734068489));
#29457=CARTESIAN_POINT('Ctrl Pts',(-0.337678570790839,-17.4430701964027,
3.52377734068489));
#29458=CARTESIAN_POINT('Ctrl Pts',(0.465911600871797,-17.4215794938256,
10.5713320220547));
#29459=CARTESIAN_POINT('Ctrl Pts',(-1.94158046964024,-17.3189318268663,
-10.5713320220547));
#29460=CARTESIAN_POINT('Ctrl Pts',(-1.14272503838051,-17.4084894346279,
-3.52377734068488));
#29461=CARTESIAN_POINT('Ctrl Pts',(-0.337668195989274,-17.4426862924926,
3.52377734068488));
#29462=CARTESIAN_POINT('Ctrl Pts',(0.465904283238004,-17.4211959274498,
10.5713320220547));
#29463=CARTESIAN_POINT('Ctrl Pts',(-1.9415348092492,-17.3185509176396,-10.5713320220547));
#29464=CARTESIAN_POINT('Ctrl Pts',(-1.14269694786089,-17.4081064192637,
-3.5237773406849));
#29465=CARTESIAN_POINT('Ctrl Pts',(-0.337657821187734,-17.4423023885854,
3.52377734068489));
#29466=CARTESIAN_POINT('Ctrl Pts',(0.465896965604224,-17.4208123610767,
10.5713320220547));
#29467=CARTESIAN_POINT('Ctrl Pts',(-1.94148914886299,-17.3181700084457,
-10.5713320220547));
#29468=CARTESIAN_POINT('Ctrl Pts',(-1.14266885734454,-17.4077234039326,
-3.52377734068489));
#29469=CARTESIAN_POINT('Ctrl Pts',(-0.337647446388026,-17.4419184847113,
3.52377734068489));
#29470=CARTESIAN_POINT('Ctrl Pts',(0.46588964797019,-17.4204287947368,10.5713320220547));
#29471=CARTESIAN_POINT('Ctrl Pts',(-1.94149567299316,-17.319327360811,-10.5701811473657));
#29472=CARTESIAN_POINT('Ctrl Pts',(-1.14270896813208,-17.4088712981013,
-3.52339371578857));
#29473=CARTESIAN_POINT('Ctrl Pts',(-0.337722474799018,-17.4430653037166,
3.52339371578857));
#29474=CARTESIAN_POINT('Ctrl Pts',(0.465780373556112,-17.4215830027813,
10.5701811473657));
#29475=CARTESIAN_POINT('Ctrl Pts',(-1.94148914886299,-17.3181700084457,
-10.5713320220547));
#29476=CARTESIAN_POINT('Ctrl Pts',(-1.14266885734454,-17.4077234039326,
-3.52377734068489));
#29477=CARTESIAN_POINT('Ctrl Pts',(-0.337647446388026,-17.4419184847113,
3.52377734068488));
#29478=CARTESIAN_POINT('Ctrl Pts',(0.465889647970189,-17.4204287947368,
10.5713320220547));
#29479=CARTESIAN_POINT('Ctrl Pts',(-7.74808557101742,-15.6107551279143,
-10.5713320220547));
#29480=CARTESIAN_POINT('Ctrl Pts',(-7.02802173309331,-15.9681443885309,
-3.52377734068488));
#29481=CARTESIAN_POINT('Ctrl Pts',(-6.28319542978303,-16.2756314742303,
3.5237773406849));
#29482=CARTESIAN_POINT('Ctrl Pts',(-5.52071742216,-16.5302808452903,10.5713320220547));
#29483=CARTESIAN_POINT('Ctrl Pts',(-7.7479123856553,-15.6104128070958,-10.5713320220547));
#29484=CARTESIAN_POINT('Ctrl Pts',(-7.0278643376683,-15.9677940793406,-3.52377734068489));
#29485=CARTESIAN_POINT('Ctrl Pts',(-6.28305437778823,-16.2752742709501,
3.5237773406849));
#29486=CARTESIAN_POINT('Ctrl Pts',(-5.52059311105964,-16.5299179080192,
10.5713320220547));
#29487=CARTESIAN_POINT('Ctrl Pts',(-7.74773920029442,-15.6100704862797,
-10.5713320220547));
#29488=CARTESIAN_POINT('Ctrl Pts',(-7.0277069422445,-15.9674437701526,-3.52377734068487));
#29489=CARTESIAN_POINT('Ctrl Pts',(-6.28291332579438,-16.2749170676724,
3.52377734068489));
#29490=CARTESIAN_POINT('Ctrl Pts',(-5.52046879996019,-16.5295549707506,
10.5713320220547));
#29491=CARTESIAN_POINT('Ctrl Pts',(-7.74756601494938,-15.6097281654929,
-10.5713320220547));
#29492=CARTESIAN_POINT('Ctrl Pts',(-7.02754954683515,-15.9670934609948,
-3.52377734068488));
#29493=CARTESIAN_POINT('Ctrl Pts',(-6.28277227381364,-16.2745598644254,
3.5237773406849));
#29494=CARTESIAN_POINT('Ctrl Pts',(-5.52034448887238,-16.5291920335133,
10.5713320220547));
#29495=CARTESIAN_POINT('Ctrl Pts',(-7.74796798344821,-15.6108134895863,
-10.5701811473657));
#29496=CARTESIAN_POINT('Ctrl Pts',(-7.02797984157434,-15.9681584099774,
-3.52339371578857));
#29497=CARTESIAN_POINT('Ctrl Pts',(-6.28323501265835,-16.2756118605541,
3.52339371578857));
#29498=CARTESIAN_POINT('Ctrl Pts',(-5.52084193563372,-16.5302392602447,
10.5701811473657));
#29499=CARTESIAN_POINT('Ctrl Pts',(-7.74756601494938,-15.6097281654929,
-10.5713320220547));
#29500=CARTESIAN_POINT('Ctrl Pts',(-7.02754954683516,-15.9670934609948,
-3.52377734068488));
#29501=CARTESIAN_POINT('Ctrl Pts',(-6.28277227381364,-16.2745598644254,
3.5237773406849));
#29502=CARTESIAN_POINT('Ctrl Pts',(-5.52034448887238,-16.5291920335133,
10.5713320220547));
#29503=CARTESIAN_POINT('Ctrl Pts',(-12.620011542574,-12.019310061098,-10.5713320220547));
#29504=CARTESIAN_POINT('Ctrl Pts',(-12.0656071937211,-12.6014224490979,
-3.52377734068488));
#29505=CARTESIAN_POINT('Ctrl Pts',(-11.4708661898549,-13.1451113935275,
3.52377734068489));
#29506=CARTESIAN_POINT('Ctrl Pts',(-10.8414664469677,-13.6451863658503,
10.5713320220547));
#29507=CARTESIAN_POINT('Ctrl Pts',(-12.6197317209518,-12.0190476176333,
-10.5713320220547));
#29508=CARTESIAN_POINT('Ctrl Pts',(-12.0653394776022,-12.6011470985426,
-3.52377734068489));
#29509=CARTESIAN_POINT('Ctrl Pts',(-11.4706114736191,-13.1448239748645,
3.5237773406849));
#29510=CARTESIAN_POINT('Ctrl Pts',(-10.8412255008865,-13.6448878332752,
10.5713320220547));
#29511=CARTESIAN_POINT('Ctrl Pts',(-12.6194518993316,-12.0187851741704,
-10.5713320220547));
#29512=CARTESIAN_POINT('Ctrl Pts',(-12.0650717614852,-12.6008717479891,
-3.52377734068487));
#29513=CARTESIAN_POINT('Ctrl Pts',(-11.4703567573851,-13.1445365562034,
3.52377734068488));
#29514=CARTESIAN_POINT('Ctrl Pts',(-10.8409845548071,-13.6445893007021,
10.5713320220547));
#29515=CARTESIAN_POINT('Ctrl Pts',(-12.6191720777362,-12.0185227307296,
-10.5713320220547));
#29516=CARTESIAN_POINT('Ctrl Pts',(-12.0648040453921,-12.600596397459,-3.52377734068488));
#29517=CARTESIAN_POINT('Ctrl Pts',(-11.4701020411739,-13.1442491375668,
3.52377734068489));
#29518=CARTESIAN_POINT('Ctrl Pts',(-10.8407436087492,-13.6442907681545,
10.5713320220547));
#29519=CARTESIAN_POINT('Ctrl Pts',(-12.6199210072703,-12.0194051204477,
-10.5701811473657));
#29520=CARTESIAN_POINT('Ctrl Pts',(-12.065572624187,-12.601449952691,-3.52339371578857));
#29521=CARTESIAN_POINT('Ctrl Pts',(-11.4708966773184,-13.1450794245601,
3.52339371578857));
#29522=CARTESIAN_POINT('Ctrl Pts',(-10.8415692284369,-13.6451047025737,
10.5701811473657));
#29523=CARTESIAN_POINT('Ctrl Pts',(-12.6191720777362,-12.0185227307296,
-10.5713320220547));
#29524=CARTESIAN_POINT('Ctrl Pts',(-12.0648040453921,-12.600596397459,-3.52377734068488));
#29525=CARTESIAN_POINT('Ctrl Pts',(-11.4701020411739,-13.1442491375668,
3.52377734068489));
#29526=CARTESIAN_POINT('Ctrl Pts',(-10.8407436087492,-13.6442907681545,
10.5713320220547));
#29527=CARTESIAN_POINT('Ctrl Pts',(-15.9697778705622,-6.97815881478883,
-10.5713320220547));
#29528=CARTESIAN_POINT('Ctrl Pts',(-15.6479023573888,-7.71478298511549,
-3.52377734068489));
#29529=CARTESIAN_POINT('Ctrl Pts',(-15.2749811954754,-8.42909687758284,
3.52377734068489));
#29530=CARTESIAN_POINT('Ctrl Pts',(-14.8545746152671,-9.11428102918566,
10.5713320220547));
#29531=CARTESIAN_POINT('Ctrl Pts',(-15.9694251632972,-6.97800790323301,
-10.5713320220547));
#29532=CARTESIAN_POINT('Ctrl Pts',(-15.647556611091,-7.7146158045359,-3.52377734068489));
#29533=CARTESIAN_POINT('Ctrl Pts',(-15.2746435375359,-8.42891391046955,
3.52377734068488));
#29534=CARTESIAN_POINT('Ctrl Pts',(-14.8542460958585,-9.11408290874099,
10.5713320220547));
#29535=CARTESIAN_POINT('Ctrl Pts',(-15.9690724560347,-6.97785699167819,
-10.5713320220547));
#29536=CARTESIAN_POINT('Ctrl Pts',(-15.6472108647957,-7.71444862395734,
-3.5237773406849));
#29537=CARTESIAN_POINT('Ctrl Pts',(-15.2743058795987,-8.42873094335756,
3.52377734068489));
#29538=CARTESIAN_POINT('Ctrl Pts',(-14.8539175764522,-9.11388478829765,
10.5713320220547));
#29539=CARTESIAN_POINT('Ctrl Pts',(-15.9687197488033,-6.97770608013569,
-10.5713320220547));
#29540=CARTESIAN_POINT('Ctrl Pts',(-15.6468651185308,-7.71428144339257,
-3.52377734068489));
#29541=CARTESIAN_POINT('Ctrl Pts',(-15.2739682216914,-8.42854797626068,
3.52377734068489));
#29542=CARTESIAN_POINT('Ctrl Pts',(-14.8535890570749,-9.11368666787078,
10.5713320220547));
#29543=CARTESIAN_POINT('Ctrl Pts',(-15.9697253074178,-6.97827910625587,
-10.5701811473657));
#29544=CARTESIAN_POINT('Ctrl Pts',(-15.6478792794356,-7.71482065351599,
-3.52339371578857));
#29545=CARTESIAN_POINT('Ctrl Pts',(-15.274998910289,-8.4290564092534,3.52339371578858));
#29546=CARTESIAN_POINT('Ctrl Pts',(-14.8546432677697,-9.11416913747445,
10.5701811473657));
#29547=CARTESIAN_POINT('Ctrl Pts',(-15.9687197488033,-6.97770608013569,
-10.5713320220547));
#29548=CARTESIAN_POINT('Ctrl Pts',(-15.6468651185308,-7.71428144339257,
-3.52377734068489));
#29549=CARTESIAN_POINT('Ctrl Pts',(-15.2739682216914,-8.42854797626068,
3.52377734068489));
#29550=CARTESIAN_POINT('Ctrl Pts',(-14.8535890570749,-9.11368666787078,
10.5713320220547));
#29551=CARTESIAN_POINT('Ctrl Pts',(-17.3933532985407,-1.09533862876043,
-10.5713320220547));
#29552=CARTESIAN_POINT('Ctrl Pts',(-17.3428295583123,-1.89762683505751,
-3.52377734068489));
#29553=CARTESIAN_POINT('Ctrl Pts',(-17.2367080342085,-2.69640887798077,
3.5237773406849));
#29554=CARTESIAN_POINT('Ctrl Pts',(-17.0760018547927,-3.48405888793926,
10.5713320220547));
#29555=CARTESIAN_POINT('Ctrl Pts',(-17.3929702473346,-1.09531745127434,
-10.5713320220547));
#29556=CARTESIAN_POINT('Ctrl Pts',(-17.3424474839418,-1.89758798889885,
-3.52377734068489));
#29557=CARTESIAN_POINT('Ctrl Pts',(-17.2363281610962,-2.69635243095141,
3.5237773406849));
#29558=CARTESIAN_POINT('Ctrl Pts',(-17.0756253863458,-3.48398507587459,
10.5713320220547));
#29559=CARTESIAN_POINT('Ctrl Pts',(-17.3925871961311,-1.09529627378836,
-10.5713320220547));
#29560=CARTESIAN_POINT('Ctrl Pts',(-17.342065409574,-1.89754914274033,-3.52377734068488));
#29561=CARTESIAN_POINT('Ctrl Pts',(-17.2359482879864,-2.69629598392249,
3.52377734068489));
#29562=CARTESIAN_POINT('Ctrl Pts',(-17.0752489179014,-3.48391126381038,
10.5713320220547));
#29563=CARTESIAN_POINT('Ctrl Pts',(-17.392204144961,-1.09527509630334,-10.5713320220547));
#29564=CARTESIAN_POINT('Ctrl Pts',(-17.3416833352395,-1.89751029658436,
-3.52377734068489));
#29565=CARTESIAN_POINT('Ctrl Pts',(-17.2355684149098,-2.69623953689756,
3.5237773406849));
#29566=CARTESIAN_POINT('Ctrl Pts',(-17.07487244949,-3.48383745175174,10.5713320220547));
#29567=CARTESIAN_POINT('Ctrl Pts',(-17.3933450474466,-1.09546964341852,
-10.5701811473657));
#29568=CARTESIAN_POINT('Ctrl Pts',(-17.3428207554817,-1.89767012490037,
-3.52339371578857));
#29569=CARTESIAN_POINT('Ctrl Pts',(-17.2367108397044,-2.6963647913671,3.52339371578857));
#29570=CARTESIAN_POINT('Ctrl Pts',(-17.0760280978237,-3.48393026358512,
10.5701811473657));
#29571=CARTESIAN_POINT('Ctrl Pts',(-17.392204144961,-1.09527509630334,-10.5713320220547));
#29572=CARTESIAN_POINT('Ctrl Pts',(-17.3416833352395,-1.89751029658436,
-3.52377734068489));
#29573=CARTESIAN_POINT('Ctrl Pts',(-17.2355684149098,-2.69623953689756,
3.52377734068489));
#29574=CARTESIAN_POINT('Ctrl Pts',(-17.07487244949,-3.48383745175174,10.5713320220547));
#29575=CARTESIAN_POINT('Ctrl Pts',(-16.7190336201597,4.91959556137296,-10.5713320220547));
#29576=CARTESIAN_POINT('Ctrl Pts',(-16.9459555615988,4.14841111729777,-3.52377734068488));
#29577=CARTESIAN_POINT('Ctrl Pts',(-17.1194334972985,3.36150582706257,3.5237773406849));
#29578=CARTESIAN_POINT('Ctrl Pts',(-17.2378112556832,2.56639217442551,10.5713320220547));
#29579=CARTESIAN_POINT('Ctrl Pts',(-16.7186664266411,4.91948445047194,-10.5713320220547));
#29580=CARTESIAN_POINT('Ctrl Pts',(-16.9455832429635,4.14831694361545,-3.52377734068487));
#29581=CARTESIAN_POINT('Ctrl Pts',(-17.1190572273169,3.36142894566318,3.52377734068489));
#29582=CARTESIAN_POINT('Ctrl Pts',(-17.2374322458487,2.56633277528582,10.5713320220547));
#29583=CARTESIAN_POINT('Ctrl Pts',(-16.718299233125,4.91937333957173,-10.5713320220547));
#29584=CARTESIAN_POINT('Ctrl Pts',(-16.9452109243308,4.14822276993391,-3.52377734068489));
#29585=CARTESIAN_POINT('Ctrl Pts',(-17.1186809573379,3.36135206426428,3.52377734068491));
#29586=CARTESIAN_POINT('Ctrl Pts',(-17.2370532360169,2.56627337614659,10.5713320220547));
#29587=CARTESIAN_POINT('Ctrl Pts',(-16.7179320396407,4.91926222868204,-10.5713320220547));
#29588=CARTESIAN_POINT('Ctrl Pts',(-16.9448386057302,4.14812859626137,-3.52377734068488));
#29589=CARTESIAN_POINT('Ctrl Pts',(-17.1183046873915,3.36127518287297,3.5237773406849));
#29590=CARTESIAN_POINT('Ctrl Pts',(-17.2366742262179,2.5662139770134,10.5713320220547));
#29591=CARTESIAN_POINT('Ctrl Pts',(-16.7190706763197,4.91946962582517,-10.5701811473657));
#29592=CARTESIAN_POINT('Ctrl Pts',(-16.9459620956421,4.14836742740648,-3.52339371578857));
#29593=CARTESIAN_POINT('Ctrl Pts',(-17.1194210550923,3.36154821446419,3.52339371578858));
#29594=CARTESIAN_POINT('Ctrl Pts',(-17.2377919239458,2.56652201742716,10.5701811473657));
#29595=CARTESIAN_POINT('Ctrl Pts',(-16.7179320396407,4.91926222868204,-10.5713320220547));
#29596=CARTESIAN_POINT('Ctrl Pts',(-16.9448386057302,4.14812859626138,-3.52377734068488));
#29597=CARTESIAN_POINT('Ctrl Pts',(-17.1183046873915,3.36127518287298,3.52377734068489));
#29598=CARTESIAN_POINT('Ctrl Pts',(-17.2366742262179,2.5662139770134,10.5713320220547));
#29599=CARTESIAN_POINT('Ctrl Pts',(-14.0281517405305,10.341153921307,-10.5713320220547));
#29600=CARTESIAN_POINT('Ctrl Pts',(-14.5051492284884,9.69408946487939,-3.52377734068488));
#29601=CARTESIAN_POINT('Ctrl Pts',(-14.9373026246845,9.01397331881982,3.5237773406849));
#29602=CARTESIAN_POINT('Ctrl Pts',(-15.3204862161389,8.30729846463996,10.5713320220547));
#29603=CARTESIAN_POINT('Ctrl Pts',(-14.027844693657,10.3409239236334,-10.5713320220547));
#29604=CARTESIAN_POINT('Ctrl Pts',(-14.5048315727105,9.69387363009204,-3.52377734068488));
#29605=CARTESIAN_POINT('Ctrl Pts',(-14.9369753415466,9.01377238202311,3.52377734068489));
#29606=CARTESIAN_POINT('Ctrl Pts',(-15.3201503790965,8.30711301870881,10.5713320220547));
#29607=CARTESIAN_POINT('Ctrl Pts',(-14.0275376467855,10.3406939259613,-10.5713320220547));
#29608=CARTESIAN_POINT('Ctrl Pts',(-14.5045139169348,9.69365779530625,-3.52377734068488));
#29609=CARTESIAN_POINT('Ctrl Pts',(-14.936648058411,9.01357144522771,3.52377734068489));
#29610=CARTESIAN_POINT('Ctrl Pts',(-15.3198145420564,8.30692757277895,10.5713320220547));
#29611=CARTESIAN_POINT('Ctrl Pts',(-14.0272305999403,10.34046392831,-10.5713320220547));
#29612=CARTESIAN_POINT('Ctrl Pts',(-14.5041962611863,9.69344196054,-3.52377734068488));
#29613=CARTESIAN_POINT('Ctrl Pts',(-14.9363207753034,9.01337050845064,3.5237773406849));
#29614=CARTESIAN_POINT('Ctrl Pts',(-15.3194787050451,8.30674212686605,10.5713320220547));
#29615=CARTESIAN_POINT('Ctrl Pts',(-14.0282296344247,10.3410482545552,-10.5701811473657));
#29616=CARTESIAN_POINT('Ctrl Pts',(-14.5051703113035,9.69405064458536,-3.52339371578857));
#29617=CARTESIAN_POINT('Ctrl Pts',(-14.93727643549,9.0140088944632,3.52339371578858));
#29618=CARTESIAN_POINT('Ctrl Pts',(-15.3204236413258,8.30741386530686,10.5701811473657));
#29619=CARTESIAN_POINT('Ctrl Pts',(-14.0272305999403,10.3404639283101,-10.5713320220547));
#29620=CARTESIAN_POINT('Ctrl Pts',(-14.5041962611863,9.69344196054001,-3.52377734068488));
#29621=CARTESIAN_POINT('Ctrl Pts',(-14.9363207753034,9.01337050845065,3.52377734068489));
#29622=CARTESIAN_POINT('Ctrl Pts',(-15.3194787050451,8.30674212686606,10.5713320220547));
#29623=CARTESIAN_POINT('Ctrl Pts',(-9.6452677275233,14.5154164991539,-10.5713320220547));
#29624=CARTESIAN_POINT('Ctrl Pts',(-10.314807825219,14.0705175534734,-3.52377734068489));
#29625=CARTESIAN_POINT('Ctrl Pts',(-10.9535126044255,13.5792225962495,3.52377734068488));
#29626=CARTESIAN_POINT('Ctrl Pts',(-11.5552844326327,13.046221957351,10.5713320220547));
#29627=CARTESIAN_POINT('Ctrl Pts',(-9.6450578616793,14.5150953558215,-10.5713320220547));
#29628=CARTESIAN_POINT('Ctrl Pts',(-10.3145831462735,14.0702060904417,-3.52377734068488));
#29629=CARTESIAN_POINT('Ctrl Pts',(-10.9532737833079,13.5789218399987,3.52377734068487));
#29630=CARTESIAN_POINT('Ctrl Pts',(-11.5550322752861,13.0459328321446,10.5713320220547));
#29631=CARTESIAN_POINT('Ctrl Pts',(-9.64484799583676,14.5147742124914,-10.5713320220547));
#29632=CARTESIAN_POINT('Ctrl Pts',(-10.3143584673296,14.0698946274124,-3.5237773406849));
#29633=CARTESIAN_POINT('Ctrl Pts',(-10.9530349621921,13.5786210837499,3.52377734068489));
#29634=CARTESIAN_POINT('Ctrl Pts',(-11.5547801179413,13.0456437069403,10.5713320220547));
#29635=CARTESIAN_POINT('Ctrl Pts',(-9.64463813001165,14.5144530691896,-10.5713320220547));
#29636=CARTESIAN_POINT('Ctrl Pts',(-10.3141337884043,14.0695831644105,-3.52377734068489));
#29637=CARTESIAN_POINT('Ctrl Pts',(-10.9527961410962,13.5783203275278,3.52377734068488));
#29638=CARTESIAN_POINT('Ctrl Pts',(-11.5545279606177,13.0453545817615,10.5713320220547));
#29639=CARTESIAN_POINT('Ctrl Pts',(-9.64537706399843,14.5153438461678,-10.5701811473657));
#29640=CARTESIAN_POINT('Ctrl Pts',(-10.3148409139074,14.070488285077,-3.52339371578857));
#29641=CARTESIAN_POINT('Ctrl Pts',(-10.953475827046,13.579247069187,3.52339371578858));
#29642=CARTESIAN_POINT('Ctrl Pts',(-11.55518616219,13.0463089966596,10.5701811473657));
#29643=CARTESIAN_POINT('Ctrl Pts',(-9.64463813001165,14.5144530691896,-10.5713320220547));
#29644=CARTESIAN_POINT('Ctrl Pts',(-10.3141337884043,14.0695831644105,-3.52377734068489));
#29645=CARTESIAN_POINT('Ctrl Pts',(-10.9527961410962,13.5783203275278,3.52377734068488));
#29646=CARTESIAN_POINT('Ctrl Pts',(-11.5545279606177,13.0453545817615,10.5713320220547));
#29647=CARTESIAN_POINT('Ctrl Pts',(-4.09902207758572,16.9389056224709,-10.5713320220547));
#29648=CARTESIAN_POINT('Ctrl Pts',(-4.88034836787776,16.7498335663957,-3.52377734068489));
#29649=CARTESIAN_POINT('Ctrl Pts',(-5.64856730744365,16.5066172205901,3.5237773406849));
#29650=CARTESIAN_POINT('Ctrl Pts',(-6.39634480871554,16.2115785402758,10.5713320220547));
#29651=CARTESIAN_POINT('Ctrl Pts',(-4.09893470568933,16.9385320681052,-10.5713320220547));
#29652=CARTESIAN_POINT('Ctrl Pts',(-4.88024376536137,16.749464042158,-3.52377734068488));
#29653=CARTESIAN_POINT('Ctrl Pts',(-5.6484457536978,16.5062529205276,3.52377734068489));
#29654=CARTESIAN_POINT('Ctrl Pts',(-6.39620674496223,16.211220608561,10.5713320220547));
#29655=CARTESIAN_POINT('Ctrl Pts',(-4.09884733379353,16.9381585137421,-10.5713320220547));
#29656=CARTESIAN_POINT('Ctrl Pts',(-4.8801391628456,16.7490945179231,-3.5237773406849));
#29657=CARTESIAN_POINT('Ctrl Pts',(-5.64832419995286,16.5058886204678,3.52377734068491));
#29658=CARTESIAN_POINT('Ctrl Pts',(-6.39606868120986,16.2108626768488,10.5713320220547));
#29659=CARTESIAN_POINT('Ctrl Pts',(-4.09875996190443,16.9377849594116,-10.5713320220547));
#29660=CARTESIAN_POINT('Ctrl Pts',(-4.88003456033808,16.7487249937203,-3.52377734068489));
#29661=CARTESIAN_POINT('Ctrl Pts',(-5.64820264621756,16.5055243204397,3.5237773406849));
#29662=CARTESIAN_POINT('Ctrl Pts',(-6.39593061746862,16.2105047451678,10.5713320220547));
#29663=CARTESIAN_POINT('Ctrl Pts',(-4.09914966904931,16.9388747462729,-10.5701811473657));
#29664=CARTESIAN_POINT('Ctrl Pts',(-4.88038947145514,16.7498173800975,-3.52339371578857));
#29665=CARTESIAN_POINT('Ctrl Pts',(-5.64852437777395,16.5066276390242,3.52339371578857));
#29666=CARTESIAN_POINT('Ctrl Pts',(-6.39622269550887,16.2116267200009,10.5701811473657));
#29667=CARTESIAN_POINT('Ctrl Pts',(-4.09875996190443,16.9377849594116,-10.5713320220547));
#29668=CARTESIAN_POINT('Ctrl Pts',(-4.88003456033808,16.7487249937203,-3.52377734068489));
#29669=CARTESIAN_POINT('Ctrl Pts',(-5.64820264621756,16.5055243204397,3.5237773406849));
#29670=CARTESIAN_POINT('Ctrl Pts',(-6.39593061746862,16.2105047451678,10.5713320220547));
#29671=CARTESIAN_POINT('Ctrl Pts',(1.94162613003165,17.3193127360958,-10.5713320220547));
#29672=CARTESIAN_POINT('Ctrl Pts',(1.14275312890046,17.4088724499949,-3.52377734068488));
#29673=CARTESIAN_POINT('Ctrl Pts',(0.337678570790843,17.4430701964027,3.52377734068491));
#29674=CARTESIAN_POINT('Ctrl Pts',(-0.465911600871794,17.4215794938256,
10.5713320220547));
#29675=CARTESIAN_POINT('Ctrl Pts',(1.94158046964025,17.3189318268663,-10.5713320220547));
#29676=CARTESIAN_POINT('Ctrl Pts',(1.14272503838051,17.4084894346279,-3.52377734068488));
#29677=CARTESIAN_POINT('Ctrl Pts',(0.337668195989281,17.4426862924926,3.52377734068491));
#29678=CARTESIAN_POINT('Ctrl Pts',(-0.465904283238001,17.4211959274498,
10.5713320220547));
#29679=CARTESIAN_POINT('Ctrl Pts',(1.94153480924917,17.3185509176394,-10.5713320220547));
#29680=CARTESIAN_POINT('Ctrl Pts',(1.14269694786086,17.4081064192635,-3.52377734068488));
#29681=CARTESIAN_POINT('Ctrl Pts',(0.337657821187732,17.4423023885852,3.52377734068491));
#29682=CARTESIAN_POINT('Ctrl Pts',(-0.465896965604222,17.4208123610765,
10.5713320220547));
#29683=CARTESIAN_POINT('Ctrl Pts',(1.94148914886299,17.3181700084457,-10.5713320220547));
#29684=CARTESIAN_POINT('Ctrl Pts',(1.14266885734454,17.4077234039326,-3.52377734068488));
#29685=CARTESIAN_POINT('Ctrl Pts',(0.33764744638803,17.4419184847113,3.52377734068491));
#29686=CARTESIAN_POINT('Ctrl Pts',(-0.465889647970186,17.4204287947368,
10.5713320220547));
#29687=CARTESIAN_POINT('Ctrl Pts',(1.94149567299317,17.319327360811,-10.5701811473657));
#29688=CARTESIAN_POINT('Ctrl Pts',(1.14270896813208,17.4088712981013,-3.52339371578857));
#29689=CARTESIAN_POINT('Ctrl Pts',(0.337722474799024,17.4430653037166,3.52339371578858));
#29690=CARTESIAN_POINT('Ctrl Pts',(-0.465780373556106,17.4215830027813,
10.5701811473657));
#29691=CARTESIAN_POINT('Ctrl Pts',(1.941489148863,17.3181700084458,-10.5713320220547));
#29692=CARTESIAN_POINT('Ctrl Pts',(1.14266885734455,17.4077234039326,-3.52377734068489));
#29693=CARTESIAN_POINT('Ctrl Pts',(0.337647446388033,17.4419184847113,3.52377734068488));
#29694=CARTESIAN_POINT('Ctrl Pts',(-0.465889647970182,17.4204287947368,
10.5713320220547));
#29695=CARTESIAN_POINT('Ctrl Pts',(7.74808557101742,15.6107551279143,-10.5713320220547));
#29696=CARTESIAN_POINT('Ctrl Pts',(7.02802173309331,15.9681443885309,-3.52377734068488));
#29697=CARTESIAN_POINT('Ctrl Pts',(6.28319542978303,16.2756314742303,3.52377734068489));
#29698=CARTESIAN_POINT('Ctrl Pts',(5.52071742216,16.5302808452903,10.5713320220547));
#29699=CARTESIAN_POINT('Ctrl Pts',(7.7479123856553,15.6104128070958,-10.5713320220547));
#29700=CARTESIAN_POINT('Ctrl Pts',(7.0278643376683,15.9677940793406,-3.52377734068488));
#29701=CARTESIAN_POINT('Ctrl Pts',(6.28305437778823,16.2752742709501,3.52377734068488));
#29702=CARTESIAN_POINT('Ctrl Pts',(5.52059311105964,16.5299179080192,10.5713320220547));
#29703=CARTESIAN_POINT('Ctrl Pts',(7.74773920029438,15.6100704862796,-10.5713320220547));
#29704=CARTESIAN_POINT('Ctrl Pts',(7.02770694224446,15.9674437701526,-3.52377734068489));
#29705=CARTESIAN_POINT('Ctrl Pts',(6.28291332579435,16.2749170676723,3.52377734068489));
#29706=CARTESIAN_POINT('Ctrl Pts',(5.52046879996016,16.5295549707505,10.5713320220547));
#29707=CARTESIAN_POINT('Ctrl Pts',(7.74756601494938,15.6097281654929,-10.5713320220547));
#29708=CARTESIAN_POINT('Ctrl Pts',(7.02754954683516,15.9670934609948,-3.52377734068488));
#29709=CARTESIAN_POINT('Ctrl Pts',(6.28277227381364,16.2745598644254,3.52377734068489));
#29710=CARTESIAN_POINT('Ctrl Pts',(5.52034448887238,16.5291920335133,10.5713320220547));
#29711=CARTESIAN_POINT('Ctrl Pts',(7.74796798344821,15.6108134895863,-10.5701811473657));
#29712=CARTESIAN_POINT('Ctrl Pts',(7.02797984157433,15.9681584099774,-3.52339371578857));
#29713=CARTESIAN_POINT('Ctrl Pts',(6.28323501265834,16.2756118605541,3.52339371578857));
#29714=CARTESIAN_POINT('Ctrl Pts',(5.52084193563372,16.5302392602447,10.5701811473657));
#29715=CARTESIAN_POINT('Ctrl Pts',(7.74756601494938,15.6097281654929,-10.5713320220547));
#29716=CARTESIAN_POINT('Ctrl Pts',(7.02754954683516,15.9670934609948,-3.52377734068488));
#29717=CARTESIAN_POINT('Ctrl Pts',(6.28277227381364,16.2745598644254,3.52377734068488));
#29718=CARTESIAN_POINT('Ctrl Pts',(5.52034448887238,16.5291920335133,10.5713320220547));
#29719=CARTESIAN_POINT('Ctrl Pts',(12.620011542574,12.019310061098,-10.5713320220547));
#29720=CARTESIAN_POINT('Ctrl Pts',(12.0656071937211,12.6014224490979,-3.52377734068488));
#29721=CARTESIAN_POINT('Ctrl Pts',(11.4708661898549,13.1451113935275,3.5237773406849));
#29722=CARTESIAN_POINT('Ctrl Pts',(10.8414664469677,13.6451863658503,10.5713320220547));
#29723=CARTESIAN_POINT('Ctrl Pts',(12.6197317209518,12.0190476176333,-10.5713320220547));
#29724=CARTESIAN_POINT('Ctrl Pts',(12.0653394776022,12.6011470985426,-3.52377734068489));
#29725=CARTESIAN_POINT('Ctrl Pts',(11.4706114736191,13.1448239748645,3.5237773406849));
#29726=CARTESIAN_POINT('Ctrl Pts',(10.8412255008865,13.6448878332752,10.5713320220547));
#29727=CARTESIAN_POINT('Ctrl Pts',(12.6194518993315,12.0187851741703,-10.5713320220547));
#29728=CARTESIAN_POINT('Ctrl Pts',(12.0650717614851,12.600871747989,-3.52377734068487));
#29729=CARTESIAN_POINT('Ctrl Pts',(11.470356757385,13.1445365562033,3.52377734068489));
#29730=CARTESIAN_POINT('Ctrl Pts',(10.840984554807,13.644589300702,10.5713320220547));
#29731=CARTESIAN_POINT('Ctrl Pts',(12.6191720777362,12.0185227307296,-10.5713320220547));
#29732=CARTESIAN_POINT('Ctrl Pts',(12.0648040453922,12.600596397459,-3.52377734068488));
#29733=CARTESIAN_POINT('Ctrl Pts',(11.4701020411739,13.1442491375668,3.5237773406849));
#29734=CARTESIAN_POINT('Ctrl Pts',(10.8407436087492,13.6442907681545,10.5713320220547));
#29735=CARTESIAN_POINT('Ctrl Pts',(12.6199210072703,12.0194051204477,-10.5701811473657));
#29736=CARTESIAN_POINT('Ctrl Pts',(12.065572624187,12.601449952691,-3.52339371578857));
#29737=CARTESIAN_POINT('Ctrl Pts',(11.4708966773184,13.1450794245601,3.52339371578857));
#29738=CARTESIAN_POINT('Ctrl Pts',(10.8415692284369,13.6451047025737,10.5701811473657));
#29739=CARTESIAN_POINT('Ctrl Pts',(12.6191720777363,12.0185227307296,-10.5713320220547));
#29740=CARTESIAN_POINT('Ctrl Pts',(12.0648040453922,12.600596397459,-3.52377734068488));
#29741=CARTESIAN_POINT('Ctrl Pts',(11.4701020411739,13.1442491375668,3.52377734068489));
#29742=CARTESIAN_POINT('Ctrl Pts',(10.8407436087492,13.6442907681545,10.5713320220547));
#29743=CARTESIAN_POINT('Ctrl Pts',(15.9697778705622,6.97815881478883,-10.5713320220547));
#29744=CARTESIAN_POINT('Ctrl Pts',(15.6479023573888,7.71478298511549,-3.52377734068488));
#29745=CARTESIAN_POINT('Ctrl Pts',(15.2749811954754,8.42909687758284,3.52377734068489));
#29746=CARTESIAN_POINT('Ctrl Pts',(14.8545746152671,9.11428102918567,10.5713320220547));
#29747=CARTESIAN_POINT('Ctrl Pts',(15.9694251632972,6.97800790323301,-10.5713320220547));
#29748=CARTESIAN_POINT('Ctrl Pts',(15.647556611091,7.7146158045359,-3.52377734068489));
#29749=CARTESIAN_POINT('Ctrl Pts',(15.2746435375359,8.42891391046955,3.5237773406849));
#29750=CARTESIAN_POINT('Ctrl Pts',(14.8542460958585,9.11408290874099,10.5713320220547));
#29751=CARTESIAN_POINT('Ctrl Pts',(15.9690724560348,6.9778569916782,-10.5713320220547));
#29752=CARTESIAN_POINT('Ctrl Pts',(15.6472108647957,7.71444862395735,-3.52377734068488));
#29753=CARTESIAN_POINT('Ctrl Pts',(15.2743058795988,8.42873094335758,3.52377734068489));
#29754=CARTESIAN_POINT('Ctrl Pts',(14.8539175764522,9.11388478829766,10.5713320220547));
#29755=CARTESIAN_POINT('Ctrl Pts',(15.9687197488033,6.97770608013569,-10.5713320220547));
#29756=CARTESIAN_POINT('Ctrl Pts',(15.6468651185308,7.71428144339258,-3.52377734068488));
#29757=CARTESIAN_POINT('Ctrl Pts',(15.2739682216914,8.42854797626068,3.52377734068489));
#29758=CARTESIAN_POINT('Ctrl Pts',(14.8535890570749,9.11368666787079,10.5713320220547));
#29759=CARTESIAN_POINT('Ctrl Pts',(15.9697253074178,6.97827910625586,-10.5701811473657));
#29760=CARTESIAN_POINT('Ctrl Pts',(15.6478792794356,7.71482065351598,-3.52339371578857));
#29761=CARTESIAN_POINT('Ctrl Pts',(15.274998910289,8.42905640925339,3.52339371578857));
#29762=CARTESIAN_POINT('Ctrl Pts',(14.8546432677697,9.11416913747444,10.5701811473657));
#29763=CARTESIAN_POINT('Ctrl Pts',(15.9687197488033,6.97770608013569,-10.5713320220547));
#29764=CARTESIAN_POINT('Ctrl Pts',(15.6468651185308,7.71428144339258,-3.52377734068488));
#29765=CARTESIAN_POINT('Ctrl Pts',(15.2739682216914,8.42854797626069,3.52377734068489));
#29766=CARTESIAN_POINT('Ctrl Pts',(14.8535890570749,9.11368666787079,10.5713320220547));
#29767=CARTESIAN_POINT('Ctrl Pts',(17.3933532985407,1.09533862876043,-10.5713320220547));
#29768=CARTESIAN_POINT('Ctrl Pts',(17.3428295583123,1.89762683505751,-3.52377734068489));
#29769=CARTESIAN_POINT('Ctrl Pts',(17.2367080342085,2.69640887798077,3.52377734068489));
#29770=CARTESIAN_POINT('Ctrl Pts',(17.0760018547927,3.48405888793926,10.5713320220547));
#29771=CARTESIAN_POINT('Ctrl Pts',(17.3929702473346,1.09531745127435,-10.5713320220547));
#29772=CARTESIAN_POINT('Ctrl Pts',(17.3424474839418,1.89758798889885,-3.5237773406849));
#29773=CARTESIAN_POINT('Ctrl Pts',(17.2363281610961,2.69635243095141,3.5237773406849));
#29774=CARTESIAN_POINT('Ctrl Pts',(17.0756253863458,3.48398507587458,10.5713320220547));
#29775=CARTESIAN_POINT('Ctrl Pts',(17.3925871961311,1.09529627378836,-10.5713320220547));
#29776=CARTESIAN_POINT('Ctrl Pts',(17.342065409574,1.89754914274033,-3.52377734068488));
#29777=CARTESIAN_POINT('Ctrl Pts',(17.2359482879864,2.69629598392249,3.52377734068488));
#29778=CARTESIAN_POINT('Ctrl Pts',(17.0752489179014,3.48391126381038,10.5713320220547));
#29779=CARTESIAN_POINT('Ctrl Pts',(17.392204144961,1.09527509630334,-10.5713320220547));
#29780=CARTESIAN_POINT('Ctrl Pts',(17.3416833352395,1.89751029658436,-3.52377734068489));
#29781=CARTESIAN_POINT('Ctrl Pts',(17.2355684149098,2.69623953689756,3.52377734068489));
#29782=CARTESIAN_POINT('Ctrl Pts',(17.07487244949,3.48383745175174,10.5713320220547));
#29783=CARTESIAN_POINT('Ctrl Pts',(17.3933450474466,1.09546964341852,-10.5701811473657));
#29784=CARTESIAN_POINT('Ctrl Pts',(17.3428207554817,1.89767012490037,-3.52339371578856));
#29785=CARTESIAN_POINT('Ctrl Pts',(17.2367108397044,2.6963647913671,3.52339371578857));
#29786=CARTESIAN_POINT('Ctrl Pts',(17.0760280978237,3.48393026358512,10.5701811473657));
#29787=CARTESIAN_POINT('Ctrl Pts',(17.392204144961,1.09527509630334,-10.5713320220547));
#29788=CARTESIAN_POINT('Ctrl Pts',(17.3416833352395,1.89751029658436,-3.52377734068489));
#29789=CARTESIAN_POINT('Ctrl Pts',(17.2355684149098,2.69623953689757,3.52377734068489));
#29790=CARTESIAN_POINT('Ctrl Pts',(17.07487244949,3.48383745175174,10.5713320220547));
#29791=CARTESIAN_POINT('Ctrl Pts',(15.5239408288993,-7.92059131757518,-10.5701811473657));
#29792=CARTESIAN_POINT('Ctrl Pts',(15.8892473389622,-7.20460984356022,-3.52339371578857));
#29793=CARTESIAN_POINT('Ctrl Pts',(16.2049399509463,-6.46331998146985,3.52339371578857));
#29794=CARTESIAN_POINT('Ctrl Pts',(16.4680054423355,-5.70379719401242,10.5701811473657));
#29795=CARTESIAN_POINT('Ctrl Pts',(15.5298720746603,-7.92356091115868,-10.5701811473657));
#29796=CARTESIAN_POINT('Ctrl Pts',(15.8953265065073,-7.20730043136479,-3.52339371578857));
#29797=CARTESIAN_POINT('Ctrl Pts',(16.2111160582657,-6.46573988486005,3.52339371578858));
#29798=CARTESIAN_POINT('Ctrl Pts',(16.4742895766427,-5.70592035635592,10.5701811473657));
#29799=CARTESIAN_POINT('Ctrl Pts',(15.5915703928396,-7.95274424871187,-10.5701811473657));
#29800=CARTESIAN_POINT('Ctrl Pts',(15.9583566411062,-7.23364522935241,-3.52339371578857));
#29801=CARTESIAN_POINT('Ctrl Pts',(16.2753221711908,-6.4891298445003,3.52339371578857));
#29802=CARTESIAN_POINT('Ctrl Pts',(16.5394232800143,-5.72631521703215,10.5701811473657));
#29803=CARTESIAN_POINT('Ctrl Pts',(15.8812835900794,-8.05295157643048,-10.5701811473657));
#29804=CARTESIAN_POINT('Ctrl Pts',(16.2527035030447,-7.32048471228393,-3.52339371578857));
#29805=CARTESIAN_POINT('Ctrl Pts',(16.5733417616638,-6.56230076343565,3.52339371578858));
#29806=CARTESIAN_POINT('Ctrl Pts',(16.8401885277462,-5.78560696131593,10.5701811473657));
#29807=CARTESIAN_POINT('Ctrl Pts',(16.634287410633,-8.21708494426133,-10.5701811473657));
#29808=CARTESIAN_POINT('Ctrl Pts',(17.013264495319,-7.44989503894739,-3.52339371578857));
#29809=CARTESIAN_POINT('Ctrl Pts',(17.3390909478701,-6.65644300411585,3.52339371578858));
#29810=CARTESIAN_POINT('Ctrl Pts',(17.6086335808629,-5.84431570465351,10.5701811473657));
#29811=CARTESIAN_POINT('Ctrl Pts',(17.5952076964926,-8.2428856289747,-10.5701811473657));
#29812=CARTESIAN_POINT('Ctrl Pts',(17.9754084721853,-7.43136071700242,-3.52339371578857));
#29813=CARTESIAN_POINT('Ctrl Pts',(18.2992890487802,-6.59354486117992,3.52339371578857));
#29814=CARTESIAN_POINT('Ctrl Pts',(18.5639288924223,-5.73733748808268,10.5701811473657));
#29815=CARTESIAN_POINT('Ctrl Pts',(18.2493498865067,-8.18298767653124,-10.5701811473657));
#29816=CARTESIAN_POINT('Ctrl Pts',(18.6267584093738,-7.34130729556355,-3.52339371578857));
#29817=CARTESIAN_POINT('Ctrl Pts',(18.9458430528698,-6.47348072287577,3.52339371578857));
#29818=CARTESIAN_POINT('Ctrl Pts',(19.2035582177828,-5.58779118888971,10.5701811473657));
#29819=CARTESIAN_POINT('Ctrl Pts',(15.5239408288993,-7.92059131757518,-10.5701811473657));
#29820=CARTESIAN_POINT('Ctrl Pts',(15.8892473389622,-7.20460984356022,-3.52339371578857));
#29821=CARTESIAN_POINT('Ctrl Pts',(16.2049399509463,-6.46331998146985,3.52339371578857));
#29822=CARTESIAN_POINT('Ctrl Pts',(16.4680054423355,-5.70379719401242,10.5701811473657));
#29823=CARTESIAN_POINT('Origin',(-1078.88931916128,445.504381323311,-6.00190077337249));
#29824=CARTESIAN_POINT('Origin',(-1110.51158560065,359.500118245023,6.00190077400118));
#29825=CARTESIAN_POINT('Ctrl Pts',(18.8787605016016,-6.60245423484101,-10.5701811473657));
#29826=CARTESIAN_POINT('Ctrl Pts',(19.1832730585148,-5.73174473391652,-3.52339371578857));
#29827=CARTESIAN_POINT('Ctrl Pts',(19.4274506997862,-4.83994031365006,3.52339371578858));
#29828=CARTESIAN_POINT('Ctrl Pts',(19.6089627989182,-3.93555306794902,10.5701811473657));
#29829=CARTESIAN_POINT('Ctrl Pts',(18.3002407630201,-5.94487823810955,-10.5701811473657));
#29830=CARTESIAN_POINT('Ctrl Pts',(18.5743713266435,-5.10071352016191,-3.52339371578857));
#29831=CARTESIAN_POINT('Ctrl Pts',(18.7901959736259,-4.23795805225981,3.52339371578858));
#29832=CARTESIAN_POINT('Ctrl Pts',(18.9452775557869,-3.36405225652747,10.5701811473657));
#29833=CARTESIAN_POINT('Ctrl Pts',(17.5094185149336,-5.30743865086107,-10.5701811473657));
#29834=CARTESIAN_POINT('Ctrl Pts',(17.7541962099834,-4.49986483819949,-3.52339371578858));
#29835=CARTESIAN_POINT('Ctrl Pts',(17.9430400877725,-3.6753928330489,3.52339371578858));
#29836=CARTESIAN_POINT('Ctrl Pts',(18.0740960265747,-2.84177666010401,10.5701811473657));
#29837=CARTESIAN_POINT('Ctrl Pts',(16.8624899954198,-4.96810854518302,-10.5701811473657));
#29838=CARTESIAN_POINT('Ctrl Pts',(17.0916172376515,-4.19037035031441,-3.52339371578857));
#29839=CARTESIAN_POINT('Ctrl Pts',(17.2668789301514,-3.39682252271119,3.52339371578857));
#29840=CARTESIAN_POINT('Ctrl Pts',(17.3865489833807,-2.59491537643409,10.5701811473657));
#29841=CARTESIAN_POINT('Ctrl Pts',(16.7285940831805,-4.92235069975673,-10.5701811473657));
#29842=CARTESIAN_POINT('Ctrl Pts',(16.9555961741675,-4.15074972008885,-3.52339371578857));
#29843=CARTESIAN_POINT('Ctrl Pts',(17.1292100097174,-3.36359754540394,3.52339371578857));
#29844=CARTESIAN_POINT('Ctrl Pts',(17.2476216804283,-2.56806206701449,10.5701811473657));
#29845=CARTESIAN_POINT('Ctrl Pts',(16.7190706763204,-4.91946962582535,-10.5701811473657));
#29846=CARTESIAN_POINT('Ctrl Pts',(16.9459621050428,-4.14836742961574,-3.52339371578857));
#29847=CARTESIAN_POINT('Ctrl Pts',(17.1194210645505,-3.3615482164125,3.52339371578858));
#29848=CARTESIAN_POINT('Ctrl Pts',(17.2377919239465,-2.56652201742733,10.5701811473657));
#29849=CARTESIAN_POINT('Origin',(-1137.04624834432,263.822186184469,6.0019007738112));
#29850=CARTESIAN_POINT('Origin',(-1112.84749639278,352.202734986488,-6.00190077339977));
#29851=CARTESIAN_POINT('Ctrl Pts',(18.3844122993175,-7.87485773895016,-8.00000002680495));
#29852=CARTESIAN_POINT('Ctrl Pts',(18.4531333976134,-7.71442347504144,-6.66666668453664));
#29853=CARTESIAN_POINT('Ctrl Pts',(18.5197542958142,-7.55308960393423,-5.33333334226832));
#29854=CARTESIAN_POINT('Ctrl Pts',(18.5842521656445,-7.39091140819174,-4.));
#29855=CARTESIAN_POINT('Ctrl Pts',(18.6077644958072,-7.35342624084015,-8.00000002680495));
#29856=CARTESIAN_POINT('Ctrl Pts',(18.6719352556694,-7.19104283587996,-6.66666668453664));
#29857=CARTESIAN_POINT('Ctrl Pts',(18.7339802713311,-7.02781946759158,-5.33333334226832));
#29858=CARTESIAN_POINT('Ctrl Pts',(18.7938783394501,-6.86381191269435,-4.));
#29859=CARTESIAN_POINT('Ctrl Pts',(18.8089193180918,-6.8224871635213,-8.00000002680495));
#29860=CARTESIAN_POINT('Ctrl Pts',(18.8684567600673,-6.65834835144208,-6.66666668453663));
#29861=CARTESIAN_POINT('Ctrl Pts',(18.9258454793725,-6.49343022987757,-5.33333334226832));
#29862=CARTESIAN_POINT('Ctrl Pts',(18.9810658661254,-6.32778915551913,-4.));
#29863=CARTESIAN_POINT('Ctrl Pts',(18.9871493773879,-6.2839604168677,-8.00000002680495));
#29864=CARTESIAN_POINT('Ctrl Pts',(19.041987277425,-6.11826627965564,-6.66666668453664));
#29865=CARTESIAN_POINT('Ctrl Pts',(19.0946561219624,-5.9518542763067,-5.33333334226832));
#29866=CARTESIAN_POINT('Ctrl Pts',(19.1451378635268,-5.78478142945372,-4.));
#29867=CARTESIAN_POINT('Ctrl Pts',(18.9455935099938,-6.40815781282579,4.));
#29868=CARTESIAN_POINT('Ctrl Pts',(19.0015152367791,-6.24282631897105,5.33333334226731));
#29869=CARTESIAN_POINT('Ctrl Pts',(19.0552726553178,-6.07676277090729,6.66666668453462));
#29870=CARTESIAN_POINT('Ctrl Pts',(19.1068473451265,-5.91002407186587,8.00000002680193));
#29871=CARTESIAN_POINT('Ctrl Pts',(19.1273461422817,-5.87080970260819,4.));
#29872=CARTESIAN_POINT('Ctrl Pts',(19.1785786299635,-5.70389209169295,5.33333334226731));
#29873=CARTESIAN_POINT('Ctrl Pts',(19.2276260236414,-5.53630389074425,6.66666668453462));
#29874=CARTESIAN_POINT('Ctrl Pts',(19.2744715615271,-5.36810236813545,8.00000002680193));
#29875=CARTESIAN_POINT('Ctrl Pts',(19.2862238713926,-5.32572490778714,4.));
#29876=CARTESIAN_POINT('Ctrl Pts',(19.332699596505,-5.15742082701962,5.33333334226731));
#29877=CARTESIAN_POINT('Ctrl Pts',(19.3769720788243,-4.98850842595596,6.66666668453462));
#29878=CARTESIAN_POINT('Ctrl Pts',(19.4190261906145,-4.81904542613222,8.00000002680193));
#29879=CARTESIAN_POINT('Ctrl Pts',(19.4216521852328,-4.7748744900616,4.));
#29880=CARTESIAN_POINT('Ctrl Pts',(19.4633208261226,-4.60538860052123,5.33333334226731));
#29881=CARTESIAN_POINT('Ctrl Pts',(19.5027707748587,-4.43535723991919,6.66666668453462));
#29882=CARTESIAN_POINT('Ctrl Pts',(19.5399885135466,-4.26483867109501,8.00000002680193));
#29883=CARTESIAN_POINT('Ctrl Pts',(11.8787308647727,-12.7524216806657,-10.5701811473657));
#29884=CARTESIAN_POINT('Ctrl Pts',(12.4668867829649,-12.2045613578439,-3.52339371578857));
#29885=CARTESIAN_POINT('Ctrl Pts',(13.017076865761,-11.6159499769718,3.52339371578858));
#29886=CARTESIAN_POINT('Ctrl Pts',(13.5240496594282,-10.9922057153483,10.5701811473657));
#29887=CARTESIAN_POINT('Ctrl Pts',(11.8855676953483,-12.7596503467191,-10.5701811473657));
#29888=CARTESIAN_POINT('Ctrl Pts',(12.4741202082517,-12.211467931193,-3.52339371578857));
#29889=CARTESIAN_POINT('Ctrl Pts',(13.0244969705684,-11.6225403214586,3.52339371578858));
#29890=CARTESIAN_POINT('Ctrl Pts',(13.5318181449491,-10.9984223461031,10.5701811473657));
#29891=CARTESIAN_POINT('Ctrl Pts',(11.9863857707243,-12.8589190332262,-10.5701811473657));
#29892=CARTESIAN_POINT('Ctrl Pts',(12.5794765862922,-12.3060905992801,-3.52339371578857));
#29893=CARTESIAN_POINT('Ctrl Pts',(13.1341887566198,-11.7121827924549,3.52339371578858));
#29894=CARTESIAN_POINT('Ctrl Pts',(13.6453640718532,-11.0828372673367,10.5701811473657));
#29895=CARTESIAN_POINT('Ctrl Pts',(12.5792608243648,-13.285711771797,-10.5701811473657));
#29896=CARTESIAN_POINT('Ctrl Pts',(13.1920348426239,-12.7055397408982,-3.52339371578857));
#29897=CARTESIAN_POINT('Ctrl Pts',(13.7645381666776,-12.0829230390925,3.52339371578858));
#29898=CARTESIAN_POINT('Ctrl Pts',(14.2914372818011,-11.4237804859428,10.5701811473657));
#29899=CARTESIAN_POINT('Ctrl Pts',(13.5031269323654,-13.7078792049972,-10.5701811473657));
#29900=CARTESIAN_POINT('Ctrl Pts',(14.1354964096488,-13.0850867185779,-3.52339371578858));
#29901=CARTESIAN_POINT('Ctrl Pts',(14.7242713589907,-12.4185498968891,3.52339371578858));
#29902=CARTESIAN_POINT('Ctrl Pts',(15.264700349594,-11.7144915590678,10.5701811473657));
#29903=CARTESIAN_POINT('Ctrl Pts',(14.3500311789428,-13.9311379708684,-10.5701811473657));
#29904=CARTESIAN_POINT('Ctrl Pts',(14.9925508077551,-13.2692985198616,-3.52339371578857));
#29905=CARTESIAN_POINT('Ctrl Pts',(15.5892064466918,-12.5629417452578,3.52339371578858));
#29906=CARTESIAN_POINT('Ctrl Pts',(16.1343031376281,-11.818809680468,10.5701811473657));
#29907=CARTESIAN_POINT('Ctrl Pts',(11.8787308647727,-12.7524216806657,-10.5701811473657));
#29908=CARTESIAN_POINT('Ctrl Pts',(12.4668867829649,-12.2045613578439,-3.52339371578857));
#29909=CARTESIAN_POINT('Ctrl Pts',(13.017076865761,-11.6159499769718,3.52339371578858));
#29910=CARTESIAN_POINT('Ctrl Pts',(13.5240496594282,-10.9922057153483,10.5701811473657));
#29911=CARTESIAN_POINT('Origin',(-861.45285953215,787.639059256792,-6.00190077325071));
#29912=CARTESIAN_POINT('Origin',(-920.583260311475,717.636939968545,6.00190077196125));
#29913=CARTESIAN_POINT('Ctrl Pts',(15.482059589238,-12.6611938961255,-10.5701811473657));
#29914=CARTESIAN_POINT('Ctrl Pts',(16.0660079802072,-11.9471440316185,-3.52339371578857));
#29915=CARTESIAN_POINT('Ctrl Pts',(16.6004749835089,-11.1926356705744,3.52339371578857));
#29916=CARTESIAN_POINT('Ctrl Pts',(17.0803592190431,-10.4048704436167,10.5701811473657));
#29917=CARTESIAN_POINT('Ctrl Pts',(15.1633330965618,-11.8454091804831,-10.5701811473657));
#29918=CARTESIAN_POINT('Ctrl Pts',(15.7096529021536,-11.1459119989603,-3.52339371578858));
#29919=CARTESIAN_POINT('Ctrl Pts',(16.2075414790933,-10.4090034289244,3.52339371578858));
#29920=CARTESIAN_POINT('Ctrl Pts',(16.6521638829793,-9.64084162637057,10.5701811473657));
#29921=CARTESIAN_POINT('Ctrl Pts',(14.6381973737281,-10.9759350631358,-10.5701811473657));
#29922=CARTESIAN_POINT('Ctrl Pts',(15.1444196786519,-10.3007828129816,-3.52339371578856));
#29923=CARTESIAN_POINT('Ctrl Pts',(15.6038611719969,-9.59062414299819,3.52339371578856));
#29924=CARTESIAN_POINT('Ctrl Pts',(16.0121269935487,-8.85210494768689,10.5701811473657));
#29925=CARTESIAN_POINT('Ctrl Pts',(14.1463497701535,-10.4358061880711,-10.5701811473657));
#29926=CARTESIAN_POINT('Ctrl Pts',(14.6276610777785,-9.78333747767764,-3.52339371578858));
#29927=CARTESIAN_POINT('Ctrl Pts',(15.0637626772863,-9.09759146195833,3.52339371578858));
#29928=CARTESIAN_POINT('Ctrl Pts',(15.4504841403386,-8.38497480280354,10.5701811473657));
#29929=CARTESIAN_POINT('Ctrl Pts',(14.0361933242568,-10.3470127754477,-10.5701811473657));
#29930=CARTESIAN_POINT('Ctrl Pts',(14.5134085917165,-9.69958431635719,-3.52339371578856));
#29931=CARTESIAN_POINT('Ctrl Pts',(14.9457741314539,-9.01928265528841,3.52339371578856));
#29932=CARTESIAN_POINT('Ctrl Pts',(15.3291338629752,-8.31222301326043,10.5701811473657));
#29933=CARTESIAN_POINT('Ctrl Pts',(14.0282296344253,-10.3410482545556,-10.5701811473657));
#29934=CARTESIAN_POINT('Ctrl Pts',(14.5051703193816,-9.6940506498766,-3.52339371578857));
#29935=CARTESIAN_POINT('Ctrl Pts',(14.9372764437114,-9.0140088995289,3.52339371578857));
#29936=CARTESIAN_POINT('Ctrl Pts',(15.3204236413265,-8.30741386530727,10.5701811473657));
#29937=CARTESIAN_POINT('Origin',(-978.241467171257,636.804482391533,6.00190077666473));
#29938=CARTESIAN_POINT('Origin',(-925.274150566318,711.578571311876,-6.00190077008327));
#29939=CARTESIAN_POINT('Ctrl Pts',(14.5823366026094,-13.687785036601,-8.00000002680495));
#29940=CARTESIAN_POINT('Ctrl Pts',(14.7017850615068,-13.5605301425735,-6.66666668453664));
#29941=CARTESIAN_POINT('Ctrl Pts',(14.8195676616555,-13.4317115835623,-5.33333334226832));
#29942=CARTESIAN_POINT('Ctrl Pts',(14.9356440437436,-13.3013735004543,-4.));
#29943=CARTESIAN_POINT('Ctrl Pts',(14.9705590892051,-13.2741906558372,-8.00000002680495));
#29944=CARTESIAN_POINT('Ctrl Pts',(15.0863982741561,-13.1435478609434,-6.66666668453664));
#29945=CARTESIAN_POINT('Ctrl Pts',(15.200527197346,-13.0113887113723,-5.33333334226832));
#29946=CARTESIAN_POINT('Ctrl Pts',(15.3129068573893,-12.8777583681252,-4.));
#29947=CARTESIAN_POINT('Ctrl Pts',(15.3411746506633,-12.8440701239422,-8.00000002680495));
#29948=CARTESIAN_POINT('Ctrl Pts',(15.4532603255808,-12.7101930978845,-6.66666668453664));
#29949=CARTESIAN_POINT('Ctrl Pts',(15.5635934012027,-12.5748488540185,-5.33333334226832));
#29950=CARTESIAN_POINT('Ctrl Pts',(15.6721361751441,-12.4380836433366,-4.));
#29951=CARTESIAN_POINT('Ctrl Pts',(15.6928431172612,-12.3989787844414,-8.00000002680495));
#29952=CARTESIAN_POINT('Ctrl Pts',(15.801044619823,-12.2620328928261,-6.66666668453664));
#29953=CARTESIAN_POINT('Ctrl Pts',(15.9074534016166,-12.1236705670264,-5.33333334226832));
#29954=CARTESIAN_POINT('Ctrl Pts',(16.0120330006756,-11.9839392181901,-4.));
#29955=CARTESIAN_POINT('Ctrl Pts',(15.6113153641544,-12.5014732172219,4.));
#29956=CARTESIAN_POINT('Ctrl Pts',(15.7204112993806,-12.3652387894732,5.33333334226731));
#29957=CARTESIAN_POINT('Ctrl Pts',(15.8277238274038,-12.2275762187696,6.66666668453462));
#29958=CARTESIAN_POINT('Ctrl Pts',(15.9332161765804,-12.0885326764813,8.00000002680193));
#29959=CARTESIAN_POINT('Ctrl Pts',(15.9658908491962,-12.0586942246021,4.));
#29960=CARTESIAN_POINT('Ctrl Pts',(16.0711228250241,-11.9193655201257,5.33333334226731));
#29961=CARTESIAN_POINT('Ctrl Pts',(16.1745308394401,-11.7786593209788,6.66666668453462));
#29962=CARTESIAN_POINT('Ctrl Pts',(16.2760795545783,-11.6366237089603,8.00000002680193));
#29963=CARTESIAN_POINT('Ctrl Pts',(16.3016170584982,-11.6008214488879,4.));
#29964=CARTESIAN_POINT('Ctrl Pts',(16.4028533402584,-11.4585629803066,5.33333334226731));
#29965=CARTESIAN_POINT('Ctrl Pts',(16.5022273088191,-11.3149793242161,6.66666668453462));
#29966=CARTESIAN_POINT('Ctrl Pts',(16.5997050068301,-11.1701195471274,8.00000002680193));
#29967=CARTESIAN_POINT('Ctrl Pts',(16.6172799844809,-11.1295105875044,4.));
#29968=CARTESIAN_POINT('Ctrl Pts',(16.7144032870754,-10.9844974623052,5.33333334226731));
#29969=CARTESIAN_POINT('Ctrl Pts',(16.8096282631161,-10.8382129245663,6.66666668453462));
#29970=CARTESIAN_POINT('Ctrl Pts',(16.9029222828724,-10.6907071000555,8.00000002680193));
#29971=CARTESIAN_POINT('Ctrl Pts',(6.80077064695807,-16.0461217833684,-10.5701811473657));
#29972=CARTESIAN_POINT('Ctrl Pts',(7.54083568928884,-15.7324626522293,-3.52339371578857));
#29973=CARTESIAN_POINT('Ctrl Pts',(8.25916219897089,-15.3675249720875,3.52339371578858));
#29974=CARTESIAN_POINT('Ctrl Pts',(8.94889389387818,-14.9547919997346,10.5701811473657));
#29975=CARTESIAN_POINT('Ctrl Pts',(6.80340542685227,-16.0522091553154,-10.5701811473657));
#29976=CARTESIAN_POINT('Ctrl Pts',(7.54376312530152,-15.7384313756399,-3.52339371578856));
#29977=CARTESIAN_POINT('Ctrl Pts',(8.26233788774653,-15.3733486508924,3.52339371578856));
#29978=CARTESIAN_POINT('Ctrl Pts',(8.95234307759566,-14.960457800119,10.5701811473657));
#29979=CARTESIAN_POINT('Ctrl Pts',(6.8319106026398,-16.1142229628811,-10.5701811473657));
#29980=CARTESIAN_POINT('Ctrl Pts',(7.57511310971885,-15.7991268108376,-3.52339371578859));
#29981=CARTESIAN_POINT('Ctrl Pts',(8.29648793938073,-15.4325364319894,3.52339371578859));
#29982=CARTESIAN_POINT('Ctrl Pts',(8.98912891724076,-15.0179474459438,10.5701811473657));
#29983=CARTESIAN_POINT('Ctrl Pts',(6.98943179288394,-16.3772101395062,-10.5701811473657));
#29984=CARTESIAN_POINT('Ctrl Pts',(7.74477657805409,-16.0548520865028,-3.52339371578856));
#29985=CARTESIAN_POINT('Ctrl Pts',(8.477750844465,-15.6801517612296,3.52339371578856));
#29986=CARTESIAN_POINT('Ctrl Pts',(9.18141647930957,-15.2566955850336,10.5701811473657));
#29987=CARTESIAN_POINT('Ctrl Pts',(7.46076357859375,-16.9869629346763,-10.5701811473657));
#29988=CARTESIAN_POINT('Ctrl Pts',(8.24421702180967,-16.6428631545587,-3.52339371578859));
#29989=CARTESIAN_POINT('Ctrl Pts',(9.0038352824957,-16.2444807757536,3.5233937157886));
#29990=CARTESIAN_POINT('Ctrl Pts',(9.73234227367015,-15.7956138465041,10.5701811473657));
#29991=CARTESIAN_POINT('Ctrl Pts',(8.18028559447488,-17.6243975759657,-10.5701811473657));
#29992=CARTESIAN_POINT('Ctrl Pts',(8.99317441419842,-17.2471218084677,-3.52339371578856));
#29993=CARTESIAN_POINT('Ctrl Pts',(9.77981895378818,-16.8135040854819,3.52339371578856));
#29994=CARTESIAN_POINT('Ctrl Pts',(10.5329043010263,-16.3277184354797,10.5701811473657));
#29995=CARTESIAN_POINT('Ctrl Pts',(8.71988860141418,-17.9989872709252,-10.5701811473657));
#29996=CARTESIAN_POINT('Ctrl Pts',(9.55002197921109,-17.5968162782051,-3.52339371578857));
#29997=CARTESIAN_POINT('Ctrl Pts',(10.3522831255593,-17.137126276613,3.52339371578858));
#29998=CARTESIAN_POINT('Ctrl Pts',(11.1190146190996,-16.6243049148002,10.5701811473657));
#29999=CARTESIAN_POINT('Ctrl Pts',(6.80077064695807,-16.0461217833684,-10.5701811473657));
#30000=CARTESIAN_POINT('Ctrl Pts',(7.54083568928885,-15.7324626522293,-3.52339371578856));
#30001=CARTESIAN_POINT('Ctrl Pts',(8.25916219897089,-15.3675249720875,3.52339371578858));
#30002=CARTESIAN_POINT('Ctrl Pts',(8.94889389387819,-14.9547919997346,10.5701811473657));
#30003=CARTESIAN_POINT('Origin',(-540.112471297088,1034.77284228466,-6.00190077473124));
#30004=CARTESIAN_POINT('Origin',(-619.619007474887,989.216155519852,6.00190077308503));
#30005=CARTESIAN_POINT('Ctrl Pts',(10.2179937997566,-17.1928067231421,-10.5701811473657));
#30006=CARTESIAN_POINT('Ctrl Pts',(11.0109452310822,-16.7215414469562,-3.52339371578858));
#30007=CARTESIAN_POINT('Ctrl Pts',(11.771236988334,-16.1953339887957,3.52339371578858));
#30008=CARTESIAN_POINT('Ctrl Pts',(12.4916122395345,-15.6192068930627,10.5701811473657));
#30009=CARTESIAN_POINT('Ctrl Pts',(10.2026262038395,-16.5361084032577,-10.5701811473657));
#30010=CARTESIAN_POINT('Ctrl Pts',(10.9653007820263,-16.0655207639423,-3.52339371578859));
#30011=CARTESIAN_POINT('Ctrl Pts',(11.6953369617914,-15.5421842200282,3.5233937157886));
#30012=CARTESIAN_POINT('Ctrl Pts',(12.3858181753482,-14.9709041379195,10.5701811473657));
#30013=CARTESIAN_POINT('Ctrl Pts',(10.067006500551,-15.5844556949571,-10.5701811473657));
#30014=CARTESIAN_POINT('Ctrl Pts',(10.7857775294981,-15.1201581991617,-3.52339371578856));
#30015=CARTESIAN_POINT('Ctrl Pts',(11.4723756631221,-14.6060460787458,3.52339371578856));
#30016=CARTESIAN_POINT('Ctrl Pts',(12.1202404623054,-14.047051303605,10.5701811473657));
#30017=CARTESIAN_POINT('Ctrl Pts',(9.81776698398881,-14.8551880626945,-10.5701811473657));
#30018=CARTESIAN_POINT('Ctrl Pts',(10.5029081614888,-14.4023723984214,-3.52339371578859));
#30019=CARTESIAN_POINT('Ctrl Pts',(11.1566607063147,-13.9021132965593,3.52339371578859));
#30020=CARTESIAN_POINT('Ctrl Pts',(11.7728006532305,-13.3591289277863,10.5701811473657));
#30021=CARTESIAN_POINT('Ctrl Pts',(9.685058394327,-14.578848428518,-10.5701811473657));
#30022=CARTESIAN_POINT('Ctrl Pts',(10.357449939268,-14.132166033665,-3.52339371578857));
#30023=CARTESIAN_POINT('Ctrl Pts',(10.9988888810636,-13.6388849853685,3.52339371578857));
#30024=CARTESIAN_POINT('Ctrl Pts',(11.6032469575355,-13.103733729196,10.5701811473657));
#30025=CARTESIAN_POINT('Ctrl Pts',(9.64900602019209,-14.5208962185842,-10.5701811473657));
#30026=CARTESIAN_POINT('Ctrl Pts',(10.3187301172288,-14.0758617811295,-3.52339371578858));
#30027=CARTESIAN_POINT('Ctrl Pts',(10.9576028212757,-13.584458939098,3.52339371578859));
#30028=CARTESIAN_POINT('Ctrl Pts',(11.5595462325571,-13.0513077914043,10.5701811473657));
#30029=CARTESIAN_POINT('Ctrl Pts',(9.6453770639989,-14.5153438461684,-10.5701811473657));
#30030=CARTESIAN_POINT('Ctrl Pts',(10.3148409196886,-14.070488292812,-3.52339371578858));
#30031=CARTESIAN_POINT('Ctrl Pts',(10.9534758330391,-13.5792470767591,3.52339371578858));
#30032=CARTESIAN_POINT('Ctrl Pts',(11.5551861621905,-13.0463089966602,10.5701811473657));
#30033=CARTESIAN_POINT('Origin',(-701.455017753282,932.97478721464,6.0000000302541));
#30034=CARTESIAN_POINT('Origin',(-626.092649606386,985.134825973644,-6.00000002004485));
#30035=CARTESIAN_POINT('Ctrl Pts',(9.02141589925907,-17.8497634486454,-8.00000002680495));
#30036=CARTESIAN_POINT('Ctrl Pts',(9.17718447174341,-17.7710367428009,-6.66666668453663));
#30037=CARTESIAN_POINT('Ctrl Pts',(9.33192245397616,-17.6902709152619,-5.33333334226832));
#30038=CARTESIAN_POINT('Ctrl Pts',(9.48557682353725,-17.6074936411964,-4.));
#30039=CARTESIAN_POINT('Ctrl Pts',(9.52768331452379,-17.5938917715508,-8.00000002680495));
#30040=CARTESIAN_POINT('Ctrl Pts',(9.68121900925412,-17.5107470358699,-6.66666668453663));
#30041=CARTESIAN_POINT('Ctrl Pts',(9.83366620747201,-17.4255924489156,-5.33333334226832));
#30042=CARTESIAN_POINT('Ctrl Pts',(9.98497281389113,-17.3384571088881,-4.));
#30043=CARTESIAN_POINT('Ctrl Pts',(10.0230579087404,-17.3164686691292,-8.00000002680495));
#30044=CARTESIAN_POINT('Ctrl Pts',(10.1741726299965,-17.2290009742501,-6.66666668453663));
#30045=CARTESIAN_POINT('Ctrl Pts',(10.3241422646724,-17.1395551213611,-5.33333334226832));
#30046=CARTESIAN_POINT('Ctrl Pts',(10.4729155653442,-17.0481616772035,-4.));
#30047=CARTESIAN_POINT('Ctrl Pts',(10.5057483754947,-17.0184973211735,-8.00000002680495));
#30048=CARTESIAN_POINT('Ctrl Pts',(10.6542627824881,-16.9268173707899,-6.66666668453663));
#30049=CARTESIAN_POINT('Ctrl Pts',(10.8015770320273,-16.8331932610413,-5.33333334226832));
#30050=CARTESIAN_POINT('Ctrl Pts',(10.9476406455038,-16.7376570731065,-4.));
#30051=CARTESIAN_POINT('Ctrl Pts',(10.3940821869213,-17.0869264495264,4.));
#30052=CARTESIAN_POINT('Ctrl Pts',(10.5431937507156,-16.9962209704763,5.33333334226731));
#30053=CARTESIAN_POINT('Ctrl Pts',(10.6911179135796,-16.9035635148428,6.66666668453462));
#30054=CARTESIAN_POINT('Ctrl Pts',(10.8378039879122,-16.8089858325717,8.00000002680193));
#30055=CARTESIAN_POINT('Ctrl Pts',(10.8787134882441,-16.7921222557363,4.));
#30056=CARTESIAN_POINT('Ctrl Pts',(11.0252524228747,-16.6971875557313,5.33333334226731));
#30057=CARTESIAN_POINT('Ctrl Pts',(11.1705485253506,-16.6003346026057,6.66666668453462));
#30058=CARTESIAN_POINT('Ctrl Pts',(11.3145521439962,-16.5015964922092,8.00000002680193));
#30059=CARTESIAN_POINT('Ctrl Pts',(11.3507946421043,-16.4766877133626,4.));
#30060=CARTESIAN_POINT('Ctrl Pts',(11.4945808908437,-16.3776333277898,5.33333334226731));
#30061=CARTESIAN_POINT('Ctrl Pts',(11.6370703784336,-16.2766967246661,6.66666668453462));
#30062=CARTESIAN_POINT('Ctrl Pts',(11.7782144136678,-16.1739123973319,8.00000002680193));
#30063=CARTESIAN_POINT('Ctrl Pts',(11.8086185726673,-16.1417634540114,4.));
#30064=CARTESIAN_POINT('Ctrl Pts',(11.9494820332864,-16.0387138162183,5.33333334226731));
#30065=CARTESIAN_POINT('Ctrl Pts',(12.0889964991502,-15.9338201755235,6.66666668453462));
#30066=CARTESIAN_POINT('Ctrl Pts',(12.2271141643192,-15.8271184747163,8.00000002680193));
#30067=CARTESIAN_POINT('Ctrl Pts',(0.902537120435115,-17.4044227834609,
-10.5701811473657));
#30068=CARTESIAN_POINT('Ctrl Pts',(1.70524852060254,-17.3627967643357,-3.52339371578857));
#30069=CARTESIAN_POINT('Ctrl Pts',(2.5050706787327,-17.2655496550558,3.52339371578858));
#30070=CARTESIAN_POINT('Ctrl Pts',(3.29436945311861,-17.1136096597291,10.5701811473657));
#30071=CARTESIAN_POINT('Ctrl Pts',(0.903127939532488,-17.4143548929054,
-10.5701811473657));
#30072=CARTESIAN_POINT('Ctrl Pts',(1.70635018607402,-17.3727370626202,-3.52339371578859));
#30073=CARTESIAN_POINT('Ctrl Pts',(2.50651861700806,-17.2753677032605,3.52339371578859));
#30074=CARTESIAN_POINT('Ctrl Pts',(3.29632448506016,-17.1233653614123,10.5701811473657));
#30075=CARTESIAN_POINT('Ctrl Pts',(0.916537850406112,-17.5552227079071,
-10.5701811473657));
#30076=CARTESIAN_POINT('Ctrl Pts',(1.72622304155972,-17.5129629857505,-3.52339371578856));
#30077=CARTESIAN_POINT('Ctrl Pts',(2.53291653419385,-17.4145668679413,3.52339371578856));
#30078=CARTESIAN_POINT('Ctrl Pts',(3.3290350496456,-17.2610373846323,10.5701811473657));
#30079=CARTESIAN_POINT('Ctrl Pts',(1.09636149928822,-18.2632687859998,-10.5701811473657));
#30080=CARTESIAN_POINT('Ctrl Pts',(1.93870102381171,-18.2127147721516,-3.52339371578858));
#30081=CARTESIAN_POINT('Ctrl Pts',(2.77747866403969,-18.1037632822212,3.52339371578859));
#30082=CARTESIAN_POINT('Ctrl Pts',(3.60479546944612,-17.9375150149138,10.5701811473657));
#30083=CARTESIAN_POINT('Ctrl Pts',(1.53274044321678,-19.1804873760835,-10.5701811473657));
#30084=CARTESIAN_POINT('Ctrl Pts',(2.41748686096404,-19.1098799173874,-3.52339371578856));
#30085=CARTESIAN_POINT('Ctrl Pts',(3.29695624953644,-18.9777403313293,3.52339371578857));
#30086=CARTESIAN_POINT('Ctrl Pts',(4.16350885073651,-18.785781413085,10.5701811473657));
#30087=CARTESIAN_POINT('Ctrl Pts',(2.03799876670532,-19.8958930693475,-10.5701811473657));
#30088=CARTESIAN_POINT('Ctrl Pts',(2.95561955666073,-19.8018982920477,-3.52339371578857));
#30089=CARTESIAN_POINT('Ctrl Pts',(3.86672167605729,-19.6443204619612,3.52339371578858));
#30090=CARTESIAN_POINT('Ctrl Pts',(4.76260883832891,-19.4246636277973,10.5701811473657));
#30091=CARTESIAN_POINT('Ctrl Pts',(0.902537120435115,-17.4044227834609,
-10.5701811473657));
#30092=CARTESIAN_POINT('Ctrl Pts',(1.70524852060254,-17.3627967643357,-3.52339371578857));
#30093=CARTESIAN_POINT('Ctrl Pts',(2.5050706787327,-17.2655496550558,3.52339371578858));
#30094=CARTESIAN_POINT('Ctrl Pts',(3.29436945311861,-17.1136096597291,10.5701811473657));
#30095=CARTESIAN_POINT('Origin',(-153.626547848111,1157.09774892851,-6.00190077405241));
#30096=CARTESIAN_POINT('Origin',(-243.919557730996,1141.48130344756,6.00190077308281));
#30097=CARTESIAN_POINT('Ctrl Pts',(3.72148715324783,-19.6507133122286,-10.5701811473657));
#30098=CARTESIAN_POINT('Ctrl Pts',(4.62779997921165,-19.4790741719563,-3.52339371578857));
#30099=CARTESIAN_POINT('Ctrl Pts',(5.52221408340464,-19.244636002305,3.52339371578858));
#30100=CARTESIAN_POINT('Ctrl Pts',(6.39619246301095,-18.9496364684737,10.5701811473657));
#30101=CARTESIAN_POINT('Ctrl Pts',(3.93165039025385,-19.0283627195926,-10.5701811473657));
#30102=CARTESIAN_POINT('Ctrl Pts',(4.80928051528301,-18.8470050560371,-3.52339371578858));
#30103=CARTESIAN_POINT('Ctrl Pts',(5.67428176607205,-18.6049166463696,3.52339371578858));
#30104=CARTESIAN_POINT('Ctrl Pts',(6.51851116280462,-18.3042474524345,10.5701811473657));
#30105=CARTESIAN_POINT('Ctrl Pts',(4.12969891987871,-18.0877210849008,-10.5701811473657));
#30106=CARTESIAN_POINT('Ctrl Pts',(4.96392184787266,-17.8972583245914,-3.52339371578857));
#30107=CARTESIAN_POINT('Ctrl Pts',(5.78495026151904,-17.6489806267712,3.52339371578857));
#30108=CARTESIAN_POINT('Ctrl Pts',(6.58493150569049,-17.3452801729859,10.5701811473657));
#30109=CARTESIAN_POINT('Ctrl Pts',(4.14491130701941,-17.3171860509474,-10.5701811473657));
#30110=CARTESIAN_POINT('Ctrl Pts',(4.94360549410753,-17.1260105963806,-3.52339371578858));
#30111=CARTESIAN_POINT('Ctrl Pts',(5.72903079998526,-16.8795171054837,3.52339371578858));
#30112=CARTESIAN_POINT('Ctrl Pts',(6.49372455310477,-16.5800109738984,10.5701811473657));
#30113=CARTESIAN_POINT('Ctrl Pts',(4.11471950693849,-17.0121225239123,-10.5701811473657));
#30114=CARTESIAN_POINT('Ctrl Pts',(4.89933525670706,-16.8223498262056,-3.52339371578858));
#30115=CARTESIAN_POINT('Ctrl Pts',(5.6708029003471,-16.5782020953567,3.52339371578858));
#30116=CARTESIAN_POINT('Ctrl Pts',(6.42174623445712,-16.2820270448621,10.5701811473657));
#30117=CARTESIAN_POINT('Ctrl Pts',(4.10066074919594,-16.9453334457776,-10.5701811473657));
#30118=CARTESIAN_POINT('Ctrl Pts',(4.88220628322697,-16.756197000563,-3.52339371578857));
#30119=CARTESIAN_POINT('Ctrl Pts',(5.65061991930358,-16.5129367098777,3.52339371578857));
#30120=CARTESIAN_POINT('Ctrl Pts',(6.3986101329639,-16.2178152824268,10.5701811473657));
#30121=CARTESIAN_POINT('Ctrl Pts',(4.09914966904953,-16.9388747462736,-10.5701811473657));
#30122=CARTESIAN_POINT('Ctrl Pts',(4.8803894742422,-16.7498173893433,-3.52339371578857));
#30123=CARTESIAN_POINT('Ctrl Pts',(5.64852438081578,-16.5066276481894,3.52339371578858));
#30124=CARTESIAN_POINT('Ctrl Pts',(6.39622269550912,-16.2116267200016,10.5701811473657));
#30125=CARTESIAN_POINT('Origin',(-340.055933549895,1116.62126860139,6.00000003060113));
#30126=CARTESIAN_POINT('Origin',(-251.39868836428,1139.86022417391,-6.00000002196444));
#30127=CARTESIAN_POINT('Ctrl Pts',(2.37237929653944,-19.8587969543311,-8.00000002680495));
#30128=CARTESIAN_POINT('Ctrl Pts',(2.54567999386982,-19.838094039277,-6.66666668453664));
#30129=CARTESIAN_POINT('Ctrl Pts',(2.71870967383992,-19.8151224939882,-5.33333334226832));
#30130=CARTESIAN_POINT('Ctrl Pts',(2.89140904620798,-19.78989018988,-4.));
#30131=CARTESIAN_POINT('Ctrl Pts',(2.93562831848091,-19.7915098814272,-8.00000002680495));
#30132=CARTESIAN_POINT('Ctrl Pts',(3.10834185226059,-19.765891687168,-6.66666668453664));
#30133=CARTESIAN_POINT('Ctrl Pts',(3.2807199435204,-19.738012562765,-5.33333334226832));
#30134=CARTESIAN_POINT('Ctrl Pts',(3.45270368653351,-19.7078820339451,-4.));
#30135=CARTESIAN_POINT('Ctrl Pts',(3.4960124584432,-19.70024552896,-8.00000002680495));
#30136=CARTESIAN_POINT('Ctrl Pts',(3.66792956043857,-19.6697370601475,-6.66666668453663));
#30137=CARTESIAN_POINT('Ctrl Pts',(3.83944720291044,-19.6369780881742,-5.33333334226832));
#30138=CARTESIAN_POINT('Ctrl Pts',(4.01050677459148,-19.6019798087299,-4.));
#30139=CARTESIAN_POINT('Ctrl Pts',(4.05150533131066,-19.5853339147016,-8.00000002680495));
#30140=CARTESIAN_POINT('Ctrl Pts',(4.22241961341302,-19.549977860618,-6.66666668453664));
#30141=CARTESIAN_POINT('Ctrl Pts',(4.39287105807657,-19.5123844163009,-5.33333334226832));
#30142=CARTESIAN_POINT('Ctrl Pts',(4.56280125851603,-19.4725664634964,-4.));
#30143=CARTESIAN_POINT('Ctrl Pts',(3.92316929763006,-19.6114441758411,4.));
#30144=CARTESIAN_POINT('Ctrl Pts',(4.09431143474655,-19.5772080649333,5.33333334226731));
#30145=CARTESIAN_POINT('Ctrl Pts',(4.26500539528167,-19.5407315809978,6.66666668453462));
#30146=CARTESIAN_POINT('Ctrl Pts',(4.43519268934985,-19.5020272230437,8.00000002680193));
#30147=CARTESIAN_POINT('Ctrl Pts',(4.47940272789801,-19.5001725174983,4.));
#30148=CARTESIAN_POINT('Ctrl Pts',(4.64957386313053,-19.4610823478722,5.33333334226731));
#30149=CARTESIAN_POINT('Ctrl Pts',(4.81923319936554,-19.4197645363123,6.66666668453462));
#30150=CARTESIAN_POINT('Ctrl Pts',(4.98832275984285,-19.3762332008709,8.00000002680193));
#30151=CARTESIAN_POINT('Ctrl Pts',(5.03089887198511,-19.3652222695934,4.));
#30152=CARTESIAN_POINT('Ctrl Pts',(5.19989234404657,-19.3213193878163,5.33333334226731));
#30153=CARTESIAN_POINT('Ctrl Pts',(5.36831101554159,-19.2752042816616,6.66666668453462));
#30154=CARTESIAN_POINT('Ctrl Pts',(5.53609733428556,-19.2268927108936,8.00000002680193));
#30155=CARTESIAN_POINT('Ctrl Pts',(5.57566348434081,-19.207081420908,4.));
#30156=CARTESIAN_POINT('Ctrl Pts',(5.74327689071064,-19.1584245776895,5.33333334226731));
#30157=CARTESIAN_POINT('Ctrl Pts',(5.91025334280012,-19.107573555172,6.66666668453462));
#30158=CARTESIAN_POINT('Ctrl Pts',(6.07653562456276,-19.054545777935,8.00000002680193));
#30159=CARTESIAN_POINT('Ctrl Pts',(-5.10455570284158,-16.6634935339443,
-10.5701811473657));
#30160=CARTESIAN_POINT('Ctrl Pts',(-4.33601678645625,-16.8989213390741,
-3.52339371578858));
#30161=CARTESIAN_POINT('Ctrl Pts',(-3.55116933626636,-17.0810942372497,
3.52339371578857));
#30162=CARTESIAN_POINT('Ctrl Pts',(-2.75750456340204,-17.2082734247813,
10.5701811473657));
#30163=CARTESIAN_POINT('Ctrl Pts',(-5.10739749599094,-16.673028735929,-10.5701811473657));
#30164=CARTESIAN_POINT('Ctrl Pts',(-4.33838134178576,-16.9086389558014,
-3.52339371578857));
#30165=CARTESIAN_POINT('Ctrl Pts',(-3.55316668960767,-17.0908154087531,
3.52339371578856));
#30166=CARTESIAN_POINT('Ctrl Pts',(-2.75900408080094,-17.2181094459668,
10.5701811473657));
#30167=CARTESIAN_POINT('Ctrl Pts',(-5.14297547152451,-16.8099873002577,
-10.5701811473657));
#30168=CARTESIAN_POINT('Ctrl Pts',(-4.36766659600894,-17.0472047963177,
-3.52339371578858));
#30169=CARTESIAN_POINT('Ctrl Pts',(-3.57596927094015,-17.230648054227,3.52339371578858));
#30170=CARTESIAN_POINT('Ctrl Pts',(-2.77535240081307,-17.3586661004476,
10.5701811473657));
#30171=CARTESIAN_POINT('Ctrl Pts',(-5.21616227492136,-17.5368363517824,
-10.5701811473657));
#30172=CARTESIAN_POINT('Ctrl Pts',(-4.40733153621249,-17.7774282041583,
-3.52339371578857));
#30173=CARTESIAN_POINT('Ctrl Pts',(-3.58187484240087,-17.9619260440222,
3.52339371578856));
#30174=CARTESIAN_POINT('Ctrl Pts',(-2.74759107678734,-18.0886627859074,
10.5701811473657));
#30175=CARTESIAN_POINT('Ctrl Pts',(-5.11980806768305,-18.5479914974656,
-10.5701811473657));
#30176=CARTESIAN_POINT('Ctrl Pts',(-4.26426917104801,-18.7842432821223,
-3.52339371578859));
#30177=CARTESIAN_POINT('Ctrl Pts',(-3.39264383327087,-18.9608689271937,
3.52339371578858));
#30178=CARTESIAN_POINT('Ctrl Pts',(-2.51269688917417,-19.0768649830916,
10.5701811473657));
#30179=CARTESIAN_POINT('Ctrl Pts',(-4.8897033552575,-19.3930621535491,-10.5701811473657));
#30180=CARTESIAN_POINT('Ctrl Pts',(-3.99527368840475,-19.6185807284257,
-3.52339371578858));
#30181=CARTESIAN_POINT('Ctrl Pts',(-3.08522288423935,-19.7821212566383,
3.52339371578857));
#30182=CARTESIAN_POINT('Ctrl Pts',(-2.1682371957995,-19.8821227754128,10.5701811473657));
#30183=CARTESIAN_POINT('Ctrl Pts',(-5.10455570284158,-16.6634935339443,
-10.5701811473657));
#30184=CARTESIAN_POINT('Ctrl Pts',(-4.33601678645625,-16.8989213390741,
-3.52339371578858));
#30185=CARTESIAN_POINT('Ctrl Pts',(-3.55116933626636,-17.0810942372497,
3.52339371578857));
#30186=CARTESIAN_POINT('Ctrl Pts',(-2.75750456340204,-17.2082734247813,
10.5701811473657));
#30187=CARTESIAN_POINT('Origin',(251.389004560051,1139.85959012119,-6.00190077265366));
#30188=CARTESIAN_POINT('Origin',(161.200190535201,1156.06695970641,6.00190077397515));
#30189=CARTESIAN_POINT('Ctrl Pts',(-3.22388576724348,-19.738453862219,-10.5701811473657));
#30190=CARTESIAN_POINT('Ctrl Pts',(-2.31352624920543,-19.8871430713012,
-3.52339371578857));
#30191=CARTESIAN_POINT('Ctrl Pts',(-1.39286933918329,-19.9727508933579,
3.52339371578858));
#30192=CARTESIAN_POINT('Ctrl Pts',(-0.470702522298841,-19.9944602189378,
10.5701811473657));
#30193=CARTESIAN_POINT('Ctrl Pts',(-2.81354048537626,-19.2255156632198,
-10.5701811473657));
#30194=CARTESIAN_POINT('Ctrl Pts',(-1.92680995902448,-19.3552623862032,
-3.52339371578858));
#30195=CARTESIAN_POINT('Ctrl Pts',(-1.03117555411549,-19.4236215458326,
3.5233937157886));
#30196=CARTESIAN_POINT('Ctrl Pts',(-0.135024498952067,-19.4298283822643,
10.5701811473657));
#30197=CARTESIAN_POINT('Ctrl Pts',(-2.3057142289943,-18.4093435092557,-10.5701811473657));
#30198=CARTESIAN_POINT('Ctrl Pts',(-1.45665899888873,-18.5156881042564,
-3.52339371578854));
#30199=CARTESIAN_POINT('Ctrl Pts',(-0.600227987416887,-18.5631911577295,
3.52339371578856));
#30200=CARTESIAN_POINT('Ctrl Pts',(0.255380157229872,-18.5514157821675,
10.5701811473657));
#30201=CARTESIAN_POINT('Ctrl Pts',(-2.02788285372484,-17.6904768579848,
-10.5701811473657));
#30202=CARTESIAN_POINT('Ctrl Pts',(-1.21196996348224,-17.7840001943942,
-3.52339371578858));
#30203=CARTESIAN_POINT('Ctrl Pts',(-0.389605628258797,-17.8210031964624,
3.5233937157886));
#30204=CARTESIAN_POINT('Ctrl Pts',(0.431408578760403,-17.8011001617737,
10.5701811473657));
#30205=CARTESIAN_POINT('Ctrl Pts',(-1.95191613165044,-17.3934844692986,
-10.5701811473657));
#30206=CARTESIAN_POINT('Ctrl Pts',(-1.14971241617157,-17.4835108568284,
-3.52339371578855));
#30207=CARTESIAN_POINT('Ctrl Pts',(-0.341266322086584,-17.5179443719088,
3.52339371578856));
#30208=CARTESIAN_POINT('Ctrl Pts',(0.465687420824633,-17.4964686092598,
10.5701811473657));
#30209=CARTESIAN_POINT('Ctrl Pts',(-1.94228472746017,-17.3259133729229,
-10.5701811473657));
#30210=CARTESIAN_POINT('Ctrl Pts',(-1.14318368222263,-17.4154875665979,
-3.52339371578858));
#30211=CARTESIAN_POINT('Ctrl Pts',(-0.337911139204659,-17.449710608455,
3.5233937157886));
#30212=CARTESIAN_POINT('Ctrl Pts',(0.465907217907244,-17.4282149009259,
10.5701811473657));
#30213=CARTESIAN_POINT('Ctrl Pts',(-1.9414956729932,-17.3193273608118,-10.5701811473657));
#30214=CARTESIAN_POINT('Ctrl Pts',(-1.14270896867536,-17.4088713077428,
-3.52339371578857));
#30215=CARTESIAN_POINT('Ctrl Pts',(-0.337722475075313,-17.4430653133694,
3.52339371578858));
#30216=CARTESIAN_POINT('Ctrl Pts',(0.465780373556093,-17.4215830027821,
10.5701811473657));
#30217=CARTESIAN_POINT('Origin',(62.3589149196093,1165.5867454631,6.00000002996901));
#30218=CARTESIAN_POINT('Origin',(153.617664909995,1157.10165684081,-6.00000002140803));
#30219=CARTESIAN_POINT('Ctrl Pts',(-4.5628012619323,-19.4725664626959,-8.00000002680495));
#30220=CARTESIAN_POINT('Ctrl Pts',(-4.39287106149983,-19.5123844155302,
-6.66666668453663));
#30221=CARTESIAN_POINT('Ctrl Pts',(-4.22241961684288,-19.5499778598772,
-5.33333334226832));
#30222=CARTESIAN_POINT('Ctrl Pts',(-4.05150533474672,-19.5853339139908,
-4.));
#30223=CARTESIAN_POINT('Ctrl Pts',(-4.01050677803046,-19.6019798080263,
-8.00000002680495));
#30224=CARTESIAN_POINT('Ctrl Pts',(-3.83944720635556,-19.6369780875006,
-6.66666668453663));
#30225=CARTESIAN_POINT('Ctrl Pts',(-3.66792956388944,-19.669737059504,-5.33333334226832));
#30226=CARTESIAN_POINT('Ctrl Pts',(-3.49601246189942,-19.7002455283466,
-4.));
#30227=CARTESIAN_POINT('Ctrl Pts',(-3.45270368999107,-19.7078820333394,
-8.00000002680495));
#30228=CARTESIAN_POINT('Ctrl Pts',(-3.28071994698324,-19.7380125621894,
-6.66666668453664));
#30229=CARTESIAN_POINT('Ctrl Pts',(-3.10834185572832,-19.7658916866227,
-5.33333334226832));
#30230=CARTESIAN_POINT('Ctrl Pts',(-2.93562832195314,-19.7915098809122,
-4.));
#30231=CARTESIAN_POINT('Ctrl Pts',(-2.89140904967993,-19.7898901893727,
-8.00000002680495));
#30232=CARTESIAN_POINT('Ctrl Pts',(-2.71870967731629,-19.8151224935112,
-6.66666668453663));
#30233=CARTESIAN_POINT('Ctrl Pts',(-2.54567999735022,-19.8380940388304,
-5.33333334226832));
#30234=CARTESIAN_POINT('Ctrl Pts',(-2.37237930002347,-19.8587969539149,
-4.));
#30235=CARTESIAN_POINT('Ctrl Pts',(-3.02093570876772,-19.770532300459,4.));
#30236=CARTESIAN_POINT('Ctrl Pts',(-2.84840526585423,-19.7968949379402,
5.33333334226731));
#30237=CARTESIAN_POINT('Ctrl Pts',(-2.67552971846301,-19.8209990280008,
6.66666668453462));
#30238=CARTESIAN_POINT('Ctrl Pts',(-2.50236830402083,-19.8428363111485,
8.00000002680193));
#30239=CARTESIAN_POINT('Ctrl Pts',(-2.46019011037601,-19.8562141817544,
4.));
#30240=CARTESIAN_POINT('Ctrl Pts',(-2.28691192490911,-19.8776833938736,
5.33333334226731));
#30241=CARTESIAN_POINT('Ctrl Pts',(-2.11335277477,-19.8968842617394,6.66666668453462));
#30242=CARTESIAN_POINT('Ctrl Pts',(-1.93957196895072,-19.9138102227615,
8.00000002680193));
#30243=CARTESIAN_POINT('Ctrl Pts',(-1.8957975502552,-19.9180252198692,4.));
#30244=CARTESIAN_POINT('Ctrl Pts',(-1.72197996168025,-19.9345691773675,
5.33333334226731));
#30245=CARTESIAN_POINT('Ctrl Pts',(-1.5479458836573,-19.9488377305707,6.66666668453462));
#30246=CARTESIAN_POINT('Ctrl Pts',(-1.37375478770641,-19.9608260048063,
8.00000002680193));
#30247=CARTESIAN_POINT('Ctrl Pts',(-1.32979890822622,-19.9557419021113,
4.));
#30248=CARTESIAN_POINT('Ctrl Pts',(-1.15565220662434,-19.967346586858,5.33333334226731));
#30249=CARTESIAN_POINT('Ctrl Pts',(-0.981353592741149,-19.9766715663146,
6.66666668453462));
#30250=CARTESIAN_POINT('Ctrl Pts',(-0.806962791630511,-19.9837136451893,
8.00000002680193));
#30251=CARTESIAN_POINT('Ctrl Pts',(-10.4959637731368,-13.9127010372614,
-10.5701811473657));
#30252=CARTESIAN_POINT('Ctrl Pts',(-9.85429447627607,-14.3967865988031,
-3.52339371578858));
#30253=CARTESIAN_POINT('Ctrl Pts',(-9.17908591963407,-14.8364067643287,
3.52339371578858));
#30254=CARTESIAN_POINT('Ctrl Pts',(-8.47678283314334,-15.2273654477372,
10.5701811473657));
#30255=CARTESIAN_POINT('Ctrl Pts',(-10.4999182019386,-13.9180265095572,
-10.5701811473657));
#30256=CARTESIAN_POINT('Ctrl Pts',(-9.85799982437182,-14.4023061944638,
-3.52339371578858));
#30257=CARTESIAN_POINT('Ctrl Pts',(-9.18254152903514,-14.8420688308859,
3.52339371578858));
#30258=CARTESIAN_POINT('Ctrl Pts',(-8.47996496835057,-15.2331854286516,
10.5701811473657));
#30259=CARTESIAN_POINT('Ctrl Pts',(-10.5393711248066,-13.973719613416,-10.5701811473657));
#30260=CARTESIAN_POINT('Ctrl Pts',(-9.89488859896267,-14.459803788681,-3.52339371578858));
#30261=CARTESIAN_POINT('Ctrl Pts',(-9.21672460434447,-14.9012375244241,
3.52339371578859));
#30262=CARTESIAN_POINT('Ctrl Pts',(-8.51135952136975,-15.2937877139302,
10.5701811473657));
#30263=CARTESIAN_POINT('Ctrl Pts',(-10.6883641017228,-14.2416305529824,
-10.5701811473657));
#30264=CARTESIAN_POINT('Ctrl Pts',(-10.0315214461224,-14.7345992990542,
-3.52339371578858));
#30265=CARTESIAN_POINT('Ctrl Pts',(-9.34053431369458,-15.1820234679673,
3.52339371578859));
#30266=CARTESIAN_POINT('Ctrl Pts',(-8.62197769029708,-15.5796876954148,
10.5701811473657));
#30267=CARTESIAN_POINT('Ctrl Pts',(-10.9807596939227,-14.9546925405834,
-10.5701811473657));
#30268=CARTESIAN_POINT('Ctrl Pts',(-10.2910338072701,-15.4611332407784,
-3.52339371578857));
#30269=CARTESIAN_POINT('Ctrl Pts',(-9.56621540573719,-15.9197907568141,
3.52339371578858));
#30270=CARTESIAN_POINT('Ctrl Pts',(-8.81323173181656,-16.3262628571379,
10.5701811473657));
#30271=CARTESIAN_POINT('Ctrl Pts',(-11.1730334267767,-15.896534887177,-10.5701811473657));
#30272=CARTESIAN_POINT('Ctrl Pts',(-10.4398585735504,-16.4118793808757,
-3.52339371578858));
#30273=CARTESIAN_POINT('Ctrl Pts',(-9.67101229504736,-16.8763246803408,
3.52339371578859));
#30274=CARTESIAN_POINT('Ctrl Pts',(-8.8737668624215,-17.2856229001588,10.5701811473657));
#30275=CARTESIAN_POINT('Ctrl Pts',(-11.2276360580494,-16.5511403577636,
-10.5701811473657));
#30276=CARTESIAN_POINT('Ctrl Pts',(-10.464278995546,-17.068971461469,-3.52339371578858));
#30277=CARTESIAN_POINT('Ctrl Pts',(-9.66504512535763,-17.5339049951292,
3.52339371578858));
#30278=CARTESIAN_POINT('Ctrl Pts',(-8.83756297427066,-17.9415032611597,
10.5701811473657));
#30279=CARTESIAN_POINT('Ctrl Pts',(-10.4959637731368,-13.9127010372614,
-10.5701811473657));
#30280=CARTESIAN_POINT('Ctrl Pts',(-9.85429447627607,-14.3967865988031,
-3.52339371578858));
#30281=CARTESIAN_POINT('Ctrl Pts',(-9.17908591963407,-14.8364067643287,
3.52339371578858));
#30282=CARTESIAN_POINT('Ctrl Pts',(-8.47678283314334,-15.2273654477372,
10.5701811473657));
#30283=CARTESIAN_POINT('Origin',(626.083332913132,985.137542209956,-6.00190077217363));
#30284=CARTESIAN_POINT('Origin',(546.876816795099,1031.21387892502,6.00190077273223));
#30285=CARTESIAN_POINT('Ctrl Pts',(-9.78041048471869,-17.4454455678722,
-10.5701811473657));
#30286=CARTESIAN_POINT('Ctrl Pts',(-8.97580706795737,-17.8965290132744,
-3.52339371578857));
#30287=CARTESIAN_POINT('Ctrl Pts',(-8.13995216290365,-18.2918572602622,
3.52339371578859));
#30288=CARTESIAN_POINT('Ctrl Pts',(-7.28082383659005,-18.6276569801929,
10.5701811473657));
#30289=CARTESIAN_POINT('Ctrl Pts',(-9.21937685503484,-17.1037876794706,
-10.5701811473657));
#30290=CARTESIAN_POINT('Ctrl Pts',(-8.43049871558726,-17.5289894193433,
-3.52339371578856));
#30291=CARTESIAN_POINT('Ctrl Pts',(-7.61225788394638,-17.8995510247446,
3.52339371578858));
#30292=CARTESIAN_POINT('Ctrl Pts',(-6.7722742133858,-18.2118852554664,10.5701811473657));
#30293=CARTESIAN_POINT('Ctrl Pts',(-8.46303091716765,-16.5105131633497,
-10.5701811473657));
#30294=CARTESIAN_POINT('Ctrl Pts',(-7.70155197642183,-16.9008383860245,
-3.52339371578858));
#30295=CARTESIAN_POINT('Ctrl Pts',(-6.91301848801586,-17.2383936822946,
3.5233937157886));
#30296=CARTESIAN_POINT('Ctrl Pts',(-6.10498241256954,-17.5199636690347,
10.5701811473657));
#30297=CARTESIAN_POINT('Ctrl Pts',(-7.95608662604428,-15.9300303080035,
-10.5701811473657));
#30298=CARTESIAN_POINT('Ctrl Pts',(-7.22136616880224,-16.2969721407607,
-3.52339371578855));
#30299=CARTESIAN_POINT('Ctrl Pts',(-6.46125271583016,-16.6130088782682,
3.52339371578857));
#30300=CARTESIAN_POINT('Ctrl Pts',(-5.68294448515699,-16.8751095401972,
10.5701811473657));
#30301=CARTESIAN_POINT('Ctrl Pts',(-7.78312379466279,-15.6769313836482,
-10.5701811473657));
#30302=CARTESIAN_POINT('Ctrl Pts',(-7.0600897208263,-16.0358983454305,-3.52339371578857));
#30303=CARTESIAN_POINT('Ctrl Pts',(-6.31217625428559,-16.3447602199671,
3.52339371578859));
#30304=CARTESIAN_POINT('Ctrl Pts',(-5.54654263333713,-16.6005740390878,
10.5701811473657));
#30305=CARTESIAN_POINT('Ctrl Pts',(-7.75096200091494,-15.6167324440469,
-10.5701811473657));
#30306=CARTESIAN_POINT('Ctrl Pts',(-7.03068882400192,-15.97421330688,-3.52339371578857));
#30307=CARTESIAN_POINT('Ctrl Pts',(-6.28568512728736,-16.2817918773532,
3.52339371578859));
#30308=CARTESIAN_POINT('Ctrl Pts',(-5.52299098368707,-16.5365145893167,
10.5701811473657));
#30309=CARTESIAN_POINT('Ctrl Pts',(-7.74796798344853,-15.610813489587,-10.5701811473657));
#30310=CARTESIAN_POINT('Ctrl Pts',(-7.02797984538244,-15.9681584188516,
-3.52339371578857));
#30311=CARTESIAN_POINT('Ctrl Pts',(-6.28323501621945,-16.2756118695303,
3.52339371578859));
#30312=CARTESIAN_POINT('Ctrl Pts',(-5.52084193563401,-16.5302392602455,
10.5701811473657));
#30313=CARTESIAN_POINT('Origin',(457.252357934138,1073.96525857621,6.0000000290552));
#30314=CARTESIAN_POINT('Origin',(540.105460663215,1034.77955266834,-6.00000002228318));
#30315=CARTESIAN_POINT('Ctrl Pts',(-10.9476406484403,-16.7376570711859,
-8.00000002680495));
#30316=CARTESIAN_POINT('Ctrl Pts',(-10.8015770349805,-16.8331932591463,
-6.66666668453663));
#30317=CARTESIAN_POINT('Ctrl Pts',(-10.6542627854578,-16.9268173689207,
-5.33333334226832));
#30318=CARTESIAN_POINT('Ctrl Pts',(-10.5057483784805,-17.0184973193304,
-4.));
#30319=CARTESIAN_POINT('Ctrl Pts',(-10.4729155683351,-17.0481616753661,
-8.00000002680495));
#30320=CARTESIAN_POINT('Ctrl Pts',(-10.3241422676794,-17.1395551195498,
-6.66666668453663));
#30321=CARTESIAN_POINT('Ctrl Pts',(-10.1741726330192,-17.2290009724651,
-5.33333334226832));
#30322=CARTESIAN_POINT('Ctrl Pts',(-10.0230579117785,-17.3164686673708,
-4.));
#30323=CARTESIAN_POINT('Ctrl Pts',(-9.98497281693299,-17.3384571071364,
-8.00000002680495));
#30324=CARTESIAN_POINT('Ctrl Pts',(-9.83366621052917,-17.4255924471903,
-6.66666668453663));
#30325=CARTESIAN_POINT('Ctrl Pts',(-9.68121901232622,-17.5107470341715,
-5.33333334226832));
#30326=CARTESIAN_POINT('Ctrl Pts',(-9.52768331761047,-17.5938917698793,
-4.));
#30327=CARTESIAN_POINT('Ctrl Pts',(-9.48557682662632,-17.6074936395323,
-8.00000002680495));
#30328=CARTESIAN_POINT('Ctrl Pts',(-9.33192245707975,-17.6902709136247,
-6.66666668453663));
#30329=CARTESIAN_POINT('Ctrl Pts',(-9.17718447486117,-17.7710367411908,
-5.33333334226832));
#30330=CARTESIAN_POINT('Ctrl Pts',(-9.02141590239064,-17.8497634470626,
-4.));
#30331=CARTESIAN_POINT('Ctrl Pts',(-9.60067128442543,-17.5450024476604,
4.));
#30332=CARTESIAN_POINT('Ctrl Pts',(-9.44756225340845,-17.6287841103792,
5.33333334226731));
#30333=CARTESIAN_POINT('Ctrl Pts',(-9.29335646154787,-17.7105614654362,
6.66666668453462));
#30334=CARTESIAN_POINT('Ctrl Pts',(-9.13810674890371,-17.7903064910541,
8.00000002680193));
#30335=CARTESIAN_POINT('Ctrl Pts',(-9.10304771279965,-17.8173033691799,
4.));
#30336=CARTESIAN_POINT('Ctrl Pts',(-8.94756238357933,-17.896742459211,5.33333334226731));
#30337=CARTESIAN_POINT('Ctrl Pts',(-8.79103721450315,-17.9741460984632,
6.66666668453462));
#30338=CARTESIAN_POINT('Ctrl Pts',(-8.63352569325523,-18.0494878352489,
8.00000002680193));
#30339=CARTESIAN_POINT('Ctrl Pts',(-8.59383280894276,-18.0684203698839,
4.));
#30340=CARTESIAN_POINT('Ctrl Pts',(-8.43615607031084,-18.1434157212207,
5.33333334226731));
#30341=CARTESIAN_POINT('Ctrl Pts',(-8.27749766403898,-18.2163469356839,
6.66666668453462));
#30342=CARTESIAN_POINT('Ctrl Pts',(-8.11791180783962,-18.2871890921223,
8.00000002680193));
#30343=CARTESIAN_POINT('Ctrl Pts',(-8.07486792671951,-18.2974453945363,
4.));
#30344=CARTESIAN_POINT('Ctrl Pts',(-7.91519259223034,-18.3679119110009,
5.33333334226731));
#30345=CARTESIAN_POINT('Ctrl Pts',(-7.75459480176133,-18.436288162287,6.66666668453462));
#30346=CARTESIAN_POINT('Ctrl Pts',(-7.59312958565075,-18.5025507186311,
8.00000002680193));
#30347=CARTESIAN_POINT('Ctrl Pts',(-14.6214037084642,-9.48383146588572,
-10.5701811473657));
#30348=CARTESIAN_POINT('Ctrl Pts',(-14.1839988183597,-10.1581869207755,
-3.52339371578858));
#30349=CARTESIAN_POINT('Ctrl Pts',(-13.6998692722136,-10.8022296735859,
3.52339371578857));
#30350=CARTESIAN_POINT('Ctrl Pts',(-13.1736359892169,-11.4098124657167,
10.5701811473657));
#30351=CARTESIAN_POINT('Ctrl Pts',(-14.629709758007,-9.48930918495498,-10.5701811473657));
#30352=CARTESIAN_POINT('Ctrl Pts',(-14.1920565364589,-10.1641111402022,
-3.52339371578859));
#30353=CARTESIAN_POINT('Ctrl Pts',(-13.7076479822362,-10.8083926490174,
3.52339371578858));
#30354=CARTESIAN_POINT('Ctrl Pts',(-13.1811071587349,-11.4163834238845,
10.5701811473657));
#30355=CARTESIAN_POINT('Ctrl Pts',(-14.7449772223306,-9.57135777968372,
-10.5701811473657));
#30356=CARTESIAN_POINT('Ctrl Pts',(-14.3035366338093,-10.2514358632125,
-3.52339371578857));
#30357=CARTESIAN_POINT('Ctrl Pts',(-13.814976378559,-10.9008517199746,3.52339371578856));
#30358=CARTESIAN_POINT('Ctrl Pts',(-13.2839566880577,-11.5135458371245,
10.5701811473657));
#30359=CARTESIAN_POINT('Ctrl Pts',(-15.2682377029356,-10.0811139468335,
-10.5701811473657));
#30360=CARTESIAN_POINT('Ctrl Pts',(-14.803286880418,-10.7853243667584,-3.52339371578858));
#30361=CARTESIAN_POINT('Ctrl Pts',(-14.2895432842683,-11.4572463383408,
3.52339371578858));
#30362=CARTESIAN_POINT('Ctrl Pts',(-13.7319096587417,-12.0905995751469,
10.5701811473657));
#30363=CARTESIAN_POINT('Ctrl Pts',(-15.8444191030467,-10.9176358492754,
-10.5701811473657));
#30364=CARTESIAN_POINT('Ctrl Pts',(-15.3408980412456,-11.6485449936037,
-3.52339371578858));
#30365=CARTESIAN_POINT('Ctrl Pts',(-14.7867271085875,-12.3441180329291,
3.52339371578857));
#30366=CARTESIAN_POINT('Ctrl Pts',(-14.1872095083049,-12.9985951401617,
10.5701811473657));
#30367=CARTESIAN_POINT('Ctrl Pts',(-16.211349445681,-11.7129052395219,-10.5701811473657));
#30368=CARTESIAN_POINT('Ctrl Pts',(-15.6711371857387,-12.4605907660142,
-3.52339371578858));
#30369=CARTESIAN_POINT('Ctrl Pts',(-15.0791197221122,-13.1708394318101,
3.52339371578857));
#30370=CARTESIAN_POINT('Ctrl Pts',(-14.4409477424756,-13.8368720561798,
10.5701811473657));
#30371=CARTESIAN_POINT('Ctrl Pts',(-14.6214037084642,-9.48383146588572,
-10.5701811473657));
#30372=CARTESIAN_POINT('Ctrl Pts',(-14.1839988183597,-10.1581869207755,
-3.52339371578858));
#30373=CARTESIAN_POINT('Ctrl Pts',(-13.6998692722136,-10.8022296735859,
3.52339371578857));
#30374=CARTESIAN_POINT('Ctrl Pts',(-13.1736359892169,-11.4098124657167,
10.5701811473657));
#30375=CARTESIAN_POINT('Origin',(925.262771311062,711.593367601486,-6.00190077290402));
#30376=CARTESIAN_POINT('Origin',(866.592027874508,781.98118522266,6.0019007749759));
#30377=CARTESIAN_POINT('Ctrl Pts',(-15.1572749937985,-13.048259399505,-10.5701811473657));
#30378=CARTESIAN_POINT('Ctrl Pts',(-14.5554747099748,-13.7473298360336,
-3.52339371578857));
#30379=CARTESIAN_POINT('Ctrl Pts',(-13.9052382267708,-14.4046961615238,
3.52339371578859));
#30380=CARTESIAN_POINT('Ctrl Pts',(-13.2127719211995,-15.0140839465072,
10.5701811473657));
#30381=CARTESIAN_POINT('Ctrl Pts',(-14.5132212402647,-12.9190907809461,
-10.5701811473657));
#30382=CARTESIAN_POINT('Ctrl Pts',(-13.9173458198838,-13.5884619754075,
-3.52339371578857));
#30383=CARTESIAN_POINT('Ctrl Pts',(-13.2751904647928,-14.2165308697908,
3.52339371578859));
#30384=CARTESIAN_POINT('Ctrl Pts',(-12.5926885865131,-14.7973204175046,
10.5701811473657));
#30385=CARTESIAN_POINT('Ctrl Pts',(-13.5995757049001,-12.6202782881533,
-10.5701811473657));
#30386=CARTESIAN_POINT('Ctrl Pts',(-13.0175186447629,-13.2475051691757,
-3.52339371578856));
#30387=CARTESIAN_POINT('Ctrl Pts',(-12.3919905548983,-13.8343977109152,
3.52339371578858));
#30388=CARTESIAN_POINT('Ctrl Pts',(-11.7289876157166,-14.3753515760175,
10.5701811473657));
#30389=CARTESIAN_POINT('Ctrl Pts',(-12.9246670155629,-12.248189293022,-10.5701811473657));
#30390=CARTESIAN_POINT('Ctrl Pts',(-12.3597571218172,-12.8442910215617,
-3.52339371578857));
#30391=CARTESIAN_POINT('Ctrl Pts',(-11.7535751536795,-13.4012425136373,
3.52339371578859));
#30392=CARTESIAN_POINT('Ctrl Pts',(-11.1118483586176,-13.9137336641164,
10.5701811473657));
#30393=CARTESIAN_POINT('Ctrl Pts',(-12.6755702093799,-12.069510984306,-10.5701811473657));
#30394=CARTESIAN_POINT('Ctrl Pts',(-12.1189143573446,-12.6541218069529,
-3.52339371578856));
#30395=CARTESIAN_POINT('Ctrl Pts',(-11.5217426633956,-13.2001584938273,
3.52339371578858));
#30396=CARTESIAN_POINT('Ctrl Pts',(-10.8897758786539,-13.7024069727144,
10.5701811473657));
#30397=CARTESIAN_POINT('Ctrl Pts',(-12.6247588650341,-12.0239431039853,
-10.5701811473657));
#30398=CARTESIAN_POINT('Ctrl Pts',(-12.0701891316818,-12.6062131680627,
-3.52339371578857));
#30399=CARTESIAN_POINT('Ctrl Pts',(-11.4753127221783,-13.1500487521764,
3.52339371578859));
#30400=CARTESIAN_POINT('Ctrl Pts',(-10.8457349619751,-13.6502665652626,
10.5701811473657));
#30401=CARTESIAN_POINT('Ctrl Pts',(-12.6199210072709,-12.0194051204483,
-10.5701811473657));
#30402=CARTESIAN_POINT('Ctrl Pts',(-12.0655726308006,-12.6014499597276,
-3.52339371578857));
#30403=CARTESIAN_POINT('Ctrl Pts',(-11.4708966837347,-13.145079431777,3.52339371578859));
#30404=CARTESIAN_POINT('Ctrl Pts',(-10.8415692284374,-13.6451047025743,
10.5701811473657));
#30405=CARTESIAN_POINT('Origin',(796.999839514323,852.799843231391,6.00190076950591));
#30406=CARTESIAN_POINT('Origin',(861.440263999451,787.652834922883,-6.00190077470093));
#30407=CARTESIAN_POINT('Ctrl Pts',(-16.0120330027781,-11.983939215381,-8.00000002680495));
#30408=CARTESIAN_POINT('Ctrl Pts',(-15.9074534037436,-12.1236705642356,
-6.66666668453663));
#30409=CARTESIAN_POINT('Ctrl Pts',(-15.8010446219743,-12.262032890054,-5.33333334226832));
#30410=CARTESIAN_POINT('Ctrl Pts',(-15.6928431194365,-12.3989787816882,
-4.));
#30411=CARTESIAN_POINT('Ctrl Pts',(-15.6721361773262,-12.4380836405871,
-8.00000002680495));
#30412=CARTESIAN_POINT('Ctrl Pts',(-15.5635934034088,-12.574848851288,-6.66666668453663));
#30413=CARTESIAN_POINT('Ctrl Pts',(-15.4532603278107,-12.7101930951734,
-5.33333334226832));
#30414=CARTESIAN_POINT('Ctrl Pts',(-15.3411746529166,-12.8440701212508,
-4.));
#30415=CARTESIAN_POINT('Ctrl Pts',(-15.3129068596485,-12.8777583654387,
-8.00000002680495));
#30416=CARTESIAN_POINT('Ctrl Pts',(-15.2005271996287,-13.0113887087055,
-6.66666668453663));
#30417=CARTESIAN_POINT('Ctrl Pts',(-15.086398276462,-13.1435478582967,-5.33333334226832));
#30418=CARTESIAN_POINT('Ctrl Pts',(-14.970559091534,-13.2741906532108,-4.));
#30419=CARTESIAN_POINT('Ctrl Pts',(-14.9356440460772,-13.3013734978339,
-8.00000002680495));
#30420=CARTESIAN_POINT('Ctrl Pts',(-14.819567664012,-13.4317115809623,-6.66666668453663));
#30421=CARTESIAN_POINT('Ctrl Pts',(-14.7017850638858,-13.5605301399942,
-5.33333334226832));
#30422=CARTESIAN_POINT('Ctrl Pts',(-14.5823366050108,-13.6877850340427,
-4.));
#30423=CARTESIAN_POINT('Ctrl Pts',(-15.0224242123638,-13.2032863630154,
4.));
#30424=CARTESIAN_POINT('Ctrl Pts',(-14.9072038020326,-13.3343817459623,
5.33333334226731));
#30425=CARTESIAN_POINT('Ctrl Pts',(-14.7902672600361,-13.4639688100905,
6.66666668453462));
#30426=CARTESIAN_POINT('Ctrl Pts',(-14.6716546557766,-13.5920031511778,
8.00000002680193));
#30427=CARTESIAN_POINT('Ctrl Pts',(-14.6479434143837,-13.6293628148902,
4.));
#30428=CARTESIAN_POINT('Ctrl Pts',(-14.529004766833,-13.7571902561793,5.33333334226731));
#30429=CARTESIAN_POINT('Ctrl Pts',(-14.4083928242758,-13.8834606455681,
6.66666668453462));
#30430=CARTESIAN_POINT('Ctrl Pts',(-14.2861488016842,-14.0081308327355,
8.00000002680193));
#30431=CARTESIAN_POINT('Ctrl Pts',(-14.2553249994075,-14.0394973618063,
4.));
#30432=CARTESIAN_POINT('Ctrl Pts',(-14.1328072524584,-14.1638985607967,
5.33333334226731));
#30433=CARTESIAN_POINT('Ctrl Pts',(-14.0086610632827,-14.2866958557057,
6.66666668453462));
#30434=CARTESIAN_POINT('Ctrl Pts',(-13.8829288563289,-14.4078472847614,
8.00000002680193));
#30435=CARTESIAN_POINT('Ctrl Pts',(-13.845988700892,-14.4322069308464,4.));
#30436=CARTESIAN_POINT('Ctrl Pts',(-13.7200439354119,-14.5530359771683,
5.33333334226731));
#30437=CARTESIAN_POINT('Ctrl Pts',(-13.5925174320586,-14.6722163152528,
6.66666668453462));
#30438=CARTESIAN_POINT('Ctrl Pts',(-13.4634528889838,-14.78970710684,8.00000002680193));
#30439=CARTESIAN_POINT('Ctrl Pts',(-16.9832865676143,-3.9110718532786,-10.5701811473657));
#30440=CARTESIAN_POINT('Ctrl Pts',(-16.8029035694212,-4.69435998123014,
-3.52339371578858));
#30441=CARTESIAN_POINT('Ctrl Pts',(-16.5682462020274,-5.46514426027785,
3.52339371578857));
#30442=CARTESIAN_POINT('Ctrl Pts',(-16.2815542228302,-6.21606770943294,
10.5701811473657));
#30443=CARTESIAN_POINT('Ctrl Pts',(-16.9897389834304,-3.91260954390051,
-10.5701811473657));
#30444=CARTESIAN_POINT('Ctrl Pts',(-16.8092899584403,-4.69620648496864,
-3.52339371578857));
#30445=CARTESIAN_POINT('Ctrl Pts',(-16.5745328586343,-5.46726043199346,
3.52339371578856));
#30446=CARTESIAN_POINT('Ctrl Pts',(-16.2877328914428,-6.21848063638771,
10.5701811473657));
#30447=CARTESIAN_POINT('Ctrl Pts',(-17.0557613661602,-3.92991270646709,
-10.5701811473657));
#30448=CARTESIAN_POINT('Ctrl Pts',(-16.8745079936752,-4.71654017008887,
-3.52339371578859));
#30449=CARTESIAN_POINT('Ctrl Pts',(-16.6387524141882,-5.4906135647581,3.52339371578858));
#30450=CARTESIAN_POINT('Ctrl Pts',(-16.3507378099998,-6.2447243917162,10.5701811473657));
#30451=CARTESIAN_POINT('Ctrl Pts',(-17.3421065865861,-4.03937349046946,
-10.5701811473657));
#30452=CARTESIAN_POINT('Ctrl Pts',(-17.1558101221976,-4.83921977956265,
-3.52339371578857));
#30453=CARTESIAN_POINT('Ctrl Pts',(-16.9140820327623,-5.62612468710591,
3.52339371578857));
#30454=CARTESIAN_POINT('Ctrl Pts',(-16.6192493625611,-6.39263245314736,
10.5701811473657));
#30455=CARTESIAN_POINT('Ctrl Pts',(-18.0244436775357,-4.39766136660583,
-10.5701811473657));
#30456=CARTESIAN_POINT('Ctrl Pts',(-17.8216168089674,-5.228964691362,-3.52339371578859));
#30457=CARTESIAN_POINT('Ctrl Pts',(-17.5611932309208,-6.04622142745372,
3.52339371578858));
#30458=CARTESIAN_POINT('Ctrl Pts',(-17.2456495103602,-6.84160568476503,
10.5701811473657));
#30459=CARTESIAN_POINT('Ctrl Pts',(-18.7771350612562,-4.99556415374903,
-10.5701811473657));
#30460=CARTESIAN_POINT('Ctrl Pts',(-18.5467476225913,-5.86161661525365,
-3.52339371578857));
#30461=CARTESIAN_POINT('Ctrl Pts',(-18.2563169179228,-6.71160718410693,
3.52339371578856));
#30462=CARTESIAN_POINT('Ctrl Pts',(-17.9086833416741,-7.5376072656065,10.5701811473657));
#30463=CARTESIAN_POINT('Ctrl Pts',(-19.2397349758694,-5.46192256062901,
-10.5701811473657));
#30464=CARTESIAN_POINT('Ctrl Pts',(-18.9878250124769,-6.34928060711398,
-3.52339371578858));
#30465=CARTESIAN_POINT('Ctrl Pts',(-18.6744299210032,-7.21917793504633,
3.52339371578857));
#30466=CARTESIAN_POINT('Ctrl Pts',(-18.3025409945928,-8.06331154931088,
10.5701811473657));
#30467=CARTESIAN_POINT('Ctrl Pts',(-16.9832865676143,-3.9110718532786,-10.5701811473657));
#30468=CARTESIAN_POINT('Ctrl Pts',(-16.8029035694212,-4.69435998123014,
-3.52339371578857));
#30469=CARTESIAN_POINT('Ctrl Pts',(-16.5682462020274,-5.46514426027785,
3.52339371578857));
#30470=CARTESIAN_POINT('Ctrl Pts',(-16.2815542228302,-6.21606770943294,
10.5701811473657));
#30471=CARTESIAN_POINT('Origin',(1112.84186408303,352.22053088442,-6.00190077374882));
#30472=CARTESIAN_POINT('Origin',(1081.78345087015,438.430019756215,6.0019007731347));
#30473=CARTESIAN_POINT('Ctrl Pts',(-18.7059453597305,-7.07725995777758,
-10.5701811473657));
#30474=CARTESIAN_POINT('Ctrl Pts',(-18.3795342330452,-7.93999903151655,
-3.52339371578857));
#30475=CARTESIAN_POINT('Ctrl Pts',(-17.9933443266979,-8.78011521479376,
3.52339371578858));
#30476=CARTESIAN_POINT('Ctrl Pts',(-17.551061745707,-9.58958976753269,10.5701811473657));
#30477=CARTESIAN_POINT('Ctrl Pts',(-18.0565552078921,-7.17616029669807,
-10.5701811473657));
#30478=CARTESIAN_POINT('Ctrl Pts',(-17.7255539028776,-8.00896482032151,
-3.52339371578857));
#30479=CARTESIAN_POINT('Ctrl Pts',(-17.3369374692435,-8.81878654729076,
3.52339371578857));
#30480=CARTESIAN_POINT('Ctrl Pts',(-16.8942372196888,-9.59797954490641,
10.5701811473657));
#30481=CARTESIAN_POINT('Ctrl Pts',(-17.0958111919986,-7.20785561730533,
-10.5701811473657));
#30482=CARTESIAN_POINT('Ctrl Pts',(-16.7633806977716,-7.99633131329317,
-3.52339371578859));
#30483=CARTESIAN_POINT('Ctrl Pts',(-16.3763053385158,-8.76177323989865,
3.52339371578859));
#30484=CARTESIAN_POINT('Ctrl Pts',(-15.9383034918166,-9.4968639410666,10.5701811473657));
#30485=CARTESIAN_POINT('Ctrl Pts',(-16.3343420851164,-7.08903734849994,
-10.5701811473657));
#30486=CARTESIAN_POINT('Ctrl Pts',(-16.0073792251724,-7.84240030692992,
-3.52339371578856));
#30487=CARTESIAN_POINT('Ctrl Pts',(-15.6282430292672,-8.57309000696062,
3.52339371578857));
#30488=CARTESIAN_POINT('Ctrl Pts',(-15.2004993921048,-9.27415764976285,
10.5701811473657));
#30489=CARTESIAN_POINT('Ctrl Pts',(-16.0391560118722,-7.00633068060142,
-10.5701811473657));
#30490=CARTESIAN_POINT('Ctrl Pts',(-15.7160192927446,-7.74607267098129,
-3.52339371578858));
#30491=CARTESIAN_POINT('Ctrl Pts',(-15.3416169168209,-8.46342410640397,
3.52339371578859));
#30492=CARTESIAN_POINT('Ctrl Pts',(-14.9195414893457,-9.15152866611954,
10.5701811473657));
#30493=CARTESIAN_POINT('Ctrl Pts',(-15.9758234884504,-6.98088877109859,
-10.5701811473657));
#30494=CARTESIAN_POINT('Ctrl Pts',(-15.6538464930777,-7.7177176733025,-3.52339371578857));
#30495=CARTESIAN_POINT('Ctrl Pts',(-15.2808482452117,-8.43221567345478,
3.52339371578858));
#30496=CARTESIAN_POINT('Ctrl Pts',(-14.8603232378632,-9.11759493697741,
10.5701811473657));
#30497=CARTESIAN_POINT('Ctrl Pts',(-15.9697253074185,-6.97827910625621,
-10.5701811473657));
#30498=CARTESIAN_POINT('Ctrl Pts',(-15.647879288057,-7.71482065786623,-3.52339371578857));
#30499=CARTESIAN_POINT('Ctrl Pts',(-15.2749989187867,-8.42905641384053,
3.52339371578858));
#30500=CARTESIAN_POINT('Ctrl Pts',(-14.8546432677704,-9.11416913747482,
10.5701811473657));
#30501=CARTESIAN_POINT('Origin',(1040.60718933536,528.788968262105,6.00000003130594));
#30502=CARTESIAN_POINT('Origin',(1078.88826202955,445.514028129078,-6.00000002167999));
#30503=CARTESIAN_POINT('Ctrl Pts',(-19.1451378645417,-5.78478142609487,
-8.00000002680495));
#30504=CARTESIAN_POINT('Ctrl Pts',(-19.0946561230066,-5.95185427295671,
-6.66666668453663));
#30505=CARTESIAN_POINT('Ctrl Pts',(-19.0419872784984,-6.11826627631489,
-5.33333334226832));
#30506=CARTESIAN_POINT('Ctrl Pts',(-18.9871493784903,-6.28396041353657,
-4.));
#30507=CARTESIAN_POINT('Ctrl Pts',(-18.9810658672356,-6.32778915218907,
-8.00000002680495));
#30508=CARTESIAN_POINT('Ctrl Pts',(-18.9258454805117,-6.4934302265572,-6.66666668453663));
#30509=CARTESIAN_POINT('Ctrl Pts',(-18.8684567612354,-6.65834834813178,
-5.33333334226832));
#30510=CARTESIAN_POINT('Ctrl Pts',(-18.8089193192887,-6.82248716022144,
-4.));
#30511=CARTESIAN_POINT('Ctrl Pts',(-18.7938783406543,-6.86381190939714,
-8.00000002680495));
#30512=CARTESIAN_POINT('Ctrl Pts',(-18.733980272564,-7.02781946430487,-6.66666668453663));
#30513=CARTESIAN_POINT('Ctrl Pts',(-18.671935256931,-7.19104283260413,-5.33333334226832));
#30514=CARTESIAN_POINT('Ctrl Pts',(-18.6077644970973,-7.35342623757559,
-4.));
#30515=CARTESIAN_POINT('Ctrl Pts',(-18.5842521669411,-7.3909114049313,-8.00000002680495));
#30516=CARTESIAN_POINT('Ctrl Pts',(-18.5197542971393,-7.5530896006851,-6.66666668453663));
#30517=CARTESIAN_POINT('Ctrl Pts',(-18.4531333989669,-7.714423471804,-5.33333334226832));
#30518=CARTESIAN_POINT('Ctrl Pts',(-18.3844123006991,-7.87485773572478,
-4.));
#30519=CARTESIAN_POINT('Ctrl Pts',(-18.6322510729221,-7.26905908323709,
4.));
#30520=CARTESIAN_POINT('Ctrl Pts',(-18.5688165652349,-7.43165614846694,
5.33333334226731));
#30521=CARTESIAN_POINT('Ctrl Pts',(-18.5032535458669,-7.5934228092312,6.66666668453462));
#30522=CARTESIAN_POINT('Ctrl Pts',(-18.4355844806013,-7.75430363466721,
8.00000002680193));
#30523=CARTESIAN_POINT('Ctrl Pts',(-18.4260809595722,-7.79751995715235,
4.));
#30524=CARTESIAN_POINT('Ctrl Pts',(-18.3580347499332,-7.95831787374795,
5.33333334226731));
#30525=CARTESIAN_POINT('Ctrl Pts',(-18.2878836142101,-8.11822494076053,
6.66666668453462));
#30526=CARTESIAN_POINT('Ctrl Pts',(-18.215651523529,-8.2771865138012,8.00000002680193));
#30527=CARTESIAN_POINT('Ctrl Pts',(-18.1974146087534,-8.31720377098127,
4.));
#30528=CARTESIAN_POINT('Ctrl Pts',(-18.1248333019387,-8.47600619706092,
5.33333334226731));
#30529=CARTESIAN_POINT('Ctrl Pts',(-18.0501731924764,-8.63385840635456,
6.66666668453462));
#30530=CARTESIAN_POINT('Ctrl Pts',(-17.9734597945365,-8.7907064576789,8.00000002680193));
#30531=CARTESIAN_POINT('Ctrl Pts',(-17.9470788927071,-8.82623131460692,
4.));
#30532=CARTESIAN_POINT('Ctrl Pts',(-17.8700554936997,-8.9828491245528,5.33333334226731));
#30533=CARTESIAN_POINT('Ctrl Pts',(-17.7909818558573,-9.13845864174832,
6.66666668453462));
#30534=CARTESIAN_POINT('Ctrl Pts',(-17.7098850745029,-9.2930065451338,8.00000002680193));
#30535=CARTESIAN_POINT('Ctrl Pts',(-17.2967344200949,2.13342074610697,-10.5701811473657));
#30536=CARTESIAN_POINT('Ctrl Pts',(-17.3951301655649,1.33567605342619,-3.52339371578857));
#30537=CARTESIAN_POINT('Ctrl Pts',(-17.438248118605,0.531118207758816,3.52339371578858));
#30538=CARTESIAN_POINT('Ctrl Pts',(-17.4256767270215,-0.272573448002652,
10.5701811473657));
#30539=CARTESIAN_POINT('Ctrl Pts',(-17.30661823314,2.13456359558458,-10.5701811473657));
#30540=CARTESIAN_POINT('Ctrl Pts',(-17.4051107505851,1.33631723941113,-3.52339371578859));
#30541=CARTESIAN_POINT('Ctrl Pts',(-17.44816844044,0.531397153098151,3.52339371578859));
#30542=CARTESIAN_POINT('Ctrl Pts',(-17.4356237054098,-0.272804718797141,
10.5701811473657));
#30543=CARTESIAN_POINT('Ctrl Pts',(-17.4476874812993,2.1458310833851,-10.5701811473657));
#30544=CARTESIAN_POINT('Ctrl Pts',(-17.5466701372071,1.34110850589665,-3.52339371578856));
#30545=CARTESIAN_POINT('Ctrl Pts',(-17.5898512960806,0.529582293917762,
3.52339371578856));
#30546=CARTESIAN_POINT('Ctrl Pts',(-17.5768988000171,-0.28110150741043,
10.5701811473657));
#30547=CARTESIAN_POINT('Ctrl Pts',(-18.1762105609743,2.0916981433591,-10.5701811473657));
#30548=CARTESIAN_POINT('Ctrl Pts',(-18.272695299601,1.25337703656126,-3.52339371578858));
#30549=CARTESIAN_POINT('Ctrl Pts',(-18.3110538115194,0.408420040147072,
3.52339371578859));
#30550=CARTESIAN_POINT('Ctrl Pts',(-18.2909932845622,-0.435196672672694,
10.5701811473657));
#30551=CARTESIAN_POINT('Ctrl Pts',(-19.1552502593208,1.82120200778524,-10.5701811473657));
#30552=CARTESIAN_POINT('Ctrl Pts',(-19.2393500897156,0.937636019605693,
-3.52339371578856));
#30553=CARTESIAN_POINT('Ctrl Pts',(-19.2619362575252,0.0485819488860323,
3.52339371578857));
#30554=CARTESIAN_POINT('Ctrl Pts',(-19.2233689066293,-0.83813908750873,
10.5701811473657));
#30555=CARTESIAN_POINT('Ctrl Pts',(-19.947524519721,1.44784858846758,-10.5701811473657));
#30556=CARTESIAN_POINT('Ctrl Pts',(-20.0143009122587,0.527846498406004,
-3.52339371578857));
#30557=CARTESIAN_POINT('Ctrl Pts',(-20.0173282661883,-0.396777035596819,
3.52339371578858));
#30558=CARTESIAN_POINT('Ctrl Pts',(-19.9565776860253,-1.31719666779067,
10.5701811473657));
#30559=CARTESIAN_POINT('Ctrl Pts',(-17.2967344200949,2.13342074610697,-10.5701811473657));
#30560=CARTESIAN_POINT('Ctrl Pts',(-17.3951301655649,1.33567605342619,-3.52339371578857));
#30561=CARTESIAN_POINT('Ctrl Pts',(-17.438248118605,0.531118207758816,3.52339371578858));
#30562=CARTESIAN_POINT('Ctrl Pts',(-17.4256767270215,-0.272573448002652,
10.5701811473657));
#30563=CARTESIAN_POINT('Origin',(1166.19580421585,-49.6353000928601,-6.00190077381567));
#30564=CARTESIAN_POINT('Origin',(1166.49582424222,41.9977233811867,6.00190077396116));
#30565=CARTESIAN_POINT('Ctrl Pts',(-19.9984042844753,-0.25263884473002,
-10.5701811473657));
#30566=CARTESIAN_POINT('Ctrl Pts',(-19.9867522990396,-1.1749875663182,-3.52339371578857));
#30567=CARTESIAN_POINT('Ctrl Pts',(-19.9111891512377,-2.09652327146644,
3.52339371578858));
#30568=CARTESIAN_POINT('Ctrl Pts',(-19.7724360761246,-3.00845008713017,
10.5701811473657));
#30569=CARTESIAN_POINT('Ctrl Pts',(-19.4220030588742,-0.567679276212883,
-10.5701811473657));
#30570=CARTESIAN_POINT('Ctrl Pts',(-19.3957994976135,-1.46346865540102,
-3.52339371578857));
#30571=CARTESIAN_POINT('Ctrl Pts',(-19.3075948457377,-2.35736680471636,
3.52339371578857));
#30572=CARTESIAN_POINT('Ctrl Pts',(-19.158092388734,-3.24098111754682,10.5701811473657));
#30573=CARTESIAN_POINT('Ctrl Pts',(-18.5300476618897,-0.926064023779522,
-10.5701811473657));
#30574=CARTESIAN_POINT('Ctrl Pts',(-18.487339750091,-1.78068674224966,-3.52339371578858));
#30575=CARTESIAN_POINT('Ctrl Pts',(-18.385403393272,-2.63235550918581,3.52339371578858));
#30576=CARTESIAN_POINT('Ctrl Pts',(-18.225232117009,-3.47292027106663,10.5701811473657));
#30577=CARTESIAN_POINT('Ctrl Pts',(-17.7738570494612,-1.07484441701443,
-10.5701811473657));
#30578=CARTESIAN_POINT('Ctrl Pts',(-17.7242777697192,-1.89460191404476,
-3.52339371578857));
#30579=CARTESIAN_POINT('Ctrl Pts',(-17.617916529176,-2.71089820703327,3.52339371578857));
#30580=CARTESIAN_POINT('Ctrl Pts',(-17.4557482454186,-3.51598323773522,
10.5701811473657));
#30581=CARTESIAN_POINT('Ctrl Pts',(-17.4681851433452,-1.09808483323811,
-10.5701811473657));
#30582=CARTESIAN_POINT('Ctrl Pts',(-17.4175426144497,-1.90373418987339,
-3.52339371578858));
#30583=CARTESIAN_POINT('Ctrl Pts',(-17.311067802437,-2.70587750222895,3.52339371578858));
#30584=CARTESIAN_POINT('Ctrl Pts',(-17.1497922579605,-3.49684257752213,
10.5701811473657));
#30585=CARTESIAN_POINT('Ctrl Pts',(-17.3999680211064,-1.09583622546326,
-10.5701811473657));
#30586=CARTESIAN_POINT('Ctrl Pts',(-17.3494189412302,-1.898351525751,-3.52339371578857));
#30587=CARTESIAN_POINT('Ctrl Pts',(-17.2432879485624,-2.69733293825569,
3.52339371578857));
#30588=CARTESIAN_POINT('Ctrl Pts',(-17.0825372162436,-3.48520679791294,
10.5701811473657));
#30589=CARTESIAN_POINT('Ctrl Pts',(-17.3933450474474,-1.09546964341861,
-10.5701811473657));
#30590=CARTESIAN_POINT('Ctrl Pts',(-17.342820765071,-1.89767012603957,-3.52339371578857));
#30591=CARTESIAN_POINT('Ctrl Pts',(-17.2367108492585,-2.6963647927712,3.52339371578858));
#30592=CARTESIAN_POINT('Ctrl Pts',(-17.0760280978245,-3.48393026358523,
10.5701811473657));
#30593=CARTESIAN_POINT('Origin',(1158.70737566477,140.990471381257,6.00000003038105));
#30594=CARTESIAN_POINT('Origin',(1166.19811020393,49.6447266790377,-6.00000002178777));
#30595=CARTESIAN_POINT('Ctrl Pts',(-19.9690565476993,1.1121063774595,-8.00000002680495));
#30596=CARTESIAN_POINT('Ctrl Pts',(-19.9787615067239,0.937843483654576,
-6.66666668453663));
#30597=CARTESIAN_POINT('Ctrl Pts',(-19.9861852394339,0.763453546341202,
-5.33333334226832));
#30598=CARTESIAN_POINT('Ctrl Pts',(-19.9913252020177,0.588996321866058,
-4.));
#30599=CARTESIAN_POINT('Ctrl Pts',(-20.0005988828589,0.545730096184685,
-8.00000002680495));
#30600=CARTESIAN_POINT('Ctrl Pts',(-20.0053612769335,0.371191916320092,
-6.66666668453664));
#30601=CARTESIAN_POINT('Ctrl Pts',(-20.0078388404912,0.196591476450452,
-5.33333334226832));
#30602=CARTESIAN_POINT('Ctrl Pts',(-20.0080307256696,0.0219884415173641,
-4.));
#30603=CARTESIAN_POINT('Ctrl Pts',(-20.0080307256734,-0.0219884380071468,
-8.00000002680495));
#30604=CARTESIAN_POINT('Ctrl Pts',(-20.0078388405257,-0.196591472940268,
-6.66666668453663));
#30605=CARTESIAN_POINT('Ctrl Pts',(-20.0053612769986,-0.371191912810343,
-5.33333334226832));
#30606=CARTESIAN_POINT('Ctrl Pts',(-20.0005988829546,-0.545730092675771,
-4.));
#30607=CARTESIAN_POINT('Ctrl Pts',(-19.991325202121,-0.588996318358771,
-8.00000002680495));
#30608=CARTESIAN_POINT('Ctrl Pts',(-19.9861852395679,-0.763453542834817,
-6.66666668453663));
#30609=CARTESIAN_POINT('Ctrl Pts',(-19.9787615068885,-0.937843480149494,
-5.33333334226832));
#30610=CARTESIAN_POINT('Ctrl Pts',(-19.9690565478944,-1.11210637395612,
-4.));
#30611=CARTESIAN_POINT('Ctrl Pts',(-19.9947534713468,-0.458075998134003,
4.));
#30612=CARTESIAN_POINT('Ctrl Pts',(-19.9907560041241,-0.632563139902935,
5.33333334226731));
#30613=CARTESIAN_POINT('Ctrl Pts',(-19.9844743751274,-0.806997950593388,
6.66666668453462));
#30614=CARTESIAN_POINT('Ctrl Pts',(-19.9759107368159,-0.981320658482395,
8.00000002680193));
#30615=CARTESIAN_POINT('Ctrl Pts',(-19.9817612010437,-1.02518111344366,
4.));
#30616=CARTESIAN_POINT('Ctrl Pts',(-19.972814806454,-1.19955490347979,5.33333334226731));
#30617=CARTESIAN_POINT('Ctrl Pts',(-19.9615857398537,-1.37381149585751,
6.66666668453462));
#30618=CARTESIAN_POINT('Ctrl Pts',(-19.9480778372514,-1.54789134303979,
8.00000002680193));
#30619=CARTESIAN_POINT('Ctrl Pts',(-19.9446274510471,-1.59173265652136,
4.));
#30620=CARTESIAN_POINT('Ctrl Pts',(-19.9307369611545,-1.76578239343086,
5.33333334226731));
#30621=CARTESIAN_POINT('Ctrl Pts',(-19.9145680424726,-1.93965021101785,
6.66666668453462));
#30622=CARTESIAN_POINT('Ctrl Pts',(-19.8961262215074,-2.11327669479037,
8.00000002680193));
#30623=CARTESIAN_POINT('Ctrl Pts',(-19.8834864993867,-2.15568194052487,
4.));
#30624=CARTESIAN_POINT('Ctrl Pts',(-19.8646746255167,-2.32919809478258,
5.33333334226731));
#30625=CARTESIAN_POINT('Ctrl Pts',(-19.8435913009115,-2.50246798676344,
6.66666668453462));
#30626=CARTESIAN_POINT('Ctrl Pts',(-19.8202437499699,-2.67543224391478,
8.00000002680193));
#30627=CARTESIAN_POINT('Ctrl Pts',(-15.5239408288993,7.92059131757517,-10.5701811473657));
#30628=CARTESIAN_POINT('Ctrl Pts',(-15.8892473389622,7.2046098435602,-3.52339371578858));
#30629=CARTESIAN_POINT('Ctrl Pts',(-16.2049399509463,6.46331998146983,3.52339371578858));
#30630=CARTESIAN_POINT('Ctrl Pts',(-16.4680054423355,5.7037971940124,10.5701811473657));
#30631=CARTESIAN_POINT('Ctrl Pts',(-15.5328376975401,7.92504570795004,-10.5701811473657));
#30632=CARTESIAN_POINT('Ctrl Pts',(-15.8984067225336,7.20862592241769,-3.52339371578858));
#30633=CARTESIAN_POINT('Ctrl Pts',(-16.2141665992448,6.4669750542426,3.52339371578858));
#30634=CARTESIAN_POINT('Ctrl Pts',(-16.4774316437956,5.70698193752737,10.5701811473657));
#30635=CARTESIAN_POINT('Ctrl Pts',(-15.6615319819844,7.98385473667208,-10.5701811473657));
#30636=CARTESIAN_POINT('Ctrl Pts',(-16.0297765846167,7.2615169309867,-3.52339371578857));
#30637=CARTESIAN_POINT('Ctrl Pts',(-16.3479082547577,6.51370272165337,3.52339371578857));
#30638=CARTESIAN_POINT('Ctrl Pts',(-16.6130070797081,5.74747912119454,10.5701811473657));
#30639=CARTESIAN_POINT('Ctrl Pts',(-16.3646266973296,8.18213889106893,-10.5701811473657));
#30640=CARTESIAN_POINT('Ctrl Pts',(-16.7420154026786,7.42737444544043,-3.52339371578858));
#30641=CARTESIAN_POINT('Ctrl Pts',(-17.0670469793702,6.64649736821331,3.52339371578859));
#30642=CARTESIAN_POINT('Ctrl Pts',(-17.3367301609262,5.8468958518967,10.5701811473657));
#30643=CARTESIAN_POINT('Ctrl Pts',(-17.3771604885591,8.26285160192196,-10.5701811473657));
#30644=CARTESIAN_POINT('Ctrl Pts',(-17.7583858480757,7.46133495538845,-3.52339371578858));
#30645=CARTESIAN_POINT('Ctrl Pts',(-18.0836843042383,6.63362228641827,3.52339371578858));
#30646=CARTESIAN_POINT('Ctrl Pts',(-18.3507193026914,5.78718621735566,10.5701811473657));
#30647=CARTESIAN_POINT('Ctrl Pts',(-18.2493498864903,8.18298767653274,-10.5701811473657));
#30648=CARTESIAN_POINT('Ctrl Pts',(-18.6267584091773,7.34130729564938,-3.52339371578858));
#30649=CARTESIAN_POINT('Ctrl Pts',(-18.9458430530205,6.47348072277112,3.52339371578858));
#30650=CARTESIAN_POINT('Ctrl Pts',(-19.2035582177667,5.58779118889344,10.5701811473657));
#30651=CARTESIAN_POINT('Ctrl Pts',(-15.5239408288993,7.92059131757517,-10.5701811473657));
#30652=CARTESIAN_POINT('Ctrl Pts',(-15.8892473389622,7.2046098435602,-3.52339371578858));
#30653=CARTESIAN_POINT('Ctrl Pts',(-16.2049399509463,6.46331998146983,3.52339371578858));
#30654=CARTESIAN_POINT('Ctrl Pts',(-16.4680054423355,5.7037971940124,10.5701811473657));
#30655=CARTESIAN_POINT('Origin',(1078.88931916181,-445.504381322801,-6.00190077291764));
#30656=CARTESIAN_POINT('Origin',(1110.51158560098,-359.500118244419,6.00190077332084));
#30657=CARTESIAN_POINT('Ctrl Pts',(-18.8787605074989,6.60245424154421,-10.5701811473657));
#30658=CARTESIAN_POINT('Ctrl Pts',(-19.1832730647213,5.73174474034773,-3.52339371578858));
#30659=CARTESIAN_POINT('Ctrl Pts',(-19.427450706283,4.83994031978785,3.52339371578858));
#30660=CARTESIAN_POINT('Ctrl Pts',(-19.6089628056837,3.93555307377479,10.5701811473657));
#30661=CARTESIAN_POINT('Ctrl Pts',(-18.4448707027188,6.10927224303739,-10.5701811473657));
#30662=CARTESIAN_POINT('Ctrl Pts',(-18.7266254214233,5.25854342785787,-3.52339371578856));
#30663=CARTESIAN_POINT('Ctrl Pts',(-18.949471334084,4.38838616553552,3.52339371578856));
#30664=CARTESIAN_POINT('Ctrl Pts',(-19.1111988723671,3.50692746437597,10.5701811473657));
#30665=CARTESIAN_POINT('Ctrl Pts',(-17.7292751069179,5.46743648480893,-10.5701811473657));
#30666=CARTESIAN_POINT('Ctrl Pts',(-17.981440982012,4.64974685659201,-3.52339371578859));
#30667=CARTESIAN_POINT('Ctrl Pts',(-18.1769404144146,3.81457658575116,3.52339371578859));
#30668=CARTESIAN_POINT('Ctrl Pts',(-18.3139187283814,2.96992227885496,10.5701811473657));
#30669=CARTESIAN_POINT('Ctrl Pts',(-17.0695785919953,5.06899457590414,-10.5701811473657));
#30670=CARTESIAN_POINT('Ctrl Pts',(-17.3033628853044,4.28171739274745,-3.52339371578857));
#30671=CARTESIAN_POINT('Ctrl Pts',(-17.4826059195935,3.47827239356548,3.52339371578857));
#30672=CARTESIAN_POINT('Ctrl Pts',(-17.6055728776112,2.66627511145608,10.5701811473657));
#30673=CARTESIAN_POINT('Ctrl Pts',(-16.7902899423754,4.94260967296501,-10.5701811473657));
#30674=CARTESIAN_POINT('Ctrl Pts',(-17.018249840101,4.16822615260271,-3.52339371578858));
#30675=CARTESIAN_POINT('Ctrl Pts',(-17.1925455301966,3.37804172155667,3.52339371578858));
#30676=CARTESIAN_POINT('Ctrl Pts',(-17.3115220795561,2.57961819216749,10.5701811473657));
#30677=CARTESIAN_POINT('Ctrl Pts',(-16.7254196142394,4.92139034178336,-10.5701811473657));
#30678=CARTESIAN_POINT('Ctrl Pts',(-16.9523954149176,4.14998383249092,-3.52339371578857));
#30679=CARTESIAN_POINT('Ctrl Pts',(-17.1259326414904,3.36288795769156,3.52339371578857));
#30680=CARTESIAN_POINT('Ctrl Pts',(-17.244345094947,2.56754871715414,10.5701811473657));
#30681=CARTESIAN_POINT('Ctrl Pts',(-16.7190706763204,4.91946962582534,-10.5701811473657));
#30682=CARTESIAN_POINT('Ctrl Pts',(-16.9459621050428,4.14836742961573,-3.52339371578858));
#30683=CARTESIAN_POINT('Ctrl Pts',(-17.1194210645505,3.36154821641249,3.52339371578858));
#30684=CARTESIAN_POINT('Ctrl Pts',(-17.2377919239465,2.56652201742732,10.5701811473657));
#30685=CARTESIAN_POINT('Origin',(1137.05035178694,-263.813557134597,6.00000003104242));
#30686=CARTESIAN_POINT('Origin',(1112.84725512312,-352.212461496002,-6.00000002249655));
#30687=CARTESIAN_POINT('Ctrl Pts',(-18.3844122993175,7.87485773895015,-8.00000002680495));
#30688=CARTESIAN_POINT('Ctrl Pts',(-18.4531333976134,7.71442347504143,-6.66666668453663));
#30689=CARTESIAN_POINT('Ctrl Pts',(-18.5197542958142,7.55308960393422,-5.33333334226832));
#30690=CARTESIAN_POINT('Ctrl Pts',(-18.5842521656445,7.39091140819173,-4.));
#30691=CARTESIAN_POINT('Ctrl Pts',(-18.6077644958072,7.35342624084014,-8.00000002680495));
#30692=CARTESIAN_POINT('Ctrl Pts',(-18.6719352556694,7.19104283587995,-6.66666668453663));
#30693=CARTESIAN_POINT('Ctrl Pts',(-18.7339802713311,7.02781946759157,-5.33333334226832));
#30694=CARTESIAN_POINT('Ctrl Pts',(-18.7938783394501,6.86381191269434,-4.));
#30695=CARTESIAN_POINT('Ctrl Pts',(-18.8089193180918,6.82248716352129,-8.00000002680495));
#30696=CARTESIAN_POINT('Ctrl Pts',(-18.8684567600673,6.65834835144207,-6.66666668453664));
#30697=CARTESIAN_POINT('Ctrl Pts',(-18.9258454793725,6.49343022987756,-5.33333334226832));
#30698=CARTESIAN_POINT('Ctrl Pts',(-18.9810658661255,6.32778915551912,-4.));
#30699=CARTESIAN_POINT('Ctrl Pts',(-18.9871493773879,6.28396041686769,-8.00000002680495));
#30700=CARTESIAN_POINT('Ctrl Pts',(-19.041987277425,6.11826627965563,-6.66666668453663));
#30701=CARTESIAN_POINT('Ctrl Pts',(-19.0946561219624,5.95185427630669,-5.33333334226832));
#30702=CARTESIAN_POINT('Ctrl Pts',(-19.1451378635268,5.78478142945371,-4.));
#30703=CARTESIAN_POINT('Ctrl Pts',(-18.9455935099938,6.40815781282578,4.));
#30704=CARTESIAN_POINT('Ctrl Pts',(-19.0015152367791,6.24282631897104,5.33333334226731));
#30705=CARTESIAN_POINT('Ctrl Pts',(-19.0552726553178,6.07676277090728,6.66666668453462));
#30706=CARTESIAN_POINT('Ctrl Pts',(-19.1068473451265,5.91002407186586,8.00000002680193));
#30707=CARTESIAN_POINT('Ctrl Pts',(-19.1273461422817,5.87080970260818,4.));
#30708=CARTESIAN_POINT('Ctrl Pts',(-19.1785786299635,5.70389209169293,5.33333334226731));
#30709=CARTESIAN_POINT('Ctrl Pts',(-19.2276260236414,5.53630389074424,6.66666668453462));
#30710=CARTESIAN_POINT('Ctrl Pts',(-19.2744715615271,5.36810236813544,8.00000002680193));
#30711=CARTESIAN_POINT('Ctrl Pts',(-19.2862238713926,5.32572490778712,4.));
#30712=CARTESIAN_POINT('Ctrl Pts',(-19.332699596505,5.15742082701961,5.33333334226731));
#30713=CARTESIAN_POINT('Ctrl Pts',(-19.3769720788243,4.98850842595595,6.66666668453462));
#30714=CARTESIAN_POINT('Ctrl Pts',(-19.4190261906145,4.81904542613221,8.00000002680193));
#30715=CARTESIAN_POINT('Ctrl Pts',(-19.4216521852328,4.77487449006159,4.));
#30716=CARTESIAN_POINT('Ctrl Pts',(-19.4633208261226,4.60538860052122,5.33333334226731));
#30717=CARTESIAN_POINT('Ctrl Pts',(-19.5027707748587,4.43535723991918,6.66666668453462));
#30718=CARTESIAN_POINT('Ctrl Pts',(-19.5399885135466,4.264838671095,8.00000002680193));
#30719=CARTESIAN_POINT('Ctrl Pts',(-11.8787308647727,12.7524216806657,-10.5701811473657));
#30720=CARTESIAN_POINT('Ctrl Pts',(-12.4668867829649,12.2045613578439,-3.52339371578857));
#30721=CARTESIAN_POINT('Ctrl Pts',(-13.017076865761,11.6159499769718,3.52339371578858));
#30722=CARTESIAN_POINT('Ctrl Pts',(-13.5240496594282,10.9922057153483,10.5701811473657));
#30723=CARTESIAN_POINT('Ctrl Pts',(-11.8855676953475,12.7596503467182,-10.5701811473657));
#30724=CARTESIAN_POINT('Ctrl Pts',(-12.4741202082508,12.2114679311921,-3.52339371578859));
#30725=CARTESIAN_POINT('Ctrl Pts',(-13.0244969705674,11.6225403214579,3.52339371578859));
#30726=CARTESIAN_POINT('Ctrl Pts',(-13.5318181449482,10.9984223461024,10.5701811473657));
#30727=CARTESIAN_POINT('Ctrl Pts',(-11.9863857707236,12.8589190332253,-10.5701811473657));
#30728=CARTESIAN_POINT('Ctrl Pts',(-12.5794765862914,12.3060905992793,-3.52339371578856));
#30729=CARTESIAN_POINT('Ctrl Pts',(-13.134188756619,11.7121827924541,3.52339371578857));
#30730=CARTESIAN_POINT('Ctrl Pts',(-13.6453640718523,11.082837267336,10.5701811473657));
#30731=CARTESIAN_POINT('Ctrl Pts',(-12.5792608243633,13.2857117717956,-10.5701811473657));
#30732=CARTESIAN_POINT('Ctrl Pts',(-13.1920348426224,12.7055397408969,-3.52339371578859));
#30733=CARTESIAN_POINT('Ctrl Pts',(-13.764538166676,12.0829230390914,3.52339371578859));
#30734=CARTESIAN_POINT('Ctrl Pts',(-14.2914372817995,11.4237804859417,10.5701811473657));
#30735=CARTESIAN_POINT('Ctrl Pts',(-13.5031269323654,13.7078792049972,-10.5701811473657));
#30736=CARTESIAN_POINT('Ctrl Pts',(-14.1354964096488,13.0850867185779,-3.52339371578856));
#30737=CARTESIAN_POINT('Ctrl Pts',(-14.7242713589907,12.4185498968891,3.52339371578857));
#30738=CARTESIAN_POINT('Ctrl Pts',(-15.264700349594,11.7144915590679,10.5701811473657));
#30739=CARTESIAN_POINT('Ctrl Pts',(-14.3500311789428,13.9311379708684,-10.5701811473657));
#30740=CARTESIAN_POINT('Ctrl Pts',(-14.9925508077551,13.2692985198616,-3.52339371578857));
#30741=CARTESIAN_POINT('Ctrl Pts',(-15.5892064466918,12.5629417452578,3.52339371578858));
#30742=CARTESIAN_POINT('Ctrl Pts',(-16.1343031376281,11.818809680468,10.5701811473657));
#30743=CARTESIAN_POINT('Ctrl Pts',(-11.8787308647727,12.7524216806657,-10.5701811473657));
#30744=CARTESIAN_POINT('Ctrl Pts',(-12.4668867829649,12.2045613578439,-3.52339371578857));
#30745=CARTESIAN_POINT('Ctrl Pts',(-13.017076865761,11.6159499769718,3.52339371578858));
#30746=CARTESIAN_POINT('Ctrl Pts',(-13.5240496594282,10.9922057153483,10.5701811473657));
#30747=CARTESIAN_POINT('Origin',(861.452859530637,-787.639059256886,-6.00190077370807));
#30748=CARTESIAN_POINT('Origin',(920.583260312982,-717.636939968109,6.00190077196441));
#30749=CARTESIAN_POINT('Ctrl Pts',(-15.482059589238,12.6611938961255,-10.5701811473657));
#30750=CARTESIAN_POINT('Ctrl Pts',(-16.0660079802072,11.9471440316185,-3.52339371578857));
#30751=CARTESIAN_POINT('Ctrl Pts',(-16.6004749835089,11.1926356705744,3.52339371578858));
#30752=CARTESIAN_POINT('Ctrl Pts',(-17.0803592190431,10.4048704436167,10.5701811473657));
#30753=CARTESIAN_POINT('Ctrl Pts',(-15.243014719731,12.0493553593938,-10.5701811473657));
#30754=CARTESIAN_POINT('Ctrl Pts',(-15.7987439407825,11.346297558895,-3.52339371578858));
#30755=CARTESIAN_POINT('Ctrl Pts',(-16.3057619116501,10.6048349916867,3.5233937157886));
#30756=CARTESIAN_POINT('Ctrl Pts',(-16.7592127169954,9.83184883068219,10.5701811473657));
#30757=CARTESIAN_POINT('Ctrl Pts',(-14.7900894187725,11.2014790072182,-10.5701811473657));
#30758=CARTESIAN_POINT('Ctrl Pts',(-15.3067141545056,10.5193479063346,-3.52339371578855));
#30759=CARTESIAN_POINT('Ctrl Pts',(-15.7760686536943,9.80141015840479,3.52339371578856));
#30760=CARTESIAN_POINT('Ctrl Pts',(-16.1936749515119,9.0545440817974,10.5701811473657));
#30761=CARTESIAN_POINT('Ctrl Pts',(-14.3064567126843,10.601436531037,-10.5701811473657));
#30762=CARTESIAN_POINT('Ctrl Pts',(-14.7954067429393,9.94159690905795,-3.52339371578859));
#30763=CARTESIAN_POINT('Ctrl Pts',(-15.2386344956153,9.24791058685751,3.5233937157886));
#30764=CARTESIAN_POINT('Ctrl Pts',(-15.6319050654347,8.52693990941373,10.5701811473657));
#30765=CARTESIAN_POINT('Ctrl Pts',(-14.087237713241,10.3871512277472,-10.5701811473657));
#30766=CARTESIAN_POINT('Ctrl Pts',(-14.566304709585,9.7374356249061,-3.52339371578856));
#30767=CARTESIAN_POINT('Ctrl Pts',(-15.000348095257,9.05451802789469,3.52339371578857));
#30768=CARTESIAN_POINT('Ctrl Pts',(-15.3852264106871,8.34493770554008,10.5701811473657));
#30769=CARTESIAN_POINT('Ctrl Pts',(-14.0335387609796,10.345024601817,-10.5701811473657));
#30770=CARTESIAN_POINT('Ctrl Pts',(-14.5106628108441,9.69776989328862,-3.52339371578858));
#30771=CARTESIAN_POINT('Ctrl Pts',(-14.9429371059958,9.01749493499381,3.52339371578859));
#30772=CARTESIAN_POINT('Ctrl Pts',(-15.3262304557589,8.31061996394269,10.5701811473657));
#30773=CARTESIAN_POINT('Ctrl Pts',(-14.0282296344253,10.3410482545556,-10.5701811473657));
#30774=CARTESIAN_POINT('Ctrl Pts',(-14.5051703193816,9.69405064987659,-3.52339371578857));
#30775=CARTESIAN_POINT('Ctrl Pts',(-14.9372764437114,9.01400889952889,3.52339371578858));
#30776=CARTESIAN_POINT('Ctrl Pts',(-15.3204236413265,8.30741386530726,10.5701811473657));
#30777=CARTESIAN_POINT('Origin',(978.241467157012,-636.804482366658,6.00190077771329));
#30778=CARTESIAN_POINT('Origin',(925.27415056307,-711.578571311033,-6.00190076986674));
#30779=CARTESIAN_POINT('Ctrl Pts',(-14.5823366026094,13.687785036601,-8.00000002680495));
#30780=CARTESIAN_POINT('Ctrl Pts',(-14.7017850615068,13.5605301425734,-6.66666668453663));
#30781=CARTESIAN_POINT('Ctrl Pts',(-14.8195676616555,13.4317115835623,-5.33333334226832));
#30782=CARTESIAN_POINT('Ctrl Pts',(-14.9356440437436,13.3013735004542,-4.));
#30783=CARTESIAN_POINT('Ctrl Pts',(-14.9705590892051,13.2741906558372,-8.00000002680495));
#30784=CARTESIAN_POINT('Ctrl Pts',(-15.0863982741561,13.1435478609434,-6.66666668453664));
#30785=CARTESIAN_POINT('Ctrl Pts',(-15.200527197346,13.0113887113723,-5.33333334226832));
#30786=CARTESIAN_POINT('Ctrl Pts',(-15.3129068573893,12.8777583681252,-4.));
#30787=CARTESIAN_POINT('Ctrl Pts',(-15.3411746506633,12.8440701239422,-8.00000002680495));
#30788=CARTESIAN_POINT('Ctrl Pts',(-15.4532603255808,12.7101930978845,-6.66666668453663));
#30789=CARTESIAN_POINT('Ctrl Pts',(-15.5635934012027,12.5748488540185,-5.33333334226832));
#30790=CARTESIAN_POINT('Ctrl Pts',(-15.6721361751441,12.4380836433366,-4.));
#30791=CARTESIAN_POINT('Ctrl Pts',(-15.6928431172612,12.3989787844414,-8.00000002680495));
#30792=CARTESIAN_POINT('Ctrl Pts',(-15.801044619823,12.2620328928261,-6.66666668453663));
#30793=CARTESIAN_POINT('Ctrl Pts',(-15.9074534016166,12.1236705670264,-5.33333334226832));
#30794=CARTESIAN_POINT('Ctrl Pts',(-16.0120330006756,11.9839392181901,-4.));
#30795=CARTESIAN_POINT('Ctrl Pts',(-15.6113153641544,12.5014732172219,4.));
#30796=CARTESIAN_POINT('Ctrl Pts',(-15.7204112993806,12.3652387894732,5.33333334226731));
#30797=CARTESIAN_POINT('Ctrl Pts',(-15.8277238274038,12.2275762187696,6.66666668453462));
#30798=CARTESIAN_POINT('Ctrl Pts',(-15.9332161765804,12.0885326764813,8.00000002680193));
#30799=CARTESIAN_POINT('Ctrl Pts',(-15.9658908491962,12.0586942246021,4.));
#30800=CARTESIAN_POINT('Ctrl Pts',(-16.0711228250241,11.9193655201257,5.33333334226731));
#30801=CARTESIAN_POINT('Ctrl Pts',(-16.1745308394401,11.7786593209788,6.66666668453462));
#30802=CARTESIAN_POINT('Ctrl Pts',(-16.2760795545783,11.6366237089603,8.00000002680193));
#30803=CARTESIAN_POINT('Ctrl Pts',(-16.3016170584982,11.6008214488879,4.));
#30804=CARTESIAN_POINT('Ctrl Pts',(-16.4028533402584,11.4585629803066,5.33333334226731));
#30805=CARTESIAN_POINT('Ctrl Pts',(-16.502227308819,11.3149793242161,6.66666668453462));
#30806=CARTESIAN_POINT('Ctrl Pts',(-16.5997050068301,11.1701195471274,8.00000002680193));
#30807=CARTESIAN_POINT('Ctrl Pts',(-16.6172799844809,11.1295105875044,4.));
#30808=CARTESIAN_POINT('Ctrl Pts',(-16.7144032870754,10.9844974623052,5.33333334226731));
#30809=CARTESIAN_POINT('Ctrl Pts',(-16.8096282631161,10.8382129245662,6.66666668453462));
#30810=CARTESIAN_POINT('Ctrl Pts',(-16.9029222828724,10.6907071000555,8.00000002680193));
#30811=CARTESIAN_POINT('Ctrl Pts',(-6.80077064695807,16.0461217833684,-10.5701811473657));
#30812=CARTESIAN_POINT('Ctrl Pts',(-7.54083568928884,15.7324626522293,-3.52339371578857));
#30813=CARTESIAN_POINT('Ctrl Pts',(-8.25916219897089,15.3675249720875,3.52339371578858));
#30814=CARTESIAN_POINT('Ctrl Pts',(-8.94889389387818,14.9547919997346,10.5701811473657));
#30815=CARTESIAN_POINT('Ctrl Pts',(-6.80340542685265,16.0522091553162,-10.5701811473657));
#30816=CARTESIAN_POINT('Ctrl Pts',(-7.54376312530191,15.7384313756406,-3.52339371578856));
#30817=CARTESIAN_POINT('Ctrl Pts',(-8.26233788774701,15.3733486508931,3.52339371578857));
#30818=CARTESIAN_POINT('Ctrl Pts',(-8.95234307759614,14.9604578001197,10.5701811473657));
#30819=CARTESIAN_POINT('Ctrl Pts',(-6.83191060264015,16.1142229628818,-10.5701811473657));
#30820=CARTESIAN_POINT('Ctrl Pts',(-7.57511310971921,15.7991268108383,-3.52339371578858));
#30821=CARTESIAN_POINT('Ctrl Pts',(-8.29648793938119,15.4325364319901,3.52339371578859));
#30822=CARTESIAN_POINT('Ctrl Pts',(-8.98912891724121,15.0179474459445,10.5701811473657));
#30823=CARTESIAN_POINT('Ctrl Pts',(-6.98943179288406,16.3772101395067,-10.5701811473657));
#30824=CARTESIAN_POINT('Ctrl Pts',(-7.74477657805422,16.0548520865033,-3.52339371578856));
#30825=CARTESIAN_POINT('Ctrl Pts',(-8.47775084446518,15.6801517612301,3.52339371578857));
#30826=CARTESIAN_POINT('Ctrl Pts',(-9.18141647930976,15.2566955850341,10.5701811473657));
#30827=CARTESIAN_POINT('Ctrl Pts',(-7.46076357859445,16.9869629346774,-10.5701811473657));
#30828=CARTESIAN_POINT('Ctrl Pts',(-8.24421702181037,16.6428631545598,-3.52339371578858));
#30829=CARTESIAN_POINT('Ctrl Pts',(-9.00383528249654,16.2444807757546,3.52339371578859));
#30830=CARTESIAN_POINT('Ctrl Pts',(-9.73234227367099,15.7956138465051,10.5701811473657));
#30831=CARTESIAN_POINT('Ctrl Pts',(-8.18028559447402,17.6243975759645,-10.5701811473657));
#30832=CARTESIAN_POINT('Ctrl Pts',(-8.99317441419756,17.2471218084664,-3.52339371578856));
#30833=CARTESIAN_POINT('Ctrl Pts',(-9.77981895378716,16.8135040854808,3.52339371578857));
#30834=CARTESIAN_POINT('Ctrl Pts',(-10.5329043010252,16.3277184354786,10.5701811473657));
#30835=CARTESIAN_POINT('Ctrl Pts',(-8.71988860141417,17.9989872709252,-10.5701811473657));
#30836=CARTESIAN_POINT('Ctrl Pts',(-9.55002197921108,17.5968162782051,-3.52339371578857));
#30837=CARTESIAN_POINT('Ctrl Pts',(-10.3522831255593,17.137126276613,3.52339371578858));
#30838=CARTESIAN_POINT('Ctrl Pts',(-11.1190146190996,16.6243049148002,10.5701811473657));
#30839=CARTESIAN_POINT('Ctrl Pts',(-6.80077064695807,16.0461217833684,-10.5701811473657));
#30840=CARTESIAN_POINT('Ctrl Pts',(-7.54083568928884,15.7324626522293,-3.52339371578857));
#30841=CARTESIAN_POINT('Ctrl Pts',(-8.25916219897089,15.3675249720875,3.52339371578858));
#30842=CARTESIAN_POINT('Ctrl Pts',(-8.94889389387818,14.9547919997346,10.5701811473657));
#30843=CARTESIAN_POINT('Origin',(540.112471297657,-1034.77284228394,-6.00190077359785));
#30844=CARTESIAN_POINT('Origin',(619.61900747461,-989.216155520019,6.00190077285814));
#30845=CARTESIAN_POINT('Ctrl Pts',(-10.2179937997566,17.1928067231421,-10.5701811473657));
#30846=CARTESIAN_POINT('Ctrl Pts',(-11.0109452310822,16.7215414469562,-3.52339371578858));
#30847=CARTESIAN_POINT('Ctrl Pts',(-11.771236988334,16.1953339887957,3.52339371578858));
#30848=CARTESIAN_POINT('Ctrl Pts',(-12.4916122395345,15.6192068930627,10.5701811473657));
#30849=CARTESIAN_POINT('Ctrl Pts',(-10.2026262038394,16.5361084032577,-10.5701811473657));
#30850=CARTESIAN_POINT('Ctrl Pts',(-10.9653007820263,16.0655207639422,-3.52339371578858));
#30851=CARTESIAN_POINT('Ctrl Pts',(-11.6953369617913,15.5421842200282,3.52339371578858));
#30852=CARTESIAN_POINT('Ctrl Pts',(-12.3858181753482,14.9709041379195,10.5701811473657));
#30853=CARTESIAN_POINT('Ctrl Pts',(-10.0670065005512,15.5844556949577,-10.5701811473657));
#30854=CARTESIAN_POINT('Ctrl Pts',(-10.7857775294983,15.1201581991623,-3.52339371578857));
#30855=CARTESIAN_POINT('Ctrl Pts',(-11.4723756631224,14.6060460787463,3.52339371578857));
#30856=CARTESIAN_POINT('Ctrl Pts',(-12.1202404623057,14.0470513036056,10.5701811473657));
#30857=CARTESIAN_POINT('Ctrl Pts',(-9.81776698398909,14.8551880626951,-10.5701811473657));
#30858=CARTESIAN_POINT('Ctrl Pts',(-10.5029081614891,14.402372398422,-3.52339371578859));
#30859=CARTESIAN_POINT('Ctrl Pts',(-11.1566607063151,13.9021132965599,3.52339371578859));
#30860=CARTESIAN_POINT('Ctrl Pts',(-11.7728006532308,13.3591289277869,10.5701811473657));
#30861=CARTESIAN_POINT('Ctrl Pts',(-9.68505839432707,14.5788484285183,-10.5701811473657));
#30862=CARTESIAN_POINT('Ctrl Pts',(-10.3574499392681,14.1321660336653,-3.52339371578856));
#30863=CARTESIAN_POINT('Ctrl Pts',(-10.9988888810637,13.6388849853688,3.52339371578856));
#30864=CARTESIAN_POINT('Ctrl Pts',(-11.6032469575356,13.1037337291963,10.5701811473657));
#30865=CARTESIAN_POINT('Ctrl Pts',(-9.64900602019246,14.5208962185849,-10.5701811473657));
#30866=CARTESIAN_POINT('Ctrl Pts',(-10.3187301172292,14.0758617811302,-3.52339371578859));
#30867=CARTESIAN_POINT('Ctrl Pts',(-10.9576028212762,13.5844589390986,3.52339371578859));
#30868=CARTESIAN_POINT('Ctrl Pts',(-11.5595462325576,13.0513077914049,10.5701811473657));
#30869=CARTESIAN_POINT('Ctrl Pts',(-9.6453770639989,14.5153438461684,-10.5701811473657));
#30870=CARTESIAN_POINT('Ctrl Pts',(-10.3148409196886,14.070488292812,-3.52339371578858));
#30871=CARTESIAN_POINT('Ctrl Pts',(-10.9534758330391,13.5792470767591,3.52339371578858));
#30872=CARTESIAN_POINT('Ctrl Pts',(-11.5551861621905,13.0463089966602,10.5701811473657));
#30873=CARTESIAN_POINT('Origin',(701.455017736501,-932.974787184144,6.000000029911));
#30874=CARTESIAN_POINT('Origin',(626.092649606612,-985.134825974761,-6.00000001913359));
#30875=CARTESIAN_POINT('Ctrl Pts',(-9.02141589925906,17.8497634486454,-8.00000002680495));
#30876=CARTESIAN_POINT('Ctrl Pts',(-9.1771844717434,17.7710367428009,-6.66666668453663));
#30877=CARTESIAN_POINT('Ctrl Pts',(-9.33192245397615,17.6902709152619,-5.33333334226832));
#30878=CARTESIAN_POINT('Ctrl Pts',(-9.48557682353725,17.6074936411964,-4.));
#30879=CARTESIAN_POINT('Ctrl Pts',(-9.52768331452378,17.5938917715508,-8.00000002680495));
#30880=CARTESIAN_POINT('Ctrl Pts',(-9.68121900925411,17.5107470358699,-6.66666668453663));
#30881=CARTESIAN_POINT('Ctrl Pts',(-9.833666207472,17.4255924489156,-5.33333334226832));
#30882=CARTESIAN_POINT('Ctrl Pts',(-9.98497281389112,17.3384571088881,-4.));
#30883=CARTESIAN_POINT('Ctrl Pts',(-10.0230579087404,17.3164686691292,-8.00000002680495));
#30884=CARTESIAN_POINT('Ctrl Pts',(-10.1741726299965,17.2290009742501,-6.66666668453664));
#30885=CARTESIAN_POINT('Ctrl Pts',(-10.3241422646724,17.1395551213611,-5.33333334226831));
#30886=CARTESIAN_POINT('Ctrl Pts',(-10.4729155653442,17.0481616772035,-4.));
#30887=CARTESIAN_POINT('Ctrl Pts',(-10.5057483754947,17.0184973211735,-8.00000002680495));
#30888=CARTESIAN_POINT('Ctrl Pts',(-10.6542627824881,16.9268173707899,-6.66666668453663));
#30889=CARTESIAN_POINT('Ctrl Pts',(-10.8015770320273,16.8331932610413,-5.33333334226832));
#30890=CARTESIAN_POINT('Ctrl Pts',(-10.9476406455038,16.7376570731065,-4.));
#30891=CARTESIAN_POINT('Ctrl Pts',(-10.3940821869213,17.0869264495264,4.));
#30892=CARTESIAN_POINT('Ctrl Pts',(-10.5431937507156,16.9962209704763,5.33333334226731));
#30893=CARTESIAN_POINT('Ctrl Pts',(-10.6911179135796,16.9035635148428,6.66666668453462));
#30894=CARTESIAN_POINT('Ctrl Pts',(-10.8378039879122,16.8089858325717,8.00000002680193));
#30895=CARTESIAN_POINT('Ctrl Pts',(-10.8787134882441,16.7921222557363,4.));
#30896=CARTESIAN_POINT('Ctrl Pts',(-11.0252524228747,16.6971875557313,5.33333334226731));
#30897=CARTESIAN_POINT('Ctrl Pts',(-11.1705485253505,16.6003346026057,6.66666668453462));
#30898=CARTESIAN_POINT('Ctrl Pts',(-11.3145521439962,16.5015964922092,8.00000002680193));
#30899=CARTESIAN_POINT('Ctrl Pts',(-11.3507946421043,16.4766877133626,4.));
#30900=CARTESIAN_POINT('Ctrl Pts',(-11.4945808908437,16.3776333277898,5.33333334226731));
#30901=CARTESIAN_POINT('Ctrl Pts',(-11.6370703784336,16.2766967246661,6.66666668453462));
#30902=CARTESIAN_POINT('Ctrl Pts',(-11.7782144136678,16.1739123973319,8.00000002680193));
#30903=CARTESIAN_POINT('Ctrl Pts',(-11.8086185726672,16.1417634540114,4.));
#30904=CARTESIAN_POINT('Ctrl Pts',(-11.9494820332864,16.0387138162183,5.33333334226731));
#30905=CARTESIAN_POINT('Ctrl Pts',(-12.0889964991502,15.9338201755236,6.66666668453462));
#30906=CARTESIAN_POINT('Ctrl Pts',(-12.2271141643192,15.8271184747163,8.00000002680193));
#30907=CARTESIAN_POINT('Ctrl Pts',(-0.902537120435117,17.4044227834609,
-10.5701811473657));
#30908=CARTESIAN_POINT('Ctrl Pts',(-1.70524852060254,17.3627967643357,-3.52339371578858));
#30909=CARTESIAN_POINT('Ctrl Pts',(-2.5050706787327,17.2655496550558,3.52339371578857));
#30910=CARTESIAN_POINT('Ctrl Pts',(-3.29436945311861,17.1136096597291,10.5701811473657));
#30911=CARTESIAN_POINT('Ctrl Pts',(-0.903127939532374,17.4143548929044,
-10.5701811473657));
#30912=CARTESIAN_POINT('Ctrl Pts',(-1.7063501860739,17.3727370626192,-3.52339371578857));
#30913=CARTESIAN_POINT('Ctrl Pts',(-2.50651861700781,17.2753677032595,3.52339371578856));
#30914=CARTESIAN_POINT('Ctrl Pts',(-3.29632448505991,17.1233653614113,10.5701811473657));
#30915=CARTESIAN_POINT('Ctrl Pts',(-0.916537850406108,17.5552227079068,
-10.5701811473657));
#30916=CARTESIAN_POINT('Ctrl Pts',(-1.72622304155971,17.5129629857501,-3.52339371578858));
#30917=CARTESIAN_POINT('Ctrl Pts',(-2.5329165341938,17.4145668679409,3.52339371578857));
#30918=CARTESIAN_POINT('Ctrl Pts',(-3.32903504964555,17.261037384632,10.5701811473657));
#30919=CARTESIAN_POINT('Ctrl Pts',(-1.0963614992881,18.2632687859986,-10.5701811473657));
#30920=CARTESIAN_POINT('Ctrl Pts',(-1.93870102381158,18.2127147721504,-3.52339371578857));
#30921=CARTESIAN_POINT('Ctrl Pts',(-2.7774786640394,18.1037632822201,3.52339371578856));
#30922=CARTESIAN_POINT('Ctrl Pts',(-3.60479546944582,17.9375150149126,10.5701811473657));
#30923=CARTESIAN_POINT('Ctrl Pts',(-1.53274044321679,19.1804873760836,-10.5701811473657));
#30924=CARTESIAN_POINT('Ctrl Pts',(-2.41748686096405,19.1098799173875,-3.52339371578859));
#30925=CARTESIAN_POINT('Ctrl Pts',(-3.29695624953646,18.9777403313294,3.52339371578858));
#30926=CARTESIAN_POINT('Ctrl Pts',(-4.16350885073652,18.7857814130851,10.5701811473657));
#30927=CARTESIAN_POINT('Ctrl Pts',(-2.03799876670532,19.8958930693474,-10.5701811473657));
#30928=CARTESIAN_POINT('Ctrl Pts',(-2.95561955666072,19.8018982920477,-3.52339371578858));
#30929=CARTESIAN_POINT('Ctrl Pts',(-3.86672167605728,19.6443204619612,3.52339371578857));
#30930=CARTESIAN_POINT('Ctrl Pts',(-4.7626088383289,19.4246636277973,10.5701811473657));
#30931=CARTESIAN_POINT('Ctrl Pts',(-0.902537120435117,17.4044227834609,
-10.5701811473657));
#30932=CARTESIAN_POINT('Ctrl Pts',(-1.70524852060254,17.3627967643357,-3.52339371578858));
#30933=CARTESIAN_POINT('Ctrl Pts',(-2.5050706787327,17.2655496550558,3.52339371578857));
#30934=CARTESIAN_POINT('Ctrl Pts',(-3.29436945311861,17.1136096597291,10.5701811473657));
#30935=CARTESIAN_POINT('Origin',(153.626547848438,-1157.09774893006,-6.0019007738202));
#30936=CARTESIAN_POINT('Origin',(243.9195577298,-1141.48130344627,6.00190077262389));
#30937=CARTESIAN_POINT('Ctrl Pts',(-3.72148715324784,19.6507133122285,-10.5701811473657));
#30938=CARTESIAN_POINT('Ctrl Pts',(-4.62779997921166,19.4790741719562,-3.52339371578858));
#30939=CARTESIAN_POINT('Ctrl Pts',(-5.52221408340464,19.244636002305,3.52339371578858));
#30940=CARTESIAN_POINT('Ctrl Pts',(-6.39619246301094,18.9496364684737,10.5701811473657));
#30941=CARTESIAN_POINT('Ctrl Pts',(-3.93165039025384,19.0283627195925,-10.5701811473657));
#30942=CARTESIAN_POINT('Ctrl Pts',(-4.809280515283,18.847005056037,-3.52339371578858));
#30943=CARTESIAN_POINT('Ctrl Pts',(-5.67428176607203,18.6049166463695,3.52339371578858));
#30944=CARTESIAN_POINT('Ctrl Pts',(-6.5185111628046,18.3042474524344,10.5701811473657));
#30945=CARTESIAN_POINT('Ctrl Pts',(-4.12969891987873,18.0877210849009,-10.5701811473657));
#30946=CARTESIAN_POINT('Ctrl Pts',(-4.96392184787269,17.8972583245915,-3.52339371578858));
#30947=CARTESIAN_POINT('Ctrl Pts',(-5.78495026151908,17.6489806267713,3.52339371578858));
#30948=CARTESIAN_POINT('Ctrl Pts',(-6.58493150569053,17.345280172986,10.5701811473657));
#30949=CARTESIAN_POINT('Ctrl Pts',(-4.14491130701936,17.3171860509472,-10.5701811473657));
#30950=CARTESIAN_POINT('Ctrl Pts',(-4.94360549410748,17.1260105963803,-3.52339371578858));
#30951=CARTESIAN_POINT('Ctrl Pts',(-5.72903079998517,16.8795171054834,3.52339371578858));
#30952=CARTESIAN_POINT('Ctrl Pts',(-6.49372455310468,16.5800109738981,10.5701811473657));
#30953=CARTESIAN_POINT('Ctrl Pts',(-4.11471950693847,17.0121225239124,-10.5701811473657));
#30954=CARTESIAN_POINT('Ctrl Pts',(-4.89933525670704,16.8223498262057,-3.52339371578858));
#30955=CARTESIAN_POINT('Ctrl Pts',(-5.6708029003471,16.5782020953568,3.52339371578858));
#30956=CARTESIAN_POINT('Ctrl Pts',(-6.42174623445712,16.2820270448622,10.5701811473657));
#30957=CARTESIAN_POINT('Ctrl Pts',(-4.10066074919594,16.9453334457781,-10.5701811473657));
#30958=CARTESIAN_POINT('Ctrl Pts',(-4.88220628322697,16.7561970005635,-3.52339371578857));
#30959=CARTESIAN_POINT('Ctrl Pts',(-5.65061991930365,16.5129367098782,3.52339371578857));
#30960=CARTESIAN_POINT('Ctrl Pts',(-6.39861013296397,16.2178152824273,10.5701811473657));
#30961=CARTESIAN_POINT('Ctrl Pts',(-4.09914966904954,16.9388747462736,-10.5701811473657));
#30962=CARTESIAN_POINT('Ctrl Pts',(-4.88038947424221,16.7498173893433,-3.52339371578858));
#30963=CARTESIAN_POINT('Ctrl Pts',(-5.64852438081578,16.5066276481894,3.52339371578858));
#30964=CARTESIAN_POINT('Ctrl Pts',(-6.39622269550912,16.2116267200016,10.5701811473657));
#30965=CARTESIAN_POINT('Origin',(340.055933547788,-1116.62126860195,6.00000003014708));
#30966=CARTESIAN_POINT('Origin',(251.398688376256,-1139.86022419539,-6.00000002075048));
#30967=CARTESIAN_POINT('Ctrl Pts',(-2.37237929653944,19.8587969543311,-8.00000002680495));
#30968=CARTESIAN_POINT('Ctrl Pts',(-2.54567999386982,19.838094039277,-6.66666668453663));
#30969=CARTESIAN_POINT('Ctrl Pts',(-2.71870967383992,19.8151224939882,-5.33333334226832));
#30970=CARTESIAN_POINT('Ctrl Pts',(-2.89140904620798,19.7898901898799,-4.));
#30971=CARTESIAN_POINT('Ctrl Pts',(-2.93562831848091,19.7915098814272,-8.00000002680495));
#30972=CARTESIAN_POINT('Ctrl Pts',(-3.10834185226059,19.765891687168,-6.66666668453663));
#30973=CARTESIAN_POINT('Ctrl Pts',(-3.2807199435204,19.738012562765,-5.33333334226832));
#30974=CARTESIAN_POINT('Ctrl Pts',(-3.45270368653352,19.7078820339451,-4.));
#30975=CARTESIAN_POINT('Ctrl Pts',(-3.49601245844321,19.70024552896,-8.00000002680495));
#30976=CARTESIAN_POINT('Ctrl Pts',(-3.66792956043858,19.6697370601475,-6.66666668453664));
#30977=CARTESIAN_POINT('Ctrl Pts',(-3.83944720291044,19.6369780881742,-5.33333334226832));
#30978=CARTESIAN_POINT('Ctrl Pts',(-4.01050677459149,19.6019798087299,-4.));
#30979=CARTESIAN_POINT('Ctrl Pts',(-4.05150533131066,19.5853339147016,-8.00000002680495));
#30980=CARTESIAN_POINT('Ctrl Pts',(-4.22241961341303,19.549977860618,-6.66666668453663));
#30981=CARTESIAN_POINT('Ctrl Pts',(-4.39287105807657,19.5123844163008,-5.33333334226832));
#30982=CARTESIAN_POINT('Ctrl Pts',(-4.56280125851603,19.4725664634964,-4.));
#30983=CARTESIAN_POINT('Ctrl Pts',(-3.92316929763007,19.6114441758411,4.));
#30984=CARTESIAN_POINT('Ctrl Pts',(-4.09431143474655,19.5772080649333,5.33333334226731));
#30985=CARTESIAN_POINT('Ctrl Pts',(-4.26500539528168,19.5407315809978,6.66666668453462));
#30986=CARTESIAN_POINT('Ctrl Pts',(-4.43519268934985,19.5020272230437,8.00000002680193));
#30987=CARTESIAN_POINT('Ctrl Pts',(-4.47940272789802,19.5001725174983,4.));
#30988=CARTESIAN_POINT('Ctrl Pts',(-4.64957386313053,19.4610823478722,5.33333334226731));
#30989=CARTESIAN_POINT('Ctrl Pts',(-4.81923319936555,19.4197645363123,6.66666668453462));
#30990=CARTESIAN_POINT('Ctrl Pts',(-4.98832275984285,19.3762332008709,8.00000002680193));
#30991=CARTESIAN_POINT('Ctrl Pts',(-5.03089887198512,19.3652222695934,4.));
#30992=CARTESIAN_POINT('Ctrl Pts',(-5.19989234404657,19.3213193878163,5.33333334226731));
#30993=CARTESIAN_POINT('Ctrl Pts',(-5.3683110155416,19.2752042816616,6.66666668453462));
#30994=CARTESIAN_POINT('Ctrl Pts',(-5.53609733428556,19.2268927108936,8.00000002680193));
#30995=CARTESIAN_POINT('Ctrl Pts',(-5.57566348434081,19.207081420908,4.));
#30996=CARTESIAN_POINT('Ctrl Pts',(-5.74327689071064,19.1584245776895,5.33333334226731));
#30997=CARTESIAN_POINT('Ctrl Pts',(-5.91025334280012,19.107573555172,6.66666668453462));
#30998=CARTESIAN_POINT('Ctrl Pts',(-6.07653562456277,19.054545777935,8.00000002680193));
#30999=CARTESIAN_POINT('Ctrl Pts',(5.10455570284159,16.6634935339443,-10.5701811473657));
#31000=CARTESIAN_POINT('Ctrl Pts',(4.33601678645625,16.8989213390741,-3.52339371578858));
#31001=CARTESIAN_POINT('Ctrl Pts',(3.55116933626636,17.0810942372497,3.52339371578858));
#31002=CARTESIAN_POINT('Ctrl Pts',(2.75750456340205,17.2082734247813,10.5701811473657));
#31003=CARTESIAN_POINT('Ctrl Pts',(5.10739749599088,16.6730287359292,-10.5701811473657));
#31004=CARTESIAN_POINT('Ctrl Pts',(4.33838134178569,16.9086389558016,-3.52339371578858));
#31005=CARTESIAN_POINT('Ctrl Pts',(3.55316668960757,17.0908154087533,3.52339371578858));
#31006=CARTESIAN_POINT('Ctrl Pts',(2.75900408080085,17.218109445967,10.5701811473657));
#31007=CARTESIAN_POINT('Ctrl Pts',(5.14297547152441,16.8099873002576,-10.5701811473657));
#31008=CARTESIAN_POINT('Ctrl Pts',(4.36766659600884,17.0472047963176,-3.52339371578858));
#31009=CARTESIAN_POINT('Ctrl Pts',(3.57596927094007,17.2306480542269,3.52339371578858));
#31010=CARTESIAN_POINT('Ctrl Pts',(2.77535240081299,17.3586661004475,10.5701811473657));
#31011=CARTESIAN_POINT('Ctrl Pts',(5.2161622749215,17.536836351783,-10.5701811473657));
#31012=CARTESIAN_POINT('Ctrl Pts',(4.40733153621265,17.7774282041587,-3.52339371578858));
#31013=CARTESIAN_POINT('Ctrl Pts',(3.58187484240095,17.9619260440227,3.52339371578858));
#31014=CARTESIAN_POINT('Ctrl Pts',(2.74759107678742,18.0886627859078,10.5701811473657));
#31015=CARTESIAN_POINT('Ctrl Pts',(5.11980806768289,18.5479914974658,-10.5701811473657));
#31016=CARTESIAN_POINT('Ctrl Pts',(4.26426917104784,18.7842432821225,-3.52339371578857));
#31017=CARTESIAN_POINT('Ctrl Pts',(3.39264383327069,18.9608689271939,3.52339371578857));
#31018=CARTESIAN_POINT('Ctrl Pts',(2.51269688917399,19.0768649830918,10.5701811473657));
#31019=CARTESIAN_POINT('Ctrl Pts',(4.8897033552574,19.3930621535495,-10.5701811473657));
#31020=CARTESIAN_POINT('Ctrl Pts',(3.99527368840464,19.6185807284261,-3.52339371578858));
#31021=CARTESIAN_POINT('Ctrl Pts',(3.08522288423924,19.7821212566387,3.52339371578858));
#31022=CARTESIAN_POINT('Ctrl Pts',(2.16823719579937,19.8821227754131,10.5701811473657));
#31023=CARTESIAN_POINT('Ctrl Pts',(5.10455570284159,16.6634935339443,-10.5701811473657));
#31024=CARTESIAN_POINT('Ctrl Pts',(4.33601678645625,16.8989213390741,-3.52339371578858));
#31025=CARTESIAN_POINT('Ctrl Pts',(3.55116933626636,17.0810942372497,3.52339371578858));
#31026=CARTESIAN_POINT('Ctrl Pts',(2.75750456340205,17.2082734247813,10.5701811473657));
#31027=CARTESIAN_POINT('Origin',(-251.389004561992,-1139.85959012281,-6.00190077378154));
#31028=CARTESIAN_POINT('Origin',(-161.200190539747,-1156.06695970508,6.00190077397284));
#31029=CARTESIAN_POINT('Ctrl Pts',(3.22388576724349,19.7384538622191,-10.5701811473657));
#31030=CARTESIAN_POINT('Ctrl Pts',(2.31352624920544,19.8871430713012,-3.52339371578857));
#31031=CARTESIAN_POINT('Ctrl Pts',(1.39286933918331,19.9727508933579,3.52339371578858));
#31032=CARTESIAN_POINT('Ctrl Pts',(0.470702522298857,19.9944602189378,10.5701811473657));
#31033=CARTESIAN_POINT('Ctrl Pts',(2.81354048537629,19.2255156632199,-10.5701811473657));
#31034=CARTESIAN_POINT('Ctrl Pts',(1.92680995902451,19.3552623862032,-3.52339371578858));
#31035=CARTESIAN_POINT('Ctrl Pts',(1.03117555411552,19.4236215458326,3.52339371578858));
#31036=CARTESIAN_POINT('Ctrl Pts',(0.135024498952097,19.4298283822644,10.5701811473657));
#31037=CARTESIAN_POINT('Ctrl Pts',(2.30571422899442,18.4093435092564,-10.5701811473657));
#31038=CARTESIAN_POINT('Ctrl Pts',(1.45665899888885,18.5156881042572,-3.52339371578857));
#31039=CARTESIAN_POINT('Ctrl Pts',(0.600227987416909,18.5631911577303,3.52339371578857));
#31040=CARTESIAN_POINT('Ctrl Pts',(-0.255380157229852,18.5514157821683,
10.5701811473657));
#31041=CARTESIAN_POINT('Ctrl Pts',(2.02788285372489,17.6904768579854,-10.5701811473657));
#31042=CARTESIAN_POINT('Ctrl Pts',(1.21196996348229,17.7840001943948,-3.52339371578857));
#31043=CARTESIAN_POINT('Ctrl Pts',(0.389605628258776,17.8210031964629,3.52339371578858));
#31044=CARTESIAN_POINT('Ctrl Pts',(-0.431408578760428,17.8011001617743,
10.5701811473657));
#31045=CARTESIAN_POINT('Ctrl Pts',(1.95191613165048,17.393484469299,-10.5701811473657));
#31046=CARTESIAN_POINT('Ctrl Pts',(1.1497124161716,17.4835108568289,-3.52339371578858));
#31047=CARTESIAN_POINT('Ctrl Pts',(0.341266322086565,17.5179443719092,3.52339371578859));
#31048=CARTESIAN_POINT('Ctrl Pts',(-0.465687420824652,17.4964686092602,
10.5701811473657));
#31049=CARTESIAN_POINT('Ctrl Pts',(1.94228472746027,17.3259133729239,-10.5701811473657));
#31050=CARTESIAN_POINT('Ctrl Pts',(1.14318368222273,17.4154875665989,-3.52339371578856));
#31051=CARTESIAN_POINT('Ctrl Pts',(0.337911139204634,17.449710608456,3.52339371578856));
#31052=CARTESIAN_POINT('Ctrl Pts',(-0.465907217907272,17.4282149009269,
10.5701811473657));
#31053=CARTESIAN_POINT('Ctrl Pts',(1.94149567299321,17.3193273608118,-10.5701811473657));
#31054=CARTESIAN_POINT('Ctrl Pts',(1.14270896867536,17.4088713077428,-3.52339371578857));
#31055=CARTESIAN_POINT('Ctrl Pts',(0.337722475075321,17.4430653133694,3.52339371578858));
#31056=CARTESIAN_POINT('Ctrl Pts',(-0.465780373556084,17.4215830027821,
10.5701811473657));
#31057=CARTESIAN_POINT('Origin',(-62.3589149167327,-1165.58674546341,6.00000002996953));
#31058=CARTESIAN_POINT('Origin',(-153.617664909702,-1157.1016568393,-6.00000002073243));
#31059=CARTESIAN_POINT('Ctrl Pts',(4.56280126193231,19.4725664626959,-8.00000002680495));
#31060=CARTESIAN_POINT('Ctrl Pts',(4.39287106149983,19.5123844155302,-6.66666668453663));
#31061=CARTESIAN_POINT('Ctrl Pts',(4.22241961684288,19.5499778598772,-5.33333334226832));
#31062=CARTESIAN_POINT('Ctrl Pts',(4.05150533474672,19.5853339139908,-4.));
#31063=CARTESIAN_POINT('Ctrl Pts',(4.01050677803047,19.6019798080263,-8.00000002680495));
#31064=CARTESIAN_POINT('Ctrl Pts',(3.83944720635556,19.6369780875006,-6.66666668453663));
#31065=CARTESIAN_POINT('Ctrl Pts',(3.66792956388945,19.669737059504,-5.33333334226832));
#31066=CARTESIAN_POINT('Ctrl Pts',(3.49601246189943,19.7002455283466,-4.));
#31067=CARTESIAN_POINT('Ctrl Pts',(3.45270368999108,19.7078820333394,-8.00000002680495));
#31068=CARTESIAN_POINT('Ctrl Pts',(3.28071994698325,19.7380125621894,-6.66666668453664));
#31069=CARTESIAN_POINT('Ctrl Pts',(3.10834185572833,19.7658916866227,-5.33333334226832));
#31070=CARTESIAN_POINT('Ctrl Pts',(2.93562832195315,19.7915098809122,-4.));
#31071=CARTESIAN_POINT('Ctrl Pts',(2.89140904967993,19.7898901893727,-8.00000002680495));
#31072=CARTESIAN_POINT('Ctrl Pts',(2.71870967731629,19.8151224935112,-6.66666668453663));
#31073=CARTESIAN_POINT('Ctrl Pts',(2.54567999735023,19.8380940388304,-5.33333334226832));
#31074=CARTESIAN_POINT('Ctrl Pts',(2.37237930002348,19.8587969539149,-4.));
#31075=CARTESIAN_POINT('Ctrl Pts',(3.02093570876773,19.770532300459,4.));
#31076=CARTESIAN_POINT('Ctrl Pts',(2.84840526585424,19.7968949379402,5.33333334226731));
#31077=CARTESIAN_POINT('Ctrl Pts',(2.67552971846302,19.8209990280008,6.66666668453462));
#31078=CARTESIAN_POINT('Ctrl Pts',(2.50236830402084,19.8428363111485,8.00000002680193));
#31079=CARTESIAN_POINT('Ctrl Pts',(2.46019011037602,19.8562141817544,4.));
#31080=CARTESIAN_POINT('Ctrl Pts',(2.28691192490912,19.8776833938736,5.33333334226731));
#31081=CARTESIAN_POINT('Ctrl Pts',(2.11335277477001,19.8968842617394,6.66666668453462));
#31082=CARTESIAN_POINT('Ctrl Pts',(1.93957196895072,19.9138102227615,8.00000002680193));
#31083=CARTESIAN_POINT('Ctrl Pts',(1.89579755025521,19.9180252198692,4.));
#31084=CARTESIAN_POINT('Ctrl Pts',(1.72197996168025,19.9345691773675,5.33333334226731));
#31085=CARTESIAN_POINT('Ctrl Pts',(1.5479458836573,19.9488377305707,6.66666668453462));
#31086=CARTESIAN_POINT('Ctrl Pts',(1.37375478770642,19.9608260048063,8.00000002680193));
#31087=CARTESIAN_POINT('Ctrl Pts',(1.32979890822623,19.9557419021113,4.));
#31088=CARTESIAN_POINT('Ctrl Pts',(1.15565220662434,19.967346586858,5.33333334226731));
#31089=CARTESIAN_POINT('Ctrl Pts',(0.981353592741155,19.9766715663146,6.66666668453462));
#31090=CARTESIAN_POINT('Ctrl Pts',(0.806962791630517,19.9837136451893,8.00000002680193));
#31091=CARTESIAN_POINT('Ctrl Pts',(10.4959637731368,13.9127010372614,-10.5701811473657));
#31092=CARTESIAN_POINT('Ctrl Pts',(9.85429447627608,14.3967865988031,-3.52339371578857));
#31093=CARTESIAN_POINT('Ctrl Pts',(9.17908591963408,14.8364067643287,3.52339371578858));
#31094=CARTESIAN_POINT('Ctrl Pts',(8.47678283314335,15.2273654477372,10.5701811473657));
#31095=CARTESIAN_POINT('Ctrl Pts',(10.4999182019387,13.9180265095573,-10.5701811473657));
#31096=CARTESIAN_POINT('Ctrl Pts',(9.85799982437194,14.402306194464,-3.52339371578857));
#31097=CARTESIAN_POINT('Ctrl Pts',(9.18254152903524,14.8420688308861,3.52339371578857));
#31098=CARTESIAN_POINT('Ctrl Pts',(8.47996496835067,15.2331854286518,10.5701811473657));
#31099=CARTESIAN_POINT('Ctrl Pts',(10.5393711248066,13.9737196134162,-10.5701811473657));
#31100=CARTESIAN_POINT('Ctrl Pts',(9.89488859896274,14.4598037886812,-3.52339371578858));
#31101=CARTESIAN_POINT('Ctrl Pts',(9.21672460434453,14.9012375244243,3.52339371578858));
#31102=CARTESIAN_POINT('Ctrl Pts',(8.5113595213698,15.2937877139304,10.5701811473657));
#31103=CARTESIAN_POINT('Ctrl Pts',(10.6883641017233,14.2416305529831,-10.5701811473657));
#31104=CARTESIAN_POINT('Ctrl Pts',(10.0315214461228,14.7345992990549,-3.52339371578856));
#31105=CARTESIAN_POINT('Ctrl Pts',(9.34053431369493,15.182023467968,3.52339371578857));
#31106=CARTESIAN_POINT('Ctrl Pts',(8.62197769029742,15.5796876954155,10.5701811473657));
#31107=CARTESIAN_POINT('Ctrl Pts',(10.9807596939229,14.9546925405841,-10.5701811473657));
#31108=CARTESIAN_POINT('Ctrl Pts',(10.2910338072703,15.461133240779,-3.5233937157886));
#31109=CARTESIAN_POINT('Ctrl Pts',(9.56621540573734,15.9197907568147,3.5233937157886));
#31110=CARTESIAN_POINT('Ctrl Pts',(8.81323173181671,16.3262628571385,10.5701811473657));
#31111=CARTESIAN_POINT('Ctrl Pts',(11.1730334267774,15.8965348871784,-10.5701811473657));
#31112=CARTESIAN_POINT('Ctrl Pts',(10.4398585735511,16.4118793808771,-3.52339371578856));
#31113=CARTESIAN_POINT('Ctrl Pts',(9.67101229504786,16.8763246803423,3.52339371578856));
#31114=CARTESIAN_POINT('Ctrl Pts',(8.87376686242201,17.2856229001603,10.5701811473657));
#31115=CARTESIAN_POINT('Ctrl Pts',(11.2276360580494,16.5511403577636,-10.5701811473657));
#31116=CARTESIAN_POINT('Ctrl Pts',(10.464278995546,17.068971461469,-3.52339371578857));
#31117=CARTESIAN_POINT('Ctrl Pts',(9.66504512535763,17.5339049951292,3.52339371578858));
#31118=CARTESIAN_POINT('Ctrl Pts',(8.83756297427067,17.9415032611597,10.5701811473657));
#31119=CARTESIAN_POINT('Ctrl Pts',(10.4959637731368,13.9127010372614,-10.5701811473657));
#31120=CARTESIAN_POINT('Ctrl Pts',(9.85429447627608,14.3967865988031,-3.52339371578857));
#31121=CARTESIAN_POINT('Ctrl Pts',(9.17908591963408,14.8364067643287,3.52339371578858));
#31122=CARTESIAN_POINT('Ctrl Pts',(8.47678283314335,15.2273654477372,10.5701811473657));
#31123=CARTESIAN_POINT('Origin',(-626.083332913132,-985.137542209956,-6.00190077217363));
#31124=CARTESIAN_POINT('Origin',(-546.876816795099,-1031.21387892502,6.00190077273223));
#31125=CARTESIAN_POINT('Ctrl Pts',(9.78041047709324,17.4454455632284,-10.5701811473657));
#31126=CARTESIAN_POINT('Ctrl Pts',(8.97580706054609,17.896529008279,-3.52339371578857));
#31127=CARTESIAN_POINT('Ctrl Pts',(8.13995215573091,18.2918572549299,3.52339371578858));
#31128=CARTESIAN_POINT('Ctrl Pts',(7.28082382967794,18.6276569745418,10.5701811473657));
#31129=CARTESIAN_POINT('Ctrl Pts',(9.21937684849878,17.1037876754904,-10.5701811473657));
#31130=CARTESIAN_POINT('Ctrl Pts',(8.43049870923998,17.5289894151062,-3.52339371578857));
#31131=CARTESIAN_POINT('Ctrl Pts',(7.61225787779935,17.8995510201292,3.52339371578859));
#31132=CARTESIAN_POINT('Ctrl Pts',(6.77227420746117,18.2118852506227,10.5701811473657));
#31133=CARTESIAN_POINT('Ctrl Pts',(8.46303091459466,16.5105131605735,-10.5701811473657));
#31134=CARTESIAN_POINT('Ctrl Pts',(7.70155197397604,16.9008383831229,-3.52339371578856));
#31135=CARTESIAN_POINT('Ctrl Pts',(6.91301848570708,17.2383936792967,3.52339371578858));
#31136=CARTESIAN_POINT('Ctrl Pts',(6.10498241040404,17.5199636659301,10.5701811473657));
#31137=CARTESIAN_POINT('Ctrl Pts',(7.95608662513995,15.9300303069687,-10.5701811473657));
#31138=CARTESIAN_POINT('Ctrl Pts',(7.22136616794635,16.2969721396903,-3.52339371578857));
#31139=CARTESIAN_POINT('Ctrl Pts',(6.46125271502429,16.6130088771473,3.52339371578859));
#31140=CARTESIAN_POINT('Ctrl Pts',(5.68294448440402,16.8751095390476,10.5701811473657));
#31141=CARTESIAN_POINT('Ctrl Pts',(7.78312379454569,15.6769313834283,-10.5701811473657));
#31142=CARTESIAN_POINT('Ctrl Pts',(7.06008972071931,16.035898345205,-3.52339371578856));
#31143=CARTESIAN_POINT('Ctrl Pts',(6.31217625418917,16.3447602197371,3.52339371578858));
#31144=CARTESIAN_POINT('Ctrl Pts',(5.54654263325149,16.6005740388537,10.5701811473657));
#31145=CARTESIAN_POINT('Ctrl Pts',(7.7509620009088,15.6167324440349,-10.5701811473657));
#31146=CARTESIAN_POINT('Ctrl Pts',(7.0306888239964,15.9742133068677,-3.52339371578857));
#31147=CARTESIAN_POINT('Ctrl Pts',(6.2856851272823,16.2817918773406,3.52339371578859));
#31148=CARTESIAN_POINT('Ctrl Pts',(5.52299098368265,16.536514589304,10.5701811473657));
#31149=CARTESIAN_POINT('Ctrl Pts',(7.74796798344852,15.610813489587,-10.5701811473657));
#31150=CARTESIAN_POINT('Ctrl Pts',(7.02797984538244,15.9681584188516,-3.52339371578857));
#31151=CARTESIAN_POINT('Ctrl Pts',(6.28323501621944,16.2756118695303,3.52339371578858));
#31152=CARTESIAN_POINT('Ctrl Pts',(5.52084193563401,16.5302392602455,10.5701811473657));
#31153=CARTESIAN_POINT('Origin',(-457.260143339527,-1073.95971906824,6.00190077300612));
#31154=CARTESIAN_POINT('Origin',(-540.095923847419,-1034.78147929382,-6.00190077463665));
#31155=CARTESIAN_POINT('Ctrl Pts',(10.9476406484403,16.7376570711859,-8.00000002680495));
#31156=CARTESIAN_POINT('Ctrl Pts',(10.8015770349805,16.8331932591463,-6.66666668453663));
#31157=CARTESIAN_POINT('Ctrl Pts',(10.6542627854578,16.9268173689207,-5.33333334226832));
#31158=CARTESIAN_POINT('Ctrl Pts',(10.5057483784805,17.0184973193304,-4.));
#31159=CARTESIAN_POINT('Ctrl Pts',(10.4729155683351,17.0481616753661,-8.00000002680495));
#31160=CARTESIAN_POINT('Ctrl Pts',(10.3241422676794,17.1395551195499,-6.66666668453664));
#31161=CARTESIAN_POINT('Ctrl Pts',(10.1741726330192,17.2290009724651,-5.33333334226832));
#31162=CARTESIAN_POINT('Ctrl Pts',(10.0230579117785,17.3164686673708,-4.));
#31163=CARTESIAN_POINT('Ctrl Pts',(9.98497281693299,17.3384571071364,-8.00000002680495));
#31164=CARTESIAN_POINT('Ctrl Pts',(9.83366621052916,17.4255924471904,-6.66666668453663));
#31165=CARTESIAN_POINT('Ctrl Pts',(9.68121901232621,17.5107470341715,-5.33333334226832));
#31166=CARTESIAN_POINT('Ctrl Pts',(9.52768331761046,17.5938917698793,-4.));
#31167=CARTESIAN_POINT('Ctrl Pts',(9.48557682662632,17.6074936395323,-8.00000002680495));
#31168=CARTESIAN_POINT('Ctrl Pts',(9.33192245707975,17.6902709136248,-6.66666668453663));
#31169=CARTESIAN_POINT('Ctrl Pts',(9.17718447486116,17.7710367411908,-5.33333334226832));
#31170=CARTESIAN_POINT('Ctrl Pts',(9.02141590239063,17.8497634470626,-4.));
#31171=CARTESIAN_POINT('Ctrl Pts',(9.60067128442543,17.5450024476604,4.));
#31172=CARTESIAN_POINT('Ctrl Pts',(9.44756225340845,17.6287841103792,5.33333334226731));
#31173=CARTESIAN_POINT('Ctrl Pts',(9.29335646154787,17.7105614654362,6.66666668453462));
#31174=CARTESIAN_POINT('Ctrl Pts',(9.13810674890371,17.7903064910541,8.00000002680193));
#31175=CARTESIAN_POINT('Ctrl Pts',(9.10304771279964,17.8173033691799,4.));
#31176=CARTESIAN_POINT('Ctrl Pts',(8.94756238357932,17.8967424592111,5.33333334226731));
#31177=CARTESIAN_POINT('Ctrl Pts',(8.79103721450315,17.9741460984632,6.66666668453462));
#31178=CARTESIAN_POINT('Ctrl Pts',(8.63352569325523,18.049487835249,8.00000002680193));
#31179=CARTESIAN_POINT('Ctrl Pts',(8.59383280894276,18.0684203698839,4.));
#31180=CARTESIAN_POINT('Ctrl Pts',(8.43615607031084,18.1434157212207,5.33333334226731));
#31181=CARTESIAN_POINT('Ctrl Pts',(8.27749766403898,18.2163469356839,6.66666668453462));
#31182=CARTESIAN_POINT('Ctrl Pts',(8.11791180783962,18.2871890921223,8.00000002680193));
#31183=CARTESIAN_POINT('Ctrl Pts',(8.0748679267195,18.2974453945363,4.));
#31184=CARTESIAN_POINT('Ctrl Pts',(7.91519259223033,18.3679119110009,5.33333334226731));
#31185=CARTESIAN_POINT('Ctrl Pts',(7.75459480176132,18.436288162287,6.66666668453462));
#31186=CARTESIAN_POINT('Ctrl Pts',(7.59312958565075,18.5025507186311,8.00000002680193));
#31187=CARTESIAN_POINT('Ctrl Pts',(14.6214037084642,9.48383146588571,-10.5701811473657));
#31188=CARTESIAN_POINT('Ctrl Pts',(14.1839988183597,10.1581869207755,-3.52339371578857));
#31189=CARTESIAN_POINT('Ctrl Pts',(13.6998692722136,10.8022296735859,3.52339371578858));
#31190=CARTESIAN_POINT('Ctrl Pts',(13.1736359892169,11.4098124657167,10.5701811473657));
#31191=CARTESIAN_POINT('Ctrl Pts',(14.6297097580075,9.48930918495536,-10.5701811473657));
#31192=CARTESIAN_POINT('Ctrl Pts',(14.1920565364594,10.1641111402026,-3.52339371578859));
#31193=CARTESIAN_POINT('Ctrl Pts',(13.7076479822366,10.8083926490179,3.5233937157886));
#31194=CARTESIAN_POINT('Ctrl Pts',(13.1811071587353,11.4163834238849,10.5701811473657));
#31195=CARTESIAN_POINT('Ctrl Pts',(14.7449772223308,9.57135777968399,-10.5701811473657));
#31196=CARTESIAN_POINT('Ctrl Pts',(14.3035366338095,10.2514358632128,-3.52339371578855));
#31197=CARTESIAN_POINT('Ctrl Pts',(13.8149763785592,10.9008517199749,3.52339371578857));
#31198=CARTESIAN_POINT('Ctrl Pts',(13.2839566880579,11.5135458371248,10.5701811473657));
#31199=CARTESIAN_POINT('Ctrl Pts',(15.2682377029358,10.0811139468336,-10.5701811473657));
#31200=CARTESIAN_POINT('Ctrl Pts',(14.8032868804182,10.7853243667585,-3.52339371578858));
#31201=CARTESIAN_POINT('Ctrl Pts',(14.2895432842685,11.4572463383409,3.52339371578859));
#31202=CARTESIAN_POINT('Ctrl Pts',(13.7319096587419,12.090599575147,10.5701811473657));
#31203=CARTESIAN_POINT('Ctrl Pts',(15.8444191030467,10.9176358492752,-10.5701811473657));
#31204=CARTESIAN_POINT('Ctrl Pts',(15.3408980412456,11.6485449936036,-3.52339371578856));
#31205=CARTESIAN_POINT('Ctrl Pts',(14.7867271085875,12.344118032929,3.52339371578858));
#31206=CARTESIAN_POINT('Ctrl Pts',(14.1872095083049,12.9985951401616,10.5701811473657));
#31207=CARTESIAN_POINT('Ctrl Pts',(16.211349445681,11.7129052395219,-10.5701811473657));
#31208=CARTESIAN_POINT('Ctrl Pts',(15.6711371857387,12.4605907660142,-3.52339371578857));
#31209=CARTESIAN_POINT('Ctrl Pts',(15.0791197221122,13.1708394318101,3.52339371578858));
#31210=CARTESIAN_POINT('Ctrl Pts',(14.4409477424756,13.8368720561798,10.5701811473657));
#31211=CARTESIAN_POINT('Ctrl Pts',(14.6214037084642,9.48383146588571,-10.5701811473657));
#31212=CARTESIAN_POINT('Ctrl Pts',(14.1839988183597,10.1581869207755,-3.52339371578857));
#31213=CARTESIAN_POINT('Ctrl Pts',(13.6998692722136,10.8022296735859,3.52339371578858));
#31214=CARTESIAN_POINT('Ctrl Pts',(13.1736359892169,11.4098124657167,10.5701811473657));
#31215=CARTESIAN_POINT('Origin',(-925.262771311062,-711.593367601486,-6.00190077290402));
#31216=CARTESIAN_POINT('Origin',(-866.592027872364,-781.981185220022,6.00190077473778));
#31217=CARTESIAN_POINT('Ctrl Pts',(15.1572733542511,13.0482590706843,-10.5701811473657));
#31218=CARTESIAN_POINT('Ctrl Pts',(14.5554730855096,13.7473294316085,-3.52339371578856));
#31219=CARTESIAN_POINT('Ctrl Pts',(13.9052366228784,14.4046956825171,3.52339371578859));
#31220=CARTESIAN_POINT('Ctrl Pts',(13.2127703426728,15.0140833946989,10.5701811473657));
#31221=CARTESIAN_POINT('Ctrl Pts',(14.5132203124649,12.9190904765551,-10.5701811473657));
#31222=CARTESIAN_POINT('Ctrl Pts',(13.9173449061403,13.5884616281791,-3.52339371578857));
#31223=CARTESIAN_POINT('Ctrl Pts',(13.275189568012,14.216530480834,3.5233937157886));
#31224=CARTESIAN_POINT('Ctrl Pts',(12.5926877095625,14.7973199880585,10.5701811473657));
#31225=CARTESIAN_POINT('Ctrl Pts',(13.5995754203915,12.6202781311691,-10.5701811473657));
#31226=CARTESIAN_POINT('Ctrl Pts',(13.0175183674916,13.2475049990765,-3.52339371578855));
#31227=CARTESIAN_POINT('Ctrl Pts',(12.3919902857833,13.8343975281826,3.52339371578858));
#31228=CARTESIAN_POINT('Ctrl Pts',(11.7289873555787,14.3753513812935,10.5701811473657));
#31229=CARTESIAN_POINT('Ctrl Pts',(12.9246670167664,12.2481892936844,-10.5701811473657));
#31230=CARTESIAN_POINT('Ctrl Pts',(12.3597571229874,12.8442910222742,-3.52339371578857));
#31231=CARTESIAN_POINT('Ctrl Pts',(11.7535751548201,13.4012425144143,3.5233937157886));
#31232=CARTESIAN_POINT('Ctrl Pts',(11.1118483597182,13.9137336649384,10.5701811473657));
#31233=CARTESIAN_POINT('Ctrl Pts',(12.6755702095651,12.069510984472,-10.5701811473657));
#31234=CARTESIAN_POINT('Ctrl Pts',(12.1189143575221,12.6541218071276,-3.52339371578855));
#31235=CARTESIAN_POINT('Ctrl Pts',(11.5217426635648,13.2001584940098,3.52339371578858));
#31236=CARTESIAN_POINT('Ctrl Pts',(10.8897758788143,13.7024069729043,10.5701811473657));
#31237=CARTESIAN_POINT('Ctrl Pts',(12.624758865043,12.0239431039938,-10.5701811473657));
#31238=CARTESIAN_POINT('Ctrl Pts',(12.0701891316902,12.6062131680716,-3.52339371578857));
#31239=CARTESIAN_POINT('Ctrl Pts',(11.4753127221865,13.1500487521856,3.52339371578859));
#31240=CARTESIAN_POINT('Ctrl Pts',(10.8457349619827,13.6502665652722,10.5701811473657));
#31241=CARTESIAN_POINT('Ctrl Pts',(12.6199210072709,12.0194051204483,-10.5701811473657));
#31242=CARTESIAN_POINT('Ctrl Pts',(12.0655726308006,12.6014499597276,-3.52339371578856));
#31243=CARTESIAN_POINT('Ctrl Pts',(11.4708966837348,13.145079431777,3.52339371578859));
#31244=CARTESIAN_POINT('Ctrl Pts',(10.8415692284374,13.6451047025743,10.5701811473657));
#31245=CARTESIAN_POINT('Origin',(-796.994418233151,-852.807711458368,6.00000003080237));
#31246=CARTESIAN_POINT('Origin',(-861.44856672619,-787.647762729537,-6.00000001934937));
#31247=CARTESIAN_POINT('Ctrl Pts',(16.0120330027781,11.983939215381,-8.00000002680495));
#31248=CARTESIAN_POINT('Ctrl Pts',(15.9074534037436,12.1236705642356,-6.66666668453663));
#31249=CARTESIAN_POINT('Ctrl Pts',(15.8010446219743,12.262032890054,-5.33333334226832));
#31250=CARTESIAN_POINT('Ctrl Pts',(15.6928431194365,12.3989787816882,-4.));
#31251=CARTESIAN_POINT('Ctrl Pts',(15.6721361773263,12.4380836405871,-8.00000002680495));
#31252=CARTESIAN_POINT('Ctrl Pts',(15.5635934034088,12.574848851288,-6.66666668453663));
#31253=CARTESIAN_POINT('Ctrl Pts',(15.4532603278107,12.7101930951734,-5.33333334226832));
#31254=CARTESIAN_POINT('Ctrl Pts',(15.3411746529166,12.8440701212508,-4.));
#31255=CARTESIAN_POINT('Ctrl Pts',(15.3129068596486,12.8777583654387,-8.00000002680495));
#31256=CARTESIAN_POINT('Ctrl Pts',(15.2005271996287,13.0113887087055,-6.66666668453663));
#31257=CARTESIAN_POINT('Ctrl Pts',(15.086398276462,13.1435478582967,-5.33333334226832));
#31258=CARTESIAN_POINT('Ctrl Pts',(14.970559091534,13.2741906532108,-4.));
#31259=CARTESIAN_POINT('Ctrl Pts',(14.9356440460772,13.3013734978339,-8.00000002680495));
#31260=CARTESIAN_POINT('Ctrl Pts',(14.819567664012,13.4317115809623,-6.66666668453663));
#31261=CARTESIAN_POINT('Ctrl Pts',(14.7017850638858,13.5605301399942,-5.33333334226832));
#31262=CARTESIAN_POINT('Ctrl Pts',(14.5823366050108,13.6877850340427,-4.));
#31263=CARTESIAN_POINT('Ctrl Pts',(15.0224242123638,13.2032863630154,4.));
#31264=CARTESIAN_POINT('Ctrl Pts',(14.9072038020326,13.3343817459623,5.33333334226731));
#31265=CARTESIAN_POINT('Ctrl Pts',(14.7902672600361,13.4639688100905,6.66666668453462));
#31266=CARTESIAN_POINT('Ctrl Pts',(14.6716546557766,13.5920031511778,8.00000002680193));
#31267=CARTESIAN_POINT('Ctrl Pts',(14.6479434143837,13.6293628148902,4.));
#31268=CARTESIAN_POINT('Ctrl Pts',(14.529004766833,13.7571902561793,5.33333334226731));
#31269=CARTESIAN_POINT('Ctrl Pts',(14.4083928242758,13.8834606455681,6.66666668453462));
#31270=CARTESIAN_POINT('Ctrl Pts',(14.2861488016842,14.0081308327355,8.00000002680193));
#31271=CARTESIAN_POINT('Ctrl Pts',(14.2553249994075,14.0394973618063,4.));
#31272=CARTESIAN_POINT('Ctrl Pts',(14.1328072524584,14.1638985607967,5.33333334226731));
#31273=CARTESIAN_POINT('Ctrl Pts',(14.0086610632827,14.2866958557057,6.66666668453462));
#31274=CARTESIAN_POINT('Ctrl Pts',(13.882928856329,14.4078472847614,8.00000002680193));
#31275=CARTESIAN_POINT('Ctrl Pts',(13.845988700892,14.4322069308464,4.));
#31276=CARTESIAN_POINT('Ctrl Pts',(13.7200439354119,14.5530359771683,5.33333334226731));
#31277=CARTESIAN_POINT('Ctrl Pts',(13.5925174320586,14.6722163152528,6.66666668453462));
#31278=CARTESIAN_POINT('Ctrl Pts',(13.4634528889838,14.78970710684,8.00000002680193));
#31279=CARTESIAN_POINT('Ctrl Pts',(16.9832865676143,3.91107185327861,-10.5701811473657));
#31280=CARTESIAN_POINT('Ctrl Pts',(16.8029035694212,4.69435998123015,-3.52339371578857));
#31281=CARTESIAN_POINT('Ctrl Pts',(16.5682462020274,5.46514426027785,3.52339371578857));
#31282=CARTESIAN_POINT('Ctrl Pts',(16.2815542228302,6.21606770943294,10.5701811473657));
#31283=CARTESIAN_POINT('Ctrl Pts',(16.9897389834306,3.91260954390058,-10.5701811473657));
#31284=CARTESIAN_POINT('Ctrl Pts',(16.8092899584406,4.69620648496871,-3.52339371578858));
#31285=CARTESIAN_POINT('Ctrl Pts',(16.5745328586345,5.46726043199356,3.52339371578858));
#31286=CARTESIAN_POINT('Ctrl Pts',(16.287732891443,6.21848063638781,10.5701811473657));
#31287=CARTESIAN_POINT('Ctrl Pts',(17.0557613661601,3.92991270646709,-10.5701811473657));
#31288=CARTESIAN_POINT('Ctrl Pts',(16.8745079936752,4.71654017008886,-3.52339371578856));
#31289=CARTESIAN_POINT('Ctrl Pts',(16.6387524141881,5.49061356475807,3.52339371578857));
#31290=CARTESIAN_POINT('Ctrl Pts',(16.3507378099998,6.24472439171618,10.5701811473657));
#31291=CARTESIAN_POINT('Ctrl Pts',(17.3421065865863,4.03937349046947,-10.5701811473657));
#31292=CARTESIAN_POINT('Ctrl Pts',(17.1558101221977,4.83921977956265,-3.52339371578857));
#31293=CARTESIAN_POINT('Ctrl Pts',(16.9140820327625,5.62612468710593,3.52339371578857));
#31294=CARTESIAN_POINT('Ctrl Pts',(16.6192493625613,6.39263245314738,10.5701811473657));
#31295=CARTESIAN_POINT('Ctrl Pts',(18.0244436775359,4.39766136660597,-10.5701811473657));
#31296=CARTESIAN_POINT('Ctrl Pts',(17.8216168089676,5.22896469136215,-3.52339371578856));
#31297=CARTESIAN_POINT('Ctrl Pts',(17.5611932309209,6.04622142745388,3.52339371578857));
#31298=CARTESIAN_POINT('Ctrl Pts',(17.2456495103603,6.84160568476519,10.5701811473657));
#31299=CARTESIAN_POINT('Ctrl Pts',(18.7771350612562,4.99556415374892,-10.5701811473657));
#31300=CARTESIAN_POINT('Ctrl Pts',(18.5467476225913,5.86161661525353,-3.52339371578857));
#31301=CARTESIAN_POINT('Ctrl Pts',(18.2563169179228,6.7116071841068,3.52339371578858));
#31302=CARTESIAN_POINT('Ctrl Pts',(17.9086833416741,7.53760726560638,10.5701811473657));
#31303=CARTESIAN_POINT('Ctrl Pts',(19.2397349758694,5.46192256062902,-10.5701811473657));
#31304=CARTESIAN_POINT('Ctrl Pts',(18.9878250124769,6.34928060711398,-3.52339371578857));
#31305=CARTESIAN_POINT('Ctrl Pts',(18.6744299210032,7.21917793504633,3.52339371578857));
#31306=CARTESIAN_POINT('Ctrl Pts',(18.3025409945928,8.06331154931088,10.5701811473657));
#31307=CARTESIAN_POINT('Ctrl Pts',(16.9832865676143,3.91107185327861,-10.5701811473657));
#31308=CARTESIAN_POINT('Ctrl Pts',(16.8029035694212,4.69435998123015,-3.52339371578857));
#31309=CARTESIAN_POINT('Ctrl Pts',(16.5682462020274,5.46514426027785,3.52339371578857));
#31310=CARTESIAN_POINT('Ctrl Pts',(16.2815542228302,6.21606770943294,10.5701811473657));
#31311=CARTESIAN_POINT('Origin',(-1112.8418640586,-352.220530871087,-6.00190077429466));
#31312=CARTESIAN_POINT('Origin',(-1081.78345086687,-438.4300197552,6.00190077312313));
#31313=CARTESIAN_POINT('Ctrl Pts',(18.7059453597305,7.07725995777758,-10.5701811473657));
#31314=CARTESIAN_POINT('Ctrl Pts',(18.3795342330452,7.93999903151655,-3.52339371578857));
#31315=CARTESIAN_POINT('Ctrl Pts',(17.9933443266979,8.78011521479376,3.52339371578857));
#31316=CARTESIAN_POINT('Ctrl Pts',(17.5510617457069,9.58958976753269,10.5701811473657));
#31317=CARTESIAN_POINT('Ctrl Pts',(18.0565552078921,7.17616029669805,-10.5701811473657));
#31318=CARTESIAN_POINT('Ctrl Pts',(17.7255539028776,8.0089648203215,-3.52339371578857));
#31319=CARTESIAN_POINT('Ctrl Pts',(17.3369374692435,8.81878654729075,3.52339371578857));
#31320=CARTESIAN_POINT('Ctrl Pts',(16.8942372196888,9.59797954490639,10.5701811473657));
#31321=CARTESIAN_POINT('Ctrl Pts',(17.0958111919983,7.20785561730521,-10.5701811473657));
#31322=CARTESIAN_POINT('Ctrl Pts',(16.7633806977713,7.99633131329305,-3.52339371578856));
#31323=CARTESIAN_POINT('Ctrl Pts',(16.3763053385156,8.76177323989849,3.52339371578857));
#31324=CARTESIAN_POINT('Ctrl Pts',(15.9383034918164,9.49686394106645,10.5701811473657));
#31325=CARTESIAN_POINT('Ctrl Pts',(16.3343420851163,7.08903734850001,-10.5701811473657));
#31326=CARTESIAN_POINT('Ctrl Pts',(16.0073792251723,7.84240030692999,-3.52339371578856));
#31327=CARTESIAN_POINT('Ctrl Pts',(15.6282430292671,8.57309000696066,3.52339371578857));
#31328=CARTESIAN_POINT('Ctrl Pts',(15.2004993921047,9.27415764976289,10.5701811473657));
#31329=CARTESIAN_POINT('Ctrl Pts',(16.039156011872,7.00633068060153,-10.5701811473657));
#31330=CARTESIAN_POINT('Ctrl Pts',(15.7160192927444,7.7460726709814,-3.52339371578857));
#31331=CARTESIAN_POINT('Ctrl Pts',(15.3416169168207,8.46342410640404,3.52339371578857));
#31332=CARTESIAN_POINT('Ctrl Pts',(14.9195414893454,9.15152866611962,10.5701811473657));
#31333=CARTESIAN_POINT('Ctrl Pts',(15.9758234884508,6.98088877109892,-10.5701811473657));
#31334=CARTESIAN_POINT('Ctrl Pts',(15.6538464930781,7.71771767330283,-3.52339371578856));
#31335=CARTESIAN_POINT('Ctrl Pts',(15.2808482452121,8.43221567345516,3.52339371578857));
#31336=CARTESIAN_POINT('Ctrl Pts',(14.8603232378636,9.11759493697779,10.5701811473657));
#31337=CARTESIAN_POINT('Ctrl Pts',(15.9697253074185,6.97827910625622,-10.5701811473657));
#31338=CARTESIAN_POINT('Ctrl Pts',(15.647879288057,7.71482065786624,-3.52339371578857));
#31339=CARTESIAN_POINT('Ctrl Pts',(15.2749989187868,8.42905641384053,3.52339371578857));
#31340=CARTESIAN_POINT('Ctrl Pts',(14.8546432677704,9.11416913747482,10.5701811473657));
#31341=CARTESIAN_POINT('Origin',(-1040.60718933536,-528.788968262105,6.00000003130594));
#31342=CARTESIAN_POINT('Origin',(-1078.88826202927,-445.514028128251,-6.00000002213574));
#31343=CARTESIAN_POINT('Ctrl Pts',(19.1451378645417,5.78478142609488,-8.00000002680495));
#31344=CARTESIAN_POINT('Ctrl Pts',(19.0946561230066,5.95185427295671,-6.66666668453663));
#31345=CARTESIAN_POINT('Ctrl Pts',(19.0419872784984,6.11826627631489,-5.33333334226832));
#31346=CARTESIAN_POINT('Ctrl Pts',(18.9871493784903,6.28396041353657,-4.));
#31347=CARTESIAN_POINT('Ctrl Pts',(18.9810658672356,6.32778915218908,-8.00000002680495));
#31348=CARTESIAN_POINT('Ctrl Pts',(18.9258454805117,6.4934302265572,-6.66666668453664));
#31349=CARTESIAN_POINT('Ctrl Pts',(18.8684567612354,6.65834834813178,-5.33333334226832));
#31350=CARTESIAN_POINT('Ctrl Pts',(18.8089193192887,6.82248716022144,-4.));
#31351=CARTESIAN_POINT('Ctrl Pts',(18.7938783406543,6.86381190939714,-8.00000002680495));
#31352=CARTESIAN_POINT('Ctrl Pts',(18.733980272564,7.02781946430488,-6.66666668453663));
#31353=CARTESIAN_POINT('Ctrl Pts',(18.671935256931,7.19104283260414,-5.33333334226832));
#31354=CARTESIAN_POINT('Ctrl Pts',(18.6077644970973,7.35342623757559,-4.));
#31355=CARTESIAN_POINT('Ctrl Pts',(18.5842521669411,7.3909114049313,-8.00000002680495));
#31356=CARTESIAN_POINT('Ctrl Pts',(18.5197542971393,7.5530896006851,-6.66666668453663));
#31357=CARTESIAN_POINT('Ctrl Pts',(18.4531333989669,7.714423471804,-5.33333334226832));
#31358=CARTESIAN_POINT('Ctrl Pts',(18.3844123006991,7.87485773572478,-4.));
#31359=CARTESIAN_POINT('Ctrl Pts',(18.6322510729221,7.2690590832371,4.));
#31360=CARTESIAN_POINT('Ctrl Pts',(18.5688165652349,7.43165614846694,5.33333334226731));
#31361=CARTESIAN_POINT('Ctrl Pts',(18.5032535458669,7.5934228092312,6.66666668453462));
#31362=CARTESIAN_POINT('Ctrl Pts',(18.4355844806013,7.75430363466721,8.00000002680193));
#31363=CARTESIAN_POINT('Ctrl Pts',(18.4260809595722,7.79751995715235,4.));
#31364=CARTESIAN_POINT('Ctrl Pts',(18.3580347499332,7.95831787374795,5.33333334226731));
#31365=CARTESIAN_POINT('Ctrl Pts',(18.2878836142101,8.11822494076053,6.66666668453462));
#31366=CARTESIAN_POINT('Ctrl Pts',(18.215651523529,8.2771865138012,8.00000002680193));
#31367=CARTESIAN_POINT('Ctrl Pts',(18.1974146087534,8.31720377098127,4.));
#31368=CARTESIAN_POINT('Ctrl Pts',(18.1248333019387,8.47600619706092,5.33333334226731));
#31369=CARTESIAN_POINT('Ctrl Pts',(18.0501731924764,8.63385840635456,6.66666668453462));
#31370=CARTESIAN_POINT('Ctrl Pts',(17.9734597945365,8.7907064576789,8.00000002680193));
#31371=CARTESIAN_POINT('Ctrl Pts',(17.9470788927071,8.82623131460692,4.));
#31372=CARTESIAN_POINT('Ctrl Pts',(17.8700554936997,8.9828491245528,5.33333334226731));
#31373=CARTESIAN_POINT('Ctrl Pts',(17.7909818558573,9.13845864174832,6.66666668453462));
#31374=CARTESIAN_POINT('Ctrl Pts',(17.7098850745029,9.2930065451338,8.00000002680193));
#31375=CARTESIAN_POINT('Ctrl Pts',(17.2967344200949,-2.13342074610697,-10.5701811473657));
#31376=CARTESIAN_POINT('Ctrl Pts',(17.3951301655649,-1.33567605342618,-3.52339371578857));
#31377=CARTESIAN_POINT('Ctrl Pts',(17.438248118605,-0.531118207758813,3.52339371578858));
#31378=CARTESIAN_POINT('Ctrl Pts',(17.4256767270215,0.272573448002655,10.5701811473657));
#31379=CARTESIAN_POINT('Ctrl Pts',(17.3066182331392,-2.13456359558476,-10.5701811473657));
#31380=CARTESIAN_POINT('Ctrl Pts',(17.4051107505843,-1.33631723941131,-3.52339371578858));
#31381=CARTESIAN_POINT('Ctrl Pts',(17.4481684404393,-0.531397153098441,
3.52339371578859));
#31382=CARTESIAN_POINT('Ctrl Pts',(17.4356237054091,0.272804718796849,10.5701811473657));
#31383=CARTESIAN_POINT('Ctrl Pts',(17.4476874812992,-2.14583108338521,-10.5701811473657));
#31384=CARTESIAN_POINT('Ctrl Pts',(17.5466701372069,-1.34110850589676,-3.52339371578856));
#31385=CARTESIAN_POINT('Ctrl Pts',(17.5898512960804,-0.529582293917894,
3.52339371578857));
#31386=CARTESIAN_POINT('Ctrl Pts',(17.5768988000169,0.281101507410299,10.5701811473657));
#31387=CARTESIAN_POINT('Ctrl Pts',(18.176210560974,-2.09169814335911,-10.5701811473657));
#31388=CARTESIAN_POINT('Ctrl Pts',(18.2726952996008,-1.25337703656127,-3.52339371578858));
#31389=CARTESIAN_POINT('Ctrl Pts',(18.3110538115191,-0.408420040147124,
3.52339371578859));
#31390=CARTESIAN_POINT('Ctrl Pts',(18.290993284562,0.435196672672641,10.5701811473657));
#31391=CARTESIAN_POINT('Ctrl Pts',(19.1552502593208,-1.82120200778524,-10.5701811473657));
#31392=CARTESIAN_POINT('Ctrl Pts',(19.2393500897156,-0.937636019605692,
-3.52339371578856));
#31393=CARTESIAN_POINT('Ctrl Pts',(19.2619362575252,-0.0485819488860309,
3.52339371578857));
#31394=CARTESIAN_POINT('Ctrl Pts',(19.2233689066293,0.838139087508731,10.5701811473657));
#31395=CARTESIAN_POINT('Ctrl Pts',(19.947524519721,-1.44784858846757,-10.5701811473657));
#31396=CARTESIAN_POINT('Ctrl Pts',(20.0143009122587,-0.527846498406002,
-3.52339371578857));
#31397=CARTESIAN_POINT('Ctrl Pts',(20.0173282661883,0.396777035596821,3.52339371578858));
#31398=CARTESIAN_POINT('Ctrl Pts',(19.9565776860253,1.31719666779067,10.5701811473657));
#31399=CARTESIAN_POINT('Ctrl Pts',(17.2967344200949,-2.13342074610697,-10.5701811473657));
#31400=CARTESIAN_POINT('Ctrl Pts',(17.3951301655649,-1.33567605342618,-3.52339371578857));
#31401=CARTESIAN_POINT('Ctrl Pts',(17.438248118605,-0.531118207758813,3.52339371578858));
#31402=CARTESIAN_POINT('Ctrl Pts',(17.4256767270215,0.272573448002655,10.5701811473657));
#31403=CARTESIAN_POINT('Origin',(-1166.1958042159,49.6353000922384,-6.00190077381557));
#31404=CARTESIAN_POINT('Origin',(-1166.49582424371,-41.9977233820896,6.00190077373936));
#31405=CARTESIAN_POINT('Ctrl Pts',(19.9984057517891,0.252638042748192,-10.5701811473657));
#31406=CARTESIAN_POINT('Ctrl Pts',(19.9867538035289,1.17498683179843,-3.52339371578858));
#31407=CARTESIAN_POINT('Ctrl Pts',(19.911190687624,2.09652260757975,3.52339371578857));
#31408=CARTESIAN_POINT('Ctrl Pts',(19.7724376400266,3.00844949518813,10.5701811473657));
#31409=CARTESIAN_POINT('Ctrl Pts',(19.2298702051233,0.672692451092664,-10.5701811473657));
#31410=CARTESIAN_POINT('Ctrl Pts',(19.1987473490918,1.55970602327824,-3.52339371578858));
#31411=CARTESIAN_POINT('Ctrl Pts',(19.1064764398699,2.44424738876731,3.52339371578858));
#31412=CARTESIAN_POINT('Ctrl Pts',(18.9533120809235,3.31849128411775,10.5701811473657));
#31413=CARTESIAN_POINT('Ctrl Pts',(18.2687424654252,1.00123000436807,-10.5701811473657));
#31414=CARTESIAN_POINT('Ctrl Pts',(18.2225517496899,1.84382007141717,-3.52339371578857));
#31415=CARTESIAN_POINT('Ctrl Pts',(18.1180183606275,2.68316133395875,3.52339371578856));
#31416=CARTESIAN_POINT('Ctrl Pts',(17.9560571362275,3.51132808353326,10.5701811473657));
#31417=CARTESIAN_POINT('Ctrl Pts',(17.5447630935932,1.09882677893604,-10.5701811473657));
#31418=CARTESIAN_POINT('Ctrl Pts',(17.4940701434606,1.90802775378534,-3.52339371578858));
#31419=CARTESIAN_POINT('Ctrl Pts',(17.3873513571379,2.71366344201221,3.52339371578858));
#31420=CARTESIAN_POINT('Ctrl Pts',(17.225536025983,3.50813923868159,10.5701811473657));
#31421=CARTESIAN_POINT('Ctrl Pts',(17.4032795079184,1.09601951648447,-10.5701811473657));
#31422=CARTESIAN_POINT('Ctrl Pts',(17.3526886200656,1.89872655096413,-3.52339371578857));
#31423=CARTESIAN_POINT('Ctrl Pts',(17.2466103605934,2.69778706986935,3.52339371578856));
#31424=CARTESIAN_POINT('Ctrl Pts',(17.0857917754359,3.48584506507326,10.5701811473657));
#31425=CARTESIAN_POINT('Ctrl Pts',(17.3933450474474,1.09546964341861,-10.5701811473657));
#31426=CARTESIAN_POINT('Ctrl Pts',(17.342820765071,1.89767012603957,-3.52339371578858));
#31427=CARTESIAN_POINT('Ctrl Pts',(17.2367108492585,2.6963647927712,3.52339371578857));
#31428=CARTESIAN_POINT('Ctrl Pts',(17.0760280978245,3.48393026358523,10.5701811473657));
#31429=CARTESIAN_POINT('Origin',(-1158.70647098178,-140.980959266364,6.00190077354629));
#31430=CARTESIAN_POINT('Origin',(-1166.19501035542,-49.6539491257549,-6.00190077350844));
#31431=CARTESIAN_POINT('Ctrl Pts',(19.9690565476993,-1.11210637745949,-8.00000002680495));
#31432=CARTESIAN_POINT('Ctrl Pts',(19.9787615067239,-0.937843483654575,
-6.66666668453663));
#31433=CARTESIAN_POINT('Ctrl Pts',(19.9861852394339,-0.7634535463412,-5.33333334226832));
#31434=CARTESIAN_POINT('Ctrl Pts',(19.9913252020177,-0.588996321866056,
-4.));
#31435=CARTESIAN_POINT('Ctrl Pts',(20.0005988828589,-0.545730096184683,
-8.00000002680495));
#31436=CARTESIAN_POINT('Ctrl Pts',(20.0053612769335,-0.371191916320091,
-6.66666668453663));
#31437=CARTESIAN_POINT('Ctrl Pts',(20.0078388404912,-0.19659147645045,-5.33333334226832));
#31438=CARTESIAN_POINT('Ctrl Pts',(20.0080307256696,-0.0219884415173625,
-4.));
#31439=CARTESIAN_POINT('Ctrl Pts',(20.0080307256734,0.0219884380071485,
-8.00000002680495));
#31440=CARTESIAN_POINT('Ctrl Pts',(20.0078388405257,0.19659147294027,-6.66666668453663));
#31441=CARTESIAN_POINT('Ctrl Pts',(20.0053612769986,0.371191912810345,-5.33333334226832));
#31442=CARTESIAN_POINT('Ctrl Pts',(20.0005988829546,0.545730092675773,-4.));
#31443=CARTESIAN_POINT('Ctrl Pts',(19.991325202121,0.588996318358773,-8.00000002680495));
#31444=CARTESIAN_POINT('Ctrl Pts',(19.9861852395679,0.763453542834819,-6.66666668453663));
#31445=CARTESIAN_POINT('Ctrl Pts',(19.9787615068885,0.937843480149496,-5.33333334226832));
#31446=CARTESIAN_POINT('Ctrl Pts',(19.9690565478945,1.11210637395612,-4.));
#31447=CARTESIAN_POINT('Ctrl Pts',(19.9947534713468,0.458075998134004,4.));
#31448=CARTESIAN_POINT('Ctrl Pts',(19.9907560041241,0.632563139902936,5.33333334226731));
#31449=CARTESIAN_POINT('Ctrl Pts',(19.9844743751274,0.806997950593389,6.66666668453462));
#31450=CARTESIAN_POINT('Ctrl Pts',(19.9759107368159,0.981320658482397,8.00000002680193));
#31451=CARTESIAN_POINT('Ctrl Pts',(19.9817612010437,1.02518111344366,4.));
#31452=CARTESIAN_POINT('Ctrl Pts',(19.972814806454,1.19955490347979,5.33333334226731));
#31453=CARTESIAN_POINT('Ctrl Pts',(19.9615857398537,1.37381149585751,6.66666668453462));
#31454=CARTESIAN_POINT('Ctrl Pts',(19.9480778372514,1.54789134303979,8.00000002680193));
#31455=CARTESIAN_POINT('Ctrl Pts',(19.9446274510471,1.59173265652136,4.));
#31456=CARTESIAN_POINT('Ctrl Pts',(19.9307369611545,1.76578239343086,5.33333334226731));
#31457=CARTESIAN_POINT('Ctrl Pts',(19.9145680424726,1.93965021101785,6.66666668453462));
#31458=CARTESIAN_POINT('Ctrl Pts',(19.8961262215074,2.11327669479037,8.00000002680193));
#31459=CARTESIAN_POINT('Ctrl Pts',(19.8834864993867,2.15568194052487,4.));
#31460=CARTESIAN_POINT('Ctrl Pts',(19.8646746255167,2.32919809478258,5.33333334226731));
#31461=CARTESIAN_POINT('Ctrl Pts',(19.8435913009115,2.50246798676344,6.66666668453462));
#31462=CARTESIAN_POINT('Ctrl Pts',(19.8202437499699,2.67543224391478,8.00000002680193));
#31463=CARTESIAN_POINT('Ctrl Pts',(16.67120375536,-5.07536776045385,-12.));
#31464=CARTESIAN_POINT('Ctrl Pts',(16.9369493898684,-4.20246557304822,-4.));
#31465=CARTESIAN_POINT('Ctrl Pts',(17.1339941352951,-3.30865780933793,4.));
#31466=CARTESIAN_POINT('Ctrl Pts',(17.2599160133439,-2.4049307201863,12.));
#31467=CARTESIAN_POINT('Ctrl Pts',(16.0568250729579,-4.88832681229369,-12.));
#31468=CARTESIAN_POINT('Ctrl Pts',(16.312777266322,-4.04759341747401,-4.00000000000001));
#31469=CARTESIAN_POINT('Ctrl Pts',(16.5025603830837,-3.1867248730455,4.00000000000001));
#31470=CARTESIAN_POINT('Ctrl Pts',(16.6238417013591,-2.31630255698834,12.));
#31471=CARTESIAN_POINT('Ctrl Pts',(15.4424463905558,-4.70128586413353,-12.));
#31472=CARTESIAN_POINT('Ctrl Pts',(15.6886051427755,-3.89272126189979,-3.99999999999999));
#31473=CARTESIAN_POINT('Ctrl Pts',(15.8711266308723,-3.06479193675307,3.99999999999999));
#31474=CARTESIAN_POINT('Ctrl Pts',(15.9877673893743,-2.22767439379039,12.));
#31475=CARTESIAN_POINT('Ctrl Pts',(14.8280677081537,-4.51424491597337,-12.));
#31476=CARTESIAN_POINT('Ctrl Pts',(15.0644330192291,-3.73784910632557,-4.));
#31477=CARTESIAN_POINT('Ctrl Pts',(15.2396928786609,-2.94285900046064,4.));
#31478=CARTESIAN_POINT('Ctrl Pts',(15.3516930773895,-2.13904623059243,12.));
#31479=CARTESIAN_POINT('',(14.8280677332334,-4.51424491927473,-11.9999999957355));
#31480=CARTESIAN_POINT('',(15.3044692038576,-4.65928020123585,-12.));
#31481=CARTESIAN_POINT('Ctrl Pts',(15.3516930767777,-2.13904623498331,11.9999999562994));
#31482=CARTESIAN_POINT('Ctrl Pts',(15.3237029275181,-2.33992852728642,10.0007056240913));
#31483=CARTESIAN_POINT('Ctrl Pts',(15.2917618106915,-2.54031911975201,8.00083387021915));
#31484=CARTESIAN_POINT('Ctrl Pts',(15.2558790213823,-2.74010132749604,5.99999995642121));
#31485=CARTESIAN_POINT('Ctrl Pts',(15.2200100350179,-2.9398066855075,3.9999356985046));
#31486=CARTESIAN_POINT('Ctrl Pts',(15.1802231246131,-3.13878875107566,2.00006422723888));
#31487=CARTESIAN_POINT('Ctrl Pts',(15.1365413257817,-3.33693222779593,2.22044604925032E-15));
#31488=CARTESIAN_POINT('Ctrl Pts',(15.0928595269503,-3.53507570451619,-2.00006422723888));
#31489=CARTESIAN_POINT('Ctrl Pts',(15.0452912745672,-3.73234233124902,-3.99993569850461));
#31490=CARTESIAN_POINT('Ctrl Pts',(14.9938641476362,-3.92861781320467,-5.99999995642121));
#31491=CARTESIAN_POINT('Ctrl Pts',(14.9424246385123,-4.12494055272706,-8.00054577305927));
#31492=CARTESIAN_POINT('Ctrl Pts',(14.8871467284008,-4.32018647843707,-10.0004173920443));
#31493=CARTESIAN_POINT('Ctrl Pts',(14.8280677289536,-4.51424492140107,-11.9999999914697));
#31494=CARTESIAN_POINT('Ctrl Pts',(15.5228520082561,-7.92019304563387,-10.5713320279724));
#31495=CARTESIAN_POINT('Ctrl Pts',(15.8881799221207,-7.20418383869531,-3.52377734265747));
#31496=CARTESIAN_POINT('Ctrl Pts',(16.20388659607,-6.46286199768348,3.52377734265748));
#31497=CARTESIAN_POINT('Ctrl Pts',(16.4669580190248,-5.70330482702815,10.5713320279724));
#31498=CARTESIAN_POINT('Ctrl Pts',(15.5231950610407,-7.92036478087607,-10.5713320279724));
#31499=CARTESIAN_POINT('Ctrl Pts',(15.8885308963887,-7.20433975023758,-3.52377734265747));
#31500=CARTESIAN_POINT('Ctrl Pts',(16.2042443952,-6.46300153666839,3.52377734265748));
#31501=CARTESIAN_POINT('Ctrl Pts',(16.4673214812396,-5.70342760090494,10.5713320279724));
#31502=CARTESIAN_POINT('Ctrl Pts',(15.5235381138555,-7.92053651613241,-10.5713320279724));
#31503=CARTESIAN_POINT('Ctrl Pts',(15.8888818706875,-7.20449566179256,-3.52377734265747));
#31504=CARTESIAN_POINT('Ctrl Pts',(16.2046021943615,-6.46314107566464,3.52377734265748));
#31505=CARTESIAN_POINT('Ctrl Pts',(16.4676849434863,-5.70355037479156,10.5713320279724));
#31506=CARTESIAN_POINT('Ctrl Pts',(15.5238811666727,-7.92070825138992,-10.5713320279724));
#31507=CARTESIAN_POINT('Ctrl Pts',(15.8892328449888,-7.20465157334867,-3.52377734265747));
#31508=CARTESIAN_POINT('Ctrl Pts',(16.2049599935256,-6.46328061466174,3.52377734265748));
#31509=CARTESIAN_POINT('Ctrl Pts',(16.4680484057355,-5.703673148679,10.5713320279724));
#31510=CARTESIAN_POINT('Ctrl Pts',(15.5228507477964,-7.92019248660846,-10.5713320134286));
#31511=CARTESIAN_POINT('Ctrl Pts',(15.8881669516022,-7.20417811498612,-3.52377733780954));
#31512=CARTESIAN_POINT('Ctrl Pts',(16.2038734814214,-6.462856612406,3.52377733780954));
#31513=CARTESIAN_POINT('Ctrl Pts',(16.466956742565,-5.70330430555752,10.5713320134286));
#31514=CARTESIAN_POINT('Ctrl Pts',(13.7402020358534,-7.17334281440039,-12.));
#31515=CARTESIAN_POINT('Ctrl Pts',(14.1157973873101,-6.45390751815578,-4.));
#31516=CARTESIAN_POINT('Ctrl Pts',(14.4347687202385,-5.70491981764189,4.));
#31517=CARTESIAN_POINT('Ctrl Pts',(14.6931953939549,-4.93558590585175,12.));
#31518=CARTESIAN_POINT('Ctrl Pts',(14.3095066403964,-7.4705594843989,-12.));
#31519=CARTESIAN_POINT('Ctrl Pts',(14.7006642203029,-6.72131546876617,-4.00000000000001));
#31520=CARTESIAN_POINT('Ctrl Pts',(15.0328516506424,-5.94129458944342,4.00000000000001));
#31521=CARTESIAN_POINT('Ctrl Pts',(15.3019858448814,-5.14008448418318,12.));
#31522=CARTESIAN_POINT('Ctrl Pts',(14.8788112449393,-7.76777615439741,-12.));
#31523=CARTESIAN_POINT('Ctrl Pts',(15.2855310532957,-6.98872341937657,-4.));
#31524=CARTESIAN_POINT('Ctrl Pts',(15.6309345810462,-6.17766936124495,4.));
#31525=CARTESIAN_POINT('Ctrl Pts',(15.9107762958078,-5.34458306251461,12.));
#31526=CARTESIAN_POINT('Ctrl Pts',(15.4481158494822,-8.06499282439593,-12.));
#31527=CARTESIAN_POINT('Ctrl Pts',(15.8703978862885,-7.25613136998697,-4.));
#31528=CARTESIAN_POINT('Ctrl Pts',(16.2290175114501,-6.41404413304648,4.));
#31529=CARTESIAN_POINT('Ctrl Pts',(16.5195667467343,-5.54908164084604,12.));
#31530=CARTESIAN_POINT('',(13.740202059893,-7.17334282227374,-11.9999999957355));
#31531=CARTESIAN_POINT('Ctrl Pts',(13.7402020552943,-7.1733428235737,-11.9999999914697));
#31532=CARTESIAN_POINT('Ctrl Pts',(13.8340813002562,-6.99352153777388,-10.0004173920443));
#31533=CARTESIAN_POINT('Ctrl Pts',(13.9244439127861,-6.81183164507366,-8.00054577305927));
#31534=CARTESIAN_POINT('Ctrl Pts',(14.0112327972984,-6.62837502710201,-5.9999999564212));
#31535=CARTESIAN_POINT('Ctrl Pts',(14.09800079054,-6.44496256964578,-3.99993569850461));
#31536=CARTESIAN_POINT('Ctrl Pts',(14.1811591229608,-6.25986380572143,-2.00006422723887));
#31537=CARTESIAN_POINT('Ctrl Pts',(14.2606595952488,-6.07318597677024,-2.22044604925031E-15));
#31538=CARTESIAN_POINT('Ctrl Pts',(14.3401600675367,-5.88650814781905,2.00006422723888));
#31539=CARTESIAN_POINT('Ctrl Pts',(14.4159873282975,-5.69828730098519,3.99993569850461));
#31540=CARTESIAN_POINT('Ctrl Pts',(14.4880974587037,-5.50863250063969,5.99999995642122));
#31541=CARTESIAN_POINT('Ctrl Pts',(14.5602353382114,-5.31890471817277,8.00083387021916));
#31542=CARTESIAN_POINT('Ctrl Pts',(14.6286115396895,-5.127851533001,10.0007056240913));
#31543=CARTESIAN_POINT('Ctrl Pts',(14.6931953925432,-4.93558591005429,11.9999999562994));
#31544=CARTESIAN_POINT('',(13.7402020549027,-7.17334282434542,-12.));
#31545=CARTESIAN_POINT('Origin',(2.22044604925031E-15,-4.16333634234434E-16,
-6.));
#31546=CARTESIAN_POINT('',(15.364994223987,-2.04131143860991,-11.9999999957355));
#31547=CARTESIAN_POINT('Origin',(2.22044604925031E-15,-4.16333634234434E-16,
-12.));
#31548=CARTESIAN_POINT('Ctrl Pts',(15.3649942201102,-2.04131144140431,-11.9999999914697));
#31549=CARTESIAN_POINT('Ctrl Pts',(15.3917093519036,-1.84022611326084,-10.0004173920443));
#31550=CARTESIAN_POINT('Ctrl Pts',(15.4144808289508,-1.63858762813028,-8.00054577305927));
#31551=CARTESIAN_POINT('Ctrl Pts',(15.4332898445205,-1.43651125126802,-5.99999995642121));
#31552=CARTESIAN_POINT('Ctrl Pts',(15.4520943325031,-1.23448351695164,-3.99993569850461));
#31553=CARTESIAN_POINT('Ctrl Pts',(15.466930098069,-1.03210574960204,-2.00006422723889));
#31554=CARTESIAN_POINT('Ctrl Pts',(15.4777885274135,-0.829495208345887,
-6.66133814775094E-15));
#31555=CARTESIAN_POINT('Ctrl Pts',(15.4886469567579,-0.626884667089731,
2.00006422723887));
#31556=CARTESIAN_POINT('Ctrl Pts',(15.495525953138,-0.42408047564849,3.99993569850462));
#31557=CARTESIAN_POINT('Ctrl Pts',(15.4984215485681,-0.22120014213042,5.99999995642122));
#31558=CARTESIAN_POINT('Ctrl Pts',(15.5013182582685,-0.0182417370997565,
8.00083387021916));
#31559=CARTESIAN_POINT('Ctrl Pts',(15.5002268324596,0.184675569413392,10.0007056240913));
#31560=CARTESIAN_POINT('Ctrl Pts',(15.4951570864913,0.387435135136788,11.9999999562994));
#31561=CARTESIAN_POINT('Origin',(2.22044604925031E-15,-4.16333634234434E-16,
-6.));
#31562=CARTESIAN_POINT('',(12.3898631351355,-9.31350049042594,-11.9999999957355));
#31563=CARTESIAN_POINT('Ctrl Pts',(13.6942758009489,-7.26063422894488,11.9999999562994));
#31564=CARTESIAN_POINT('Ctrl Pts',(13.5992678738299,-7.43982864180721,10.0007056240913));
#31565=CARTESIAN_POINT('Ctrl Pts',(13.500715422892,-7.617209697467,8.00083387021915));
#31566=CARTESIAN_POINT('Ctrl Pts',(13.3986670912385,-7.79267092710594,5.99999995642121));
#31567=CARTESIAN_POINT('Ctrl Pts',(13.2966580142668,-7.9680646625034,3.9999356985046));
#31568=CARTESIAN_POINT('Ctrl Pts',(13.1912146735706,-8.14143871638738,2.00006422723888));
#31569=CARTESIAN_POINT('Ctrl Pts',(13.0823981492392,-8.31269262422126,-4.44089209850063E-15));
#31570=CARTESIAN_POINT('Ctrl Pts',(12.9735816249078,-8.48394653205514,-2.00006422723888));
#31571=CARTESIAN_POINT('Ctrl Pts',(12.8614129292112,-8.65304722502548,-3.99993569850461));
#31572=CARTESIAN_POINT('Ctrl Pts',(12.7459570690561,-8.81989673373664,-5.99999995642121));
#31573=CARTESIAN_POINT('Ctrl Pts',(12.630473410406,-8.98678641507513,-8.00054577305927));
#31574=CARTESIAN_POINT('Ctrl Pts',(12.5117511266867,-9.15135141196428,-10.0004173920443));
#31575=CARTESIAN_POINT('Ctrl Pts',(12.3898631303866,-9.31350049096029,-11.9999999914697));
#31576=CARTESIAN_POINT('Origin',(2.22044604925031E-15,-4.16333634234434E-16,
-12.));
#31577=CARTESIAN_POINT('Ctrl Pts',(10.4581387236936,-11.4401631786859,-12.));
#31578=CARTESIAN_POINT('Ctrl Pts',(11.0571442669941,-10.8925763156096,-4.));
#31579=CARTESIAN_POINT('Ctrl Pts',(11.613048155468,-10.2978527213822,4.));
#31580=CARTESIAN_POINT('Ctrl Pts',(12.1190174885494,-9.66330244953633,12.));
#31581=CARTESIAN_POINT('Ctrl Pts',(10.8914559714904,-11.9141691326998,-12.));
#31582=CARTESIAN_POINT('Ctrl Pts',(11.5152804085056,-11.3438938315843,-4.00000000000001));
#31583=CARTESIAN_POINT('Ctrl Pts',(12.0942173384564,-10.7245287597614,4.00000000000001));
#31584=CARTESIAN_POINT('Ctrl Pts',(12.6211507498191,-10.0636868518367,12.));
#31585=CARTESIAN_POINT('Ctrl Pts',(11.3247732192872,-12.3881750867137,-12.));
#31586=CARTESIAN_POINT('Ctrl Pts',(11.9734165500172,-11.795211347559,-3.99999999999999));
#31587=CARTESIAN_POINT('Ctrl Pts',(12.5753865214448,-11.1512047981406,3.99999999999999));
#31588=CARTESIAN_POINT('Ctrl Pts',(13.1232840110888,-10.4640712541372,12.));
#31589=CARTESIAN_POINT('Ctrl Pts',(11.7580904670839,-12.8621810407276,-12.));
#31590=CARTESIAN_POINT('Ctrl Pts',(12.4315526915288,-12.2465288635337,-4.));
#31591=CARTESIAN_POINT('Ctrl Pts',(13.0565557044332,-11.5778808365199,4.));
#31592=CARTESIAN_POINT('Ctrl Pts',(13.6254172723585,-10.8644556564376,12.));
#31593=CARTESIAN_POINT('',(10.4581387435906,-11.4401631943065,-11.9999999957355));
#31594=CARTESIAN_POINT('Ctrl Pts',(10.4581387388246,-11.4401631939552,-11.9999999914697));
#31595=CARTESIAN_POINT('Ctrl Pts',(10.6078588745025,-11.303295051446,-10.0004173920443));
#31596=CARTESIAN_POINT('Ctrl Pts',(10.7549135578339,-11.163468233693,-8.00054577305927));
#31597=CARTESIAN_POINT('Ctrl Pts',(10.8992142909491,-11.0207589502706,-5.99999995642121));
#31598=CARTESIAN_POINT('Ctrl Pts',(11.0434802889055,-10.8780840189234,-3.99993569850461));
#31599=CARTESIAN_POINT('Ctrl Pts',(11.184931066005,-10.7325899011204,-2.00006422723888));
#31600=CARTESIAN_POINT('Ctrl Pts',(11.3234846509767,-10.584360885717,0.));
#31601=CARTESIAN_POINT('Ctrl Pts',(11.4620382359483,-10.4361318703137,2.00006422723888));
#31602=CARTESIAN_POINT('Ctrl Pts',(11.5976678743505,-10.2851965800591,3.9999356985046));
#31603=CARTESIAN_POINT('Ctrl Pts',(11.7302949937737,-10.1316424808146,5.99999995642121));
#31604=CARTESIAN_POINT('Ctrl Pts',(11.8629731501784,-9.97802929156078,8.00083387021915));
#31605=CARTESIAN_POINT('Ctrl Pts',(11.99256979992,-9.82188406150686,10.0007056240913));
#31606=CARTESIAN_POINT('Ctrl Pts',(12.1190174857855,-9.66330245300261,11.9999999562994));
#31607=CARTESIAN_POINT('',(10.4581387381927,-11.4401631945464,-12.));
#31608=CARTESIAN_POINT('Ctrl Pts',(11.8778429311088,-12.7516740731249,-10.5713320220547));
#31609=CARTESIAN_POINT('Ctrl Pts',(12.466019210595,-12.2037861517057,-3.52377734068488));
#31610=CARTESIAN_POINT('Ctrl Pts',(13.0162331940139,-11.6151497981962,3.52377734068489));
#31611=CARTESIAN_POINT('Ctrl Pts',(13.5232327823929,-10.9913838744951,10.5713320220547));
#31612=CARTESIAN_POINT('Ctrl Pts',(13.9299291396692,-10.4711731300928,-12.));
#31613=CARTESIAN_POINT('Ctrl Pts',(14.4781984826686,-9.74180374592263,-4.));
#31614=CARTESIAN_POINT('Ctrl Pts',(14.9690602353605,-8.96929245803532,4.));
#31615=CARTESIAN_POINT('Ctrl Pts',(15.3964809635174,-8.1631345999333,12.));
#31616=CARTESIAN_POINT('Ctrl Pts',(13.4165737973453,-10.0852822463105,-12.));
#31617=CARTESIAN_POINT('Ctrl Pts',(13.9446379409184,-9.38279208500909,-4.00000000000001));
#31618=CARTESIAN_POINT('Ctrl Pts',(14.4174101182391,-8.63874991513855,4.00000000000001));
#31619=CARTESIAN_POINT('Ctrl Pts',(14.8290792433535,-7.86230114163155,12.));
#31620=CARTESIAN_POINT('Ctrl Pts',(12.9032184550213,-9.6993913625282,-12.));
#31621=CARTESIAN_POINT('Ctrl Pts',(13.4110773991682,-9.02378042409555,-4.));
#31622=CARTESIAN_POINT('Ctrl Pts',(13.8657600011178,-8.30820737224178,4.));
#31623=CARTESIAN_POINT('Ctrl Pts',(14.2616775231895,-7.56146768332979,12.));
#31624=CARTESIAN_POINT('Ctrl Pts',(12.3898631126974,-9.3135004787459,-12.));
#31625=CARTESIAN_POINT('Ctrl Pts',(12.877516857418,-8.66476876318201,-4.));
#31626=CARTESIAN_POINT('Ctrl Pts',(13.3141098839964,-7.977664829345,4.));
#31627=CARTESIAN_POINT('Ctrl Pts',(13.6942758030256,-7.26063422502805,12.));
#31628=CARTESIAN_POINT('',(12.787929093689,-9.61272797390185,-12.));
#31629=CARTESIAN_POINT('Ctrl Pts',(11.8778439250753,-12.7516750288689,-10.5713320279724));
#31630=CARTESIAN_POINT('Ctrl Pts',(12.4660294414806,-12.2037959661548,-3.52377734265748));
#31631=CARTESIAN_POINT('Ctrl Pts',(13.0162436756369,-11.6151593444016,3.52377734265748));
#31632=CARTESIAN_POINT('Ctrl Pts',(13.5232338028988,-10.9913848018556,10.5713320279724));
#31633=CARTESIAN_POINT('Ctrl Pts',(11.878107552328,-12.7519537381656,-10.5713320279724));
#31634=CARTESIAN_POINT('Ctrl Pts',(12.4663059245166,-12.2040625153446,-3.52377734265747));
#31635=CARTESIAN_POINT('Ctrl Pts',(13.0165321716897,-11.6154128426606,3.52377734265748));
#31636=CARTESIAN_POINT('Ctrl Pts',(13.523533354515,-10.9916244829556,10.5713320279724));
#31637=CARTESIAN_POINT('Ctrl Pts',(11.8783711796043,-12.7522324474859,-10.5713320279724));
#31638=CARTESIAN_POINT('Ctrl Pts',(12.4665824075774,-12.2043290645569,-3.52377734265747));
#31639=CARTESIAN_POINT('Ctrl Pts',(13.0168206677681,-11.615666340941,3.52377734265748));
#31640=CARTESIAN_POINT('Ctrl Pts',(13.5238329061577,-10.9918641640757,10.5713320279724));
#31641=CARTESIAN_POINT('Ctrl Pts',(11.8786348068824,-12.7525111568082,-10.5713320279724));
#31642=CARTESIAN_POINT('Ctrl Pts',(12.46685889064,-12.2045956137711,-3.52377734265748));
#31643=CARTESIAN_POINT('Ctrl Pts',(13.0171091638486,-11.6159198392231,3.52377734265748));
#31644=CARTESIAN_POINT('Ctrl Pts',(13.5241324578026,-10.9921038451975,10.5713320279724));
#31645=CARTESIAN_POINT('Ctrl Pts',(9.50849948587549,-14.604000482186,-12.));
#31646=CARTESIAN_POINT('Ctrl Pts',(10.2731631630064,-14.1061366133278,-4.));
#31647=CARTESIAN_POINT('Ctrl Pts',(10.998636751241,-13.548098063635,4.));
#31648=CARTESIAN_POINT('Ctrl Pts',(11.6760030816321,-12.9367439718926,12.));
#31649=CARTESIAN_POINT('Ctrl Pts',(9.15808571423198,-14.0658037985085,-12.));
#31650=CARTESIAN_POINT('Ctrl Pts',(9.89456947890248,-13.5862875518289,-3.99999999999999));
#31651=CARTESIAN_POINT('Ctrl Pts',(10.5933074148231,-13.0488142230957,3.99999999999998));
#31652=CARTESIAN_POINT('Ctrl Pts',(11.2457109746983,-12.4599901733872,12.));
#31653=CARTESIAN_POINT('Ctrl Pts',(8.80767194258846,-13.5276071148311,-12.));
#31654=CARTESIAN_POINT('Ctrl Pts',(9.5159757947985,-13.0664384903301,-4.00000000000001));
#31655=CARTESIAN_POINT('Ctrl Pts',(10.1879780784053,-12.5495303825563,4.00000000000001));
#31656=CARTESIAN_POINT('Ctrl Pts',(10.8154188677646,-11.9832363748819,12.));
#31657=CARTESIAN_POINT('Ctrl Pts',(8.45725817094494,-12.9894104311537,-12.));
#31658=CARTESIAN_POINT('Ctrl Pts',(9.13738211069453,-12.5465894288312,-4.));
#31659=CARTESIAN_POINT('Ctrl Pts',(9.78264874198742,-12.0502465420169,4.));
#31660=CARTESIAN_POINT('Ctrl Pts',(10.3851267608308,-11.5064825763765,12.));
#31661=CARTESIAN_POINT('',(8.45725818803503,-12.9894104498036,-11.9999999957355));
#31662=CARTESIAN_POINT('',(8.72897600508842,-13.4067388841598,-12.));
#31663=CARTESIAN_POINT('Ctrl Pts',(10.3851267575397,-11.5064825793469,11.9999999562994));
#31664=CARTESIAN_POINT('Ctrl Pts',(10.2345604107395,-11.6423756219493,10.0007056240913));
#31665=CARTESIAN_POINT('Ctrl Pts',(10.0812835057528,-11.7753523676252,8.00083387021916));
#31666=CARTESIAN_POINT('Ctrl Pts',(9.92537816662527,-11.9053294053327,5.99999995642122));
#31667=CARTESIAN_POINT('Ctrl Pts',(9.76953279922271,-12.0352564450914,3.99993569850462));
#31668=CARTESIAN_POINT('Ctrl Pts',(9.61115105130115,-12.1621110176642,2.00006422723887));
#31669=CARTESIAN_POINT('Ctrl Pts',(9.45032468026494,-12.2858196078884,-6.66133814958239E-15));
#31670=CARTESIAN_POINT('Ctrl Pts',(9.28949830922873,-12.4095281981127,-2.00006422723888));
#31671=CARTESIAN_POINT('Ctrl Pts',(9.1262583703532,-12.5300669180878,-3.9999356985046));
#31672=CARTESIAN_POINT('Ctrl Pts',(8.9606994576558,-12.6473659403674,-5.9999999564212));
#31673=CARTESIAN_POINT('Ctrl Pts',(8.79510068306996,-12.7646932049232,-8.00054577305927));
#31674=CARTESIAN_POINT('Ctrl Pts',(8.62725368531363,-12.878728305646,-10.0004173920443));
#31675=CARTESIAN_POINT('Ctrl Pts',(8.45725818338972,-12.9894104486815,-11.9999999914697));
#31676=CARTESIAN_POINT('Ctrl Pts',(5.91466953576707,-14.3271310247952,-12.));
#31677=CARTESIAN_POINT('Ctrl Pts',(6.66483636200898,-14.0174396520956,-4.));
#31678=CARTESIAN_POINT('Ctrl Pts',(7.39062259281096,-13.648712606804,4.));
#31679=CARTESIAN_POINT('Ctrl Pts',(8.08310721637552,-13.2254821026516,12.));
#31680=CARTESIAN_POINT('Ctrl Pts',(6.1597349716519,-14.9207541491876,-12.));
#31681=CARTESIAN_POINT('Ctrl Pts',(6.94098383200368,-14.5982311802709,-4.00000000000002));
#31682=CARTESIAN_POINT('Ctrl Pts',(7.69684192361464,-14.2142264844647,4.00000000000002));
#31683=CARTESIAN_POINT('Ctrl Pts',(8.41801860598166,-13.7734600609591,12.));
#31684=CARTESIAN_POINT('Ctrl Pts',(6.40480040753673,-15.51437727358,-12.));
#31685=CARTESIAN_POINT('Ctrl Pts',(7.21713130199838,-15.1790227084462,-3.99999999999999));
#31686=CARTESIAN_POINT('Ctrl Pts',(8.00306125441832,-14.7797403621254,3.99999999999999));
#31687=CARTESIAN_POINT('Ctrl Pts',(8.75292999558781,-14.3214380192667,12.));
#31688=CARTESIAN_POINT('Ctrl Pts',(6.64986584342156,-16.1080003979724,-12.));
#31689=CARTESIAN_POINT('Ctrl Pts',(7.49327877199308,-15.7598142366215,-4.));
#31690=CARTESIAN_POINT('Ctrl Pts',(8.30928058522199,-15.3452542397861,4.));
#31691=CARTESIAN_POINT('Ctrl Pts',(9.08784138519396,-14.8694159775742,12.));
#31692=CARTESIAN_POINT('',(5.91466954912158,-14.3271310462789,-11.9999999957355));
#31693=CARTESIAN_POINT('Ctrl Pts',(5.91466954476316,-14.3271310443187,-11.9999999914697));
#31694=CARTESIAN_POINT('Ctrl Pts',(6.10217211316044,-14.2497243630455,-10.0004173920443));
#31695=CARTESIAN_POINT('Ctrl Pts',(6.28818190218767,-14.1686257980847,-8.00054577305927));
#31696=CARTESIAN_POINT('Ctrl Pts',(6.47258968583999,-14.0838766949572,-5.99999995642121));
#31697=CARTESIAN_POINT('Ctrl Pts',(6.65695308001832,-13.9991479920971,-3.99993569850461));
#31698=CARTESIAN_POINT('Ctrl Pts',(6.83963525048719,-13.910807258287,-2.00006422723888));
#31699=CARTESIAN_POINT('Ctrl Pts',(7.02053034096174,-13.8189056633163,-6.66133814775094E-15));
#31700=CARTESIAN_POINT('Ctrl Pts',(7.20142543143629,-13.7270040683457,2.00006422723887));
#31701=CARTESIAN_POINT('Ctrl Pts',(7.38049851140845,-13.6315593582429,3.9999356985046));
#31702=CARTESIAN_POINT('Ctrl Pts',(7.55764583187841,-13.5326268506854,5.99999995642121));
#31703=CARTESIAN_POINT('Ctrl Pts',(7.7348613213967,-13.4336562723579,8.00083387021915));
#31704=CARTESIAN_POINT('Ctrl Pts',(7.91004715080014,-13.3312524166245,10.0007056240913));
#31705=CARTESIAN_POINT('Ctrl Pts',(8.08310721259279,-13.2254821049635,11.9999999562994));
#31706=CARTESIAN_POINT('',(5.9146695439671,-14.3271310446582,-12.));
#31707=CARTESIAN_POINT('Ctrl Pts',(6.8001919590846,-16.04511557088,-10.5713320220547));
#31708=CARTESIAN_POINT('Ctrl Pts',(7.54028557404929,-15.7314374695154,-3.52377734068488));
#31709=CARTESIAN_POINT('Ctrl Pts',(8.25864308411528,-15.3664844972649,3.52377734068489));
#31710=CARTESIAN_POINT('Ctrl Pts',(8.94840736668245,-14.9537403335486,10.5713320220547));
#31711=CARTESIAN_POINT('Ctrl Pts',(6.80019256622394,-16.0451168089422,-10.5713320279724));
#31712=CARTESIAN_POINT('Ctrl Pts',(7.54029183119773,-15.7314501912497,-3.52377734265748));
#31713=CARTESIAN_POINT('Ctrl Pts',(8.25864966862457,-15.3664970526898,3.52377734265747));
#31714=CARTESIAN_POINT('Ctrl Pts',(8.94840800846834,-14.9537415540161,10.5713320279724));
#31715=CARTESIAN_POINT('Ctrl Pts',(6.80034497061742,-16.0454688758496,-10.5713320279724));
#31716=CARTESIAN_POINT('Ctrl Pts',(7.54046047507781,-15.731795228331,-3.52377734265747));
#31717=CARTESIAN_POINT('Ctrl Pts',(8.25883406472935,-15.3668339346014,3.52377734265747));
#31718=CARTESIAN_POINT('Ctrl Pts',(8.94860751915148,-14.9540692332704,10.5713320279724));
#31719=CARTESIAN_POINT('Ctrl Pts',(6.80049737502495,-16.0458209427872,-10.5713320279724));
#31720=CARTESIAN_POINT('Ctrl Pts',(7.54062911897337,-15.732140265442,-3.52377734265749));
#31721=CARTESIAN_POINT('Ctrl Pts',(8.25901846085091,-15.3671708165418,3.52377734265748));
#31722=CARTESIAN_POINT('Ctrl Pts',(8.94880702985273,-14.9543969125528,10.5713320279724));
#31723=CARTESIAN_POINT('Ctrl Pts',(6.80064977943359,-16.0461730097273,-10.5713320279724));
#31724=CARTESIAN_POINT('Ctrl Pts',(7.54079776287007,-15.7324853025553,-3.52377734265748));
#31725=CARTESIAN_POINT('Ctrl Pts',(8.25920285697386,-15.3675076984845,3.52377734265747));
#31726=CARTESIAN_POINT('Ctrl Pts',(8.94900654055539,-14.9547245918374,10.5713320279724));
#31727=CARTESIAN_POINT('Origin',(2.22044604925031E-15,-4.16333634234434E-16,
-12.));
#31728=CARTESIAN_POINT('Origin',(2.22044604925031E-15,-4.16333634234434E-16,
-12.));
#31729=CARTESIAN_POINT('',(3.50458308761994,-15.0986058056538,-11.9999999957355));
#31730=CARTESIAN_POINT('Origin',(2.22044604925031E-15,-4.16333634234434E-16,
-12.));
#31731=CARTESIAN_POINT('',(3.61717958430867,-15.5836992225952,-12.));
#31732=CARTESIAN_POINT('',(0.65780391580271,-15.4860354481354,-11.9999999957355));
#31733=CARTESIAN_POINT('',(0.657803911513399,-15.4860354448496,-12.));
#31734=CARTESIAN_POINT('',(-1.87079645529993,-15.3866864696526,-11.9999999957355));
#31735=CARTESIAN_POINT('Origin',(2.22044604925031E-15,-4.16333634234434E-16,
-12.));
#31736=CARTESIAN_POINT('',(-1.93090207822381,-15.8810354438797,-12.));
#31737=CARTESIAN_POINT('',(-4.67840257791378,-14.7770954254049,-11.9999999957355));
#31738=CARTESIAN_POINT('',(-4.67840258082059,-14.7770954208502,-12.));
#31739=CARTESIAN_POINT('',(-7.02053033569551,-13.8189056621041,-11.9999999957355));
#31740=CARTESIAN_POINT('Origin',(2.22044604925031E-15,-4.16333634234434E-16,
-12.));
#31741=CARTESIAN_POINT('',(-7.24608845304286,-14.2628844115113,-12.));
#31742=CARTESIAN_POINT('',(-9.45032467486545,-12.285819607669,-11.9999999957355));
#31743=CARTESIAN_POINT('',(-9.45032467603913,-12.2858196023947,-12.));
#31744=CARTESIAN_POINT('',(-11.3234846456134,-10.5843608863791,-11.9999999957355));
#31745=CARTESIAN_POINT('Origin',(2.22044604925031E-15,-4.16333634234434E-16,
-12.));
#31746=CARTESIAN_POINT('',(-11.6872896195489,-10.9244190213593,-12.));
#31747=CARTESIAN_POINT('',(-13.0823981440903,-8.31269262586177,-11.9999999957355));
#31748=CARTESIAN_POINT('',(-13.0823981433893,-8.31269262050417,-12.));
#31749=CARTESIAN_POINT('',(-14.2606595904354,-6.07318597922667,-11.9999999957355));
#31750=CARTESIAN_POINT('Origin',(2.22044604925031E-15,-4.16333634234434E-16,
-12.));
#31751=CARTESIAN_POINT('',(-14.7188311719128,-6.26830746997787,-12.));
#31752=CARTESIAN_POINT('',(-15.1365413215044,-3.33693223109852,-11.9999999957355));
#31753=CARTESIAN_POINT('',(-15.1365413190133,-3.33693222630378,-12.));
#31754=CARTESIAN_POINT('',(-15.4777885237305,-0.829495212300453,-11.9999999957355));
#31755=CARTESIAN_POINT('Origin',(2.22044604925031E-15,-4.16333634234434E-16,
-12.));
#31756=CARTESIAN_POINT('',(-15.9750644581313,-0.856145527351446,-12.));
#31757=CARTESIAN_POINT('',(-15.364994223987,2.04131143860991,-11.9999999957355));
#31758=CARTESIAN_POINT('',(-15.3649942200062,2.04131144226347,-12.));
#31759=CARTESIAN_POINT('',(-14.8280677332333,4.51424491927474,-11.9999999957355));
#31760=CARTESIAN_POINT('Origin',(2.22044604925031E-15,-4.16333634234434E-16,
-12.));
#31761=CARTESIAN_POINT('',(-15.3044692038576,4.65928020123584,-12.));
#31762=CARTESIAN_POINT('',(-13.740202059893,7.17334282227373,-11.9999999957355));
#31763=CARTESIAN_POINT('',(-13.7402020549027,7.17334282434542,-12.));
#31764=CARTESIAN_POINT('',(-12.3898631351355,9.31350049042594,-11.9999999957355));
#31765=CARTESIAN_POINT('Origin',(2.22044604925031E-15,-4.16333634234434E-16,
-12.));
#31766=CARTESIAN_POINT('',(-12.787929093689,9.61272797390186,-12.));
#31767=CARTESIAN_POINT('',(-10.4581387435906,11.4401631943064,-11.9999999957355));
#31768=CARTESIAN_POINT('',(-10.4581387381927,11.4401631945464,-12.));
#31769=CARTESIAN_POINT('',(-8.45725818803502,12.9894104498036,-11.9999999957355));
#31770=CARTESIAN_POINT('Origin',(2.22044604925031E-15,-4.16333634234434E-16,
-12.));
#31771=CARTESIAN_POINT('',(-8.72897600508841,13.4067388841599,-12.));
#31772=CARTESIAN_POINT('',(-5.91466954912156,14.3271310462789,-11.9999999957355));
#31773=CARTESIAN_POINT('',(-5.91466954396709,14.3271310446582,-12.));
#31774=CARTESIAN_POINT('',(-3.50458308761994,15.0986058056538,-11.9999999957355));
#31775=CARTESIAN_POINT('Origin',(2.22044604925031E-15,-4.16333634234434E-16,
-12.));
#31776=CARTESIAN_POINT('',(-3.61717958430867,15.5836992225952,-12.));
#31777=CARTESIAN_POINT('',(-0.657803915802711,15.4860354481354,-11.9999999957355));
#31778=CARTESIAN_POINT('',(-0.6578039115134,15.4860354448496,-12.));
#31779=CARTESIAN_POINT('',(1.87079645529994,15.3866864696526,-11.9999999957355));
#31780=CARTESIAN_POINT('Origin',(2.22044604925031E-15,-4.16333634234434E-16,
-12.));
#31781=CARTESIAN_POINT('',(1.93090207822382,15.8810354438797,-12.));
#31782=CARTESIAN_POINT('',(4.67840257791379,14.7770954254049,-11.9999999957355));
#31783=CARTESIAN_POINT('',(4.6784025808206,14.7770954208502,-12.));
#31784=CARTESIAN_POINT('',(7.02053033569551,13.8189056621041,-11.9999999957355));
#31785=CARTESIAN_POINT('Origin',(2.22044604925031E-15,-4.16333634234434E-16,
-12.));
#31786=CARTESIAN_POINT('',(7.24608845304286,14.2628844115113,-12.));
#31787=CARTESIAN_POINT('',(9.45032467486545,12.285819607669,-11.9999999957355));
#31788=CARTESIAN_POINT('',(9.45032467603913,12.2858196023947,-12.));
#31789=CARTESIAN_POINT('',(11.3234846456134,10.5843608863791,-11.9999999957355));
#31790=CARTESIAN_POINT('Origin',(2.22044604925031E-15,-4.16333634234434E-16,
-12.));
#31791=CARTESIAN_POINT('',(11.6872896195489,10.9244190213593,-12.));
#31792=CARTESIAN_POINT('',(13.0823981440903,8.31269262586177,-11.9999999957355));
#31793=CARTESIAN_POINT('',(13.0823981433893,8.31269262050417,-12.));
#31794=CARTESIAN_POINT('',(14.2606595904354,6.07318597922668,-11.9999999957355));
#31795=CARTESIAN_POINT('Origin',(2.22044604925031E-15,-4.16333634234434E-16,
-12.));
#31796=CARTESIAN_POINT('',(14.7188311719128,6.26830746997787,-12.));
#31797=CARTESIAN_POINT('',(15.1365413215044,3.33693223109852,-11.9999999957355));
#31798=CARTESIAN_POINT('',(15.1365413190133,3.33693222630378,-12.));
#31799=CARTESIAN_POINT('',(15.4777885237305,0.829495212300455,-11.9999999957355));
#31800=CARTESIAN_POINT('Origin',(2.22044604925031E-15,-4.16333634234434E-16,
-12.));
#31801=CARTESIAN_POINT('',(15.9750644581313,0.856145527351446,-12.));
#31802=CARTESIAN_POINT('',(15.3649942200062,-2.04131144226347,-12.));
#31803=CARTESIAN_POINT('Origin',(2.22044604925031E-15,-4.16333634234434E-16,
-6.));
#31804=CARTESIAN_POINT('Ctrl Pts',(5.82337815902385,-14.3644793130828,11.9999999562994));
#31805=CARTESIAN_POINT('Ctrl Pts',(5.63541391608915,-14.4406802789199,10.0007056240913));
#31806=CARTESIAN_POINT('Ctrl Pts',(5.44590001392117,-14.5132137565555,8.00083387021915));
#31807=CARTESIAN_POINT('Ctrl Pts',(5.25494215213615,-14.5820294533272,5.99999995642121));
#31808=CARTESIAN_POINT('Ctrl Pts',(5.06405774564414,-14.6508186789333,3.9999356985046));
#31809=CARTESIAN_POINT('Ctrl Pts',(4.87184076676219,-14.7158532365687,2.00006422723887));
#31810=CARTESIAN_POINT('Ctrl Pts',(4.67840258291259,-14.7770954274579,-2.22044604925031E-15));
#31811=CARTESIAN_POINT('Ctrl Pts',(4.48496439906298,-14.8383376183471,-2.00006422723887));
#31812=CARTESIAN_POINT('Ctrl Pts',(4.29034236280191,-14.895775616736,-3.99993569850461));
#31813=CARTESIAN_POINT('Ctrl Pts',(4.0946492458228,-14.949376159348,-5.99999995642121));
#31814=CARTESIAN_POINT('Ctrl Pts',(3.89890901149391,-15.0029896074497,-8.00054577305927));
#31815=CARTESIAN_POINT('Ctrl Pts',(3.70218212478788,-15.05274049588,-10.0004173920443));
#31816=CARTESIAN_POINT('Ctrl Pts',(3.50458308363856,-15.0986058030105,-11.9999999914697));
#31817=CARTESIAN_POINT('Ctrl Pts',(3.94020446357842,-16.9753698440352,-12.));
#31818=CARTESIAN_POINT('Ctrl Pts',(4.82903275014493,-16.7690612207615,-4.));
#31819=CARTESIAN_POINT('Ctrl Pts',(5.70161535233114,-16.4928030941281,4.));
#31820=CARTESIAN_POINT('Ctrl Pts',(6.54722690864904,-16.1499910948348,12.));
#31821=CARTESIAN_POINT('Ctrl Pts',(3.794997335032,-16.3497818234513,-12.));
#31822=CARTESIAN_POINT('Ctrl Pts',(4.65106990943784,-16.1510762276491,-3.99999999999999));
#31823=CARTESIAN_POINT('Ctrl Pts',(5.49149549661271,-15.8849989557599,3.99999999999999));
#31824=CARTESIAN_POINT('Ctrl Pts',(6.30594399347681,-15.5548205003623,12.));
#31825=CARTESIAN_POINT('Ctrl Pts',(3.64979020648557,-15.7241938028674,-12.));
#31826=CARTESIAN_POINT('Ctrl Pts',(4.47310706873074,-15.5330912345367,-4.00000000000001));
#31827=CARTESIAN_POINT('Ctrl Pts',(5.28137564089428,-15.2771948173917,4.00000000000001));
#31828=CARTESIAN_POINT('Ctrl Pts',(6.06466107830459,-14.9596499058898,12.));
#31829=CARTESIAN_POINT('Ctrl Pts',(3.50458307793915,-15.0986057822834,-12.));
#31830=CARTESIAN_POINT('Ctrl Pts',(4.29514422802365,-14.9151062414243,-4.));
#31831=CARTESIAN_POINT('Ctrl Pts',(5.07125578517585,-14.6693906790234,4.));
#31832=CARTESIAN_POINT('Ctrl Pts',(5.82337816313236,-14.3644793114172,12.));
#31833=CARTESIAN_POINT('Ctrl Pts',(0.902337623732299,-17.403280701153,-10.5713320279724));
#31834=CARTESIAN_POINT('Ctrl Pts',(1.70508374321692,-17.361659351802,-3.52377734265747));
#31835=CARTESIAN_POINT('Ctrl Pts',(2.50494062688806,-17.2644084310805,3.52377734265748));
#31836=CARTESIAN_POINT('Ctrl Pts',(3.29427214377962,-17.1124563810414,10.5713320279724));
#31837=CARTESIAN_POINT('Ctrl Pts',(0.902360423042107,-17.4036636612004,
-10.5713320279724));
#31838=CARTESIAN_POINT('Ctrl Pts',(1.70512420699455,-17.3620412602053,-3.52377734265748));
#31839=CARTESIAN_POINT('Ctrl Pts',(2.50499868214735,-17.264788063709,3.52377734265749));
#31840=CARTESIAN_POINT('Ctrl Pts',(3.29434754959081,-17.1128325354912,10.5713320279724));
#31841=CARTESIAN_POINT('Ctrl Pts',(0.902383222354776,-17.404046621281,-10.5713320279724));
#31842=CARTESIAN_POINT('Ctrl Pts',(1.70516467077662,-17.3624231686417,-3.52377734265746));
#31843=CARTESIAN_POINT('Ctrl Pts',(2.50505673741252,-17.2651676963705,3.52377734265747));
#31844=CARTESIAN_POINT('Ctrl Pts',(3.29442295540941,-17.1132086899734,10.5713320279724));
#31845=CARTESIAN_POINT('Ctrl Pts',(0.902406021667647,-17.4044295813643,
-10.5713320279724));
#31846=CARTESIAN_POINT('Ctrl Pts',(1.70520513455892,-17.3628050770807,-3.52377734265747));
#31847=CARTESIAN_POINT('Ctrl Pts',(2.50511479267822,-17.2655473290345,3.52377734265748));
#31848=CARTESIAN_POINT('Ctrl Pts',(3.29449836122858,-17.1135848444583,10.5713320279724));
#31849=CARTESIAN_POINT('Ctrl Pts',(0.902337477632692,-17.4032793300502,
-10.5713320134286));
#31850=CARTESIAN_POINT('Ctrl Pts',(1.70508221483526,-17.361645257149,-3.52377733780954));
#31851=CARTESIAN_POINT('Ctrl Pts',(2.50493873335086,-17.2643943808229,3.52377733780954));
#31852=CARTESIAN_POINT('Ctrl Pts',(3.29427195715649,-17.1124550148594,10.5713320134286));
#31853=CARTESIAN_POINT('Ctrl Pts',(0.657803910601427,-15.4860354233799,
-12.));
#31854=CARTESIAN_POINT('Ctrl Pts',(1.46865082925679,-15.4515928911625,-4.));
#31855=CARTESIAN_POINT('Ctrl Pts',(2.2767788714881,-15.3533363183005,4.));
#31856=CARTESIAN_POINT('Ctrl Pts',(3.07225491994942,-15.1924734268593,12.));
#31857=CARTESIAN_POINT('Ctrl Pts',(0.685059026225968,-16.1276760084048,
-12.));
#31858=CARTESIAN_POINT('Ctrl Pts',(1.52950216735065,-16.0918064016704,-4.00000000000001));
#31859=CARTESIAN_POINT('Ctrl Pts',(2.37111377949615,-15.9894787155008,4.));
#31860=CARTESIAN_POINT('Ctrl Pts',(3.19954918153982,-15.8219507121087,12.));
#31861=CARTESIAN_POINT('Ctrl Pts',(0.712314141850509,-16.7693165934297,
-12.));
#31862=CARTESIAN_POINT('Ctrl Pts',(1.59035350544451,-16.7320199121783,-4.));
#31863=CARTESIAN_POINT('Ctrl Pts',(2.4654486875042,-16.6256211127012,3.99999999999999));
#31864=CARTESIAN_POINT('Ctrl Pts',(3.32684344313023,-16.4514279973581,12.));
#31865=CARTESIAN_POINT('Ctrl Pts',(0.739569257475051,-17.4109571784546,
-12.));
#31866=CARTESIAN_POINT('Ctrl Pts',(1.65120484353838,-17.3722334226862,-4.));
#31867=CARTESIAN_POINT('Ctrl Pts',(2.55978359551225,-17.2617635099015,4.));
#31868=CARTESIAN_POINT('Ctrl Pts',(3.45413770472063,-17.0809052826075,12.));
#31869=CARTESIAN_POINT('Ctrl Pts',(0.657803912377566,-15.4860354448028,
-11.9999999914697));
#31870=CARTESIAN_POINT('Ctrl Pts',(0.860473336502315,-15.4774266129281,
-10.0004173920443));
#31871=CARTESIAN_POINT('Ctrl Pts',(1.06300270545654,-15.4648379845811,-8.00054577305927));
#31872=CARTESIAN_POINT('Ctrl Pts',(1.26527523936852,-15.4482710543491,-5.99999995642121));
#31873=CARTESIAN_POINT('Ctrl Pts',(1.46749908351692,-15.4317081120036,-3.99993569850461));
#31874=CARTESIAN_POINT('Ctrl Pts',(1.66937848149492,-15.4111759584542,-2.00006422723887));
#31875=CARTESIAN_POINT('Ctrl Pts',(1.87079645983396,-15.3866864725929,2.22030256658689E-15));
#31876=CARTESIAN_POINT('Ctrl Pts',(2.072214438173,-15.3621969867316,2.00006422723887));
#31877=CARTESIAN_POINT('Ctrl Pts',(2.2731321034333,-15.3337548974327,3.9999356985046));
#31878=CARTESIAN_POINT('Ctrl Pts',(2.47343304368529,-15.301376702062,5.99999995642121));
#31879=CARTESIAN_POINT('Ctrl Pts',(2.67381106285918,-15.2689860470573,8.00083387021915));
#31880=CARTESIAN_POINT('Ctrl Pts',(2.87345607543091,-15.2326749819658,10.0007056240913));
#31881=CARTESIAN_POINT('Ctrl Pts',(3.07225491560408,-15.192473427738,11.9999999562994));
#31882=CARTESIAN_POINT('Origin',(2.22044604925031E-15,-4.16333634234434E-16,
-6.));
#31883=CARTESIAN_POINT('Origin',(2.22044604925031E-15,-4.16333634234434E-16,
-6.));
#31884=CARTESIAN_POINT('Ctrl Pts',(0.559244210621348,-15.4899078445247,
11.9999999562994));
#31885=CARTESIAN_POINT('Ctrl Pts',(0.356553333306836,-15.4972257725099,
10.0007056240913));
#31886=CARTESIAN_POINT('Ctrl Pts',(0.15366060748641,-15.5005673742223,8.00083387021916));
#31887=CARTESIAN_POINT('Ctrl Pts',(-0.0493174405869348,-15.499921541416,
5.99999995642122));
#31888=CARTESIAN_POINT('Ctrl Pts',(-0.252217409591645,-15.4992759570407,
3.99993569850462));
#31889=CARTESIAN_POINT('Ctrl Pts',(-0.455085414960348,-15.4946463722799,
2.00006422723889));
#31890=CARTESIAN_POINT('Ctrl Pts',(-0.657803911807544,-15.4860354517744,
8.88178419700125E-15));
#31891=CARTESIAN_POINT('Ctrl Pts',(-0.86052240865474,-15.4774245312688,
-2.00006422723887));
#31892=CARTESIAN_POINT('Ctrl Pts',(-1.06305225241292,-15.4648339377712,
-3.99993569850461));
#31893=CARTESIAN_POINT('Ctrl Pts',(-1.26527609564326,-15.4482709842168,
-5.99999995642121));
#31894=CARTESIAN_POINT('Ctrl Pts',(-1.46754862863696,-15.4317040427731,
-8.00054577305927));
#31895=CARTESIAN_POINT('Ctrl Pts',(-1.66942723837632,-15.4111700275214,
-10.0004173920443));
#31896=CARTESIAN_POINT('Ctrl Pts',(-1.87079645813715,-15.3866864658071,
-11.9999999914697));
#31897=CARTESIAN_POINT('Ctrl Pts',(-4.6784025743345,-14.7770954003634,-12.));
#31898=CARTESIAN_POINT('Ctrl Pts',(-3.90467566848155,-15.0220559863311,
-4.));
#31899=CARTESIAN_POINT('Ctrl Pts',(-3.11167798341368,-15.2061210786984,
4.));
#31900=CARTESIAN_POINT('Ctrl Pts',(-2.30915666147617,-15.3270282387598,
12.));
#31901=CARTESIAN_POINT('Ctrl Pts',(-4.87224514815724,-15.3893621218603,
-12.));
#31902=CARTESIAN_POINT('Ctrl Pts',(-4.06646003173275,-15.6444722812593,
-4.));
#31903=CARTESIAN_POINT('Ctrl Pts',(-3.240605680342,-15.8361638338742,4.));
#31904=CARTESIAN_POINT('Ctrl Pts',(-2.40483309451253,-15.9620806002547,
12.));
#31905=CARTESIAN_POINT('Ctrl Pts',(-5.06608772197997,-16.0016288433572,
-12.));
#31906=CARTESIAN_POINT('Ctrl Pts',(-4.22824439498395,-16.2668885761874,
-4.00000000000001));
#31907=CARTESIAN_POINT('Ctrl Pts',(-3.36953337727031,-16.4662065890499,
4.00000000000001));
#31908=CARTESIAN_POINT('Ctrl Pts',(-2.50050952754889,-16.5971329617496,
12.));
#31909=CARTESIAN_POINT('Ctrl Pts',(-5.2599302958027,-16.6138955648541,-12.));
#31910=CARTESIAN_POINT('Ctrl Pts',(-4.39002875823514,-16.8893048711156,
-4.));
#31911=CARTESIAN_POINT('Ctrl Pts',(-3.49846107419862,-17.0962493442257,
4.));
#31912=CARTESIAN_POINT('Ctrl Pts',(-2.59618596058525,-17.2321853232445,
12.));
#31913=CARTESIAN_POINT('Ctrl Pts',(-4.67840257999253,-14.7770954211018,
-11.9999999914697));
#31914=CARTESIAN_POINT('Ctrl Pts',(-4.48501122377192,-14.8383227908024,
-10.0004173920443));
#31915=CARTESIAN_POINT('Ctrl Pts',(-4.29039030580172,-14.8957624734364,
-8.00054577305927));
#31916=CARTESIAN_POINT('Ctrl Pts',(-4.09465007444454,-14.9493759323877,
-5.99999995642121));
#31917=CARTESIAN_POINT('Ctrl Pts',(-3.89895696043642,-15.0029764858466,
-3.99993569850461));
#31918=CARTESIAN_POINT('Ctrl Pts',(-3.70222996976806,-15.0527293932983,
-2.00006422723888));
#31919=CARTESIAN_POINT('Ctrl Pts',(-3.50458308436497,-15.0986058099674,
-6.66133814775094E-15));
#31920=CARTESIAN_POINT('Ctrl Pts',(-3.30693619896188,-15.1444822266366,
2.00006422723887));
#31921=CARTESIAN_POINT('Ctrl Pts',(-3.10840758407278,-15.1864732938717,
3.99993569850461));
#31922=CARTESIAN_POINT('Ctrl Pts',(-2.90911227356018,-15.2245546989007,
5.99999995642122));
#31923=CARTESIAN_POINT('Ctrl Pts',(-2.70974027110768,-15.2626507582476,
8.00083387021915));
#31924=CARTESIAN_POINT('Ctrl Pts',(-2.50971621033041,-15.2968121341423,
10.0007056240913));
#31925=CARTESIAN_POINT('Ctrl Pts',(-2.30915666586,-15.3270282380994,11.9999999562994));
#31926=CARTESIAN_POINT('Ctrl Pts',(-5.10435222255114,-16.6623507570641,
-10.5713320220547));
#31927=CARTESIAN_POINT('Ctrl Pts',(-4.33577922443239,-16.8977823962929,
-3.52377734068488));
#31928=CARTESIAN_POINT('Ctrl Pts',(-3.55089819699268,-17.0799635066964,
3.52377734068489));
#31929=CARTESIAN_POINT('Ctrl Pts',(-2.7572012668629,-17.2071550680903,10.5713320220547));
#31930=CARTESIAN_POINT('Ctrl Pts',(-2.1033373682508,-17.299259072917,-12.));
#31931=CARTESIAN_POINT('Ctrl Pts',(-1.19755028131709,-17.4093895599857,
-4.));
#31932=CARTESIAN_POINT('Ctrl Pts',(-0.283105004950502,-17.4482326636193,
4.));
#31933=CARTESIAN_POINT('Ctrl Pts',(0.628758543704759,-17.4153109432562,
12.));
#31934=CARTESIAN_POINT('Ctrl Pts',(-2.02582373096845,-16.6617348634049,
-12.));
#31935=CARTESIAN_POINT('Ctrl Pts',(-1.15341733358622,-16.7678067459162,
-4.));
#31936=CARTESIAN_POINT('Ctrl Pts',(-0.272671824331076,-16.8052183767432,
4.));
#31937=CARTESIAN_POINT('Ctrl Pts',(0.605587100820427,-16.7735099102924,
12.));
#31938=CARTESIAN_POINT('Ctrl Pts',(-1.94831009368611,-16.0242106538928,
-12.));
#31939=CARTESIAN_POINT('Ctrl Pts',(-1.10928438585536,-16.1262239318468,
-4.));
#31940=CARTESIAN_POINT('Ctrl Pts',(-0.262238643711649,-16.162204089867,
4.));
#31941=CARTESIAN_POINT('Ctrl Pts',(0.582415657936094,-16.1317088773286,
12.));
#31942=CARTESIAN_POINT('Ctrl Pts',(-1.87079645640376,-15.3866864443807,
-12.));
#31943=CARTESIAN_POINT('Ctrl Pts',(-1.0651514381245,-15.4846411177773,-4.));
#31944=CARTESIAN_POINT('Ctrl Pts',(-0.251805463092223,-15.5191898029909,
4.));
#31945=CARTESIAN_POINT('Ctrl Pts',(0.559244215051762,-15.4899078443647,
12.));
#31946=CARTESIAN_POINT('Ctrl Pts',(-5.10435255326646,-16.6623520957364,
-10.5713320279724));
#31947=CARTESIAN_POINT('Ctrl Pts',(-4.33578260855181,-16.8977961637243,
-3.52377734265748));
#31948=CARTESIAN_POINT('Ctrl Pts',(-3.5509012234375,-17.0799773571509,3.52377734265748));
#31949=CARTESIAN_POINT('Ctrl Pts',(-2.75720155972776,-17.2071564155546,
10.5713320279724));
#31950=CARTESIAN_POINT('Ctrl Pts',(-5.10446210897357,-16.6627197582901,
-10.5713320279724));
#31951=CARTESIAN_POINT('Ctrl Pts',(-4.33587520540538,-16.8981688796597,
-3.52377734265747));
#31952=CARTESIAN_POINT('Ctrl Pts',(-3.55097651134477,-17.0803539511987,
3.52377734265748));
#31953=CARTESIAN_POINT('Ctrl Pts',(-2.75725935384223,-17.2075356754217,
10.5713320279724));
#31954=CARTESIAN_POINT('Ctrl Pts',(-5.10457166468936,-16.6630874208762,
-10.5713320279724));
#31955=CARTESIAN_POINT('Ctrl Pts',(-4.33596780226611,-16.8985415956278,
-3.52377734265748));
#31956=CARTESIAN_POINT('Ctrl Pts',(-3.55105179925777,-17.0807305452794,
3.52377734265749));
#31957=CARTESIAN_POINT('Ctrl Pts',(-2.75731714796086,-17.2079149353218,
10.5713320279724));
#31958=CARTESIAN_POINT('Ctrl Pts',(-5.10468122040586,-16.6634550834647,
-10.5713320279724));
#31959=CARTESIAN_POINT('Ctrl Pts',(-4.33606039912753,-16.8989143115984,
-3.52377734265748));
#31960=CARTESIAN_POINT('Ctrl Pts',(-3.55112708717115,-17.0811071393627,
3.52377734265748));
#31961=CARTESIAN_POINT('Ctrl Pts',(-2.75737494207985,-17.2082941952246,
10.5713320279724));
#31962=CARTESIAN_POINT('Ctrl Pts',(-7.89318567151549,-15.5366023477324,
-12.));
#31963=CARTESIAN_POINT('Ctrl Pts',(-7.07969107489246,-15.94988858305,-4.));
#31964=CARTESIAN_POINT('Ctrl Pts',(-6.23367872045025,-16.2991478653893,
4.));
#31965=CARTESIAN_POINT('Ctrl Pts',(-5.36554738109814,-16.5800872693051,
12.));
#31966=CARTESIAN_POINT('Ctrl Pts',(-7.60230055704008,-14.9640367778145,
-12.));
#31967=CARTESIAN_POINT('Ctrl Pts',(-6.81878542355292,-15.3620923041542,
-3.99999999999999));
#31968=CARTESIAN_POINT('Ctrl Pts',(-6.00395089905301,-15.6984804428827,
3.99999999999999));
#31969=CARTESIAN_POINT('Ctrl Pts',(-5.16781253370865,-15.9690664743998,
12.));
#31970=CARTESIAN_POINT('Ctrl Pts',(-7.31141544256466,-14.3914712078966,
-12.));
#31971=CARTESIAN_POINT('Ctrl Pts',(-6.55787977221338,-14.7742960252583,
-4.00000000000001));
#31972=CARTESIAN_POINT('Ctrl Pts',(-5.77422307765577,-15.0978130203761,
4.00000000000001));
#31973=CARTESIAN_POINT('Ctrl Pts',(-4.97007768631916,-15.3580456794946,
12.));
#31974=CARTESIAN_POINT('Ctrl Pts',(-7.02053032808925,-13.8189056379787,
-12.));
#31975=CARTESIAN_POINT('Ctrl Pts',(-6.29697412087384,-14.1864997463625,
-4.));
#31976=CARTESIAN_POINT('Ctrl Pts',(-5.54449525625854,-14.4971455978694,
4.));
#31977=CARTESIAN_POINT('Ctrl Pts',(-4.77234283892968,-14.7470248845893,
12.));
#31978=CARTESIAN_POINT('Ctrl Pts',(-4.77234284314764,-14.7470248832244,
11.9999999562994));
#31979=CARTESIAN_POINT('Ctrl Pts',(-4.96531284363905,-14.6845771232416,
10.0007056240913));
#31980=CARTESIAN_POINT('Ctrl Pts',(-5.15711253600029,-14.6183238025476,
8.00083387021916));
#31981=CARTESIAN_POINT('Ctrl Pts',(-5.34762862212736,-14.5482943371312,
5.99999995642122));
#31982=CARTESIAN_POINT('Ctrl Pts',(-5.53807142289819,-14.4782918097778,
3.99993569850462));
#31983=CARTESIAN_POINT('Ctrl Pts',(-5.72712157929328,-14.4045564788684,
2.00006422723887));
#31984=CARTESIAN_POINT('Ctrl Pts',(-5.91466954661191,-14.3271310510647,
-2.22044604925031E-15));
#31985=CARTESIAN_POINT('Ctrl Pts',(-6.10221751393055,-14.249705623261,-2.00006422723887));
#31986=CARTESIAN_POINT('Ctrl Pts',(-6.28822707700645,-14.1686050492701,
-3.99993569850461));
#31987=CARTESIAN_POINT('Ctrl Pts',(-6.47259046648839,-14.0838763361911,
-5.9999999564212));
#31988=CARTESIAN_POINT('Ctrl Pts',(-6.6569982454432,-13.9991272228421,-8.00054577305927));
#31989=CARTESIAN_POINT('Ctrl Pts',(-6.83967903847032,-13.9107850091975,
-10.0004173920443));
#31990=CARTESIAN_POINT('Ctrl Pts',(-7.02053033704636,-13.8189056575201,
-11.9999999914697));
#31991=CARTESIAN_POINT('Ctrl Pts',(-9.4503246629373,-12.2858195853618,-12.));
#31992=CARTESIAN_POINT('Ctrl Pts',(-8.8070406537256,-12.7806374276138,-4.));
#31993=CARTESIAN_POINT('Ctrl Pts',(-8.12482055003974,-13.2248232185595,
4.));
#31994=CARTESIAN_POINT('Ctrl Pts',(-7.41204987000498,-13.6129172422203,
12.));
#31995=CARTESIAN_POINT('Ctrl Pts',(-9.84188465099258,-12.7948640406237,
-12.));
#31996=CARTESIAN_POINT('Ctrl Pts',(-9.17194713643085,-13.3101839159077,
-3.99999999999999));
#31997=CARTESIAN_POINT('Ctrl Pts',(-8.4614602688847,-13.7727738769957,3.99999999999998));
#31998=CARTESIAN_POINT('Ctrl Pts',(-7.71915700781015,-14.1769479927898,
12.));
#31999=CARTESIAN_POINT('Ctrl Pts',(-10.2334446390479,-13.3039084958857,
-12.));
#32000=CARTESIAN_POINT('Ctrl Pts',(-9.53685361913611,-13.8397304042016,
-4.00000000000001));
#32001=CARTESIAN_POINT('Ctrl Pts',(-8.79809998772967,-14.3207245354319,
4.00000000000001));
#32002=CARTESIAN_POINT('Ctrl Pts',(-8.02626414561533,-14.7409787433592,
12.));
#32003=CARTESIAN_POINT('Ctrl Pts',(-10.6250046271031,-13.8129529511477,
-12.));
#32004=CARTESIAN_POINT('Ctrl Pts',(-9.90176010184136,-14.3692768924954,
-4.));
#32005=CARTESIAN_POINT('Ctrl Pts',(-9.13473970657464,-14.8686751938681,
4.));
#32006=CARTESIAN_POINT('Ctrl Pts',(-8.3333712834205,-15.3050094939286,12.));
#32007=CARTESIAN_POINT('Ctrl Pts',(-9.45032467534708,-12.2858196029144,
-11.9999999914697));
#32008=CARTESIAN_POINT('Ctrl Pts',(-9.28953723874319,-12.4094982497846,
-10.0004173920443));
#32009=CARTESIAN_POINT('Ctrl Pts',(-9.12629892676312,-12.5300381699545,
-8.00054577305927));
#32010=CARTESIAN_POINT('Ctrl Pts',(-8.96070015868055,-12.6473654436892,
-5.99999995642121));
#32011=CARTESIAN_POINT('Ctrl Pts',(-8.79514125248487,-12.7646644751455,
-3.99993569850461));
#32012=CARTESIAN_POINT('Ctrl Pts',(-8.62729484758191,-12.8787015086849,
-2.00006422723887));
#32013=CARTESIAN_POINT('Ctrl Pts',(-8.45725818645174,-12.9894104549704,
4.4407486176685E-15));
#32014=CARTESIAN_POINT('Ctrl Pts',(-8.28722152532158,-13.1001194012559,
2.00006422723889));
#32015=CARTESIAN_POINT('Ctrl Pts',(-8.11502744172963,-13.2074788825944,
3.9999356985046));
#32016=CARTESIAN_POINT('Ctrl Pts',(-7.94077571668976,-13.311426708555,5.99999995642122));
#32017=CARTESIAN_POINT('Ctrl Pts',(-7.76645693687179,-13.4154145352581,
8.00083387021915));
#32018=CARTESIAN_POINT('Ctrl Pts',(-7.59017968165941,-13.5159279860378,
10.0007056240913));
#32019=CARTESIAN_POINT('Ctrl Pts',(-7.41204987389855,-13.6129172401003,
11.9999999562994));
#32020=CARTESIAN_POINT('Ctrl Pts',(-10.4953817114971,-13.9116967726179,
-10.5713320220547));
#32021=CARTESIAN_POINT('Ctrl Pts',(-9.85368169962205,-14.3957975936737,
-3.52377734068489));
#32022=CARTESIAN_POINT('Ctrl Pts',(-9.17844439943352,-14.8354369602649,
3.52377734068489));
#32023=CARTESIAN_POINT('Ctrl Pts',(-8.47611532710788,-15.2264182697331,
10.5713320220547));
#32024=CARTESIAN_POINT('Ctrl Pts',(-10.4953824801207,-13.9116979174471,
-10.5713320279724));
#32025=CARTESIAN_POINT('Ctrl Pts',(-9.85368958839295,-14.3958093733904,
-3.52377734265748));
#32026=CARTESIAN_POINT('Ctrl Pts',(-9.17845198049581,-14.8354489403297,
3.52377734265748));
#32027=CARTESIAN_POINT('Ctrl Pts',(-8.47611606317077,-15.2264194357697,
10.5713320279724));
#32028=CARTESIAN_POINT('Ctrl Pts',(-10.4956111768096,-13.9120059369772,
-10.5713320279724));
#32029=CARTESIAN_POINT('Ctrl Pts',(-9.85390407733061,-14.3961279418154,
-3.52377734265748));
#32030=CARTESIAN_POINT('Ctrl Pts',(-9.17865153073689,-14.8357770729966,
3.52377734265749));
#32031=CARTESIAN_POINT('Ctrl Pts',(-8.47630008638775,-15.2267560567168,
10.5713320279724));
#32032=CARTESIAN_POINT('Ctrl Pts',(-10.4958398735176,-13.9123139565346,
-10.5713320279724));
#32033=CARTESIAN_POINT('Ctrl Pts',(-9.85411856628614,-14.3964465102686,
-3.52377734265747));
#32034=CARTESIAN_POINT('Ctrl Pts',(-9.17885108099462,-14.8361052056924,
3.52377734265747));
#32035=CARTESIAN_POINT('Ctrl Pts',(-8.47648410961995,-15.2270926776936,
10.5713320279724));
#32036=CARTESIAN_POINT('Ctrl Pts',(-10.4960685702272,-13.9126219760941,
-10.5713320279724));
#32037=CARTESIAN_POINT('Ctrl Pts',(-9.85433305524321,-14.396765078724,-3.52377734265748));
#32038=CARTESIAN_POINT('Ctrl Pts',(-9.17905063125361,-14.8364333383906,
3.52377734265748));
#32039=CARTESIAN_POINT('Ctrl Pts',(-8.4766681328534,-15.2274292986728,10.5713320279724));
#32040=CARTESIAN_POINT('Origin',(2.22044604925031E-15,-4.16333634234434E-16,
-6.));
#32041=CARTESIAN_POINT('Ctrl Pts',(-9.52831491775384,-12.2254330780995,
11.9999999562994));
#32042=CARTESIAN_POINT('Ctrl Pts',(-9.68828901142903,-12.1007517516335,
10.0007056240913));
#32043=CARTESIAN_POINT('Ctrl Pts',(-9.84586179677031,-11.9728946368036,
8.00083387021915));
#32044=CARTESIAN_POINT('Ctrl Pts',(-10.0009368692462,-11.8419281258312,
5.99999995642122));
#32045=CARTESIAN_POINT('Ctrl Pts',(-10.1559522893738,-11.7110119934259,
3.99993569850463));
#32046=CARTESIAN_POINT('Ctrl Pts',(-10.3083823578508,-11.577064485493,2.00006422723886));
#32047=CARTESIAN_POINT('Ctrl Pts',(-10.4581387428691,-11.440163199662,-2.22058953008229E-15));
#32048=CARTESIAN_POINT('Ctrl Pts',(-10.6078951278873,-11.3032619138309,
-2.00006422723889));
#32049=CARTESIAN_POINT('Ctrl Pts',(-10.7549489117653,-11.1634332854871,
-3.9999356985046));
#32050=CARTESIAN_POINT('Ctrl Pts',(-10.8992149018134,-11.0207583461433,
-5.99999995642121));
#32051=CARTESIAN_POINT('Ctrl Pts',(-11.0435156270184,-10.8780490547226,
-8.00054577305927));
#32052=CARTESIAN_POINT('Ctrl Pts',(-11.1849646036129,-10.732554017443,-10.0004173920443));
#32053=CARTESIAN_POINT('Ctrl Pts',(-11.323484645315,-10.5843608816095,-11.9999999914697));
#32054=CARTESIAN_POINT('Ctrl Pts',(-12.7309992917815,-11.9000020835813,
-12.));
#32055=CARTESIAN_POINT('Ctrl Pts',(-12.1079166397235,-12.5665956477133,
-4.));
#32056=CARTESIAN_POINT('Ctrl Pts',(-11.432378782964,-13.1841452847902,4.));
#32057=CARTESIAN_POINT('Ctrl Pts',(-10.7126891046949,-13.7450603746485,
12.));
#32058=CARTESIAN_POINT('Ctrl Pts',(-12.2618277379259,-11.4614550111576,
-12.));
#32059=CARTESIAN_POINT('Ctrl Pts',(-11.6617073568841,-12.1034828101751,
-4.00000000000001));
#32060=CARTESIAN_POINT('Ctrl Pts',(-11.011064886471,-12.6982740827144,4.00000000000001));
#32061=CARTESIAN_POINT('Ctrl Pts',(-10.3178977078823,-13.238517943374,12.));
#32062=CARTESIAN_POINT('Ctrl Pts',(-11.7926561840702,-11.0229079387338,
-12.));
#32063=CARTESIAN_POINT('Ctrl Pts',(-11.2154980740448,-11.6403699726369,
-4.));
#32064=CARTESIAN_POINT('Ctrl Pts',(-10.589750989978,-12.2124028806386,3.99999999999999));
#32065=CARTESIAN_POINT('Ctrl Pts',(-9.92310631106972,-12.7319755120994,
12.));
#32066=CARTESIAN_POINT('Ctrl Pts',(-11.3234846302145,-10.5843608663101,
-12.));
#32067=CARTESIAN_POINT('Ctrl Pts',(-10.7692887912054,-11.1772571350987,
-4.));
#32068=CARTESIAN_POINT('Ctrl Pts',(-10.168437093485,-11.7265316785628,4.));
#32069=CARTESIAN_POINT('Ctrl Pts',(-9.52831491425713,-12.2254330808248,
12.));
#32070=CARTESIAN_POINT('Ctrl Pts',(-14.6205143845238,-9.48308765551918,
-10.5713320279724));
#32071=CARTESIAN_POINT('Ctrl Pts',(-14.1830961789038,-10.1574755131067,
-3.52377734265747));
#32072=CARTESIAN_POINT('Ctrl Pts',(-13.6989459691819,-10.801546433397,3.52377734265748));
#32073=CARTESIAN_POINT('Ctrl Pts',(-13.1726858752452,-11.4091515540133,
10.5713320279724));
#32074=CARTESIAN_POINT('Ctrl Pts',(-14.6208346379921,-9.48329888032005,
-10.5713320279724));
#32075=CARTESIAN_POINT('Ctrl Pts',(-14.1834066893878,-10.1577015099631,
-3.52377734265748));
#32076=CARTESIAN_POINT('Ctrl Pts',(-13.6992457130466,-10.8017865270358,
3.52377734265748));
#32077=CARTESIAN_POINT('Ctrl Pts',(-13.172973931643,-11.4094049345811,10.5713320279724));
#32078=CARTESIAN_POINT('Ctrl Pts',(-14.6211548914877,-9.48351010514003,
-10.5713320279724));
#32079=CARTESIAN_POINT('Ctrl Pts',(-14.1837171998983,-10.1579275068399,
-3.52377734265746));
#32080=CARTESIAN_POINT('Ctrl Pts',(-13.6995454569368,-10.8020266206961,
3.52377734265747));
#32081=CARTESIAN_POINT('Ctrl Pts',(-13.1732619880652,-11.4096583151716,
10.5713320279724));
#32082=CARTESIAN_POINT('Ctrl Pts',(-14.6214751449855,-9.4837213299615,-10.5713320279724));
#32083=CARTESIAN_POINT('Ctrl Pts',(-14.1840277104109,-10.1581535037183,
-3.52377734265747));
#32084=CARTESIAN_POINT('Ctrl Pts',(-13.6998452008291,-10.8022667143581,
3.52377734265748));
#32085=CARTESIAN_POINT('Ctrl Pts',(-13.1735500444894,-11.4099116957638,
10.5713320279724));
#32086=CARTESIAN_POINT('Ctrl Pts',(-14.6205132701638,-9.4830868434418,-10.5713320134286));
#32087=CARTESIAN_POINT('Ctrl Pts',(-14.1830847367669,-10.1574671421628,
-3.52377733780954));
#32088=CARTESIAN_POINT('Ctrl Pts',(-13.6989347480705,-10.8015377684169,
3.52377733780955));
#32089=CARTESIAN_POINT('Ctrl Pts',(-13.1726847854084,-11.4091507093019,
10.5713320134286));
#32090=CARTESIAN_POINT('Ctrl Pts',(-13.082398125252,-8.31269260897955,-12.));
#32091=CARTESIAN_POINT('Ctrl Pts',(-12.6471465580533,-8.99768537300669,
-4.));
#32092=CARTESIAN_POINT('Ctrl Pts',(-12.1579898487504,-9.64841650065859,
4.));
#32093=CARTESIAN_POINT('Ctrl Pts',(-11.6209404740055,-10.2568875210076,
12.));
#32094=CARTESIAN_POINT('Ctrl Pts',(-13.6244476141704,-8.65711652400593,
-12.));
#32095=CARTESIAN_POINT('Ctrl Pts',(-13.1711620529523,-9.37049093290421,
-3.99999999999999));
#32096=CARTESIAN_POINT('Ctrl Pts',(-12.6617378711462,-10.0481841260574,
3.99999999999998));
#32097=CARTESIAN_POINT('Ctrl Pts',(-12.1024366633415,-10.6818662279256,
12.));
#32098=CARTESIAN_POINT('Ctrl Pts',(-14.1664971030888,-9.00154043903231,
-12.));
#32099=CARTESIAN_POINT('Ctrl Pts',(-13.6951775478512,-9.74329649280173,
-4.00000000000001));
#32100=CARTESIAN_POINT('Ctrl Pts',(-13.165485893542,-10.4479517514562,4.00000000000001));
#32101=CARTESIAN_POINT('Ctrl Pts',(-12.5839328526776,-11.1068449348435,
12.));
#32102=CARTESIAN_POINT('Ctrl Pts',(-14.7085465920072,-9.34596435405869,
-12.));
#32103=CARTESIAN_POINT('Ctrl Pts',(-14.2191930427501,-10.1161020526992,
-4.));
#32104=CARTESIAN_POINT('Ctrl Pts',(-13.6692339159378,-10.847719376855,4.));
#32105=CARTESIAN_POINT('Ctrl Pts',(-13.0654290420136,-11.5318236417615,
12.));
#32106=CARTESIAN_POINT('Ctrl Pts',(-13.0823981429167,-8.31269262122918,
-11.9999999914697));
#32107=CARTESIAN_POINT('Ctrl Pts',(-12.9736079637539,-8.48390507515421,
-10.0004173920443));
#32108=CARTESIAN_POINT('Ctrl Pts',(-12.8614412073296,-8.65300633950755,
-8.00054577305927));
#32109=CARTESIAN_POINT('Ctrl Pts',(-12.7459575579299,-8.81989602724713,
-5.9999999564212));
#32110=CARTESIAN_POINT('Ctrl Pts',(-12.630501707023,-8.98674554235783,-3.99993569850462));
#32111=CARTESIAN_POINT('Ctrl Pts',(-12.5117806414659,-9.1513121527328,-2.00006422723887));
#32112=CARTESIAN_POINT('Ctrl Pts',(-12.3898631354148,-9.31350049582264,
-6.66148162858282E-15));
#32113=CARTESIAN_POINT('Ctrl Pts',(-12.2679456293637,-9.47568883891247,
2.00006422723888));
#32114=CARTESIAN_POINT('Ctrl Pts',(-12.1428552248642,-9.63546759644758,
3.99993569850459));
#32115=CARTESIAN_POINT('Ctrl Pts',(-12.0146644150184,-9.79274420142234,
5.99999995642121));
#32116=CARTESIAN_POINT('Ctrl Pts',(-11.8864242753522,-9.95008132888459,
8.00083387021915));
#32117=CARTESIAN_POINT('Ctrl Pts',(-11.7551554642586,-10.1048234489648,
10.0007056240913));
#32118=CARTESIAN_POINT('Ctrl Pts',(-11.6209404769392,-10.2568875176838,
11.9999999562994));
#32119=CARTESIAN_POINT('Origin',(2.22044604925031E-15,-4.16333634234434E-16,
-6.));
#32120=CARTESIAN_POINT('Origin',(2.22044604925031E-15,-4.16333634234434E-16,
-6.));
#32121=CARTESIAN_POINT('Ctrl Pts',(-13.1350315903275,-8.22927361557979,
11.9999999562994));
#32122=CARTESIAN_POINT('Ctrl Pts',(-13.2427145405231,-8.05739713070269,
10.0007056240913));
#32123=CARTESIAN_POINT('Ctrl Pts',(-13.3470548154056,-7.88335767675537,
8.00083387021915));
#32124=CARTESIAN_POINT('Ctrl Pts',(-13.4479845318255,-7.70725061431012,
5.99999995642121));
#32125=CARTESIAN_POINT('Ctrl Pts',(-13.5488754238585,-7.53121129453728,
3.9999356985046));
#32126=CARTESIAN_POINT('Ctrl Pts',(-13.646300088531,-7.35320765589251,2.00006422723887));
#32127=CARTESIAN_POINT('Ctrl Pts',(-13.7402020610468,-7.17334282755303,
-2.22058953191374E-15));
#32128=CARTESIAN_POINT('Ctrl Pts',(-13.8341040335625,-6.99347799921355,
-2.00006422723888));
#32129=CARTESIAN_POINT('Ctrl Pts',(-13.9244651816241,-6.81178671274575,
-3.9999356985046));
#32130=CARTESIAN_POINT('Ctrl Pts',(-14.0112331646994,-6.6283742504801,-5.99999995642121));
#32131=CARTESIAN_POINT('Ctrl Pts',(-14.0980220390429,-6.44491762769787,
-8.00054577305927));
#32132=CARTESIAN_POINT('Ctrl Pts',(-14.1811783650629,-6.25981861555704,
-10.0004173920443));
#32133=CARTESIAN_POINT('Ctrl Pts',(-14.2606595885237,-6.0731859748468,-11.9999999914697));
#32134=CARTESIAN_POINT('Ctrl Pts',(-15.1365412980281,-3.33693222167749,
-12.));
#32135=CARTESIAN_POINT('Ctrl Pts',(-14.9618199354756,-4.12947967072155,
-4.));
#32136=CARTESIAN_POINT('Ctrl Pts',(-14.7247261388817,-4.90826835731623,
4.));
#32137=CARTESIAN_POINT('Ctrl Pts',(-14.4281741500255,-5.66372578922348,
12.));
#32138=CARTESIAN_POINT('Ctrl Pts',(-15.7637011196476,-3.4751929891605,-12.));
#32139=CARTESIAN_POINT('Ctrl Pts',(-15.5817404402384,-4.300578449675,-4.00000000000001));
#32140=CARTESIAN_POINT('Ctrl Pts',(-15.3348230187984,-5.11163507411277,
4.00000000000001));
#32141=CARTESIAN_POINT('Ctrl Pts',(-15.0259838443316,-5.89839374841795,
12.));
#32142=CARTESIAN_POINT('Ctrl Pts',(-16.3908609412671,-3.61345375664351,
-12.));
#32143=CARTESIAN_POINT('Ctrl Pts',(-16.2016609450012,-4.47167722862845,
-4.));
#32144=CARTESIAN_POINT('Ctrl Pts',(-15.9449198987151,-5.3150017909093,3.99999999999999));
#32145=CARTESIAN_POINT('Ctrl Pts',(-15.6237935386376,-6.13306170761243,
12.));
#32146=CARTESIAN_POINT('Ctrl Pts',(-17.0180207628866,-3.75171452412652,
-12.));
#32147=CARTESIAN_POINT('Ctrl Pts',(-16.8215814497639,-4.64277600758191,
-4.));
#32148=CARTESIAN_POINT('Ctrl Pts',(-16.5550167786318,-5.51836850770584,
4.));
#32149=CARTESIAN_POINT('Ctrl Pts',(-16.2216032329437,-6.36772966680691,
12.));
#32150=CARTESIAN_POINT('Ctrl Pts',(-15.1365413188172,-3.33693222714671,
-11.9999999914697));
#32151=CARTESIAN_POINT('Ctrl Pts',(-15.0928700982745,-3.53502773935638,
-10.0004173920443));
#32152=CARTESIAN_POINT('Ctrl Pts',(-15.0453038636357,-3.73229423974341,
-8.00054577305927));
#32153=CARTESIAN_POINT('Ctrl Pts',(-14.9938643653936,-3.92861698211701,
-5.99999995642121));
#32154=CARTESIAN_POINT('Ctrl Pts',(-14.9424372493419,-4.12489246692319,
-3.99993569850461));
#32155=CARTESIAN_POINT('Ctrl Pts',(-14.8871610357731,-4.32013949217793,
-2.00006422723887));
#32156=CARTESIAN_POINT('Ctrl Pts',(-14.8280677353416,-4.51424492425044,
8.88178419516979E-15));
#32157=CARTESIAN_POINT('Ctrl Pts',(-14.7689744349101,-4.70835035632295,
2.00006422723889));
#32158=CARTESIAN_POINT('Ctrl Pts',(-14.7060754584233,-4.90127671381264,
3.9999356985046));
#32159=CARTESIAN_POINT('Ctrl Pts',(-14.6394072673339,-5.09291221808617,
5.9999999564212));
#32160=CARTESIAN_POINT('Ctrl Pts',(-14.5727134212861,-5.28462146668684,
8.00083387021915));
#32161=CARTESIAN_POINT('Ctrl Pts',(-14.5022860102504,-5.47492807263538,
10.0007056240913));
#32162=CARTESIAN_POINT('Ctrl Pts',(-14.4281741516455,-5.66372578509675,
11.9999999562994));
#32163=CARTESIAN_POINT('Ctrl Pts',(-16.9821951536599,-3.91067668393918,
-10.5713320220547));
#32164=CARTESIAN_POINT('Ctrl Pts',(-16.8017984350274,-4.69399624458723,
-3.52377734068488));
#32165=CARTESIAN_POINT('Ctrl Pts',(-16.5671313910066,-5.46481370850019,
3.52377734068489));
#32166=CARTESIAN_POINT('Ctrl Pts',(-16.2804340492558,-6.21577119359523,
10.5713320220547));
#32167=CARTESIAN_POINT('Ctrl Pts',(-16.03326650792,-6.82808594282421,-12.));
#32168=CARTESIAN_POINT('Ctrl Pts',(-15.6757487639857,-7.66758581406302,
-4.));
#32169=CARTESIAN_POINT('Ctrl Pts',(-15.252165240311,-8.478940205584,4.));
#32170=CARTESIAN_POINT('Ctrl Pts',(-14.7677224198127,-9.25217634332294,
12.));
#32171=CARTESIAN_POINT('Ctrl Pts',(-15.4423975283137,-6.57645261709439,
-12.));
#32172=CARTESIAN_POINT('Ctrl Pts',(-15.0980552745046,-7.38501466090712,
-4.00000000000001));
#32173=CARTESIAN_POINT('Ctrl Pts',(-14.6900819425702,-8.16646846160462,
4.));
#32174=CARTESIAN_POINT('Ctrl Pts',(-14.223492142533,-8.91120876866085,12.));
#32175=CARTESIAN_POINT('Ctrl Pts',(-14.8515285487074,-6.32481929136457,
-12.));
#32176=CARTESIAN_POINT('Ctrl Pts',(-14.5203617850235,-7.10244350775121,
-4.));
#32177=CARTESIAN_POINT('Ctrl Pts',(-14.1279986448294,-7.85399671762523,
3.99999999999999));
#32178=CARTESIAN_POINT('Ctrl Pts',(-13.6792618652534,-8.57024119399876,
12.));
#32179=CARTESIAN_POINT('Ctrl Pts',(-14.2606595691012,-6.07318596563475,
-12.));
#32180=CARTESIAN_POINT('Ctrl Pts',(-13.9426682955425,-6.81987235459531,
-4.));
#32181=CARTESIAN_POINT('Ctrl Pts',(-13.5659153470886,-7.54152497364585,
4.));
#32182=CARTESIAN_POINT('Ctrl Pts',(-13.1350315879738,-8.22927361933666,
12.));
#32183=CARTESIAN_POINT('Ctrl Pts',(-16.9821964783418,-3.91067706686746,
-10.5713320279724));
#32184=CARTESIAN_POINT('Ctrl Pts',(-16.8018120500324,-4.69400019756954,
-3.52377734265748));
#32185=CARTESIAN_POINT('Ctrl Pts',(-16.5671448990744,-5.46481801274933,
3.52377734265749));
#32186=CARTESIAN_POINT('Ctrl Pts',(-16.2804353626266,-6.215771613699,10.5713320279725));
#32187=CARTESIAN_POINT('Ctrl Pts',(-16.9825696612994,-3.91076602011706,
-10.5713320279724));
#32188=CARTESIAN_POINT('Ctrl Pts',(-16.8021811299201,-4.69410636430758,
-3.52377734265748));
#32189=CARTESIAN_POINT('Ctrl Pts',(-16.5675086830329,-5.46494110853041,
3.5237773426575));
#32190=CARTESIAN_POINT('Ctrl Pts',(-16.280792708356,-6.21591119245835,10.5713320279725));
#32191=CARTESIAN_POINT('Ctrl Pts',(-16.9829428442892,-3.91085497337525,
-10.5713320279724));
#32192=CARTESIAN_POINT('Ctrl Pts',(-16.8025502098397,-4.69421253105573,
-3.52377734265747));
#32193=CARTESIAN_POINT('Ctrl Pts',(-16.5678724670228,-5.465064204323,3.52377734265748));
#32194=CARTESIAN_POINT('Ctrl Pts',(-16.2811500541162,-6.21605077123067,
10.5713320279725));
#32195=CARTESIAN_POINT('Ctrl Pts',(-16.9833160272816,-3.9109439266341,-10.5713320279724));
#32196=CARTESIAN_POINT('Ctrl Pts',(-16.8029192897619,-4.69431869780458,
-3.52377734265748));
#32197=CARTESIAN_POINT('Ctrl Pts',(-16.5682362510152,-5.46518730011656,
3.52377734265749));
#32198=CARTESIAN_POINT('Ctrl Pts',(-16.2815073998789,-6.21619035000399,
10.5713320279725));
#32199=CARTESIAN_POINT('Ctrl Pts',(-17.401685157391,-0.932601865546468,
-12.));
#32200=CARTESIAN_POINT('Ctrl Pts',(-17.3528542378989,-1.84375196972217,
-4.));
#32201=CARTESIAN_POINT('Ctrl Pts',(-17.2323154716912,-2.75104980175429,
4.));
#32202=CARTESIAN_POINT('Ctrl Pts',(-17.0415504627302,-3.6433432974125,12.));
#32203=CARTESIAN_POINT('Ctrl Pts',(-16.760386271272,-0.898232979305966,
-12.));
#32204=CARTESIAN_POINT('Ctrl Pts',(-16.7133549024554,-1.77580475232522,
-4.00000000000001));
#32205=CARTESIAN_POINT('Ctrl Pts',(-16.5972583138761,-2.64966621978703,
4.00000000000001));
#32206=CARTESIAN_POINT('Ctrl Pts',(-16.413523508407,-3.50907630101261,12.));
#32207=CARTESIAN_POINT('Ctrl Pts',(-16.1190873851531,-0.863864093065465,
-12.));
#32208=CARTESIAN_POINT('Ctrl Pts',(-16.0738555670119,-1.70785753492828,
-4.));
#32209=CARTESIAN_POINT('Ctrl Pts',(-15.962201156061,-2.54828263781977,4.));
#32210=CARTESIAN_POINT('Ctrl Pts',(-15.7854965540837,-3.37480930461271,
12.));
#32211=CARTESIAN_POINT('Ctrl Pts',(-15.4777884990342,-0.829495206824964,
-12.));
#32212=CARTESIAN_POINT('Ctrl Pts',(-15.4343562315683,-1.63991031753134,
-4.));
#32213=CARTESIAN_POINT('Ctrl Pts',(-15.3271439982459,-2.44689905585252,
4.));
#32214=CARTESIAN_POINT('Ctrl Pts',(-15.1574695997605,-3.24054230821282,
12.));
#32215=CARTESIAN_POINT('Ctrl Pts',(-15.1574696006874,-3.24054230387749,
11.9999999562994));
#32216=CARTESIAN_POINT('Ctrl Pts',(-15.1998732543785,-3.04220150129224,
10.0007056240913));
#32217=CARTESIAN_POINT('Ctrl Pts',(-15.2383960417531,-2.84297143492238,
8.00083387021915));
#32218=CARTESIAN_POINT('Ctrl Pts',(-15.2730067887526,-2.64296493179857,
5.99999995642121));
#32219=CARTESIAN_POINT('Ctrl Pts',(-15.3076042221209,-2.44303536468648,
3.9999356985046));
#32220=CARTESIAN_POINT('Ctrl Pts',(-15.3382726305944,-2.24244546120419,
2.00006422723888));
#32221=CARTESIAN_POINT('Ctrl Pts',(-15.3649942268768,-2.04131144317626,
2.22044604925031E-15));
#32222=CARTESIAN_POINT('Ctrl Pts',(-15.3917158231593,-1.84017742514834,
-2.00006422723888));
#32223=CARTESIAN_POINT('Ctrl Pts',(-15.4144854473596,-1.63853813118234,
-3.99993569850461));
#32224=CARTESIAN_POINT('Ctrl Pts',(-15.4332899241442,-1.43651039582365,
-5.99999995642121));
#32225=CARTESIAN_POINT('Ctrl Pts',(-15.4520989285132,-1.23443401791884,
-8.00054577305927));
#32226=CARTESIAN_POINT('Ctrl Pts',(-15.466932723784,-1.03205670355153,-10.0004173920443));
#32227=CARTESIAN_POINT('Ctrl Pts',(-15.477788520436,-0.829495208838559,
-11.9999999914697));
#32228=CARTESIAN_POINT('Ctrl Pts',(-15.3649941987044,2.04131143943342,-12.));
#32229=CARTESIAN_POINT('Ctrl Pts',(-15.4718770157346,1.23680222448176,-4.));
#32230=CARTESIAN_POINT('Ctrl Pts',(-15.5154431428507,0.423889388244509,
4.));
#32231=CARTESIAN_POINT('Ctrl Pts',(-15.4951570863805,-0.387435139568704,
12.));
#32232=CARTESIAN_POINT('Ctrl Pts',(-16.0016196226445,2.12589010856384,-12.));
#32233=CARTESIAN_POINT('Ctrl Pts',(-16.1129309684345,1.2880472643632,-4.));
#32234=CARTESIAN_POINT('Ctrl Pts',(-16.1583021924993,0.441452607469,4.));
#32235=CARTESIAN_POINT('Ctrl Pts',(-16.1371756137918,-0.403487931830612,
12.));
#32236=CARTESIAN_POINT('Ctrl Pts',(-16.6382450465846,2.21046877769426,-12.));
#32237=CARTESIAN_POINT('Ctrl Pts',(-16.7539849211345,1.33929230424465,-4.00000000000001));
#32238=CARTESIAN_POINT('Ctrl Pts',(-16.801161242148,0.459015826693492,4.00000000000001));
#32239=CARTESIAN_POINT('Ctrl Pts',(-16.7791941412031,-0.41954072409252,
12.));
#32240=CARTESIAN_POINT('Ctrl Pts',(-17.2748704705247,2.29504744682469,-12.));
#32241=CARTESIAN_POINT('Ctrl Pts',(-17.3950388738344,1.39053734412609,-4.));
#32242=CARTESIAN_POINT('Ctrl Pts',(-17.4440202917966,0.476579045917982,
4.));
#32243=CARTESIAN_POINT('Ctrl Pts',(-17.4212126686144,-0.435593516354428,
12.));
#32244=CARTESIAN_POINT('Ctrl Pts',(-15.3649942201102,2.04131144140431,-11.9999999914697));
#32245=CARTESIAN_POINT('Ctrl Pts',(-15.3917093519036,1.84022611326084,-10.0004173920443));
#32246=CARTESIAN_POINT('Ctrl Pts',(-15.4144808289508,1.63858762813028,-8.00054577305927));
#32247=CARTESIAN_POINT('Ctrl Pts',(-15.4332898445205,1.43651125126802,-5.99999995642121));
#32248=CARTESIAN_POINT('Ctrl Pts',(-15.4520943325031,1.23448351695164,-3.9999356985046));
#32249=CARTESIAN_POINT('Ctrl Pts',(-15.466930098069,1.03210574960204,-2.00006422723889));
#32250=CARTESIAN_POINT('Ctrl Pts',(-15.4777885274135,0.829495208345887,
-6.66133814775094E-15));
#32251=CARTESIAN_POINT('Ctrl Pts',(-15.4886469567579,0.626884667089732,
2.00006422723887));
#32252=CARTESIAN_POINT('Ctrl Pts',(-15.495525953138,0.424080475648491,3.99993569850462));
#32253=CARTESIAN_POINT('Ctrl Pts',(-15.4984215485681,0.221200142130421,
5.99999995642122));
#32254=CARTESIAN_POINT('Ctrl Pts',(-15.5013182582685,0.0182417370997574,
8.00083387021916));
#32255=CARTESIAN_POINT('Ctrl Pts',(-15.5002268324596,-0.184675569413391,
10.0007056240913));
#32256=CARTESIAN_POINT('Ctrl Pts',(-15.4951570864913,-0.387435135136787,
11.9999999562994));
#32257=CARTESIAN_POINT('Ctrl Pts',(-17.2955736705817,2.13341879826209,-10.5713320220547));
#32258=CARTESIAN_POINT('Ctrl Pts',(-17.3939672736713,1.33563987584167,-3.52377734068488));
#32259=CARTESIAN_POINT('Ctrl Pts',(-17.4370874835488,0.531047536999957,
3.52377734068489));
#32260=CARTESIAN_POINT('Ctrl Pts',(-17.4245226937903,-0.272677936184493,
10.5713320220547));
#32261=CARTESIAN_POINT('Ctrl Pts',(-17.2955750463446,2.1334188914951,-10.5713320279724));
#32262=CARTESIAN_POINT('Ctrl Pts',(-17.3939814195907,1.33564081785934,-3.52377734265747));
#32263=CARTESIAN_POINT('Ctrl Pts',(-17.4371016491204,0.531048112360097,
3.52377734265749));
#32264=CARTESIAN_POINT('Ctrl Pts',(-17.4245240716391,-0.272677881753643,
10.5713320279725));
#32265=CARTESIAN_POINT('Ctrl Pts',(-17.295956147427,2.13346293887238,-10.5713320279724));
#32266=CARTESIAN_POINT('Ctrl Pts',(-17.3943645524084,1.33566728651567,-3.52377734265748));
#32267=CARTESIAN_POINT('Ctrl Pts',(-17.4374855954662,0.531056861604773,
3.52377734265749));
#32268=CARTESIAN_POINT('Ctrl Pts',(-17.4249076055392,-0.272686823446403,
10.5713320279725));
#32269=CARTESIAN_POINT('Ctrl Pts',(-17.2963372485426,2.13350698625262,-10.5713320279724));
#32270=CARTESIAN_POINT('Ctrl Pts',(-17.3947476852595,1.33569375517339,-3.52377734265747));
#32271=CARTESIAN_POINT('Ctrl Pts',(-17.4378695418455,0.531065610849369,
3.52377734265748));
#32272=CARTESIAN_POINT('Ctrl Pts',(-17.4252911394727,-0.272695765140821,
10.5713320279725));
#32273=CARTESIAN_POINT('Ctrl Pts',(-17.2967183496608,2.13355103363312,-10.5713320279724));
#32274=CARTESIAN_POINT('Ctrl Pts',(-17.3951308181133,1.33572022383134,-3.52377734265747));
#32275=CARTESIAN_POINT('Ctrl Pts',(-17.4382534882274,0.531074360093894,
3.52377734265749));
#32276=CARTESIAN_POINT('Ctrl Pts',(-17.4256746734088,-0.272704706835343,
10.5713320279725));
#32277=CARTESIAN_POINT('Origin',(2.22044604925031E-15,-4.16333634234434E-16,
-6.));
#32278=CARTESIAN_POINT('Ctrl Pts',(-15.3516930767777,2.1390462349833,11.9999999562994));
#32279=CARTESIAN_POINT('Ctrl Pts',(-15.3237029275181,2.33992852728641,10.0007056240913));
#32280=CARTESIAN_POINT('Ctrl Pts',(-15.2917618106915,2.540319119752,8.00083387021915));
#32281=CARTESIAN_POINT('Ctrl Pts',(-15.2558790213823,2.74010132749603,5.99999995642122));
#32282=CARTESIAN_POINT('Ctrl Pts',(-15.2200100350179,2.9398066855075,3.9999356985046));
#32283=CARTESIAN_POINT('Ctrl Pts',(-15.1802231246131,3.13878875107565,2.00006422723889));
#32284=CARTESIAN_POINT('Ctrl Pts',(-15.1365413257817,3.33693222779592,-2.22044604925031E-15));
#32285=CARTESIAN_POINT('Ctrl Pts',(-15.0928595269503,3.53507570451619,-2.00006422723887));
#32286=CARTESIAN_POINT('Ctrl Pts',(-15.0452912745672,3.73234233124902,-3.99993569850461));
#32287=CARTESIAN_POINT('Ctrl Pts',(-14.9938641476362,3.92861781320468,-5.99999995642121));
#32288=CARTESIAN_POINT('Ctrl Pts',(-14.9424246385123,4.12494055272707,-8.00054577305927));
#32289=CARTESIAN_POINT('Ctrl Pts',(-14.8871467284008,4.32018647843708,-10.0004173920443));
#32290=CARTESIAN_POINT('Ctrl Pts',(-14.8280677289535,4.51424492140109,-11.9999999914697));
#32291=CARTESIAN_POINT('Ctrl Pts',(-16.67120375536,5.07536776045384,-12.));
#32292=CARTESIAN_POINT('Ctrl Pts',(-16.9369493898684,4.20246557304821,-4.));
#32293=CARTESIAN_POINT('Ctrl Pts',(-17.1339941352951,3.30865780933792,4.));
#32294=CARTESIAN_POINT('Ctrl Pts',(-17.2599160133439,2.40493072018629,12.));
#32295=CARTESIAN_POINT('Ctrl Pts',(-16.0568250729579,4.88832681229368,-12.));
#32296=CARTESIAN_POINT('Ctrl Pts',(-16.312777266322,4.047593417474,-4.));
#32297=CARTESIAN_POINT('Ctrl Pts',(-16.5025603830837,3.18672487304549,4.));
#32298=CARTESIAN_POINT('Ctrl Pts',(-16.6238417013591,2.31630255698833,12.));
#32299=CARTESIAN_POINT('Ctrl Pts',(-15.4424463905558,4.70128586413352,-12.));
#32300=CARTESIAN_POINT('Ctrl Pts',(-15.6886051427755,3.89272126189978,-4.));
#32301=CARTESIAN_POINT('Ctrl Pts',(-15.8711266308723,3.06479193675306,4.));
#32302=CARTESIAN_POINT('Ctrl Pts',(-15.9877673893743,2.22767439379038,12.));
#32303=CARTESIAN_POINT('Ctrl Pts',(-14.8280677081536,4.51424491597336,-12.));
#32304=CARTESIAN_POINT('Ctrl Pts',(-15.0644330192291,3.73784910632557,-4.));
#32305=CARTESIAN_POINT('Ctrl Pts',(-15.2396928786609,2.94285900046063,4.));
#32306=CARTESIAN_POINT('Ctrl Pts',(-15.3516930773895,2.13904623059242,12.));
#32307=CARTESIAN_POINT('Ctrl Pts',(-15.5228520082561,7.92019304563385,-10.5713320279724));
#32308=CARTESIAN_POINT('Ctrl Pts',(-15.8881799221207,7.2041838386953,-3.52377734265748));
#32309=CARTESIAN_POINT('Ctrl Pts',(-16.20388659607,6.46286199768347,3.52377734265748));
#32310=CARTESIAN_POINT('Ctrl Pts',(-16.4669580190248,5.70330482702814,10.5713320279724));
#32311=CARTESIAN_POINT('Ctrl Pts',(-15.5231950610337,7.92036478087257,-10.5713320279724));
#32312=CARTESIAN_POINT('Ctrl Pts',(-15.8885308963815,7.2043397502344,-3.52377734265747));
#32313=CARTESIAN_POINT('Ctrl Pts',(-16.2042443951928,6.46300153666554,3.52377734265747));
#32314=CARTESIAN_POINT('Ctrl Pts',(-16.4673214812322,5.70342760090243,10.5713320279724));
#32315=CARTESIAN_POINT('Ctrl Pts',(-15.5235381138415,7.92053651612543,-10.5713320279724));
#32316=CARTESIAN_POINT('Ctrl Pts',(-15.8888818706732,7.20449566178622,-3.52377734265749));
#32317=CARTESIAN_POINT('Ctrl Pts',(-16.204602194347,6.46314107565896,3.52377734265749));
#32318=CARTESIAN_POINT('Ctrl Pts',(-16.4676849434715,5.70355037478656,10.5713320279724));
#32319=CARTESIAN_POINT('Ctrl Pts',(-15.5238811666517,7.92070825137944,-10.5713320279724));
#32320=CARTESIAN_POINT('Ctrl Pts',(-15.8892328449674,7.20465157333916,-3.52377734265748));
#32321=CARTESIAN_POINT('Ctrl Pts',(-16.2049599935037,6.46328061465322,3.52377734265748));
#32322=CARTESIAN_POINT('Ctrl Pts',(-16.4680484057134,5.7036731486715,10.5713320279724));
#32323=CARTESIAN_POINT('Ctrl Pts',(-15.5228507477965,7.92019248660845,-10.5713320134286));
#32324=CARTESIAN_POINT('Ctrl Pts',(-15.8881669516022,7.20417811498611,-3.52377733780954));
#32325=CARTESIAN_POINT('Ctrl Pts',(-16.2038734814214,6.46285661240599,3.52377733780955));
#32326=CARTESIAN_POINT('Ctrl Pts',(-16.466956742565,5.70330430555751,10.5713320134286));
#32327=CARTESIAN_POINT('Ctrl Pts',(-13.7402020358534,7.17334281440038,-12.));
#32328=CARTESIAN_POINT('Ctrl Pts',(-14.1157973873101,6.45390751815577,-4.));
#32329=CARTESIAN_POINT('Ctrl Pts',(-14.4347687202385,5.70491981764188,4.00000000000001));
#32330=CARTESIAN_POINT('Ctrl Pts',(-14.6931953939549,4.93558590585174,12.));
#32331=CARTESIAN_POINT('Ctrl Pts',(-14.3095066403964,7.47055948439889,-12.));
#32332=CARTESIAN_POINT('Ctrl Pts',(-14.7006642203029,6.72131546876616,-3.99999999999999));
#32333=CARTESIAN_POINT('Ctrl Pts',(-15.0328516506423,5.94129458944341,4.));
#32334=CARTESIAN_POINT('Ctrl Pts',(-15.3019858448814,5.14008448418317,12.));
#32335=CARTESIAN_POINT('Ctrl Pts',(-14.8788112449393,7.76777615439741,-12.));
#32336=CARTESIAN_POINT('Ctrl Pts',(-15.2855310532957,6.98872341937656,-4.00000000000001));
#32337=CARTESIAN_POINT('Ctrl Pts',(-15.6309345810462,6.17766936124494,4.00000000000002));
#32338=CARTESIAN_POINT('Ctrl Pts',(-15.9107762958078,5.3445830625146,12.));
#32339=CARTESIAN_POINT('Ctrl Pts',(-15.4481158494823,8.06499282439592,-12.));
#32340=CARTESIAN_POINT('Ctrl Pts',(-15.8703978862885,7.25613136998696,-4.));
#32341=CARTESIAN_POINT('Ctrl Pts',(-16.2290175114501,6.41404413304647,4.00000000000001));
#32342=CARTESIAN_POINT('Ctrl Pts',(-16.5195667467343,5.54908164084603,12.));
#32343=CARTESIAN_POINT('Ctrl Pts',(-13.7402020552943,7.17334282357369,-11.9999999914697));
#32344=CARTESIAN_POINT('Ctrl Pts',(-13.8340813002562,6.99352153777387,-10.0004173920443));
#32345=CARTESIAN_POINT('Ctrl Pts',(-13.9244439127861,6.81183164507365,-8.00054577305927));
#32346=CARTESIAN_POINT('Ctrl Pts',(-14.0112327972984,6.628375027102,-5.99999995642121));
#32347=CARTESIAN_POINT('Ctrl Pts',(-14.09800079054,6.44496256964577,-3.99993569850462));
#32348=CARTESIAN_POINT('Ctrl Pts',(-14.1811591229608,6.25986380572142,-2.00006422723887));
#32349=CARTESIAN_POINT('Ctrl Pts',(-14.2606595952488,6.07318597677023,-4.44089209839888E-15));
#32350=CARTESIAN_POINT('Ctrl Pts',(-14.3401600675367,5.88650814781904,2.00006422723887));
#32351=CARTESIAN_POINT('Ctrl Pts',(-14.4159873282975,5.69828730098518,3.99993569850462));
#32352=CARTESIAN_POINT('Ctrl Pts',(-14.4880974587037,5.50863250063968,5.99999995642122));
#32353=CARTESIAN_POINT('Ctrl Pts',(-14.5602353382114,5.31890471817276,8.00083387021916));
#32354=CARTESIAN_POINT('Ctrl Pts',(-14.6286115396895,5.12785153300099,10.0007056240913));
#32355=CARTESIAN_POINT('Ctrl Pts',(-14.6931953925432,4.93558591005428,11.9999999562994));
#32356=CARTESIAN_POINT('Origin',(2.22044604925031E-15,-4.16333634234434E-16,
-6.));
#32357=CARTESIAN_POINT('Origin',(2.22044604925031E-15,-4.16333634234434E-16,
-6.));
#32358=CARTESIAN_POINT('Ctrl Pts',(-13.6942758009489,7.26063422894488,11.9999999562994));
#32359=CARTESIAN_POINT('Ctrl Pts',(-13.5992678738299,7.43982864180721,10.0007056240913));
#32360=CARTESIAN_POINT('Ctrl Pts',(-13.500715422892,7.617209697467,8.00083387021915));
#32361=CARTESIAN_POINT('Ctrl Pts',(-13.3986670912385,7.79267092710594,5.99999995642121));
#32362=CARTESIAN_POINT('Ctrl Pts',(-13.2966580142668,7.9680646625034,3.9999356985046));
#32363=CARTESIAN_POINT('Ctrl Pts',(-13.1912146735706,8.14143871638738,2.00006422723888));
#32364=CARTESIAN_POINT('Ctrl Pts',(-13.0823981492392,8.31269262422126,2.22030256658695E-15));
#32365=CARTESIAN_POINT('Ctrl Pts',(-12.9735816249078,8.48394653205514,-2.00006422723887));
#32366=CARTESIAN_POINT('Ctrl Pts',(-12.8614129292112,8.65304722502548,-3.9999356985046));
#32367=CARTESIAN_POINT('Ctrl Pts',(-12.7459570690561,8.81989673373664,-5.99999995642121));
#32368=CARTESIAN_POINT('Ctrl Pts',(-12.630473410406,8.98678641507513,-8.00054577305927));
#32369=CARTESIAN_POINT('Ctrl Pts',(-12.5117511266867,9.15135141196428,-10.0004173920443));
#32370=CARTESIAN_POINT('Ctrl Pts',(-12.3898631303866,9.31350049096029,-11.9999999914697));
#32371=CARTESIAN_POINT('Ctrl Pts',(-10.4581387236936,11.4401631786859,-12.));
#32372=CARTESIAN_POINT('Ctrl Pts',(-11.0571442669941,10.8925763156096,-4.));
#32373=CARTESIAN_POINT('Ctrl Pts',(-11.613048155468,10.2978527213822,4.));
#32374=CARTESIAN_POINT('Ctrl Pts',(-12.1190174885494,9.66330244953633,12.));
#32375=CARTESIAN_POINT('Ctrl Pts',(-10.8914559714904,11.9141691326998,-12.));
#32376=CARTESIAN_POINT('Ctrl Pts',(-11.5152804085056,11.3438938315843,-4.00000000000002));
#32377=CARTESIAN_POINT('Ctrl Pts',(-12.0942173384564,10.7245287597614,4.00000000000001));
#32378=CARTESIAN_POINT('Ctrl Pts',(-12.6211507498191,10.0636868518367,12.));
#32379=CARTESIAN_POINT('Ctrl Pts',(-11.3247732192871,12.3881750867137,-12.));
#32380=CARTESIAN_POINT('Ctrl Pts',(-11.9734165500172,11.795211347559,-3.99999999999999));
#32381=CARTESIAN_POINT('Ctrl Pts',(-12.5753865214448,11.1512047981406,3.99999999999998));
#32382=CARTESIAN_POINT('Ctrl Pts',(-13.1232840110888,10.4640712541372,12.));
#32383=CARTESIAN_POINT('Ctrl Pts',(-11.7580904670839,12.8621810407276,-12.));
#32384=CARTESIAN_POINT('Ctrl Pts',(-12.4315526915288,12.2465288635337,-4.));
#32385=CARTESIAN_POINT('Ctrl Pts',(-13.0565557044332,11.5778808365198,4.));
#32386=CARTESIAN_POINT('Ctrl Pts',(-13.6254172723584,10.8644556564376,12.));
#32387=CARTESIAN_POINT('Ctrl Pts',(-10.4581387388246,11.4401631939552,-11.9999999914697));
#32388=CARTESIAN_POINT('Ctrl Pts',(-10.6078588745025,11.303295051446,-10.0004173920443));
#32389=CARTESIAN_POINT('Ctrl Pts',(-10.7549135578339,11.163468233693,-8.00054577305927));
#32390=CARTESIAN_POINT('Ctrl Pts',(-10.8992142909491,11.0207589502706,-5.99999995642121));
#32391=CARTESIAN_POINT('Ctrl Pts',(-11.0434802889055,10.8780840189234,-3.99993569850461));
#32392=CARTESIAN_POINT('Ctrl Pts',(-11.184931066005,10.7325899011204,-2.00006422723887));
#32393=CARTESIAN_POINT('Ctrl Pts',(-11.3234846509767,10.584360885717,2.2202945954294E-15));
#32394=CARTESIAN_POINT('Ctrl Pts',(-11.4620382359483,10.4361318703137,2.00006422723887));
#32395=CARTESIAN_POINT('Ctrl Pts',(-11.5976678743505,10.2851965800591,3.99993569850461));
#32396=CARTESIAN_POINT('Ctrl Pts',(-11.7302949937737,10.1316424808146,5.99999995642121));
#32397=CARTESIAN_POINT('Ctrl Pts',(-11.8629731501784,9.97802929156078,8.00083387021915));
#32398=CARTESIAN_POINT('Ctrl Pts',(-11.99256979992,9.82188406150686,10.0007056240913));
#32399=CARTESIAN_POINT('Ctrl Pts',(-12.1190174857855,9.66330245300261,11.9999999562994));
#32400=CARTESIAN_POINT('Ctrl Pts',(-11.8778429311088,12.7516740731249,-10.5713320220547));
#32401=CARTESIAN_POINT('Ctrl Pts',(-12.466019210595,12.2037861517057,-3.52377734068488));
#32402=CARTESIAN_POINT('Ctrl Pts',(-13.0162331940139,11.6151497981962,3.52377734068489));
#32403=CARTESIAN_POINT('Ctrl Pts',(-13.5232327823929,10.9913838744951,10.5713320220547));
#32404=CARTESIAN_POINT('Ctrl Pts',(-13.9299291396692,10.4711731300928,-12.));
#32405=CARTESIAN_POINT('Ctrl Pts',(-14.4781984826686,9.74180374592263,-4.));
#32406=CARTESIAN_POINT('Ctrl Pts',(-14.9690602353605,8.96929245803532,4.));
#32407=CARTESIAN_POINT('Ctrl Pts',(-15.3964809635174,8.1631345999333,12.));
#32408=CARTESIAN_POINT('Ctrl Pts',(-13.4165737973453,10.0852822463105,-12.));
#32409=CARTESIAN_POINT('Ctrl Pts',(-13.9446379409184,9.38279208500909,-4.00000000000001));
#32410=CARTESIAN_POINT('Ctrl Pts',(-14.4174101182391,8.63874991513855,4.));
#32411=CARTESIAN_POINT('Ctrl Pts',(-14.8290792433535,7.86230114163155,12.));
#32412=CARTESIAN_POINT('Ctrl Pts',(-12.9032184550213,9.6993913625282,-12.));
#32413=CARTESIAN_POINT('Ctrl Pts',(-13.4110773991682,9.02378042409555,-4.));
#32414=CARTESIAN_POINT('Ctrl Pts',(-13.8657600011178,8.30820737224178,3.99999999999999));
#32415=CARTESIAN_POINT('Ctrl Pts',(-14.2616775231895,7.56146768332979,12.));
#32416=CARTESIAN_POINT('Ctrl Pts',(-12.3898631126974,9.3135004787459,-12.));
#32417=CARTESIAN_POINT('Ctrl Pts',(-12.877516857418,8.66476876318201,-4.));
#32418=CARTESIAN_POINT('Ctrl Pts',(-13.3141098839964,7.977664829345,4.));
#32419=CARTESIAN_POINT('Ctrl Pts',(-13.6942758030256,7.26063422502805,12.));
#32420=CARTESIAN_POINT('Ctrl Pts',(-11.8778439250753,12.7516750288689,-10.5713320279724));
#32421=CARTESIAN_POINT('Ctrl Pts',(-12.4660294414806,12.2037959661548,-3.52377734265748));
#32422=CARTESIAN_POINT('Ctrl Pts',(-13.0162436756369,11.6151593444016,3.52377734265749));
#32423=CARTESIAN_POINT('Ctrl Pts',(-13.5232338028988,10.9913848018556,10.5713320279725));
#32424=CARTESIAN_POINT('Ctrl Pts',(-11.8781075523334,12.7519537381713,-10.5713320279724));
#32425=CARTESIAN_POINT('Ctrl Pts',(-12.4663059245223,12.20406251535,-3.52377734265749));
#32426=CARTESIAN_POINT('Ctrl Pts',(-13.0165321716956,11.6154128426657,3.52377734265749));
#32427=CARTESIAN_POINT('Ctrl Pts',(-13.5235333545211,10.9916244829605,10.5713320279725));
#32428=CARTESIAN_POINT('Ctrl Pts',(-11.878371179615,12.7522324474973,-10.5713320279724));
#32429=CARTESIAN_POINT('Ctrl Pts',(-12.4665824075886,12.2043290645677,-3.52377734265747));
#32430=CARTESIAN_POINT('Ctrl Pts',(-13.0168206677798,11.6156663409513,3.52377734265748));
#32431=CARTESIAN_POINT('Ctrl Pts',(-13.5238329061699,10.9918641640855,10.5713320279725));
#32432=CARTESIAN_POINT('Ctrl Pts',(-11.8786348068985,12.7525111568252,-10.5713320279724));
#32433=CARTESIAN_POINT('Ctrl Pts',(-12.4668588906568,12.2045956137873,-3.52377734265748));
#32434=CARTESIAN_POINT('Ctrl Pts',(-13.0171091638662,11.6159198392386,3.52377734265749));
#32435=CARTESIAN_POINT('Ctrl Pts',(-13.5241324578209,10.9921038452121,10.5713320279725));
#32436=CARTESIAN_POINT('Ctrl Pts',(-9.50849948587548,14.604000482186,-12.));
#32437=CARTESIAN_POINT('Ctrl Pts',(-10.2731631630064,14.1061366133278,-4.));
#32438=CARTESIAN_POINT('Ctrl Pts',(-10.9986367512409,13.5480980636351,4.));
#32439=CARTESIAN_POINT('Ctrl Pts',(-11.6760030816321,12.9367439718926,12.));
#32440=CARTESIAN_POINT('Ctrl Pts',(-9.15808571423197,14.0658037985085,-12.));
#32441=CARTESIAN_POINT('Ctrl Pts',(-9.89456947890246,13.5862875518289,-3.99999999999999));
#32442=CARTESIAN_POINT('Ctrl Pts',(-10.5933074148231,13.0488142230957,4.));
#32443=CARTESIAN_POINT('Ctrl Pts',(-11.2457109746983,12.4599901733872,12.));
#32444=CARTESIAN_POINT('Ctrl Pts',(-8.80767194258845,13.5276071148311,-12.));
#32445=CARTESIAN_POINT('Ctrl Pts',(-9.51597579479849,13.0664384903301,-4.));
#32446=CARTESIAN_POINT('Ctrl Pts',(-10.1879780784053,12.5495303825563,4.00000000000001));
#32447=CARTESIAN_POINT('Ctrl Pts',(-10.8154188677646,11.9832363748819,12.));
#32448=CARTESIAN_POINT('Ctrl Pts',(-8.45725817094493,12.9894104311537,-12.));
#32449=CARTESIAN_POINT('Ctrl Pts',(-9.13738211069452,12.5465894288312,-4.));
#32450=CARTESIAN_POINT('Ctrl Pts',(-9.78264874198741,12.0502465420169,4.));
#32451=CARTESIAN_POINT('Ctrl Pts',(-10.3851267608308,11.5064825763765,12.));
#32452=CARTESIAN_POINT('Ctrl Pts',(-10.3851267575397,11.5064825793468,11.9999999562994));
#32453=CARTESIAN_POINT('Ctrl Pts',(-10.2345604107395,11.6423756219493,10.0007056240913));
#32454=CARTESIAN_POINT('Ctrl Pts',(-10.0812835057528,11.7753523676252,8.00083387021915));
#32455=CARTESIAN_POINT('Ctrl Pts',(-9.92537816662526,11.9053294053327,5.99999995642121));
#32456=CARTESIAN_POINT('Ctrl Pts',(-9.7695327992227,12.0352564450914,3.99993569850461));
#32457=CARTESIAN_POINT('Ctrl Pts',(-9.61115105130114,12.1621110176642,2.00006422723887));
#32458=CARTESIAN_POINT('Ctrl Pts',(-9.45032468026493,12.2858196078884,-2.22030256658673E-15));
#32459=CARTESIAN_POINT('Ctrl Pts',(-9.28949830922872,12.4095281981127,-2.00006422723889));
#32460=CARTESIAN_POINT('Ctrl Pts',(-9.12625837035319,12.5300669180878,-3.99993569850459));
#32461=CARTESIAN_POINT('Ctrl Pts',(-8.9606994576558,12.6473659403674,-5.9999999564212));
#32462=CARTESIAN_POINT('Ctrl Pts',(-8.79510068306996,12.7646932049232,-8.00054577305927));
#32463=CARTESIAN_POINT('Ctrl Pts',(-8.62725368531362,12.878728305646,-10.0004173920443));
#32464=CARTESIAN_POINT('Ctrl Pts',(-8.45725818338971,12.9894104486815,-11.9999999914697));
#32465=CARTESIAN_POINT('Ctrl Pts',(-5.91466953576705,14.3271310247952,-12.));
#32466=CARTESIAN_POINT('Ctrl Pts',(-6.66483636200897,14.0174396520956,-4.));
#32467=CARTESIAN_POINT('Ctrl Pts',(-7.39062259281095,13.648712606804,4.));
#32468=CARTESIAN_POINT('Ctrl Pts',(-8.08310721637551,13.2254821026516,12.));
#32469=CARTESIAN_POINT('Ctrl Pts',(-6.15973497165189,14.9207541491876,-12.));
#32470=CARTESIAN_POINT('Ctrl Pts',(-6.94098383200367,14.5982311802709,-4.));
#32471=CARTESIAN_POINT('Ctrl Pts',(-7.69684192361463,14.2142264844647,4.));
#32472=CARTESIAN_POINT('Ctrl Pts',(-8.41801860598165,13.7734600609591,12.));
#32473=CARTESIAN_POINT('Ctrl Pts',(-6.40480040753672,15.51437727358,-12.));
#32474=CARTESIAN_POINT('Ctrl Pts',(-7.21713130199837,15.1790227084462,-4.00000000000001));
#32475=CARTESIAN_POINT('Ctrl Pts',(-8.00306125441831,14.7797403621254,4.00000000000001));
#32476=CARTESIAN_POINT('Ctrl Pts',(-8.7529299955878,14.3214380192667,12.));
#32477=CARTESIAN_POINT('Ctrl Pts',(-6.64986584342155,16.1080003979724,-12.));
#32478=CARTESIAN_POINT('Ctrl Pts',(-7.49327877199307,15.7598142366215,-4.));
#32479=CARTESIAN_POINT('Ctrl Pts',(-8.30928058522199,15.3452542397861,4.));
#32480=CARTESIAN_POINT('Ctrl Pts',(-9.08784138519395,14.8694159775742,12.));
#32481=CARTESIAN_POINT('Ctrl Pts',(-5.91466954476314,14.3271310443187,-11.9999999914697));
#32482=CARTESIAN_POINT('Ctrl Pts',(-6.10217211316042,14.2497243630455,-10.0004173920443));
#32483=CARTESIAN_POINT('Ctrl Pts',(-6.28818190218765,14.1686257980847,-8.00054577305927));
#32484=CARTESIAN_POINT('Ctrl Pts',(-6.47258968583998,14.0838766949572,-5.99999995642121));
#32485=CARTESIAN_POINT('Ctrl Pts',(-6.65695308001831,13.9991479920971,-3.99993569850461));
#32486=CARTESIAN_POINT('Ctrl Pts',(-6.83963525048718,13.910807258287,-2.00006422723887));
#32487=CARTESIAN_POINT('Ctrl Pts',(-7.02053034096173,13.8189056633163,0.));
#32488=CARTESIAN_POINT('Ctrl Pts',(-7.20142543143627,13.7270040683457,2.00006422723886));
#32489=CARTESIAN_POINT('Ctrl Pts',(-7.38049851140844,13.6315593582429,3.99993569850462));
#32490=CARTESIAN_POINT('Ctrl Pts',(-7.5576458318784,13.5326268506854,5.99999995642121));
#32491=CARTESIAN_POINT('Ctrl Pts',(-7.73486132139669,13.4336562723579,8.00083387021915));
#32492=CARTESIAN_POINT('Ctrl Pts',(-7.91004715080012,13.3312524166245,10.0007056240913));
#32493=CARTESIAN_POINT('Ctrl Pts',(-8.08310721259277,13.2254821049635,11.9999999562994));
#32494=CARTESIAN_POINT('Ctrl Pts',(-6.80019195908459,16.04511557088,-10.5713320220547));
#32495=CARTESIAN_POINT('Ctrl Pts',(-7.54028557404928,15.7314374695154,-3.52377734068489));
#32496=CARTESIAN_POINT('Ctrl Pts',(-8.25864308411527,15.3664844972649,3.52377734068488));
#32497=CARTESIAN_POINT('Ctrl Pts',(-8.94840736668244,14.9537403335486,10.5713320220547));
#32498=CARTESIAN_POINT('Ctrl Pts',(-6.80019256622393,16.0451168089422,-10.5713320279724));
#32499=CARTESIAN_POINT('Ctrl Pts',(-7.54029183119772,15.7314501912497,-3.52377734265748));
#32500=CARTESIAN_POINT('Ctrl Pts',(-8.25864966862456,15.3664970526898,3.52377734265748));
#32501=CARTESIAN_POINT('Ctrl Pts',(-8.94840800846833,14.9537415540161,10.5713320279724));
#32502=CARTESIAN_POINT('Ctrl Pts',(-6.80034497061741,16.0454688758496,-10.5713320279724));
#32503=CARTESIAN_POINT('Ctrl Pts',(-7.54046047507779,15.731795228331,-3.52377734265747));
#32504=CARTESIAN_POINT('Ctrl Pts',(-8.25883406472934,15.3668339346014,3.52377734265747));
#32505=CARTESIAN_POINT('Ctrl Pts',(-8.94860751915147,14.9540692332704,10.5713320279724));
#32506=CARTESIAN_POINT('Ctrl Pts',(-6.80049737502494,16.0458209427872,-10.5713320279724));
#32507=CARTESIAN_POINT('Ctrl Pts',(-7.54062911897336,15.732140265442,-3.52377734265749));
#32508=CARTESIAN_POINT('Ctrl Pts',(-8.2590184608509,15.3671708165418,3.52377734265749));
#32509=CARTESIAN_POINT('Ctrl Pts',(-8.94880702985271,14.9543969125528,10.5713320279724));
#32510=CARTESIAN_POINT('Ctrl Pts',(-6.80064977943358,16.0461730097273,-10.5713320279724));
#32511=CARTESIAN_POINT('Ctrl Pts',(-7.54079776287006,15.7324853025554,-3.52377734265748));
#32512=CARTESIAN_POINT('Ctrl Pts',(-8.25920285697384,15.3675076984845,3.52377734265748));
#32513=CARTESIAN_POINT('Ctrl Pts',(-8.94900654055538,14.9547245918374,10.5713320279724));
#32514=CARTESIAN_POINT('Origin',(2.22044604925031E-15,-4.16333634234434E-16,
-6.));
#32515=CARTESIAN_POINT('Ctrl Pts',(-5.82337815902385,14.3644793130828,11.9999999562994));
#32516=CARTESIAN_POINT('Ctrl Pts',(-5.63541391608915,14.4406802789199,10.0007056240913));
#32517=CARTESIAN_POINT('Ctrl Pts',(-5.44590001392117,14.5132137565555,8.00083387021915));
#32518=CARTESIAN_POINT('Ctrl Pts',(-5.25494215213615,14.5820294533272,5.99999995642121));
#32519=CARTESIAN_POINT('Ctrl Pts',(-5.06405774564414,14.6508186789333,3.9999356985046));
#32520=CARTESIAN_POINT('Ctrl Pts',(-4.87184076676219,14.7158532365687,2.00006422723888));
#32521=CARTESIAN_POINT('Ctrl Pts',(-4.67840258291259,14.7770954274579,2.22044604925031E-15));
#32522=CARTESIAN_POINT('Ctrl Pts',(-4.48496439906298,14.8383376183471,-2.00006422723888));
#32523=CARTESIAN_POINT('Ctrl Pts',(-4.29034236280191,14.895775616736,-3.99993569850461));
#32524=CARTESIAN_POINT('Ctrl Pts',(-4.0946492458228,14.949376159348,-5.99999995642121));
#32525=CARTESIAN_POINT('Ctrl Pts',(-3.89890901149391,15.0029896074497,-8.00054577305927));
#32526=CARTESIAN_POINT('Ctrl Pts',(-3.70218212478788,15.05274049588,-10.0004173920443));
#32527=CARTESIAN_POINT('Ctrl Pts',(-3.50458308363856,15.0986058030105,-11.9999999914697));
#32528=CARTESIAN_POINT('Ctrl Pts',(-3.94020446357842,16.9753698440352,-12.));
#32529=CARTESIAN_POINT('Ctrl Pts',(-4.82903275014493,16.7690612207615,-4.));
#32530=CARTESIAN_POINT('Ctrl Pts',(-5.70161535233114,16.4928030941281,4.));
#32531=CARTESIAN_POINT('Ctrl Pts',(-6.54722690864904,16.1499910948348,12.));
#32532=CARTESIAN_POINT('Ctrl Pts',(-3.794997335032,16.3497818234513,-12.));
#32533=CARTESIAN_POINT('Ctrl Pts',(-4.65106990943784,16.1510762276491,-4.));
#32534=CARTESIAN_POINT('Ctrl Pts',(-5.49149549661271,15.8849989557599,4.));
#32535=CARTESIAN_POINT('Ctrl Pts',(-6.30594399347681,15.5548205003623,12.));
#32536=CARTESIAN_POINT('Ctrl Pts',(-3.64979020648557,15.7241938028673,-12.));
#32537=CARTESIAN_POINT('Ctrl Pts',(-4.47310706873074,15.5330912345367,-4.));
#32538=CARTESIAN_POINT('Ctrl Pts',(-5.28137564089428,15.2771948173917,4.));
#32539=CARTESIAN_POINT('Ctrl Pts',(-6.06466107830459,14.9596499058898,12.));
#32540=CARTESIAN_POINT('Ctrl Pts',(-3.50458307793915,15.0986057822834,-12.));
#32541=CARTESIAN_POINT('Ctrl Pts',(-4.29514422802365,14.9151062414243,-4.));
#32542=CARTESIAN_POINT('Ctrl Pts',(-5.07125578517585,14.6693906790234,4.));
#32543=CARTESIAN_POINT('Ctrl Pts',(-5.82337816313236,14.3644793114172,12.));
#32544=CARTESIAN_POINT('Ctrl Pts',(-0.902337623732298,17.403280701153,-10.5713320279724));
#32545=CARTESIAN_POINT('Ctrl Pts',(-1.70508374321692,17.361659351802,-3.52377734265748));
#32546=CARTESIAN_POINT('Ctrl Pts',(-2.50494062688805,17.2644084310805,3.52377734265748));
#32547=CARTESIAN_POINT('Ctrl Pts',(-3.29427214377962,17.1124563810414,10.5713320279724));
#32548=CARTESIAN_POINT('Ctrl Pts',(-0.902360423041643,17.4036636611926,
-10.5713320279724));
#32549=CARTESIAN_POINT('Ctrl Pts',(-1.70512420699373,17.3620412601975,-3.52377734265747));
#32550=CARTESIAN_POINT('Ctrl Pts',(-2.50499868214617,17.2647880637013,3.52377734265747));
#32551=CARTESIAN_POINT('Ctrl Pts',(-3.29434754958927,17.1128325354835,10.5713320279724));
#32552=CARTESIAN_POINT('Ctrl Pts',(-0.902383222353851,17.4040466212655,
-10.5713320279724));
#32553=CARTESIAN_POINT('Ctrl Pts',(-1.70516467077498,17.3624231686262,-3.52377734265748));
#32554=CARTESIAN_POINT('Ctrl Pts',(-2.50505673741016,17.265167696355,3.52377734265748));
#32555=CARTESIAN_POINT('Ctrl Pts',(-3.29442295540635,17.1132086899581,10.5713320279724));
#32556=CARTESIAN_POINT('Ctrl Pts',(-0.902406021666259,17.4044295813409,
-10.5713320279724));
#32557=CARTESIAN_POINT('Ctrl Pts',(-1.70520513455646,17.3628050770574,-3.52377734265748));
#32558=CARTESIAN_POINT('Ctrl Pts',(-2.50511479267468,17.2655473290114,3.52377734265748));
#32559=CARTESIAN_POINT('Ctrl Pts',(-3.29449836122398,17.1135848444354,10.5713320279724));
#32560=CARTESIAN_POINT('Ctrl Pts',(-0.902337477632694,17.4032793300502,
-10.5713320134286));
#32561=CARTESIAN_POINT('Ctrl Pts',(-1.70508221483526,17.361645257149,-3.52377733780954));
#32562=CARTESIAN_POINT('Ctrl Pts',(-2.50493873335086,17.2643943808229,3.52377733780954));
#32563=CARTESIAN_POINT('Ctrl Pts',(-3.29427195715649,17.1124550148594,10.5713320134286));
#32564=CARTESIAN_POINT('Ctrl Pts',(-0.657803910601428,15.4860354233799,
-12.));
#32565=CARTESIAN_POINT('Ctrl Pts',(-1.46865082925679,15.4515928911625,-4.));
#32566=CARTESIAN_POINT('Ctrl Pts',(-2.2767788714881,15.3533363183005,4.));
#32567=CARTESIAN_POINT('Ctrl Pts',(-3.07225491994942,15.1924734268593,12.));
#32568=CARTESIAN_POINT('Ctrl Pts',(-0.685059026225969,16.1276760084048,
-12.));
#32569=CARTESIAN_POINT('Ctrl Pts',(-1.52950216735065,16.0918064016704,-4.00000000000002));
#32570=CARTESIAN_POINT('Ctrl Pts',(-2.37111377949615,15.9894787155008,4.00000000000002));
#32571=CARTESIAN_POINT('Ctrl Pts',(-3.19954918153982,15.8219507121087,12.));
#32572=CARTESIAN_POINT('Ctrl Pts',(-0.712314141850511,16.7693165934297,
-12.));
#32573=CARTESIAN_POINT('Ctrl Pts',(-1.59035350544452,16.7320199121783,-3.99999999999998));
#32574=CARTESIAN_POINT('Ctrl Pts',(-2.4654486875042,16.6256211127011,3.99999999999999));
#32575=CARTESIAN_POINT('Ctrl Pts',(-3.32684344313022,16.4514279973581,12.));
#32576=CARTESIAN_POINT('Ctrl Pts',(-0.739569257475053,17.4109571784546,
-12.));
#32577=CARTESIAN_POINT('Ctrl Pts',(-1.65120484353838,17.3722334226862,-4.));
#32578=CARTESIAN_POINT('Ctrl Pts',(-2.55978359551225,17.2617635099015,4.));
#32579=CARTESIAN_POINT('Ctrl Pts',(-3.45413770472063,17.0809052826075,12.));
#32580=CARTESIAN_POINT('Ctrl Pts',(-0.657803912377567,15.4860354448028,
-11.9999999914697));
#32581=CARTESIAN_POINT('Ctrl Pts',(-0.860473336502316,15.4774266129281,
-10.0004173920443));
#32582=CARTESIAN_POINT('Ctrl Pts',(-1.06300270545654,15.4648379845811,-8.00054577305927));
#32583=CARTESIAN_POINT('Ctrl Pts',(-1.26527523936852,15.4482710543491,-5.99999995642121));
#32584=CARTESIAN_POINT('Ctrl Pts',(-1.46749908351692,15.4317081120036,-3.99993569850461));
#32585=CARTESIAN_POINT('Ctrl Pts',(-1.66937848149492,15.4111759584542,-2.00006422723887));
#32586=CARTESIAN_POINT('Ctrl Pts',(-1.87079645983396,15.3866864725929,1.8314671836973E-24));
#32587=CARTESIAN_POINT('Ctrl Pts',(-2.072214438173,15.3621969867316,2.00006422723887));
#32588=CARTESIAN_POINT('Ctrl Pts',(-2.2731321034333,15.3337548974327,3.99993569850461));
#32589=CARTESIAN_POINT('Ctrl Pts',(-2.47343304368529,15.301376702062,5.99999995642121));
#32590=CARTESIAN_POINT('Ctrl Pts',(-2.67381106285918,15.2689860470573,8.00083387021915));
#32591=CARTESIAN_POINT('Ctrl Pts',(-2.87345607543091,15.2326749819658,10.0007056240913));
#32592=CARTESIAN_POINT('Ctrl Pts',(-3.07225491560408,15.192473427738,11.9999999562994));
#32593=CARTESIAN_POINT('Origin',(2.22044604925031E-15,-4.16333634234434E-16,
-6.));
#32594=CARTESIAN_POINT('Origin',(2.22044604925031E-15,-4.16333634234434E-16,
-6.));
#32595=CARTESIAN_POINT('Ctrl Pts',(-0.559244210621343,15.4899078445247,
11.9999999562994));
#32596=CARTESIAN_POINT('Ctrl Pts',(-0.356553333306831,15.4972257725099,
10.0007056240913));
#32597=CARTESIAN_POINT('Ctrl Pts',(-0.153660607486406,15.5005673742223,
8.00083387021916));
#32598=CARTESIAN_POINT('Ctrl Pts',(0.0493174405869389,15.499921541416,5.99999995642122));
#32599=CARTESIAN_POINT('Ctrl Pts',(0.252217409591649,15.4992759570407,3.99993569850462));
#32600=CARTESIAN_POINT('Ctrl Pts',(0.455085414960353,15.4946463722799,2.00006422723887));
#32601=CARTESIAN_POINT('Ctrl Pts',(0.657803911807549,15.4860354517744,-2.22030256841817E-15));
#32602=CARTESIAN_POINT('Ctrl Pts',(0.860522408654744,15.4774245312688,-2.00006422723887));
#32603=CARTESIAN_POINT('Ctrl Pts',(1.06305225241292,15.4648339377712,-3.99993569850461));
#32604=CARTESIAN_POINT('Ctrl Pts',(1.26527609564327,15.4482709842168,-5.99999995642121));
#32605=CARTESIAN_POINT('Ctrl Pts',(1.46754862863696,15.4317040427731,-8.00054577305927));
#32606=CARTESIAN_POINT('Ctrl Pts',(1.66942723837633,15.4111700275214,-10.0004173920443));
#32607=CARTESIAN_POINT('Ctrl Pts',(1.87079645813716,15.3866864658071,-11.9999999914697));
#32608=CARTESIAN_POINT('Ctrl Pts',(4.67840257433451,14.7770954003634,-12.));
#32609=CARTESIAN_POINT('Ctrl Pts',(3.90467566848156,15.0220559863311,-4.));
#32610=CARTESIAN_POINT('Ctrl Pts',(3.11167798341369,15.2061210786984,4.));
#32611=CARTESIAN_POINT('Ctrl Pts',(2.30915666147617,15.3270282387598,12.));
#32612=CARTESIAN_POINT('Ctrl Pts',(4.87224514815724,15.3893621218603,-12.));
#32613=CARTESIAN_POINT('Ctrl Pts',(4.06646003173275,15.6444722812593,-4.));
#32614=CARTESIAN_POINT('Ctrl Pts',(3.240605680342,15.8361638338742,4.));
#32615=CARTESIAN_POINT('Ctrl Pts',(2.40483309451253,15.9620806002547,12.));
#32616=CARTESIAN_POINT('Ctrl Pts',(5.06608772197997,16.0016288433572,-12.));
#32617=CARTESIAN_POINT('Ctrl Pts',(4.22824439498395,16.2668885761874,-4.));
#32618=CARTESIAN_POINT('Ctrl Pts',(3.36953337727032,16.4662065890499,4.));
#32619=CARTESIAN_POINT('Ctrl Pts',(2.50050952754889,16.5971329617496,12.));
#32620=CARTESIAN_POINT('Ctrl Pts',(5.25993029580271,16.6138955648541,-12.));
#32621=CARTESIAN_POINT('Ctrl Pts',(4.39002875823515,16.8893048711156,-4.));
#32622=CARTESIAN_POINT('Ctrl Pts',(3.49846107419863,17.0962493442257,4.));
#32623=CARTESIAN_POINT('Ctrl Pts',(2.59618596058525,17.2321853232445,12.));
#32624=CARTESIAN_POINT('Ctrl Pts',(4.67840257999254,14.7770954211018,-11.9999999914697));
#32625=CARTESIAN_POINT('Ctrl Pts',(4.48501122377193,14.8383227908024,-10.0004173920443));
#32626=CARTESIAN_POINT('Ctrl Pts',(4.29039030580173,14.8957624734364,-8.00054577305927));
#32627=CARTESIAN_POINT('Ctrl Pts',(4.09465007444455,14.9493759323877,-5.99999995642121));
#32628=CARTESIAN_POINT('Ctrl Pts',(3.89895696043642,15.0029764858466,-3.99993569850461));
#32629=CARTESIAN_POINT('Ctrl Pts',(3.70222996976807,15.0527293932983,-2.00006422723887));
#32630=CARTESIAN_POINT('Ctrl Pts',(3.50458308436498,15.0986058099674,8.88178419700125E-15));
#32631=CARTESIAN_POINT('Ctrl Pts',(3.30693619896189,15.1444822266365,2.00006422723889));
#32632=CARTESIAN_POINT('Ctrl Pts',(3.10840758407279,15.1864732938717,3.99993569850461));
#32633=CARTESIAN_POINT('Ctrl Pts',(2.90911227356018,15.2245546989007,5.99999995642121));
#32634=CARTESIAN_POINT('Ctrl Pts',(2.70974027110769,15.2626507582476,8.00083387021915));
#32635=CARTESIAN_POINT('Ctrl Pts',(2.50971621033041,15.2968121341423,10.0007056240913));
#32636=CARTESIAN_POINT('Ctrl Pts',(2.30915666586,15.3270282380994,11.9999999562994));
#32637=CARTESIAN_POINT('Ctrl Pts',(5.10435222255114,16.662350757064,-10.5713320220547));
#32638=CARTESIAN_POINT('Ctrl Pts',(4.33577922443239,16.8977823962929,-3.52377734068488));
#32639=CARTESIAN_POINT('Ctrl Pts',(3.55089819699268,17.0799635066964,3.52377734068489));
#32640=CARTESIAN_POINT('Ctrl Pts',(2.75720126686291,17.2071550680903,10.5713320220547));
#32641=CARTESIAN_POINT('Ctrl Pts',(2.1033373682508,17.299259072917,-12.));
#32642=CARTESIAN_POINT('Ctrl Pts',(1.19755028131709,17.4093895599857,-4.));
#32643=CARTESIAN_POINT('Ctrl Pts',(0.283105004950508,17.4482326636193,4.));
#32644=CARTESIAN_POINT('Ctrl Pts',(-0.628758543704754,17.4153109432562,
12.));
#32645=CARTESIAN_POINT('Ctrl Pts',(2.02582373096846,16.6617348634049,-12.));
#32646=CARTESIAN_POINT('Ctrl Pts',(1.15341733358623,16.7678067459162,-4.00000000000002));
#32647=CARTESIAN_POINT('Ctrl Pts',(0.27267182433108,16.8052183767432,4.00000000000002));
#32648=CARTESIAN_POINT('Ctrl Pts',(-0.605587100820421,16.7735099102924,
12.));
#32649=CARTESIAN_POINT('Ctrl Pts',(1.94831009368611,16.0242106538928,-12.));
#32650=CARTESIAN_POINT('Ctrl Pts',(1.10928438585537,16.1262239318468,-3.99999999999998));
#32651=CARTESIAN_POINT('Ctrl Pts',(0.262238643711656,16.162204089867,3.99999999999999));
#32652=CARTESIAN_POINT('Ctrl Pts',(-0.582415657936089,16.1317088773286,
12.));
#32653=CARTESIAN_POINT('Ctrl Pts',(1.87079645640377,15.3866864443807,-12.));
#32654=CARTESIAN_POINT('Ctrl Pts',(1.0651514381245,15.4846411177773,-4.));
#32655=CARTESIAN_POINT('Ctrl Pts',(0.251805463092228,15.5191898029909,4.));
#32656=CARTESIAN_POINT('Ctrl Pts',(-0.559244215051757,15.4899078443647,
12.));
#32657=CARTESIAN_POINT('Ctrl Pts',(5.10435255326647,16.6623520957364,-10.5713320279724));
#32658=CARTESIAN_POINT('Ctrl Pts',(4.33578260855181,16.8977961637243,-3.52377734265748));
#32659=CARTESIAN_POINT('Ctrl Pts',(3.5509012234375,17.0799773571509,3.52377734265749));
#32660=CARTESIAN_POINT('Ctrl Pts',(2.75720155972776,17.2071564155546,10.5713320279724));
#32661=CARTESIAN_POINT('Ctrl Pts',(5.10446210897357,16.6627197582901,-10.5713320279724));
#32662=CARTESIAN_POINT('Ctrl Pts',(4.33587520540538,16.8981688796597,-3.52377734265747));
#32663=CARTESIAN_POINT('Ctrl Pts',(3.55097651134477,17.0803539511987,3.52377734265748));
#32664=CARTESIAN_POINT('Ctrl Pts',(2.75725935384223,17.2075356754217,10.5713320279724));
#32665=CARTESIAN_POINT('Ctrl Pts',(5.10457166468936,16.6630874208762,-10.5713320279724));
#32666=CARTESIAN_POINT('Ctrl Pts',(4.33596780226612,16.8985415956278,-3.52377734265749));
#32667=CARTESIAN_POINT('Ctrl Pts',(3.55105179925777,17.0807305452793,3.5237773426575));
#32668=CARTESIAN_POINT('Ctrl Pts',(2.75731714796087,17.2079149353218,10.5713320279724));
#32669=CARTESIAN_POINT('Ctrl Pts',(5.10468122040587,16.6634550834647,-10.5713320279724));
#32670=CARTESIAN_POINT('Ctrl Pts',(4.33606039912754,16.8989143115984,-3.52377734265748));
#32671=CARTESIAN_POINT('Ctrl Pts',(3.55112708717116,17.0811071393627,3.52377734265749));
#32672=CARTESIAN_POINT('Ctrl Pts',(2.75737494207986,17.2082941952246,10.5713320279724));
#32673=CARTESIAN_POINT('Ctrl Pts',(7.89318567151549,15.5366023477324,-12.));
#32674=CARTESIAN_POINT('Ctrl Pts',(7.07969107489245,15.94988858305,-4.));
#32675=CARTESIAN_POINT('Ctrl Pts',(6.23367872045024,16.2991478653893,4.));
#32676=CARTESIAN_POINT('Ctrl Pts',(5.36554738109813,16.5800872693051,12.));
#32677=CARTESIAN_POINT('Ctrl Pts',(7.60230055704008,14.9640367778145,-12.));
#32678=CARTESIAN_POINT('Ctrl Pts',(6.81878542355292,15.3620923041542,-4.00000000000001));
#32679=CARTESIAN_POINT('Ctrl Pts',(6.00395089905301,15.6984804428827,4.00000000000001));
#32680=CARTESIAN_POINT('Ctrl Pts',(5.16781253370865,15.9690664743998,12.));
#32681=CARTESIAN_POINT('Ctrl Pts',(7.31141544256466,14.3914712078966,-12.));
#32682=CARTESIAN_POINT('Ctrl Pts',(6.55787977221338,14.7742960252583,-4.));
#32683=CARTESIAN_POINT('Ctrl Pts',(5.77422307765577,15.0978130203761,3.99999999999999));
#32684=CARTESIAN_POINT('Ctrl Pts',(4.97007768631916,15.3580456794946,12.));
#32685=CARTESIAN_POINT('Ctrl Pts',(7.02053032808925,13.8189056379787,-12.));
#32686=CARTESIAN_POINT('Ctrl Pts',(6.29697412087384,14.1864997463625,-4.));
#32687=CARTESIAN_POINT('Ctrl Pts',(5.54449525625854,14.4971455978694,4.));
#32688=CARTESIAN_POINT('Ctrl Pts',(4.77234283892968,14.7470248845893,12.));
#32689=CARTESIAN_POINT('Ctrl Pts',(4.77234284314764,14.7470248832244,11.9999999562994));
#32690=CARTESIAN_POINT('Ctrl Pts',(4.96531284363905,14.6845771232416,10.0007056240913));
#32691=CARTESIAN_POINT('Ctrl Pts',(5.15711253600028,14.6183238025476,8.00083387021916));
#32692=CARTESIAN_POINT('Ctrl Pts',(5.34762862212736,14.5482943371312,5.99999995642122));
#32693=CARTESIAN_POINT('Ctrl Pts',(5.53807142289819,14.4782918097778,3.99993569850461));
#32694=CARTESIAN_POINT('Ctrl Pts',(5.72712157929327,14.4045564788684,2.00006422723889));
#32695=CARTESIAN_POINT('Ctrl Pts',(5.91466954661191,14.3271310510647,-2.22058953008253E-15));
#32696=CARTESIAN_POINT('Ctrl Pts',(6.10221751393055,14.249705623261,-2.00006422723888));
#32697=CARTESIAN_POINT('Ctrl Pts',(6.28822707700645,14.1686050492701,-3.9999356985046));
#32698=CARTESIAN_POINT('Ctrl Pts',(6.47259046648839,14.0838763361911,-5.99999995642121));
#32699=CARTESIAN_POINT('Ctrl Pts',(6.6569982454432,13.9991272228421,-8.00054577305927));
#32700=CARTESIAN_POINT('Ctrl Pts',(6.83967903847032,13.9107850091975,-10.0004173920443));
#32701=CARTESIAN_POINT('Ctrl Pts',(7.0205303370464,13.8189056575201,-11.9999999914697));
#32702=CARTESIAN_POINT('Ctrl Pts',(9.4503246629373,12.2858195853618,-12.));
#32703=CARTESIAN_POINT('Ctrl Pts',(8.8070406537256,12.7806374276138,-4.));
#32704=CARTESIAN_POINT('Ctrl Pts',(8.12482055003974,13.2248232185595,4.));
#32705=CARTESIAN_POINT('Ctrl Pts',(7.41204987000498,13.6129172422203,12.));
#32706=CARTESIAN_POINT('Ctrl Pts',(9.84188465099258,12.7948640406238,-12.));
#32707=CARTESIAN_POINT('Ctrl Pts',(9.17194713643085,13.3101839159077,-4.));
#32708=CARTESIAN_POINT('Ctrl Pts',(8.4614602688847,13.7727738769957,4.));
#32709=CARTESIAN_POINT('Ctrl Pts',(7.71915700781016,14.1769479927898,12.));
#32710=CARTESIAN_POINT('Ctrl Pts',(10.2334446390479,13.3039084958857,-12.));
#32711=CARTESIAN_POINT('Ctrl Pts',(9.53685361913611,13.8397304042016,-4.00000000000001));
#32712=CARTESIAN_POINT('Ctrl Pts',(8.79809998772967,14.3207245354319,4.00000000000001));
#32713=CARTESIAN_POINT('Ctrl Pts',(8.02626414561533,14.7409787433592,12.));
#32714=CARTESIAN_POINT('Ctrl Pts',(10.6250046271031,13.8129529511477,-12.));
#32715=CARTESIAN_POINT('Ctrl Pts',(9.90176010184136,14.3692768924954,-4.));
#32716=CARTESIAN_POINT('Ctrl Pts',(9.13473970657463,14.8686751938681,4.));
#32717=CARTESIAN_POINT('Ctrl Pts',(8.3333712834205,15.3050094939286,12.));
#32718=CARTESIAN_POINT('Ctrl Pts',(9.45032467534708,12.2858196029144,-11.9999999914697));
#32719=CARTESIAN_POINT('Ctrl Pts',(9.28953723874319,12.4094982497846,-10.0004173920443));
#32720=CARTESIAN_POINT('Ctrl Pts',(9.12629892676312,12.5300381699545,-8.00054577305927));
#32721=CARTESIAN_POINT('Ctrl Pts',(8.96070015868055,12.6473654436892,-5.99999995642121));
#32722=CARTESIAN_POINT('Ctrl Pts',(8.79514125248487,12.7646644751455,-3.9999356985046));
#32723=CARTESIAN_POINT('Ctrl Pts',(8.62729484758191,12.8787015086849,-2.00006422723888));
#32724=CARTESIAN_POINT('Ctrl Pts',(8.45725818645174,12.9894104549704,-2.22044604925031E-15));
#32725=CARTESIAN_POINT('Ctrl Pts',(8.28722152532158,13.1001194012559,2.00006422723888));
#32726=CARTESIAN_POINT('Ctrl Pts',(8.11502744172963,13.2074788825944,3.9999356985046));
#32727=CARTESIAN_POINT('Ctrl Pts',(7.94077571668976,13.311426708555,5.99999995642122));
#32728=CARTESIAN_POINT('Ctrl Pts',(7.76645693687179,13.4154145352581,8.00083387021915));
#32729=CARTESIAN_POINT('Ctrl Pts',(7.59017968165941,13.5159279860378,10.0007056240913));
#32730=CARTESIAN_POINT('Ctrl Pts',(7.41204987389855,13.6129172401003,11.9999999562994));
#32731=CARTESIAN_POINT('Ctrl Pts',(10.4953817114971,13.9116967726179,-10.5713320220547));
#32732=CARTESIAN_POINT('Ctrl Pts',(9.85368169962204,14.3957975936737,-3.52377734068489));
#32733=CARTESIAN_POINT('Ctrl Pts',(9.17844439943351,14.8354369602649,3.52377734068489));
#32734=CARTESIAN_POINT('Ctrl Pts',(8.47611532710788,15.2264182697331,10.5713320220547));
#32735=CARTESIAN_POINT('Ctrl Pts',(10.4953824801207,13.9116979174471,-10.5713320279724));
#32736=CARTESIAN_POINT('Ctrl Pts',(9.85368958839295,14.3958093733904,-3.52377734265747));
#32737=CARTESIAN_POINT('Ctrl Pts',(9.1784519804958,14.8354489403297,3.52377734265748));
#32738=CARTESIAN_POINT('Ctrl Pts',(8.47611606317077,15.2264194357697,10.5713320279724));
#32739=CARTESIAN_POINT('Ctrl Pts',(10.4956111768049,13.912005936971,-10.5713320279724));
#32740=CARTESIAN_POINT('Ctrl Pts',(9.85390407732624,14.3961279418089,-3.52377734265748));
#32741=CARTESIAN_POINT('Ctrl Pts',(9.17865153073284,14.8357770729899,3.52377734265748));
#32742=CARTESIAN_POINT('Ctrl Pts',(8.47630008638401,15.22675605671,10.5713320279724));
#32743=CARTESIAN_POINT('Ctrl Pts',(10.4958398735083,13.9123139565221,-10.5713320279724));
#32744=CARTESIAN_POINT('Ctrl Pts',(9.85411856627743,14.3964465102557,-3.52377734265747));
#32745=CARTESIAN_POINT('Ctrl Pts',(9.17885108098651,14.8361052056791,3.52377734265748));
#32746=CARTESIAN_POINT('Ctrl Pts',(8.47648410961248,15.22709267768,10.5713320279724));
#32747=CARTESIAN_POINT('Ctrl Pts',(10.4960685702133,13.9126219760754,-10.5713320279724));
#32748=CARTESIAN_POINT('Ctrl Pts',(9.85433305523014,14.3967650787046,-3.52377734265747));
#32749=CARTESIAN_POINT('Ctrl Pts',(9.17905063124145,14.8364333383706,3.52377734265748));
#32750=CARTESIAN_POINT('Ctrl Pts',(8.47666813284218,15.2274292986523,10.5713320279724));
#32751=CARTESIAN_POINT('Origin',(2.22044604925031E-15,-4.16333634234434E-16,
-6.));
#32752=CARTESIAN_POINT('Ctrl Pts',(9.52831491775384,12.2254330780995,11.9999999562994));
#32753=CARTESIAN_POINT('Ctrl Pts',(9.68828901142903,12.1007517516335,10.0007056240913));
#32754=CARTESIAN_POINT('Ctrl Pts',(9.84586179677031,11.9728946368036,8.00083387021915));
#32755=CARTESIAN_POINT('Ctrl Pts',(10.0009368692462,11.8419281258312,5.99999995642121));
#32756=CARTESIAN_POINT('Ctrl Pts',(10.1559522893738,11.7110119934259,3.99993569850462));
#32757=CARTESIAN_POINT('Ctrl Pts',(10.3083823578509,11.5770644854931,2.00006422723886));
#32758=CARTESIAN_POINT('Ctrl Pts',(10.4581387428691,11.440163199662,-6.66133814775096E-15));
#32759=CARTESIAN_POINT('Ctrl Pts',(10.6078951278873,11.3032619138309,-2.0000642272389));
#32760=CARTESIAN_POINT('Ctrl Pts',(10.7549489117653,11.1634332854871,-3.9999356985046));
#32761=CARTESIAN_POINT('Ctrl Pts',(10.8992149018134,11.0207583461433,-5.99999995642121));
#32762=CARTESIAN_POINT('Ctrl Pts',(11.0435156270184,10.8780490547226,-8.00054577305927));
#32763=CARTESIAN_POINT('Ctrl Pts',(11.1849646036129,10.732554017443,-10.0004173920443));
#32764=CARTESIAN_POINT('Ctrl Pts',(11.323484645315,10.5843608816095,-11.9999999914697));
#32765=CARTESIAN_POINT('Ctrl Pts',(12.7309992917815,11.9000020835813,-12.));
#32766=CARTESIAN_POINT('Ctrl Pts',(12.1079166397235,12.5665956477133,-4.));
#32767=CARTESIAN_POINT('Ctrl Pts',(11.432378782964,13.1841452847902,4.));
#32768=CARTESIAN_POINT('Ctrl Pts',(10.7126891046949,13.7450603746485,12.));
#32769=CARTESIAN_POINT('Ctrl Pts',(12.2618277379259,11.4614550111576,-12.));
#32770=CARTESIAN_POINT('Ctrl Pts',(11.6617073568841,12.1034828101751,-3.99999999999999));
#32771=CARTESIAN_POINT('Ctrl Pts',(11.011064886471,12.6982740827144,3.99999999999999));
#32772=CARTESIAN_POINT('Ctrl Pts',(10.3178977078823,13.238517943374,12.));
#32773=CARTESIAN_POINT('Ctrl Pts',(11.7926561840702,11.0229079387338,-12.));
#32774=CARTESIAN_POINT('Ctrl Pts',(11.2154980740448,11.6403699726369,-4.00000000000001));
#32775=CARTESIAN_POINT('Ctrl Pts',(10.589750989978,12.2124028806386,4.00000000000001));
#32776=CARTESIAN_POINT('Ctrl Pts',(9.92310631106972,12.7319755120994,12.));
#32777=CARTESIAN_POINT('Ctrl Pts',(11.3234846302145,10.5843608663101,-12.));
#32778=CARTESIAN_POINT('Ctrl Pts',(10.7692887912054,11.1772571350987,-4.));
#32779=CARTESIAN_POINT('Ctrl Pts',(10.168437093485,11.7265316785628,4.));
#32780=CARTESIAN_POINT('Ctrl Pts',(9.52831491425713,12.2254330808248,12.));
#32781=CARTESIAN_POINT('Ctrl Pts',(14.6205143845238,9.48308765551917,-10.5713320279724));
#32782=CARTESIAN_POINT('Ctrl Pts',(14.1830961789038,10.1574755131067,-3.52377734265748));
#32783=CARTESIAN_POINT('Ctrl Pts',(13.6989459691819,10.801546433397,3.52377734265748));
#32784=CARTESIAN_POINT('Ctrl Pts',(13.1726858752452,11.4091515540133,10.5713320279724));
#32785=CARTESIAN_POINT('Ctrl Pts',(14.6208346379986,9.48329888032434,-10.5713320279724));
#32786=CARTESIAN_POINT('Ctrl Pts',(14.1834066893941,10.1577015099677,-3.52377734265748));
#32787=CARTESIAN_POINT('Ctrl Pts',(13.6992457130527,10.8017865270407,3.52377734265748));
#32788=CARTESIAN_POINT('Ctrl Pts',(13.1729739316488,11.4094049345862,10.5713320279724));
#32789=CARTESIAN_POINT('Ctrl Pts',(14.6211548915007,9.48351010514861,-10.5713320279724));
#32790=CARTESIAN_POINT('Ctrl Pts',(14.1837171999109,10.1579275068491,-3.52377734265747));
#32791=CARTESIAN_POINT('Ctrl Pts',(13.699545456949,10.8020266207058,3.52377734265748));
#32792=CARTESIAN_POINT('Ctrl Pts',(13.1732619880769,11.4096583151819,10.5713320279724));
#32793=CARTESIAN_POINT('Ctrl Pts',(14.621475145005,9.48372132997438,-10.5713320279724));
#32794=CARTESIAN_POINT('Ctrl Pts',(14.1840277104299,10.1581535037321,-3.52377734265748));
#32795=CARTESIAN_POINT('Ctrl Pts',(13.6998452008473,10.8022667143728,3.52377734265748));
#32796=CARTESIAN_POINT('Ctrl Pts',(13.173550044507,11.4099116957793,10.5713320279724));
#32797=CARTESIAN_POINT('Ctrl Pts',(14.6205132701638,9.48308684344182,-10.5713320134285));
#32798=CARTESIAN_POINT('Ctrl Pts',(14.183084736767,10.1574671421628,-3.52377733780948));
#32799=CARTESIAN_POINT('Ctrl Pts',(13.6989347480705,10.8015377684169,3.52377733780958));
#32800=CARTESIAN_POINT('Ctrl Pts',(13.1726847854084,11.4091507093019,10.5713320134286));
#32801=CARTESIAN_POINT('Ctrl Pts',(13.082398125252,8.31269260897954,-12.));
#32802=CARTESIAN_POINT('Ctrl Pts',(12.6471465580533,8.99768537300669,-4.));
#32803=CARTESIAN_POINT('Ctrl Pts',(12.1579898487504,9.64841650065859,4.));
#32804=CARTESIAN_POINT('Ctrl Pts',(11.6209404740055,10.2568875210076,12.));
#32805=CARTESIAN_POINT('Ctrl Pts',(13.6244476141704,8.65711652400593,-12.));
#32806=CARTESIAN_POINT('Ctrl Pts',(13.1711620529523,9.37049093290421,-4.));
#32807=CARTESIAN_POINT('Ctrl Pts',(12.6617378711462,10.0481841260574,3.99999999999999));
#32808=CARTESIAN_POINT('Ctrl Pts',(12.1024366633415,10.6818662279256,12.));
#32809=CARTESIAN_POINT('Ctrl Pts',(14.1664971030888,9.00154043903231,-12.));
#32810=CARTESIAN_POINT('Ctrl Pts',(13.6951775478512,9.74329649280173,-4.00000000000002));
#32811=CARTESIAN_POINT('Ctrl Pts',(13.165485893542,10.4479517514562,4.00000000000001));
#32812=CARTESIAN_POINT('Ctrl Pts',(12.5839328526776,11.1068449348435,12.));
#32813=CARTESIAN_POINT('Ctrl Pts',(14.7085465920072,9.3459643540587,-12.));
#32814=CARTESIAN_POINT('Ctrl Pts',(14.2191930427502,10.1161020526992,-4.));
#32815=CARTESIAN_POINT('Ctrl Pts',(13.6692339159378,10.847719376855,4.));
#32816=CARTESIAN_POINT('Ctrl Pts',(13.0654290420136,11.5318236417615,12.));
#32817=CARTESIAN_POINT('Ctrl Pts',(13.0823981429167,8.31269262122918,-11.9999999914697));
#32818=CARTESIAN_POINT('Ctrl Pts',(12.9736079637539,8.48390507515421,-10.0004173920443));
#32819=CARTESIAN_POINT('Ctrl Pts',(12.8614412073296,8.65300633950756,-8.00054577305927));
#32820=CARTESIAN_POINT('Ctrl Pts',(12.7459575579299,8.81989602724713,-5.99999995642121));
#32821=CARTESIAN_POINT('Ctrl Pts',(12.630501707023,8.98674554235783,-3.99993569850462));
#32822=CARTESIAN_POINT('Ctrl Pts',(12.5117806414659,9.1513121527328,-2.00006422723887));
#32823=CARTESIAN_POINT('Ctrl Pts',(12.3898631354148,9.31350049582264,-1.43482765123828E-19));
#32824=CARTESIAN_POINT('Ctrl Pts',(12.2679456293637,9.47568883891247,2.00006422723888));
#32825=CARTESIAN_POINT('Ctrl Pts',(12.1428552248642,9.63546759644758,3.9999356985046));
#32826=CARTESIAN_POINT('Ctrl Pts',(12.0146644150184,9.79274420142234,5.99999995642121));
#32827=CARTESIAN_POINT('Ctrl Pts',(11.8864242753522,9.95008132888459,8.00083387021915));
#32828=CARTESIAN_POINT('Ctrl Pts',(11.7551554642586,10.1048234489648,10.0007056240913));
#32829=CARTESIAN_POINT('Ctrl Pts',(11.6209404769392,10.2568875176838,11.9999999562994));
#32830=CARTESIAN_POINT('Origin',(2.22044604925031E-15,-4.16333634234434E-16,
-6.));
#32831=CARTESIAN_POINT('Origin',(2.22044604925031E-15,-4.16333634234434E-16,
-6.));
#32832=CARTESIAN_POINT('Ctrl Pts',(13.1350315903275,8.2292736155798,11.9999999562994));
#32833=CARTESIAN_POINT('Ctrl Pts',(13.2427145405231,8.05739713070271,10.0007056240913));
#32834=CARTESIAN_POINT('Ctrl Pts',(13.3470548154056,7.88335767675537,8.00083387021915));
#32835=CARTESIAN_POINT('Ctrl Pts',(13.4479845318255,7.70725061431013,5.99999995642122));
#32836=CARTESIAN_POINT('Ctrl Pts',(13.5488754238585,7.53121129453729,3.99993569850461));
#32837=CARTESIAN_POINT('Ctrl Pts',(13.646300088531,7.35320765589252,2.00006422723887));
#32838=CARTESIAN_POINT('Ctrl Pts',(13.7402020610468,7.17334282755306,-6.66133814775094E-15));
#32839=CARTESIAN_POINT('Ctrl Pts',(13.8341040335626,6.9934779992136,-2.00006422723889));
#32840=CARTESIAN_POINT('Ctrl Pts',(13.9244651816241,6.81178671274576,-3.9999356985046));
#32841=CARTESIAN_POINT('Ctrl Pts',(14.0112331646994,6.62837425048013,-5.99999995642121));
#32842=CARTESIAN_POINT('Ctrl Pts',(14.098022039043,6.44491762769792,-8.00054577305927));
#32843=CARTESIAN_POINT('Ctrl Pts',(14.181178365063,6.25981861555709,-10.0004173920443));
#32844=CARTESIAN_POINT('Ctrl Pts',(14.2606595885237,6.07318597484681,-11.9999999914697));
#32845=CARTESIAN_POINT('Ctrl Pts',(15.1365412980281,3.33693222167749,-12.));
#32846=CARTESIAN_POINT('Ctrl Pts',(14.9618199354756,4.12947967072155,-4.));
#32847=CARTESIAN_POINT('Ctrl Pts',(14.7247261388817,4.90826835731624,4.));
#32848=CARTESIAN_POINT('Ctrl Pts',(14.4281741500255,5.66372578922348,12.));
#32849=CARTESIAN_POINT('Ctrl Pts',(15.7637011196476,3.4751929891605,-12.));
#32850=CARTESIAN_POINT('Ctrl Pts',(15.5817404402384,4.300578449675,-3.99999999999999));
#32851=CARTESIAN_POINT('Ctrl Pts',(15.3348230187984,5.11163507411277,3.99999999999999));
#32852=CARTESIAN_POINT('Ctrl Pts',(15.0259838443316,5.89839374841796,12.));
#32853=CARTESIAN_POINT('Ctrl Pts',(16.3908609412671,3.61345375664351,-12.));
#32854=CARTESIAN_POINT('Ctrl Pts',(16.2016609450012,4.47167722862846,-4.00000000000001));
#32855=CARTESIAN_POINT('Ctrl Pts',(15.9449198987151,5.31500179090931,4.00000000000001));
#32856=CARTESIAN_POINT('Ctrl Pts',(15.6237935386377,6.13306170761243,12.));
#32857=CARTESIAN_POINT('Ctrl Pts',(17.0180207628866,3.75171452412652,-12.));
#32858=CARTESIAN_POINT('Ctrl Pts',(16.8215814497639,4.64277600758191,-4.));
#32859=CARTESIAN_POINT('Ctrl Pts',(16.5550167786318,5.51836850770584,4.));
#32860=CARTESIAN_POINT('Ctrl Pts',(16.2216032329437,6.36772966680691,12.));
#32861=CARTESIAN_POINT('Ctrl Pts',(15.1365413188172,3.33693222714671,-11.9999999914697));
#32862=CARTESIAN_POINT('Ctrl Pts',(15.0928700982745,3.53502773935638,-10.0004173920443));
#32863=CARTESIAN_POINT('Ctrl Pts',(15.0453038636357,3.73229423974341,-8.00054577305927));
#32864=CARTESIAN_POINT('Ctrl Pts',(14.9938643653936,3.92861698211701,-5.99999995642121));
#32865=CARTESIAN_POINT('Ctrl Pts',(14.9424372493419,4.12489246692319,-3.99993569850461));
#32866=CARTESIAN_POINT('Ctrl Pts',(14.8871610357731,4.32013949217793,-2.00006422723889));
#32867=CARTESIAN_POINT('Ctrl Pts',(14.8280677353416,4.51424492425044,-6.66133814775094E-15));
#32868=CARTESIAN_POINT('Ctrl Pts',(14.7689744349101,4.70835035632295,2.00006422723887));
#32869=CARTESIAN_POINT('Ctrl Pts',(14.7060754584233,4.90127671381265,3.9999356985046));
#32870=CARTESIAN_POINT('Ctrl Pts',(14.6394072673339,5.09291221808618,5.99999995642121));
#32871=CARTESIAN_POINT('Ctrl Pts',(14.5727134212861,5.28462146668684,8.00083387021915));
#32872=CARTESIAN_POINT('Ctrl Pts',(14.5022860102504,5.47492807263538,10.0007056240913));
#32873=CARTESIAN_POINT('Ctrl Pts',(14.4281741516455,5.66372578509675,11.9999999562994));
#32874=CARTESIAN_POINT('Ctrl Pts',(16.9821951536599,3.91067668393918,-10.5713320220547));
#32875=CARTESIAN_POINT('Ctrl Pts',(16.8017984350274,4.69399624458723,-3.52377734068488));
#32876=CARTESIAN_POINT('Ctrl Pts',(16.5671313910066,5.46481370850019,3.52377734068489));
#32877=CARTESIAN_POINT('Ctrl Pts',(16.2804340492558,6.21577119359523,10.5713320220547));
#32878=CARTESIAN_POINT('Ctrl Pts',(16.03326650792,6.82808594282421,-12.));
#32879=CARTESIAN_POINT('Ctrl Pts',(15.6757487639857,7.66758581406302,-4.));
#32880=CARTESIAN_POINT('Ctrl Pts',(15.252165240311,8.478940205584,4.));
#32881=CARTESIAN_POINT('Ctrl Pts',(14.7677224198127,9.25217634332295,12.));
#32882=CARTESIAN_POINT('Ctrl Pts',(15.4423975283137,6.5764526170944,-12.));
#32883=CARTESIAN_POINT('Ctrl Pts',(15.0980552745046,7.38501466090712,-4.00000000000002));
#32884=CARTESIAN_POINT('Ctrl Pts',(14.6900819425702,8.16646846160462,4.00000000000002));
#32885=CARTESIAN_POINT('Ctrl Pts',(14.223492142533,8.91120876866085,12.));
#32886=CARTESIAN_POINT('Ctrl Pts',(14.8515285487075,6.32481929136458,-12.));
#32887=CARTESIAN_POINT('Ctrl Pts',(14.5203617850236,7.10244350775122,-3.99999999999999));
#32888=CARTESIAN_POINT('Ctrl Pts',(14.1279986448294,7.85399671762524,3.99999999999999));
#32889=CARTESIAN_POINT('Ctrl Pts',(13.6792618652534,8.57024119399876,12.));
#32890=CARTESIAN_POINT('Ctrl Pts',(14.2606595691012,6.07318596563476,-12.));
#32891=CARTESIAN_POINT('Ctrl Pts',(13.9426682955425,6.81987235459531,-4.));
#32892=CARTESIAN_POINT('Ctrl Pts',(13.5659153470886,7.54152497364586,4.));
#32893=CARTESIAN_POINT('Ctrl Pts',(13.1350315879738,8.22927361933667,12.));
#32894=CARTESIAN_POINT('Ctrl Pts',(16.9821964783418,3.91067706686746,-10.5713320279724));
#32895=CARTESIAN_POINT('Ctrl Pts',(16.8018120500324,4.69400019756955,-3.52377734265747));
#32896=CARTESIAN_POINT('Ctrl Pts',(16.5671448990744,5.46481801274934,3.52377734265748));
#32897=CARTESIAN_POINT('Ctrl Pts',(16.2804353626266,6.215771613699,10.5713320279724));
#32898=CARTESIAN_POINT('Ctrl Pts',(16.982569661307,3.91076602011887,-10.5713320279724));
#32899=CARTESIAN_POINT('Ctrl Pts',(16.8021811299277,4.69410636430973,-3.52377734265748));
#32900=CARTESIAN_POINT('Ctrl Pts',(16.5675086830403,5.46494110853292,3.52377734265749));
#32901=CARTESIAN_POINT('Ctrl Pts',(16.2807927083633,6.21591119246119,10.5713320279724));
#32902=CARTESIAN_POINT('Ctrl Pts',(16.9829428443044,3.91085497337887,-10.5713320279724));
#32903=CARTESIAN_POINT('Ctrl Pts',(16.8025502098547,4.69421253106005,-3.52377734265747));
#32904=CARTESIAN_POINT('Ctrl Pts',(16.5678724670376,5.46506420432801,3.52377734265747));
#32905=CARTESIAN_POINT('Ctrl Pts',(16.2811500541308,6.21605077123634,10.5713320279724));
#32906=CARTESIAN_POINT('Ctrl Pts',(16.9833160273043,3.91094392663953,-10.5713320279724));
#32907=CARTESIAN_POINT('Ctrl Pts',(16.8029192897844,4.69431869781105,-3.52377734265747));
#32908=CARTESIAN_POINT('Ctrl Pts',(16.5682362510374,5.46518730012407,3.52377734265748));
#32909=CARTESIAN_POINT('Ctrl Pts',(16.2815073999007,6.2161903500125,10.5713320279724));
#32910=CARTESIAN_POINT('Ctrl Pts',(17.401685157391,0.93260186554647,-12.));
#32911=CARTESIAN_POINT('Ctrl Pts',(17.3528542378989,1.84375196972217,-4.));
#32912=CARTESIAN_POINT('Ctrl Pts',(17.2323154716912,2.75104980175429,4.));
#32913=CARTESIAN_POINT('Ctrl Pts',(17.0415504627302,3.64334329741251,12.));
#32914=CARTESIAN_POINT('Ctrl Pts',(16.760386271272,0.898232979305968,-12.));
#32915=CARTESIAN_POINT('Ctrl Pts',(16.7133549024554,1.77580475232523,-3.99999999999999));
#32916=CARTESIAN_POINT('Ctrl Pts',(16.5972583138761,2.64966621978703,4.));
#32917=CARTESIAN_POINT('Ctrl Pts',(16.413523508407,3.50907630101261,12.));
#32918=CARTESIAN_POINT('Ctrl Pts',(16.1190873851531,0.863864093065467,-12.));
#32919=CARTESIAN_POINT('Ctrl Pts',(16.0738555670119,1.70785753492828,-4.00000000000001));
#32920=CARTESIAN_POINT('Ctrl Pts',(15.962201156061,2.54828263781977,4.00000000000001));
#32921=CARTESIAN_POINT('Ctrl Pts',(15.7854965540837,3.37480930461272,12.));
#32922=CARTESIAN_POINT('Ctrl Pts',(15.4777884990342,0.829495206824966,-12.));
#32923=CARTESIAN_POINT('Ctrl Pts',(15.4343562315684,1.63991031753134,-4.));
#32924=CARTESIAN_POINT('Ctrl Pts',(15.3271439982459,2.44689905585252,4.));
#32925=CARTESIAN_POINT('Ctrl Pts',(15.1574695997605,3.24054230821282,12.));
#32926=CARTESIAN_POINT('Ctrl Pts',(15.1574696006874,3.24054230387749,11.9999999562994));
#32927=CARTESIAN_POINT('Ctrl Pts',(15.1998732543785,3.04220150129224,10.0007056240913));
#32928=CARTESIAN_POINT('Ctrl Pts',(15.2383960417531,2.84297143492237,8.00083387021915));
#32929=CARTESIAN_POINT('Ctrl Pts',(15.2730067887526,2.64296493179857,5.99999995642122));
#32930=CARTESIAN_POINT('Ctrl Pts',(15.3076042221209,2.44303536468648,3.99993569850461));
#32931=CARTESIAN_POINT('Ctrl Pts',(15.3382726305943,2.24244546120418,2.00006422723887));
#32932=CARTESIAN_POINT('Ctrl Pts',(15.3649942268768,2.04131144317626,-2.22044604741885E-15));
#32933=CARTESIAN_POINT('Ctrl Pts',(15.3917158231593,1.84017742514833,-2.00006422723887));
#32934=CARTESIAN_POINT('Ctrl Pts',(15.4144854473596,1.63853813118233,-3.99993569850461));
#32935=CARTESIAN_POINT('Ctrl Pts',(15.4332899241442,1.43651039582365,-5.99999995642121));
#32936=CARTESIAN_POINT('Ctrl Pts',(15.4520989285132,1.23443401791883,-8.00054577305927));
#32937=CARTESIAN_POINT('Ctrl Pts',(15.466932723784,1.03205670355153,-10.0004173920443));
#32938=CARTESIAN_POINT('Ctrl Pts',(15.4777885204361,0.829495208838567,-11.9999999914697));
#32939=CARTESIAN_POINT('Ctrl Pts',(15.3649941987044,-2.04131143943342,-12.));
#32940=CARTESIAN_POINT('Ctrl Pts',(15.4718770157346,-1.23680222448176,-4.));
#32941=CARTESIAN_POINT('Ctrl Pts',(15.5154431428507,-0.423889388244508,
4.));
#32942=CARTESIAN_POINT('Ctrl Pts',(15.4951570863805,0.387435139568705,12.));
#32943=CARTESIAN_POINT('Ctrl Pts',(16.0016196226445,-2.12589010856384,-12.));
#32944=CARTESIAN_POINT('Ctrl Pts',(16.1129309684345,-1.2880472643632,-3.99999999999999));
#32945=CARTESIAN_POINT('Ctrl Pts',(16.1583021924993,-0.441452607468999,
3.99999999999999));
#32946=CARTESIAN_POINT('Ctrl Pts',(16.1371756137918,0.403487931830613,12.));
#32947=CARTESIAN_POINT('Ctrl Pts',(16.6382450465846,-2.21046877769426,-12.));
#32948=CARTESIAN_POINT('Ctrl Pts',(16.7539849211345,-1.33929230424465,-4.00000000000001));
#32949=CARTESIAN_POINT('Ctrl Pts',(16.801161242148,-0.459015826693489,4.00000000000001));
#32950=CARTESIAN_POINT('Ctrl Pts',(16.7791941412031,0.419540724092521,12.));
#32951=CARTESIAN_POINT('Ctrl Pts',(17.2748704705247,-2.29504744682469,-12.));
#32952=CARTESIAN_POINT('Ctrl Pts',(17.3950388738344,-1.39053734412609,-4.));
#32953=CARTESIAN_POINT('Ctrl Pts',(17.4440202917966,-0.47657904591798,4.));
#32954=CARTESIAN_POINT('Ctrl Pts',(17.4212126686144,0.435593516354429,12.));
#32955=CARTESIAN_POINT('Ctrl Pts',(17.2955736705817,-2.13341879826209,-10.5713320220547));
#32956=CARTESIAN_POINT('Ctrl Pts',(17.3939672736713,-1.33563987584167,-3.52377734068488));
#32957=CARTESIAN_POINT('Ctrl Pts',(17.4370874835488,-0.531047536999956,
3.52377734068489));
#32958=CARTESIAN_POINT('Ctrl Pts',(17.4245226937903,0.272677936184493,10.5713320220547));
#32959=CARTESIAN_POINT('Ctrl Pts',(17.2955750463447,-2.1334188914951,-10.5713320279724));
#32960=CARTESIAN_POINT('Ctrl Pts',(17.3939814195907,-1.33564081785934,-3.52377734265747));
#32961=CARTESIAN_POINT('Ctrl Pts',(17.4371016491204,-0.531048112360096,
3.52377734265748));
#32962=CARTESIAN_POINT('Ctrl Pts',(17.4245240716391,0.272677881753644,10.5713320279724));
#32963=CARTESIAN_POINT('Ctrl Pts',(17.295956147427,-2.13346293887238,-10.5713320279724));
#32964=CARTESIAN_POINT('Ctrl Pts',(17.3943645524084,-1.33566728651567,-3.52377734265748));
#32965=CARTESIAN_POINT('Ctrl Pts',(17.4374855954662,-0.531056861604771,
3.52377734265749));
#32966=CARTESIAN_POINT('Ctrl Pts',(17.4249076055392,0.272686823446403,10.5713320279724));
#32967=CARTESIAN_POINT('Ctrl Pts',(17.2963372485426,-2.13350698625262,-10.5713320279724));
#32968=CARTESIAN_POINT('Ctrl Pts',(17.3947476852595,-1.33569375517339,-3.52377734265746));
#32969=CARTESIAN_POINT('Ctrl Pts',(17.4378695418455,-0.531065610849369,
3.52377734265747));
#32970=CARTESIAN_POINT('Ctrl Pts',(17.4252911394727,0.27269576514082,10.5713320279724));
#32971=CARTESIAN_POINT('Ctrl Pts',(17.2967183496608,-2.13355103363312,-10.5713320279724));
#32972=CARTESIAN_POINT('Ctrl Pts',(17.3951308181133,-1.33572022383133,-3.52377734265747));
#32973=CARTESIAN_POINT('Ctrl Pts',(17.4382534882275,-0.531074360093895,
3.52377734265748));
#32974=CARTESIAN_POINT('Ctrl Pts',(17.4256746734088,0.272704706835342,10.5713320279724));
#32975=CARTESIAN_POINT('Origin',(2.22044604925031E-15,-4.16333634234434E-16,
-6.));
#32976=CARTESIAN_POINT('',(0.,0.,0.));
#32977=CARTESIAN_POINT('Origin',(26.3408711739,15.6090782051017,5.99920149541289));
#32978=CARTESIAN_POINT('',(26.3408711739,14.6090782051017,5.99920149541289));
#32979=CARTESIAN_POINT('Origin',(26.3408711739,15.6090782051017,5.99920149541289));
#32980=CARTESIAN_POINT('',(23.3408711739,14.6090782051017,5.99920149541289));
#32981=CARTESIAN_POINT('',(26.3408711739,14.6090782051017,5.99920149541289));
#32982=CARTESIAN_POINT('Origin',(23.3408711739,15.6090782051017,5.99920149541289));
#32983=CARTESIAN_POINT('Origin',(26.3408711739,36.3909217948983,5.99920149541289));
#32984=CARTESIAN_POINT('',(26.3408711739,35.3909217948983,5.99920149541289));
#32985=CARTESIAN_POINT('Origin',(26.3408711739,36.3909217948983,5.99920149541289));
#32986=CARTESIAN_POINT('',(23.3408711739,35.3909217948983,5.99920149541289));
#32987=CARTESIAN_POINT('',(26.3408711739,35.3909217948983,5.99920149541289));
#32988=CARTESIAN_POINT('Origin',(23.3408711739,36.3909217948983,5.99920149541289));
#32989=CARTESIAN_POINT('Origin',(26.3408711739,26.,-11.9984029908258));
#32990=CARTESIAN_POINT('',(26.3408711739,25.,-11.9984029908258));
#32991=CARTESIAN_POINT('Origin',(26.3408711739,26.,-11.9984029908258));
#32992=CARTESIAN_POINT('',(23.3408711739,25.,-11.9984029908258));
#32993=CARTESIAN_POINT('',(26.3408711739,25.,-11.9984029908258));
#32994=CARTESIAN_POINT('Origin',(23.3408711739,26.,-11.9984029908258));
#32995=CARTESIAN_POINT('Origin',(26.0408711739,26.,7.77156117237612E-15));
#32996=CARTESIAN_POINT('',(26.3408711739,26.,13.2));
#32997=CARTESIAN_POINT('Origin',(26.3408711739,26.,7.77156117237612E-15));
#32998=CARTESIAN_POINT('',(26.0408711739,26.,13.5));
#32999=CARTESIAN_POINT('Origin',(26.0408711739,26.,13.2));
#33000=CARTESIAN_POINT('',(26.0408711739,30.,12.8937969582276));
#33001=CARTESIAN_POINT('Origin',(26.0408711739,26.,7.77156117237612E-15));
#33002=CARTESIAN_POINT('Origin',(26.0408711739,26.,7.77156117237612E-15));
#33003=CARTESIAN_POINT('Origin',(23.3408711739,26.,7.77156117237612E-15));
#33004=CARTESIAN_POINT('',(23.3408711739,30.,12.8937969582276));
#33005=CARTESIAN_POINT('',(23.3408711739,30.,12.8937969582276));
#33006=CARTESIAN_POINT('Origin',(23.3408711739,26.,7.77156117237612E-15));
#33007=CARTESIAN_POINT('Origin',(26.3408711739,26.,1.11022302462516E-14));
#33008=CARTESIAN_POINT('',(26.3408711739,20.5,7.09800543284508E-15));
#33009=CARTESIAN_POINT('Origin',(26.3408711739,26.,7.77156117237612E-15));
#33010=CARTESIAN_POINT('Origin',(23.3408711739,26.,7.77156117237612E-15));
#33011=CARTESIAN_POINT('',(23.3408711739,20.5,7.09800543284508E-15));
#33012=CARTESIAN_POINT('Origin',(23.3408711739,26.,7.77156117237612E-15));
#33013=CARTESIAN_POINT('',(23.3408711739,20.5,7.09800543284507E-15));
#33014=CARTESIAN_POINT('Origin',(23.3408711739,26.,1.11022302462516E-14));
#33015=CARTESIAN_POINT('',(0.,0.,0.));
#33016=CARTESIAN_POINT('Origin',(0.,0.,-63.6971797838103));
#33017=CARTESIAN_POINT('',(3.09908550384722,6.01564277861011,-58.9542133848184));
#33018=CARTESIAN_POINT('',(3.09908550384721,6.01564277861012,-59.3485564563465));
#33019=CARTESIAN_POINT('',(3.09908550384721,6.01564277861012,-63.6971797838103));
#33020=CARTESIAN_POINT('',(-3.92879594989319,-5.50970519938253,-59.9999154487532));
#33021=CARTESIAN_POINT('Ctrl Pts',(-3.92879594989319,-5.50970519938253,
-59.9999154487532));
#33022=CARTESIAN_POINT('Ctrl Pts',(-3.78616780238278,-5.61140880565578,
-59.9916558525619));
#33023=CARTESIAN_POINT('Ctrl Pts',(-3.63945151853262,-5.70766793724715,
-59.9833962563706));
#33024=CARTESIAN_POINT('Ctrl Pts',(-3.48909951756589,-5.79814397514597,
-59.9751366601792));
#33025=CARTESIAN_POINT('Ctrl Pts',(-3.33886313431323,-5.88855043876168,
-59.9668834154539));
#33026=CARTESIAN_POINT('Ctrl Pts',(-3.18499690519244,-5.97318248597719,
-59.9586301707286));
#33027=CARTESIAN_POINT('Ctrl Pts',(-3.02798303470171,-6.05174419002973,
-59.9503769260034));
#33028=CARTESIAN_POINT('Ctrl Pts',(-2.87105955583084,-6.13026066674238,
-59.9421284326045));
#33029=CARTESIAN_POINT('Ctrl Pts',(-2.71099236144859,-6.20271360500805,
-59.9338799392057));
#33030=CARTESIAN_POINT('Ctrl Pts',(-2.54828924529006,-6.26885244062572,
-59.9256314458069));
#33031=CARTESIAN_POINT('Ctrl Pts',(-2.38564835479305,-6.33496598150475,
-59.917386107037));
#33032=CARTESIAN_POINT('Ctrl Pts',(-2.22037387867933,-6.39477009881011,
-59.9091407682672));
#33033=CARTESIAN_POINT('Ctrl Pts',(-2.0529947640175,-6.44806184050035,-59.9008954294973));
#33034=CARTESIAN_POINT('Ctrl Pts',(-1.88561604710717,-6.50135345555071,
-59.8926501103212));
#33035=CARTESIAN_POINT('Ctrl Pts',(-1.71613303568899,-6.54813260926387,
-59.8844047911452));
#33036=CARTESIAN_POINT('Ctrl Pts',(-1.54509150386976,-6.58824568794072,
-59.8761594719691));
#33037=CARTESIAN_POINT('Ctrl Pts',(-1.37404290093257,-6.62836042495346,
-59.867913811919));
#33038=CARTESIAN_POINT('Ctrl Pts',(-1.20143599365608,-6.66180845615694,
-59.8596681518688));
#33039=CARTESIAN_POINT('Ctrl Pts',(-1.02782835956988,-6.68848696367601,
-59.8514224918187));
#33040=CARTESIAN_POINT('Ctrl Pts',(-0.854183138462646,-6.71517124724075,
-59.8431750465372));
#33041=CARTESIAN_POINT('Ctrl Pts',(-0.679537108659508,-6.73508303288056,
-59.8349276012556));
#33042=CARTESIAN_POINT('Ctrl Pts',(-0.50445472251315,-6.74817119173293,
-59.8266801559741));
#33043=CARTESIAN_POINT('Ctrl Pts',(-0.329303761043839,-6.76126447688464,
-59.8184294803778));
#33044=CARTESIAN_POINT('Ctrl Pts',(-0.153716455416029,-6.76752878371977,
-59.8101788047815));
#33045=CARTESIAN_POINT('Ctrl Pts',(0.0217408595481048,-6.76696507564699,
-59.8019281291851));
#33046=CARTESIAN_POINT('Ctrl Pts',(0.197400711700603,-6.76640071686411,
-59.7936679295137));
#33047=CARTESIAN_POINT('Ctrl Pts',(0.372929919136183,-6.75899259768538,
-59.7854077298423));
#33048=CARTESIAN_POINT('Ctrl Pts',(0.547764280922616,-6.74479379169929,
-59.777147530171));
#33049=CARTESIAN_POINT('Ctrl Pts',(0.722705693314107,-6.73058629182285,
-59.7688822728017));
#33050=CARTESIAN_POINT('Ctrl Pts',(0.896951061004835,-6.70957985753265,
-59.7606170154325));
#33051=CARTESIAN_POINT('Ctrl Pts',(1.06994451776254,-6.68187905674069,-59.7523517580633));
#33052=CARTESIAN_POINT('Ctrl Pts',(1.24319838124092,-6.65413655798612,-59.7440740590179));
#33053=CARTESIAN_POINT('Ctrl Pts',(1.41519622119219,-6.6196796249656,-59.7357963599725));
#33054=CARTESIAN_POINT('Ctrl Pts',(1.58539423346844,-6.57866355154944,-59.7275186609271));
#33055=CARTESIAN_POINT('Ctrl Pts',(1.71981373436326,-6.54626975303482,-59.7209810747394));
#33056=CARTESIAN_POINT('Ctrl Pts',(1.85311081155622,-6.50978565693524,-59.7144434885516));
#33057=CARTESIAN_POINT('Ctrl Pts',(1.98502604839901,-6.46930912750175,-59.7079059023639));
#33058=CARTESIAN_POINT('Ctrl Pts',(2.14752882658301,-6.41944719614633,-59.6998524284548));
#33059=CARTESIAN_POINT('Ctrl Pts',(2.30845684016059,-6.36336465789081,-59.6917989545457));
#33060=CARTESIAN_POINT('Ctrl Pts',(2.46728415220246,-6.30117432803526,-59.6837454806366));
#33061=CARTESIAN_POINT('Ctrl Pts',(2.62591184948028,-6.23906215922054,-59.6757021283639));
#33062=CARTESIAN_POINT('Ctrl Pts',(2.78244375381319,-6.17085760612302,-59.6676587760911));
#33063=CARTESIAN_POINT('Ctrl Pts',(2.93636597617378,-6.09672402639065,-59.6596154238184));
#33064=CARTESIAN_POINT('Ctrl Pts',(3.09012877219892,-6.02266723118471,-59.6515804025206));
#33065=CARTESIAN_POINT('Ctrl Pts',(3.24128693032771,-5.94269379026002,-59.6435453812228));
#33066=CARTESIAN_POINT('Ctrl Pts',(3.38934366436051,-5.85701617932368,-59.635510359925));
#33067=CARTESIAN_POINT('Ctrl Pts',(3.53727971653349,-5.77140840468016,-59.6274818880173));
#33068=CARTESIAN_POINT('Ctrl Pts',(3.68211905324582,-5.68010589995175,-59.6194534161096));
#33069=CARTESIAN_POINT('Ctrl Pts',(3.82338687555638,-5.58336832027256,-59.611424944202));
#33070=CARTESIAN_POINT('Ctrl Pts',(3.96457068211584,-5.48668827301855,-59.6034012470412));
#33071=CARTESIAN_POINT('Ctrl Pts',(4.10218689409652,-5.38457979610277,-59.5953775498804));
#33072=CARTESIAN_POINT('Ctrl Pts',(4.23578736063623,-5.27734729153525,-59.5873538527197));
#33073=CARTESIAN_POINT('Ctrl Pts',(4.37244519402079,-5.16766083517663,-59.5791465380439));
#33074=CARTESIAN_POINT('Ctrl Pts',(4.50490092736726,-5.05261321034467,-59.5709392233681));
#33075=CARTESIAN_POINT('Ctrl Pts',(4.63270806050258,-4.93257590171245,-59.5627319086923));
#33076=CARTESIAN_POINT('Ctrl Pts',(4.75761514036353,-4.81526234238441,-59.5547108250133));
#33077=CARTESIAN_POINT('Ctrl Pts',(4.87808203600149,-4.69318338095779,-59.5466897413343));
#33078=CARTESIAN_POINT('Ctrl Pts',(4.99372736342137,-4.56672486797888,-59.5386686576553));
#33079=CARTESIAN_POINT('Ctrl Pts',(5.10938492623287,-4.44025297556245,-59.5306467253376));
#33080=CARTESIAN_POINT('Ctrl Pts',(5.22021965194513,-4.30940088575895,-59.5226247930199));
#33081=CARTESIAN_POINT('Ctrl Pts',(5.32588903417308,-4.17458920082862,-59.5146028607022));
#33082=CARTESIAN_POINT('Ctrl Pts',(5.4315906722701,-4.03973636426131,-59.5065784796676));
#33083=CARTESIAN_POINT('Ctrl Pts',(5.53212359742655,-3.90092182192332,-59.4985540986331));
#33084=CARTESIAN_POINT('Ctrl Pts',(5.6271874968476,-3.75859679605595,-59.4905297175985));
#33085=CARTESIAN_POINT('Ctrl Pts',(5.72606100290402,-3.61056821325239,-59.4821837661737));
#33086=CARTESIAN_POINT('Ctrl Pts',(5.81901783100488,-3.45874234298609,-59.4738378147489));
#33087=CARTESIAN_POINT('Ctrl Pts',(5.9057722739808,-3.30365598207194,-59.4654918633241));
#33088=CARTESIAN_POINT('Ctrl Pts',(5.98933252273465,-3.15427971439291,-59.4574531997903));
#33089=CARTESIAN_POINT('Ctrl Pts',(6.06713887644236,-3.00187913474258,-59.4494145362565));
#33090=CARTESIAN_POINT('Ctrl Pts',(6.13898512302111,-2.8469546289545,-59.4413758727227));
#33091=CARTESIAN_POINT('Ctrl Pts',(6.21088610655917,-2.69191209199885,-59.4333310848328));
#33092=CARTESIAN_POINT('Ctrl Pts',(6.2768177989628,-2.53434214405691,-59.4252862969429));
#33093=CARTESIAN_POINT('Ctrl Pts',(6.33662354414647,-2.37476126374181,-59.417241509053));
#33094=CARTESIAN_POINT('Ctrl Pts',(6.39651438611868,-2.21495331794356,-59.4091852743429));
#33095=CARTESIAN_POINT('Ctrl Pts',(6.45026177378931,-2.05312908358832,-59.4011290396328));
#33096=CARTESIAN_POINT('Ctrl Pts',(6.49775974844085,-1.88981672432591,-59.3930728049227));
#33097=CARTESIAN_POINT('Ctrl Pts',(6.50305517106833,-1.87160946456526,-59.3921746367821));
#33098=CARTESIAN_POINT('Ctrl Pts',(6.50827297002536,-1.85338371455738,-59.3912764686414));
#33099=CARTESIAN_POINT('Ctrl Pts',(6.51341303837296,-1.83514021032541,-59.3903783005008));
#33100=CARTESIAN_POINT('Ctrl Pts',(6.56098236751811,-1.66630368931335,-59.3820661044326));
#33101=CARTESIAN_POINT('Ctrl Pts',(6.60204676745149,-1.49538953721762,-59.3737539083644));
#33102=CARTESIAN_POINT('Ctrl Pts',(6.6364246288501,-1.32293504964979,-59.3654417122962));
#33103=CARTESIAN_POINT('Ctrl Pts',(6.67076098999591,-1.15068874562037,-59.3571395505415));
#33104=CARTESIAN_POINT('Ctrl Pts',(6.69842682295797,-0.976906150286582,
-59.3488373887868));
#33105=CARTESIAN_POINT('Ctrl Pts',(6.71929018662497,-0.802139880522974,
-59.3405352270321));
#33106=CARTESIAN_POINT('Ctrl Pts',(6.74013227686411,-0.627551812016343,
-59.332241530616));
#33107=CARTESIAN_POINT('Ctrl Pts',(6.75418567433934,-0.451982412657481,
-59.3239478342));
#33108=CARTESIAN_POINT('Ctrl Pts',(6.76136937595525,-0.27599485845678,-59.3156541377839));
#33109=CARTESIAN_POINT('Ctrl Pts',(6.76854709903521,-0.100153767454843,
-59.3073673436816));
#33110=CARTESIAN_POINT('Ctrl Pts',(6.7688665030028,0.0761044366957623,-59.2990805495792));
#33111=CARTESIAN_POINT('Ctrl Pts',(6.76229832759216,0.252210881296477,-59.2907937554769));
#33112=CARTESIAN_POINT('Ctrl Pts',(6.75573438801983,0.428203754261234,-59.2825123055558));
#33113=CARTESIAN_POINT('Ctrl Pts',(6.74229173332196,0.604044713762333,-59.2742308556347));
#33114=CARTESIAN_POINT('Ctrl Pts',(6.72199317861293,0.779164107670035,-59.2659494057136));
#33115=CARTESIAN_POINT('Ctrl Pts',(6.70170311045125,0.954210286560716,-59.2576714181532));
#33116=CARTESIAN_POINT('Ctrl Pts',(6.6745628934783,1.12853515361881,-59.2493934305928));
#33117=CARTESIAN_POINT('Ctrl Pts',(6.64064728551256,1.30157313640636,-59.2411154430323));
#33118=CARTESIAN_POINT('Ctrl Pts',(6.60673902095445,1.47457365300886,-59.2328392478218));
#33119=CARTESIAN_POINT('Ctrl Pts',(6.56605835500911,1.64628749694697,-59.2245630526113));
#33120=CARTESIAN_POINT('Ctrl Pts',(6.51873139201793,1.81615804343124,-59.2162868574008));
#33121=CARTESIAN_POINT('Ctrl Pts',(6.4714066414513,1.98602064886578,-59.208011049083));
#33122=CARTESIAN_POINT('Ctrl Pts',(6.41743630702645,2.15403979126329,-59.1997352407652));
#33123=CARTESIAN_POINT('Ctrl Pts',(6.35699676481274,2.31967263469663,-59.1914594324474));
#33124=CARTESIAN_POINT('Ctrl Pts',(6.29654978744763,2.48532585395053,-59.1831826060562));
#33125=CARTESIAN_POINT('Ctrl Pts',(6.22963213723469,2.6485918605976,-59.174905779665));
#33126=CARTESIAN_POINT('Ctrl Pts',(6.15646892023154,2.80894632099353,-59.1666289532739));
#33127=CARTESIAN_POINT('Ctrl Pts',(6.08325293945296,2.96941642565832,-59.1583461578094));
#33128=CARTESIAN_POINT('Ctrl Pts',(6.00378253740903,3.12697046947339,-59.1500633623449));
#33129=CARTESIAN_POINT('Ctrl Pts',(5.91832991542423,3.28110652253088,-59.1417805668804));
#33130=CARTESIAN_POINT('Ctrl Pts',(5.83284544338531,3.43530002545378,-59.1334946842375));
#33131=CARTESIAN_POINT('Ctrl Pts',(5.74137448411693,3.58607269616141,-59.1252088015947));
#33132=CARTESIAN_POINT('Ctrl Pts',(5.64423353598856,3.73295014582597,-59.1169229189518));
#33133=CARTESIAN_POINT('Ctrl Pts',(5.54698573089441,3.8799891635925,-59.108627921674));
#33134=CARTESIAN_POINT('Ctrl Pts',(5.44405567499194,4.0231241113357,-59.1003329243962));
#33135=CARTESIAN_POINT('Ctrl Pts',(5.33580190541095,4.1619114630435,-59.0920379271185));
#33136=CARTESIAN_POINT('Ctrl Pts',(5.25233433488648,4.26892152940345,-59.0856421842916));
#33137=CARTESIAN_POINT('Ctrl Pts',(5.1657026947281,4.3733475872308,-59.0792464414647));
#33138=CARTESIAN_POINT('Ctrl Pts',(5.07608662186546,4.47500096171146,-59.0728506986378));
#33139=CARTESIAN_POINT('Ctrl Pts',(4.95683725234456,4.61026800063953,-59.0643400791098));
#33140=CARTESIAN_POINT('Ctrl Pts',(4.83208539855738,4.74087032477467,-59.0558294595818));
#33141=CARTESIAN_POINT('Ctrl Pts',(4.70221964422388,4.86635586630027,-59.0473188400538));
#33142=CARTESIAN_POINT('Ctrl Pts',(4.57250400499067,4.99169635592401,-59.0388180581656));
#33143=CARTESIAN_POINT('Ctrl Pts',(4.43768648991991,5.11193163799852,-59.0303172762773));
#33144=CARTESIAN_POINT('Ctrl Pts',(4.29819366261953,5.22664521836113,-59.021816494389));
#33145=CARTESIAN_POINT('Ctrl Pts',(4.1587975426097,5.34127927033681,-59.0133216059048));
#33146=CARTESIAN_POINT('Ctrl Pts',(4.01473282041731,5.45039904588738,-59.0048267174205));
#33147=CARTESIAN_POINT('Ctrl Pts',(3.86646118280567,5.55362646582006,-58.9963318289362));
#33148=CARTESIAN_POINT('Ctrl Pts',(3.71829552336917,5.65678010324271,-58.987843012232));
#33149=CARTESIAN_POINT('Ctrl Pts',(3.56592921152458,5.75404960117541,-58.9793541955279));
#33150=CARTESIAN_POINT('Ctrl Pts',(3.40985530824554,5.84509844030276,-58.9708653788237));
#33151=CARTESIAN_POINT('Ctrl Pts',(3.30780175581451,5.90463342521983,-58.9653147141553));
#33152=CARTESIAN_POINT('Ctrl Pts',(3.20416364447007,5.96150955388916,-58.9597640494868));
#33153=CARTESIAN_POINT('Ctrl Pts',(3.09908550384722,6.01564277861012,-58.9542133848184));
#33154=CARTESIAN_POINT('',(3.92888236737293,-5.50964357679751,-60.));
#33155=CARTESIAN_POINT('Origin',(0.,0.,-60.));
#33156=CARTESIAN_POINT('Ctrl Pts',(3.92888236737219,-5.50964357679804,-60.));
#33157=CARTESIAN_POINT('Ctrl Pts',(4.08454665498865,-5.39864062963439,-59.9910067718568));
#33158=CARTESIAN_POINT('Ctrl Pts',(4.23546571391035,-5.28106458098038,-59.9820135437135));
#33159=CARTESIAN_POINT('Ctrl Pts',(4.38111815764509,-5.15733387408189,-59.9730203155703));
#33160=CARTESIAN_POINT('Ctrl Pts',(4.52681461814809,-5.03356577525429,-59.9640243696365));
#33161=CARTESIAN_POINT('Ctrl Pts',(4.66724109992879,-4.9036394621831,-59.9550284237026));
#33162=CARTESIAN_POINT('Ctrl Pts',(4.8019104597316,-4.76801268210565,-59.9460324777688));
#33163=CARTESIAN_POINT('Ctrl Pts',(4.93660339059607,-4.63236216339008,-59.9370349572824));
#33164=CARTESIAN_POINT('Ctrl Pts',(5.06553701451811,-4.49100935692313,-59.9280374367959));
#33165=CARTESIAN_POINT('Ctrl Pts',(5.18826127518279,-4.34444863480266,-59.9190399163094));
#33166=CARTESIAN_POINT('Ctrl Pts',(5.31096445637577,-4.19791308637299,-59.910043941263));
#33167=CARTESIAN_POINT('Ctrl Pts',(5.42746025016464,-4.04617159716448,-59.9010479662165));
#33168=CARTESIAN_POINT('Ctrl Pts',(5.53733860434853,-3.88975194334954,-59.89205199117));
#33169=CARTESIAN_POINT('Ctrl Pts',(5.64716492430394,-3.73340636396049,-59.8830602762767));
#33170=CARTESIAN_POINT('Ctrl Pts',(5.75037992649799,-3.57238724563523,-59.8740685613834));
#33171=CARTESIAN_POINT('Ctrl Pts',(5.84661613452195,-3.40725237919759,-59.8650768464901));
#33172=CARTESIAN_POINT('Ctrl Pts',(5.93166974709466,-3.26130609514683,-59.8571299640162));
#33173=CARTESIAN_POINT('Ctrl Pts',(6.01127273786878,-3.11214551538678,-59.8491830815423));
#33174=CARTESIAN_POINT('Ctrl Pts',(6.08520006302371,-2.96017384505982,-59.8412361990685));
#33175=CARTESIAN_POINT('Ctrl Pts',(6.16124224316641,-2.8038546882748,-59.833061978408));
#33176=CARTESIAN_POINT('Ctrl Pts',(6.2313015947187,-2.6445121253944,-59.8248877577476));
#33177=CARTESIAN_POINT('Ctrl Pts',(6.29513685779775,-2.48264796972834,-59.8167135370872));
#33178=CARTESIAN_POINT('Ctrl Pts',(6.35895158460461,-2.320835886948,-59.8085419461335));
#33179=CARTESIAN_POINT('Ctrl Pts',(6.41654607795235,-2.15650416350157,-59.8003703551797));
#33180=CARTESIAN_POINT('Ctrl Pts',(6.46772691028241,-1.99017527218303,-59.792198764226));
#33181=CARTESIAN_POINT('Ctrl Pts',(6.51890081155432,-1.82386890560989,-59.7840282798931));
#33182=CARTESIAN_POINT('Ctrl Pts',(6.56366267642554,-1.65556625626644,-59.7758577955601));
#33183=CARTESIAN_POINT('Ctrl Pts',(6.60186871410054,-1.48580566756911,-59.7676873112272));
#33184=CARTESIAN_POINT('Ctrl Pts',(6.64008724617722,-1.31598956259443,-59.7595141549262));
#33185=CARTESIAN_POINT('Ctrl Pts',(6.67174558567356,-1.14471491876742,-59.7513409986251));
#33186=CARTESIAN_POINT('Ctrl Pts',(6.69675082102834,-0.972531460188462,
-59.7431678423241));
#33187=CARTESIAN_POINT('Ctrl Pts',(6.72176059840295,-0.800316725731716,
-59.7349932014285));
#33188=CARTESIAN_POINT('Ctrl Pts',(6.7401148193439,-0.627193207152181,-59.7268185605328));
#33189=CARTESIAN_POINT('Ctrl Pts',(6.75177239074758,-0.453716413124641,
-59.7186439196372));
#33190=CARTESIAN_POINT('Ctrl Pts',(6.76343839782527,-0.280114087489199,
-59.7104633633923));
#33191=CARTESIAN_POINT('Ctrl Pts',(6.76839806132776,-0.106158337728105,
-59.7022828071475));
#33192=CARTESIAN_POINT('Ctrl Pts',(6.76666240052332,0.0675940629346515,
-59.6941022509026));
#33193=CARTESIAN_POINT('Ctrl Pts',(6.76583990227248,0.149932181798813,-59.6902256333141));
#33194=CARTESIAN_POINT('Ctrl Pts',(6.76351463202272,0.232224668894347,-59.6863490157255));
#33195=CARTESIAN_POINT('Ctrl Pts',(6.75969183463654,0.314412628162514,-59.6824723981369));
#33196=CARTESIAN_POINT('Ctrl Pts',(6.75053673949748,0.511241941980218,-59.6731884107173));
#33197=CARTESIAN_POINT('Ctrl Pts',(6.73278303022695,0.707614036394523,-59.6639044232977));
#33198=CARTESIAN_POINT('Ctrl Pts',(6.70650466938329,0.902820092565595,-59.6546204358781));
#33199=CARTESIAN_POINT('Ctrl Pts',(6.68022095811821,1.09806589378281,-59.6453345581866));
#33200=CARTESIAN_POINT('Ctrl Pts',(6.64540915427849,1.29214499852165,-59.6360486804952));
#33201=CARTESIAN_POINT('Ctrl Pts',(6.60219482000945,1.48435594068281,-59.6267628028037));
#33202=CARTESIAN_POINT('Ctrl Pts',(6.55901279252097,1.67642318708115,-59.6174838671795));
#33203=CARTESIAN_POINT('Ctrl Pts',(6.50744083197316,1.86662488169894,-59.6082049315553));
#33204=CARTESIAN_POINT('Ctrl Pts',(6.44765515910135,2.05427163474398,-59.598925995931));
#33205=CARTESIAN_POINT('Ctrl Pts',(6.38792781219889,2.24173532254547,-59.5896561126916));
#33206=CARTESIAN_POINT('Ctrl Pts',(6.32000281232516,2.42664886995839,-59.5803862294521));
#33207=CARTESIAN_POINT('Ctrl Pts',(6.24410612644912,2.60833810723238,-59.5711163462127));
#33208=CARTESIAN_POINT('Ctrl Pts',(6.16838528934056,2.78960637976899,-59.561867940822));
#33209=CARTESIAN_POINT('Ctrl Pts',(6.08472971602274,2.96766508685266,-59.5526195354313));
#33210=CARTESIAN_POINT('Ctrl Pts',(5.99341314440184,3.14186057623683,-59.5433711300406));
#33211=CARTESIAN_POINT('Ctrl Pts',(5.92869874186293,3.26530976864924,-59.5368169524289));
#33212=CARTESIAN_POINT('Ctrl Pts',(5.86013778368322,3.38681906079107,-59.5302627748172));
#33213=CARTESIAN_POINT('Ctrl Pts',(5.78784254158412,3.50616139300933,-59.5237085972055));
#33214=CARTESIAN_POINT('Ctrl Pts',(5.69664729943196,3.65670315163194,-59.5154409740943));
#33215=CARTESIAN_POINT('Ctrl Pts',(5.59955034278513,3.80372530703444,-59.5071733509831));
#33216=CARTESIAN_POINT('Ctrl Pts',(5.49685920736974,3.9467490234818,-59.4989057278719));
#33217=CARTESIAN_POINT('Ctrl Pts',(5.39417722332246,4.0897599943044,-59.4906388415338));
#33218=CARTESIAN_POINT('Ctrl Pts',(5.28590225919402,4.22877295083797,-59.4823719551956));
#33219=CARTESIAN_POINT('Ctrl Pts',(5.17238440972565,4.36333914772013,-59.4741050688575));
#33220=CARTESIAN_POINT('Ctrl Pts',(5.05885715554715,4.49791649312282,-59.4658374976256));
#33221=CARTESIAN_POINT('Ctrl Pts',(4.94008637812876,4.62804607686222,-59.4575699263937));
#33222=CARTESIAN_POINT('Ctrl Pts',(4.81646166447886,4.75331316395265,-59.4493023551617));
#33223=CARTESIAN_POINT('Ctrl Pts',(4.69276225450659,4.87865593971764,-59.4410297885115));
#33224=CARTESIAN_POINT('Ctrl Pts',(4.56420329656194,4.99913009910557,-59.4327572218612));
#33225=CARTESIAN_POINT('Ctrl Pts',(4.43121088660897,5.11435812965793,-59.4244846552109));
#33226=CARTESIAN_POINT('Ctrl Pts',(4.29817261410477,5.22962589669944,-59.4162092357586));
#33227=CARTESIAN_POINT('Ctrl Pts',(4.16069811336844,5.3396437052627,-59.4079338163063));
#33228=CARTESIAN_POINT('Ctrl Pts',(4.01924569645935,5.44407503911298,-59.399658396854));
#33229=CARTESIAN_POINT('Ctrl Pts',(3.87766517540032,5.54860094955335,-59.3913754828987));
#33230=CARTESIAN_POINT('Ctrl Pts',(3.73209983098276,5.64753007916108,-59.3830925689433));
#33231=CARTESIAN_POINT('Ctrl Pts',(3.58303667177545,5.74056941502429,-59.3748096549879));
#33232=CARTESIAN_POINT('Ctrl Pts',(3.52385914830318,5.77750568761618,-59.3715213687499));
#33233=CARTESIAN_POINT('Ctrl Pts',(3.46413062657364,5.81351419890145,-59.368233082512));
#33234=CARTESIAN_POINT('Ctrl Pts',(3.40388261093338,5.84857864536208,-59.364944796274));
#33235=CARTESIAN_POINT('Ctrl Pts',(3.30379349775918,5.90683067761398,-59.3594820162981));
#33236=CARTESIAN_POINT('Ctrl Pts',(3.20214889935663,5.96254749241124,-59.3540192363223));
#33237=CARTESIAN_POINT('Ctrl Pts',(3.09908550384721,6.01564277861012,-59.3485564563465));
#33238=CARTESIAN_POINT('Origin',(0.,0.,-63.6971797838103));
#33239=CARTESIAN_POINT('',(3.0990855038472,6.01564277861012,-56.9542436419538));
#33240=CARTESIAN_POINT('',(3.09908550384721,6.01564277861012,-57.3484848024));
#33241=CARTESIAN_POINT('',(3.09908550384721,6.01564277861012,-63.6971797838103));
#33242=CARTESIAN_POINT('',(-6.767,9.61385986553327E-13,-58.30282021619));
#33243=CARTESIAN_POINT('Ctrl Pts',(-6.767,1.03350959928159E-12,-58.30282021619));
#33244=CARTESIAN_POINT('Ctrl Pts',(-6.76700000000003,-0.186007249558951,
-58.2940707043773));
#33245=CARTESIAN_POINT('Ctrl Pts',(-6.75932637294252,-0.372014355815112,
-58.2853211925645));
#33246=CARTESIAN_POINT('Ctrl Pts',(-6.74400518263371,-0.557389537585464,
-58.2765716807518));
#33247=CARTESIAN_POINT('Ctrl Pts',(-6.72868405703739,-0.742763936381938,
-58.2678222058946));
#33248=CARTESIAN_POINT('Ctrl Pts',(-6.70571545643574,-0.927506130404251,
-58.2590727310374));
#33249=CARTESIAN_POINT('Ctrl Pts',(-6.67517739401586,-1.11098864009477,
-58.2503232561802));
#33250=CARTESIAN_POINT('Ctrl Pts',(-6.64463945804403,-1.29447039004469,
-58.2415738175517));
#33251=CARTESIAN_POINT('Ctrl Pts',(-6.60653217002741,-1.47669218339202,
-58.2328243789232));
#33252=CARTESIAN_POINT('Ctrl Pts',(-6.560984960855,-1.65703510627703,-58.2240749402946));
#33253=CARTESIAN_POINT('Ctrl Pts',(-6.51543793649581,-1.83737729739921,
-58.215325537168));
#33254=CARTESIAN_POINT('Ctrl Pts',(-6.46245112156926,-2.01584035544857,
-58.2065761340414));
#33255=CARTESIAN_POINT('Ctrl Pts',(-6.40220448361752,-2.19181813797306,
-58.1978267309148));
#33256=CARTESIAN_POINT('Ctrl Pts',(-6.34195808512012,-2.36779522106198,
-58.1890773625632));
#33257=CARTESIAN_POINT('Ctrl Pts',(-6.27445201416397,-2.54128677725638,
-58.1803279942117));
#33258=CARTESIAN_POINT('Ctrl Pts',(-6.19991555052772,-2.7117035542855,-58.1715786258602));
#33259=CARTESIAN_POINT('Ctrl Pts',(-6.12537937695159,-2.88211966813434,
-58.162829291557));
#33260=CARTESIAN_POINT('Ctrl Pts',(-6.0438129802838,-3.04946076419812,-58.1540799572538));
#33261=CARTESIAN_POINT('Ctrl Pts',(-5.95549339308897,-3.21315848424469,
-58.1453306229506));
#33262=CARTESIAN_POINT('Ctrl Pts',(-5.86717414225717,-3.37685558085242,
-58.1365813219691));
#33263=CARTESIAN_POINT('Ctrl Pts',(-5.77210188843968,-3.53690907700161,
-58.1278320209875));
#33264=CARTESIAN_POINT('Ctrl Pts',(-5.67059953311265,-3.69277537024154,
-58.1190827200059));
#33265=CARTESIAN_POINT('Ctrl Pts',(-5.56909755592591,-3.84864108281195,
-58.1103334516193));
#33266=CARTESIAN_POINT('Ctrl Pts',(-5.46116568154839,-4.00031938355002,
-58.1015841832327));
#33267=CARTESIAN_POINT('Ctrl Pts',(-5.34717048488239,-4.14729511918343,
-58.0928349148461));
#33268=CARTESIAN_POINT('Ctrl Pts',(-5.23317570343164,-4.29427031947351,
-58.0840856783277));
#33269=CARTESIAN_POINT('Ctrl Pts',(-5.11311781951404,-4.4365427624972,-58.0753364418094));
#33270=CARTESIAN_POINT('Ctrl Pts',(-4.98740458929099,-4.57362924412541,
-58.066587205291));
#33271=CARTESIAN_POINT('Ctrl Pts',(-4.86169180652584,-4.71071523781429,
-58.0578379999143));
#33272=CARTESIAN_POINT('Ctrl Pts',(-4.73032391141404,-4.84261509584654,
-58.0490887945376));
#33273=CARTESIAN_POINT('Ctrl Pts',(-4.59374706947147,-4.96888084599765,
-58.0403395891609));
#33274=CARTESIAN_POINT('Ctrl Pts',(-4.45717070231349,-5.0951461572088,-58.0315904141992));
#33275=CARTESIAN_POINT('Ctrl Pts',(-4.31538563497227,-5.21577720520694,
-58.0228412392375));
#33276=CARTESIAN_POINT('Ctrl Pts',(-4.1688734095193,-5.33036429293561,-58.0140920642758));
#33277=CARTESIAN_POINT('Ctrl Pts',(-4.02236168122419,-5.44495099183754,
-58.0053429190025));
#33278=CARTESIAN_POINT('Ctrl Pts',(-3.87112305263127,-5.55349359497965,
-57.9965937737293));
#33279=CARTESIAN_POINT('Ctrl Pts',(-3.71567116928955,-5.65562346357238,
-57.9878446284561));
#33280=CARTESIAN_POINT('Ctrl Pts',(-3.56021980053291,-5.75775299408939,
-57.9790955121447));
#33281=CARTESIAN_POINT('Ctrl Pts',(-3.40055544442085,-5.85346967519877,
-57.9703463958333));
#33282=CARTESIAN_POINT('Ctrl Pts',(-3.23722035886867,-5.9424484304137,-57.961597279522));
#33283=CARTESIAN_POINT('Ctrl Pts',(-3.07388580043522,-6.03142689847434,
-57.952848191446));
#33284=CARTESIAN_POINT('Ctrl Pts',(-2.90688078789264,-6.11366734707882,
-57.94409910337));
#33285=CARTESIAN_POINT('Ctrl Pts',(-2.73677250610444,-6.18889047001406,
-57.935350015294));
#33286=CARTESIAN_POINT('Ctrl Pts',(-2.56666475916994,-6.26411335643309,
-57.9266009547268));
#33287=CARTESIAN_POINT('Ctrl Pts',(-2.3934540245716,-6.3323188454523,-57.9178518941596));
#33288=CARTESIAN_POINT('Ctrl Pts',(-2.21772855944141,-6.39327529804856,
-57.9091028335925));
#33289=CARTESIAN_POINT('Ctrl Pts',(-2.04200363223706,-6.45423156404665,
-57.9003537998077));
#33290=CARTESIAN_POINT('Ctrl Pts',(-1.86376426061188,-6.50793874412408,
-57.8916047660229));
#33291=CARTESIAN_POINT('Ctrl Pts',(-1.68361577621882,-6.55421443943263,
-57.8828557322381));
#33292=CARTESIAN_POINT('Ctrl Pts',(-1.50346782833416,-6.60048999692542,
-57.8741067245092));
#33293=CARTESIAN_POINT('Ctrl Pts',(-1.32141105657594,-6.63933404265121,
-57.8653577167803));
#33294=CARTESIAN_POINT('Ctrl Pts',(-1.13806375346749,-6.67061465631493,
-57.8566087090514));
#33295=CARTESIAN_POINT('Ctrl Pts',(-0.954716981172254,-6.70189517941739,
-57.847859726652));
#33296=CARTESIAN_POINT('Ctrl Pts',(-0.770079967444639,-6.72561226608977,
-57.8391107442526));
#33297=CARTESIAN_POINT('Ctrl Pts',(-0.584779764075532,-6.74168536995963,
-57.8303617618531));
#33298=CARTESIAN_POINT('Ctrl Pts',(-0.391489587595349,-6.75845153117859,
-57.8212355314375));
#33299=CARTESIAN_POINT('Ctrl Pts',(-0.197478091807549,-6.76689985146387,
-57.8121093010219));
#33300=CARTESIAN_POINT('Ctrl Pts',(-0.00346214753326795,-6.76699911434415,
-57.8029830706063));
#33301=CARTESIAN_POINT('Ctrl Pts',(0.184490798482439,-6.76709527525941,
-57.7941420348912));
#33302=CARTESIAN_POINT('Ctrl Pts',(0.372447602152615,-6.75935633790775,
-57.785300999176));
#33303=CARTESIAN_POINT('Ctrl Pts',(0.559756448192091,-6.74380914014531,
-57.7764599634609));
#33304=CARTESIAN_POINT('Ctrl Pts',(0.745136131041261,-6.72842206873178,
-57.7677099848476));
#33305=CARTESIAN_POINT('Ctrl Pts',(0.929880851942979,-6.70538686355752,
-57.7589600062343));
#33306=CARTESIAN_POINT('Ctrl Pts',(1.1133630505726,-6.67478177303346,-57.750210027621));
#33307=CARTESIAN_POINT('Ctrl Pts',(1.2968433708992,-6.644176995813,-57.741460138581));
#33308=CARTESIAN_POINT('Ctrl Pts',(1.47906091204987,-6.60600253548105,-57.732710249541));
#33309=CARTESIAN_POINT('Ctrl Pts',(1.65939671095019,-6.56038806441263,-57.723960360501));
#33310=CARTESIAN_POINT('Ctrl Pts',(1.83973072368972,-6.51477404513903,-57.7152105581255));
#33311=CARTESIAN_POINT('Ctrl Pts',(2.01818275356862,-6.46172023288715,-57.70646075575));
#33312=CARTESIAN_POINT('Ctrl Pts',(2.19414664033166,-6.40140683918163,-57.6977109533745));
#33313=CARTESIAN_POINT('Ctrl Pts',(2.37010884271092,-6.34109402281559,-57.688961234755));
#33314=CARTESIAN_POINT('Ctrl Pts',(2.54358267847633,-6.27352185699862,-57.6802115161355));
#33315=CARTESIAN_POINT('Ctrl Pts',(2.71397890841562,-6.1989198643534,-57.6714617975159));
#33316=CARTESIAN_POINT('Ctrl Pts',(2.88437356388773,-6.12431856103323,-57.6627121597441));
#33317=CARTESIAN_POINT('Ctrl Pts',(3.05169040787014,-6.04268767582637,-57.6539625219723));
#33318=CARTESIAN_POINT('Ctrl Pts',(3.21536112511906,-5.95430447954025,-57.6452128842005));
#33319=CARTESIAN_POINT('Ctrl Pts',(3.37903038442696,-5.86592207055127,-57.6364633243684));
#33320=CARTESIAN_POINT('Ctrl Pts',(3.53905332979827,-5.77078760703466,-57.6277137645363));
#33321=CARTESIAN_POINT('Ctrl Pts',(3.69488643041747,-5.66922422085393,-57.6189642047043));
#33322=CARTESIAN_POINT('Ctrl Pts',(3.85071819468604,-5.56766170563254,-57.6102147199043));
#33323=CARTESIAN_POINT('Ctrl Pts',(4.00235994599093,-5.45967053456348,-57.6014652351043));
#33324=CARTESIAN_POINT('Ctrl Pts',(4.14929662974176,-5.34561750206781,-57.5927157503043));
#33325=CARTESIAN_POINT('Ctrl Pts',(4.2962321022492,-5.23156540974568,-57.5839663376289));
#33326=CARTESIAN_POINT('Ctrl Pts',(4.43846235841994,-5.11145173172293,-57.5752169249536));
#33327=CARTESIAN_POINT('Ctrl Pts',(4.57550431797306,-4.98568443006674,-57.5664675122782));
#33328=CARTESIAN_POINT('Ctrl Pts',(4.71254519337388,-4.85991812336793,-57.5577181688203));
#33329=CARTESIAN_POINT('Ctrl Pts',(4.84439764314893,-4.72849847631194,-57.5489688253624));
#33330=CARTESIAN_POINT('Ctrl Pts',(4.9706138419661,-4.59187184425426,-57.5402194819045));
#33331=CARTESIAN_POINT('Ctrl Pts',(5.09682908420133,-4.45524624767831,-57.5314702047571));
#33332=CARTESIAN_POINT('Ctrl Pts',(5.217407966501,-4.31341395556978,-57.5227209276098));
#33333=CARTESIAN_POINT('Ctrl Pts',(5.33194095942183,-4.16685668162943,-57.5139716504624));
#33334=CARTESIAN_POINT('Ctrl Pts',(5.44647312235069,-4.02030046975302,-57.5052224367189));
#33335=CARTESIAN_POINT('Ctrl Pts',(5.55495930712227,-3.86901957035635,-57.4964732229753));
#33336=CARTESIAN_POINT('Ctrl Pts',(5.65703106079737,-3.71352778058462,-57.4877240092318));
#33337=CARTESIAN_POINT('Ctrl Pts',(5.75910210868671,-3.55803706597707,-57.4789748559856));
#33338=CARTESIAN_POINT('Ctrl Pts',(5.85475865698478,-3.39833575881021,-57.4702257027394));
#33339=CARTESIAN_POINT('Ctrl Pts',(5.94367583068987,-3.23496624706859,-57.4614765494932));
#33340=CARTESIAN_POINT('Ctrl Pts',(6.03259241910004,-3.07159781070243,-57.4527274538381));
#33341=CARTESIAN_POINT('Ctrl Pts',(6.11476958470897,-2.90456146975982,-57.443978358183));
#33342=CARTESIAN_POINT('Ctrl Pts',(6.18992823574318,-2.7344245164841,-57.4352292625279));
#33343=CARTESIAN_POINT('Ctrl Pts',(6.26508641700876,-2.56428862662561,-57.4264802215577));
#33344=CARTESIAN_POINT('Ctrl Pts',(6.33322605570246,-2.39105242531414,-57.4177311805876));
#33345=CARTESIAN_POINT('Ctrl Pts',(6.39411573747723,-2.21530425353857,-57.4089821396175));
#33346=CARTESIAN_POINT('Ctrl Pts',(6.45500505889087,-2.03955712188685,-57.4002331504265));
#33347=CARTESIAN_POINT('Ctrl Pts',(6.50864441544895,-1.86129832025691,-57.3914841612355));
#33348=CARTESIAN_POINT('Ctrl Pts',(6.55485164049877,-1.68113324012423,-57.3827351720445));
#33349=CARTESIAN_POINT('Ctrl Pts',(6.60199852639086,-1.49730435913003,-57.3738082651676));
#33350=CARTESIAN_POINT('Ctrl Pts',(6.64140767440991,-1.31149113173747,-57.3648813582907));
#33351=CARTESIAN_POINT('Ctrl Pts',(6.67293975269588,-1.12435050446518,-57.3559544514138));
#33352=CARTESIAN_POINT('Ctrl Pts',(6.70384664831495,-0.940920291564619,
-57.3472045372298));
#33353=CARTESIAN_POINT('Ctrl Pts',(6.72718585889656,-0.756215114278821,
-57.3384546230458));
#33354=CARTESIAN_POINT('Ctrl Pts',(6.74287810451857,-0.570862389376028,
-57.3297047088619));
#33355=CARTESIAN_POINT('Ctrl Pts',(6.75857004154118,-0.385513309569033,
-57.3209549667513));
#33356=CARTESIAN_POINT('Ctrl Pts',(6.76661529035553,-0.199516993260188,
-57.3122052246407));
#33357=CARTESIAN_POINT('Ctrl Pts',(6.76698652348896,-0.013505218206075,
-57.3034554825301));
#33358=CARTESIAN_POINT('Ctrl Pts',(6.76735774981526,0.172503146036848,-57.2947059008595));
#33359=CARTESIAN_POINT('Ctrl Pts',(6.7600552414749,0.358526681831404,-57.2859563191888));
#33360=CARTESIAN_POINT('Ctrl Pts',(6.74510380214898,0.543933542112777,-57.2772067375182));
#33361=CARTESIAN_POINT('Ctrl Pts',(6.73015261711002,0.729337249082645,-57.2684573046563));
#33362=CARTESIAN_POINT('Ctrl Pts',(6.70755278444634,0.914124015852599,-57.2597078717943));
#33363=CARTESIAN_POINT('Ctrl Pts',(6.67738106408323,1.09766621749181,-57.2509584389324));
#33364=CARTESIAN_POINT('Ctrl Pts',(6.64720981677293,1.28120554143119,-57.24220914325));
#33365=CARTESIAN_POINT('Ctrl Pts',(6.60946696581567,1.46350005650419,-57.2334598475677));
#33366=CARTESIAN_POINT('Ctrl Pts',(6.56428070011044,1.64393062206335,-57.2247105518853));
#33367=CARTESIAN_POINT('Ctrl Pts',(6.51909508282795,1.82435859844456,-57.2159613817554));
#33368=CARTESIAN_POINT('Ctrl Pts',(6.46646633415721,2.00292240086371,-57.2072122116254));
#33369=CARTESIAN_POINT('Ctrl Pts',(6.40657319597256,2.17901557696266,-57.1984630414954));
#33370=CARTESIAN_POINT('Ctrl Pts',(6.34668083768363,2.35510646007252,-57.1897139852923));
#33371=CARTESIAN_POINT('Ctrl Pts',(6.27952437143956,2.52872650996354,-57.1809649290892));
#33372=CARTESIAN_POINT('Ctrl Pts',(6.2053318733521,2.69928607997755,-57.1722158728861));
#33373=CARTESIAN_POINT('Ctrl Pts',(6.12831449784328,2.87633970115236,-57.1631336965973));
#33374=CARTESIAN_POINT('Ctrl Pts',(6.0437148946323,3.05009490562197,-57.1540515203084));
#33375=CARTESIAN_POINT('Ctrl Pts',(5.95184265120568,3.21991584599488,-57.1449693440196));
#33376=CARTESIAN_POINT('Ctrl Pts',(5.86333281335572,3.38352155905163,-57.1362195636652));
#33377=CARTESIAN_POINT('Ctrl Pts',(5.76807337235766,3.54347560903692,-57.1274697833108));
#33378=CARTESIAN_POINT('Ctrl Pts',(5.66638790086438,3.6992346717852,-57.1187200029563));
#33379=CARTESIAN_POINT('Ctrl Pts',(5.56470608502828,3.85498813489641,-57.1099705371621));
#33380=CARTESIAN_POINT('Ctrl Pts',(5.4565988576704,4.00654667256142,-57.1012210713678));
#33381=CARTESIAN_POINT('Ctrl Pts',(5.34243340580597,4.15339551506095,-57.0924716055735));
#33382=CARTESIAN_POINT('Ctrl Pts',(5.22827145140687,4.30023985883757,-57.0837224078197));
#33383=CARTESIAN_POINT('Ctrl Pts',(5.10805181978186,4.44237456992932,-57.0749732100658));
#33384=CARTESIAN_POINT('Ctrl Pts',(4.98218281282651,4.5793169162634,-57.0662240123119));
#33385=CARTESIAN_POINT('Ctrl Pts',(4.85631699296328,4.71625579512059,-57.0574750360939));
#33386=CARTESIAN_POINT('Ctrl Pts',(4.72480227791936,4.84800236135674,-57.0487260598759));
#33387=CARTESIAN_POINT('Ctrl Pts',(4.5880853084821,4.97410918678819,-57.0399770836579));
#33388=CARTESIAN_POINT('Ctrl Pts',(4.45135945057063,5.10022421088928,-57.0312275386367));
#33389=CARTESIAN_POINT('Ctrl Pts',(4.30943087208128,5.22069856611914,-57.0224779936155));
#33390=CARTESIAN_POINT('Ctrl Pts',(4.1627816432255,5.33512305301619,-57.0137284485943));
#33391=CARTESIAN_POINT('Ctrl Pts',(4.01614103534475,5.44954081331364,-57.0049794179271));
#33392=CARTESIAN_POINT('Ctrl Pts',(3.864780558335,5.55790924068277,-56.9962303872598));
#33393=CARTESIAN_POINT('Ctrl Pts',(3.7092142581204,5.65986029751233,-56.9874813565925));
#33394=CARTESIAN_POINT('Ctrl Pts',(3.55364584530212,5.76181273884597,-56.9787322071127));
#33395=CARTESIAN_POINT('Ctrl Pts',(3.39387173464441,5.85734747818007,-56.9699830576328));
#33396=CARTESIAN_POINT('Ctrl Pts',(3.23043456092505,5.94614005448753,-56.961233908153));
#33397=CARTESIAN_POINT('Ctrl Pts',(3.18690768806459,5.96978744811246,-56.9589038194199));
#33398=CARTESIAN_POINT('Ctrl Pts',(3.14312114982915,5.99295688499283,-56.9565737306869));
#33399=CARTESIAN_POINT('Ctrl Pts',(3.0990855038472,6.01564277861012,-56.9542436419538));
#33400=CARTESIAN_POINT('Ctrl Pts',(3.09908550384722,6.01564277861012,-58.9542133848184));
#33401=CARTESIAN_POINT('Ctrl Pts',(2.9385078993557,6.09836772499351,-58.9457310075084));
#33402=CARTESIAN_POINT('Ctrl Pts',(2.77456632796542,6.1746848698411,-58.9372486301984));
#33403=CARTESIAN_POINT('Ctrl Pts',(2.60779751086059,6.24433192121858,-58.9287662528885));
#33404=CARTESIAN_POINT('Ctrl Pts',(2.51159575789531,6.28450830759401,-58.9238731344944));
#33405=CARTESIAN_POINT('Ctrl Pts',(2.41445365413025,6.32246597896167,-58.9189800161003));
#33406=CARTESIAN_POINT('Ctrl Pts',(2.31647755692632,6.35816174127842,-58.9140868977063));
#33407=CARTESIAN_POINT('Ctrl Pts',(2.14471510779725,6.42074018371518,-58.9055087442257));
#33408=CARTESIAN_POINT('Ctrl Pts',(1.97046722237144,6.47633555656743,-58.8969305907451));
#33409=CARTESIAN_POINT('Ctrl Pts',(1.79432006926173,6.52477620221909,-58.8883524372645));
#33410=CARTESIAN_POINT('Ctrl Pts',(1.61808399810324,6.57324130042429,-58.8797699535824));
#33411=CARTESIAN_POINT('Ctrl Pts',(1.43994704554636,6.61454438269761,-58.8711874699003));
#33412=CARTESIAN_POINT('Ctrl Pts',(1.26050759114,6.64856447759052,-58.8626049862182));
#33413=CARTESIAN_POINT('Ctrl Pts',(1.07359002331164,6.68400235503898,-58.8536648287646));
#33414=CARTESIAN_POINT('Ctrl Pts',(0.885259433514967,6.71153712926666,-58.844724671311));
#33415=CARTESIAN_POINT('Ctrl Pts',(0.696199858256236,6.73109164678093,-58.8357845138573));
#33416=CARTESIAN_POINT('Ctrl Pts',(0.514391573134188,6.74989616007148,-58.827187251893));
#33417=CARTESIAN_POINT('Ctrl Pts',(0.331909494109158,6.76132118859279,-58.8185899899287));
#33418=CARTESIAN_POINT('Ctrl Pts',(0.149363924244205,6.76535138911013,-58.8099927279644));
#33419=CARTESIAN_POINT('Ctrl Pts',(-0.0332950379045321,6.76938409307712,
-58.8013901256175));
#33420=CARTESIAN_POINT('Ctrl Pts',(-0.216017259489319,6.76601280294623,
-58.7927875232707));
#33421=CARTESIAN_POINT('Ctrl Pts',(-0.398194069133422,6.75527427150867,
-58.7841849209238));
#33422=CARTESIAN_POINT('Ctrl Pts',(-0.58056151314086,6.74452450300363,-58.7755733165991));
#33423=CARTESIAN_POINT('Ctrl Pts',(-0.762382095803028,6.72639211564653,
-58.7669617122743));
#33424=CARTESIAN_POINT('Ctrl Pts',(-0.943052648207334,6.70096565449407,
-58.7583501079495));
#33425=CARTESIAN_POINT('Ctrl Pts',(-0.964221440163454,6.69798648905093,
-58.7573411042246));
#33426=CARTESIAN_POINT('Ctrl Pts',(-0.985374455570215,6.69490724591875,
-58.7563321004997));
#33427=CARTESIAN_POINT('Ctrl Pts',(-1.00651073389821,6.6917281133163,-58.7553230967747));
#33428=CARTESIAN_POINT('Ctrl Pts',(-1.19639319196643,6.66316766839261,-58.7462584873617));
#33429=CARTESIAN_POINT('Ctrl Pts',(-1.38510326363246,6.62651425917618,-58.7371938779487));
#33430=CARTESIAN_POINT('Ctrl Pts',(-1.5719757120565,6.58188281274473,-58.7281292685357));
#33431=CARTESIAN_POINT('Ctrl Pts',(-1.75868033247639,6.53729144930379,-58.7190727999445));
#33432=CARTESIAN_POINT('Ctrl Pts',(-1.94355039732936,6.48473640864038,-58.7100163313533));
#33433=CARTESIAN_POINT('Ctrl Pts',(-2.12593175892476,6.42438348453726,-58.7009598627621));
#33434=CARTESIAN_POINT('Ctrl Pts',(-2.3079879218244,6.36413817390973,-58.6919195424865));
#33435=CARTESIAN_POINT('Ctrl Pts',(-2.48756402096188,6.29612281874464,-58.6828792222108));
#33436=CARTESIAN_POINT('Ctrl Pts',(-2.66402210667442,6.22055264547693,-58.6738389019351));
#33437=CARTESIAN_POINT('Ctrl Pts',(-2.8402535542687,6.14507953254961,-58.6648101928088));
#33438=CARTESIAN_POINT('Ctrl Pts',(-3.01337476617588,6.06207105819907,-58.6557814836824));
#33439=CARTESIAN_POINT('Ctrl Pts',(-3.18276633312787,5.97179097664242,-58.646752774556));
#33440=CARTESIAN_POINT('Ctrl Pts',(-3.35176147924415,5.88172217423043,-58.6377451949846));
#33441=CARTESIAN_POINT('Ctrl Pts',(-3.51704419658996,5.78441584249337,-58.6287376154131));
#33442=CARTESIAN_POINT('Ctrl Pts',(-3.67801877212276,5.68018194355714,-58.6197300358416));
#33443=CARTESIAN_POINT('Ctrl Pts',(-3.81604697405473,5.59080622939292,-58.6120064558422));
#33444=CARTESIAN_POINT('Ctrl Pts',(-3.95090794947756,5.4963379921662,-58.6042828758427));
#33445=CARTESIAN_POINT('Ctrl Pts',(-4.08223937590867,5.39700015543643,-58.5965592958432));
#33446=CARTESIAN_POINT('Ctrl Pts',(-4.22032311992663,5.29255493016897,-58.5884386131359));
#33447=CARTESIAN_POINT('Ctrl Pts',(-4.35444043945768,5.18277314809975,-58.5803179304286));
#33448=CARTESIAN_POINT('Ctrl Pts',(-4.4841587435886,5.06799855586975,-58.5721972477212));
#33449=CARTESIAN_POINT('Ctrl Pts',(-4.61386773174815,4.95323220639951,-58.5640771482165));
#33450=CARTESIAN_POINT('Ctrl Pts',(-4.73917805946965,4.83347400370038,-58.5559570487117));
#33451=CARTESIAN_POINT('Ctrl Pts',(-4.85969140119417,4.70910697321259,-58.5478369492069));
#33452=CARTESIAN_POINT('Ctrl Pts',(-4.98021909909504,4.58472512747699,-58.5397158823937));
#33453=CARTESIAN_POINT('Ctrl Pts',(-5.09594841911797,4.45573362459593,-58.5315948155804));
#33454=CARTESIAN_POINT('Ctrl Pts',(-5.20651902378243,4.32255117436354,-58.5234737487671));
#33455=CARTESIAN_POINT('Ctrl Pts',(-5.31717012042056,4.18927177143464,-58.5153467700689));
#33456=CARTESIAN_POINT('Ctrl Pts',(-5.42265476702151,4.05179560985903,-58.5072197913706));
#33457=CARTESIAN_POINT('Ctrl Pts',(-5.52265355950414,3.91057369981647,-58.4990928126724));
#33458=CARTESIAN_POINT('Ctrl Pts',(-5.62269307460422,3.76929427982127,-58.4909625244157));
#33459=CARTESIAN_POINT('Ctrl Pts',(-5.71724208271152,3.62426637746686,-58.4828322361591));
#33460=CARTESIAN_POINT('Ctrl Pts',(-5.80602556896683,3.47596836759247,-58.4747019479024));
#33461=CARTESIAN_POINT('Ctrl Pts',(-5.8949056740352,3.32750897210123,-58.4665628118427));
#33462=CARTESIAN_POINT('Ctrl Pts',(-5.97800754972974,3.17577268211546,-58.458423675783));
#33463=CARTESIAN_POINT('Ctrl Pts',(-6.0551026827931,3.02126140888732,-58.4502845397233));
#33464=CARTESIAN_POINT('Ctrl Pts',(-6.09453539262529,2.94223180013108,-58.4461215247861));
#33465=CARTESIAN_POINT('Ctrl Pts',(-6.1323974378594,2.86247654218005,-58.4419585098489));
#33466=CARTESIAN_POINT('Ctrl Pts',(-6.16866320271028,2.78206457357269,-58.4377954949117));
#33467=CARTESIAN_POINT('Ctrl Pts',(-6.24890574610109,2.60414302947599,-58.4285843033621));
#33468=CARTESIAN_POINT('Ctrl Pts',(-6.32146502909445,2.42270742807501,-58.4193731118125));
#33469=CARTESIAN_POINT('Ctrl Pts',(-6.38606698025806,2.23840066200352,-58.4101619202629));
#33470=CARTESIAN_POINT('Ctrl Pts',(-6.45054079326273,2.05445946894117,-58.4009689991387));
#33471=CARTESIAN_POINT('Ctrl Pts',(-6.50708872917064,1.86765867644806,-58.3917760780145));
#33472=CARTESIAN_POINT('Ctrl Pts',(-6.55548604261071,1.67865772125712,-58.3825831568902));
#33473=CARTESIAN_POINT('Ctrl Pts',(-6.60380870361076,1.48994829841517,-58.3734044157678));
#33474=CARTESIAN_POINT('Ctrl Pts',(-6.64400578671844,1.29904568319861,-58.3642256746454));
#33475=CARTESIAN_POINT('Ctrl Pts',(-6.67590239598728,1.10662378397148,-58.355046933523));
#33476=CARTESIAN_POINT('Ctrl Pts',(-6.70769975114459,0.91480065260973,-58.3458967543016));
#33477=CARTESIAN_POINT('Ctrl Pts',(-6.73124814657676,0.721467872861489,
-58.3367465750801));
#33478=CARTESIAN_POINT('Ctrl Pts',(-6.74642391635618,0.527307633945599,
-58.3275963958587));
#33479=CARTESIAN_POINT('Ctrl Pts',(-6.76012119264503,0.352063381074478,
-58.3193376693025));
#33480=CARTESIAN_POINT('Ctrl Pts',(-6.76699835261893,0.176145328877515,
-58.3110789427462));
#33481=CARTESIAN_POINT('Ctrl Pts',(-6.76699999970395,6.32990448600232E-5,
-58.30282021619));
#33482=CARTESIAN_POINT('',(-6.76699969186032,0.00204214650334386,-58.697179783784));
#33483=CARTESIAN_POINT('Ctrl Pts',(3.09908550384721,6.01564277861012,-59.3485564563465));
#33484=CARTESIAN_POINT('Ctrl Pts',(2.94204903435842,6.09654343446331,-59.3402328834935));
#33485=CARTESIAN_POINT('Ctrl Pts',(2.78171749018946,6.17135568762416,-59.3319093106405));
#33486=CARTESIAN_POINT('Ctrl Pts',(2.61859746282639,6.23981060030504,-59.3235857377875));
#33487=CARTESIAN_POINT('Ctrl Pts',(2.45558899639079,6.30821869535309,-59.3152678575863));
#33488=CARTESIAN_POINT('Ctrl Pts',(2.28979616522525,6.3702779803494,-59.306949977385));
#33489=CARTESIAN_POINT('Ctrl Pts',(2.12174835011713,6.42576633085699,-59.2986320971838));
#33490=CARTESIAN_POINT('Ctrl Pts',(1.95378515990411,6.48122673874694,-59.2903184056698));
#33491=CARTESIAN_POINT('Ctrl Pts',(1.78356957698955,6.5301226983669,-59.2820047141558));
#33492=CARTESIAN_POINT('Ctrl Pts',(1.61164929851767,6.5722808475131,-59.2736910226418));
#33493=CARTESIAN_POINT('Ctrl Pts',(1.43978460285766,6.61442536668793,-59.2653800189919));
#33494=CARTESIAN_POINT('Ctrl Pts',(1.26621664615083,6.64983633512498,-59.257069015342));
#33495=CARTESIAN_POINT('Ctrl Pts',(1.09150680360186,6.67839066674681,-59.2487580116922));
#33496=CARTESIAN_POINT('Ctrl Pts',(0.91515314059552,6.7072136620786,-59.2403688109721));
#33497=CARTESIAN_POINT('Ctrl Pts',(0.737636340209878,6.72905024018178,-59.2319796102521));
#33498=CARTESIAN_POINT('Ctrl Pts',(0.559543225414115,6.74382683488338,-59.223590409532));
#33499=CARTESIAN_POINT('Ctrl Pts',(0.38308548831206,6.75846774037885,-59.2152782444219));
#33500=CARTESIAN_POINT('Ctrl Pts',(0.206062329101349,6.76617778150654,-59.2069660793118));
#33501=CARTESIAN_POINT('Ctrl Pts',(0.0290485527314963,6.76693765166964,
-59.1986539142017));
#33502=CARTESIAN_POINT('Ctrl Pts',(-0.148006811632621,6.76769770035826,
-59.1903397962138));
#33503=CARTESIAN_POINT('Ctrl Pts',(-0.325052442269068,6.76150432174146,
-59.1820256782259));
#33504=CARTESIAN_POINT('Ctrl Pts',(-0.50151435591173,6.74839035258146,-59.1737115602379));
#33505=CARTESIAN_POINT('Ctrl Pts',(-0.678046593149869,6.73527115724293,
-59.165394128908));
#33506=CARTESIAN_POINT('Ctrl Pts',(-0.85399430440421,6.71522589991034,-59.1570766975781));
#33507=CARTESIAN_POINT('Ctrl Pts',(-1.0287892300239,6.68833923483153,-59.1487592662482));
#33508=CARTESIAN_POINT('Ctrl Pts',(-1.20626870261506,6.66103963719731,-59.1403140935951));
#33509=CARTESIAN_POINT('Ctrl Pts',(-1.38255932370079,6.62668682920984,-59.131868920942));
#33510=CARTESIAN_POINT('Ctrl Pts',(-1.55707840793328,6.58542298045828,-59.1234237482889));
#33511=CARTESIAN_POINT('Ctrl Pts',(-1.72926629274015,6.54471032793222,-59.1150913849696));
#33512=CARTESIAN_POINT('Ctrl Pts',(-1.89972935757813,6.49727027205983,-59.1067590216504));
#33513=CARTESIAN_POINT('Ctrl Pts',(-2.06792469169362,6.44328925856071,-59.0984266583311));
#33514=CARTESIAN_POINT('Ctrl Pts',(-2.23953574405249,6.38821199626507,-59.0899250810111));
#33515=CARTESIAN_POINT('Ctrl Pts',(-2.40878561572041,6.32632540951042,-59.081423503691));
#33516=CARTESIAN_POINT('Ctrl Pts',(-2.57512064742921,6.25787844650116,-59.072921926371));
#33517=CARTESIAN_POINT('Ctrl Pts',(-2.74145567913801,6.1894314834919,-59.0644203490509));
#33518=CARTESIAN_POINT('Ctrl Pts',(-2.90487555119516,6.11442435236039,-59.0559187717309));
#33519=CARTESIAN_POINT('Ctrl Pts',(-3.06485477752562,6.03315458053897,-59.0474171944109));
#33520=CARTESIAN_POINT('Ctrl Pts',(-3.21640177601162,5.95616839758458,-59.0393637205018));
#33521=CARTESIAN_POINT('Ctrl Pts',(-3.36533074803328,5.87332373605608,-59.0313102465927));
#33522=CARTESIAN_POINT('Ctrl Pts',(-3.51114288843178,5.78482191748501,-59.0232567726836));
#33523=CARTESIAN_POINT('Ctrl Pts',(-3.65677177158295,5.69643132833291,-59.0152134204109));
#33524=CARTESIAN_POINT('Ctrl Pts',(-3.79929130074251,5.60239791966642,-59.0071700681381));
#33525=CARTESIAN_POINT('Ctrl Pts',(-3.93822320620494,5.50297074116417,-58.9991267158654));
#33526=CARTESIAN_POINT('Ctrl Pts',(-4.07701121168828,5.40364654526234,-58.9910916945676));
#33527=CARTESIAN_POINT('Ctrl Pts',(-4.21221868567955,5.29893991223907,-58.9830566732698));
#33528=CARTESIAN_POINT('Ctrl Pts',(-4.34339262978699,5.18914535000824,-58.975021651972));
#33529=CARTESIAN_POINT('Ctrl Pts',(-4.47445965328987,5.07944028192999,-58.9669931800643));
#33530=CARTESIAN_POINT('Ctrl Pts',(-4.6014994043802,4.96465577743627,-58.9589647081566));
#33531=CARTESIAN_POINT('Ctrl Pts',(-4.72408863568108,4.84512905527076,-58.950936236249));
#33532=CARTESIAN_POINT('Ctrl Pts',(-4.8466049598885,4.72567341884265,-58.9429125390882));
#33533=CARTESIAN_POINT('Ctrl Pts',(-4.96467576547952,4.60148143953182,-58.9348888419275));
#33534=CARTESIAN_POINT('Ctrl Pts',(-5.07791173080715,4.47292985124193,-58.9268651447667));
#33535=CARTESIAN_POINT('Ctrl Pts',(-5.19373903353787,4.3414364366692,-58.9186578300909));
#33536=CARTESIAN_POINT('Ctrl Pts',(-5.30450724105058,4.20538173634522,-58.9104505154151));
#33537=CARTESIAN_POINT('Ctrl Pts',(-5.40984015990395,4.06520829039428,-58.9022432007393));
#33538=CARTESIAN_POINT('Ctrl Pts',(-5.51278298464656,3.92821549994307,-58.8942221170603));
#33539=CARTESIAN_POINT('Ctrl Pts',(-5.61053430555352,3.78728918931021,-58.8862010333813));
#33540=CARTESIAN_POINT('Ctrl Pts',(-5.70278454423253,3.64287488696258,-58.8781799497023));
#33541=CARTESIAN_POINT('Ctrl Pts',(-5.79504454307941,3.49844530543676,-58.8701580173846));
#33542=CARTESIAN_POINT('Ctrl Pts',(-5.8818020988733,3.35052731348723,-58.8621360850669));
#33543=CARTESIAN_POINT('Ctrl Pts',(-5.96279189361212,3.19959401072598,-58.8541141527492));
#33544=CARTESIAN_POINT('Ctrl Pts',(-6.04380641070806,3.04861463515984,-58.8460897717146));
#33545=CARTESIAN_POINT('Ctrl Pts',(-6.11904948530044,2.89461844711971,-58.8380653906801));
#33546=CARTESIAN_POINT('Ctrl Pts',(-6.1883026182268,2.7381014782596,-58.8300410096455));
#33547=CARTESIAN_POINT('Ctrl Pts',(-6.26033101280687,2.57531222216166,-58.8216950582207));
#33548=CARTESIAN_POINT('Ctrl Pts',(-6.32587926744313,2.40979638277819,-58.8133491067959));
#33549=CARTESIAN_POINT('Ctrl Pts',(-6.38475794488179,2.24213179480353,-58.8050031553711));
#33550=CARTESIAN_POINT('Ctrl Pts',(-6.44146878025008,2.08064041525226,-58.7969644918373));
#33551=CARTESIAN_POINT('Ctrl Pts',(-6.49199238196718,1.91715607036079,-58.7889258283035));
#33552=CARTESIAN_POINT('Ctrl Pts',(-6.53621138762681,1.75220709285677,-58.7808871647698));
#33553=CARTESIAN_POINT('Ctrl Pts',(-6.58046408208749,1.58713244691668,-58.7728423768799));
#33554=CARTESIAN_POINT('Ctrl Pts',(-6.61840253497921,1.42059130980724,-58.76479758899));
#33555=CARTESIAN_POINT('Ctrl Pts',(-6.64996096528673,1.25311937187275,-58.7567528011001));
#33556=CARTESIAN_POINT('Ctrl Pts',(-6.68156429965934,1.08540914037527,-58.74869656639));
#33557=CARTESIAN_POINT('Ctrl Pts',(-6.70676944525687,0.916765832943588,
-58.7406403316799));
#33558=CARTESIAN_POINT('Ctrl Pts',(-6.72556257117393,0.747727959370447,
-58.7325840969698));
#33559=CARTESIAN_POINT('Ctrl Pts',(-6.72765776670496,0.728882377275807,
-58.7316859288292));
#33560=CARTESIAN_POINT('Ctrl Pts',(-6.72967331775269,0.710031888070401,
-58.7307877606885));
#33561=CARTESIAN_POINT('Ctrl Pts',(-6.73160924515994,0.691177235213417,
-58.7298895925479));
#33562=CARTESIAN_POINT('Ctrl Pts',(-6.75511034417722,0.462292070372445,
-58.7189863229686));
#33563=CARTESIAN_POINT('Ctrl Pts',(-6.76693020279762,0.232305909665429,
-58.7080830533894));
#33564=CARTESIAN_POINT('Ctrl Pts',(-6.76699969186015,0.0020421470552204,
-58.6971797838101));
#33565=CARTESIAN_POINT('Ctrl Pts',(-6.76699969186032,0.00204214650334836,
-58.697179783784));
#33566=CARTESIAN_POINT('Ctrl Pts',(-6.76705174932313,-0.170459108531269,
-58.6890116392827));
#33567=CARTESIAN_POINT('Ctrl Pts',(-6.760503606502,-0.343228945885599,-58.6808434947815));
#33568=CARTESIAN_POINT('Ctrl Pts',(-6.74731979635412,-0.51571752513159,
-58.6726753502803));
#33569=CARTESIAN_POINT('Ctrl Pts',(-6.73415147684863,-0.688003434673666,
-58.6645168031416));
#33570=CARTESIAN_POINT('Ctrl Pts',(-6.71436303929249,-0.860008384080678,
-58.6563582560029));
#33571=CARTESIAN_POINT('Ctrl Pts',(-6.68797097171816,-1.03118052806252,
-58.6481997088642));
#33572=CARTESIAN_POINT('Ctrl Pts',(-6.66160439981937,-1.20218731366787,
-58.6400490431721));
#33573=CARTESIAN_POINT('Ctrl Pts',(-6.62864695501451,-1.37236253781669,
-58.63189837748));
#33574=CARTESIAN_POINT('Ctrl Pts',(-6.58916706896801,-1.54115746672023,
-58.6237477117878));
#33575=CARTESIAN_POINT('Ctrl Pts',(-6.54971707722324,-1.7098245835392,-58.615603217807));
#33576=CARTESIAN_POINT('Ctrl Pts',(-6.5037545622998,-1.87711313297762,-58.6074587238262));
#33577=CARTESIAN_POINT('Ctrl Pts',(-6.45139937517315,-2.04248258303848,
-58.5993142298454));
#33578=CARTESIAN_POINT('Ctrl Pts',(-6.3990721435299,-2.20776373271935,-58.5911740846843));
#33579=CARTESIAN_POINT('Ctrl Pts',(-6.34035914781289,-2.37112747711318,
-58.5830339395231));
#33580=CARTESIAN_POINT('Ctrl Pts',(-6.27543063422767,-2.53204647567869,
-58.574893794362));
#33581=CARTESIAN_POINT('Ctrl Pts',(-6.21052006539869,-2.69292099991323,
-58.5667558989508));
#33582=CARTESIAN_POINT('Ctrl Pts',(-6.13939753469528,-2.85135178557048,
-58.5586180035396));
#33583=CARTESIAN_POINT('Ctrl Pts',(-6.06228219297214,-3.0068294951282,-58.5504801081284));
#33584=CARTESIAN_POINT('Ctrl Pts',(-5.98517358418205,-3.16229362994209,
-58.5423429232361));
#33585=CARTESIAN_POINT('Ctrl Pts',(-5.90207336845691,-3.31480487554985,
-58.5342057383437));
#33586=CARTESIAN_POINT('Ctrl Pts',(-5.81324759547167,-3.46387664239691,
-58.5260685534514));
#33587=CARTESIAN_POINT('Ctrl Pts',(-5.72441278368444,-3.61296357860458,
-58.5179305405291));
#33588=CARTESIAN_POINT('Ctrl Pts',(-5.62985144195675,-3.75861002640123,
-58.5097925276068));
#33589=CARTESIAN_POINT('Ctrl Pts',(-5.52987404155567,-3.90035666119508,
-58.5016545146845));
#33590=CARTESIAN_POINT('Ctrl Pts',(-5.4298244899644,-4.04220559099123,-58.4935106287617));
#33591=CARTESIAN_POINT('Ctrl Pts',(-5.3243512822683,-4.18014878748545,-58.4853667428389));
#33592=CARTESIAN_POINT('Ctrl Pts',(-5.2138068521877,-4.31375788704937,-58.4772228569162));
#33593=CARTESIAN_POINT('Ctrl Pts',(-5.10321950396809,-4.44741885945667,
-58.4690758091839));
#33594=CARTESIAN_POINT('Ctrl Pts',(-4.98755725111889,-4.57674210857437,
-58.4609287614517));
#33595=CARTESIAN_POINT('Ctrl Pts',(-4.86721064423119,-4.70133486838394,
-58.4527817137194));
#33596=CARTESIAN_POINT('Ctrl Pts',(-4.74672937326799,-4.82606704358085,
-58.4446255496965));
#33597=CARTESIAN_POINT('Ctrl Pts',(-4.62155353956678,-4.94605790233777,
-58.4364693856735));
#33598=CARTESIAN_POINT('Ctrl Pts',(-4.49210876334145,-5.06095325589072,
-58.4283132216506));
#33599=CARTESIAN_POINT('Ctrl Pts',(-4.40772254464528,-5.13585457454431,
-58.422996144662));
#33600=CARTESIAN_POINT('Ctrl Pts',(-4.321522767971,-5.20859120198429,-58.4176790676734));
#33601=CARTESIAN_POINT('Ctrl Pts',(-4.23363416781977,-5.27907479896516,
-58.4123619906848));
#33602=CARTESIAN_POINT('Ctrl Pts',(-4.09297788917386,-5.39187623669255,
-58.4038525792116));
#33603=CARTESIAN_POINT('Ctrl Pts',(-3.94770173405893,-5.49914015861868,
-58.3953431677384));
#33604=CARTESIAN_POINT('Ctrl Pts',(-3.79826584460406,-5.60048797639225,
-58.3868337562653));
#33605=CARTESIAN_POINT('Ctrl Pts',(-3.64896159635609,-5.7017465147491,-58.378331840911));
#33606=CARTESIAN_POINT('Ctrl Pts',(-3.49550518616764,-5.79709915785418,
-58.3698299255567));
#33607=CARTESIAN_POINT('Ctrl Pts',(-3.33838846695244,-5.88620857969873,
-58.3613280102024));
#33608=CARTESIAN_POINT('Ctrl Pts',(-3.18139142156546,-5.97525012801782,
-58.3528325706501));
#33609=CARTESIAN_POINT('Ctrl Pts',(-3.02073990693433,-6.05805777719225,
-58.3443371310978));
#33610=CARTESIAN_POINT('Ctrl Pts',(-2.856953699825,-6.13433815150879,-58.3358416915454));
#33611=CARTESIAN_POINT('Ctrl Pts',(-2.6932945390989,-6.21055935633945,-58.3273528417719));
#33612=CARTESIAN_POINT('Ctrl Pts',(-2.52650582994074,-6.2802632510887,-58.3188639919983));
#33613=CARTESIAN_POINT('Ctrl Pts',(-2.35713103877984,-6.34320283973489,
-58.3103751422247));
#33614=CARTESIAN_POINT('Ctrl Pts',(-2.18783652024992,-6.40611259911109,
-58.3018903156137));
#33615=CARTESIAN_POINT('Ctrl Pts',(-2.01595866646391,-6.46226433152078,
-58.2934054890026));
#33616=CARTESIAN_POINT('Ctrl Pts',(-1.842060715962,-6.51145923113319,-58.2849206623915));
#33617=CARTESIAN_POINT('Ctrl Pts',(-1.66823269249806,-6.56063434872054,
-58.2764392476596));
#33618=CARTESIAN_POINT('Ctrl Pts',(-1.49238650401947,-6.6028581257128,-58.2679578329277));
#33619=CARTESIAN_POINT('Ctrl Pts',(-1.31510071641706,-6.63798155358083,
-58.2594764181957));
#33620=CARTESIAN_POINT('Ctrl Pts',(-1.27414346293795,-6.6460959047519,-58.2575170087149));
#33621=CARTESIAN_POINT('Ctrl Pts',(-1.23310943135344,-6.65383150798569,
-58.2555575992342));
#33622=CARTESIAN_POINT('Ctrl Pts',(-1.19200584984678,-6.66118691029842,
-58.2535981897534));
#33623=CARTESIAN_POINT('Ctrl Pts',(-1.01205733259058,-6.69338833147594,
-58.2450200362728));
#33624=CARTESIAN_POINT('Ctrl Pts',(-0.830857499226969,-6.71828394247207,
-58.2364418827922));
#33625=CARTESIAN_POINT('Ctrl Pts',(-0.649013270227526,-6.73580513191026,
-58.2278637293117));
#33626=CARTESIAN_POINT('Ctrl Pts',(-0.46707724732893,-6.75333516594201,
-58.2192812456296));
#33627=CARTESIAN_POINT('Ctrl Pts',(-0.284496488699637,-6.76348332093542,
-58.2106987619475));
#33628=CARTESIAN_POINT('Ctrl Pts',(-0.1018812542915,-6.76623301475969,-58.2021162782654));
#33629=CARTESIAN_POINT('Ctrl Pts',(0.0883444437133825,-6.76909730167812,
-58.1931761208118));
#33630=CARTESIAN_POINT('Ctrl Pts',(0.278607176176113,-6.76393324505317,
-58.1842359633581));
#33631=CARTESIAN_POINT('Ctrl Pts',(0.468219807672953,-6.75078211851802,
-58.1752958059045));
#33632=CARTESIAN_POINT('Ctrl Pts',(0.650559936823868,-6.73813539718956,
-58.1666985439402));
#33633=CARTESIAN_POINT('Ctrl Pts',(0.832298598842978,-6.71810294428104,
-58.1581012819758));
#33634=CARTESIAN_POINT('Ctrl Pts',(1.01283189780068,-6.69077428604474,-58.1495040200115));
#33635=CARTESIAN_POINT('Ctrl Pts',(1.19347733907426,-6.6634286519982,-58.1409014176647));
#33636=CARTESIAN_POINT('Ctrl Pts',(1.3729156176953,-6.62877782194559,-58.1322988153179));
#33637=CARTESIAN_POINT('Ctrl Pts',(1.55055337761689,-6.58696236691549,-58.1236962129711));
#33638=CARTESIAN_POINT('Ctrl Pts',(1.7283770221265,-6.54510315514901,-58.1150846086463));
#33639=CARTESIAN_POINT('Ctrl Pts',(1.9043960833695,-6.49606441709743,-58.1064730043216));
#33640=CARTESIAN_POINT('Ctrl Pts',(2.07803150655507,-6.44003680562188,-58.0978613999968));
#33641=CARTESIAN_POINT('Ctrl Pts',(2.09837600708972,-6.43347216719323,-58.0968523962718));
#33642=CARTESIAN_POINT('Ctrl Pts',(2.11868780543457,-6.42681163814909,-58.0958433925468));
#33643=CARTESIAN_POINT('Ctrl Pts',(2.13896598755644,-6.42005556861284,-58.0948343888218));
#33644=CARTESIAN_POINT('Ctrl Pts',(2.32113954745933,-6.35936091506975,-58.0857697794088));
#33645=CARTESIAN_POINT('Ctrl Pts',(2.50077046684595,-6.29089416141631,-58.0767051699957));
#33646=CARTESIAN_POINT('Ctrl Pts',(2.67722306560071,-6.21488259398483,-58.0676405605827));
#33647=CARTESIAN_POINT('Ctrl Pts',(2.8535171942986,-6.13893929167099,-58.0585840919915));
#33648=CARTESIAN_POINT('Ctrl Pts',(3.02663848676848,-6.05546479693483,-58.0495276234003));
#33649=CARTESIAN_POINT('Ctrl Pts',(3.19597090940745,-5.96473460819686,-58.0404711548091));
#33650=CARTESIAN_POINT('Ctrl Pts',(3.36500140051961,-5.87416619771721,-58.0314308345334));
#33651=CARTESIAN_POINT('Ctrl Pts',(3.53025630660027,-5.77636803855244,-58.0223905142577));
#33652=CARTESIAN_POINT('Ctrl Pts',(3.6911440278994,-5.67166155242911,-58.013350193982));
#33653=CARTESIAN_POINT('Ctrl Pts',(3.85182510924757,-5.56708954855827,-58.0043214848556));
#33654=CARTESIAN_POINT('Ctrl Pts',(4.0081500044057,-5.45562705271022,-57.9952927757291));
#33655=CARTESIAN_POINT('Ctrl Pts',(4.15955370000717,-5.3376401168266,-57.9862640666026));
#33656=CARTESIAN_POINT('Ctrl Pts',(4.31060307112361,-5.21992930141765,-57.9772564870312));
#33657=CARTESIAN_POINT('Ctrl Pts',(4.45675404689378,-5.09572466732177,-57.9682489074597));
#33658=CARTESIAN_POINT('Ctrl Pts',(4.59747288204903,-4.96543372716058,-57.9592413278882));
#33659=CARTESIAN_POINT('Ctrl Pts',(4.71813272991491,-4.85371531362478,-57.9515177478889));
#33660=CARTESIAN_POINT('Ctrl Pts',(4.83479909263464,-4.73752284250249,-57.9437941678896));
#33661=CARTESIAN_POINT('Ctrl Pts',(4.94715323566637,-4.61713805975474,-57.9360705878902));
#33662=CARTESIAN_POINT('Ctrl Pts',(5.06528399193408,-4.49056377379272,-57.9279499051829));
#33663=CARTESIAN_POINT('Ctrl Pts',(5.1785920583601,-4.35941204046347,-57.9198292224756));
#33664=CARTESIAN_POINT('Ctrl Pts',(5.28671018883337,-4.22409568775205,-57.9117085397683));
#33665=CARTESIAN_POINT('Ctrl Pts',(5.39482055459339,-4.08878905304696,-57.9035884402635));
#33666=CARTESIAN_POINT('Ctrl Pts',(5.49774149818126,-3.94931868085896,-57.8954683407588));
#33667=CARTESIAN_POINT('Ctrl Pts',(5.59514626613433,-3.80613022117782,-57.887348241254));
#33668=CARTESIAN_POINT('Ctrl Pts',(5.69256263745054,-3.66292470414177,-57.8792271744407));
#33669=CARTESIAN_POINT('Ctrl Pts',(5.784461319662,-3.51600052118882,-57.8711061076275));
#33670=CARTESIAN_POINT('Ctrl Pts',(5.87055910324752,-3.36583196480124,-57.8629850408142));
#33671=CARTESIAN_POINT('Ctrl Pts',(5.95671956335136,-3.21555409035823,-57.8548580621159));
#33672=CARTESIAN_POINT('Ctrl Pts',(6.03707050829024,-3.06202744342804,-57.8467310834177));
#33673=CARTESIAN_POINT('Ctrl Pts',(6.11137459397512,-2.90575112012633,-57.8386041047194));
#33674=CARTESIAN_POINT('Ctrl Pts',(6.18570893859352,-2.74941115624775,-57.8304738164628));
#33675=CARTESIAN_POINT('Ctrl Pts',(6.25399137123533,-2.59031962037084,-57.8223435282062));
#33676=CARTESIAN_POINT('Ctrl Pts',(6.31603297161226,-2.42899495707726,-57.8142132399496));
#33677=CARTESIAN_POINT('Ctrl Pts',(6.3781420888897,-2.26749473188369,-57.8060741038899));
#33678=CARTESIAN_POINT('Ctrl Pts',(6.43399669087256,-2.10375687163168,-57.7979349678302));
#33679=CARTESIAN_POINT('Ctrl Pts',(6.483457705782,-1.93831503562658,-57.7897958317704));
#33680=CARTESIAN_POINT('Ctrl Pts',(6.50875608418085,-1.85369464969391,-57.7856328168332));
#33681=CARTESIAN_POINT('Ctrl Pts',(6.53238263822974,-1.76862866598685,-57.781469801896));
#33682=CARTESIAN_POINT('Ctrl Pts',(6.55432395165231,-1.6831893942147,-57.7773067869588));
#33683=CARTESIAN_POINT('Ctrl Pts',(6.5988065897061,-1.50997441256694,-57.7688669145091));
#33684=CARTESIAN_POINT('Ctrl Pts',(6.63645154722509,-1.33486650797698,-57.7604270420594));
#33685=CARTESIAN_POINT('Ctrl Pts',(6.66710754627038,-1.15843254722258,-57.7519871696097));
#33686=CARTESIAN_POINT('Ctrl Pts',(6.6977403006791,-0.98213236593789,-57.7435536966177));
#33687=CARTESIAN_POINT('Ctrl Pts',(6.72139460354281,-0.804508460243176,
-57.7351202236257));
#33688=CARTESIAN_POINT('Ctrl Pts',(6.73796991017135,-0.626139353199828,
-57.7266867506337));
#33689=CARTESIAN_POINT('Ctrl Pts',(6.75453519834567,-0.447878056091589,
-57.7182583750051));
#33690=CARTESIAN_POINT('Ctrl Pts',(6.76402998967732,-0.268872786861646,
-57.7098299993766));
#33691=CARTESIAN_POINT('Ctrl Pts',(6.76640534414454,-0.0897090783152398,
-57.7014016237481));
#33692=CARTESIAN_POINT('Ctrl Pts',(6.76877962787636,0.0893738688426241,
-57.6929770473673));
#33693=CARTESIAN_POINT('Ctrl Pts',(6.76404086914789,0.268614779974892,-57.6845524709865));
#33694=CARTESIAN_POINT('Ctrl Pts',(6.7521921726132,0.447425819662907,-57.6761278946058));
#33695=CARTESIAN_POINT('Ctrl Pts',(6.74034699804638,0.626183708632252,-57.6677058223897));
#33696=CARTESIAN_POINT('Ctrl Pts',(6.7213961222744,0.804511648534019,-57.6592837501736));
#33697=CARTESIAN_POINT('Ctrl Pts',(6.69539469960215,0.981824228942961,-57.6508616779575));
#33698=CARTESIAN_POINT('Ctrl Pts',(6.66939289198227,1.15913943444125,-57.6424394810537));
#33699=CARTESIAN_POINT('Ctrl Pts',(6.63634037071619,1.33543891953788,-57.63401728415));
#33700=CARTESIAN_POINT('Ctrl Pts',(6.59634396466023,1.51014413215779,-57.6255950872462));
#33701=CARTESIAN_POINT('Ctrl Pts',(6.55634621297761,1.68485522250557,-57.6171726069887));
#33702=CARTESIAN_POINT('Ctrl Pts',(6.50940418498622,1.85797160819041,-57.6087501267312));
#33703=CARTESIAN_POINT('Ctrl Pts',(6.45567551203003,2.02892648545378,-57.6003276464736));
#33704=CARTESIAN_POINT('Ctrl Pts',(6.40193752585657,2.19991099568271,-57.5919037062808));
#33705=CARTESIAN_POINT('Ctrl Pts',(6.34141064938845,2.36873293225993,-57.5834797660879));
#33706=CARTESIAN_POINT('Ctrl Pts',(6.27430202976855,2.53484181740049,-57.575055825895));
#33707=CARTESIAN_POINT('Ctrl Pts',(6.2071724001284,2.70100270705346,-57.5666292483784));
#33708=CARTESIAN_POINT('Ctrl Pts',(6.13345704402997,2.8644485426354,-57.5582026708618));
#33709=CARTESIAN_POINT('Ctrl Pts',(6.05341091752872,3.0246496100448,-57.5497760933452));
#33710=CARTESIAN_POINT('Ctrl Pts',(5.97329300358367,3.18499434992935,-57.5413419586552));
#33711=CARTESIAN_POINT('Ctrl Pts',(5.8868331238357,3.34208820835713,-57.5329078239652));
#33712=CARTESIAN_POINT('Ctrl Pts',(5.79433234132488,3.49542582788943,-57.5244736892752));
#33713=CARTESIAN_POINT('Ctrl Pts',(5.70178685276455,3.64883755619169,-57.5160354783295));
#33714=CARTESIAN_POINT('Ctrl Pts',(5.6031948177927,3.79848914375275,-57.5075972673837));
#33715=CARTESIAN_POINT('Ctrl Pts',(5.49890045757043,3.94390450666997,-57.499159056438));
#33716=CARTESIAN_POINT('Ctrl Pts',(5.39449009093992,4.08948161480446,-57.4907114596871));
#33717=CARTESIAN_POINT('Ctrl Pts',(5.28436492650002,4.23081281689812,-57.4822638629363));
#33718=CARTESIAN_POINT('Ctrl Pts',(5.16891001645091,4.3674544350037,-57.4738162661854));
#33719=CARTESIAN_POINT('Ctrl Pts',(5.10496086490121,4.44313866134377,-57.4691372391555));
#33720=CARTESIAN_POINT('Ctrl Pts',(5.03937727196056,4.51738478329513,-57.4644582121256));
#33721=CARTESIAN_POINT('Ctrl Pts',(4.97222950422016,4.59012230309418,-57.4597791850957));
#33722=CARTESIAN_POINT('Ctrl Pts',(4.85390604080383,4.718295666894,-57.4515341055909));
#33723=CARTESIAN_POINT('Ctrl Pts',(4.73046040637767,4.84206744563971,-57.443289026086));
#33724=CARTESIAN_POINT('Ctrl Pts',(4.60225118473719,4.96100524416021,-57.4350439465811));
#33725=CARTESIAN_POINT('Ctrl Pts',(4.47422936691191,5.07976919093333,-57.4268109189344));
#33726=CARTESIAN_POINT('Ctrl Pts',(4.34145809775002,5.19371299996821,-57.4185778912877));
#33727=CARTESIAN_POINT('Ctrl Pts',(4.20433473594713,5.3024389131897,-57.410344863641));
#33728=CARTESIAN_POINT('Ctrl Pts',(4.06732711311721,5.41107305630459,-57.4021187850813));
#33729=CARTESIAN_POINT('Ctrl Pts',(3.92597498720908,5.51449785168672,-57.3938927065215));
#33730=CARTESIAN_POINT('Ctrl Pts',(3.78071153043142,5.61235327858671,-57.3856666279618));
#33731=CARTESIAN_POINT('Ctrl Pts',(3.63556788838887,5.71012799336326,-57.3774473343529));
#33732=CARTESIAN_POINT('Ctrl Pts',(3.48651963768592,5.80234229538776,-57.3692280407441));
#33733=CARTESIAN_POINT('Ctrl Pts',(3.33403176483176,5.88867737196502,-57.3610087471353));
#33734=CARTESIAN_POINT('Ctrl Pts',(3.25658189369875,5.93252768235372,-57.3568340988902));
#33735=CARTESIAN_POINT('Ctrl Pts',(3.17824519961803,5.97486198848,-57.3526594506451));
#33736=CARTESIAN_POINT('Ctrl Pts',(3.09908550384721,6.01564277861012,-57.3484848024));
#33737=CARTESIAN_POINT('Origin',(0.,0.,-63.6971797838103));
#33738=CARTESIAN_POINT('',(3.09908550384721,6.01564277861012,-54.9544629019808));
#33739=CARTESIAN_POINT('',(3.09908550384722,6.01564277861011,-55.3486963765549));
#33740=CARTESIAN_POINT('',(3.09908550384721,6.01564277861012,-63.6971797838103));
#33741=CARTESIAN_POINT('',(-6.76699956244302,-0.00224392468289009,-56.30282021619));
#33742=CARTESIAN_POINT('Ctrl Pts',(-6.76699948538929,-0.00263907960515001,
-56.30282021619));
#33743=CARTESIAN_POINT('Ctrl Pts',(-6.76692693805531,-0.188661422665976,
-56.2940962489685));
#33744=CARTESIAN_POINT('Ctrl Pts',(-6.75917963189646,-0.37450585182449,
-56.285372281747));
#33745=CARTESIAN_POINT('Ctrl Pts',(-6.74382674775489,-0.559544275518678,
-56.2766483145255));
#33746=CARTESIAN_POINT('Ctrl Pts',(-6.72845327550817,-0.744830834383355,
-56.2679126485278));
#33747=CARTESIAN_POINT('Ctrl Pts',(-6.70545389015303,-0.929308946509522,
-56.2591769825302));
#33748=CARTESIAN_POINT('Ctrl Pts',(-6.67494911439005,-1.11235934854863,
-56.2504413165326));
#33749=CARTESIAN_POINT('Ctrl Pts',(-6.64438168603178,-1.29578571082576,
-56.2416877086838));
#33750=CARTESIAN_POINT('Ctrl Pts',(-6.60627809895353,-1.47777821971559,
-56.232934100835));
#33751=CARTESIAN_POINT('Ctrl Pts',(-6.56080958945618,-1.65772932980626,
-56.2241804929862));
#33752=CARTESIAN_POINT('Ctrl Pts',(-6.54509139510451,-1.71993736243086,
-56.2211544226143));
#33753=CARTESIAN_POINT('Ctrl Pts',(-6.52849349090117,-1.7819015937994,-56.2181283522424));
#33754=CARTESIAN_POINT('Ctrl Pts',(-6.51102430173979,-1.84359744579825,
-56.2151022818704));
#33755=CARTESIAN_POINT('Ctrl Pts',(-6.4622969571836,-2.01568757604209,-56.206661571068));
#33756=CARTESIAN_POINT('Ctrl Pts',(-6.40670677850405,-2.18597184016191,
-56.1982208602656));
#33757=CARTESIAN_POINT('Ctrl Pts',(-6.34440843207874,-2.35388416175652,
-56.1897801494632));
#33758=CARTESIAN_POINT('Ctrl Pts',(-6.28215717440228,-2.52166956535741,
-56.1813458186457));
#33759=CARTESIAN_POINT('Ctrl Pts',(-6.21320797213382,-2.68708628890399,
-56.1729114878282));
#33760=CARTESIAN_POINT('Ctrl Pts',(-6.13776519577141,-2.8495837242617,-56.1644771570107));
#33761=CARTESIAN_POINT('Ctrl Pts',(-6.06236785829259,-3.01198328806158,
-56.156047906157));
#33762=CARTESIAN_POINT('Ctrl Pts',(-5.98048488404462,-3.17146676740238,
-56.1476186553034));
#33763=CARTESIAN_POINT('Ctrl Pts',(-5.89236876185276,-3.32750347473023,
-56.1391894044497));
#33764=CARTESIAN_POINT('Ctrl Pts',(-5.80429219518604,-3.48347013682976,
-56.1307639375057));
#33765=CARTESIAN_POINT('Ctrl Pts',(-5.70998822331743,-3.63599282215774,
-56.1223384705617));
#33766=CARTESIAN_POINT('Ctrl Pts',(-5.60975546457031,-3.78456505132671,
-56.1139130036177));
#33767=CARTESIAN_POINT('Ctrl Pts',(-5.50955233830795,-3.93309335708809,
-56.1054900275511));
#33768=CARTESIAN_POINT('Ctrl Pts',(-5.40342410685413,-4.07767325964716,
-56.0970670514846));
#33769=CARTESIAN_POINT('Ctrl Pts',(-5.29171314321519,-4.21782657418766,
-56.0886440754181));
#33770=CARTESIAN_POINT('Ctrl Pts',(-5.18000033079129,-4.35798220822601,
-56.0802209599536));
#33771=CARTESIAN_POINT('Ctrl Pts',(-5.06270480417671,-4.49371084309492,
-56.0717978444892));
#33772=CARTESIAN_POINT('Ctrl Pts',(-4.94021013663323,-4.62456622894583,
-56.0633747290248));
#33773=CARTESIAN_POINT('Ctrl Pts',(-4.81771123355154,-4.75542613942625,
-56.0549513223116));
#33774=CARTESIAN_POINT('Ctrl Pts',(-4.69001305889338,-4.88141222132429,
-56.0465279155983));
#33775=CARTESIAN_POINT('Ctrl Pts',(-4.55753717157229,-5.00211394609687,
-56.0381045088851));
#33776=CARTESIAN_POINT('Ctrl Pts',(-4.42503822772495,-5.12283667818289,
-56.0296796361353));
#33777=CARTESIAN_POINT('Ctrl Pts',(-4.28776015990397,-5.23827299492014,
-56.0212547633854));
#33778=CARTESIAN_POINT('Ctrl Pts',(-4.1461590977859,-5.34805139614862,-56.0128298906356));
#33779=CARTESIAN_POINT('Ctrl Pts',(-4.00451363635481,-5.45786421862739,
-56.0044023762491));
#33780=CARTESIAN_POINT('Ctrl Pts',(-3.85854274161604,-5.56201538436767,
-55.9959748618625));
#33781=CARTESIAN_POINT('Ctrl Pts',(-3.70873340663003,-5.66017539644722,
-55.987547347476));
#33782=CARTESIAN_POINT('Ctrl Pts',(-3.55878972829389,-5.75842343471601,
-55.9791122756131));
#33783=CARTESIAN_POINT('Ctrl Pts',(-3.40500101097334,-5.85066940107159,
-55.9706772037501));
#33784=CARTESIAN_POINT('Ctrl Pts',(-3.2478818329335,-5.93662804960025,-55.9622421318872));
#33785=CARTESIAN_POINT('Ctrl Pts',(-3.09068671811301,-6.02262824253566,
-55.9538029832959));
#33786=CARTESIAN_POINT('Ctrl Pts',(-2.93015822857286,-6.10233490447294,
-55.9453638347046));
#33787=CARTESIAN_POINT('Ctrl Pts',(-2.7668335065865,-6.17550980460968,-55.9369246861134));
#33788=CARTESIAN_POINT('Ctrl Pts',(-2.60332728413809,-6.2487660229818,-55.9284761592152));
#33789=CARTESIAN_POINT('Ctrl Pts',(-2.43701892780129,-6.31547584685385,
-55.920027632317));
#33790=CARTESIAN_POINT('Ctrl Pts',(-2.26846455665855,-6.37544959631742,
-55.9115791054189));
#33791=CARTESIAN_POINT('Ctrl Pts',(-2.17533166904081,-6.40858744039074,
-55.9069109636151));
#33792=CARTESIAN_POINT('Ctrl Pts',(-2.08151335051161,-6.43966964643707,
-55.9022428218113));
#33793=CARTESIAN_POINT('Ctrl Pts',(-1.98710511392526,-6.46867082685555,
-55.8975746800075));
#33794=CARTESIAN_POINT('Ctrl Pts',(-1.82044403495016,-6.51986729227915,
-55.8893338995633));
#33795=CARTESIAN_POINT('Ctrl Pts',(-1.65157302759785,-6.56468945802155,
-55.8810931191192));
#33796=CARTESIAN_POINT('Ctrl Pts',(-1.48101887055946,-6.60294419975262,
-55.872852338675));
#33797=CARTESIAN_POINT('Ctrl Pts',(-1.31065362102099,-6.64115657014695,
-55.8646206858022));
#33798=CARTESIAN_POINT('Ctrl Pts',(-1.13860927801477,-6.67281592349907,
-55.8563890329293));
#33799=CARTESIAN_POINT('Ctrl Pts',(-0.965429278168779,-6.69777838606612,
-55.8481573800565));
#33800=CARTESIAN_POINT('Ctrl Pts',(-0.792410232061655,-6.72271764848486,
-55.8399333776935));
#33801=CARTESIAN_POINT('Ctrl Pts',(-0.618257981217408,-6.74097236515085,
-55.8317093753306));
#33802=CARTESIAN_POINT('Ctrl Pts',(-0.443527794631489,-6.75244934045338,
-55.8234853729677));
#33803=CARTESIAN_POINT('Ctrl Pts',(-0.2689519837863,-6.76391617574177,-55.8152686365871));
#33804=CARTESIAN_POINT('Ctrl Pts',(-0.0937996085672701,-6.76861718154645,
-55.8070519002066));
#33805=CARTESIAN_POINT('Ctrl Pts',(0.0813673975475972,-6.76651079557377,
-55.798835163826));
#33806=CARTESIAN_POINT('Ctrl Pts',(0.25644465855948,-6.76440548878735,-55.79062263721));
#33807=CARTESIAN_POINT('Ctrl Pts',(0.431536180653232,-6.75549974061508,
-55.782410110594));
#33808=CARTESIAN_POINT('Ctrl Pts',(0.606078053571137,-6.73980403223858,
-55.774197583978));
#33809=CARTESIAN_POINT('Ctrl Pts',(0.780561557681218,-6.72411357268731,
-55.7659878037253));
#33810=CARTESIAN_POINT('Ctrl Pts',(0.954495424817928,-6.70163770814786,
-55.7577780234726));
#33811=CARTESIAN_POINT('Ctrl Pts',(1.1273187995095,-6.67243893372375,-55.7495682432198));
#33812=CARTESIAN_POINT('Ctrl Pts',(1.20280291385807,-6.65968577674251,-55.7459824551719));
#33813=CARTESIAN_POINT('Ctrl Pts',(1.27807524536973,-6.64565076977929,-55.7423966671239));
#33814=CARTESIAN_POINT('Ctrl Pts',(1.35308947604327,-6.63034221362827,-55.738810879076));
#33815=CARTESIAN_POINT('Ctrl Pts',(1.5384126622837,-6.59252231762753,-55.7299521643993));
#33816=CARTESIAN_POINT('Ctrl Pts',(1.72196784688877,-6.54696537009473,-55.7210934497226));
#33817=CARTESIAN_POINT('Ctrl Pts',(1.9031332698811,-6.4938719387644,-55.7122347350459));
#33818=CARTESIAN_POINT('Ctrl Pts',(2.08463762197831,-6.44067917882677,-55.7033594472496));
#33819=CARTESIAN_POINT('Ctrl Pts',(2.26374302893443,-6.37992183123153,-55.6944841594532));
#33820=CARTESIAN_POINT('Ctrl Pts',(2.43984584190009,-6.31184927479759,-55.6856088716569));
#33821=CARTESIAN_POINT('Ctrl Pts',(2.61644882401098,-6.24358337794057,-55.6767083761705));
#33822=CARTESIAN_POINT('Ctrl Pts',(2.79003190314272,-6.16796078954175,-55.6678078806842));
#33823=CARTESIAN_POINT('Ctrl Pts',(2.96001146623973,-6.08527905027611,-55.6589073851979));
#33824=CARTESIAN_POINT('Ctrl Pts',(3.13022112985471,-6.00248538513724,-55.6499948411536));
#33825=CARTESIAN_POINT('Ctrl Pts',(3.2968173029028,-5.912613599898,-55.6410822971093));
#33826=CARTESIAN_POINT('Ctrl Pts',(3.45924252893128,-5.81600637259221,-55.632169753065));
#33827=CARTESIAN_POINT('Ctrl Pts',(3.62202640506276,-5.71918582748553,-55.6232375292892));
#33828=CARTESIAN_POINT('Ctrl Pts',(3.78062068915887,-5.61560022599677,-55.6143053055134));
#33829=CARTESIAN_POINT('Ctrl Pts',(3.93449600083651,-5.50563622294477,-55.6053730817375));
#33830=CARTESIAN_POINT('Ctrl Pts',(4.07992625405044,-5.40170731691095,-55.5969310805398));
#33831=CARTESIAN_POINT('Ctrl Pts',(4.22114142569898,-5.29208138818329,-55.5884890793421));
#33832=CARTESIAN_POINT('Ctrl Pts',(4.3577229824198,-5.17711690118065,-55.5800470781444));
#33833=CARTESIAN_POINT('Ctrl Pts',(4.49077712664718,-5.06512153517421,-55.5718231036057));
#33834=CARTESIAN_POINT('Ctrl Pts',(4.61968740222887,-4.94784506964502,-55.563599129067));
#33835=CARTESIAN_POINT('Ctrl Pts',(4.74400940944454,-4.8256257338403,-55.5553751545283));
#33836=CARTESIAN_POINT('Ctrl Pts',(4.8682001205618,-4.70353547350902,-55.5471598653044));
#33837=CARTESIAN_POINT('Ctrl Pts',(4.98781195904097,-4.5765129872896,-55.5389445760806));
#33838=CARTESIAN_POINT('Ctrl Pts',(5.10243315790944,-4.44493699269925,-55.5307292868567));
#33839=CARTESIAN_POINT('Ctrl Pts',(5.21695629624148,-4.31347356378383,-55.5225210259633));
#33840=CARTESIAN_POINT('Ctrl Pts',(5.32649706405495,-4.17746465385995,-55.5143127650699));
#33841=CARTESIAN_POINT('Ctrl Pts',(5.43068011653878,-4.03732615375949,-55.5061045041765));
#33842=CARTESIAN_POINT('Ctrl Pts',(5.53479492945887,-3.89727944392511,-55.4979016196676));
#33843=CARTESIAN_POINT('Ctrl Pts',(5.63355880399971,-3.75310881848125,-55.4896987351586));
#33844=CARTESIAN_POINT('Ctrl Pts',(5.72663626209239,-3.60526366881655,-55.4814958506497));
#33845=CARTESIAN_POINT('Ctrl Pts',(5.81967141497185,-3.4574857171685,-55.4732966944847));
#33846=CARTESIAN_POINT('Ctrl Pts',(5.90702510988222,-3.30603687147461,-55.4650975383197));
#33847=CARTESIAN_POINT('Ctrl Pts',(5.98840480156228,-3.15139602916323,-55.4568983821547));
#33848=CARTESIAN_POINT('Ctrl Pts',(6.06977741517949,-2.99676863686106,-55.4486999391178));
#33849=CARTESIAN_POINT('Ctrl Pts',(6.14517688609919,-2.83895011405359,-55.4405014960809));
#33850=CARTESIAN_POINT('Ctrl Pts',(6.2143561395723,-2.67844484179907,-55.432303053044));
#33851=CARTESIAN_POINT('Ctrl Pts',(6.28353470409734,-2.51794116799774,-55.4241046916544));
#33852=CARTESIAN_POINT('Ctrl Pts',(6.34649303161368,-2.3547511270299,-55.4159063302648));
#33853=CARTESIAN_POINT('Ctrl Pts',(6.4030318683709,-2.18939989326452,-55.4077079688752));
#33854=CARTESIAN_POINT('Ctrl Pts',(6.45958041274809,-2.02402026897978,-55.3995081998413));
#33855=CARTESIAN_POINT('Ctrl Pts',(6.50970715437334,-1.8564790520249,-55.3913084308073));
#33856=CARTESIAN_POINT('Ctrl Pts',(6.55326245241661,-1.68731746560824,-55.3831086617733));
#33857=CARTESIAN_POINT('Ctrl Pts',(6.59683314104232,-1.5180961047105,-55.3749059952911));
#33858=CARTESIAN_POINT('Ctrl Pts',(6.6338276711041,-1.34725358093727,-55.3667033288089));
#33859=CARTESIAN_POINT('Ctrl Pts',(6.66414732397989,-1.17534226687024,-55.3585006623267));
#33860=CARTESIAN_POINT('Ctrl Pts',(6.69450141239539,-1.00323570456255,-55.3502886796676));
#33861=CARTESIAN_POINT('Ctrl Pts',(6.71816541592229,-0.830058280472868,
-55.3420766970086));
#33862=CARTESIAN_POINT('Ctrl Pts',(6.73509228255465,-0.656369519000377,
-55.3338647143496));
#33863=CARTESIAN_POINT('Ctrl Pts',(6.75202913287981,-0.4825783135686,-55.3256478881531));
#33864=CARTESIAN_POINT('Ctrl Pts',(6.76222090449828,-0.308275527055722,
-55.3174310619567));
#33865=CARTESIAN_POINT('Ctrl Pts',(6.76567271029664,-0.134021554786235,
-55.3092142357602));
#33866=CARTESIAN_POINT('Ctrl Pts',(6.76912983927692,0.0405011422167447,
-55.3009847380338));
#33867=CARTESIAN_POINT('Ctrl Pts',(6.76582623826288,0.214974516173924,-55.2927552403074));
#33868=CARTESIAN_POINT('Ctrl Pts',(6.75581909213108,0.388841091446277,-55.284525742581));
#33869=CARTESIAN_POINT('Ctrl Pts',(6.74689915031543,0.543818316190675,-55.2771903204811));
#33870=CARTESIAN_POINT('Ctrl Pts',(6.73265387911371,0.698313339590443,-55.2698548983812));
#33871=CARTESIAN_POINT('Ctrl Pts',(6.71315796159024,0.851938485301359,-55.2625194762814));
#33872=CARTESIAN_POINT('Ctrl Pts',(6.69170690993703,1.02096981875415,-55.2544484266284));
#33873=CARTESIAN_POINT('Ctrl Pts',(6.66382835574612,1.18949909330404,-55.2463773769754));
#33874=CARTESIAN_POINT('Ctrl Pts',(6.62954566461423,1.35698683884359,-55.2383063273224));
#33875=CARTESIAN_POINT('Ctrl Pts',(6.59530579751382,1.52426536800451,-55.2302453595759));
#33876=CARTESIAN_POINT('Ctrl Pts',(6.55467778501534,1.69050459604163,-55.2221843918294));
#33877=CARTESIAN_POINT('Ctrl Pts',(6.50773684329409,1.85516850405365,-55.2141234240828));
#33878=CARTESIAN_POINT('Ctrl Pts',(6.46084424350325,2.01966283363607,-55.2060707578898));
#33879=CARTESIAN_POINT('Ctrl Pts',(6.40765175409085,2.1825847160492,-55.1980180916969));
#33880=CARTESIAN_POINT('Ctrl Pts',(6.34828588222641,2.34340678447531,-55.1899654255039));
#33881=CARTESIAN_POINT('Ctrl Pts',(6.28896814852193,2.5040984466897,-55.1819192889974));
#33882=CARTESIAN_POINT('Ctrl Pts',(6.22348712451107,2.66269333576979,-55.173873152491));
#33883=CARTESIAN_POINT('Ctrl Pts',(6.15201951764226,2.81867785575946,-55.1658270159845));
#33884=CARTESIAN_POINT('Ctrl Pts',(6.08059422865249,2.97457001314822,-55.1577856438104));
#33885=CARTESIAN_POINT('Ctrl Pts',(6.0031895687952,3.1278545403016,-55.1497442716363));
#33886=CARTESIAN_POINT('Ctrl Pts',(5.92003083518417,3.27803659382695,-55.1417028994622));
#33887=CARTESIAN_POINT('Ctrl Pts',(5.8368929307542,3.42818103050739,-55.1336635414505));
#33888=CARTESIAN_POINT('Ctrl Pts',(5.748003996651,3.57522421132448,-55.1256241834388));
#33889=CARTESIAN_POINT('Ctrl Pts',(5.65363590927376,3.7186946641759,-55.1175848254271));
#33890=CARTESIAN_POINT('Ctrl Pts',(5.559277401509,3.86215055287348,-55.1095462835169));
#33891=CARTESIAN_POINT('Ctrl Pts',(5.4594410517705,4.00203412297442,-55.1015077416067));
#33892=CARTESIAN_POINT('Ctrl Pts',(5.35444269168022,4.13790193957183,-55.0934691996965));
#33893=CARTESIAN_POINT('Ctrl Pts',(5.24943420515712,4.27378285976739,-55.0854298825193));
#33894=CARTESIAN_POINT('Ctrl Pts',(5.13926294560076,4.40564696001497,-55.0773905653422));
#33895=CARTESIAN_POINT('Ctrl Pts',(5.02428564383119,4.53308314165886,-55.0693512481651));
#33896=CARTESIAN_POINT('Ctrl Pts',(4.90927448809729,4.66055684566483,-55.0613095638881));
#33897=CARTESIAN_POINT('Ctrl Pts',(4.78945472376362,4.78359975919453,-55.0532678796111));
#33898=CARTESIAN_POINT('Ctrl Pts',(4.66522049469816,4.90183707765244,-55.0452261953341));
#33899=CARTESIAN_POINT('Ctrl Pts',(4.54085398567013,5.02020029078671,-55.0371759485723));
#33900=CARTESIAN_POINT('Ctrl Pts',(4.41206389566123,5.13374743267266,-55.0291257018105));
#33901=CARTESIAN_POINT('Ctrl Pts',(4.2792786470111,5.24214300274562,-55.0210754550487));
#33902=CARTESIAN_POINT('Ctrl Pts',(4.14641810207679,5.3506000388604,-55.0130206433697));
#33903=CARTESIAN_POINT('Ctrl Pts',(4.00955818376298,5.45389946088245,-55.0049658316907));
#33904=CARTESIAN_POINT('Ctrl Pts',(3.86915651691859,5.55174898996581,-54.9969110200117));
#33905=CARTESIAN_POINT('Ctrl Pts',(3.7285473720021,5.64974311584853,-54.9888443053629));
#33906=CARTESIAN_POINT('Ctrl Pts',(3.58438633853291,5.74227106255868,-54.9807775907141));
#33907=CARTESIAN_POINT('Ctrl Pts',(3.43715672144868,5.82908592081127,-54.9727108760654));
#33908=CARTESIAN_POINT('Ctrl Pts',(3.32613910754568,5.89454814645175,-54.9666282180372));
#33909=CARTESIAN_POINT('Ctrl Pts',(3.21337727196016,5.95676295897932,-54.960545560009));
#33910=CARTESIAN_POINT('Ctrl Pts',(3.09908550384721,6.01564277861012,-54.9544629019808));
#33911=CARTESIAN_POINT('Ctrl Pts',(3.0990855038472,6.01564277861012,-56.9542436419538));
#33912=CARTESIAN_POINT('Ctrl Pts',(2.93373232018328,6.1008279655248,-56.9454941940545));
#33913=CARTESIAN_POINT('Ctrl Pts',(2.76486502144425,6.17919158180191,-56.9367447461552));
#33914=CARTESIAN_POINT('Ctrl Pts',(2.59305716434349,6.2504674659138,-56.927995298256));
#33915=CARTESIAN_POINT('Ctrl Pts',(2.42125069459281,6.32174277447225,-56.9192459210085));
#33916=CARTESIAN_POINT('Ctrl Pts',(2.24650397871057,6.38593035557826,-56.9104965437611));
#33917=CARTESIAN_POINT('Ctrl Pts',(2.06941053323771,6.44281220003539,-56.9017471665137));
#33918=CARTESIAN_POINT('Ctrl Pts',(1.8923184589668,6.49969360406686,-56.8929978570111));
#33919=CARTESIAN_POINT('Ctrl Pts',(1.71287996431499,6.54926929700882,-56.8842485475085));
#33920=CARTESIAN_POINT('Ctrl Pts',(1.53170449173495,6.59137090065481,-56.8754992380059));
#33921=CARTESIAN_POINT('Ctrl Pts',(1.35053036178164,6.63347219230085,-56.8667499933413));
#33922=CARTESIAN_POINT('Ctrl Pts',(1.1676195587884,6.66809944062455,-56.8580007486767));
#33923=CARTESIAN_POINT('Ctrl Pts',(0.983593309310466,6.69513503985392,-56.8492515040121));
#33924=CARTESIAN_POINT('Ctrl Pts',(0.799568362460043,6.72217044771213,-56.840502321279));
#33925=CARTESIAN_POINT('Ctrl Pts',(0.614428268438739,6.74161427235976,-56.8317531385458));
#33926=CARTESIAN_POINT('Ctrl Pts',(0.428801816330496,6.75340047696801,-56.8230039558126));
#33927=CARTESIAN_POINT('Ctrl Pts',(0.243176616522996,6.76518660206241,-56.8142548321045));
#33928=CARTESIAN_POINT('Ctrl Pts',(0.0570653511656601,6.76931519233997,
-56.8055057083964));
#33929=CARTESIAN_POINT('Ctrl Pts',(-0.128899900799846,6.76577222610796,
-56.7967565846882));
#33930=CARTESIAN_POINT('Ctrl Pts',(-0.314863959941722,6.76222928260134,
-56.788007517099));
#33931=CARTESIAN_POINT('Ctrl Pts',(-0.500681721080267,6.75101488651279,
-56.7792584495097));
#33932=CARTESIAN_POINT('Ctrl Pts',(-0.685722110172772,6.73216712415996,
-56.7705093819205));
#33933=CARTESIAN_POINT('Ctrl Pts',(-0.870761373826947,6.71331947644153,
-56.7617603675441));
#33934=CARTESIAN_POINT('Ctrl Pts',(-1.05502298984263,6.68683858440009,-56.7530113531678));
#33935=CARTESIAN_POINT('Ctrl Pts',(-1.23788117675966,6.65281438131443,-56.7442623387914));
#33936=CARTESIAN_POINT('Ctrl Pts',(-1.43009641451704,6.61704912302397,-56.7350656279039));
#33937=CARTESIAN_POINT('Ctrl Pts',(-1.62076048992612,6.57294837083186,-56.7258689170163));
#33938=CARTESIAN_POINT('Ctrl Pts',(-1.80915798961053,6.52067760042071,-56.7166722061288));
#33939=CARTESIAN_POINT('Ctrl Pts',(-1.98840443002927,6.47094578577435,-56.7079222084223));
#33940=CARTESIAN_POINT('Ctrl Pts',(-2.16559895952101,6.41381888474506,-56.6991722107158));
#33941=CARTESIAN_POINT('Ctrl Pts',(-2.34013966242226,6.3494909528527,-56.6904222130093));
#33942=CARTESIAN_POINT('Ctrl Pts',(-2.51467682553918,6.28516432556724,-56.6816723927577));
#33943=CARTESIAN_POINT('Ctrl Pts',(-2.68656000078745,6.21363705879703,-56.6729225725061));
#33944=CARTESIAN_POINT('Ctrl Pts',(-2.85520533840792,6.13515211510904,-56.6641727522545));
#33945=CARTESIAN_POINT('Ctrl Pts',(-3.02384747998232,6.05666865881169,-56.6554230978233));
#33946=CARTESIAN_POINT('Ctrl Pts',(-3.18925164684443,5.97122791039894,-56.646673443392));
#33947=CARTESIAN_POINT('Ctrl Pts',(-3.35085601829066,5.8791200825196,-56.6379237889608));
#33948=CARTESIAN_POINT('Ctrl Pts',(-3.51245754191324,5.78701387778231,-56.6291742887176));
#33949=CARTESIAN_POINT('Ctrl Pts',(-3.6702591551084,5.68824097061044,-56.6204247884745));
#33950=CARTESIAN_POINT('Ctrl Pts',(-3.82372487928737,5.58313684656921,-56.6116752882314));
#33951=CARTESIAN_POINT('Ctrl Pts',(-3.97718810300709,5.47803443501838,-56.6029259305462));
#33952=CARTESIAN_POINT('Ctrl Pts',(-4.12631534262945,5.36660117496438,-56.5941765728611));
#33953=CARTESIAN_POINT('Ctrl Pts',(-4.27060009886153,5.24921554097409,-56.585427215176));
#33954=CARTESIAN_POINT('Ctrl Pts',(-4.41488269594157,5.13183166360341,-56.5766779884208));
#33955=CARTESIAN_POINT('Ctrl Pts',(-4.55432273235047,5.00849577139509,-56.5679287616656));
#33956=CARTESIAN_POINT('Ctrl Pts',(-4.68844662480179,4.87962675277369,-56.5591795349104));
#33957=CARTESIAN_POINT('Ctrl Pts',(-4.82256868835105,4.75075949139934,-56.5504304274589));
#33958=CARTESIAN_POINT('Ctrl Pts',(-4.95137454637787,4.61635945312604,-56.5416813200075));
#33959=CARTESIAN_POINT('Ctrl Pts',(-5.07442674460983,4.47688309134699,-56.532932212556));
#33960=CARTESIAN_POINT('Ctrl Pts',(-5.19747742838454,4.33740844616453,-56.5241832127836));
#33961=CARTESIAN_POINT('Ctrl Pts',(-5.31477440450853,4.19285781736123,-56.5154342130112));
#33962=CARTESIAN_POINT('Ctrl Pts',(-5.42591931531088,4.04372211999493,-56.5066852132389));
#33963=CARTESIAN_POINT('Ctrl Pts',(-5.53707636462921,3.89457013500887,-56.4979352579583));
#33964=CARTESIAN_POINT('Ctrl Pts',(-5.64207983273414,3.74083230916506,-56.4891853026777));
#33965=CARTESIAN_POINT('Ctrl Pts',(-5.74057303468694,3.58303087251913,-56.4804353473971));
#33966=CARTESIAN_POINT('Ctrl Pts',(-5.83906243363715,3.42523552887516,-56.4716857299683));
#33967=CARTESIAN_POINT('Ctrl Pts',(-5.93104191768379,3.26337713157077,-56.4629361125395));
#33968=CARTESIAN_POINT('Ctrl Pts',(-6.01619906699613,3.09800545291239,-56.4541864951107));
#33969=CARTESIAN_POINT('Ctrl Pts',(-6.10135338095344,2.93263928039677,-56.4454371690053));
#33970=CARTESIAN_POINT('Ctrl Pts',(-6.17968568352803,2.76376031540304,-56.4366878428999));
#33971=CARTESIAN_POINT('Ctrl Pts',(-6.25092992694854,2.5919421383162,-56.4279385167945));
#33972=CARTESIAN_POINT('Ctrl Pts',(-6.32217217691057,2.42012876880939,-56.4191894355007));
#33973=CARTESIAN_POINT('Ctrl Pts',(-6.38632665483793,2.2453766164783,-56.410440354207));
#33974=CARTESIAN_POINT('Ctrl Pts',(-6.44317547869285,2.06827917621659,-56.4016912729132));
#33975=CARTESIAN_POINT('Ctrl Pts',(-6.50002944235876,1.89116572423629,-56.3929414005982));
#33976=CARTESIAN_POINT('Ctrl Pts',(-6.54957634250344,1.71170683289406,-56.3841915282833));
#33977=CARTESIAN_POINT('Ctrl Pts',(-6.59164787708347,1.53051209225574,-56.3754416559683));
#33978=CARTESIAN_POINT('Ctrl Pts',(-6.63371649074968,1.34932993148233,-56.3666923911335));
#33979=CARTESIAN_POINT('Ctrl Pts',(-6.6683107125709,1.16641244174199,-56.3579431262987));
#33980=CARTESIAN_POINT('Ctrl Pts',(-6.69531304840305,0.982380875161888,
-56.3491938614639));
#33981=CARTESIAN_POINT('Ctrl Pts',(-6.72231677033021,0.798339861797759,
-56.3404441475083));
#33982=CARTESIAN_POINT('Ctrl Pts',(-6.74172778477872,0.613184940732107,
-56.3316944335526));
#33983=CARTESIAN_POINT('Ctrl Pts',(-6.75348015835505,0.427545027692543,
-56.322944719597));
#33984=CARTESIAN_POINT('Ctrl Pts',(-6.76249038365215,0.285219953548515,
-56.3162365517946));
#33985=CARTESIAN_POINT('Ctrl Pts',(-6.76699999999998,0.142609995758698,
-56.3095283839923));
#33986=CARTESIAN_POINT('Ctrl Pts',(-6.767,1.01112582279511E-12,-56.30282021619));
#33987=CARTESIAN_POINT('',(-6.76699856490775,0.00440710069189511,-56.6971797838425));
#33988=CARTESIAN_POINT('Ctrl Pts',(3.09908550384721,6.01564277861012,-57.3484848024));
#33989=CARTESIAN_POINT('Ctrl Pts',(2.94333909626799,6.09587883180818,-57.3402711974745));
#33990=CARTESIAN_POINT('Ctrl Pts',(2.78440536102775,6.170098280044,-57.3320575925491));
#33991=CARTESIAN_POINT('Ctrl Pts',(2.62278972093599,6.23804962145642,-57.3238439876236));
#33992=CARTESIAN_POINT('Ctrl Pts',(2.47306012011007,6.30100347431057,-57.3162344531372));
#33993=CARTESIAN_POINT('Ctrl Pts',(2.32102905734274,6.35857765802904,-57.3086249186507));
#33994=CARTESIAN_POINT('Ctrl Pts',(2.167115085328,6.41060848960096,-57.3010153841643));
#33995=CARTESIAN_POINT('Ctrl Pts',(1.98797087251385,6.47116843904546,-57.2921584620303));
#33996=CARTESIAN_POINT('Ctrl Pts',(1.8064616568237,6.52415593640569,-57.2833015398964));
#33997=CARTESIAN_POINT('Ctrl Pts',(1.62322537182426,6.56943135988694,-57.2744446177625));
#33998=CARTESIAN_POINT('Ctrl Pts',(1.43964794173174,6.61479107610835,-57.265571206015));
#33999=CARTESIAN_POINT('Ctrl Pts',(1.25433726871447,6.65240996260301,-57.2566977942675));
#34000=CARTESIAN_POINT('Ctrl Pts',(1.06794020261944,6.68219969198985,-57.24782438252));
#34001=CARTESIAN_POINT('Ctrl Pts',(0.881015653119109,6.71207372306785,-57.2389258599833));
#34002=CARTESIAN_POINT('Ctrl Pts',(0.692998816427942,6.73407421991262,-57.2300273374466));
#34003=CARTESIAN_POINT('Ctrl Pts',(0.504543460320005,6.74816455761478,-57.2211288149098));
#34004=CARTESIAN_POINT('Ctrl Pts',(0.315833885501937,6.76227390261687,-57.2122182886234));
#34005=CARTESIAN_POINT('Ctrl Pts',(0.126684869057916,6.76845176086734,-57.203307762337));
#34006=CARTESIAN_POINT('Ctrl Pts',(-0.062249707707935,6.76671367606834,
-57.1943972360506));
#34007=CARTESIAN_POINT('Ctrl Pts',(-0.251600724309423,6.76497176027259,
-57.1854670696423));
#34008=CARTESIAN_POINT('Ctrl Pts',(-0.440736095090732,6.75527900524688,
-57.1765369032341));
#34009=CARTESIAN_POINT('Ctrl Pts',(-0.629004072485149,6.73770308612639,
-57.1676067368259));
#34010=CARTESIAN_POINT('Ctrl Pts',(-0.807185279317851,6.72106882615598,
-57.1591550189615));
#34011=CARTESIAN_POINT('Ctrl Pts',(-0.984589419232587,6.69737393988361,
-57.1507033010971));
#34012=CARTESIAN_POINT('Ctrl Pts',(-1.16067243003436,6.66671797139778,-57.1422515832327));
#34013=CARTESIAN_POINT('Ctrl Pts',(-1.33201456931112,6.63688738639106,-57.1340274200221));
#34014=CARTESIAN_POINT('Ctrl Pts',(-1.50243299280958,6.60040750138087,-57.1258032568115));
#34015=CARTESIAN_POINT('Ctrl Pts',(-1.67137344457976,6.55734700993882,-57.1175790936009));
#34016=CARTESIAN_POINT('Ctrl Pts',(-1.84013553582849,6.5143319800285,-57.1093636131304));
#34017=CARTESIAN_POINT('Ctrl Pts',(-2.0074224180065,6.46475026641791,-57.10114813266));
#34018=CARTESIAN_POINT('Ctrl Pts',(-2.17268766443286,6.40872197187718,-57.0929326521895));
#34019=CARTESIAN_POINT('Ctrl Pts',(-2.33781157417631,6.35274159335915,-57.0847241976896));
#34020=CARTESIAN_POINT('Ctrl Pts',(-2.50091695382658,6.29032572847284,-57.0765157431897));
#34021=CARTESIAN_POINT('Ctrl Pts',(-2.66147014843813,6.22164493112334,-57.0683072886898));
#34022=CARTESIAN_POINT('Ctrl Pts',(-2.82191822571081,6.15300910044465,-57.0601042084267));
#34023=CARTESIAN_POINT('Ctrl Pts',(-2.97981711783748,6.07811664814091,-57.0519011281637));
#34024=CARTESIAN_POINT('Ctrl Pts',(-3.13465076611339,5.99718713852626,-57.0436980479006));
#34025=CARTESIAN_POINT('Ctrl Pts',(-3.28941407823135,5.91629439269541,-57.0354986940443));
#34026=CARTESIAN_POINT('Ctrl Pts',(-3.44111460348834,5.82937021899216,-57.027299340188));
#34027=CARTESIAN_POINT('Ctrl Pts',(-3.58925853872999,5.73668128295044,-57.0190999863316));
#34028=CARTESIAN_POINT('Ctrl Pts',(-3.73738963002714,5.6440003829552,-57.0109013433518));
#34029=CARTESIAN_POINT('Ctrl Pts',(-3.88196443722821,5.54555589895962,-57.002702700372));
#34030=CARTESIAN_POINT('Ctrl Pts',(-4.02251562939745,5.441659398681,-56.9945040573922));
#34031=CARTESIAN_POINT('Ctrl Pts',(-4.16306544503295,5.33776391594649,-56.9863054947085));
#34032=CARTESIAN_POINT('Ctrl Pts',(-4.29959143506934,5.22841673564294,-56.9781069320248));
#34033=CARTESIAN_POINT('Ctrl Pts',(-4.43165713198777,5.1139714571458,-56.969908369341));
#34034=CARTESIAN_POINT('Ctrl Pts',(-4.56374552258772,4.99950651279475,-56.9617083978466));
#34035=CARTESIAN_POINT('Ctrl Pts',(-4.69137182202745,4.8799419598243,-56.9535084263521));
#34036=CARTESIAN_POINT('Ctrl Pts',(-4.81413436184852,4.75567023100524,-56.9453084548577));
#34037=CARTESIAN_POINT('Ctrl Pts',(-4.93694029433773,4.63135457606753,-56.9371055849331));
#34038=CARTESIAN_POINT('Ctrl Pts',(-5.05487879064621,4.50232868589586,-56.9289027150085));
#34039=CARTESIAN_POINT('Ctrl Pts',(-5.16758657796395,4.36902025164073,-56.920699845084));
#34040=CARTESIAN_POINT('Ctrl Pts',(-5.28042237586932,4.23556040911639,-56.912487658552));
#34041=CARTESIAN_POINT('Ctrl Pts',(-5.38801536420717,4.09780857935904,-56.9042754720201));
#34042=CARTESIAN_POINT('Ctrl Pts',(-5.49004332048786,3.95622463204084,-56.8960632854882));
#34043=CARTESIAN_POINT('Ctrl Pts',(-5.59213145950119,3.81455716929061,-56.8878462548739));
#34044=CARTESIAN_POINT('Ctrl Pts',(-5.68864782508761,3.66905338152276,-56.8796292242596));
#34045=CARTESIAN_POINT('Ctrl Pts',(-5.77931483598359,3.52020014013124,-56.8714121936453));
#34046=CARTESIAN_POINT('Ctrl Pts',(-5.87012165340361,3.3711173703361,-56.8631824925517));
#34047=CARTESIAN_POINT('Ctrl Pts',(-5.95506091731349,3.21867513890646,-56.854952791458));
#34048=CARTESIAN_POINT('Ctrl Pts',(-6.03390151478836,3.06338399647102,-56.8467230903644));
#34049=CARTESIAN_POINT('Ctrl Pts',(-6.10415205719658,2.92501255667112,-56.8393900540328));
#34050=CARTESIAN_POINT('Ctrl Pts',(-6.16956110168431,2.78437964804174,-56.8320570177012));
#34051=CARTESIAN_POINT('Ctrl Pts',(-6.2299982336486,2.64185749213226,-56.8247239813697));
#34052=CARTESIAN_POINT('Ctrl Pts',(-6.30414378120452,2.46700830678371,-56.8157276578119));
#34053=CARTESIAN_POINT('Ctrl Pts',(-6.37101372039897,2.28882562406587,-56.8067313342542));
#34054=CARTESIAN_POINT('Ctrl Pts',(-6.43032076247517,2.1079050955109,-56.7977350106965));
#34055=CARTESIAN_POINT('Ctrl Pts',(-6.48936336453937,1.92779126081666,-56.7887788002152));
#34056=CARTESIAN_POINT('Ctrl Pts',(-6.54091023374025,1.74496415253537,-56.7798225897338));
#34057=CARTESIAN_POINT('Ctrl Pts',(-6.58472273487644,1.5600370203304,-56.7708663792525));
#34058=CARTESIAN_POINT('Ctrl Pts',(-6.62841626139362,1.37561206523308,-56.761934489723));
#34059=CARTESIAN_POINT('Ctrl Pts',(-6.66441723913493,1.18909868970128,-56.7530026001935));
#34060=CARTESIAN_POINT('Ctrl Pts',(-6.69253560599246,1.0011274456947,-56.744070710664));
#34061=CARTESIAN_POINT('Ctrl Pts',(-6.72053001562576,0.813984855562639,
-56.7351781965449));
#34062=CARTESIAN_POINT('Ctrl Pts',(-6.74071105790939,0.625397449691096,
-56.7262856824257));
#34063=CARTESIAN_POINT('Ctrl Pts',(-6.7529391756948,0.436006295099548,-56.7173931683065));
#34064=CARTESIAN_POINT('Ctrl Pts',(-6.76220433373509,0.292505961727163,
-56.7106553734852));
#34065=CARTESIAN_POINT('Ctrl Pts',(-6.76690469337939,0.148544605610245,
-56.7039175786638));
#34066=CARTESIAN_POINT('Ctrl Pts',(-6.76699856490775,0.00440710069191697,
-56.6971797838425));
#34067=CARTESIAN_POINT('Ctrl Pts',(-6.7669985649082,0.00440709999955857,
-56.6971797838101));
#34068=CARTESIAN_POINT('Ctrl Pts',(-6.76711176756178,-0.169412916424865,
-56.6890544620406));
#34069=CARTESIAN_POINT('Ctrl Pts',(-6.760523406653,-0.343245640998958,-56.6809291402712));
#34070=CARTESIAN_POINT('Ctrl Pts',(-6.74725724048585,-0.51653531409893,
-56.6728038185017));
#34071=CARTESIAN_POINT('Ctrl Pts',(-6.73398872311116,-0.689855699914266,
-56.664677056654));
#34072=CARTESIAN_POINT('Ctrl Pts',(-6.7140400698679,-0.862632479764062,
-56.6565502948063));
#34073=CARTESIAN_POINT('Ctrl Pts',(-6.68748697795196,-1.03431471019365,
-56.6484235329585));
#34074=CARTESIAN_POINT('Ctrl Pts',(-6.66092419577455,-1.20605959418192,
-56.6402938053376));
#34075=CARTESIAN_POINT('Ctrl Pts',(-6.62775222944934,-1.37670877380828,
-56.6321640777167));
#34076=CARTESIAN_POINT('Ctrl Pts',(-6.58809797633348,-1.54572120844306,
-56.6240343500958));
#34077=CARTESIAN_POINT('Ctrl Pts',(-6.54842180790742,-1.71482704945025,
-56.6159001295016));
#34078=CARTESIAN_POINT('Ctrl Pts',(-6.50225629983729,-1.88229399027416,
-56.6077659089073));
#34079=CARTESIAN_POINT('Ctrl Pts',(-6.44977830005002,-2.04759587814683,
-56.5996316883131));
#34080=CARTESIAN_POINT('Ctrl Pts',(-6.39722493119822,-2.21313517309873,
-56.5914857853262));
#34081=CARTESIAN_POINT('Ctrl Pts',(-6.33834107144428,-2.37650285742089,
-56.5833398823394));
#34082=CARTESIAN_POINT('Ctrl Pts',(-6.27335225792795,-2.53719144881703,
-56.5751939793525));
#34083=CARTESIAN_POINT('Ctrl Pts',(-6.20831329348684,-2.69800404126851,
-56.5670417902905));
#34084=CARTESIAN_POINT('Ctrl Pts',(-6.13716013734437,-2.85613309152384,
-56.5588896012284));
#34085=CARTESIAN_POINT('Ctrl Pts',(-6.06016429834327,-3.01109576019855,
-56.5507374121664));
#34086=CARTESIAN_POINT('Ctrl Pts',(-5.9830309230542,-3.16633523591242,-56.542570660995));
#34087=CARTESIAN_POINT('Ctrl Pts',(-5.90003418832372,-3.31839671261976,
-56.5344039098237));
#34088=CARTESIAN_POINT('Ctrl Pts',(-5.8114896335024,-3.46682523927788,-56.5262371586524));
#34089=CARTESIAN_POINT('Ctrl Pts',(-5.74267576135428,-3.58217893524706,
-56.5198902322705));
#34090=CARTESIAN_POINT('Ctrl Pts',(-5.67051196301427,-3.69533894750056,
-56.5135433058886));
#34091=CARTESIAN_POINT('Ctrl Pts',(-5.59516271184839,-3.80610604528321,
-56.5071963795066));
#34092=CARTESIAN_POINT('Ctrl Pts',(-5.49622606261029,-3.95154777603536,
-56.4988626055212));
#34093=CARTESIAN_POINT('Ctrl Pts',(-5.39148830522668,-4.09331550672587,
-56.4905288315358));
#34094=CARTESIAN_POINT('Ctrl Pts',(-5.28124753162088,-4.23092348190657,
-56.4821950575504));
#34095=CARTESIAN_POINT('Ctrl Pts',(-5.17113670044219,-4.36836925653569,
-56.4738711067074));
#34096=CARTESIAN_POINT('Ctrl Pts',(-5.05553599034082,-4.50166477403508,
-56.4655471558644));
#34097=CARTESIAN_POINT('Ctrl Pts',(-4.93478703369493,-4.63035267901662,
-56.4572232050214));
#34098=CARTESIAN_POINT('Ctrl Pts',(-4.8141582648331,-4.7589124941615,-56.4489075394442));
#34099=CARTESIAN_POINT('Ctrl Pts',(-4.68839169532107,-4.882873581931,-56.440591873867));
#34100=CARTESIAN_POINT('Ctrl Pts',(-4.55786966514336,-5.00181098359044,
-56.4322762082899));
#34101=CARTESIAN_POINT('Ctrl Pts',(-4.42745363360745,-5.12065179463588,
-56.4239672959731));
#34102=CARTESIAN_POINT('Ctrl Pts',(-4.29229009275337,-5.23447681567917,
-56.4156583836563));
#34103=CARTESIAN_POINT('Ctrl Pts',(-4.15279888755748,-5.34289719155267,
-56.4073494713396));
#34104=CARTESIAN_POINT('Ctrl Pts',(-4.01339541871077,-5.45124937382253,
-56.3990457851131));
#34105=CARTESIAN_POINT('Ctrl Pts',(-3.86966998402319,-5.55420347266158,
-56.3907420988866));
#34106=CARTESIAN_POINT('Ctrl Pts',(-3.72207639083078,-5.65141011967988,
-56.3824384126601));
#34107=CARTESIAN_POINT('Ctrl Pts',(-3.57454272183674,-5.74857730000946,
-56.3741380977978));
#34108=CARTESIAN_POINT('Ctrl Pts',(-3.42314431371191,-5.84000148720765,
-56.3658377829354));
#34109=CARTESIAN_POINT('Ctrl Pts',(-3.26836514484309,-5.9253757923,-56.357537468073));
#34110=CARTESIAN_POINT('Ctrl Pts',(-3.11361861699007,-6.01073209300544,
-56.3492389036445));
#34111=CARTESIAN_POINT('Ctrl Pts',(-2.95549305315079,-6.09004088551378,
-56.3409403392161));
#34112=CARTESIAN_POINT('Ctrl Pts',(-2.79449850700662,-6.16304040992251,
-56.3326417747876));
#34113=CARTESIAN_POINT('Ctrl Pts',(-2.63351118738645,-6.23603665761889,
-56.3243435828548));
#34114=CARTESIAN_POINT('Ctrl Pts',(-2.46965545889241,-6.30272405811027,
-56.3160453909221));
#34115=CARTESIAN_POINT('Ctrl Pts',(-2.30346307484728,-6.36288824849338,
-56.3077471989893));
#34116=CARTESIAN_POINT('Ctrl Pts',(-2.13725056377429,-6.42305972516907,
-56.2994480020891));
#34117=CARTESIAN_POINT('Ctrl Pts',(-1.96870116047762,-6.4767062997432,-56.2911488051888));
#34118=CARTESIAN_POINT('Ctrl Pts',(-1.79836374314003,-6.52366283979785,
-56.2828496082886));
#34119=CARTESIAN_POINT('Ctrl Pts',(-1.62790670984997,-6.57065235411824,
-56.2745445834478));
#34120=CARTESIAN_POINT('Ctrl Pts',(-1.45565948931181,-6.61094235407167,
-56.266239558607));
#34121=CARTESIAN_POINT('Ctrl Pts',(-1.28218405512426,-6.64441818737993,
-56.2579345337662));
#34122=CARTESIAN_POINT('Ctrl Pts',(-1.10864535746443,-6.67790622874208,
-56.2496264802274));
#34123=CARTESIAN_POINT('Ctrl Pts',(-0.933877896255326,-6.70457509187546,
-56.2413184266885));
#34124=CARTESIAN_POINT('Ctrl Pts',(-0.758451057576164,-6.72436175359875,
-56.2330103731497));
#34125=CARTESIAN_POINT('Ctrl Pts',(-0.582837719315061,-6.74416945089542,
-56.2246934871624));
#34126=CARTESIAN_POINT('Ctrl Pts',(-0.406563949608596,-6.75708029673793,
-56.2163766011751));
#34127=CARTESIAN_POINT('Ctrl Pts',(-0.230202543461308,-6.76308330489755,
-56.2080597151878));
#34128=CARTESIAN_POINT('Ctrl Pts',(-0.100207911230814,-6.76750807591199,
-56.201929402673));
#34129=CARTESIAN_POINT('Ctrl Pts',(0.0298342774740913,-6.76818087208289,
-56.1957990901583));
#34130=CARTESIAN_POINT('Ctrl Pts',(0.159695758183085,-6.76511539183319,
-56.1896687776436));
#34131=CARTESIAN_POINT('Ctrl Pts',(0.338719994825503,-6.76088938687276,
-56.1812176610204));
#34132=CARTESIAN_POINT('Ctrl Pts',(0.51772782472298,-6.74954924328847,-56.1727665443972));
#34133=CARTESIAN_POINT('Ctrl Pts',(0.696130930947859,-6.73109877560697,
-56.164315427774));
#34134=CARTESIAN_POINT('Ctrl Pts',(0.874376954411912,-6.71266455344083,
-56.1558717523034));
#34135=CARTESIAN_POINT('Ctrl Pts',(1.05201898730338,-6.68713251967139,-56.1474280768328));
#34136=CARTESIAN_POINT('Ctrl Pts',(1.22847073063158,-6.6545584875318,-56.1389844013622));
#34137=CARTESIAN_POINT('Ctrl Pts',(1.40479109173087,-6.62200870932627,-56.1305470128734));
#34138=CARTESIAN_POINT('Ctrl Pts',(1.57992260509171,-6.5824274450482,-56.1221096243846));
#34139=CARTESIAN_POINT('Ctrl Pts',(1.75328570422906,-6.5359221414691,-56.1136722358958));
#34140=CARTESIAN_POINT('Ctrl Pts',(1.92652510020139,-6.48945002172942,-56.1052408679019));
#34141=CARTESIAN_POINT('Ctrl Pts',(2.09799827954512,-6.43606380331171,-56.0968094999081));
#34142=CARTESIAN_POINT('Ctrl Pts',(2.26713724714957,-6.37592171396317,-56.0883781319142));
#34143=CARTESIAN_POINT('Ctrl Pts',(2.43620370120311,-6.31580540883526,-56.0799503786311));
#34144=CARTESIAN_POINT('Ctrl Pts',(2.60293762676839,-6.24893911770795,-56.0715226253479));
#34145=CARTESIAN_POINT('Ctrl Pts',(2.76678690873883,-6.17553068178205,-56.0630948720647));
#34146=CARTESIAN_POINT('Ctrl Pts',(2.93058572378656,-6.10214485625649,-56.0546697145987));
#34147=CARTESIAN_POINT('Ctrl Pts',(3.09150136497608,-6.02222103979339,-56.0462445571326));
#34148=CARTESIAN_POINT('Ctrl Pts',(3.24900205829669,-5.93601504590276,-56.0378193996666));
#34149=CARTESIAN_POINT('Ctrl Pts',(3.29208835128823,-5.91243231345828,-56.0355145920151));
#34150=CARTESIAN_POINT('Ctrl Pts',(3.33491921080571,-5.88837971668314,-56.0332097843636));
#34151=CARTESIAN_POINT('Ctrl Pts',(3.37748405502412,-5.86386310021455,-56.0309049767121));
#34152=CARTESIAN_POINT('Ctrl Pts',(3.53665745527955,-5.7721819657544,-56.0222860312523));
#34153=CARTESIAN_POINT('Ctrl Pts',(3.69203774818405,-5.67404935571939,-56.0136670857925));
#34154=CARTESIAN_POINT('Ctrl Pts',(3.84311305874793,-5.56980888520254,-56.0050481403327));
#34155=CARTESIAN_POINT('Ctrl Pts',(3.99427886399721,-5.46550597424754,-55.9964240320917));
#34156=CARTESIAN_POINT('Ctrl Pts',(4.14113429025835,-5.35508807403767,-55.9877999238508));
#34157=CARTESIAN_POINT('Ctrl Pts',(4.28319857888049,-5.23894063087912,-55.9791758156099));
#34158=CARTESIAN_POINT('Ctrl Pts',(4.43012971213035,-5.11881420352095,-55.9702562622908));
#34159=CARTESIAN_POINT('Ctrl Pts',(4.57193535247314,-4.99255894827847,-55.9613367089717));
#34160=CARTESIAN_POINT('Ctrl Pts',(4.70812351663489,-4.86064419106249,-55.9524171556526));
#34161=CARTESIAN_POINT('Ctrl Pts',(4.84004596352177,-4.73286129847755,-55.943776982652));
#34162=CARTESIAN_POINT('Ctrl Pts',(4.96669733450544,-4.59976832619409,-55.9351368096513));
#34163=CARTESIAN_POINT('Ctrl Pts',(5.0876699251174,-4.46182739839362,-55.9264966366507));
#34164=CARTESIAN_POINT('Ctrl Pts',(5.2145099956208,-4.31719598297125,-55.9174373931724));
#34165=CARTESIAN_POINT('Ctrl Pts',(5.33510647330544,-4.16723494342464,-55.908378149694));
#34166=CARTESIAN_POINT('Ctrl Pts',(5.4490386102138,-4.01251382856175,-55.8993189062157));
#34167=CARTESIAN_POINT('Ctrl Pts',(5.56297074712216,-3.85779271369887,-55.8902596627373));
#34168=CARTESIAN_POINT('Ctrl Pts',(5.67023835718177,-3.69831185952653,-55.881200419259));
#34169=CARTESIAN_POINT('Ctrl Pts',(5.77047404941831,-3.5346737112483,-55.8721411757806));
#34170=CARTESIAN_POINT('Ctrl Pts',(5.8705354600804,-3.37132008351845,-55.8630976837694));
#34171=CARTESIAN_POINT('Ctrl Pts',(5.96368229599236,-3.20367354758897,-55.8540541917582));
#34172=CARTESIAN_POINT('Ctrl Pts',(6.04957529512622,-3.03231392645922,-55.8450106997471));
#34173=CARTESIAN_POINT('Ctrl Pts',(6.13538972613476,-2.86111105156402,-55.8359754800075));
#34174=CARTESIAN_POINT('Ctrl Pts',(6.2139634610426,-2.68620208513048,-55.8269402602678));
#34175=CARTESIAN_POINT('Ctrl Pts',(6.28500326369497,-2.50819117599588,-55.8179050405282));
#34176=CARTESIAN_POINT('Ctrl Pts',(6.35591790733133,-2.33049388921657,-55.8088857391776));
#34177=CARTESIAN_POINT('Ctrl Pts',(6.41932503590296,-2.14970579360339,-55.799866437827));
#34178=CARTESIAN_POINT('Ctrl Pts',(6.47497962988298,-1.96645055686649,-55.7908471364763));
#34179=CARTESIAN_POINT('Ctrl Pts',(6.53056440038258,-1.78342522960366,-55.7818391506159));
#34180=CARTESIAN_POINT('Ctrl Pts',(6.5784159775054,-1.59793916539026,-55.7728311647554));
#34181=CARTESIAN_POINT('Ctrl Pts',(6.6183383989632,-1.41063313331614,-55.763823178895));
#34182=CARTESIAN_POINT('Ctrl Pts',(6.65817065333218,-1.22375014270622,-55.7548355380895));
#34183=CARTESIAN_POINT('Ctrl Pts',(6.69010944941164,-1.03505562160223,-55.7458478972841));
#34184=CARTESIAN_POINT('Ctrl Pts',(6.7140094194478,-0.845202056058933,-55.7368602564786));
#34185=CARTESIAN_POINT('Ctrl Pts',(6.73482467673501,-0.679852442327279,
-55.7290326292688));
#34186=CARTESIAN_POINT('Ctrl Pts',(6.74954301569771,-0.513624002901764,
-55.7212050020589));
#34187=CARTESIAN_POINT('Ctrl Pts',(6.75809963956551,-0.346955705680907,
-55.713377374849));
#34188=CARTESIAN_POINT('Ctrl Pts',(6.76697932707497,-0.173994685082054,
-55.7052542079741));
#34189=CARTESIAN_POINT('Ctrl Pts',(6.76921759228954,-0.00063720007779014,
-55.6971310410991));
#34190=CARTESIAN_POINT('Ctrl Pts',(6.76479937800053,0.172564119687984,-55.6890078742242));
#34191=CARTESIAN_POINT('Ctrl Pts',(6.76038147514405,0.345753230782343,-55.6808852799377));
#34192=CARTESIAN_POINT('Ctrl Pts',(6.74930803672678,0.518785832660119,-55.6727626856512));
#34193=CARTESIAN_POINT('Ctrl Pts',(6.73161612080699,0.69111026767913,-55.6646400913647));
#34194=CARTESIAN_POINT('Ctrl Pts',(6.71392207873954,0.863455411998051,-55.6565165209355));
#34195=CARTESIAN_POINT('Ctrl Pts',(6.68960801394717,1.03509185601515,-55.6483929505063));
#34196=CARTESIAN_POINT('Ctrl Pts',(6.6587627423749,1.20547407303511,-55.6402693800771));
#34197=CARTESIAN_POINT('Ctrl Pts',(6.62789500306871,1.37598039667254,-55.6321398924292));
#34198=CARTESIAN_POINT('Ctrl Pts',(6.59048662059584,1.54523030811715,-55.6240104047812));
#34199=CARTESIAN_POINT('Ctrl Pts',(6.54667747308637,1.71268884021105,-55.6158809171333));
#34200=CARTESIAN_POINT('Ctrl Pts',(6.5028504648281,1.88021564422865,-55.6077481151379));
#34201=CARTESIAN_POINT('Ctrl Pts',(6.45261759600558,2.0459492630818,-55.5996153131425));
#34202=CARTESIAN_POINT('Ctrl Pts',(6.39616825237131,2.20937110675353,-55.5914825111471));
#34203=CARTESIAN_POINT('Ctrl Pts',(6.33965752792579,2.3729706489545,-55.5833408658605));
#34204=CARTESIAN_POINT('Ctrl Pts',(6.27691696022806,2.53425305454727,-55.5751992205739));
#34205=CARTESIAN_POINT('Ctrl Pts',(6.20818387171808,2.69272018875699,-55.5670575752873));
#34206=CARTESIAN_POINT('Ctrl Pts',(6.17316577985995,2.77345592728628,-55.5629095748307));
#34207=CARTESIAN_POINT('Ctrl Pts',(6.13659295702548,2.85346129374103,-55.5587615743741));
#34208=CARTESIAN_POINT('Ctrl Pts',(6.09850128228009,2.93267303155809,-55.5546135739175));
#34209=CARTESIAN_POINT('Ctrl Pts',(6.01971100139163,3.09651762789013,-55.5460336906941));
#34210=CARTESIAN_POINT('Ctrl Pts',(5.93425450913703,3.25730806693052,-55.5374538074706));
#34211=CARTESIAN_POINT('Ctrl Pts',(5.84239419721187,3.4144866443413,-55.5288739242472));
#34212=CARTESIAN_POINT('Ctrl Pts',(5.75209760226665,3.56898960694923,-55.5204400944041));
#34213=CARTESIAN_POINT('Ctrl Pts',(5.6556136276282,3.72000238227505,-55.5120062645611));
#34214=CARTESIAN_POINT('Ctrl Pts',(5.55323872585679,3.86701805706212,-55.5035724347181));
#34215=CARTESIAN_POINT('Ctrl Pts',(5.45092220118252,4.01394989930645,-55.495143414086));
#34216=CARTESIAN_POINT('Ctrl Pts',(5.34272163532201,4.15688891143084,-55.486714393454));
#34217=CARTESIAN_POINT('Ctrl Pts',(5.22897745193762,4.29535607454469,-55.478285372822));
#34218=CARTESIAN_POINT('Ctrl Pts',(5.11528224480755,4.43376361612192,-55.4698599815787));
#34219=CARTESIAN_POINT('Ctrl Pts',(4.99604839027207,4.56770289028908,-55.4614345903354));
#34220=CARTESIAN_POINT('Ctrl Pts',(4.8716575757501,4.69672667553017,-55.4530091990921));
#34221=CARTESIAN_POINT('Ctrl Pts',(4.74331974761238,4.82984448201438,-55.4443164638807));
#34222=CARTESIAN_POINT('Ctrl Pts',(4.60949252562073,4.95772942708577,-55.4356237286692));
#34223=CARTESIAN_POINT('Ctrl Pts',(4.47063809897705,5.07992952588664,-55.4269309934578));
#34224=CARTESIAN_POINT('Ctrl Pts',(4.33610052849683,5.19833053622895,-55.4185085073733));
#34225=CARTESIAN_POINT('Ctrl Pts',(4.19684392465754,5.31139465328017,-55.4100860212888));
#34226=CARTESIAN_POINT('Ctrl Pts',(4.0533241961618,5.41875003675288,-55.4016635352044));
#34227=CARTESIAN_POINT('Ctrl Pts',(3.90289687275794,5.53127242763291,-55.3928356754295));
#34228=CARTESIAN_POINT('Ctrl Pts',(3.74778621850906,5.63752272742884,-55.3840078156545));
#34229=CARTESIAN_POINT('Ctrl Pts',(3.58855372598737,5.73712220156606,-55.3751799558796));
#34230=CARTESIAN_POINT('Ctrl Pts',(3.42932123346567,5.83672167570329,-55.3663520961047));
#34231=CARTESIAN_POINT('Ctrl Pts',(3.26596726665884,5.92967011184458,-55.3575242363298));
#34232=CARTESIAN_POINT('Ctrl Pts',(3.09908550384722,6.01564277861012,-55.3486963765549));
#34233=CARTESIAN_POINT('Origin',(0.,0.,-63.6971797838103));
#34234=CARTESIAN_POINT('',(3.09908550384721,6.01564277861012,-52.953975806663));
#34235=CARTESIAN_POINT('',(3.0990855038472,6.01564277861013,-53.3487566918479));
#34236=CARTESIAN_POINT('',(3.09908550384721,6.01564277861012,-63.6971797838103));
#34237=CARTESIAN_POINT('',(-6.76699999907272,0.000112025758056779,-54.3028202161463));
#34238=CARTESIAN_POINT('Ctrl Pts',(-6.76699999907272,0.000112025758070302,
-54.3028202161463));
#34239=CARTESIAN_POINT('Ctrl Pts',(-6.76700315016816,-0.190232259186009,
-54.2938337921293));
#34240=CARTESIAN_POINT('Ctrl Pts',(-6.75897086966551,-0.380644028120085,
-54.2848473681123));
#34241=CARTESIAN_POINT('Ctrl Pts',(-6.74291213548057,-0.570460281867895,
-54.2758609440953));
#34242=CARTESIAN_POINT('Ctrl Pts',(-6.72686977671977,-0.760082976047031,
-54.2668836837212));
#34243=CARTESIAN_POINT('Ctrl Pts',(-6.70281732287362,-0.949111119762301,
-54.257906423347));
#34244=CARTESIAN_POINT('Ctrl Pts',(-6.67081572306745,-1.1368845978709,-54.2489291629729));
#34245=CARTESIAN_POINT('Ctrl Pts',(-6.6388707111414,-1.32432603935843,-54.2399677769343));
#34246=CARTESIAN_POINT('Ctrl Pts',(-6.59900466007583,-1.5105170002127,-54.2310063908957));
#34247=CARTESIAN_POINT('Ctrl Pts',(-6.5513299045297,-1.69480544075564,-54.2220450048571));
#34248=CARTESIAN_POINT('Ctrl Pts',(-6.5037136720446,-1.87886765835247,-54.213094619352));
#34249=CARTESIAN_POINT('Ctrl Pts',(-6.44830792390815,-2.06103177573666,
-54.2041442338468));
#34250=CARTESIAN_POINT('Ctrl Pts',(-6.38527585279149,-2.24065644036695,
-54.1951938483417));
#34251=CARTESIAN_POINT('Ctrl Pts',(-6.3223714695473,-2.41991722846802,-54.1862615941729));
#34252=CARTESIAN_POINT('Ctrl Pts',(-6.25187168159047,-2.59664859765189,
-54.1773293400041));
#34253=CARTESIAN_POINT('Ctrl Pts',(-6.1739891715736,-2.77022502863792,-54.1683970858353));
#34254=CARTESIAN_POINT('Ctrl Pts',(-6.12392845320755,-2.88179514655903,
-54.1626556804771));
#34255=CARTESIAN_POINT('Ctrl Pts',(-6.0708185362946,-2.99206203359894,-54.1569142751189));
#34256=CARTESIAN_POINT('Ctrl Pts',(-6.01472678269943,-3.10086290078716,
-54.1511728697608));
#34257=CARTESIAN_POINT('Ctrl Pts',(-5.93536603808171,-3.25479850239856,
-54.1430497112718));
#34258=CARTESIAN_POINT('Ctrl Pts',(-5.85006649384746,-3.40573474770476,
-54.1349265527829));
#34259=CARTESIAN_POINT('Ctrl Pts',(-5.75909322121416,-3.55318649515687,
-54.126803394294));
#34260=CARTESIAN_POINT('Ctrl Pts',(-5.66812636266667,-3.70062784649884,
-54.1186808085297));
#34261=CARTESIAN_POINT('Ctrl Pts',(-5.57148676472573,-3.8445848778403,-54.1105582227654));
#34262=CARTESIAN_POINT('Ctrl Pts',(-5.46948404592724,-3.98459951203974,
-54.1024356370011));
#34263=CARTESIAN_POINT('Ctrl Pts',(-5.3674690704458,-4.12463097044742,-54.094312075224));
#34264=CARTESIAN_POINT('Ctrl Pts',(-5.26008990737592,-4.26071879329549,
-54.086188513447));
#34265=CARTESIAN_POINT('Ctrl Pts',(-5.14769781774396,-4.39243624622988,
-54.0780649516699));
#34266=CARTESIAN_POINT('Ctrl Pts',(-5.03522386380352,-4.5242496397081,-54.0699354728414));
#34267=CARTESIAN_POINT('Ctrl Pts',(-4.91772992847697,-4.65168602667329,
-54.061805994013));
#34268=CARTESIAN_POINT('Ctrl Pts',(-4.79560608559244,-4.77435349255046,
-54.0536765151845));
#34269=CARTESIAN_POINT('Ctrl Pts',(-4.6734324549609,-4.89707096780019,-54.0455437221103));
#34270=CARTESIAN_POINT('Ctrl Pts',(-4.54662542218313,-5.01501539747717,
-54.037410929036));
#34271=CARTESIAN_POINT('Ctrl Pts',(-4.41560960305938,-5.12783393192192,
-54.0292781359618));
#34272=CARTESIAN_POINT('Ctrl Pts',(-4.28445132410331,-5.24077513941186,
-54.0211364997085));
#34273=CARTESIAN_POINT('Ctrl Pts',(-4.14907540421544,-5.3485790916189,-54.0129948634553));
#34274=CARTESIAN_POINT('Ctrl Pts',(-4.00993759149697,-5.45093473748306,
-54.004853227202));
#34275=CARTESIAN_POINT('Ctrl Pts',(-3.93904877082046,-5.50308354507984,
-54.0007051744111));
#34276=CARTESIAN_POINT('Ctrl Pts',(-3.86718389971976,-5.55381880843328,
-53.9965571216202));
#34277=CARTESIAN_POINT('Ctrl Pts',(-3.79440581706842,-5.6031039161698,-53.9924090688293));
#34278=CARTESIAN_POINT('Ctrl Pts',(-3.64631246278333,-5.70339230870645,
-53.9839683538615));
#34279=CARTESIAN_POINT('Ctrl Pts',(-3.49413123723308,-5.79787991970299,
-53.9755276388938));
#34280=CARTESIAN_POINT('Ctrl Pts',(-3.33834498347224,-5.88623324132894,
-53.967086923926));
#34281=CARTESIAN_POINT('Ctrl Pts',(-3.18267648030597,-5.97451978134929,
-53.9586525888486));
#34282=CARTESIAN_POINT('Ctrl Pts',(-3.0234086697346,-6.056681110859,-53.9502182537711));
#34283=CARTESIAN_POINT('Ctrl Pts',(-2.86105246267856,-6.13242756221392,
-53.9417839186936));
#34284=CARTESIAN_POINT('Ctrl Pts',(-2.69879404044821,-6.20812839256256,
-53.9333546634958));
#34285=CARTESIAN_POINT('Ctrl Pts',(-2.5334512315112,-6.27742190678962,-53.9249254082979));
#34286=CARTESIAN_POINT('Ctrl Pts',(-2.36555893444202,-6.34006466273662,
-53.9164961531));
#34287=CARTESIAN_POINT('Ctrl Pts',(-2.19774200309267,-6.40267929877295,
-53.908070681738));
#34288=CARTESIAN_POINT('Ctrl Pts',(-2.02737817738107,-6.45864901290426,
-53.8996452103759));
#34289=CARTESIAN_POINT('Ctrl Pts',(-1.85502206103716,-6.50777858820239,
-53.8912197390139));
#34290=CARTESIAN_POINT('Ctrl Pts',(-1.68271689816403,-6.55689363937203,
-53.8827967584657));
#34291=CARTESIAN_POINT('Ctrl Pts',(-1.50842093951769,-6.5991724930234,-53.8743737779176));
#34292=CARTESIAN_POINT('Ctrl Pts',(-1.33270404571539,-6.63446975473804,
-53.8659507973694));
#34293=CARTESIAN_POINT('Ctrl Pts',(-1.15698424240966,-6.66976760090135,
-53.8575276773543));
#34294=CARTESIAN_POINT('Ctrl Pts',(-0.979843782440087,-6.69808355203235,
-53.8491045573393));
#34295=CARTESIAN_POINT('Ctrl Pts',(-0.801863484820748,-6.71932317660872,
-53.8406814373242));
#34296=CARTESIAN_POINT('Ctrl Pts',(-0.623877032347734,-6.74056353568651,
-53.8322580260237));
#34297=CARTESIAN_POINT('Ctrl Pts',(-0.445051015453118,-6.75472704060123,
-53.8238346147232));
#34298=CARTESIAN_POINT('Ctrl Pts',(-0.265972313979574,-6.76177104967303,
-53.8154112034227));
#34299=CARTESIAN_POINT('Ctrl Pts',(-0.0868624445075006,-6.76881628472907,
-53.806986326058));
#34300=CARTESIAN_POINT('Ctrl Pts',(0.0924998639961541,-6.76873954039166,
-53.7985614486933));
#34301=CARTESIAN_POINT('Ctrl Pts',(0.27152641305435,-6.76155029612395,-53.7901365713286));
#34302=CARTESIAN_POINT('Ctrl Pts',(0.450609096630224,-6.75435879763885,
-53.7817090523086));
#34303=CARTESIAN_POINT('Ctrl Pts',(0.62935547777268,-6.74005036627477,-53.7732815332886));
#34304=CARTESIAN_POINT('Ctrl Pts',(0.807180791421248,-6.71868649141784,
-53.7648540142686));
#34305=CARTESIAN_POINT('Ctrl Pts',(0.985165571938591,-6.6973034582636,-53.7564189377753));
#34306=CARTESIAN_POINT('Ctrl Pts',(1.16222730311712,-6.66885237908188,-53.747983861282));
#34307=CARTESIAN_POINT('Ctrl Pts',(1.33778860880441,-6.63344636204689,-53.7395487847887));
#34308=CARTESIAN_POINT('Ctrl Pts',(1.5134347644261,-6.59802323305087,-53.7311096315674));
#34309=CARTESIAN_POINT('Ctrl Pts',(1.68757872324648,-6.5556385361644,-53.722670478346));
#34310=CARTESIAN_POINT('Ctrl Pts',(1.85965611955421,-6.5064558798938,-53.7142313251247));
#34311=CARTESIAN_POINT('Ctrl Pts',(2.0319247420978,-6.45721856790182,-53.705782793638));
#34312=CARTESIAN_POINT('Ctrl Pts',(2.20212189499794,-6.40116830115896,-53.6973342621512));
#34313=CARTESIAN_POINT('Ctrl Pts',(2.36969995644507,-6.33851805364821,-53.6888857306644));
#34314=CARTESIAN_POINT('Ctrl Pts',(2.46229227524887,-6.3039017581704,-53.684217642765));
#34315=CARTESIAN_POINT('Ctrl Pts',(2.55408536270464,-6.26727139338636,-53.6795495548656));
#34316=CARTESIAN_POINT('Ctrl Pts',(2.64498979819252,-6.22866903659662,-53.6748814669662));
#34317=CARTESIAN_POINT('Ctrl Pts',(2.8054672934996,-6.1605226420085,-53.6666406913654));
#34318=CARTESIAN_POINT('Ctrl Pts',(2.96353105095224,-6.08607630748875,-53.6583999157647));
#34319=CARTESIAN_POINT('Ctrl Pts',(3.11865367989214,-6.00552147818116,-53.6501591401639));
#34320=CARTESIAN_POINT('Ctrl Pts',(3.27360449370238,-5.92505587208063,-53.6419274921155));
#34321=CARTESIAN_POINT('Ctrl Pts',(3.42562035253868,-5.83849540570367,-53.6336958440672));
#34322=CARTESIAN_POINT('Ctrl Pts',(3.57419283431532,-5.74607993184302,-53.6254641960189));
#34323=CARTESIAN_POINT('Ctrl Pts',(3.72262723296485,-5.65375034883826,-53.6172401984566));
#34324=CARTESIAN_POINT('Ctrl Pts',(3.86762432766157,-5.55557678236179,-53.6090162008943));
#34325=CARTESIAN_POINT('Ctrl Pts',(4.00869927613141,-5.45184547777572,-53.6007922033321));
#34326=CARTESIAN_POINT('Ctrl Pts',(4.1496495843348,-5.34820582020128,-53.5925754717037));
#34327=CARTESIAN_POINT('Ctrl Pts',(4.28668436733827,-5.23901842118942,-53.5843587400753));
#34328=CARTESIAN_POINT('Ctrl Pts',(4.41934693165567,-5.1246133217703,-53.5761420084469));
#34329=CARTESIAN_POINT('Ctrl Pts',(4.55194152802915,-5.0102668363198,-53.5679294865544));
#34330=CARTESIAN_POINT('Ctrl Pts',(4.68016809823934,-4.89070820624697,-53.5597169646619));
#34331=CARTESIAN_POINT('Ctrl Pts',(4.80360194823375,-4.76630856354527,-53.5515044427694));
#34332=CARTESIAN_POINT('Ctrl Pts',(4.92699452135417,-4.64195052068328,-53.5432946671837));
#34333=CARTESIAN_POINT('Ctrl Pts',(5.04559731672299,-4.51275494242931,-53.5350848915981));
#34334=CARTESIAN_POINT('Ctrl Pts',(5.15902147030627,-4.37913078919995,-53.5268751160124));
#34335=CARTESIAN_POINT('Ctrl Pts',(5.20856219346421,-4.32076723105808,-53.5232892993532));
#34336=CARTESIAN_POINT('Ctrl Pts',(5.25711545816215,-4.26155929676581,-53.519703482694));
#34337=CARTESIAN_POINT('Ctrl Pts',(5.30465117116476,-4.20154316320329,-53.5161176660348));
#34338=CARTESIAN_POINT('Ctrl Pts',(5.42208758626565,-4.05327401715283,-53.5072589485134));
#34339=CARTESIAN_POINT('Ctrl Pts',(5.53318926672605,-3.90022376079815,-53.498400230992));
#34340=CARTESIAN_POINT('Ctrl Pts',(5.63760965823033,-3.74294621139926,-53.4895415134706));
#34341=CARTESIAN_POINT('Ctrl Pts',(5.74222540351655,-3.58537442096521,-53.4806662227115));
#34342=CARTESIAN_POINT('Ctrl Pts',(5.84013473676203,-3.42355974877974,-53.4717909319523));
#34343=CARTESIAN_POINT('Ctrl Pts',(5.93103639079377,-3.25808169496715,-53.4629156411932));
#34344=CARTESIAN_POINT('Ctrl Pts',(6.02219622596247,-3.09213364627349,-53.4540151426127));
#34345=CARTESIAN_POINT('Ctrl Pts',(6.10630842715907,-2.92250162334648,-53.4451146440322));
#34346=CARTESIAN_POINT('Ctrl Pts',(6.18311806884459,-2.74978907313408,-53.4362141454517));
#34347=CARTESIAN_POINT('Ctrl Pts',(6.26003168784538,-2.57684272171012,-53.4273015982543));
#34348=CARTESIAN_POINT('Ctrl Pts',(6.32962290111525,-2.400807752545,-53.4183890510568));
#34349=CARTESIAN_POINT('Ctrl Pts',(6.3916858602023,-2.22230530406827,-53.4094765038594));
#34350=CARTESIAN_POINT('Ctrl Pts',(6.45388586036458,-2.04340870475132,-53.4005442768873));
#34351=CARTESIAN_POINT('Ctrl Pts',(6.50852427183568,-1.86203397431315,-53.3916120499152));
#34352=CARTESIAN_POINT('Ctrl Pts',(6.55544504450166,-1.67881781873992,-53.3826798229431));
#34353=CARTESIAN_POINT('Ctrl Pts',(6.59979059289516,-1.5056573946505,-53.3742378369965));
#34354=CARTESIAN_POINT('Ctrl Pts',(6.63724280979381,-1.3308524048672,-53.3657958510498));
#34355=CARTESIAN_POINT('Ctrl Pts',(6.66771230148169,-1.154946606848,-53.3573538651031));
#34356=CARTESIAN_POINT('Ctrl Pts',(6.69739492849889,-0.983583518607065,
-53.3491298906862));
#34357=CARTESIAN_POINT('Ctrl Pts',(6.72050650524564,-0.810848222265133,
-53.3409059162692));
#34358=CARTESIAN_POINT('Ctrl Pts',(6.73692481753425,-0.63728565250693,-53.3326819418522));
#34359=CARTESIAN_POINT('Ctrl Pts',(6.75332579049209,-0.463906381662319,
-53.3244666527502));
#34360=CARTESIAN_POINT('Ctrl Pts',(6.76304754173078,-0.289701931241656,
-53.3162513636481));
#34361=CARTESIAN_POINT('Ctrl Pts',(6.76601889535557,-0.115227200310467,
-53.3080360745461));
#34362=CARTESIAN_POINT('Ctrl Pts',(6.76898770693284,0.0590982642884879,
-53.2998278137745));
#34363=CARTESIAN_POINT('Ctrl Pts',(6.76521761649876,0.23369319236014,-53.291619553003));
#34364=CARTESIAN_POINT('Ctrl Pts',(6.75468925113634,0.40799769678658,-53.2834112922314));
#34365=CARTESIAN_POINT('Ctrl Pts',(6.74416778181926,0.582188032325334,-53.2752084078442));
#34366=CARTESIAN_POINT('Ctrl Pts',(6.72689687653686,0.756087966466645,-53.2670055234569));
#34367=CARTESIAN_POINT('Ctrl Pts',(6.70290923580914,0.929137652075598,-53.2588026390697));
#34368=CARTESIAN_POINT('Ctrl Pts',(6.6789324978523,1.1021086838021,-53.2506034830261));
#34369=CARTESIAN_POINT('Ctrl Pts',(6.64824515568848,1.27422988244227,-53.2424043269826));
#34370=CARTESIAN_POINT('Ctrl Pts',(6.61093175694738,1.44494647132155,-53.234205170939));
#34371=CARTESIAN_POINT('Ctrl Pts',(6.57362160356463,1.61564821200889,-53.2260067280227));
#34372=CARTESIAN_POINT('Ctrl Pts',(6.52968660969767,1.78494523439371,-53.2178082851063));
#34373=CARTESIAN_POINT('Ctrl Pts',(6.47926252155291,1.95229254385705,-53.20960984219));
#34374=CARTESIAN_POINT('Ctrl Pts',(6.4288389355724,2.11963818673923,-53.2014114809204));
#34375=CARTESIAN_POINT('Ctrl Pts',(6.37192648650464,2.28503381162324,-53.1932131196509));
#34376=CARTESIAN_POINT('Ctrl Pts',(6.30871089728012,2.44794930800028,-53.1850147583813));
#34377=CARTESIAN_POINT('Ctrl Pts',(6.24548445404361,2.61089277669829,-53.1768149894667));
#34378=CARTESIAN_POINT('Ctrl Pts',(6.17595284427489,2.77135493408912,-53.1686152205521));
#34379=CARTESIAN_POINT('Ctrl Pts',(6.10035008355252,2.92882533758856,-53.1604154516375));
#34380=CARTESIAN_POINT('Ctrl Pts',(6.02472060803572,3.08635138441928,-53.1522127852739));
#34381=CARTESIAN_POINT('Ctrl Pts',(5.94301586327166,3.24088324831998,-53.1440101189103));
#34382=CARTESIAN_POINT('Ctrl Pts',(5.85551600434688,3.39193474625288,-53.1358074525467));
#34383=CARTESIAN_POINT('Ctrl Pts',(5.76791676745299,3.54315780093203,-53.1275954700044));
#34384=CARTESIAN_POINT('Ctrl Pts',(5.67450944722322,3.69089228197221,-53.1193834874621));
#34385=CARTESIAN_POINT('Ctrl Pts',(5.57561833368542,3.83467980372169,-53.1111715049198));
#34386=CARTESIAN_POINT('Ctrl Pts',(5.47666889283215,3.97855213329507,-53.1029546788392));
#34387=CARTESIAN_POINT('Ctrl Pts',(5.37222942552659,4.11847257613394,-53.0947378527586));
#34388=CARTESIAN_POINT('Ctrl Pts',(5.26266469357066,4.25401567028671,-53.0865210266779));
#34389=CARTESIAN_POINT('Ctrl Pts',(5.15293099697428,4.38976779146632,-53.0782915290648));
#34390=CARTESIAN_POINT('Ctrl Pts',(5.03805647683891,4.52112880420129,-53.0700620314517));
#34391=CARTESIAN_POINT('Ctrl Pts',(4.91844385480994,4.64770901058601,-53.0618325338385));
#34392=CARTESIAN_POINT('Ctrl Pts',(4.8118262599465,4.76053721327173,-53.0544971103058));
#34393=CARTESIAN_POINT('Ctrl Pts',(4.70144479333497,4.86956739768718,-53.047161686773));
#34394=CARTESIAN_POINT('Ctrl Pts',(4.58760622732013,4.97455104537621,-53.0398262632402));
#34395=CARTESIAN_POINT('Ctrl Pts',(4.46236151905179,5.09005360999957,-53.0317558613321));
#34396=CARTESIAN_POINT('Ctrl Pts',(4.33252320066664,5.20103397968373,-53.0236854594239));
#34397=CARTESIAN_POINT('Ctrl Pts',(4.19845643524763,5.3070945498764,-53.0156150575158));
#34398=CARTESIAN_POINT('Ctrl Pts',(4.06453646939973,5.41303898654285,-53.0075534924848));
#34399=CARTESIAN_POINT('Ctrl Pts',(3.92639755208268,5.51407410735804,-52.9994919274538));
#34400=CARTESIAN_POINT('Ctrl Pts',(3.78444247203027,5.6098381595099,-52.9914303624229));
#34401=CARTESIAN_POINT('Ctrl Pts',(3.64265125331076,5.70549166947318,-52.9833781030032));
#34402=CARTESIAN_POINT('Ctrl Pts',(3.49705294931979,5.79588601843103,-52.9753258435834));
#34403=CARTESIAN_POINT('Ctrl Pts',(3.34808386484208,5.88069923002224,-52.9672735841637));
#34404=CARTESIAN_POINT('Ctrl Pts',(3.26607964562807,5.92738704595367,-52.9628409916635));
#34405=CARTESIAN_POINT('Ctrl Pts',(3.18305458350682,5.97238433273468,-52.9584083991633));
#34406=CARTESIAN_POINT('Ctrl Pts',(3.09908550384721,6.01564277861012,-52.953975806663));
#34407=CARTESIAN_POINT('Ctrl Pts',(3.09908550384721,6.01564277861012,-54.9544629019808));
#34408=CARTESIAN_POINT('Ctrl Pts',(3.0397660155061,6.04620246660676,-54.9513058927933));
#34409=CARTESIAN_POINT('Ctrl Pts',(2.98003448412068,6.07586403636278,-54.9481488836058));
#34410=CARTESIAN_POINT('Ctrl Pts',(2.91992138371238,6.10461695054974,-54.9449918744183));
#34411=CARTESIAN_POINT('Ctrl Pts',(2.76123539795879,6.180518617575,-54.9366580318525));
#34412=CARTESIAN_POINT('Ctrl Pts',(2.59938502055361,6.25032607350716,-54.9283241892866));
#34413=CARTESIAN_POINT('Ctrl Pts',(2.43487229791274,6.31376954701842,-54.9199903467208));
#34414=CARTESIAN_POINT('Ctrl Pts',(2.2705534743535,6.37713824436008,-54.911666326644));
#34415=CARTESIAN_POINT('Ctrl Pts',(2.10357887834545,6.434157777379,-54.9033423065672));
#34416=CARTESIAN_POINT('Ctrl Pts',(1.93447389087424,6.48460482724475,-54.8950182864904));
#34417=CARTESIAN_POINT('Ctrl Pts',(1.76553720989281,6.53500166826681,-54.8867025511284));
#34418=CARTESIAN_POINT('Ctrl Pts',(1.59447469311592,6.57883896006349,-54.8783868157665));
#34419=CARTESIAN_POINT('Ctrl Pts',(1.42183059699803,6.61594186442416,-54.8700710804045));
#34420=CARTESIAN_POINT('Ctrl Pts',(1.24932669690675,6.65301463928788,-54.8617620978542));
#34421=CARTESIAN_POINT('Ctrl Pts',(1.07524411522569,6.68336385079959,-54.8534531153038));
#34422=CARTESIAN_POINT('Ctrl Pts',(0.90014135101851,6.70686473310642,-54.8451441327535));
#34423=CARTESIAN_POINT('Ctrl Pts',(0.725148713666631,6.73035083507395,-54.8368403759466));
#34424=CARTESIAN_POINT('Ctrl Pts',(0.549137516245436,6.74699714528917,-54.8285366191396));
#34425=CARTESIAN_POINT('Ctrl Pts',(0.372675736634933,6.75673011117979,-54.8202328623327));
#34426=CARTESIAN_POINT('Ctrl Pts',(0.196285596261459,6.76645912572042,-54.8119324766513));
#34427=CARTESIAN_POINT('Ctrl Pts',(0.0194455849327746,6.7692803692821,-54.8036320909699));
#34428=CARTESIAN_POINT('Ctrl Pts',(-0.157271622801084,6.76517218085848,
-54.7953317052884));
#34429=CARTESIAN_POINT('Ctrl Pts',(-0.333951565470907,6.76106485874498,
-54.7870330699425));
#34430=CARTESIAN_POINT('Ctrl Pts',(-0.510508408640314,6.7500310238645,-54.7787344345966));
#34431=CARTESIAN_POINT('Ctrl Pts',(-0.686369653741176,6.73210113548684,
-54.7704357992507));
#34432=CARTESIAN_POINT('Ctrl Pts',(-0.862223005230163,6.71417205190037,
-54.7621375363927));
#34433=CARTESIAN_POINT('Ctrl Pts',(-1.03738047491462,6.68934756708489,-54.7538392735348));
#34434=CARTESIAN_POINT('Ctrl Pts',(-1.21127466263797,6.65771001859132,-54.7455410106769));
#34435=CARTESIAN_POINT('Ctrl Pts',(-1.38518990820995,6.62606863892481,-54.7372417429346));
#34436=CARTESIAN_POINT('Ctrl Pts',(-1.55784122495393,6.58761261444436,-54.7289424751922));
#34437=CARTESIAN_POINT('Ctrl Pts',(-1.72867118702229,6.54247544337455,-54.7206432074499));
#34438=CARTESIAN_POINT('Ctrl Pts',(-1.8996210992816,6.4973065787293,-54.7123381122828));
#34439=CARTESIAN_POINT('Ctrl Pts',(-2.06874676477396,6.44544728251986,-54.7040330171157));
#34440=CARTESIAN_POINT('Ctrl Pts',(-2.23550484287439,6.38708126592148,-54.6957279219486));
#34441=CARTESIAN_POINT('Ctrl Pts',(-2.40232372965176,6.32869396603484,-54.6874197983114));
#34442=CARTESIAN_POINT('Ctrl Pts',(-2.56677298250584,6.26379533852226,-54.6791116746742));
#34443=CARTESIAN_POINT('Ctrl Pts',(-2.72832883504125,6.19261744078241,-54.6708035510371));
#34444=CARTESIAN_POINT('Ctrl Pts',(-2.89005642055325,6.12136388133143,-54.6624865959105));
#34445=CARTESIAN_POINT('Ctrl Pts',(-3.04888414519265,6.0438178625554,-54.6541696407839));
#34446=CARTESIAN_POINT('Ctrl Pts',(-3.20431148179891,5.96025812592137,-54.6458526856573));
#34447=CARTESIAN_POINT('Ctrl Pts',(-3.31885909485103,5.89867585482487,-54.6397232146233));
#34448=CARTESIAN_POINT('Ctrl Pts',(-3.43156029632883,5.83382822072068,-54.6335937435893));
#34449=CARTESIAN_POINT('Ctrl Pts',(-3.54222479973134,5.76584186985459,-54.6274642725554));
#34450=CARTESIAN_POINT('Ctrl Pts',(-3.69480376105335,5.67210551826684,-54.6190132490107));
#34451=CARTESIAN_POINT('Ctrl Pts',(-3.84378878812548,5.57222972919851,-54.610562225466));
#34452=CARTESIAN_POINT('Ctrl Pts',(-3.98867340368538,5.46651383230052,-54.6021112019213));
#34453=CARTESIAN_POINT('Ctrl Pts',(-4.13343045263647,5.36089101511573,-54.5936676192524));
#34454=CARTESIAN_POINT('Ctrl Pts',(-4.27409401953163,5.24943853364486,-54.5852240365834));
#34455=CARTESIAN_POINT('Ctrl Pts',(-4.41018553649275,5.13249963796493,-54.5767804539144));
#34456=CARTESIAN_POINT('Ctrl Pts',(-4.54617572906893,5.0156478069452,-54.5683431577564));
#34457=CARTESIAN_POINT('Ctrl Pts',(-4.67760040689393,4.89331791991543,-54.5599058615985));
#34458=CARTESIAN_POINT('Ctrl Pts',(-4.80401280203065,4.76589445937755,-54.5514685654405));
#34459=CARTESIAN_POINT('Ctrl Pts',(-4.93033501154598,4.63856190577927,-54.5430372886511));
#34460=CARTESIAN_POINT('Ctrl Pts',(-5.05165183817416,4.50614326180706,-54.5346060118617));
#34461=CARTESIAN_POINT('Ctrl Pts',(-5.16755206655165,4.36906107069674,-54.5261747350723));
#34462=CARTESIAN_POINT('Ctrl Pts',(-5.2834026158868,4.23203763798641,-54.5177470722339));
#34463=CARTESIAN_POINT('Ctrl Pts',(-5.39384098185699,4.09035489583673,-54.5093194093956));
#34464=CARTESIAN_POINT('Ctrl Pts',(-5.49849463773981,3.94447027099287,-54.5008917465573));
#34465=CARTESIAN_POINT('Ctrl Pts',(-5.60311607707546,3.79863055522418,-54.492466678088));
#34466=CARTESIAN_POINT('Ctrl Pts',(-5.70195616462208,3.64859180537235,-54.4840416096186));
#34467=CARTESIAN_POINT('Ctrl Pts',(-5.79468409162147,3.494842668606,-54.4756165411493));
#34468=CARTESIAN_POINT('Ctrl Pts',(-5.82005728957281,3.45277220064388,-54.4733111846408));
#34469=CARTESIAN_POINT('Ctrl Pts',(-5.84497309589304,3.41042409212107,-54.4710058281323));
#34470=CARTESIAN_POINT('Ctrl Pts',(-5.86942530269911,3.36780872616535,-54.4687004716238));
#34471=CARTESIAN_POINT('Ctrl Pts',(-5.96084426146999,3.20848354074512,-54.4600814830281));
#34472=CARTESIAN_POINT('Ctrl Pts',(-6.04573886810129,3.04549186441933,-54.4514624944324));
#34473=CARTESIAN_POINT('Ctrl Pts',(-6.12383968349658,2.87938822162496,-54.4428435058367));
#34474=CARTESIAN_POINT('Ctrl Pts',(-6.20198728826842,2.71318506788629,-54.4342193536956));
#34475=CARTESIAN_POINT('Ctrl Pts',(-6.27333284973063,2.5438665022574,-54.4255952015546));
#34476=CARTESIAN_POINT('Ctrl Pts',(-6.33765486817745,2.3720075404321,-54.4169710494135));
#34477=CARTESIAN_POINT('Ctrl Pts',(-6.40417993222563,2.19426236516003,-54.4080515178534));
#34478=CARTESIAN_POINT('Ctrl Pts',(-6.4631917009667,2.01380003230584,-54.3991319862933));
#34479=CARTESIAN_POINT('Ctrl Pts',(-6.51450118719296,1.83127367754293,-54.3902124547332));
#34480=CARTESIAN_POINT('Ctrl Pts',(-6.5642039255264,1.65446310474291,-54.381572236797));
#34481=CARTESIAN_POINT('Ctrl Pts',(-6.60667944680759,1.4757161298277,-54.3729320188608));
#34482=CARTESIAN_POINT('Ctrl Pts',(-6.64180796657907,1.29563726987412,-54.3642918009246));
#34483=CARTESIAN_POINT('Ctrl Pts',(-6.67863989375865,1.10682625536108,-54.3552326125526));
#34484=CARTESIAN_POINT('Ctrl Pts',(-6.70739452440246,0.916551359942948,
-54.3461734241805));
#34485=CARTESIAN_POINT('Ctrl Pts',(-6.72799486069623,0.7255164742755,-54.3371142358084));
#34486=CARTESIAN_POINT('Ctrl Pts',(-6.74859519698999,0.53448158860806,-54.3280550474364));
#34487=CARTESIAN_POINT('Ctrl Pts',(-6.76104124721361,0.342687096659948,
-54.3189958590643));
#34488=CARTESIAN_POINT('Ctrl Pts',(-6.76531867369208,0.150838467882794,
-54.3099366706923));
#34489=CARTESIAN_POINT('Ctrl Pts',(-6.76643871924403,0.100602840364678,
-54.3075645191915));
#34490=CARTESIAN_POINT('Ctrl Pts',(-6.76699916726937,0.0503573167275674,
-54.3051923676907));
#34491=CARTESIAN_POINT('Ctrl Pts',(-6.76699999907271,0.000112026683497747,
-54.30282021619));
#34492=CARTESIAN_POINT('',(-6.76699743900148,-0.00588732090316101,-54.6971797837852));
#34493=CARTESIAN_POINT('Ctrl Pts',(3.09908550384722,6.01564277861012,-55.3486963765549));
#34494=CARTESIAN_POINT('Ctrl Pts',(2.93976283080413,6.09772122053783,-55.3402683842273));
#34495=CARTESIAN_POINT('Ctrl Pts',(2.77722522026857,6.17344176643959,-55.3318403918997));
#34496=CARTESIAN_POINT('Ctrl Pts',(2.61201193932657,6.24257019414403,-55.3234123995721));
#34497=CARTESIAN_POINT('Ctrl Pts',(2.44664966910367,6.31176096184121,-55.3149768068839));
#34498=CARTESIAN_POINT('Ctrl Pts',(2.27860721536357,6.37434760490997,-55.3065412141957));
#34499=CARTESIAN_POINT('Ctrl Pts',(2.10844277015434,6.43014448398976,-55.2981056215075));
#34500=CARTESIAN_POINT('Ctrl Pts',(1.93819294341394,6.48596935965229,-55.2896657961853));
#34501=CARTESIAN_POINT('Ctrl Pts',(1.76581932084211,6.53499758082109,-55.281225970863));
#34502=CARTESIAN_POINT('Ctrl Pts',(1.59189359642014,6.57709387021932,-55.2727861455408));
#34503=CARTESIAN_POINT('Ctrl Pts',(1.41778013607079,6.61923559847345,-55.2643372102468));
#34504=CARTESIAN_POINT('Ctrl Pts',(1.24211155260136,6.65443037598622,-55.2558882749528));
#34505=CARTESIAN_POINT('Ctrl Pts',(1.06546914519395,6.68259414453996,-55.2474393396589));
#34506=CARTESIAN_POINT('Ctrl Pts',(0.993316315092483,6.69409815219757,-55.2439882171241));
#34507=CARTESIAN_POINT('Ctrl Pts',(0.921001067625565,6.70442966308823,-55.2405370945893));
#34508=CARTESIAN_POINT('Ctrl Pts',(0.848563193888828,6.71358544341079,-55.2370859720545));
#34509=CARTESIAN_POINT('Ctrl Pts',(0.675592049779231,6.73544811987978,-55.2288451916103));
#34510=CARTESIAN_POINT('Ctrl Pts',(0.50153663813381,6.7506519793541,-55.2206044111662));
#34511=CARTESIAN_POINT('Ctrl Pts',(0.326949049670479,6.75909707867253,-55.212363630722));
#34512=CARTESIAN_POINT('Ctrl Pts',(0.152554836175986,6.76753282411403,-55.2041319778492));
#34513=CARTESIAN_POINT('Ctrl Pts',(-0.0223700281979955,6.76922469849558,
-55.1959003249763));
#34514=CARTESIAN_POINT('Ctrl Pts',(-0.197265485963421,6.76412413606134,
-55.1876686721034));
#34515=CARTESIAN_POINT('Ctrl Pts',(-0.371998395639786,6.75902831409715,
-55.1794446697405));
#34516=CARTESIAN_POINT('Ctrl Pts',(-0.546701599591087,6.74715263797038,
-55.1712206673777));
#34517=CARTESIAN_POINT('Ctrl Pts',(-0.720812072433768,6.72850049834536,
-55.1629966650148));
#34518=CARTESIAN_POINT('Ctrl Pts',(-0.894768717059198,6.70986483805866,
-55.1547799286342));
#34519=CARTESIAN_POINT('Ctrl Pts',(-1.06813332192174,6.6844646848864,-55.1465631922537));
#34520=CARTESIAN_POINT('Ctrl Pts',(-1.24034514887233,6.65235544086971,-55.1383464558732));
#34521=CARTESIAN_POINT('Ctrl Pts',(-1.41246874477662,6.62026264771036,-55.1301339292572));
#34522=CARTESIAN_POINT('Ctrl Pts',(-1.58344039014235,6.58146767457903,-55.1219214026412));
#34523=CARTESIAN_POINT('Ctrl Pts',(-1.75270632266394,6.5360775352266,-55.1137088760253));
#34524=CARTESIAN_POINT('Ctrl Pts',(-1.92191565071386,6.49070257485803,-55.1054990957725));
#34525=CARTESIAN_POINT('Ctrl Pts',(-2.08942005897657,6.43873693393464,-55.0972893155198));
#34526=CARTESIAN_POINT('Ctrl Pts',(-2.25467771297685,6.38033834609149,-55.089079535267));
#34527=CARTESIAN_POINT('Ctrl Pts',(-2.32685734535631,6.35483157832634,-55.085493747219));
#34528=CARTESIAN_POINT('Ctrl Pts',(-2.39860854577049,6.3280982554676,-55.081907959171));
#34529=CARTESIAN_POINT('Ctrl Pts',(-2.46988710538396,6.30015449704673,-55.0783221711229));
#34530=CARTESIAN_POINT('Ctrl Pts',(-2.64598128990308,6.2311192446762,-55.0694634564463));
#34531=CARTESIAN_POINT('Ctrl Pts',(-2.81900706367222,6.1547646582062,-55.0606047417697));
#34532=CARTESIAN_POINT('Ctrl Pts',(-2.98838626350261,6.07139494186541,-55.0517460270931));
#34533=CARTESIAN_POINT('Ctrl Pts',(-3.1580823424592,5.98786925523493,-55.0428707392967));
#34534=CARTESIAN_POINT('Ctrl Pts',(-3.32411798127155,5.89730232566225,-55.0339954515003));
#34535=CARTESIAN_POINT('Ctrl Pts',(-3.48594122879942,5.80004334029983,-55.0251201637039));
#34536=CARTESIAN_POINT('Ctrl Pts',(-3.64822408849316,5.70250811889843,-55.0162196682176));
#34537=CARTESIAN_POINT('Ctrl Pts',(-3.80627039163525,5.59824294110568,-55.0073191727313));
#34538=CARTESIAN_POINT('Ctrl Pts',(-3.95955618398132,5.48764100738152,-54.998418677245));
#34539=CARTESIAN_POINT('Ctrl Pts',(-4.11304947856779,5.37688935235125,-54.9895061332007));
#34540=CARTESIAN_POINT('Ctrl Pts',(-4.26176918308157,5.2597839632968,-54.9805935891564));
#34541=CARTESIAN_POINT('Ctrl Pts',(-4.40522485176231,5.13675802480667,-54.9716810451121));
#34542=CARTESIAN_POINT('Ctrl Pts',(-4.54899728398812,5.01346043352812,-54.9627488213363));
#34543=CARTESIAN_POINT('Ctrl Pts',(-4.6874822338197,4.8842163139173,-54.9538165975605));
#34544=CARTESIAN_POINT('Ctrl Pts',(-4.82022445603094,4.74949736219332,-54.9448843737847));
#34545=CARTESIAN_POINT('Ctrl Pts',(-4.94568145610411,4.62217212042211,-54.9364423725869));
#34546=CARTESIAN_POINT('Ctrl Pts',(-5.06600898626905,4.48995693809524,-54.9280003713892));
#34547=CARTESIAN_POINT('Ctrl Pts',(-5.18085617329275,4.35327673272151,-54.9195583701915));
#34548=CARTESIAN_POINT('Ctrl Pts',(-5.2907928346339,4.22244056825272,-54.9114773239702));
#34549=CARTESIAN_POINT('Ctrl Pts',(-5.39594419765033,4.08722990267799,-54.903396277749));
#34550=CARTESIAN_POINT('Ctrl Pts',(-5.49593488230195,3.94803606486779,-54.8953152315278));
#34551=CARTESIAN_POINT('Ctrl Pts',(-5.59808594525775,3.80583483343557,-54.8870595878729));
#34552=CARTESIAN_POINT('Ctrl Pts',(-5.69485048431008,3.65947658957157,-54.878803944218));
#34553=CARTESIAN_POINT('Ctrl Pts',(-5.7858686313026,3.50941778380811,-54.8705483005631));
#34554=CARTESIAN_POINT('Ctrl Pts',(-5.87476860139071,3.36285115083847,-54.862484782482));
#34555=CARTESIAN_POINT('Ctrl Pts',(-5.95818644517708,3.21275461464334,-54.854421264401));
#34556=CARTESIAN_POINT('Ctrl Pts',(-6.03582831224443,3.05958585189378,-54.8463577463199));
#34557=CARTESIAN_POINT('Ctrl Pts',(-6.11342479917093,2.90650661326683,-54.8382989412062));
#34558=CARTESIAN_POINT('Ctrl Pts',(-6.18525185970134,2.75035905233115,-54.8302401360925));
#34559=CARTESIAN_POINT('Ctrl Pts',(-6.25106040147808,2.59162745337225,-54.8221813309788));
#34560=CARTESIAN_POINT('Ctrl Pts',(-6.31684345972862,2.43295732121918,-54.8141256465356));
#34561=CARTESIAN_POINT('Ctrl Pts',(-6.37661249610298,2.2717054863293,-54.8060699620924));
#34562=CARTESIAN_POINT('Ctrl Pts',(-6.43016565495611,2.10837820369659,-54.7980142776491));
#34563=CARTESIAN_POINT('Ctrl Pts',(-6.48602688876846,1.93801171704167,-54.7896114031625));
#34564=CARTESIAN_POINT('Ctrl Pts',(-6.53512436688111,1.76538729719315,-54.7812085286759));
#34565=CARTESIAN_POINT('Ctrl Pts',(-6.5772859921995,1.59109961247443,-54.7728056541894));
#34566=CARTESIAN_POINT('Ctrl Pts',(-6.61770753693504,1.42400507113478,-54.7647495803449));
#34567=CARTESIAN_POINT('Ctrl Pts',(-6.6517542056154,1.2553821973894,-54.7566935065005));
#34568=CARTESIAN_POINT('Ctrl Pts',(-6.6793262126381,1.08576716894813,-54.748637432656));
#34569=CARTESIAN_POINT('Ctrl Pts',(-6.7069026960708,0.9161246029246,-54.7405800508804));
#34570=CARTESIAN_POINT('Ctrl Pts',(-6.72800237314028,0.7454899302217,-54.7325226691047));
#34571=CARTESIAN_POINT('Ctrl Pts',(-6.7425771674299,0.574405902870916,-54.724465287329));
#34572=CARTESIAN_POINT('Ctrl Pts',(-6.75716071565542,0.403219118762315,
-54.716403066116));
#34573=CARTESIAN_POINT('Ctrl Pts',(-6.76521153804951,0.231582812735872,
-54.7083408449029));
#34574=CARTESIAN_POINT('Ctrl Pts',(-6.76673363030631,0.0600414563578614,
-54.7002786236899));
#34575=CARTESIAN_POINT('Ctrl Pts',(-6.76692864356885,0.038063261923281,
-54.6992456770633));
#34576=CARTESIAN_POINT('Ctrl Pts',(-6.76701655643823,0.0160866226493078,
-54.6982127304367));
#34577=CARTESIAN_POINT('Ctrl Pts',(-6.76699743900194,-0.00588732037279986,
-54.6971797838101));
#34578=CARTESIAN_POINT('Ctrl Pts',(-6.76699743900148,-0.00588732090315215,
-54.6971797837852));
#34579=CARTESIAN_POINT('Ctrl Pts',(-6.76680418587059,-0.228016106365009,
-54.6867379991958));
#34580=CARTESIAN_POINT('Ctrl Pts',(-6.75567034531407,-0.449632090273862,
-54.6762962146064));
#34581=CARTESIAN_POINT('Ctrl Pts',(-6.73376803723041,-0.669818647675761,
-54.6658544300171));
#34582=CARTESIAN_POINT('Ctrl Pts',(-6.71136652631499,-0.895023751641342,
-54.6551746536866));
#34583=CARTESIAN_POINT('Ctrl Pts',(-6.67770007774188,-1.11873373341628,
-54.6444948773561));
#34584=CARTESIAN_POINT('Ctrl Pts',(-6.63300103649544,-1.33999486933738,
-54.6338151010255));
#34585=CARTESIAN_POINT('Ctrl Pts',(-6.58865774832616,-1.55949502050875,
-54.6232203234598));
#34586=CARTESIAN_POINT('Ctrl Pts',(-6.53345690463797,-1.77658548395082,
-54.6126255458941));
#34587=CARTESIAN_POINT('Ctrl Pts',(-6.46767094968983,-1.9903571253768,-54.6020307683284));
#34588=CARTESIAN_POINT('Ctrl Pts',(-6.41755664466207,-2.15320369731077,
-54.5939598979572));
#34589=CARTESIAN_POINT('Ctrl Pts',(-6.36119638138062,-2.31445365969866,
-54.5858890275861));
#34590=CARTESIAN_POINT('Ctrl Pts',(-6.29870566844256,-2.47357957266986,
-54.5778181572149));
#34591=CARTESIAN_POINT('Ctrl Pts',(-6.23629272032192,-2.6325074658556,-54.5697573304123));
#34592=CARTESIAN_POINT('Ctrl Pts',(-6.16776463673065,-2.78931622614659,
-54.5616965036098));
#34593=CARTESIAN_POINT('Ctrl Pts',(-6.093287415256,-2.94349069559984,-54.5536356768072));
#34594=CARTESIAN_POINT('Ctrl Pts',(-6.01888654315695,-3.09750711505818,
-54.5455831134586));
#34595=CARTESIAN_POINT('Ctrl Pts',(-5.93854883066954,-3.24889428475438,
-54.53753055011));
#34596=CARTESIAN_POINT('Ctrl Pts',(-5.85248932311385,-3.39715435664003,
-54.5294779867614));
#34597=CARTESIAN_POINT('Ctrl Pts',(-5.76649919452756,-3.54529490505545,
-54.521431915183));
#34598=CARTESIAN_POINT('Ctrl Pts',(-5.67479663819831,-3.69031305234391,
-54.5133858436046));
#34599=CARTESIAN_POINT('Ctrl Pts',(-5.5776437966822,-3.83173311666308,-54.5053397720262));
#34600=CARTESIAN_POINT('Ctrl Pts',(-5.48054802622102,-3.97307010577691,
-54.4972984269981));
#34601=CARTESIAN_POINT('Ctrl Pts',(-5.3780085549301,-4.11081291292901,-54.48925708197));
#34602=CARTESIAN_POINT('Ctrl Pts',(-5.27033218331351,-4.244512654891,-54.4812157369419));
#34603=CARTESIAN_POINT('Ctrl Pts',(-5.1605801467745,-4.38078971126618,-54.4730193798388));
#34604=CARTESIAN_POINT('Ctrl Pts',(-5.04549134299811,-4.51286589513378,
-54.4648230227356));
#34605=CARTESIAN_POINT('Ctrl Pts',(-4.92543570251534,-4.64029871240929,
-54.4566266656324));
#34606=CARTESIAN_POINT('Ctrl Pts',(-4.80768803261037,-4.76528173897328,
-54.4485878767281));
#34607=CARTESIAN_POINT('Ctrl Pts',(-4.68516304162269,-4.88579804282406,
-54.4405490878238));
#34608=CARTESIAN_POINT('Ctrl Pts',(-4.55824866500417,-5.00146559600161,
-54.4325102989195));
#34609=CARTESIAN_POINT('Ctrl Pts',(-4.43132070737851,-5.11714552667261,
-54.4244706497908));
#34610=CARTESIAN_POINT('Ctrl Pts',(-4.30000270485133,-5.22797542187798,
-54.4164310006621));
#34611=CARTESIAN_POINT('Ctrl Pts',(-4.16471727806585,-5.33361219004342,
-54.4083913515333));
#34612=CARTESIAN_POINT('Ctrl Pts',(-4.02939058746502,-5.43928117879758,
-54.400349250207));
#34613=CARTESIAN_POINT('Ctrl Pts',(-3.89009435806851,-5.53975365790169,
-54.3923071488807));
#34614=CARTESIAN_POINT('Ctrl Pts',(-3.7472817766384,-5.63472876778233,-54.3842650475544));
#34615=CARTESIAN_POINT('Ctrl Pts',(-3.5996498416032,-5.73290890787539,-54.3759515574636));
#34616=CARTESIAN_POINT('Ctrl Pts',(-3.44826044016032,-5.82521391636151,
-54.3676380673729));
#34617=CARTESIAN_POINT('Ctrl Pts',(-3.2936426797554,-5.91136252467176,-54.3593245772821));
#34618=CARTESIAN_POINT('Ctrl Pts',(-3.14380883632135,-5.99484567082402,
-54.3512683089117));
#34619=CARTESIAN_POINT('Ctrl Pts',(-2.99094379298023,-6.07254760376807,
-54.3432120405414));
#34620=CARTESIAN_POINT('Ctrl Pts',(-2.83554971402137,-6.14426129158855,
-54.335155772171));
#34621=CARTESIAN_POINT('Ctrl Pts',(-2.67271346758084,-6.21940950715334,
-54.3267136712201));
#34622=CARTESIAN_POINT('Ctrl Pts',(-2.50710043562913,-6.28798160598858,
-54.3182715702691));
#34623=CARTESIAN_POINT('Ctrl Pts',(-2.33930596094258,-6.34979815593366,
-54.3098294693182));
#34624=CARTESIAN_POINT('Ctrl Pts',(-2.17151148625601,-6.41161470587875,
-54.3013873683672));
#34625=CARTESIAN_POINT('Ctrl Pts',(-2.00153603392613,-6.46667564716504,
-54.2929452674163));
#34626=CARTESIAN_POINT('Ctrl Pts',(-1.82998604543771,-6.51486301264296,
-54.2845031664654));
#34627=CARTESIAN_POINT('Ctrl Pts',(-1.66063595065124,-6.56243244114074,
-54.2761693238995));
#34628=CARTESIAN_POINT('Ctrl Pts',(-1.48921323568788,-6.60345534162941,
-54.2678354813336));
#34629=CARTESIAN_POINT('Ctrl Pts',(-1.31625876710413,-6.6377520184187,-54.2595016387678));
#34630=CARTESIAN_POINT('Ctrl Pts',(-1.14350814726892,-6.6720082722302,-54.251177618691));
#34631=CARTESIAN_POINT('Ctrl Pts',(-0.969229708560848,-6.69955402796864,
-54.2428535986142));
#34632=CARTESIAN_POINT('Ctrl Pts',(-0.793979341825377,-6.72025935546795,
-54.2345295785374));
#34633=CARTESIAN_POINT('Ctrl Pts',(-0.618903397940909,-6.74094407540837,
-54.2262138431754));
#34634=CARTESIAN_POINT('Ctrl Pts',(-0.442857796587523,-6.75480189061367,
-54.2178981078135));
#34635=CARTESIAN_POINT('Ctrl Pts',(-0.266408712091897,-6.76175386997498,
-54.2095823724515));
#34636=CARTESIAN_POINT('Ctrl Pts',(-0.0901029134722441,-6.7687002039658,
-54.2012733899012));
#34637=CARTESIAN_POINT('Ctrl Pts',(0.0866053693430223,-6.7687518627516,
-54.1929644073508));
#34638=CARTESIAN_POINT('Ctrl Pts',(0.263144515717021,-6.76188168809896,
-54.1846554248005));
#34639=CARTESIAN_POINT('Ctrl Pts',(0.439572631856113,-6.75501583428463,
-54.1763516679936));
#34640=CARTESIAN_POINT('Ctrl Pts',(0.615831476951372,-6.74123683624038,
-54.1680479111866));
#34641=CARTESIAN_POINT('Ctrl Pts',(0.791348872924406,-6.72056961583773,
-54.1597441543797));
#34642=CARTESIAN_POINT('Ctrl Pts',(0.966795013057527,-6.69991078582932,
-54.1514437686983));
#34643=CARTESIAN_POINT('Ctrl Pts',(1.14149995897005,-6.67236934622123,-54.1431433830168));
#34644=CARTESIAN_POINT('Ctrl Pts',(1.31489580276888,-6.6380221472861,-54.1348429973354));
#34645=CARTESIAN_POINT('Ctrl Pts',(1.48825508189294,-6.60368219128212,-54.1265443619895));
#34646=CARTESIAN_POINT('Ctrl Pts',(1.66030546790751,-6.56253940267501,-54.1182457266435));
#34647=CARTESIAN_POINT('Ctrl Pts',(1.83048816281293,-6.51472194999923,-54.1099470912976));
#34648=CARTESIAN_POINT('Ctrl Pts',(2.00066321899095,-6.46690664363148,-54.1016488284397));
#34649=CARTESIAN_POINT('Ctrl Pts',(2.16897041636322,-6.41241736445312,-54.0933505655818));
#34650=CARTESIAN_POINT('Ctrl Pts',(2.33486487486542,-6.35143251685159,-54.0850523027239));
#34651=CARTESIAN_POINT('Ctrl Pts',(2.50077942248289,-6.29044028424368,-54.0767530349815));
#34652=CARTESIAN_POINT('Ctrl Pts',(2.66428032284196,-6.22295103640304,-54.0684537672391));
#34653=CARTESIAN_POINT('Ctrl Pts',(2.82484129446398,-6.14919187057056,-54.0601544994968));
#34654=CARTESIAN_POINT('Ctrl Pts',(2.98551500578896,-6.07538091390522,-54.0518494043297));
#34655=CARTESIAN_POINT('Ctrl Pts',(3.14324434711673,-5.99529138764948,-54.0435443091626));
#34656=CARTESIAN_POINT('Ctrl Pts',(3.29752552309412,-5.90919744335412,-54.0352392139955));
#34657=CARTESIAN_POINT('Ctrl Pts',(3.45186295802048,-5.82307210472443,-54.0269310903583));
#34658=CARTESIAN_POINT('Ctrl Pts',(3.60274942141719,-5.73093815994321,-54.0186229667211));
#34659=CARTESIAN_POINT('Ctrl Pts',(3.74970869170949,-5.63311403464534,-54.0103148430839));
#34660=CARTESIAN_POINT('Ctrl Pts',(3.89682417889221,-5.53518592284406,-54.0019978879573));
#34661=CARTESIAN_POINT('Ctrl Pts',(4.04000384669348,-5.43155574446703,-53.9936809328307));
#34662=CARTESIAN_POINT('Ctrl Pts',(4.17880237305546,-5.32258393329275,-53.9853639777042));
#34663=CARTESIAN_POINT('Ctrl Pts',(4.2810948026693,-5.2422733448693,-53.9792345066702));
#34664=CARTESIAN_POINT('Ctrl Pts',(4.38100828633158,-5.1590623345053,-53.9731050356363));
#34665=CARTESIAN_POINT('Ctrl Pts',(4.47837707016747,-5.07310829939577,-53.9669755646024));
#34666=CARTESIAN_POINT('Ctrl Pts',(4.61262452482687,-4.9545989581411,-53.9585245410577));
#34667=CARTESIAN_POINT('Ctrl Pts',(4.74227860219775,-4.83065731156955,-53.950073517513));
#34668=CARTESIAN_POINT('Ctrl Pts',(4.86689164827471,-4.70166509695809,-53.9416224939683));
#34669=CARTESIAN_POINT('Ctrl Pts',(4.9913949762588,-4.57278645616757,-53.9331789112993));
#34670=CARTESIAN_POINT('Ctrl Pts',(5.1108658904331,-4.43886634810276,-53.9247353286303));
#34671=CARTESIAN_POINT('Ctrl Pts',(5.22489176344625,-4.30032499472674,-53.9162917459613));
#34672=CARTESIAN_POINT('Ctrl Pts',(5.33883274063569,-4.16188678971523,-53.9078544498034));
#34673=CARTESIAN_POINT('Ctrl Pts',(5.4473365481612,-4.018834453297,-53.8994171536454));
#34674=CARTESIAN_POINT('Ctrl Pts',(5.55002895738425,-3.87162337685321,-53.8909798574874));
#34675=CARTESIAN_POINT('Ctrl Pts',(5.65264810339016,-3.72451732430692,-53.882548580698));
#34676=CARTESIAN_POINT('Ctrl Pts',(5.74946393177135,-3.57325872101615,-53.8741173039086));
#34677=CARTESIAN_POINT('Ctrl Pts',(5.84014376584591,-3.41833435963353,-53.8656860271192));
#34678=CARTESIAN_POINT('Ctrl Pts',(5.93078473125402,-3.26347640445234,-53.8572583642809));
#34679=CARTESIAN_POINT('Ctrl Pts',(6.01529477845574,-3.1049561091485,-53.8488307014425));
#34680=CARTESIAN_POINT('Ctrl Pts',(6.09338532758643,-2.94328799976394,-53.8404030386042));
#34681=CARTESIAN_POINT('Ctrl Pts',(6.17145183734821,-2.7816696582369,-53.8319779701349));
#34682=CARTESIAN_POINT('Ctrl Pts',(6.24310264602628,-2.61690573324335,-53.8235529016655));
#34683=CARTESIAN_POINT('Ctrl Pts',(6.30809562696466,-2.44953435596836,-53.8151278331961));
#34684=CARTESIAN_POINT('Ctrl Pts',(6.3258796950885,-2.40373642621558,-53.8128224766877));
#34685=CARTESIAN_POINT('Ctrl Pts',(6.34316554090043,-2.35774339158578,-53.8105171201793));
#34686=CARTESIAN_POINT('Ctrl Pts',(6.35994882873505,-2.3115665458454,-53.8082117636709));
#34687=CARTESIAN_POINT('Ctrl Pts',(6.42269615910115,-2.13892612976682,-53.7995927750752));
#34688=CARTESIAN_POINT('Ctrl Pts',(6.47838710060114,-1.96379218154052,-53.7909737864795));
#34689=CARTESIAN_POINT('Ctrl Pts',(6.5268512827126,-1.7867572116415,-53.7823547978838));
#34690=CARTESIAN_POINT('Ctrl Pts',(6.57534449920554,-1.6096161819551,-53.7737306457427));
#34691=CARTESIAN_POINT('Ctrl Pts',(6.61660223568956,-1.43057215109361,-53.7651064936017));
#34692=CARTESIAN_POINT('Ctrl Pts',(6.65050486452753,-1.25022959767221,-53.7564823414606));
#34693=CARTESIAN_POINT('Ctrl Pts',(6.685568667084,-1.06371026561931,-53.7475628099005));
#34694=CARTESIAN_POINT('Ctrl Pts',(6.71276455494065,-0.875802239944836,
-53.7386432783404));
#34695=CARTESIAN_POINT('Ctrl Pts',(6.73201832590055,-0.687181387800304,
-53.7297237467803));
#34696=CARTESIAN_POINT('Ctrl Pts',(6.7506691682756,-0.504467165774861,-53.7210835288441));
#34697=CARTESIAN_POINT('Ctrl Pts',(6.76186780567942,-0.321084392675276,
-53.7124433109079));
#34698=CARTESIAN_POINT('Ctrl Pts',(6.7655998777319,-0.137649171570764,-53.7038030929718));
#34699=CARTESIAN_POINT('Ctrl Pts',(6.76951292066569,0.0546809564807878,
-53.6947439045997));
#34700=CARTESIAN_POINT('Ctrl Pts',(6.7652172860921,0.247068357662824,-53.6856847162276));
#34701=CARTESIAN_POINT('Ctrl Pts',(6.75275780520025,0.438806363111455,-53.6766255278555));
#34702=CARTESIAN_POINT('Ctrl Pts',(6.74029832430841,0.630544368560078,-53.6675663394835));
#34703=CARTESIAN_POINT('Ctrl Pts',(6.71967507109066,0.821632601412444,-53.6585071511114));
#34704=CARTESIAN_POINT('Ctrl Pts',(6.69099487965136,1.01137358106649,-53.6494479627393));
#34705=CARTESIAN_POINT('Ctrl Pts',(6.66236437472461,1.20078584716971,-53.6404044688049));
#34706=CARTESIAN_POINT('Ctrl Pts',(6.6256792856349,1.38903014656108,-53.6313609748705));
#34707=CARTESIAN_POINT('Ctrl Pts',(6.58105340602497,1.57544440303274,-53.6223174809361));
#34708=CARTESIAN_POINT('Ctrl Pts',(6.53646834555174,1.76168814703307,-53.6132822590541));
#34709=CARTESIAN_POINT('Ctrl Pts',(6.48395705137221,1.94610495878242,-53.6042470371721));
#34710=CARTESIAN_POINT('Ctrl Pts',(6.42368419507574,2.12804378759793,-53.5952118152901));
#34711=CARTESIAN_POINT('Ctrl Pts',(6.363517526431,2.30966207980415,-53.5861925115021));
#34712=CARTESIAN_POINT('Ctrl Pts',(6.29561667608616,2.48881088105503,-53.5771732077142));
#34713=CARTESIAN_POINT('Ctrl Pts',(6.22019577440718,2.66485525461462,-53.5681539039262));
#34714=CARTESIAN_POINT('Ctrl Pts',(6.1448694935097,2.84067876822908,-53.5591459154839));
#34715=CARTESIAN_POINT('Ctrl Pts',(6.06204208263578,3.01340540847851,-53.5501379270417));
#34716=CARTESIAN_POINT('Ctrl Pts',(5.97197621739012,3.18241874349162,-53.5411299385994));
#34717=CARTESIAN_POINT('Ctrl Pts',(5.88211376902373,3.35105035602785,-53.5321422950113));
#34718=CARTESIAN_POINT('Ctrl Pts',(5.78504561075211,3.51598519407826,-53.5231546514232));
#34719=CARTESIAN_POINT('Ctrl Pts',(5.68108067246096,3.67663044008921,-53.5141670078351));
#34720=CARTESIAN_POINT('Ctrl Pts',(5.59053440879704,3.81654132774757,-53.5063393924927));
#34721=CARTESIAN_POINT('Ctrl Pts',(5.49475756233667,3.95319867699258,-53.4985117771502));
#34722=CARTESIAN_POINT('Ctrl Pts',(5.39398321700737,4.086224914838,-53.4906841618078));
#34723=CARTESIAN_POINT('Ctrl Pts',(5.2894070098332,4.2242697650731,-53.4825612380512));
#34724=CARTESIAN_POINT('Ctrl Pts',(5.17949452655395,4.35834164200837,-53.4744383142946));
#34725=CARTESIAN_POINT('Ctrl Pts',(5.06459006469176,4.4880080744831,-53.466315390538));
#34726=CARTESIAN_POINT('Ctrl Pts',(4.94969501309805,4.61766388773624,-53.4581931320201));
#34727=CARTESIAN_POINT('Ctrl Pts',(4.82980904049795,4.74291470176019,-53.4500708735022));
#34728=CARTESIAN_POINT('Ctrl Pts',(4.705315673836,4.8633623563902,-53.4419486149843));
#34729=CARTESIAN_POINT('Ctrl Pts',(4.58076338501893,4.98386701835788,-53.4338225122376));
#34730=CARTESIAN_POINT('Ctrl Pts',(4.45159960678405,5.09956372221323,-53.425696409491));
#34731=CARTESIAN_POINT('Ctrl Pts',(4.31824396242724,5.21009194553808,-53.4175703067444));
#34732=CARTESIAN_POINT('Ctrl Pts',(4.18485735873682,5.32064582867023,-53.409442317473));
#34733=CARTESIAN_POINT('Ctrl Pts',(4.04727723757417,5.42602861391727,-53.4013143282016));
#34734=CARTESIAN_POINT('Ctrl Pts',(3.90595485003789,5.52592125436705,-53.3931863389302));
#34735=CARTESIAN_POINT('Ctrl Pts',(3.76449776475138,5.62590910488345,-53.3850506026776));
#34736=CARTESIAN_POINT('Ctrl Pts',(3.61929159131145,5.72039615221774,-53.3769148664251));
#34737=CARTESIAN_POINT('Ctrl Pts',(3.47081568271612,5.80910728912901,-53.3687791301726));
#34738=CARTESIAN_POINT('Ctrl Pts',(3.34901356465853,5.88188141439495,-53.3621049840644));
#34739=CARTESIAN_POINT('Ctrl Pts',(3.22501158011935,5.9507692992674,-53.3554308379562));
#34740=CARTESIAN_POINT('Ctrl Pts',(3.0990855038472,6.01564277861013,-53.3487566918479));
#34741=CARTESIAN_POINT('Origin',(0.,0.,-63.6971797838103));
#34742=CARTESIAN_POINT('',(3.0990855038472,6.01564277861013,-50.9542788176482));
#34743=CARTESIAN_POINT('',(3.09908550384718,6.01564277861014,-51.3484212393497));
#34744=CARTESIAN_POINT('',(3.09908550384721,6.01564277861012,-63.6971797838103));
#34745=CARTESIAN_POINT('',(-6.76699979006582,0.00168560055385441,-52.3028202161503));
#34746=CARTESIAN_POINT('Ctrl Pts',(-6.76699979006581,0.00168560055384907,
-52.3028202161503));
#34747=CARTESIAN_POINT('Ctrl Pts',(-6.76704222219873,-0.16866213331645,
-52.2948235459384));
#34748=CARTESIAN_POINT('Ctrl Pts',(-6.76064800700029,-0.339088473983994,
-52.2868268757265));
#34749=CARTESIAN_POINT('Ctrl Pts',(-6.74782562800835,-0.509056277825701,
-52.2788302055146));
#34750=CARTESIAN_POINT('Ctrl Pts',(-6.73500408146496,-0.67901304709633,
-52.2708340544588));
#34751=CARTESIAN_POINT('Ctrl Pts',(-6.7157552265512,-0.848510960915059,
-52.262837903403));
#34752=CARTESIAN_POINT('Ctrl Pts',(-6.69013956762023,-1.01701601057322,
-52.2548417523472));
#34753=CARTESIAN_POINT('Ctrl Pts',(-6.68070580473756,-1.07907323452712,
-52.2518969210924));
#34754=CARTESIAN_POINT('Ctrl Pts',(-6.67040901238627,-1.14099585344223,
-52.2489520898375));
#34755=CARTESIAN_POINT('Ctrl Pts',(-6.65925397533337,-1.20275745352367,
-52.2460072585826));
#34756=CARTESIAN_POINT('Ctrl Pts',(-6.62660519921238,-1.38352248768456,
-52.2373882700576));
#34757=CARTESIAN_POINT('Ctrl Pts',(-6.58660376208147,-1.56289156319099,
-52.2287692815326));
#34758=CARTESIAN_POINT('Ctrl Pts',(-6.53940058769381,-1.74026692023662,
-52.2201502930077));
#34759=CARTESIAN_POINT('Ctrl Pts',(-6.49216913439221,-1.91774854095037,
-52.2115261409394));
#34760=CARTESIAN_POINT('Ctrl Pts',(-6.4377274116605,-2.09323376559209,-52.2029019888711));
#34761=CARTESIAN_POINT('Ctrl Pts',(-6.37627621605827,-2.2661400257993,-52.1942778368028));
#34762=CARTESIAN_POINT('Ctrl Pts',(-6.31272030048007,-2.44496837191978,
-52.1853583052069));
#34763=CARTESIAN_POINT('Ctrl Pts',(-6.24166638578727,-2.62103763086395,
-52.1764387736109));
#34764=CARTESIAN_POINT('Ctrl Pts',(-6.16339044666578,-2.79372640069656,
-52.1675192420149));
#34765=CARTESIAN_POINT('Ctrl Pts',(-6.08756570632921,-2.96100744872433,
-52.1588790241551));
#34766=CARTESIAN_POINT('Ctrl Pts',(-6.00496458775122,-3.12511627111526,
-52.1502388062953));
#34767=CARTESIAN_POINT('Ctrl Pts',(-5.91588470560768,-3.28551322474239,
-52.1415985884355));
#34768=CARTESIAN_POINT('Ctrl Pts',(-5.82248527358039,-3.45368794620801,
-52.1325393999714));
#34769=CARTESIAN_POINT('Ctrl Pts',(-5.7219633396515,-3.61778153595023,-52.1234802115074));
#34770=CARTESIAN_POINT('Ctrl Pts',(-5.61471324293254,-3.77720587202206,
-52.1144210230433));
#34771=CARTESIAN_POINT('Ctrl Pts',(-5.5074631462136,-3.93663020809387,-52.1053618345792));
#34772=CARTESIAN_POINT('Ctrl Pts',(-5.39348514028475,-4.09138500205531,
-52.0963026461151));
#34773=CARTESIAN_POINT('Ctrl Pts',(-5.27322252168265,-4.24092127217883,
-52.0872434576511));
#34774=CARTESIAN_POINT('Ctrl Pts',(-5.15316824962704,-4.39019848120908,
-52.0781999635952));
#34775=CARTESIAN_POINT('Ctrl Pts',(-5.02674118180533,-4.53441328467973,
-52.0691564695394));
#34776=CARTESIAN_POINT('Ctrl Pts',(-4.89437281339686,-4.67305079829887,
-52.0601129754835));
#34777=CARTESIAN_POINT('Ctrl Pts',(-4.76212552185087,-4.81156150069134,
-52.0510777534786));
#34778=CARTESIAN_POINT('Ctrl Pts',(-4.6239479439629,-4.94450492639516,-52.0420425314737));
#34779=CARTESIAN_POINT('Ctrl Pts',(-4.48030999396894,-5.07140132093113,
-52.0330073094688));
#34780=CARTESIAN_POINT('Ctrl Pts',(-4.33692510277304,-5.19807415164515,
-52.023988005558));
#34781=CARTESIAN_POINT('Ctrl Pts',(-4.18809922758639,-5.31872106758195,
-52.0149687016473));
#34782=CARTESIAN_POINT('Ctrl Pts',(-4.03433691479374,-5.43290112720014,
-52.0059493977366));
#34783=CARTESIAN_POINT('Ctrl Pts',(-3.88076750756243,-5.54693793995833,
-51.9969414091727));
#34784=CARTESIAN_POINT('Ctrl Pts',(-3.72227421261627,-5.65452394588214,
-51.9879334206087));
#34785=CARTESIAN_POINT('Ctrl Pts',(-3.55939421592283,-5.75525862282966,
-51.9789254320447));
#34786=CARTESIAN_POINT('Ctrl Pts',(-3.39688208940721,-5.8557657869808,-51.9699377883385));
#34787=CARTESIAN_POINT('Ctrl Pts',(-3.23000323957779,-5.94945238460827,
-51.9609501446322));
#34788=CARTESIAN_POINT('Ctrl Pts',(-3.0593229411224,-6.03596157558364,-51.9519625009259));
#34789=CARTESIAN_POINT('Ctrl Pts',(-2.9106722310024,-6.11130508497971,-51.9441348861905));
#34790=CARTESIAN_POINT('Ctrl Pts',(-2.75913860364769,-6.18120494807919,
-51.936307271455));
#34791=CARTESIAN_POINT('Ctrl Pts',(-2.60511347837555,-6.24545216655976,
-51.9284796567195));
#34792=CARTESIAN_POINT('Ctrl Pts',(-2.44527289609821,-6.31212513821611,
-51.9203564982741));
#34793=CARTESIAN_POINT('Ctrl Pts',(-2.28281992949351,-6.37267921076693,
-51.9122333398287));
#34794=CARTESIAN_POINT('Ctrl Pts',(-2.11826977509098,-6.42691389081385,
-51.9041101813833));
#34795=CARTESIAN_POINT('Ctrl Pts',(-1.95373122233573,-6.48114474703192,
-51.8959875956631));
#34796=CARTESIAN_POINT('Ctrl Pts',(-1.78709612394014,-6.52905698366225,
-51.8878650099429));
#34797=CARTESIAN_POINT('Ctrl Pts',(-1.61889633192939,-6.57049949900809,
-51.8797424242227));
#34798=CARTESIAN_POINT('Ctrl Pts',(-1.45067632898252,-6.61194699409868,
-51.8716188624902));
#34799=CARTESIAN_POINT('Ctrl Pts',(-1.28089161371526,-6.64692313351184,
-51.8634953007577));
#34800=CARTESIAN_POINT('Ctrl Pts',(-1.11008571625013,-6.67532761013101,
-51.8553717390253));
#34801=CARTESIAN_POINT('Ctrl Pts',(-0.939155406957264,-6.70375277604081,
-51.847242260242));
#34802=CARTESIAN_POINT('Ctrl Pts',(-0.767202791315418,-6.72559665880027,
-51.8391127814588));
#34803=CARTESIAN_POINT('Ctrl Pts',(-0.594778673665024,-6.74081058399903,
-51.8309833026756));
#34804=CARTESIAN_POINT('Ctrl Pts',(-0.422284261736473,-6.75603071164733,
-51.8228505096469));
#34805=CARTESIAN_POINT('Ctrl Pts',(-0.249318329956004,-6.76461547588664,
-51.8147177166183));
#34806=CARTESIAN_POINT('Ctrl Pts',(-0.0764329557722841,-6.7665683328606,
-51.8065849235896));
#34807=CARTESIAN_POINT('Ctrl Pts',(0.0966404050276211,-6.76852331327026,
-51.7984432873824));
#34808=CARTESIAN_POINT('Ctrl Pts',(0.269632667839708,-6.76383199327735,
-51.7903016511751));
#34809=CARTESIAN_POINT('Ctrl Pts',(0.441994851095807,-6.75254985554382,
-51.7821600149679));
#34810=CARTESIAN_POINT('Ctrl Pts',(0.529811042273336,-6.74680175961359,
-51.7780119619079));
#34811=CARTESIAN_POINT('Ctrl Pts',(0.617463792326182,-6.7393436725938,-51.773863908848));
#34812=CARTESIAN_POINT('Ctrl Pts',(0.704881448879159,-6.73018804663183,
-51.769715855788));
#34813=CARTESIAN_POINT('Ctrl Pts',(0.882764304366164,-6.71155761252841,
-51.76127514081));
#34814=CARTESIAN_POINT('Ctrl Pts',(1.06003951795542,-6.68585678030588,-51.7528344258319));
#34815=CARTESIAN_POINT('Ctrl Pts',(1.2361229175544,-6.65314129811601,-51.7443937108538));
#34816=CARTESIAN_POINT('Ctrl Pts',(1.41207322502415,-6.62045054382891,-51.7359593757658));
#34817=CARTESIAN_POINT('Ctrl Pts',(1.58683318762128,-6.58075576948503,-51.7275250406778));
#34818=CARTESIAN_POINT('Ctrl Pts',(1.75982538832982,-6.53416433850495,-51.7190907055898));
#34819=CARTESIAN_POINT('Ctrl Pts',(1.93271339830978,-6.48760096887746,-51.7106614503811));
#34820=CARTESIAN_POINT('Ctrl Pts',(2.10383544789739,-6.43414931024615,-51.7022321951725));
#34821=CARTESIAN_POINT('Ctrl Pts',(2.27262553283553,-6.37396753894339,-51.6938029399639));
#34822=CARTESIAN_POINT('Ctrl Pts',(2.44133984904713,-6.31381278283038,-51.6853774685909));
#34823=CARTESIAN_POINT('Ctrl Pts',(2.60772397429615,-6.24693404959369,-51.6769519972179));
#34824=CARTESIAN_POINT('Ctrl Pts',(2.77122788126819,-6.17353910087899,-51.6685265258449));
#34825=CARTESIAN_POINT('Ctrl Pts',(2.93468345174203,-6.10016584984035,-51.6601035452856));
#34826=CARTESIAN_POINT('Ctrl Pts',(3.09526019812638,-6.02028036136421,-51.6516805647264));
#34827=CARTESIAN_POINT('Ctrl Pts',(3.25242850190691,-5.9341383401454,-51.6432575841671));
#34828=CARTESIAN_POINT('Ctrl Pts',(3.40959940806831,-5.84799489259352,-51.6348344641408));
#34829=CARTESIAN_POINT('Ctrl Pts',(3.5633614633841,-5.75559485972933,-51.6264113441145));
#34830=CARTESIAN_POINT('Ctrl Pts',(3.71320948120089,-5.65723999391221,-51.6179882240881));
#34831=CARTESIAN_POINT('Ctrl Pts',(3.86306268101168,-5.55888172682004,-51.6095648127763));
#34832=CARTESIAN_POINT('Ctrl Pts',(4.00900129454074,-5.45456839904279,-51.6011414014645));
#34833=CARTESIAN_POINT('Ctrl Pts',(4.15054884657595,-5.34464528965086,-51.5927179901526));
#34834=CARTESIAN_POINT('Ctrl Pts',(4.29212103445023,-5.23470304853962,-51.5842931127765));
#34835=CARTESIAN_POINT('Ctrl Pts',(4.42930037375532,-5.11914928378067,-51.5758682354004));
#34836=CARTESIAN_POINT('Ctrl Pts',(4.56164294226869,-4.99837000103537,-51.5674433580243));
#34837=CARTESIAN_POINT('Ctrl Pts',(4.6940270073443,-4.87755284744411,-51.5590158389929));
#34838=CARTESIAN_POINT('Ctrl Pts',(4.82157103172609,-4.7515071338917,-51.5505883199615));
#34839=CARTESIAN_POINT('Ctrl Pts',(4.94386721032279,-4.62065644759434,-51.5421608009301));
#34840=CARTESIAN_POINT('Ctrl Pts',(5.06627305940608,-4.4896884194585,-51.5337257244254));
#34841=CARTESIAN_POINT('Ctrl Pts',(5.18342143138052,-4.35390705262337,-51.5252906479206));
#34842=CARTESIAN_POINT('Ctrl Pts',(5.29494341274326,-4.21377066958404,-51.5168555714158));
#34843=CARTESIAN_POINT('Ctrl Pts',(5.40651929341353,-4.07356655770854,-51.5084164181831));
#34844=CARTESIAN_POINT('Ctrl Pts',(5.51246315903988,-3.9290034976198,-51.4999772649503));
#34845=CARTESIAN_POINT('Ctrl Pts',(5.61244856850397,-3.78057007154976,-51.4915381117176));
#34846=CARTESIAN_POINT('Ctrl Pts',(5.71254508979103,-3.63197169432685,-51.4830895802195));
#34847=CARTESIAN_POINT('Ctrl Pts',(5.80666974468458,-3.47949463808175,-51.4746410487214));
#34848=CARTESIAN_POINT('Ctrl Pts',(5.89454069013699,-3.32365447246241,-51.4661925172233));
#34849=CARTESIAN_POINT('Ctrl Pts',(5.94309223848076,-3.23754772470849,-51.4615244294572));
#34850=CARTESIAN_POINT('Ctrl Pts',(5.98973540072815,-3.15041466906316,-51.4568563416911));
#34851=CARTESIAN_POINT('Ctrl Pts',(6.03442885626921,-3.06234507830608,-51.452188253925));
#34852=CARTESIAN_POINT('Ctrl Pts',(6.11332813070659,-2.90687205151481,-51.4439474783282));
#34853=CARTESIAN_POINT('Ctrl Pts',(6.18632401263804,-2.74813324297844,-51.4357067027315));
#34854=CARTESIAN_POINT('Ctrl Pts',(6.25313627486011,-2.58661472353897,-51.4274659271348));
#34855=CARTESIAN_POINT('Ctrl Pts',(6.31987453525838,-2.42527510337069,-51.4192342790904));
#34856=CARTESIAN_POINT('Ctrl Pts',(6.38044267881536,-2.26116222869414,-51.4110026310461));
#34857=CARTESIAN_POINT('Ctrl Pts',(6.43460616171242,-2.09478699242967,-51.4027709830017));
#34858=CARTESIAN_POINT('Ctrl Pts',(6.48871930511851,-1.9285663851561,-51.3945469854435));
#34859=CARTESIAN_POINT('Ctrl Pts',(6.53643953293929,-1.76008794008611,-51.3863229878852));
#34860=CARTESIAN_POINT('Ctrl Pts',(6.57758021521458,-1.58988286122523,-51.378098990327));
#34861=CARTESIAN_POINT('Ctrl Pts',(6.61868454953738,-1.41982815921224,-51.3698822587025));
#34862=CARTESIAN_POINT('Ctrl Pts',(6.65322084107363,-1.2480502083729,-51.361665527078));
#34863=CARTESIAN_POINT('Ctrl Pts',(6.68105219721329,-1.07509559487122,-51.3534487954535));
#34864=CARTESIAN_POINT('Ctrl Pts',(6.70886929431887,-0.902229592420915,
-51.3452362735648));
#34865=CARTESIAN_POINT('Ctrl Pts',(6.7299882411787,-0.72818847834672,-51.3370237516761));
#34866=CARTESIAN_POINT('Ctrl Pts',(6.74432308701853,-0.553529672112451,
-51.3288112297874));
#34867=CARTESIAN_POINT('Ctrl Pts',(6.7586531392169,-0.378929272623817,-51.3206014542056));
#34868=CARTESIAN_POINT('Ctrl Pts',(6.76620358071624,-0.203711946670291,
-51.3123916786238));
#34869=CARTESIAN_POINT('Ctrl Pts',(6.76694023251375,-0.0284409842788165,
-51.3041819030419));
#34870=CARTESIAN_POINT('Ctrl Pts',(6.76726198288057,0.0481128185252991,
-51.3005960863591));
#34871=CARTESIAN_POINT('Ctrl Pts',(6.76628452514981,0.124676802548317,-51.2970102696763));
#34872=CARTESIAN_POINT('Ctrl Pts',(6.76400813024382,0.201203911481814,-51.2934244529935));
#34873=CARTESIAN_POINT('Ctrl Pts',(6.75838432366806,0.390263225096315,-51.2845657354717));
#34874=CARTESIAN_POINT('Ctrl Pts',(6.74483520472732,0.578901465519504,-51.2757070179499));
#34875=CARTESIAN_POINT('Ctrl Pts',(6.72345224154194,0.766471757930234,-51.2668483004281));
#34876=CARTESIAN_POINT('Ctrl Pts',(6.70202927426651,0.954392964234585,-51.2579730096685));
#34877=CARTESIAN_POINT('Ctrl Pts',(6.67274320337633,1.1412419720629,-51.2490977189089));
#34878=CARTESIAN_POINT('Ctrl Pts',(6.63573668356482,1.3263814181419,-51.2402224281493));
#34879=CARTESIAN_POINT('Ctrl Pts',(6.5986250569168,1.51204670187304,-51.2313219295685));
#34880=CARTESIAN_POINT('Ctrl Pts',(6.55374915226288,1.69599245141979,-51.2224214309877));
#34881=CARTESIAN_POINT('Ctrl Pts',(6.50130249978103,1.87759282229693,-51.2135209324069));
#34882=CARTESIAN_POINT('Ctrl Pts',(6.4487848501955,2.05943902583927,-51.2046083852093));
#34883=CARTESIAN_POINT('Ctrl Pts',(6.38867605897881,2.23893326127338,-51.1956958380116));
#34884=CARTESIAN_POINT('Ctrl Pts',(6.32121859672582,2.41546775023134,-51.186783290814));
#34885=CARTESIAN_POINT('Ctrl Pts',(6.25361218180803,2.59239204458193,-51.1778510638417));
#34886=CARTESIAN_POINT('Ctrl Pts',(6.17862473295434,2.76634327730635,-51.1689188368694));
#34887=CARTESIAN_POINT('Ctrl Pts',(6.09654684536151,2.93673382558118,-51.1599866098971));
#34888=CARTESIAN_POINT('Ctrl Pts',(6.01897376357476,3.09777256968948,-51.151544623952));
#34889=CARTESIAN_POINT('Ctrl Pts',(5.93506767619839,3.25563080195445,-51.143102638007));
#34890=CARTESIAN_POINT('Ctrl Pts',(5.84511032528628,3.40983493518847,-51.1346606520619));
#34891=CARTESIAN_POINT('Ctrl Pts',(5.75748275492568,3.56004537822453,-51.126437302776));
#34892=CARTESIAN_POINT('Ctrl Pts',(5.66394502973031,3.70707493802655,-51.1182139534901));
#34893=CARTESIAN_POINT('Ctrl Pts',(5.56475447860908,3.85042810513327,-51.1099906042042));
#34894=CARTESIAN_POINT('Ctrl Pts',(5.46566367724758,3.99363711088779,-51.1017755246286));
#34895=CARTESIAN_POINT('Ctrl Pts',(5.3609315701396,4.13317679234455,-51.0935604450529));
#34896=CARTESIAN_POINT('Ctrl Pts',(5.25086098479114,4.26857680244812,-51.0853453654773));
#34897=CARTESIAN_POINT('Ctrl Pts',(5.14088108712865,4.40386525583054,-51.0771370543453));
#34898=CARTESIAN_POINT('Ctrl Pts',(5.02557169463353,4.53502055289682,-51.0689287432133));
#34899=CARTESIAN_POINT('Ctrl Pts',(4.90527851016717,4.66160184246705,-51.0607204320813));
#34900=CARTESIAN_POINT('Ctrl Pts',(4.78506257820663,4.78810184129871,-51.0525173923419));
#34901=CARTESIAN_POINT('Ctrl Pts',(4.65986947517496,4.91003342419929,-51.0443143526025));
#34902=CARTESIAN_POINT('Ctrl Pts',(4.53008473553831,5.02698928672449,-51.0361113128631));
#34903=CARTESIAN_POINT('Ctrl Pts',(4.40035875462369,5.14389219867141,-51.0279119869666));
#34904=CARTESIAN_POINT('Ctrl Pts',(4.26604554444756,5.25582363856319,-51.0197126610701));
#34905=CARTESIAN_POINT('Ctrl Pts',(4.12756704767444,5.36241356731763,-51.0115133351736));
#34906=CARTESIAN_POINT('Ctrl Pts',(3.98912446940028,5.46897584881755,-51.0033161360151));
#34907=CARTESIAN_POINT('Ctrl Pts',(3.84651904166094,5.57019916198439,-50.9951189368566));
#34908=CARTESIAN_POINT('Ctrl Pts',(3.70020534501819,5.66575408967763,-50.9869217376981));
#34909=CARTESIAN_POINT('Ctrl Pts',(3.55388787310107,5.76131148293684,-50.9787243270305));
#34910=CARTESIAN_POINT('Ctrl Pts',(3.40386223999461,5.85120000058006,-50.9705269163629));
#34911=CARTESIAN_POINT('Ctrl Pts',(3.25061171475611,5.93513373732137,-50.9623295056953));
#34912=CARTESIAN_POINT('Ctrl Pts',(3.20044253240569,5.96261088258645,-50.9596459430129));
#34913=CARTESIAN_POINT('Ctrl Pts',(3.14992794992446,5.98945021807804,-50.9569623803306));
#34914=CARTESIAN_POINT('Ctrl Pts',(3.0990855038472,6.01564277861013,-50.9542788176482));
#34915=CARTESIAN_POINT('Ctrl Pts',(3.09908550384721,6.01564277861012,-52.953975806663));
#34916=CARTESIAN_POINT('Ctrl Pts',(2.94671772071282,6.09413826202614,-52.9459325567485));
#34917=CARTESIAN_POINT('Ctrl Pts',(2.79124015761376,6.16690566284332,-52.9378893068339));
#34918=CARTESIAN_POINT('Ctrl Pts',(2.63313311030458,6.23369064226143,-52.9298460569193));
#34919=CARTESIAN_POINT('Ctrl Pts',(2.47509990216388,6.30044443175201,-52.9218065633641));
#34920=CARTESIAN_POINT('Ctrl Pts',(2.31443999788565,6.36122121755229,-52.9137670698089));
#34921=CARTESIAN_POINT('Ctrl Pts',(2.15165623983891,6.41581362147953,-52.9057275762537));
#34922=CARTESIAN_POINT('Ctrl Pts',(1.98888382565985,6.4704022210407,-52.8976886429445));
#34923=CARTESIAN_POINT('Ctrl Pts',(1.8239882027693,6.51880716831367,-52.8896497096353));
#34924=CARTESIAN_POINT('Ctrl Pts',(1.65749021622967,6.56087000199691,-52.8816107763261));
#34925=CARTESIAN_POINT('Ctrl Pts',(1.49098986403336,6.60293343332236,-52.8735717287971));
#34926=CARTESIAN_POINT('Ctrl Pts',(1.32288746473816,6.63865447925112,-52.8655326812682));
#34927=CARTESIAN_POINT('Ctrl Pts',(1.15371665645136,6.66792523028166,-52.8574936337392));
#34928=CARTESIAN_POINT('Ctrl Pts',(0.98450995214953,6.69720219221424,-52.8494528804209));
#34929=CARTESIAN_POINT('Ctrl Pts',(0.814234755517338,6.72002607104307,-52.8414121271026));
#34930=CARTESIAN_POINT('Ctrl Pts',(0.643432323578413,6.7363405380796,-52.8333713737842));
#34931=CARTESIAN_POINT('Ctrl Pts',(0.472559823838546,6.75266169775402,-52.8253273219303));
#34932=CARTESIAN_POINT('Ctrl Pts',(0.301160029581996,6.7624680949701,-52.8172832700763));
#34933=CARTESIAN_POINT('Ctrl Pts',(0.129776564540633,6.76575546729972,-52.8092392182224));
#34934=CARTESIAN_POINT('Ctrl Pts',(-0.04181352272107,6.76904680292982,-52.8011854683509));
#34935=CARTESIAN_POINT('Ctrl Pts',(-0.21338686816161,6.7658034131288,-52.7931317184794));
#34936=CARTESIAN_POINT('Ctrl Pts',(-0.384401786763039,6.75607313950444,
-52.7850779686079));
#34937=CARTESIAN_POINT('Ctrl Pts',(-0.555530896877247,6.74633636870034,
-52.7770188410191));
#34938=CARTESIAN_POINT('Ctrl Pts',(-0.726100467547313,6.73010412384681,
-52.7689597134303));
#34939=CARTESIAN_POINT('Ctrl Pts',(-0.895577197395139,6.70747571620695,
-52.7609005858415));
#34940=CARTESIAN_POINT('Ctrl Pts',(-1.06531579411278,6.68481234429628,-52.7528290056965));
#34941=CARTESIAN_POINT('Ctrl Pts',(-1.23395781225078,6.65573313888357,-52.7447574255514));
#34942=CARTESIAN_POINT('Ctrl Pts',(-1.40098241985301,6.620387999148,-52.7366858454064));
#34943=CARTESIAN_POINT('Ctrl Pts',(-1.5002200628672,6.59938769021317,-52.7318901173966));
#34944=CARTESIAN_POINT('Ctrl Pts',(-1.59888704844799,6.57617636648305,-52.7270943893869));
#34945=CARTESIAN_POINT('Ctrl Pts',(-1.69687740114419,6.55079354624203,-52.7222986613771));
#34946=CARTESIAN_POINT('Ctrl Pts',(-1.8671614921318,6.50668419922451,-52.7139648186845));
#34947=CARTESIAN_POINT('Ctrl Pts',(-2.03594244851621,6.45587460051241,-52.7056309759919));
#34948=CARTESIAN_POINT('Ctrl Pts',(-2.20266244707944,6.39848162802911,-52.6972971332993));
#34949=CARTESIAN_POINT('Ctrl Pts',(-2.36918594503202,6.34115630042487,-52.6889731130946));
#34950=CARTESIAN_POINT('Ctrl Pts',(-2.53365299804881,6.27726316861511,-52.68064909289));
#34951=CARTESIAN_POINT('Ctrl Pts',(-2.6955178415194,6.20696967658539,-52.6723250726853));
#34952=CARTESIAN_POINT('Ctrl Pts',(-2.85722158447954,6.1367461461187,-52.6640093371945));
#34953=CARTESIAN_POINT('Ctrl Pts',(-3.01632796080577,6.06013508456906,-52.6556936017037));
#34954=CARTESIAN_POINT('Ctrl Pts',(-3.17230798206915,5.97735318237933,-52.6473778662128));
#34955=CARTESIAN_POINT('Ctrl Pts',(-3.32816133942105,5.89463850341119,-52.6390688835329));
#34956=CARTESIAN_POINT('Ctrl Pts',(-3.48089309451044,5.80576313114855,-52.6307599008529));
#34957=CARTESIAN_POINT('Ctrl Pts',(-3.62999560460828,5.71099123712553,-52.6224509181729));
#34958=CARTESIAN_POINT('Ctrl Pts',(-3.77900434012526,5.61627894769692,-52.6141471612358));
#34959=CARTESIAN_POINT('Ctrl Pts',(-3.92438808676057,5.51567771318103,-52.6058434042986));
#34960=CARTESIAN_POINT('Ctrl Pts',(-4.06566492689051,5.40949699161136,-52.5975396473614));
#34961=CARTESIAN_POINT('Ctrl Pts',(-4.20688441202795,5.30335937685584,-52.5892392615495));
#34962=CARTESIAN_POINT('Ctrl Pts',(-4.34400003529086,5.19164699714928,-52.5809388757375));
#34963=CARTESIAN_POINT('Ctrl Pts',(-4.47655969970676,5.07471203665403,-52.5726384899255));
#34964=CARTESIAN_POINT('Ctrl Pts',(-4.60909141073858,4.95780173469936,-52.564339854449));
#34965=CARTESIAN_POINT('Ctrl Pts',(-4.73706881627237,4.83567127596755,-52.5560412189724));
#34966=CARTESIAN_POINT('Ctrl Pts',(-4.86007351528718,4.70871260813443,-52.5477425834958));
#34967=CARTESIAN_POINT('Ctrl Pts',(-4.98307269317888,4.58175963890015,-52.5394443205074));
#34968=CARTESIAN_POINT('Ctrl Pts',(-5.10109936747627,4.44997914231351,-52.5311460575189));
#34969=CARTESIAN_POINT('Ctrl Pts',(-5.21377244339826,4.31379947476247,-52.5228477945305));
#34970=CARTESIAN_POINT('Ctrl Pts',(-5.32645916355048,4.17760331643294,-52.5145485266577));
#34971=CARTESIAN_POINT('Ctrl Pts',(-5.43379077228881,4.03700719395469,-52.5062492587849));
#34972=CARTESIAN_POINT('Ctrl Pts',(-5.53542674950234,3.89247218370202,-52.4979499909121));
#34973=CARTESIAN_POINT('Ctrl Pts',(-5.63713409155239,3.74783568657767,-52.4896448956156));
#34974=CARTESIAN_POINT('Ctrl Pts',(-5.73313761057706,3.59925506009198,-52.4813398003192));
#34975=CARTESIAN_POINT('Ctrl Pts',(-5.82313989610666,3.44722072840875,-52.4730347050228));
#34976=CARTESIAN_POINT('Ctrl Pts',(-5.91317500114936,3.29513095710296,-52.4647265812568));
#34977=CARTESIAN_POINT('Ctrl Pts',(-5.99720434021798,3.13958527344085,-52.4564184574908));
#34978=CARTESIAN_POINT('Ctrl Pts',(-6.07497661005813,2.98109848667344,-52.4481103337248));
#34979=CARTESIAN_POINT('Ctrl Pts',(-6.15283155137186,2.82244322936722,-52.4397933784712));
#34980=CARTESIAN_POINT('Ctrl Pts',(-6.22441598780934,2.66084093815967,-52.4314764232176));
#34981=CARTESIAN_POINT('Ctrl Pts',(-6.28952645710395,2.4968271757151,-52.423159467964));
#34982=CARTESIAN_POINT('Ctrl Pts',(-6.33751188234869,2.37595152818625,-52.4170299984807));
#34983=CARTESIAN_POINT('Ctrl Pts',(-6.38198199989548,2.25376651867671,-52.4109005289974));
#34984=CARTESIAN_POINT('Ctrl Pts',(-6.42287277311734,2.13049157246586,-52.4047710595141));
#34985=CARTESIAN_POINT('Ctrl Pts',(-6.48252027860105,1.95067000268968,-52.3958299822047));
#34986=CARTESIAN_POINT('Ctrl Pts',(-6.53464595542439,1.7682396727302,-52.3868889048954));
#34987=CARTESIAN_POINT('Ctrl Pts',(-6.57904187216683,1.58382355212808,-52.377947827586));
#34988=CARTESIAN_POINT('Ctrl Pts',(-6.6233814392243,1.3996415023834,-52.3690180987727));
#34989=CARTESIAN_POINT('Ctrl Pts',(-6.66001076183165,1.21347893703743,-52.3600883699595));
#34990=CARTESIAN_POINT('Ctrl Pts',(-6.68877173731219,1.0259735114191,-52.3511586411462));
#34991=CARTESIAN_POINT('Ctrl Pts',(-6.71747212389303,0.838863091437286,
-52.3422477240191));
#34992=CARTESIAN_POINT('Ctrl Pts',(-6.7383372084734,0.650415708016407,-52.333336806892));
#34993=CARTESIAN_POINT('Ctrl Pts',(-6.75125997573567,0.461278375852977,
-52.3244258897648));
#34994=CARTESIAN_POINT('Ctrl Pts',(-6.76170428381188,0.308415716815962,
-52.3172239985732));
#34995=CARTESIAN_POINT('Ctrl Pts',(-6.76696157518998,0.155102687705959,
-52.3100221073816));
#34996=CARTESIAN_POINT('Ctrl Pts',(-6.7669997900656,0.00168560139907666,
-52.30282021619));
#34997=CARTESIAN_POINT('',(-6.76699988382611,0.00125391286841605,-52.6971797837818));
#34998=CARTESIAN_POINT('Ctrl Pts',(3.0990855038472,6.01564277861013,-53.3487566918479));
#34999=CARTESIAN_POINT('Ctrl Pts',(2.99319764624946,6.07019314614216,-53.3431445815241));
#35000=CARTESIAN_POINT('Ctrl Pts',(2.88594953658319,6.12190541594522,-53.3375324712002));
#35001=CARTESIAN_POINT('Ctrl Pts',(2.77750956863615,6.17071548494457,-53.3319203608763));
#35002=CARTESIAN_POINT('Ctrl Pts',(2.61441390448676,6.24412670749781,-53.3234796459085));
#35003=CARTESIAN_POINT('Ctrl Pts',(2.44828550491286,6.31112214687189,-53.3150389309408));
#35004=CARTESIAN_POINT('Ctrl Pts',(2.27965724571934,6.37145602213806,-53.306598215973));
#35005=CARTESIAN_POINT('Ctrl Pts',(2.11115644371377,6.43174429421697,-53.2981638808955));
#35006=CARTESIAN_POINT('Ctrl Pts',(1.94015986151861,6.48538092748719,-53.2897295458181));
#35007=CARTESIAN_POINT('Ctrl Pts',(1.7672205103348,6.5321681444871,-53.2812952107406));
#35008=CARTESIAN_POINT('Ctrl Pts',(1.59438531805329,6.57892718221416,-53.2728659555427));
#35009=CARTESIAN_POINT('Ctrl Pts',(1.41961001059839,6.61884494123383,-53.2644367003449));
#35010=CARTESIAN_POINT('Ctrl Pts',(1.24346330579621,6.6517732979363,-53.256007445147));
#35011=CARTESIAN_POINT('Ctrl Pts',(1.06739567206154,6.68468687332158,-53.247581973785));
#35012=CARTESIAN_POINT('Ctrl Pts',(0.889958195636715,6.71061724106131,-53.2391565024229));
#35013=CARTESIAN_POINT('Ctrl Pts',(0.711730739017968,6.72946716725306,-53.2307310310608));
#35014=CARTESIAN_POINT('Ctrl Pts',(0.533555971609326,6.74831152085942,-53.2223080505127));
#35015=CARTESIAN_POINT('Ctrl Pts',(0.354592020952775,6.76007957217432,-53.2138850699646));
#35016=CARTESIAN_POINT('Ctrl Pts',(0.175425237951395,6.76472578793034,-53.2054620894164));
#35017=CARTESIAN_POINT('Ctrl Pts',(-0.00374451167684181,6.76937208061796,
-53.1970389694014));
#35018=CARTESIAN_POINT('Ctrl Pts',(-0.183116767313299,6.7668962868897,-53.1886158493863));
#35019=CARTESIAN_POINT('Ctrl Pts',(-0.362103120012962,6.75730496059464,
-53.1801927293712));
#35020=CARTESIAN_POINT('Ctrl Pts',(-0.541095662357151,6.74771330261563,
-53.1717693180707));
#35021=CARTESIAN_POINT('Ctrl Pts',(-0.71970194211908,6.73100563912223,-53.1633459067702));
#35022=CARTESIAN_POINT('Ctrl Pts',(-0.897336459140573,6.70724058604558,
-53.1549224954697));
#35023=CARTESIAN_POINT('Ctrl Pts',(-1.07500189280553,6.68347139674764,-53.146497618105));
#35024=CARTESIAN_POINT('Ctrl Pts',(-1.25169489599059,6.65264241319582,-53.1380727407404));
#35025=CARTESIAN_POINT('Ctrl Pts',(-1.42683760609694,6.61486382670328,-53.1296478633757));
#35026=CARTESIAN_POINT('Ctrl Pts',(-1.60203523292746,6.57707339457804,-53.1212203443557));
#35027=CARTESIAN_POINT('Ctrl Pts',(-1.77568127166105,6.53232908531064,-53.1127928253357));
#35028=CARTESIAN_POINT('Ctrl Pts',(-1.9472101598671,6.4807917412389,-53.1043653063157));
#35029=CARTESIAN_POINT('Ctrl Pts',(-2.11889286855081,6.42920818046882,-53.0959302298224));
#35030=CARTESIAN_POINT('Ctrl Pts',(-2.2884543133863,6.37081950879481,-53.0874951533291));
#35031=CARTESIAN_POINT('Ctrl Pts',(-2.45534506196263,6.30583615603004,-53.0790600768357));
#35032=CARTESIAN_POINT('Ctrl Pts',(-2.6223164699364,6.24082139638309,-53.0706209236144));
#35033=CARTESIAN_POINT('Ctrl Pts',(-2.78661429978894,6.16920572749927,-53.0621817703931));
#35034=CARTESIAN_POINT('Ctrl Pts',(-2.94771059564376,6.09124710090877,-53.0537426171718));
#35035=CARTESIAN_POINT('Ctrl Pts',(-3.10898591465231,6.01320184042568,-53.045294085685));
#35036=CARTESIAN_POINT('Ctrl Pts',(-3.26705229410281,5.92879969030739,-53.0368455541982));
#35037=CARTESIAN_POINT('Ctrl Pts',(-3.42140673824391,5.83834436561421,-53.0283970227115));
#35038=CARTESIAN_POINT('Ctrl Pts',(-3.50669257922616,5.78836486239545,-53.023728934812));
#35039=CARTESIAN_POINT('Ctrl Pts',(-3.59084569318444,5.73653815171483,-53.0190608469127));
#35040=CARTESIAN_POINT('Ctrl Pts',(-3.67378519826791,5.68292101977387,-53.0143927590132));
#35041=CARTESIAN_POINT('Ctrl Pts',(-3.8202018606275,5.58826839921398,-53.0061519834125));
#35042=CARTESIAN_POINT('Ctrl Pts',(-3.96316034508716,5.48782299183043,-52.9979112078117));
#35043=CARTESIAN_POINT('Ctrl Pts',(-4.10217389612254,5.38186383383776,-52.9896704322109));
#35044=CARTESIAN_POINT('Ctrl Pts',(-4.2410334745788,5.27602203710028,-52.9814387841626));
#35045=CARTESIAN_POINT('Ctrl Pts',(-4.37595653949345,5.16467886384185,-52.9732071361142));
#35046=CARTESIAN_POINT('Ctrl Pts',(-4.5064833229646,5.04815778872273,-52.9649754880659));
#35047=CARTESIAN_POINT('Ctrl Pts',(-4.63688879496296,4.93174500818391,-52.9567514905037));
#35048=CARTESIAN_POINT('Ctrl Pts',(-4.76290585886092,4.81016414525168,-52.9485274929414));
#35049=CARTESIAN_POINT('Ctrl Pts',(-4.88410593182653,4.68378033715255,-52.9403034953792));
#35050=CARTESIAN_POINT('Ctrl Pts',(-5.00519892405635,4.55750818963937,-52.9320867637508));
#35051=CARTESIAN_POINT('Ctrl Pts',(-5.12148316235565,4.42644181035422,-52.9238700321225));
#35052=CARTESIAN_POINT('Ctrl Pts',(-5.23256530501393,4.29098465725112,-52.9156533004941));
#35053=CARTESIAN_POINT('Ctrl Pts',(-5.34359053617773,4.15559690386283,-52.9074407786015));
#35054=CARTESIAN_POINT('Ctrl Pts',(-5.44941875472911,4.01582313131885,-52.899228256709));
#35055=CARTESIAN_POINT('Ctrl Pts',(-5.54969518995384,3.8721017934196,-52.8910157348164));
#35056=CARTESIAN_POINT('Ctrl Pts',(-5.64993809225506,3.7284285166288,-52.8828059592308));
#35057=CARTESIAN_POINT('Ctrl Pts',(-5.74463270632478,3.58081059571235,-52.8745961836452));
#35058=CARTESIAN_POINT('Ctrl Pts',(-5.83346604690986,3.42971760930108,-52.8663864080595));
#35059=CARTESIAN_POINT('Ctrl Pts',(-5.8722661418999,3.36372411872112,-52.8628005914003));
#35060=CARTESIAN_POINT('Ctrl Pts',(-5.90994862520771,3.29706806537326,-52.859214774741));
#35061=CARTESIAN_POINT('Ctrl Pts',(-5.9464900521143,3.22979025017194,-52.8556289580817));
#35062=CARTESIAN_POINT('Ctrl Pts',(-6.03671973994501,3.06366492947592,-52.8467747029205));
#35063=CARTESIAN_POINT('Ctrl Pts',(-6.11989614724476,2.8939185407244,-52.8379204477593));
#35064=CARTESIAN_POINT('Ctrl Pts',(-6.19577291945262,2.72115544035573,-52.8290661925981));
#35065=CARTESIAN_POINT('Ctrl Pts',(-6.27179059181142,2.5480715257746,-52.8201954954369));
#35066=CARTESIAN_POINT('Ctrl Pts',(-6.34048143590617,2.37195994293093,-52.8113247982758));
#35067=CARTESIAN_POINT('Ctrl Pts',(-6.40164811785171,2.19344258534517,-52.8024541011146));
#35068=CARTESIAN_POINT('Ctrl Pts',(-6.46298755491246,2.01442103518764,-52.7935583501453));
#35069=CARTESIAN_POINT('Ctrl Pts',(-6.51676022021659,1.83298036107809,-52.784662599176));
#35070=CARTESIAN_POINT('Ctrl Pts',(-6.56281854556193,1.6497580846986,-52.7757668482068));
#35071=CARTESIAN_POINT('Ctrl Pts',(-6.60893902019319,1.46628857541269,-52.7668590936623));
#35072=CARTESIAN_POINT('Ctrl Pts',(-6.64732430461649,1.28103291561712,-52.7579513391179));
#35073=CARTESIAN_POINT('Ctrl Pts',(-6.67787821435154,1.0946376360646,-52.7490435845735));
#35074=CARTESIAN_POINT('Ctrl Pts',(-6.70849946755582,0.907831525136283,
-52.7401161965648));
#35075=CARTESIAN_POINT('Ctrl Pts',(-6.731254779247,0.71988102823706,-52.7311888085561));
#35076=CARTESIAN_POINT('Ctrl Pts',(-6.74609969577474,0.531439455317279,
-52.7222614205475));
#35077=CARTESIAN_POINT('Ctrl Pts',(-6.76000203777315,0.354962936331661,
-52.7139008749683));
#35078=CARTESIAN_POINT('Ctrl Pts',(-6.76696712271792,0.178055918259438,
-52.7055403293892));
#35079=CARTESIAN_POINT('Ctrl Pts',(-6.766999883826,0.0012539134656088,-52.69717978381));
#35080=CARTESIAN_POINT('Ctrl Pts',(-6.76699988382611,0.00125391286840704,
-52.6971797837818));
#35081=CARTESIAN_POINT('Ctrl Pts',(-6.76700029478462,-0.000963909669029427,
-52.697074908238));
#35082=CARTESIAN_POINT('Ctrl Pts',(-6.76699961543752,-0.0031817380629446,
-52.6969700326941));
#35083=CARTESIAN_POINT('Ctrl Pts',(-6.76699784576786,-0.00539957157367193,
-52.6968651571502));
#35084=CARTESIAN_POINT('Ctrl Pts',(-6.76685907444447,-0.179314341218538,
-52.6886411827333));
#35085=CARTESIAN_POINT('Ctrl Pts',(-6.76001128430234,-0.353454329022078,
-52.6804172083163));
#35086=CARTESIAN_POINT('Ctrl Pts',(-6.74642750524413,-0.527261715361,-52.6721932338993));
#35087=CARTESIAN_POINT('Ctrl Pts',(-6.73285807197459,-0.700885544236132,
-52.6639779447973));
#35088=CARTESIAN_POINT('Ctrl Pts',(-6.71256684358021,-0.874177116575075,
-52.6557626556952));
#35089=CARTESIAN_POINT('Ctrl Pts',(-6.68557884092691,-1.04657754693592,
-52.6475473665932));
#35090=CARTESIAN_POINT('Ctrl Pts',(-6.65861392700485,-1.21883048556674,
-52.6393391058216));
#35091=CARTESIAN_POINT('Ctrl Pts',(-6.62496370427886,-1.39019344831153,
-52.6311308450501));
#35092=CARTESIAN_POINT('Ctrl Pts',(-6.58470508469999,-1.56011151765705,
-52.6229225842785));
#35093=CARTESIAN_POINT('Ctrl Pts',(-6.54447283438675,-1.72991829121661,
-52.6147196998912));
#35094=CARTESIAN_POINT('Ctrl Pts',(-6.49764089147426,-1.89828170881955,
-52.606516815504));
#35095=CARTESIAN_POINT('Ctrl Pts',(-6.44433746334812,-2.06465582083017,
-52.5983139311167));
#35096=CARTESIAN_POINT('Ctrl Pts',(-6.39105826249282,-2.23095431311399,
-52.5901147750731));
#35097=CARTESIAN_POINT('Ctrl Pts',(-6.33131354563359,-2.39526496035845,
-52.5819156190296));
#35098=CARTESIAN_POINT('Ctrl Pts',(-6.26528173009178,-2.5570556979812,-52.573716462986));
#35099=CARTESIAN_POINT('Ctrl Pts',(-6.19925565771237,-2.71883236374372,
-52.5655180200697));
#35100=CARTESIAN_POINT('Ctrl Pts',(-6.12694370334506,-2.87808922146103,
-52.5573195771533));
#35101=CARTESIAN_POINT('Ctrl Pts',(-6.04857304747007,-3.03431262222907,
-52.549121134237));
#35102=CARTESIAN_POINT('Ctrl Pts',(-5.9702031720742,-3.19053446719664,-52.5409227729674));
#35103=CARTESIAN_POINT('Ctrl Pts',(-5.88577487524587,-3.34372259429593,
-52.5327244116979));
#35104=CARTESIAN_POINT('Ctrl Pts',(-5.79556202206993,-3.49338658730189,
-52.5245260504283));
#35105=CARTESIAN_POINT('Ctrl Pts',(-5.70533367949665,-3.64307627736733,
-52.5163262815138));
#35106=CARTESIAN_POINT('Ctrl Pts',(-5.60931898701095,-3.78924032061379,
-52.5081265125992));
#35107=CARTESIAN_POINT('Ctrl Pts',(-5.50783601493496,-3.93141595771618,
-52.4999267436846));
#35108=CARTESIAN_POINT('Ctrl Pts',(-5.40631718309977,-4.07364183363209,
-52.491724077321));
#35109=CARTESIAN_POINT('Ctrl Pts',(-5.29932643084953,-4.21187620421581,
-52.4835214109574));
#35110=CARTESIAN_POINT('Ctrl Pts',(-5.18722312521175,-4.34568812149106,
-52.4753187445938));
#35111=CARTESIAN_POINT('Ctrl Pts',(-5.07499249823927,-4.4796520156577,-52.4671067620515));
#35112=CARTESIAN_POINT('Ctrl Pts',(-4.95763794804585,-4.60918314670217,
-52.4588947795091));
#35113=CARTESIAN_POINT('Ctrl Pts',(-4.83555755688677,-4.7338855197433,-52.4506827969668));
#35114=CARTESIAN_POINT('Ctrl Pts',(-4.71340516106317,-4.85866144392928,
-52.4424659708862));
#35115=CARTESIAN_POINT('Ctrl Pts',(-4.58652162829243,-4.97860268690591,
-52.4342491448056));
#35116=CARTESIAN_POINT('Ctrl Pts',(-4.45533926818216,-5.09335262920152,
-52.426032318725));
#35117=CARTESIAN_POINT('Ctrl Pts',(-4.32395460592637,-5.20827953248111,
-52.4178028211119));
#35118=CARTESIAN_POINT('Ctrl Pts',(-4.18825814709303,-5.3179989113675,-52.4095733234987));
#35119=CARTESIAN_POINT('Ctrl Pts',(-4.04871346690596,-5.42219588938783,
-52.4013438258856));
#35120=CARTESIAN_POINT('Ctrl Pts',(-3.92432928465839,-5.51507263600657,
-52.3940084023528));
#35121=CARTESIAN_POINT('Ctrl Pts',(-3.79688817561486,-5.60356225692823,
-52.38667297882));
#35122=CARTESIAN_POINT('Ctrl Pts',(-3.66673498003497,-5.68747251300505,
-52.3793375552872));
#35123=CARTESIAN_POINT('Ctrl Pts',(-3.52353267668539,-5.77979557807707,
-52.3712666851003));
#35124=CARTESIAN_POINT('Ctrl Pts',(-3.37657972706634,-5.86687518962925,
-52.3631958149133));
#35125=CARTESIAN_POINT('Ctrl Pts',(-3.22630413519261,-5.94838218570723,
-52.3551249447264));
#35126=CARTESIAN_POINT('Ctrl Pts',(-3.07621554961226,-6.029787752664,-52.3470641181101));
#35127=CARTESIAN_POINT('Ctrl Pts',(-2.92281287269902,-6.10563432685951,
-52.3390032914938));
#35128=CARTESIAN_POINT('Ctrl Pts',(-2.76655482863393,-6.17563465403859,
-52.3309424648774));
#35129=CARTESIAN_POINT('Ctrl Pts',(-2.6104569705547,-6.24556322125493,-52.322889901717));
#35130=CARTESIAN_POINT('Ctrl Pts',(-2.45150990799485,-6.30965731695414,
-52.3148373385566));
#35131=CARTESIAN_POINT('Ctrl Pts',(-2.29019874499602,-6.36767451338546,
-52.3067847753962));
#35132=CARTESIAN_POINT('Ctrl Pts',(-2.12901762696162,-6.42564493782588,
-52.2987387040078));
#35133=CARTESIAN_POINT('Ctrl Pts',(-1.96547655106936,-6.47754808820998,
-52.2906926326193));
#35134=CARTESIAN_POINT('Ctrl Pts',(-1.80008238183293,-6.52318882285456,
-52.2826465612309));
#35135=CARTESIAN_POINT('Ctrl Pts',(-1.63478537108558,-6.56880274648858,
-52.2746052163945));
#35136=CARTESIAN_POINT('Ctrl Pts',(-1.46763779269884,-6.6081614788189,-52.2665638715581));
#35137=CARTESIAN_POINT('Ctrl Pts',(-1.29916342247539,-6.64111913774343,
-52.2585225267216));
#35138=CARTESIAN_POINT('Ctrl Pts',(-1.12744138480924,-6.67471211891748,
-52.2503261695009));
#35139=CARTESIAN_POINT('Ctrl Pts',(-0.954341253873892,-6.70165459061485,
-52.2421298122802));
#35140=CARTESIAN_POINT('Ctrl Pts',(-0.780430991748114,-6.7218462097194,
-52.2339334550594));
#35141=CARTESIAN_POINT('Ctrl Pts',(-0.609864017430613,-6.74164966085067,
-52.2258946663504));
#35142=CARTESIAN_POINT('Ctrl Pts',(-0.438518164373885,-6.75495944178028,
-52.2178558776413));
#35143=CARTESIAN_POINT('Ctrl Pts',(-0.266936234653601,-6.76173306531905,
-52.2098170889323));
#35144=CARTESIAN_POINT('Ctrl Pts',(-0.0953359441126302,-6.7685074136969,
-52.20177744));
#35145=CARTESIAN_POINT('Ctrl Pts',(0.0765001001908305,-6.76874419718307,
-52.1937377910677));
#35146=CARTESIAN_POINT('Ctrl Pts',(0.248027630732855,-6.76245305302692,
-52.1856981421355));
#35147=CARTESIAN_POINT('Ctrl Pts',(0.419607479380795,-6.75615998999077,
-52.1776560410067));
#35148=CARTESIAN_POINT('Ctrl Pts',(0.590878253952469,-6.74333504971082,
-52.169613939878));
#35149=CARTESIAN_POINT('Ctrl Pts',(0.761299495061186,-6.72403986297074,
-52.1615718387493));
#35150=CARTESIAN_POINT('Ctrl Pts',(0.937471783458669,-6.70409353949051,
-52.1532583483055));
#35151=CARTESIAN_POINT('Ctrl Pts',(1.11273576417626,-6.67723268701323,-52.1449448578618));
#35152=CARTESIAN_POINT('Ctrl Pts',(1.28650550641272,-6.64358281215563,-52.136631367418));
#35153=CARTESIAN_POINT('Ctrl Pts',(1.45489875266539,-6.6109740760757,-52.1285750992467));
#35154=CARTESIAN_POINT('Ctrl Pts',(1.62188850625641,-6.57199032598076,-52.1205188310754));
#35155=CARTESIAN_POINT('Ctrl Pts',(1.78695725300251,-6.52679651712398,-52.1124625629041));
#35156=CARTESIAN_POINT('Ctrl Pts',(1.95993152571549,-6.47943827171273,-52.1040204613241));
#35157=CARTESIAN_POINT('Ctrl Pts',(2.13079580024639,-6.42526065884737,-52.0955783597441));
#35158=CARTESIAN_POINT('Ctrl Pts',(2.29897904412963,-6.36450974974921,-52.0871362581641));
#35159=CARTESIAN_POINT('Ctrl Pts',(2.46716228801287,-6.30375884065107,-52.0786941565841));
#35160=CARTESIAN_POINT('Ctrl Pts',(2.63266410692396,-6.23643488907362,-52.0702520550041));
#35161=CARTESIAN_POINT('Ctrl Pts',(2.79494455544576,-6.16283813936275,-52.0618099534241));
#35162=CARTESIAN_POINT('Ctrl Pts',(2.95514396992221,-6.09018517150096,-52.0534761107315));
#35163=CARTESIAN_POINT('Ctrl Pts',(3.11271368751341,-6.01118890160491,-52.0451422680389));
#35164=CARTESIAN_POINT('Ctrl Pts',(3.26712418554607,-5.92606012087457,-52.0368084253463));
#35165=CARTESIAN_POINT('Ctrl Pts',(3.42135269127273,-5.84103167518175,-52.0284844051416));
#35166=CARTESIAN_POINT('Ctrl Pts',(3.57242909304589,-5.74988528387595,-52.0201603849369));
#35167=CARTESIAN_POINT('Ctrl Pts',(3.71984441825884,-5.65287948783172,-52.0118363647322));
#35168=CARTESIAN_POINT('Ctrl Pts',(3.86711302424635,-5.55597023951913,-52.0035206292415));
#35169=CARTESIAN_POINT('Ctrl Pts',(4.01072752454583,-5.45321339525729,-51.9952048937507));
#35170=CARTESIAN_POINT('Ctrl Pts',(4.15020391807029,-5.34491313665938,-51.9868891582599));
#35171=CARTESIAN_POINT('Ctrl Pts',(4.28956704949117,-5.23670082351804,-51.9785801755799));
#35172=CARTESIAN_POINT('Ctrl Pts',(4.42479849641288,-5.12295427820283,-51.9702711928999));
#35173=CARTESIAN_POINT('Ctrl Pts',(4.55544342842863,-5.00402080035509,-51.96196221022));
#35174=CARTESIAN_POINT('Ctrl Pts',(4.68600619432943,-4.88516212297349,-51.9536584532829));
#35175=CARTESIAN_POINT('Ctrl Pts',(4.81198793749897,-4.76112324778029,-51.9453546963458));
#35176=CARTESIAN_POINT('Ctrl Pts',(4.93296693647855,-4.63229167946163,-51.9370509394087));
#35177=CARTESIAN_POINT('Ctrl Pts',(5.05389682090104,-4.50351241365391,-51.9287505535967));
#35178=CARTESIAN_POINT('Ctrl Pts',(5.16982777032636,-4.36994458486356,-51.9204501677848));
#35179=CARTESIAN_POINT('Ctrl Pts',(5.28037476813952,-4.23201267814683,-51.9121497819729));
#35180=CARTESIAN_POINT('Ctrl Pts',(5.39089845446724,-4.09410985768027,-51.9038511464963));
#35181=CARTESIAN_POINT('Ctrl Pts',(5.49604023366747,-3.95184506391964,-51.8955525110197));
#35182=CARTESIAN_POINT('Ctrl Pts',(5.59545510391203,-3.80567617909155,-51.8872538755432));
#35183=CARTESIAN_POINT('Ctrl Pts',(5.69486551187465,-3.65951385512073,-51.8789556125547));
#35184=CARTESIAN_POINT('Ctrl Pts',(5.78854932769342,-3.50944807694209,-51.8706573495662));
#35185=CARTESIAN_POINT('Ctrl Pts',(5.87620454593848,-3.35596619981369,-51.8623590865777));
#35186=CARTESIAN_POINT('Ctrl Pts',(5.96387037885675,-3.20246573668435,-51.8540598187049));
#35187=CARTESIAN_POINT('Ctrl Pts',(6.04550598757024,-3.04554865259202,-51.8457605508321));
#35188=CARTESIAN_POINT('Ctrl Pts',(6.1208549506089,-2.88572758132269,-51.8374612829594));
#35189=CARTESIAN_POINT('Ctrl Pts',(6.19625682076367,-2.72579428990284,-51.8291561876629));
#35190=CARTESIAN_POINT('Ctrl Pts',(6.26536307632958,-2.56295325185163,-51.8208510923665));
#35191=CARTESIAN_POINT('Ctrl Pts',(6.32796479903219,-2.39773862257953,-51.8125459970701));
#35192=CARTESIAN_POINT('Ctrl Pts',(6.39058934957813,-2.23246374746257,-51.8042378733041));
#35193=CARTESIAN_POINT('Ctrl Pts',(6.44670452346408,-2.06481388378804,-51.795929749538));
#35194=CARTESIAN_POINT('Ctrl Pts',(6.49615100789215,-1.89533930541784,-51.787621625772));
#35195=CARTESIAN_POINT('Ctrl Pts',(6.54565005364756,-1.72568457654975,-51.7793046705184));
#35196=CARTESIAN_POINT('Ctrl Pts',(6.58846615637215,-1.55420159368787,-51.7709877152648));
#35197=CARTESIAN_POINT('Ctrl Pts',(6.62449069415686,-1.38145287398055,-51.7626707600112));
#35198=CARTESIAN_POINT('Ctrl Pts',(6.65104023040786,-1.25413969584648,-51.7565412905279));
#35199=CARTESIAN_POINT('Ctrl Pts',(6.67390201399178,-1.12613927883489,-51.7504118210445));
#35200=CARTESIAN_POINT('Ctrl Pts',(6.69305057914302,-0.997678778481976,
-51.7442823515612));
#35201=CARTESIAN_POINT('Ctrl Pts',(6.71945171793614,-0.820563497391044,
-51.7358313280364));
#35202=CARTESIAN_POINT('Ctrl Pts',(6.73884052608722,-0.642249769575589,
-51.7273803045117));
#35203=CARTESIAN_POINT('Ctrl Pts',(6.7511203152946,-0.463317912902791,-51.7189292809869));
#35204=CARTESIAN_POINT('Ctrl Pts',(6.76338929251252,-0.284543600412125,
-51.7104856983372));
#35205=CARTESIAN_POINT('Ctrl Pts',(6.76856170412666,-0.105152573017721,
-51.7020421156875));
#35206=CARTESIAN_POINT('Ctrl Pts',(6.76659244153974,0.0742679614456169,
-51.6935985330379));
#35207=CARTESIAN_POINT('Ctrl Pts',(6.76462464513015,0.253554911732638,-51.6851612368984));
#35208=CARTESIAN_POINT('Ctrl Pts',(6.75552577772988,0.432870994911237,-51.676723940759));
#35209=CARTESIAN_POINT('Ctrl Pts',(6.73930275561423,0.611626821003214,-51.6682866446196));
#35210=CARTESIAN_POINT('Ctrl Pts',(6.72309130738794,0.790255118442305,-51.6598553678477));
#35211=CARTESIAN_POINT('Ctrl Pts',(6.69976587231466,0.968323626735281,-51.6514240910758));
#35212=CARTESIAN_POINT('Ctrl Pts',(6.66938537767895,1.14524568717907,-51.6429928143039));
#35213=CARTESIAN_POINT('Ctrl Pts',(6.63901790522285,1.3220919124241,-51.6345651514823));
#35214=CARTESIAN_POINT('Ctrl Pts',(6.60160145778941,1.49779234336162,-51.6261374886608));
#35215=CARTESIAN_POINT('Ctrl Pts',(6.55724655890211,1.67176749752065,-51.6177098258393));
#35216=CARTESIAN_POINT('Ctrl Pts',(6.51290531420719,1.84568909524546,-51.6092847573858));
#35217=CARTESIAN_POINT('Ctrl Pts',(6.46162995944129,2.01788615452275,-51.6008596889322));
#35218=CARTESIAN_POINT('Ctrl Pts',(6.40358175896227,2.18779104493223,-51.5924346204787));
#35219=CARTESIAN_POINT('Ctrl Pts',(6.38769799448225,2.23428222365952,-51.5901292638623));
#35220=CARTESIAN_POINT('Ctrl Pts',(6.37130741179366,2.2806018601415,-51.5878239072459));
#35221=CARTESIAN_POINT('Ctrl Pts',(6.35441396599858,2.32673852177725,-51.5855185506295));
#35222=CARTESIAN_POINT('Ctrl Pts',(6.29125479382549,2.49922869288211,-51.5768995621046));
#35223=CARTESIAN_POINT('Ctrl Pts',(6.22109119538753,2.66908289411008,-51.5682805735796));
#35224=CARTESIAN_POINT('Ctrl Pts',(6.14417435104374,2.83573809509558,-51.5596615850546));
#35225=CARTESIAN_POINT('Ctrl Pts',(6.06721142664618,3.00249313741863,-51.5510374329864));
#35226=CARTESIAN_POINT('Ctrl Pts',(5.98348730962295,3.16604507861792,-51.5424132809181));
#35227=CARTESIAN_POINT('Ctrl Pts',(5.89329970986362,3.3258544059717,-51.5337891288499));
#35228=CARTESIAN_POINT('Ctrl Pts',(5.80002316055734,3.49113724576673,-51.5248695972539));
#35229=CARTESIAN_POINT('Ctrl Pts',(5.69983272053446,3.65241625390595,-51.5159500656579));
#35230=CARTESIAN_POINT('Ctrl Pts',(5.59310682289629,3.8091265491804,-51.5070305340619));
#35231=CARTESIAN_POINT('Ctrl Pts',(5.4897230300421,3.96092948608048,-51.4983903162021));
#35232=CARTESIAN_POINT('Ctrl Pts',(5.38020711750334,4.10844529973347,-51.4897500983423));
#35233=CARTESIAN_POINT('Ctrl Pts',(5.26494481958201,4.25119336736835,-51.4811098804825));
#35234=CARTESIAN_POINT('Ctrl Pts',(5.14409336691997,4.40086339520475,-51.4720506920185));
#35235=CARTESIAN_POINT('Ctrl Pts',(5.01692463720449,4.54529150735008,-51.4629915035544));
#35236=CARTESIAN_POINT('Ctrl Pts',(4.88392796895243,4.68396590445364,-51.4539323150903));
#35237=CARTESIAN_POINT('Ctrl Pts',(4.75093130070036,4.8226403015572,-51.4448731266262));
#35238=CARTESIAN_POINT('Ctrl Pts',(4.61210699319241,4.95556074292922,-51.4358139381622));
#35239=CARTESIAN_POINT('Ctrl Pts',(4.46798590640481,5.0822623840341,-51.4267547496981));
#35240=CARTESIAN_POINT('Ctrl Pts',(4.32411342256124,5.20874547002193,-51.4177111879613));
#35241=CARTESIAN_POINT('Ctrl Pts',(4.17483043324289,5.32914835120471,-51.4086676262245));
#35242=CARTESIAN_POINT('Ctrl Pts',(4.02065033715821,5.44303774250276,-51.3996240644878));
#35243=CARTESIAN_POINT('Ctrl Pts',(3.86666731860615,5.55678155703184,-51.3905920624975));
#35244=CARTESIAN_POINT('Ctrl Pts',(3.70779988610797,5.66402836840122,-51.3815600605073));
#35245=CARTESIAN_POINT('Ctrl Pts',(3.54459266539005,5.76438650998205,-51.3725280585171));
#35246=CARTESIAN_POINT('Ctrl Pts',(3.39939019677095,5.853673306482,-51.364492452128));
#35247=CARTESIAN_POINT('Ctrl Pts',(3.25075318376519,5.93750796816106,-51.3564568457388));
#35248=CARTESIAN_POINT('Ctrl Pts',(3.09908550384718,6.01564277861014,-51.3484212393497));
#35249=CARTESIAN_POINT('Origin',(0.,0.,-63.6971797838103));
#35250=CARTESIAN_POINT('',(3.09908550384721,6.01564277861012,-48.954361679463));
#35251=CARTESIAN_POINT('',(3.0990855038472,6.01564277861013,-49.3486032095739));
#35252=CARTESIAN_POINT('',(3.09908550384721,6.01564277861012,-63.6971797838103));
#35253=CARTESIAN_POINT('',(-6.76699999643594,-0.000219627007310033,-50.3028202161602));
#35254=CARTESIAN_POINT('Ctrl Pts',(-6.76699999643594,-0.000219627007290654,
-50.3028202161602));
#35255=CARTESIAN_POINT('Ctrl Pts',(-6.76699376355498,-0.192262973378822,
-50.2938218191915));
#35256=CARTESIAN_POINT('Ctrl Pts',(-6.75880815810201,-0.384103022895448,
-50.2848234222228));
#35257=CARTESIAN_POINT('Ctrl Pts',(-6.74252052002201,-0.575070462710529,
-50.2758250252541));
#35258=CARTESIAN_POINT('Ctrl Pts',(-6.72617712925943,-0.766691585214444,
-50.2667958267188));
#35259=CARTESIAN_POINT('Ctrl Pts',(-6.70167620673784,-0.957433885510391,
-50.2577666281834));
#35260=CARTESIAN_POINT('Ctrl Pts',(-6.6691469286502,-1.14663343928025,-50.2487374296481));
#35261=CARTESIAN_POINT('Ctrl Pts',(-6.63656304962023,-1.33615056769457,
-50.2396930754506));
#35262=CARTESIAN_POINT('Ctrl Pts',(-6.5959239287075,-1.52411954709816,-50.2306487212531));
#35263=CARTESIAN_POINT('Ctrl Pts',(-6.5474093650472,-1.70988877021058,-50.2216043670556));
#35264=CARTESIAN_POINT('Ctrl Pts',(-6.49878671787905,-1.89607186057788,
-50.2125398633308));
#35265=CARTESIAN_POINT('Ctrl Pts',(-6.44225359159685,-2.08004516723249,
-50.2034753596059));
#35266=CARTESIAN_POINT('Ctrl Pts',(-6.37803978603545,-2.26117170682567,
-50.1944108558811));
#35267=CARTESIAN_POINT('Ctrl Pts',(-6.34891704925298,-2.34331760194549,
-50.190299852745));
#35268=CARTESIAN_POINT('Ctrl Pts',(-6.31821514885094,-2.42487823106995,
-50.1861888496089));
#35269=CARTESIAN_POINT('Ctrl Pts',(-6.2859587357902,-2.50579563650807,-50.1820778464728));
#35270=CARTESIAN_POINT('Ctrl Pts',(-6.21964895771645,-2.67213822354038,
-50.1736268229477));
#35271=CARTESIAN_POINT('Ctrl Pts',(-6.14667628219524,-2.83598784984301,
-50.1651757994225));
#35272=CARTESIAN_POINT('Ctrl Pts',(-6.06724917150553,-2.99679436913271,
-50.1567247758973));
#35273=CARTESIAN_POINT('Ctrl Pts',(-5.98789199402615,-3.15745930306146,
-50.1482811932472));
#35274=CARTESIAN_POINT('Ctrl Pts',(-5.90209185466891,-3.31508617463203,
-50.1398376105971));
#35275=CARTESIAN_POINT('Ctrl Pts',(-5.81010525632382,-3.46914483849238,
-50.131394027947));
#35276=CARTESIAN_POINT('Ctrl Pts',(-5.71818714486636,-3.62308880087893,
-50.1229567318071));
#35277=CARTESIAN_POINT('Ctrl Pts',(-5.62009192566996,-3.77346956776266,
-50.1145194356673));
#35278=CARTESIAN_POINT('Ctrl Pts',(-5.51612215794817,-3.91978128708647,
-50.1060821395274));
#35279=CARTESIAN_POINT('Ctrl Pts',(-5.41222656472862,-4.06598862415387,
-50.0976508627551));
#35280=CARTESIAN_POINT('Ctrl Pts',(-5.30246497426804,-4.20813243453552,
-50.0892195859827));
#35281=CARTESIAN_POINT('Ctrl Pts',(-5.18718351767982,-4.34573539851552,
-50.0807883092104));
#35282=CARTESIAN_POINT('Ctrl Pts',(-5.07195147489672,-4.48327938088436,
-50.0723606463885));
#35283=CARTESIAN_POINT('Ctrl Pts',(-4.95120449523002,-4.61628614339895,
-50.0639329835665));
#35284=CARTESIAN_POINT('Ctrl Pts',(-4.82532968654888,-4.74431053116363,
-50.0555053207446));
#35285=CARTESIAN_POINT('Ctrl Pts',(-4.69949362711262,-4.87229550795797,
-50.0470802522906));
#35286=CARTESIAN_POINT('Ctrl Pts',(-4.56853311881905,-4.99530093263866,
-50.0386551838367));
#35287=CARTESIAN_POINT('Ctrl Pts',(-4.43287315419674,-5.11291742538464,
-50.0302301153827));
#35288=CARTESIAN_POINT('Ctrl Pts',(-4.39575243543028,-5.14510089794912,
-50.0279247587689));
#35289=CARTESIAN_POINT('Ctrl Pts',(-4.35828006070707,-5.17688109700189,
-50.0256194021551));
#35290=CARTESIAN_POINT('Ctrl Pts',(-4.32046520081324,-5.20825013306407,
-50.0233140455413));
#35291=CARTESIAN_POINT('Ctrl Pts',(-4.17908757553354,-5.32552889168528,
-50.0146950570169));
#35292=CARTESIAN_POINT('Ctrl Pts',(-4.03298337072702,-5.43700508445549,
-50.0060760684924));
#35293=CARTESIAN_POINT('Ctrl Pts',(-3.88265296675354,-5.5423185527142,-49.9974570799679));
#35294=CARTESIAN_POINT('Ctrl Pts',(-3.73223250145224,-5.6476951131388,-49.9888329279001));
#35295=CARTESIAN_POINT('Ctrl Pts',(-3.57758103325063,-5.74690140639123,
-49.9802087758323));
#35296=CARTESIAN_POINT('Ctrl Pts',(-3.41922731773806,-5.83962101078775,
-49.9715846237645));
#35297=CARTESIAN_POINT('Ctrl Pts',(-3.2554499448681,-5.93551628657874,-49.9626650921683));
#35298=CARTESIAN_POINT('Ctrl Pts',(-3.08771254162915,-6.0244724909439,-49.953745560572));
#35299=CARTESIAN_POINT('Ctrl Pts',(-2.91662638756051,-6.10619189965282,
-49.9448260289758));
#35300=CARTESIAN_POINT('Ctrl Pts',(-2.75089776964948,-6.18535227785855,
-49.9361858111165));
#35301=CARTESIAN_POINT('Ctrl Pts',(-2.58202725636523,-6.25772216189874,
-49.9275455932573));
#35302=CARTESIAN_POINT('Ctrl Pts',(-2.410590037677,-6.32308031502466,-49.918905375398));
#35303=CARTESIAN_POINT('Ctrl Pts',(-2.2308397004448,-6.39160773372144,-49.9098461869333));
#35304=CARTESIAN_POINT('Ctrl Pts',(-2.04826791438665,-6.4524263849406,-49.9007869984686));
#35305=CARTESIAN_POINT('Ctrl Pts',(-1.86355508911284,-6.50534022398842,
-49.8917278100039));
#35306=CARTESIAN_POINT('Ctrl Pts',(-1.67884226383904,-6.55825406303623,
-49.8826686215392));
#35307=CARTESIAN_POINT('Ctrl Pts',(-1.49198877909424,-6.60326303251488,
-49.8736094330745));
#35308=CARTESIAN_POINT('Ctrl Pts',(-1.30368729826192,-6.64023255830325,
-49.8645502446098));
#35309=CARTESIAN_POINT('Ctrl Pts',(-1.11571203653408,-6.67713803698195,
-49.8555067505535));
#35310=CARTESIAN_POINT('Ctrl Pts',(-0.926120782753142,-6.70606673400241,
-49.8464632564972));
#35311=CARTESIAN_POINT('Ctrl Pts',(-0.735575215138369,-6.72690256380113,
-49.8374197624409));
#35312=CARTESIAN_POINT('Ctrl Pts',(-0.545203938857249,-6.74771933514254,
-49.8283845404356));
#35313=CARTESIAN_POINT('Ctrl Pts',(-0.353880327978583,-6.76045799255479,
-49.8193493184303));
#35314=CARTESIAN_POINT('Ctrl Pts',(-0.162272834050877,-6.76505406684449,
-49.8103140964249));
#35315=CARTESIAN_POINT('Ctrl Pts',(0.0289970891847575,-6.76964204385183,
-49.8012947925138));
#35316=CARTESIAN_POINT('Ctrl Pts',(0.220549659042468,-6.76611607813147,
-49.7922754886027));
#35317=CARTESIAN_POINT('Ctrl Pts',(0.411714919618717,-6.75446369632433,
-49.7832561846916));
#35318=CARTESIAN_POINT('Ctrl Pts',(0.602640350023257,-6.74282593324405,
-49.7742481961272));
#35319=CARTESIAN_POINT('Ctrl Pts',(0.793179203908962,-6.72308211454778,
-49.7652402075629));
#35320=CARTESIAN_POINT('Ctrl Pts',(0.982662579947927,-6.69527170874865,
-49.7562322189985));
#35321=CARTESIAN_POINT('Ctrl Pts',(1.17171800114492,-6.66752411372516,-49.7472445752918));
#35322=CARTESIAN_POINT('Ctrl Pts',(1.35972246771617,-6.63174633224124,-49.7382569315852));
#35323=CARTESIAN_POINT('Ctrl Pts',(1.54601371560388,-6.58802934049058,-49.7292692878785));
#35324=CARTESIAN_POINT('Ctrl Pts',(1.70826048063626,-6.54995487070782,-49.7214416731451));
#35325=CARTESIAN_POINT('Ctrl Pts',(1.86920766915795,-6.50585913879513,-49.7136140584117));
#35326=CARTESIAN_POINT('Ctrl Pts',(2.02842123090489,-6.45583428458432,-49.7057864436783));
#35327=CARTESIAN_POINT('Ctrl Pts',(2.19364614714791,-6.40392066456125,-49.697663285233));
#35328=CARTESIAN_POINT('Ctrl Pts',(2.35692969512879,-6.34564335320328,-49.6895401267877));
#35329=CARTESIAN_POINT('Ctrl Pts',(2.51774860006068,-6.28118070006687,-49.6814169683424));
#35330=CARTESIAN_POINT('Ctrl Pts',(2.67855616641804,-6.2167225918849,-49.6732943826223));
#35331=CARTESIAN_POINT('Ctrl Pts',(2.836899096113,-6.14608014677511,-49.6651717969022));
#35332=CARTESIAN_POINT('Ctrl Pts',(2.99227317568785,-6.06948022832754,-49.6570492111821));
#35333=CARTESIAN_POINT('Ctrl Pts',(3.1476659250574,-5.99287110561144,-49.6489256494497));
#35334=CARTESIAN_POINT('Ctrl Pts',(3.30008878619914,-5.91030324705111,-49.6408020877173));
#35335=CARTESIAN_POINT('Ctrl Pts',(3.44906131849665,-5.82204989855379,-49.6326785259849));
#35336=CARTESIAN_POINT('Ctrl Pts',(3.59814235960617,-5.73373226796464,-49.6245490472018));
#35337=CARTESIAN_POINT('Ctrl Pts',(3.74376773720741,-5.63972106311222,-49.6164195684187));
#35338=CARTESIAN_POINT('Ctrl Pts',(3.88548469258686,-5.54033371771712,-49.6082900896356));
#35339=CARTESIAN_POINT('Ctrl Pts',(4.02725942347458,-5.44090585385068,-49.600157296607));
#35340=CARTESIAN_POINT('Ctrl Pts',(4.16512226485639,-5.33609770197789,-49.5920245035785));
#35341=CARTESIAN_POINT('Ctrl Pts',(4.29865305189998,-5.22626740029546,-49.58389171055));
#35342=CARTESIAN_POINT('Ctrl Pts',(4.43232903341692,-5.11631767482196,-49.5757500743428));
#35343=CARTESIAN_POINT('Ctrl Pts',(4.5616632791119,-5.00133513542633,-49.5676084381357));
#35344=CARTESIAN_POINT('Ctrl Pts',(4.6862714937236,-4.88171573190345,-49.5594668019286));
#35345=CARTESIAN_POINT('Ctrl Pts',(4.74975768652857,-4.82077127058576,-49.555318748868));
#35346=CARTESIAN_POINT('Ctrl Pts',(4.81201773362238,-4.75862375098831,-49.5511706958074));
#35347=CARTESIAN_POINT('Ctrl Pts',(4.87300483250201,-4.69532883858118,-49.5470226427468));
#35348=CARTESIAN_POINT('Ctrl Pts',(4.99710515413813,-4.56653243521136,-49.5385819277687));
#35349=CARTESIAN_POINT('Ctrl Pts',(5.1161877999895,-4.43271779629924,-49.5301412127906));
#35350=CARTESIAN_POINT('Ctrl Pts',(5.22984172174294,-4.29430373466024,-49.5217004978125));
#35351=CARTESIAN_POINT('Ctrl Pts',(5.34340973850756,-4.15599429289035,-49.5132661627245));
#35352=CARTESIAN_POINT('Ctrl Pts',(5.45155700000134,-4.01309261526358,-49.5048318276365));
#35353=CARTESIAN_POINT('Ctrl Pts',(5.55391086229364,-3.8660526553187,-49.4963974925485));
#35354=CARTESIAN_POINT('Ctrl Pts',(5.65620307831851,-3.71910125543876,-49.4879682373399));
#35355=CARTESIAN_POINT('Ctrl Pts',(5.75270866154225,-3.56801681523327,-49.4795389821312));
#35356=CARTESIAN_POINT('Ctrl Pts',(5.84309641932045,-3.41328481591042,-49.4711097269226));
#35357=CARTESIAN_POINT('Ctrl Pts',(5.93344360264594,-3.25862227473479,-49.4626842555496));
#35358=CARTESIAN_POINT('Ctrl Pts',(6.01767826836475,-3.10031572659021,-49.4542587841766));
#35359=CARTESIAN_POINT('Ctrl Pts',(6.09551337666583,-2.93887830215679,-49.4458333128036));
#35360=CARTESIAN_POINT('Ctrl Pts',(6.17332547465082,-2.77748860330949,-49.4374103322443));
#35361=CARTESIAN_POINT('Ctrl Pts',(6.24474164344188,-2.61297017399657,-49.4289873516851));
#35362=CARTESIAN_POINT('Ctrl Pts',(6.30952132935479,-2.44585968412274,-49.4205643711259));
#35363=CARTESIAN_POINT('Ctrl Pts',(6.3743020878849,-2.27874642724589,-49.4121412510995));
#35364=CARTESIAN_POINT('Ctrl Pts',(6.43244601734344,-2.10904133246272,-49.4037181310732));
#35365=CARTESIAN_POINT('Ctrl Pts',(6.48376090770987,-1.93730056822717,-49.3952950110469));
#35366=CARTESIAN_POINT('Ctrl Pts',(6.53507757263076,-1.76555386490967,-49.386871599735));
#35367=CARTESIAN_POINT('Ctrl Pts',(6.5795646319486,-1.591771671276,-49.3784481884232));
#35368=CARTESIAN_POINT('Ctrl Pts',(6.61707987028794,-1.41652496985763,-49.3700247771113));
#35369=CARTESIAN_POINT('Ctrl Pts',(6.65460163801874,-1.24124776738511,-49.3615998997352));
#35370=CARTESIAN_POINT('Ctrl Pts',(6.68514909576253,-1.06450587504572,-49.3531750223591));
#35371=CARTESIAN_POINT('Ctrl Pts',(6.70863115887434,-0.886880473446274,
-49.344750144983));
#35372=CARTESIAN_POINT('Ctrl Pts',(6.73212058488464,-0.709199376663938,
-49.3363226259515));
#35373=CARTESIAN_POINT('Ctrl Pts',(6.7485401556958,-0.530634548786091,-49.3278951069201));
#35374=CARTESIAN_POINT('Ctrl Pts',(6.75785061913856,-0.35177266722784,-49.3194675878887));
#35375=CARTESIAN_POINT('Ctrl Pts',(6.7671694318451,-0.172750389246998,-49.3110325113839));
#35376=CARTESIAN_POINT('Ctrl Pts',(6.76936638132112,0.0065691413373811,
-49.3025974348791));
#35377=CARTESIAN_POINT('Ctrl Pts',(6.76445433781425,0.18559771449576,-49.2941623583743));
#35378=CARTESIAN_POINT('Ctrl Pts',(6.75953992028441,0.364712813341815,-49.2857232051416));
#35379=CARTESIAN_POINT('Ctrl Pts',(6.74750967465999,0.543536341425885,-49.2772840519088));
#35380=CARTESIAN_POINT('Ctrl Pts',(6.7284284513529,0.721484286055326,-49.268844898676));
#35381=CARTESIAN_POINT('Ctrl Pts',(6.70932602345691,0.899629980742703,-49.2603963671779));
#35382=CARTESIAN_POINT('Ctrl Pts',(6.68315700487441,1.0768978170993,-49.2519478356798));
#35383=CARTESIAN_POINT('Ctrl Pts',(6.65003774541412,1.25271185217012,-49.2434993041817));
#35384=CARTESIAN_POINT('Ctrl Pts',(6.63173828000527,1.34985481084729,-49.2388312164157));
#35385=CARTESIAN_POINT('Ctrl Pts',(6.61131786213327,1.44655414126861,-49.2341631286497));
#35386=CARTESIAN_POINT('Ctrl Pts',(6.58880268423295,1.54271455177059,-49.2294950408837));
#35387=CARTESIAN_POINT('Ctrl Pts',(6.54905567477237,1.71247064976259,-49.221254265287));
#35388=CARTESIAN_POINT('Ctrl Pts',(6.5026891205378,1.88092405804825,-49.2130134896902));
#35389=CARTESIAN_POINT('Ctrl Pts',(6.44980161272551,2.04752244346269,-49.2047727140935));
#35390=CARTESIAN_POINT('Ctrl Pts',(6.39697268356182,2.21393630310386,-49.1965410660491));
#35391=CARTESIAN_POINT('Ctrl Pts',(6.33763728916775,2.37849889490668,-49.1883094180047));
#35392=CARTESIAN_POINT('Ctrl Pts',(6.27194495619697,2.54066831098343,-49.1800777699603));
#35393=CARTESIAN_POINT('Ctrl Pts',(6.20631367761972,2.70268700695481,-49.171853772402));
#35394=CARTESIAN_POINT('Ctrl Pts',(6.13433735949582,2.86231662897421,-49.1636297748437));
#35395=CARTESIAN_POINT('Ctrl Pts',(6.05621526573445,3.01903058200558,-49.1554057772855));
#35396=CARTESIAN_POINT('Ctrl Pts',(5.97816219314641,3.17560607765067,-49.147189045661));
#35397=CARTESIAN_POINT('Ctrl Pts',(5.89397432524319,3.32927072135779,-49.1389723140365));
#35398=CARTESIAN_POINT('Ctrl Pts',(5.80389888449294,3.47951817621085,-49.130755582412));
#35399=CARTESIAN_POINT('Ctrl Pts',(5.71386959272571,3.62968865373038,-49.1225430605233));
#35400=CARTESIAN_POINT('Ctrl Pts',(5.61795891812474,3.77644512480496,-49.1143305386346));
#35401=CARTESIAN_POINT('Ctrl Pts',(5.51646003415715,3.91930576652893,-49.1061180167459));
#35402=CARTESIAN_POINT('Ctrl Pts',(5.41499509190489,4.06211863496669,-49.097908241164));
#35403=CARTESIAN_POINT('Ctrl Pts',(5.30794586884362,4.20103797963546,-49.0896984655822));
#35404=CARTESIAN_POINT('Ctrl Pts',(5.19564892880966,4.33561082300511,-49.0814886900003));
#35405=CARTESIAN_POINT('Ctrl Pts',(5.14660054289747,4.39438874476237,-49.0779028733176));
#35406=CARTESIAN_POINT('Ctrl Pts',(5.09655158672348,4.45233786950648,-49.0743170566349));
#35407=CARTESIAN_POINT('Ctrl Pts',(5.04553256808488,4.50942236926136,-49.0707312399522));
#35408=CARTESIAN_POINT('Ctrl Pts',(4.91955089499462,4.65038158365912,-49.0618767539755));
#35409=CARTESIAN_POINT('Ctrl Pts',(4.7877822974446,4.78592055307892,-49.0530222679987));
#35410=CARTESIAN_POINT('Ctrl Pts',(4.65071258853474,4.9156038712293,-49.044167782022));
#35411=CARTESIAN_POINT('Ctrl Pts',(4.51325128960666,5.04565767745704,-49.0352879999506));
#35412=CARTESIAN_POINT('Ctrl Pts',(4.37045876470817,5.1698221793112,-49.0264082178793));
#35413=CARTESIAN_POINT('Ctrl Pts',(4.22285535174613,5.28770098230121,-49.0175284358079));
#35414=CARTESIAN_POINT('Ctrl Pts',(4.07503400119427,5.4057538342627,-49.0086355426691));
#35415=CARTESIAN_POINT('Ctrl Pts',(3.92238777843376,5.51750229011527,-48.9997426495303));
#35416=CARTESIAN_POINT('Ctrl Pts',(3.76546632465436,5.62259302794485,-48.9908497563915));
#35417=CARTESIAN_POINT('Ctrl Pts',(3.60821568568681,5.72790422201843,-48.9819382080043));
#35418=CARTESIAN_POINT('Ctrl Pts',(3.44667209776304,5.82652962585396,-48.9730266596171));
#35419=CARTESIAN_POINT('Ctrl Pts',(3.28141222117305,5.91816042657988,-48.9641151112299));
#35420=CARTESIAN_POINT('Ctrl Pts',(3.22112150400139,5.95158951296656,-48.9608639673076));
#35421=CARTESIAN_POINT('Ctrl Pts',(3.16033637079744,5.98408810010785,-48.9576128233853));
#35422=CARTESIAN_POINT('Ctrl Pts',(3.09908550384721,6.01564277861012,-48.954361679463));
#35423=CARTESIAN_POINT('Ctrl Pts',(3.0990855038472,6.01564277861013,-50.9542788176482));
#35424=CARTESIAN_POINT('Ctrl Pts',(2.94371885527148,6.09568319093221,-50.9460782653071));
#35425=CARTESIAN_POINT('Ctrl Pts',(2.78528905180417,6.16968031566986,-50.9378777129661));
#35426=CARTESIAN_POINT('Ctrl Pts',(2.62431077295935,6.2374098764575,-50.9296771606251));
#35427=CARTESIAN_POINT('Ctrl Pts',(2.46326604928346,6.30516739306164,-50.9214732234527));
#35428=CARTESIAN_POINT('Ctrl Pts',(2.29967108513821,6.3666520534542,-50.9132692862804));
#35429=CARTESIAN_POINT('Ctrl Pts',(2.13405869120049,6.421688446391,-50.9050653491081));
#35430=CARTESIAN_POINT('Ctrl Pts',(1.96825491490221,6.47678843960884,-50.8968519314324));
#35431=CARTESIAN_POINT('Ctrl Pts',(1.8004293927172,6.5254251684168,-50.8886385137566));
#35432=CARTESIAN_POINT('Ctrl Pts',(1.63112914484802,6.5674733888176,-50.8804250960809));
#35433=CARTESIAN_POINT('Ctrl Pts',(1.4617200186328,6.60954865076589,-50.8722063962905));
#35434=CARTESIAN_POINT('Ctrl Pts',(1.29083462661431,6.64502688625558,-50.8639876965));
#35435=CARTESIAN_POINT('Ctrl Pts',(1.1190281028488,6.6738343630206,-50.8557689967096));
#35436=CARTESIAN_POINT('Ctrl Pts',(0.946972562451434,6.70268359338543,-50.8475383847234));
#35437=CARTESIAN_POINT('Ctrl Pts',(0.773993578147219,6.72484270590575,-50.8393077727373));
#35438=CARTESIAN_POINT('Ctrl Pts',(0.600650386828964,6.74028991311221,-50.8310771607511));
#35439=CARTESIAN_POINT('Ctrl Pts',(0.502759058404987,6.74901334564153,-50.8264291239004));
#35440=CARTESIAN_POINT('Ctrl Pts',(0.404751579198324,6.75559719899961,-50.8217810870496));
#35441=CARTESIAN_POINT('Ctrl Pts',(0.306728244600427,6.76004488032175,-50.8171330501989));
#35442=CARTESIAN_POINT('Ctrl Pts',(0.13652012573504,6.76776785234939,-50.8090621800125));
#35443=CARTESIAN_POINT('Ctrl Pts',(-0.0342906662540302,6.7690722624394,
-50.8009913098261));
#35444=CARTESIAN_POINT('Ctrl Pts',(-0.205168628666277,6.76388903174876,
-50.7929204396397));
#35445=CARTESIAN_POINT('Ctrl Pts',(-0.375833946736591,6.75871225118583,
-50.7848596130239));
#35446=CARTESIAN_POINT('Ctrl Pts',(-0.546565900771842,6.74706390500711,
-50.7767987864081));
#35447=CARTESIAN_POINT('Ctrl Pts',(-0.716823528716951,6.72892658814746,
-50.7687379597922));
#35448=CARTESIAN_POINT('Ctrl Pts',(-0.886906619177028,6.7108078645321,-50.7606853966324));
#35449=CARTESIAN_POINT('Ctrl Pts',(-1.05651598341785,6.68621344732343,-50.7526328334725));
#35450=CARTESIAN_POINT('Ctrl Pts',(-1.22511041953536,6.65517794352232,-50.7445802703126));
#35451=CARTESIAN_POINT('Ctrl Pts',(-1.39356893909867,6.62416745975646,-50.7365341989247));
#35452=CARTESIAN_POINT('Ctrl Pts',(-1.56101379407839,6.58672629176055,-50.7284881275368));
#35453=CARTESIAN_POINT('Ctrl Pts',(-1.72690877231002,6.54294085959202,-50.7204420561489));
#35454=CARTESIAN_POINT('Ctrl Pts',(-1.89270629785877,6.49918114856274,-50.712400711313));
#35455=CARTESIAN_POINT('Ctrl Pts',(-2.05695539937716,6.44908468743227,-50.7043593664771));
#35456=CARTESIAN_POINT('Ctrl Pts',(-2.21913003802878,6.3927889746431,-50.6963180216413));
#35457=CARTESIAN_POINT('Ctrl Pts',(-2.38443090470133,6.33540805373358,-50.6881216644202));
#35458=CARTESIAN_POINT('Ctrl Pts',(-2.54757612479494,6.27158651133287,-50.6799253071992));
#35459=CARTESIAN_POINT('Ctrl Pts',(-2.70802439040033,6.20152343388275,-50.6717289499781));
#35460=CARTESIAN_POINT('Ctrl Pts',(-2.86538816445975,6.13280726391876,-50.6636901612696));
#35461=CARTESIAN_POINT('Ctrl Pts',(-3.02015739141042,6.05808753417179,-50.6556513725611));
#35462=CARTESIAN_POINT('Ctrl Pts',(-3.17184161906389,5.9776006677909,-50.6476125838526));
#35463=CARTESIAN_POINT('Ctrl Pts',(-3.32354207830387,5.89710518858615,-50.6395729349209));
#35464=CARTESIAN_POINT('Ctrl Pts',(-3.47215655094803,5.81084151891391,-50.6315332859892));
#35465=CARTESIAN_POINT('Ctrl Pts',(-3.61721954755021,5.71909186364589,-50.6234936370575));
#35466=CARTESIAN_POINT('Ctrl Pts',(-3.76232679023396,5.6273142235518,-50.6154515359294));
#35467=CARTESIAN_POINT('Ctrl Pts',(-3.90388008522075,5.53004746669188,-50.6074094348013));
#35468=CARTESIAN_POINT('Ctrl Pts',(-4.04144339720263,5.42761681285694,-50.5993673336731));
#35469=CARTESIAN_POINT('Ctrl Pts',(-4.18364893049433,5.32172952689267,-50.5910538432284));
#35470=CARTESIAN_POINT('Ctrl Pts',(-4.32159012595492,5.21032398423091,-50.5827403527836));
#35471=CARTESIAN_POINT('Ctrl Pts',(-4.45482379577049,5.09380348547498,-50.5744268623388));
#35472=CARTESIAN_POINT('Ctrl Pts',(-4.58393516969235,4.98088817131105,-50.566370594168));
#35473=CARTESIAN_POINT('Ctrl Pts',(-4.70862576761979,4.86317001060159,-50.5583143259973));
#35474=CARTESIAN_POINT('Ctrl Pts',(-4.82853137587974,4.74105196682603,-50.5502580578265));
#35475=CARTESIAN_POINT('Ctrl Pts',(-4.95417954246217,4.61308540604791,-50.5418159562447));
#35476=CARTESIAN_POINT('Ctrl Pts',(-5.07457279345764,4.48028751760336,-50.533373854663));
#35477=CARTESIAN_POINT('Ctrl Pts',(-5.18934148411168,4.34315829337104,-50.5249317530812));
#35478=CARTESIAN_POINT('Ctrl Pts',(-5.30411017476572,4.2060290691387,-50.5164896514994));
#35479=CARTESIAN_POINT('Ctrl Pts',(-5.4132540920048,4.0645689268294,-50.5080475499177));
#35480=CARTESIAN_POINT('Ctrl Pts',(-5.5164577155674,3.91930902996394,-50.4996054483359));
#35481=CARTESIAN_POINT('Ctrl Pts',(-5.62099658766643,3.77216976047574,-50.4910541228394));
#35482=CARTESIAN_POINT('Ctrl Pts',(-5.71975709886979,3.62068774169861,-50.4825027973429));
#35483=CARTESIAN_POINT('Ctrl Pts',(-5.81237669910402,3.46533780571429,-50.4739514718463));
#35484=CARTESIAN_POINT('Ctrl Pts',(-5.9048762937362,3.31018915393491,-50.4654112261533));
#35485=CARTESIAN_POINT('Ctrl Pts',(-5.99125067460389,3.15118284725474,-50.4568709804602));
#35486=CARTESIAN_POINT('Ctrl Pts',(-6.0711794357131,2.98882405962184,-50.4483307347671));
#35487=CARTESIAN_POINT('Ctrl Pts',(-6.15101355609578,2.82665751509901,-50.439800601267));
#35488=CARTESIAN_POINT('Ctrl Pts',(-6.22441713018384,2.6611466881456,-50.4312704677669));
#35489=CARTESIAN_POINT('Ctrl Pts',(-6.29111445915045,2.49282327128663,-50.4227403342668));
#35490=CARTESIAN_POINT('Ctrl Pts',(-6.35774023414615,2.32468043450573,-50.4142193520316));
#35491=CARTESIAN_POINT('Ctrl Pts',(-6.41767398982197,2.15373131958206,-50.4056983697963));
#35492=CARTESIAN_POINT('Ctrl Pts',(-6.47068694435408,1.9805300977682,-50.3971773875611));
#35493=CARTESIAN_POINT('Ctrl Pts',(-6.52363271889448,1.8075483629976,-50.3886672034321));
#35494=CARTESIAN_POINT('Ctrl Pts',(-6.56967509607546,1.63232052007738,-50.3801570193032));
#35495=CARTESIAN_POINT('Ctrl Pts',(-6.60863420702198,1.45541846826916,-50.3716468351742));
#35496=CARTESIAN_POINT('Ctrl Pts',(-6.64756370104846,1.27865089832662,-50.3631431205318));
#35497=CARTESIAN_POINT('Ctrl Pts',(-6.67942059378738,1.10021196802362,-50.3546394058893));
#35498=CARTESIAN_POINT('Ctrl Pts',(-6.70407512900704,0.920687604255242,
-50.3461356912469));
#35499=CARTESIAN_POINT('Ctrl Pts',(-6.72870903519254,0.741313452778424,
-50.3376390918641));
#35500=CARTESIAN_POINT('Ctrl Pts',(-6.74615256207308,0.560855995920925,
-50.3291424924813));
#35501=CARTESIAN_POINT('Ctrl Pts',(-6.75632719034912,0.379910380154642,
-50.3206458930985));
#35502=CARTESIAN_POINT('Ctrl Pts',(-6.76344257177574,0.253370418327687,
-50.3147040007956));
#35503=CARTESIAN_POINT('Ctrl Pts',(-6.76700411216908,0.126591947465235,
-50.3087621084928));
#35504=CARTESIAN_POINT('Ctrl Pts',(-6.76699999643596,-0.000219626373065103,
-50.3028202161899));
#35505=CARTESIAN_POINT('',(-6.76699981440648,0.000570866902357549,-50.6971797838101));
#35506=CARTESIAN_POINT('Ctrl Pts',(3.09908550384718,6.01564277861014,-51.3484212393497));
#35507=CARTESIAN_POINT('Ctrl Pts',(2.92904011259127,6.10324525542459,-51.3394119511931));
#35508=CARTESIAN_POINT('Ctrl Pts',(2.75518479088681,6.18368201021633,-51.3304026630366));
#35509=CARTESIAN_POINT('Ctrl Pts',(2.57811484594898,6.25664549428026,-51.32139337488));
#35510=CARTESIAN_POINT('Ctrl Pts',(2.40144887074735,6.32944251847761,-51.3124046406337));
#35511=CARTESIAN_POINT('Ctrl Pts',(2.2215831314487,6.3948002148617,-51.3034159063874));
#35512=CARTESIAN_POINT('Ctrl Pts',(2.03913343426668,6.45245874355317,-51.2944271721411));
#35513=CARTESIAN_POINT('Ctrl Pts',(1.86026950611045,6.50898408227805,-51.2856150976829));
#35514=CARTESIAN_POINT('Ctrl Pts',(1.67892245044474,6.55810994139659,-51.2768030232247));
#35515=CARTESIAN_POINT('Ctrl Pts',(1.49569253948088,6.59963581020508,-51.2679909487665));
#35516=CARTESIAN_POINT('Ctrl Pts',(1.32678729409768,6.63791524298957,-51.2598677903211));
#35517=CARTESIAN_POINT('Ctrl Pts',(1.15635749427144,6.66971847226523,-51.2517446318757));
#35518=CARTESIAN_POINT('Ctrl Pts',(0.984945083573756,6.69493630905805,-51.2436214734303));
#35519=CARTESIAN_POINT('Ctrl Pts',(0.81354475834823,6.7201523678614,-51.2354988877101));
#35520=CARTESIAN_POINT('Ctrl Pts',(0.641162322375299,6.73878390575607,-51.2273763019899));
#35521=CARTESIAN_POINT('Ctrl Pts',(0.468347659396175,6.75077324977948,-51.2192537162697));
#35522=CARTESIAN_POINT('Ctrl Pts',(0.295512230956435,6.76276403444598,-51.2111301545372));
#35523=CARTESIAN_POINT('Ctrl Pts',(0.122244837314489,6.76811101184451,-51.2030065928047));
#35524=CARTESIAN_POINT('Ctrl Pts',(-0.0509018418445705,6.76680855370512,
-51.1948830310722));
#35525=CARTESIAN_POINT('Ctrl Pts',(-0.224174637812543,6.76550514687954,
-51.186753552289));
#35526=CARTESIAN_POINT('Ctrl Pts',(-0.397326177299663,6.75754263387956,
-51.1786240735057));
#35527=CARTESIAN_POINT('Ctrl Pts',(-0.569805467044783,6.74296750175514,
-51.1704945947225));
#35528=CARTESIAN_POINT('Ctrl Pts',(-0.742355073561008,6.72838642760584,
-51.1623618016939));
#35529=CARTESIAN_POINT('Ctrl Pts',(-0.914231521030211,6.70718740547868,
-51.1542290086652));
#35530=CARTESIAN_POINT('Ctrl Pts',(-1.08489150021608,6.6794684992714,-51.1460962156366));
#35531=CARTESIAN_POINT('Ctrl Pts',(-1.25573704623894,6.65171945295878,-51.1379545794293));
#35532=CARTESIAN_POINT('Ctrl Pts',(-1.42536312374954,6.61743643522956,-51.129812943222));
#35533=CARTESIAN_POINT('Ctrl Pts',(-1.5932383939877,6.57676823522948,-51.1216713070148));
#35534=CARTESIAN_POINT('Ctrl Pts',(-1.67876856392686,6.55604833972497,-51.1175232539549));
#35535=CARTESIAN_POINT('Ctrl Pts',(-1.76384451885883,6.5336717996434,-51.113375200895));
#35536=CARTESIAN_POINT('Ctrl Pts',(-1.84839780253586,6.50966316821236,-51.1092271478351));
#35537=CARTESIAN_POINT('Ctrl Pts',(-2.02045205489797,6.46080891972589,-51.100786432857));
#35538=CARTESIAN_POINT('Ctrl Pts',(-2.19069537674778,6.40509316346649,-51.092345717879));
#35539=CARTESIAN_POINT('Ctrl Pts',(-2.35856180545217,6.34267098388859,-51.0839050029009));
#35540=CARTESIAN_POINT('Ctrl Pts',(-2.52630135280056,6.28029598593509,-51.0754706678129));
#35541=CARTESIAN_POINT('Ctrl Pts',(-2.69166727696468,6.2112247852629,-51.0670363327249));
#35542=CARTESIAN_POINT('Ctrl Pts',(-2.85410912028243,6.13566215901109,-51.0586019976369));
#35543=CARTESIAN_POINT('Ctrl Pts',(-3.01645312720168,6.06014504304816,-51.0501727424283));
#35544=CARTESIAN_POINT('Ctrl Pts',(-3.175876262803,5.97814443633935,-51.0417434872197));
#35545=CARTESIAN_POINT('Ctrl Pts',(-3.33184802553106,5.88991321962937,-51.0333142320111));
#35546=CARTESIAN_POINT('Ctrl Pts',(-3.48774977359163,5.80172160931475,-51.024888760638));
#35547=CARTESIAN_POINT('Ctrl Pts',(-3.64020294819763,5.70730512957085,-51.0164632892649));
#35548=CARTESIAN_POINT('Ctrl Pts',(-3.78870129001075,5.60696277275594,-51.0080378178918));
#35549=CARTESIAN_POINT('Ctrl Pts',(-3.93715573140377,5.50665008005419,-50.9996148373327));
#35550=CARTESIAN_POINT('Ctrl Pts',(-4.08165739561812,5.4004151903653,-50.9911918567735));
#35551=CARTESIAN_POINT('Ctrl Pts',(-4.2217283501773,5.2886008298329,-50.9827688762143));
#35552=CARTESIAN_POINT('Ctrl Pts',(-4.3618016240215,5.17678461788618,-50.974345756188));
#35553=CARTESIAN_POINT('Ctrl Pts',(-4.49744377700071,5.05938895330167,-50.9659226361617));
#35554=CARTESIAN_POINT('Ctrl Pts',(-4.62820884200249,4.93679773890018,-50.9574995161354));
#35555=CARTESIAN_POINT('Ctrl Pts',(-4.75897842907795,4.81420228509039,-50.9490761048236));
#35556=CARTESIAN_POINT('Ctrl Pts',(-4.88487034847325,4.68641115119791,-50.9406526935117));
#35557=CARTESIAN_POINT('Ctrl Pts',(-5.00547438240334,4.55384619932469,-50.9322292821999));
#35558=CARTESIAN_POINT('Ctrl Pts',(-5.12609940702924,4.42125817500115,-50.9238044048238));
#35559=CARTESIAN_POINT('Ctrl Pts',(-5.24143448689091,4.28389492287238,-50.9153795274477));
#35560=CARTESIAN_POINT('Ctrl Pts',(-5.35110845808286,4.14221284699785,-50.9069546500717));
#35561=CARTESIAN_POINT('Ctrl Pts',(-5.46081681800385,4.00048634612017,-50.8985271310403));
#35562=CARTESIAN_POINT('Ctrl Pts',(-5.56486032620094,3.85443858522592,-50.8900996120089));
#35563=CARTESIAN_POINT('Ctrl Pts',(-5.66290984476275,3.70455680076432,-50.8816720929776));
#35564=CARTESIAN_POINT('Ctrl Pts',(-5.76104729034368,3.55454060811059,-50.8732370164728));
#35565=CARTESIAN_POINT('Ctrl Pts',(-5.8531798231717,3.40068380120735,-50.8648019399681));
#35566=CARTESIAN_POINT('Ctrl Pts',(-5.93902257667899,3.24350116906057,-50.8563668634633));
#35567=CARTESIAN_POINT('Ctrl Pts',(-6.0249068185538,3.08624256951358,-50.8479277102306));
#35568=CARTESIAN_POINT('Ctrl Pts',(-6.10449506578661,2.92565523530496,-50.8394885569979));
#35569=CARTESIAN_POINT('Ctrl Pts',(-6.17754948354762,2.7622764847713,-50.8310494037651));
#35570=CARTESIAN_POINT('Ctrl Pts',(-6.25068508524938,2.59871617463853,-50.8226008722671));
#35571=CARTESIAN_POINT('Ctrl Pts',(-6.31727222048796,2.4323585575581,-50.814152340769));
#35572=CARTESIAN_POINT('Ctrl Pts',(-6.37712161930826,2.26375989286657,-50.8057038092709));
#35573=CARTESIAN_POINT('Ctrl Pts',(-6.41019035397727,2.17060366042096,-50.8010357215046));
#35574=CARTESIAN_POINT('Ctrl Pts',(-6.44120299326327,2.07676352947594,-50.7963676337383));
#35575=CARTESIAN_POINT('Ctrl Pts',(-6.4701342208643,1.98233502819294,-50.791699545972));
#35576=CARTESIAN_POINT('Ctrl Pts',(-6.52561322009058,1.80125737667182,-50.7827479438781));
#35577=CARTESIAN_POINT('Ctrl Pts',(-6.57354245803368,1.61766672833935,-50.7737963417841));
#35578=CARTESIAN_POINT('Ctrl Pts',(-6.61370831146901,1.43218412601375,-50.7648447396901));
#35579=CARTESIAN_POINT('Ctrl Pts',(-6.65378960644619,1.24709200768197,-50.7559119827994));
#35580=CARTESIAN_POINT('Ctrl Pts',(-6.68614005816093,1.06011612052976,-50.7469792259087));
#35581=CARTESIAN_POINT('Ctrl Pts',(-6.71059549156741,0.871892853827292,
-50.7380464690179));
#35582=CARTESIAN_POINT('Ctrl Pts',(-6.73497102105433,0.684284574253256,
-50.7291428983729));
#35583=CARTESIAN_POINT('Ctrl Pts',(-6.75150295156409,0.495437290930622,
-50.7202393277279));
#35584=CARTESIAN_POINT('Ctrl Pts',(-6.76007802694969,0.305996845657041,
-50.7113357570829));
#35585=CARTESIAN_POINT('Ctrl Pts',(-6.7646225908784,0.205598403017538,-50.7066170993253));
#35586=CARTESIAN_POINT('Ctrl Pts',(-6.76693313590177,0.105033600446035,
-50.7018984415677));
#35587=CARTESIAN_POINT('Ctrl Pts',(-6.76699856951929,0.0044000140721489,
-50.6971797838101));
#35588=CARTESIAN_POINT('Ctrl Pts',(-6.767,7.54030492757439E-13,-50.6971797838101));
#35589=CARTESIAN_POINT('Ctrl Pts',(-6.76700000000002,-0.186007249559271,
-50.6884302719974));
#35590=CARTESIAN_POINT('Ctrl Pts',(-6.75932637294251,-0.372014355815471,
-50.6796807601846));
#35591=CARTESIAN_POINT('Ctrl Pts',(-6.74400518263367,-0.557389537585863,
-50.6709312483719));
#35592=CARTESIAN_POINT('Ctrl Pts',(-6.72868405703733,-0.742763936382495,
-50.6621817735147));
#35593=CARTESIAN_POINT('Ctrl Pts',(-6.70571545643565,-0.927506130404962,
-50.6534322986575));
#35594=CARTESIAN_POINT('Ctrl Pts',(-6.67517739401572,-1.11098864009564,
-50.6446828238003));
#35595=CARTESIAN_POINT('Ctrl Pts',(-6.64463945804386,-1.29447039004558,
-50.6359333851717));
#35596=CARTESIAN_POINT('Ctrl Pts',(-6.6065321700272,-1.47669218339293,-50.6271839465432));
#35597=CARTESIAN_POINT('Ctrl Pts',(-6.56098496085476,-1.65703510627797,
-50.6184345079147));
#35598=CARTESIAN_POINT('Ctrl Pts',(-6.5154379364955,-1.83737729740029,-50.6096851047881));
#35599=CARTESIAN_POINT('Ctrl Pts',(-6.46245112156888,-2.01584035544979,
-50.6009357016615));
#35600=CARTESIAN_POINT('Ctrl Pts',(-6.40220448361706,-2.19181813797441,
-50.5921862985348));
#35601=CARTESIAN_POINT('Ctrl Pts',(-6.34195808511951,-2.36779522106362,
-50.5834369301833));
#35602=CARTESIAN_POINT('Ctrl Pts',(-6.2744520141632,-2.54128677725829,-50.5746875618317));
#35603=CARTESIAN_POINT('Ctrl Pts',(-6.19991555052676,-2.71170355428768,
-50.5659381934802));
#35604=CARTESIAN_POINT('Ctrl Pts',(-6.12537937695062,-2.8821196681364,-50.557188859177));
#35605=CARTESIAN_POINT('Ctrl Pts',(-6.04381298028282,-3.04946076420006,
-50.5484395248738));
#35606=CARTESIAN_POINT('Ctrl Pts',(-5.95549339308799,-3.21315848424651,
-50.5396901905706));
#35607=CARTESIAN_POINT('Ctrl Pts',(-5.86717414225612,-3.37685558085424,
-50.5309408895891));
#35608=CARTESIAN_POINT('Ctrl Pts',(-5.77210188843856,-3.53690907700344,
-50.5221915886075));
#35609=CARTESIAN_POINT('Ctrl Pts',(-5.67059953311147,-3.69277537024336,
-50.513442287626));
#35610=CARTESIAN_POINT('Ctrl Pts',(-5.56909755592466,-3.84864108281377,
-50.5046930192393));
#35611=CARTESIAN_POINT('Ctrl Pts',(-5.46116568154707,-4.00031938355183,
-50.4959437508527));
#35612=CARTESIAN_POINT('Ctrl Pts',(-5.347170484881,-4.14729511918522,-50.4871944824661));
#35613=CARTESIAN_POINT('Ctrl Pts',(-5.23317570343005,-4.29427031947545,
-50.4784452459477));
#35614=CARTESIAN_POINT('Ctrl Pts',(-5.11311781951224,-4.43654276249929,
-50.4696960094294));
#35615=CARTESIAN_POINT('Ctrl Pts',(-4.98740458928897,-4.57362924412761,
-50.460946772911));
#35616=CARTESIAN_POINT('Ctrl Pts',(-4.86169180652367,-4.71071523781654,
-50.4521975675343));
#35617=CARTESIAN_POINT('Ctrl Pts',(-4.73032391141173,-4.84261509584881,
-50.4434483621576));
#35618=CARTESIAN_POINT('Ctrl Pts',(-4.593747069469,-4.96888084599993,-50.4346991567808));
#35619=CARTESIAN_POINT('Ctrl Pts',(-4.45717070231126,-5.09514615721074,
-50.4259499818192));
#35620=CARTESIAN_POINT('Ctrl Pts',(-4.31538563497031,-5.21577720520855,
-50.4172008068575));
#35621=CARTESIAN_POINT('Ctrl Pts',(-4.16887340951763,-5.33036429293692,
-50.4084516318958));
#35622=CARTESIAN_POINT('Ctrl Pts',(-4.02236168122246,-5.44495099183882,
-50.3997024866226));
#35623=CARTESIAN_POINT('Ctrl Pts',(-3.87112305262948,-5.5534935949809,-50.3909533413493));
#35624=CARTESIAN_POINT('Ctrl Pts',(-3.71567116928769,-5.6556234635736,-50.3822041960761));
#35625=CARTESIAN_POINT('Ctrl Pts',(-3.56021980053097,-5.75775299409059,
-50.3734550797647));
#35626=CARTESIAN_POINT('Ctrl Pts',(-3.40055544441883,-5.85346967519995,
-50.3647059634533));
#35627=CARTESIAN_POINT('Ctrl Pts',(-3.23722035886657,-5.94244843041484,
-50.355956847142));
#35628=CARTESIAN_POINT('Ctrl Pts',(-3.07388580043289,-6.03142689847554,
-50.347207759066));
#35629=CARTESIAN_POINT('Ctrl Pts',(-2.90688078789007,-6.11366734708005,
-50.3384586709899));
#35630=CARTESIAN_POINT('Ctrl Pts',(-2.73677250610162,-6.18889047001531,
-50.3297095829139));
#35631=CARTESIAN_POINT('Ctrl Pts',(-2.56666475916715,-6.26411335643424,
-50.3209605223468));
#35632=CARTESIAN_POINT('Ctrl Pts',(-2.39345402456885,-6.33231884545334,
-50.3122114617796));
#35633=CARTESIAN_POINT('Ctrl Pts',(-2.2177285594387,-6.39327529804951,-50.3034624012124));
#35634=CARTESIAN_POINT('Ctrl Pts',(-2.04200363223416,-6.45423156404757,
-50.2947133674276));
#35635=CARTESIAN_POINT('Ctrl Pts',(-1.86376426060879,-6.50793874412497,
-50.2859643336429));
#35636=CARTESIAN_POINT('Ctrl Pts',(-1.68361577621555,-6.55421443943346,
-50.2772152998581));
#35637=CARTESIAN_POINT('Ctrl Pts',(-1.50346782833097,-6.60048999692614,
-50.2684662921292));
#35638=CARTESIAN_POINT('Ctrl Pts',(-1.32141105657284,-6.63933404265182,
-50.2597172844003));
#35639=CARTESIAN_POINT('Ctrl Pts',(-1.13806375346447,-6.67061465631544,
-50.2509682766714));
#35640=CARTESIAN_POINT('Ctrl Pts',(-0.954716981169393,-6.70189517941779,
-50.242219294272));
#35641=CARTESIAN_POINT('Ctrl Pts',(-0.77007996744194,-6.72561226609007,
-50.2334703118726));
#35642=CARTESIAN_POINT('Ctrl Pts',(-0.584779764073002,-6.74168536995985,
-50.2247213294731));
#35643=CARTESIAN_POINT('Ctrl Pts',(-0.391489587592836,-6.75845153117873,
-50.2155950990575));
#35644=CARTESIAN_POINT('Ctrl Pts',(-0.197478091805063,-6.76689985146395,
-50.2064688686419));
#35645=CARTESIAN_POINT('Ctrl Pts',(-0.00346214753080522,-6.76699911434415,
-50.1973426382263));
#35646=CARTESIAN_POINT('Ctrl Pts',(0.184490798484886,-6.76709527525934,
-50.1885016025112));
#35647=CARTESIAN_POINT('Ctrl Pts',(0.372447602155044,-6.75935633790762,
-50.179660566796));
#35648=CARTESIAN_POINT('Ctrl Pts',(0.559756448194499,-6.74380914014511,
-50.1708195310809));
#35649=CARTESIAN_POINT('Ctrl Pts',(0.745136131043656,-6.72842206873151,
-50.1620695524676));
#35650=CARTESIAN_POINT('Ctrl Pts',(0.929880851945357,-6.70538686355719,
-50.1533195738543));
#35651=CARTESIAN_POINT('Ctrl Pts',(1.11336305057495,-6.67478177303307,-50.144569595241));
#35652=CARTESIAN_POINT('Ctrl Pts',(1.29684337090154,-6.64417699581255,-50.135819706201));
#35653=CARTESIAN_POINT('Ctrl Pts',(1.47906091205219,-6.60600253548053,-50.127069817161));
#35654=CARTESIAN_POINT('Ctrl Pts',(1.65939671095249,-6.56038806441205,-50.118319928121));
#35655=CARTESIAN_POINT('Ctrl Pts',(1.83973072369188,-6.51477404513842,-50.1095701257455));
#35656=CARTESIAN_POINT('Ctrl Pts',(2.01818275357064,-6.46172023288652,-50.1008203233701));
#35657=CARTESIAN_POINT('Ctrl Pts',(2.19414664033354,-6.40140683918098,-50.0920705209946));
#35658=CARTESIAN_POINT('Ctrl Pts',(2.37010884271288,-6.34109402281487,-50.083320802375));
#35659=CARTESIAN_POINT('Ctrl Pts',(2.54358267847834,-6.2735218569978,-50.0745710837555));
#35660=CARTESIAN_POINT('Ctrl Pts',(2.71397890841771,-6.19891986435249,-50.0658213651359));
#35661=CARTESIAN_POINT('Ctrl Pts',(2.88437356388977,-6.12431856103227,-50.0570717273641));
#35662=CARTESIAN_POINT('Ctrl Pts',(3.05169040787213,-6.04268767582537,-50.0483220895923));
#35663=CARTESIAN_POINT('Ctrl Pts',(3.215361125121,-5.95430447953921,-50.0395724518205));
#35664=CARTESIAN_POINT('Ctrl Pts',(3.3790303844288,-5.86592207055021,-50.0308228919884));
#35665=CARTESIAN_POINT('Ctrl Pts',(3.53905332980003,-5.77078760703359,-50.0220733321563));
#35666=CARTESIAN_POINT('Ctrl Pts',(3.69488643041914,-5.66922422085284,-50.0133237723243));
#35667=CARTESIAN_POINT('Ctrl Pts',(3.85071819468771,-5.56766170563139,-50.0045742875243));
#35668=CARTESIAN_POINT('Ctrl Pts',(4.0023599459926,-5.45967053456226,-49.9958248027243));
#35669=CARTESIAN_POINT('Ctrl Pts',(4.14929662974342,-5.34561750206652,-49.9870753179243));
#35670=CARTESIAN_POINT('Ctrl Pts',(4.29623210225083,-5.23156540974434,-49.9783259052489));
#35671=CARTESIAN_POINT('Ctrl Pts',(4.43846235842153,-5.11145173172155,-49.9695764925736));
#35672=CARTESIAN_POINT('Ctrl Pts',(4.57550431797461,-4.98568443006531,-49.9608270798982));
#35673=CARTESIAN_POINT('Ctrl Pts',(4.71254519337526,-4.85991812336658,-49.9520777364403));
#35674=CARTESIAN_POINT('Ctrl Pts',(4.84439764315016,-4.72849847631068,-49.9433283929824));
#35675=CARTESIAN_POINT('Ctrl Pts',(4.97061384196717,-4.5918718442531,-49.9345790495245));
#35676=CARTESIAN_POINT('Ctrl Pts',(5.09682908420235,-4.45524624767715,-49.9258297723772));
#35677=CARTESIAN_POINT('Ctrl Pts',(5.21740796650197,-4.31341395556861,-49.9170804952298));
#35678=CARTESIAN_POINT('Ctrl Pts',(5.33194095942275,-4.16685668162826,-49.9083312180825));
#35679=CARTESIAN_POINT('Ctrl Pts',(5.44647312235168,-4.02030046975168,-49.8995820043389));
#35680=CARTESIAN_POINT('Ctrl Pts',(5.55495930712333,-3.86901957035484,-49.8908327905954));
#35681=CARTESIAN_POINT('Ctrl Pts',(5.65703106079848,-3.71352778058294,-49.8820835768518));
#35682=CARTESIAN_POINT('Ctrl Pts',(5.75910210868779,-3.55803706597532,-49.8733344236056));
#35683=CARTESIAN_POINT('Ctrl Pts',(5.85475865698584,-3.39833575880839,-49.8645852703594));
#35684=CARTESIAN_POINT('Ctrl Pts',(5.9436758306909,-3.23496624706672,-49.8558361171132));
#35685=CARTESIAN_POINT('Ctrl Pts',(6.03259241910112,-3.07159781070032,-49.8470870214581));
#35686=CARTESIAN_POINT('Ctrl Pts',(6.11476958471009,-2.90456146975747,-49.838337925803));
#35687=CARTESIAN_POINT('Ctrl Pts',(6.18992823574433,-2.73442451648151,-49.8295888301478));
#35688=CARTESIAN_POINT('Ctrl Pts',(6.26508641700982,-2.56428862662302,-49.8208397891777));
#35689=CARTESIAN_POINT('Ctrl Pts',(6.33322605570343,-2.39105242531156,-49.8120907482076));
#35690=CARTESIAN_POINT('Ctrl Pts',(6.39411573747812,-2.215304253536,-49.8033417072375));
#35691=CARTESIAN_POINT('Ctrl Pts',(6.45500505889165,-2.03955712188435,-49.7945927180465));
#35692=CARTESIAN_POINT('Ctrl Pts',(6.50864441544964,-1.86129832025448,-49.7858437288555));
#35693=CARTESIAN_POINT('Ctrl Pts',(6.55485164049937,-1.68113324012188,-49.7770947396645));
#35694=CARTESIAN_POINT('Ctrl Pts',(6.60199852639138,-1.49730435912772,-49.7681678327876));
#35695=CARTESIAN_POINT('Ctrl Pts',(6.64140767441036,-1.3114911317352,-49.7592409259107));
#35696=CARTESIAN_POINT('Ctrl Pts',(6.67293975269625,-1.12435050446295,-49.7503140190338));
#35697=CARTESIAN_POINT('Ctrl Pts',(6.70384664831526,-0.940920291562351,
-49.7415641048498));
#35698=CARTESIAN_POINT('Ctrl Pts',(6.72718585889682,-0.756215114276515,
-49.7328141906658));
#35699=CARTESIAN_POINT('Ctrl Pts',(6.74287810451877,-0.570862389373684,
-49.7240642764819));
#35700=CARTESIAN_POINT('Ctrl Pts',(6.75857004154131,-0.385513309566699,
-49.7153145343713));
#35701=CARTESIAN_POINT('Ctrl Pts',(6.7666152903556,-0.199516993257867,-49.7065647922607));
#35702=CARTESIAN_POINT('Ctrl Pts',(6.76698652348897,-0.0135052182037693,
-49.6978150501501));
#35703=CARTESIAN_POINT('Ctrl Pts',(6.76735774981521,0.172503146039211,-49.6890654684795));
#35704=CARTESIAN_POINT('Ctrl Pts',(6.76005524147477,0.358526681833818,-49.6803158868088));
#35705=CARTESIAN_POINT('Ctrl Pts',(6.74510380214878,0.543933542115243,-49.6715663051382));
#35706=CARTESIAN_POINT('Ctrl Pts',(6.73015261710975,0.729337249085073,-49.6628168722762));
#35707=CARTESIAN_POINT('Ctrl Pts',(6.70755278444601,0.914124015854987,-49.6540674394143));
#35708=CARTESIAN_POINT('Ctrl Pts',(6.67738106408284,1.09766621749415,-49.6453180065524));
#35709=CARTESIAN_POINT('Ctrl Pts',(6.64720981677249,1.28120554143349,-49.63656871087));
#35710=CARTESIAN_POINT('Ctrl Pts',(6.60946696581517,1.46350005650645,-49.6278194151877));
#35711=CARTESIAN_POINT('Ctrl Pts',(6.56428070010989,1.64393062206556,-49.6190701195054));
#35712=CARTESIAN_POINT('Ctrl Pts',(6.51909508282734,1.82435859844675,-49.6103209493754));
#35713=CARTESIAN_POINT('Ctrl Pts',(6.46646633415654,2.00292240086586,-49.6015717792454));
#35714=CARTESIAN_POINT('Ctrl Pts',(6.40657319597184,2.17901557696477,-49.5928226091154));
#35715=CARTESIAN_POINT('Ctrl Pts',(6.34668083768285,2.35510646007461,-49.5840735529123));
#35716=CARTESIAN_POINT('Ctrl Pts',(6.27952437143873,2.5287265099656,-49.5753244967092));
#35717=CARTESIAN_POINT('Ctrl Pts',(6.20533187335121,2.69928607997958,-49.5665754405061));
#35718=CARTESIAN_POINT('Ctrl Pts',(6.12831449784238,2.87633970115428,-49.5574932642173));
#35719=CARTESIAN_POINT('Ctrl Pts',(6.04371489463139,3.05009490562377,-49.5484110879285));
#35720=CARTESIAN_POINT('Ctrl Pts',(5.95184265120477,3.21991584599657,-49.5393289116396));
#35721=CARTESIAN_POINT('Ctrl Pts',(5.86333281335475,3.38352155905331,-49.5305791312852));
#35722=CARTESIAN_POINT('Ctrl Pts',(5.76807337235663,3.5434756090386,-49.5218293509308));
#35723=CARTESIAN_POINT('Ctrl Pts',(5.66638790086329,3.69923467178687,-49.5130795705764));
#35724=CARTESIAN_POINT('Ctrl Pts',(5.56470608502714,3.85498813489805,-49.5043301047821));
#35725=CARTESIAN_POINT('Ctrl Pts',(5.45659885766922,4.00654667256303,-49.4955806389878));
#35726=CARTESIAN_POINT('Ctrl Pts',(5.34243340580475,4.15339551506252,-49.4868311731936));
#35727=CARTESIAN_POINT('Ctrl Pts',(5.22827145140558,4.30023985883914,-49.4780819754397));
#35728=CARTESIAN_POINT('Ctrl Pts',(5.10805181978051,4.44237456993087,-49.4693327776858));
#35729=CARTESIAN_POINT('Ctrl Pts',(4.9821828128251,4.57931691626494,-49.4605835799319));
#35730=CARTESIAN_POINT('Ctrl Pts',(4.85631699296187,4.71625579512204,-49.4518346037139));
#35731=CARTESIAN_POINT('Ctrl Pts',(4.72480227791797,4.8480023613581,-49.4430856274959));
#35732=CARTESIAN_POINT('Ctrl Pts',(4.58808530848072,4.97410918678947,-49.4343366512779));
#35733=CARTESIAN_POINT('Ctrl Pts',(4.45135945056923,5.1002242108905,-49.4255871062567));
#35734=CARTESIAN_POINT('Ctrl Pts',(4.30943087207987,5.22069856612031,-49.4168375612355));
#35735=CARTESIAN_POINT('Ctrl Pts',(4.16278164322408,5.3351230530173,-49.4080880162143));
#35736=CARTESIAN_POINT('Ctrl Pts',(4.01614103534339,5.44954081331465,-49.3993389855471));
#35737=CARTESIAN_POINT('Ctrl Pts',(3.8647805583337,5.55790924068367,-49.3905899548798));
#35738=CARTESIAN_POINT('Ctrl Pts',(3.70921425811917,5.65986029751313,-49.3818409242126));
#35739=CARTESIAN_POINT('Ctrl Pts',(3.55364584530093,5.7618127388467,-49.3730917747327));
#35740=CARTESIAN_POINT('Ctrl Pts',(3.39387173464324,5.85734747818075,-49.3643426252529));
#35741=CARTESIAN_POINT('Ctrl Pts',(3.23043456092393,5.94614005448814,-49.355593475773));
#35742=CARTESIAN_POINT('Ctrl Pts',(3.18690768806384,5.96978744811286,-49.35326338704));
#35743=CARTESIAN_POINT('Ctrl Pts',(3.14312114982877,5.99295688499302,-49.350933298307));
#35744=CARTESIAN_POINT('Ctrl Pts',(3.0990855038472,6.01564277861013,-49.3486032095739));
#35745=CARTESIAN_POINT('Origin',(0.,0.,-63.6971797838103));
#35746=CARTESIAN_POINT('',(3.0990855038472,6.01564277861013,-46.9540128207846));
#35747=CARTESIAN_POINT('',(3.0990855038472,6.01564277861012,-47.3486841594369));
#35748=CARTESIAN_POINT('',(3.09908550384721,6.01564277861012,-63.6971797838103));
#35749=CARTESIAN_POINT('',(-6.76699650576387,-0.00687684372451031,-48.3028202162139));
#35750=CARTESIAN_POINT('Ctrl Pts',(-6.76699650576336,-0.00687684422915549,
-48.30282021619));
#35751=CARTESIAN_POINT('Ctrl Pts',(-6.76681092372738,-0.189494473350243,
-48.2941842225582));
#35752=CARTESIAN_POINT('Ctrl Pts',(-6.75923366544663,-0.37185469943169,
-48.2855482289264));
#35753=CARTESIAN_POINT('Ctrl Pts',(-6.74432341447577,-0.553525682289361,
-48.2769122352947));
#35754=CARTESIAN_POINT('Ctrl Pts',(-6.72993483437743,-0.728840470316843,
-48.268578392602));
#35755=CARTESIAN_POINT('Ctrl Pts',(-6.70868774546245,-0.903818148243271,
-48.2602445499093));
#35756=CARTESIAN_POINT('Ctrl Pts',(-6.68060207070955,-1.07788912826471,
-48.2519107072166));
#35757=CARTESIAN_POINT('Ctrl Pts',(-6.65254949847752,-1.25175494361415,
-48.2435866870119));
#35758=CARTESIAN_POINT('Ctrl Pts',(-6.617674451869,-1.42471584944315,-48.2352626668071));
#35759=CARTESIAN_POINT('Ctrl Pts',(-6.57604873628253,-1.5962055062043,-48.2269386466024));
#35760=CARTESIAN_POINT('Ctrl Pts',(-6.53446444985352,-1.76752448308903,
-48.2186229111115));
#35761=CARTESIAN_POINT('Ctrl Pts',(-6.48614296206281,-1.93737479235349,
-48.2103071756207));
#35762=CARTESIAN_POINT('Ctrl Pts',(-6.43120746594508,-2.10519821631414,
-48.2019914401298));
#35763=CARTESIAN_POINT('Ctrl Pts',(-6.37631658031481,-2.27288535890342,
-48.1936824574498));
#35764=CARTESIAN_POINT('Ctrl Pts',(-6.31482249617295,-2.43854856671804,
-48.1853734747698));
#35765=CARTESIAN_POINT('Ctrl Pts',(-6.24689883491245,-2.60164254777044,
-48.1770644920897));
#35766=CARTESIAN_POINT('Ctrl Pts',(-6.17901789267081,-2.76463395462818,
-48.1687607351526));
#35767=CARTESIAN_POINT('Ctrl Pts',(-6.10471556539651,-2.92505903475394,
-48.1604569782154));
#35768=CARTESIAN_POINT('Ctrl Pts',(-6.02421448818061,-3.08239011164954,
-48.1521532212782));
#35769=CARTESIAN_POINT('Ctrl Pts',(-5.94374609246139,-3.23965731592076,
-48.1438528354662));
#35770=CARTESIAN_POINT('Ctrl Pts',(-5.8570841193892,-3.39383271067024,-48.1355524496542));
#35771=CARTESIAN_POINT('Ctrl Pts',(-5.76449839422093,-3.54441070744128,
-48.1272520638422));
#35772=CARTESIAN_POINT('Ctrl Pts',(-5.67193219297302,-3.69495695123081,
-48.1189534283655));
#35773=CARTESIAN_POINT('Ctrl Pts',(-5.57344491033089,-3.84190701225639,
-48.1106547928889));
#35774=CARTESIAN_POINT('Ctrl Pts',(-5.4693513042428,-3.98478171431981,-48.1023561574123));
#35775=CARTESIAN_POINT('Ctrl Pts',(-5.36526237044381,-4.12765000338693,
-48.0940578944237));
#35776=CARTESIAN_POINT('Ctrl Pts',(-5.25556781958377,-4.2664430170399,-48.0857596314351));
#35777=CARTESIAN_POINT('Ctrl Pts',(-5.14062465315402,-4.40071212139412,
-48.0774613684465));
#35778=CARTESIAN_POINT('Ctrl Pts',(-5.02566756759752,-4.53499748516367,
-48.0691621005737));
#35779=CARTESIAN_POINT('Ctrl Pts',(-4.90546082660754,-4.66475758423433,
-48.0608628327009));
#35780=CARTESIAN_POINT('Ctrl Pts',(-4.78040059868223,-4.78957817726348,
-48.0525635648281));
#35781=CARTESIAN_POINT('Ctrl Pts',(-4.65525255832012,-4.91448641446711,
-48.0442584695316));
#35782=CARTESIAN_POINT('Ctrl Pts',(-4.52524446783627,-5.03444796931389,
-48.035953374235));
#35783=CARTESIAN_POINT('Ctrl Pts',(-4.39080877285501,-5.14908606649952,
-48.0276482789385));
#35784=CARTESIAN_POINT('Ctrl Pts',(-4.25632405562877,-5.26376596669652,
-48.0193401551724));
#35785=CARTESIAN_POINT('Ctrl Pts',(-4.11740878530932,-5.37311832013723,
-48.0110320314063));
#35786=CARTESIAN_POINT('Ctrl Pts',(-3.97452730659566,-5.47680761841471,
-48.0027239076402));
#35787=CARTESIAN_POINT('Ctrl Pts',(-3.83149394569557,-5.58060713781724,
-47.9944069523865));
#35788=CARTESIAN_POINT('Ctrl Pts',(-3.68448623877602,-5.678731376263,-47.9860899971329));
#35789=CARTESIAN_POINT('Ctrl Pts',(-3.53399714727165,-5.77088842060526,
-47.9777730418792));
#35790=CARTESIAN_POINT('Ctrl Pts',(-3.42308897646928,-5.83880676014987,
-47.9716435723967));
#35791=CARTESIAN_POINT('Ctrl Pts',(-3.31029048939629,-5.90348495750656,
-47.9655141029141));
#35792=CARTESIAN_POINT('Ctrl Pts',(-3.19580695641193,-5.96482245312877,
-47.9593846334316));
#35793=CARTESIAN_POINT('Ctrl Pts',(-3.03796245889818,-6.04939170010127,
-47.9509336099064));
#35794=CARTESIAN_POINT('Ctrl Pts',(-2.87662549678967,-6.1277632259886,-47.9424825863812));
#35795=CARTESIAN_POINT('Ctrl Pts',(-2.71230981342227,-6.19965035110959,
-47.9340315628561));
#35796=CARTESIAN_POINT('Ctrl Pts',(-2.54813880513028,-6.27147418175354,
-47.9255879802059));
#35797=CARTESIAN_POINT('Ctrl Pts',(-2.38099460535192,-6.33682485914442,
-47.9171443975558));
#35798=CARTESIAN_POINT('Ctrl Pts',(-2.21141483392661,-6.3954619404926,-47.9087008149056));
#35799=CARTESIAN_POINT('Ctrl Pts',(-2.04196131992396,-6.45405536470702,
-47.9002635187658));
#35800=CARTESIAN_POINT('Ctrl Pts',(-1.87007616138224,-6.50594504914093,
-47.891826222626));
#35801=CARTESIAN_POINT('Ctrl Pts',(-1.69631657254045,-6.55093879422825,
-47.8833889264862));
#35802=CARTESIAN_POINT('Ctrl Pts',(-1.52268094791664,-6.59590043970909,
-47.8749576497138));
#35803=CARTESIAN_POINT('Ctrl Pts',(-1.34717388051281,-6.63397587616908,
-47.8665263729415));
#35804=CARTESIAN_POINT('Ctrl Pts',(-1.1703675485453,-6.66502279075714,-47.8580950961691));
#35805=CARTESIAN_POINT('Ctrl Pts',(-0.99363700217148,-6.69605639751381,
-47.8496674333472));
#35806=CARTESIAN_POINT('Ctrl Pts',(-0.815608627353799,-6.7200674310835,
-47.8412397705252));
#35807=CARTESIAN_POINT('Ctrl Pts',(-0.636865241733313,-6.73696457344641,
-47.8328121077033));
#35808=CARTESIAN_POINT('Ctrl Pts',(-0.458176880396861,-6.75385651420056,
-47.8243870392493));
#35809=CARTESIAN_POINT('Ctrl Pts',(-0.278774276837421,-6.76363889987786,
-47.8159619707953));
#35810=CARTESIAN_POINT('Ctrl Pts',(-0.0992461976646876,-6.76627217840438,
-47.8075369023414));
#35811=CARTESIAN_POINT('Ctrl Pts',(-0.0501218199894398,-6.76699272401182,
-47.8052315457276));
#35812=CARTESIAN_POINT('Ctrl Pts',(-0.000988069017895526,-6.76717828963977,
-47.8029261891139));
#35813=CARTESIAN_POINT('Ctrl Pts',(0.0481429585539462,-6.76682874436332,
-47.8006208325001));
#35814=CARTESIAN_POINT('Ctrl Pts',(0.231828103105414,-6.76552190675368,
-47.7920018439757));
#35815=CARTESIAN_POINT('Ctrl Pts',(0.415393127712019,-6.75673202860711,
-47.7833828554512));
#35816=CARTESIAN_POINT('Ctrl Pts',(0.598223281609024,-6.74050576035218,
-47.7747638669267));
#35817=CARTESIAN_POINT('Ctrl Pts',(0.781162967084149,-6.72426977111452,
-47.7661397148589));
#35818=CARTESIAN_POINT('Ctrl Pts',(0.963366600276988,-6.70058852771357,
-47.7575155627911));
#35819=CARTESIAN_POINT('Ctrl Pts',(1.14422588387882,-6.6695604147996,-47.7488914107233));
#35820=CARTESIAN_POINT('Ctrl Pts',(1.33127964660014,-6.6374695806709,-47.7399718791271));
#35821=CARTESIAN_POINT('Ctrl Pts',(1.51689498925224,-6.59751977075137,-47.7310523475308));
#35822=CARTESIAN_POINT('Ctrl Pts',(1.70041251574297,-6.54987681382671,-47.7221328159346));
#35823=CARTESIAN_POINT('Ctrl Pts',(1.87818321959255,-6.50372578864709,-47.7134925980753));
#35824=CARTESIAN_POINT('Ctrl Pts',(2.05398522635387,-6.45035627683088,-47.7048523802161));
#35825=CARTESIAN_POINT('Ctrl Pts',(2.2272360036432,-6.38996938835199,-47.6962121623568));
#35826=CARTESIAN_POINT('Ctrl Pts',(2.40888784028563,-6.32665429463097,-47.6871529738921));
#35827=CARTESIAN_POINT('Ctrl Pts',(2.58773451367977,-6.25562449231842,-47.6780937854274));
#35828=CARTESIAN_POINT('Ctrl Pts',(2.76312921036194,-6.17716811871302,-47.6690345969626));
#35829=CARTESIAN_POINT('Ctrl Pts',(2.93852390704411,-6.09871174510763,-47.6599754084979));
#35830=CARTESIAN_POINT('Ctrl Pts',(3.11046629951489,-6.01282900082008,-47.6509162200332));
#35831=CARTESIAN_POINT('Ctrl Pts',(3.27833978119587,-5.9198629442774,-47.6418570315685));
#35832=CARTESIAN_POINT('Ctrl Pts',(3.44592243384757,-5.82705794490533,-47.6328135375122));
#35833=CARTESIAN_POINT('Ctrl Pts',(3.60960505752249,-5.72710939950069,-47.6237700434559));
#35834=CARTESIAN_POINT('Ctrl Pts',(3.76880665731814,-5.62035455996813,-47.6147265493996));
#35835=CARTESIAN_POINT('Ctrl Pts',(3.9278626359926,-5.51369736869691,-47.6056913273943));
#35836=CARTESIAN_POINT('Ctrl Pts',(4.0824455764349,-5.40024644540185,-47.596656105389));
#35837=CARTESIAN_POINT('Ctrl Pts',(4.23200253835245,-5.28038289476989,-47.5876208833837));
#35838=CARTESIAN_POINT('Ctrl Pts',(4.38129601346128,-5.16073051762015,-47.5786015794725));
#35839=CARTESIAN_POINT('Ctrl Pts',(4.52558100619863,-5.03468822184525,-47.5695822755614));
#35840=CARTESIAN_POINT('Ctrl Pts',(4.66433690647915,-4.90267786243972,-47.5605629716503));
#35841=CARTESIAN_POINT('Ctrl Pts',(4.80291872779106,-4.77083311925062,-47.551554983086));
#35842=CARTESIAN_POINT('Ctrl Pts',(4.93598512779966,-4.63303541823355,-47.5425469945216));
#35843=CARTESIAN_POINT('Ctrl Pts',(5.06304974969824,-4.48974567565698,-47.5335390059572));
#35844=CARTESIAN_POINT('Ctrl Pts',(5.18982739169751,-4.34677955798311,-47.5245513622505));
#35845=CARTESIAN_POINT('Ctrl Pts',(5.31063015538514,-4.1983463360139,-47.5155637185439));
#35846=CARTESIAN_POINT('Ctrl Pts',(5.42500992892582,-4.04494206028422,-47.5065760748372));
#35847=CARTESIAN_POINT('Ctrl Pts',(5.52462678399769,-3.91133756860077,-47.4987484601039));
#35848=CARTESIAN_POINT('Ctrl Pts',(5.61937212936148,-3.77396307825581,-47.4909208453705));
#35849=CARTESIAN_POINT('Ctrl Pts',(5.7089732071335,-3.63316857855946,-47.4830932306371));
#35850=CARTESIAN_POINT('Ctrl Pts',(5.80195731230526,-3.4870581645678,-47.4749700721918));
#35851=CARTESIAN_POINT('Ctrl Pts',(5.88935838056739,-3.33732902469527,-47.4668469137465));
#35852=CARTESIAN_POINT('Ctrl Pts',(5.97089090122295,-3.18445456015517,-47.4587237553012));
#35853=CARTESIAN_POINT('Ctrl Pts',(6.05241767340907,-3.03159087406493,-47.4506011695811));
#35854=CARTESIAN_POINT('Ctrl Pts',(6.12807654991875,-2.87558262799833,-47.442478583861));
#35855=CARTESIAN_POINT('Ctrl Pts',(6.19762784291046,-2.71692806691327,-47.4343559981409));
#35856=CARTESIAN_POINT('Ctrl Pts',(6.26718749320598,-2.55825444184951,-47.4262324364085));
#35857=CARTESIAN_POINT('Ctrl Pts',(6.33063795278142,-2.39693420429176,-47.4181088746761));
#35858=CARTESIAN_POINT('Ctrl Pts',(6.38778758873765,-2.2334857781435,-47.4099853129437));
#35859=CARTESIAN_POINT('Ctrl Pts',(6.44497885142188,-2.06991829921278,-47.4018558341606));
#35860=CARTESIAN_POINT('Ctrl Pts',(6.49586000331293,-1.90421988153315,-47.3937263553775));
#35861=CARTESIAN_POINT('Ctrl Pts',(6.54028904416195,-1.73692493183075,-47.3855968765943));
#35862=CARTESIAN_POINT('Ctrl Pts',(6.58473619794893,-1.56956177892189,-47.3774640835658));
#35863=CARTESIAN_POINT('Ctrl Pts',(6.62272591726439,-1.40060115345188,-47.3693312905373));
#35864=CARTESIAN_POINT('Ctrl Pts',(6.65416734963562,-1.23058761697138,-47.3611984975087));
#35865=CARTESIAN_POINT('Ctrl Pts',(6.68564296979464,-1.06038921656236,-47.3530568613016));
#35866=CARTESIAN_POINT('Ctrl Pts',(6.71055602893938,-0.889135980215188,
-47.3449152250944));
#35867=CARTESIAN_POINT('Ctrl Pts',(6.72886746579591,-0.717378301702387,
-47.3367735888873));
#35868=CARTESIAN_POINT('Ctrl Pts',(6.73819689415205,-0.629870097465948,
-47.3326255358267));
#35869=CARTESIAN_POINT('Ctrl Pts',(6.74581353386546,-0.542230982593186,
-47.3284774827661));
#35870=CARTESIAN_POINT('Ctrl Pts',(6.7517174208235,-0.454533683403681,-47.3243294297055));
#35871=CARTESIAN_POINT('Ctrl Pts',(6.76373101523702,-0.276081793807462,
-47.3158887147275));
#35872=CARTESIAN_POINT('Ctrl Pts',(6.76867427935843,-0.0970214736078914,
-47.3074479997494));
#35873=CARTESIAN_POINT('Ctrl Pts',(6.76650240531966,0.0820621642614203,
-47.2990072847713));
#35874=CARTESIAN_POINT('Ctrl Pts',(6.76433217288562,0.261010442279826,-47.2905729496833));
#35875=CARTESIAN_POINT('Ctrl Pts',(6.75505752695338,0.439981670637915,-47.2821386145952));
#35876=CARTESIAN_POINT('Ctrl Pts',(6.73868567038815,0.618388579863343,-47.2737042795072));
#35877=CARTESIAN_POINT('Ctrl Pts',(6.72232367435799,0.796688037158855,-47.2652750242986));
#35878=CARTESIAN_POINT('Ctrl Pts',(6.69887302004291,0.974423521735699,-47.25684576909));
#35879=CARTESIAN_POINT('Ctrl Pts',(6.66839292568548,1.15101033386669,-47.2484165138813));
#35880=CARTESIAN_POINT('Ctrl Pts',(6.63792651363609,1.32751787737294,-47.2399910425083));
#35881=CARTESIAN_POINT('Ctrl Pts',(6.60043700983284,1.50287744853693,-47.2315655711353));
#35882=CARTESIAN_POINT('Ctrl Pts',(6.55603521757861,1.67651162413774,-47.2231400997623));
#35883=CARTESIAN_POINT('Ctrl Pts',(6.51164655178232,1.85009446843894,-47.2147171192031));
#35884=CARTESIAN_POINT('Ctrl Pts',(6.46034975520118,2.021952611711,-47.2062941386438));
#35885=CARTESIAN_POINT('Ctrl Pts',(6.40230635471168,2.19152055441387,-47.1978711580846));
#35886=CARTESIAN_POINT('Ctrl Pts',(6.34426199314389,2.36109130481006,-47.1894480380582));
#35887=CARTESIAN_POINT('Ctrl Pts',(6.27947090616957,2.5283714613647,-47.1810249180319));
#35888=CARTESIAN_POINT('Ctrl Pts',(6.20814416355303,2.6928117358149,-47.1726017980056));
#35889=CARTESIAN_POINT('Ctrl Pts',(6.13681495433881,2.85725769688395,-47.1641783866937));
#35890=CARTESIAN_POINT('Ctrl Pts',(6.05894977139855,3.01886327400483,-47.1557549753819));
#35891=CARTESIAN_POINT('Ctrl Pts',(5.97480747411099,3.17710003734655,-47.14733156407));
#35892=CARTESIAN_POINT('Ctrl Pts',(5.89065053216109,3.33536434122428,-47.1389066866939));
#35893=CARTESIAN_POINT('Ctrl Pts',(5.80021445429574,3.4902583679092,-47.1304818093178));
#35894=CARTESIAN_POINT('Ctrl Pts',(5.7038037863806,3.64127880921941,-47.1220569319417));
#35895=CARTESIAN_POINT('Ctrl Pts',(5.60736288849981,3.79234660361671,-47.1136294129102));
#35896=CARTESIAN_POINT('Ctrl Pts',(5.50494384497838,3.93953811011377,-47.1052018938788));
#35897=CARTESIAN_POINT('Ctrl Pts',(5.39689439782721,4.08237919094997,-47.0967743748474));
#35898=CARTESIAN_POINT('Ctrl Pts',(5.28874805610789,4.22534836614671,-47.0883392983426));
#35899=CARTESIAN_POINT('Ctrl Pts',(5.17496142325378,4.36395905411746,-47.0799042218378));
#35900=CARTESIAN_POINT('Ctrl Pts',(5.0559231066275,4.49776950719689,-47.071469145333));
#35901=CARTESIAN_POINT('Ctrl Pts',(4.93682725799934,4.63164463174897,-47.0630299921003));
#35902=CARTESIAN_POINT('Ctrl Pts',(4.81247489104588,4.76071465088317,-47.0545908388675));
#35903=CARTESIAN_POINT('Ctrl Pts',(4.68329168001268,4.8845744993729,-47.0461516856347));
#35904=CARTESIAN_POINT('Ctrl Pts',(4.55396491021281,5.008571990881,-47.0377031541366));
#35905=CARTESIAN_POINT('Ctrl Pts',(4.41979681578023,5.1273475177224,-47.0292546226385));
#35906=CARTESIAN_POINT('Ctrl Pts',(4.28124727649392,5.240535350278,-47.0208060911404));
#35907=CARTESIAN_POINT('Ctrl Pts',(4.20469416078772,5.30307530015296,-47.0161380033744));
#35908=CARTESIAN_POINT('Ctrl Pts',(4.126803981546,5.36391010883663,-47.0114699156085));
#35909=CARTESIAN_POINT('Ctrl Pts',(4.04765813864944,5.42298373523515,-47.0068018278425));
#35910=CARTESIAN_POINT('Ctrl Pts',(3.90790280804022,5.5272956470863,-46.9985589419856));
#35911=CARTESIAN_POINT('Ctrl Pts',(3.76391957585603,5.62634572550133,-46.9903160561287));
#35912=CARTESIAN_POINT('Ctrl Pts',(3.61613986786052,5.71977459836222,-46.9820731702718));
#35913=CARTESIAN_POINT('Ctrl Pts',(3.46854919040335,5.81308396286589,-46.9738408281978));
#35914=CARTESIAN_POINT('Ctrl Pts',(3.31717201017708,5.90078625774799,-46.9656084861237));
#35915=CARTESIAN_POINT('Ctrl Pts',(3.16247180109459,5.98256308844976,-46.9573761440496));
#35916=CARTESIAN_POINT('Ctrl Pts',(3.14140421151363,5.99369972954853,-46.9562550362946));
#35917=CARTESIAN_POINT('Ctrl Pts',(3.12027504089109,6.00472654081099,-46.9551339285396));
#35918=CARTESIAN_POINT('Ctrl Pts',(3.0990855038472,6.01564277861013,-46.9540128207846));
#35919=CARTESIAN_POINT('Ctrl Pts',(3.09908550384721,6.01564277861012,-48.954361679463));
#35920=CARTESIAN_POINT('Ctrl Pts',(2.93076068015984,6.10235886868149,-48.9454271409862));
#35921=CARTESIAN_POINT('Ctrl Pts',(2.75891733807477,6.18194282230756,-48.9364926025095));
#35922=CARTESIAN_POINT('Ctrl Pts',(2.5841629993212,6.25414986972164,-48.9275580640327));
#35923=CARTESIAN_POINT('Ctrl Pts',(2.48251516857192,6.29614991267796,-48.9223611890287));
#35924=CARTESIAN_POINT('Ctrl Pts',(2.37988278964582,6.33565504789918,-48.9171643140247));
#35925=CARTESIAN_POINT('Ctrl Pts',(2.2763878057268,6.3726248562063,-48.9119674390207));
#35926=CARTESIAN_POINT('Ctrl Pts',(2.11260859236491,6.43112900677864,-48.9037434646031));
#35927=CARTESIAN_POINT('Ctrl Pts',(1.94635542308809,6.48339286898614,-48.8955194901855));
#35928=CARTESIAN_POINT('Ctrl Pts',(1.77814436547817,6.52920298470788,-48.887295515768));
#35929=CARTESIAN_POINT('Ctrl Pts',(1.61011095506566,6.57496472050272,-48.8790802266653));
#35930=CARTESIAN_POINT('Ctrl Pts',(1.44012411697685,6.61428618887802,-48.8708649375627));
#35931=CARTESIAN_POINT('Ctrl Pts',(1.26871845079435,6.64700251937774,-48.86264964846));
#35932=CARTESIAN_POINT('Ctrl Pts',(1.09745942530239,6.67969086045679,-48.8544413876878));
#35933=CARTESIAN_POINT('Ctrl Pts',(0.924784339437631,6.70578525098115,-48.8462331269156));
#35934=CARTESIAN_POINT('Ctrl Pts',(0.751241552077881,6.72517101124065,-48.8380248661435));
#35935=CARTESIAN_POINT('Ctrl Pts',(0.577812434683422,6.74454407388979,-48.8298219817556));
#35936=CARTESIAN_POINT('Ctrl Pts',(0.403517102976043,6.75721721925584,-48.8216190973677));
#35937=CARTESIAN_POINT('Ctrl Pts',(0.228912767094718,6.76312708331442,-48.8134162129798));
#35938=CARTESIAN_POINT('Ctrl Pts',(0.0543877917091412,6.76903426124417,
-48.8052170569356));
#35939=CARTESIAN_POINT('Ctrl Pts',(-0.120445550391488,6.76818427001214,
-48.7970179008914));
#35940=CARTESIAN_POINT('Ctrl Pts',(-0.295026193065019,6.7605656971444,-48.7888187448472));
#35941=CARTESIAN_POINT('Ctrl Pts',(-0.469591651468012,6.75294778690724,
-48.7806203019302));
#35942=CARTESIAN_POINT('Ctrl Pts',(-0.643904095868667,6.73856247474029,
-48.7724218590132));
#35943=CARTESIAN_POINT('Ctrl Pts',(-0.817403357264144,6.71745046513432,
-48.7642234160962));
#35944=CARTESIAN_POINT('Ctrl Pts',(-0.990900890812345,6.69633866577898,
-48.7560250548259));
#35945=CARTESIAN_POINT('Ctrl Pts',(-1.16358490128616,6.66850034469401,-48.7478266935557));
#35946=CARTESIAN_POINT('Ctrl Pts',(-1.33490135257533,6.63402799051169,-48.7396283322855));
#35947=CARTESIAN_POINT('Ctrl Pts',(-1.50624721861559,6.59954971748322,-48.7314285633702));
#35948=CARTESIAN_POINT('Ctrl Pts',(-1.67622470600697,6.55843521279149,-48.7232287944549));
#35949=CARTESIAN_POINT('Ctrl Pts',(-1.84429091263455,6.5108279066163,-48.7150290255396));
#35950=CARTESIAN_POINT('Ctrl Pts',(-2.01241650669963,6.46320377804728,-48.7068263591753));
#35951=CARTESIAN_POINT('Ctrl Pts',(-2.1786291297559,6.40908237545152,-48.698623692811));
#35952=CARTESIAN_POINT('Ctrl Pts',(-2.34240190550047,6.34865673297177,-48.6904210264467));
#35953=CARTESIAN_POINT('Ctrl Pts',(-2.50636068618298,6.28816246206567,-48.6822090439037));
#35954=CARTESIAN_POINT('Ctrl Pts',(-2.66787374666015,6.22134977120187,-48.6739970613607));
#35955=CARTESIAN_POINT('Ctrl Pts',(-2.82643406458156,6.14845992737799,-48.6657850788177));
#35956=CARTESIAN_POINT('Ctrl Pts',(-2.98508790352148,6.07552709213909,-48.6575682527364));
#35957=CARTESIAN_POINT('Ctrl Pts',(-3.1407852090137,5.99651012103758,-48.6493514266551));
#35958=CARTESIAN_POINT('Ctrl Pts',(-3.29304448913009,5.91169577977504,-48.6411346005738));
#35959=CARTESIAN_POINT('Ctrl Pts',(-3.44553857504676,5.82675064254879,-48.6329051029599));
#35960=CARTESIAN_POINT('Ctrl Pts',(-3.59458373427576,5.73599045547337,-48.6246756053461));
#35961=CARTESIAN_POINT('Ctrl Pts',(-3.73972723282283,5.63974549284658,-48.6164461077323));
#35962=CARTESIAN_POINT('Ctrl Pts',(-3.86910196305317,5.55395683403295,-48.6091106842074));
#35963=CARTESIAN_POINT('Ctrl Pts',(-3.99537705743535,5.46381111992917,-48.6017752606825));
#35964=CARTESIAN_POINT('Ctrl Pts',(-4.11825527025049,5.36956818832335,-48.5944398371577));
#35965=CARTESIAN_POINT('Ctrl Pts',(-4.25206793835219,5.26693894397657,-48.586451662761));
#35966=CARTESIAN_POINT('Ctrl Pts',(-4.38230611285813,5.15910143668588,-48.5784634883643));
#35967=CARTESIAN_POINT('Ctrl Pts',(-4.50852037101767,5.04633858001212,-48.5704753139677));
#35968=CARTESIAN_POINT('Ctrl Pts',(-4.63457795032364,4.93371570399797,-48.5624970558675));
#35969=CARTESIAN_POINT('Ctrl Pts',(-4.7566212692965,4.81617988999997,-48.5545187977673));
#35970=CARTESIAN_POINT('Ctrl Pts',(-4.87422961755164,4.69405737453031,-48.5465405396672));
#35971=CARTESIAN_POINT('Ctrl Pts',(-4.99171865488284,4.57205874950186,-48.5385703753236));
#35972=CARTESIAN_POINT('Ctrl Pts',(-5.10478141064177,4.44548295121236,-48.53060021098));
#35973=CARTESIAN_POINT('Ctrl Pts',(-5.21303020169676,4.31469641066408,-48.5226300466365));
#35974=CARTESIAN_POINT('Ctrl Pts',(-5.32119366389288,4.18401296471992,-48.5146661649038));
#35975=CARTESIAN_POINT('Ctrl Pts',(-5.42455047063288,4.0491256722081,-48.5067022831711));
#35976=CARTESIAN_POINT('Ctrl Pts',(-5.52274993362333,3.91043759324497,-48.4987384014383));
#35977=CARTESIAN_POINT('Ctrl Pts',(-5.62340782270726,3.76827745464124,-48.4905751437207));
#35978=CARTESIAN_POINT('Ctrl Pts',(-5.71864645666591,3.6221240072378,-48.482411886003));
#35979=CARTESIAN_POINT('Ctrl Pts',(-5.80813185606154,3.47244774512204,-48.4742486282853));
#35980=CARTESIAN_POINT('Ctrl Pts',(-5.89536366442474,3.32654091449287,-48.4662909532047));
#35981=CARTESIAN_POINT('Ctrl Pts',(-5.97712833485484,3.17728692360154,-48.4583332781241));
#35982=CARTESIAN_POINT('Ctrl Pts',(-6.05316052074016,3.02515069213961,-48.4503756030435));
#35983=CARTESIAN_POINT('Ctrl Pts',(-6.12918825432945,2.87302336947769,-48.4424183939488));
#35984=CARTESIAN_POINT('Ctrl Pts',(-6.19948400072992,2.71801448226019,-48.434461184854));
#35985=CARTESIAN_POINT('Ctrl Pts',(-6.26382885480873,2.56061263717603,-48.4265039757593));
#35986=CARTESIAN_POINT('Ctrl Pts',(-6.3281830729576,2.40318788549077,-48.4185456086565));
#35987=CARTESIAN_POINT('Ctrl Pts',(-6.38658453224515,2.24336983552793,-48.4105872415536));
#35988=CARTESIAN_POINT('Ctrl Pts',(-6.43886295915178,2.08166586974548,-48.4026288744508));
#35989=CARTESIAN_POINT('Ctrl Pts',(-6.49349979164998,1.91266704909369,-48.3943114862644));
#35990=CARTESIAN_POINT('Ctrl Pts',(-6.5414481535414,1.74160864021316,-48.385994098078));
#35991=CARTESIAN_POINT('Ctrl Pts',(-6.58257252794975,1.56908505642021,-48.3776767098916));
#35992=CARTESIAN_POINT('Ctrl Pts',(-6.62197743791774,1.40377491165765,-48.3697070826968));
#35993=CARTESIAN_POINT('Ctrl Pts',(-6.65511740779374,1.23712001178683,-48.3617374555019));
#35994=CARTESIAN_POINT('Ctrl Pts',(-6.68192607887337,1.06965081988094,-48.3537678283071));
#35995=CARTESIAN_POINT('Ctrl Pts',(-6.70875183033336,0.902074929754604,
-48.3457931234916));
#35996=CARTESIAN_POINT('Ctrl Pts',(-6.72923820885137,0.733684090666321,
-48.3378184186761));
#35997=CARTESIAN_POINT('Ctrl Pts',(-6.74337090337002,0.565011380047041,
-48.3298437138605));
#35998=CARTESIAN_POINT('Ctrl Pts',(-6.7575215467703,0.396124450793563,-48.321858880967));
#35999=CARTESIAN_POINT('Ctrl Pts',(-6.76530239298436,0.226955312878489,
-48.3138740480734));
#36000=CARTESIAN_POINT('Ctrl Pts',(-6.76675113645843,0.0580349656550752,
-48.3058892151799));
#36001=CARTESIAN_POINT('Ctrl Pts',(-6.76693674636341,0.0363932532619834,
-48.3048662155245));
#36002=CARTESIAN_POINT('Ctrl Pts',(-6.76701848937722,0.0147556145212476,
-48.3038432158692));
#36003=CARTESIAN_POINT('Ctrl Pts',(-6.76699650576387,-0.00687684372454104,
-48.3028202162139));
#36004=CARTESIAN_POINT('',(-6.76728246533827,-0.0010053267103838,-48.6966910258876));
#36005=CARTESIAN_POINT('Ctrl Pts',(3.0990855038472,6.01564277861013,-49.3486032095739));
#36006=CARTESIAN_POINT('Ctrl Pts',(2.93373232018331,6.10082796552479,-49.3398537616746));
#36007=CARTESIAN_POINT('Ctrl Pts',(2.7648650214443,6.17919158180189,-49.3311043137754));
#36008=CARTESIAN_POINT('Ctrl Pts',(2.59305716434358,6.25046746591377,-49.3223548658761));
#36009=CARTESIAN_POINT('Ctrl Pts',(2.42125069459287,6.32174277447223,-49.3136054886286));
#36010=CARTESIAN_POINT('Ctrl Pts',(2.24650397871061,6.38593035557825,-49.3048561113812));
#36011=CARTESIAN_POINT('Ctrl Pts',(2.06941053323773,6.44281220003538,-49.2961067341338));
#36012=CARTESIAN_POINT('Ctrl Pts',(1.89231845896684,6.49969360406685,-49.2873574246312));
#36013=CARTESIAN_POINT('Ctrl Pts',(1.71287996431505,6.54926929700881,-49.2786081151286));
#36014=CARTESIAN_POINT('Ctrl Pts',(1.53170449173504,6.59137090065479,-49.269858805626));
#36015=CARTESIAN_POINT('Ctrl Pts',(1.35053036178169,6.63347219230084,-49.2611095609614));
#36016=CARTESIAN_POINT('Ctrl Pts',(1.16761955878841,6.66809944062455,-49.2523603162968));
#36017=CARTESIAN_POINT('Ctrl Pts',(0.983593309310438,6.69513503985392,-49.2436110716323));
#36018=CARTESIAN_POINT('Ctrl Pts',(0.799568362459991,6.72217044771214,-49.2348618888991));
#36019=CARTESIAN_POINT('Ctrl Pts',(0.614428268438663,6.74161427235976,-49.2261127061659));
#36020=CARTESIAN_POINT('Ctrl Pts',(0.428801816330396,6.75340047696801,-49.2173635234327));
#36021=CARTESIAN_POINT('Ctrl Pts',(0.243176616522864,6.76518660206242,-49.2086143997246));
#36022=CARTESIAN_POINT('Ctrl Pts',(0.0570653511654939,6.76931519233997,
-49.1998652760165));
#36023=CARTESIAN_POINT('Ctrl Pts',(-0.128899900800044,6.76577222610795,
-49.1911161523083));
#36024=CARTESIAN_POINT('Ctrl Pts',(-0.314863959941968,6.76222928260133,
-49.1823670847191));
#36025=CARTESIAN_POINT('Ctrl Pts',(-0.500681721080561,6.75101488651277,
-49.1736180171298));
#36026=CARTESIAN_POINT('Ctrl Pts',(-0.685722110173113,6.73216712415993,
-49.1648689495406));
#36027=CARTESIAN_POINT('Ctrl Pts',(-0.870761373827375,6.71331947644148,
-49.1561199351642));
#36028=CARTESIAN_POINT('Ctrl Pts',(-1.05502298984314,6.68683858440001,-49.1473709207878));
#36029=CARTESIAN_POINT('Ctrl Pts',(-1.23788117676026,6.65281438131432,-49.1386219064115));
#36030=CARTESIAN_POINT('Ctrl Pts',(-1.43009641451763,6.61704912302384,-49.1294251955239));
#36031=CARTESIAN_POINT('Ctrl Pts',(-1.62076048992669,6.57294837083172,-49.1202284846364));
#36032=CARTESIAN_POINT('Ctrl Pts',(-1.80915798961109,6.52067760042056,-49.1110317737489));
#36033=CARTESIAN_POINT('Ctrl Pts',(-1.98840443002984,6.47094578577417,-49.1022817760424));
#36034=CARTESIAN_POINT('Ctrl Pts',(-2.16559895952159,6.41381888474486,-49.0935317783359));
#36035=CARTESIAN_POINT('Ctrl Pts',(-2.34013966242285,6.34949095285248,-49.0847817806294));
#36036=CARTESIAN_POINT('Ctrl Pts',(-2.51467682553977,6.285164325567,-49.0760319603778));
#36037=CARTESIAN_POINT('Ctrl Pts',(-2.68656000078803,6.21363705879677,-49.0672821401262));
#36038=CARTESIAN_POINT('Ctrl Pts',(-2.85520533840849,6.13515211510877,-49.0585323198746));
#36039=CARTESIAN_POINT('Ctrl Pts',(-3.02384747998281,6.05666865881144,-49.0497826654434));
#36040=CARTESIAN_POINT('Ctrl Pts',(-3.18925164684485,5.97122791039871,-49.0410330110121));
#36041=CARTESIAN_POINT('Ctrl Pts',(-3.350856018291,5.87912008251941,-49.0322833565809));
#36042=CARTESIAN_POINT('Ctrl Pts',(-3.5124575419136,5.78701387778209,-49.0235338563377));
#36043=CARTESIAN_POINT('Ctrl Pts',(-3.67025915510879,5.68824097061019,-49.0147843560946));
#36044=CARTESIAN_POINT('Ctrl Pts',(-3.82372487928777,5.58313684656894,-49.0060348558514));
#36045=CARTESIAN_POINT('Ctrl Pts',(-3.97718810300748,5.4780344350181,-48.9972854981663));
#36046=CARTESIAN_POINT('Ctrl Pts',(-4.12631534262981,5.3666011749641,-48.9885361404812));
#36047=CARTESIAN_POINT('Ctrl Pts',(-4.27060009886187,5.24921554097382,-48.9797867827961));
#36048=CARTESIAN_POINT('Ctrl Pts',(-4.41488269594177,5.13183166360322,-48.9710375560409));
#36049=CARTESIAN_POINT('Ctrl Pts',(-4.55432273235054,5.00849577139502,-48.9622883292857));
#36050=CARTESIAN_POINT('Ctrl Pts',(-4.68844662480174,4.87962675277374,-48.9535391025305));
#36051=CARTESIAN_POINT('Ctrl Pts',(-4.8225686883511,4.75075949139929,-48.9447899950791));
#36052=CARTESIAN_POINT('Ctrl Pts',(-4.951374546378,4.61635945312591,-48.9360408876276));
#36053=CARTESIAN_POINT('Ctrl Pts',(-5.07442674461004,4.47688309134675,-48.9272917801761));
#36054=CARTESIAN_POINT('Ctrl Pts',(-5.19747742838482,4.3374084461642,-48.9185427804037));
#36055=CARTESIAN_POINT('Ctrl Pts',(-5.31477440450887,4.19285781736081,-48.9097937806313));
#36056=CARTESIAN_POINT('Ctrl Pts',(-5.42591931531128,4.0437221199944,-48.9010447808589));
#36057=CARTESIAN_POINT('Ctrl Pts',(-5.53707636462958,3.89457013500834,-48.8922948255784));
#36058=CARTESIAN_POINT('Ctrl Pts',(-5.64207983273449,3.74083230916453,-48.8835448702978));
#36059=CARTESIAN_POINT('Ctrl Pts',(-5.74057303468728,3.58303087251859,-48.8747949150172));
#36060=CARTESIAN_POINT('Ctrl Pts',(-5.83906243363747,3.42523552887462,-48.8660452975884));
#36061=CARTESIAN_POINT('Ctrl Pts',(-5.93104191768408,3.26337713157024,-48.8572956801596));
#36062=CARTESIAN_POINT('Ctrl Pts',(-6.0161990669964,3.09800545291187,-48.8485460627308));
#36063=CARTESIAN_POINT('Ctrl Pts',(-6.10135338095371,2.9326392803962,-48.8397967366254));
#36064=CARTESIAN_POINT('Ctrl Pts',(-6.17968568352831,2.76376031540242,-48.83104741052));
#36065=CARTESIAN_POINT('Ctrl Pts',(-6.25092992694882,2.59194213831553,-48.8222980844146));
#36066=CARTESIAN_POINT('Ctrl Pts',(-6.32217217691094,2.42012876880843,-48.8135490031208));
#36067=CARTESIAN_POINT('Ctrl Pts',(-6.38632665483837,2.24537661647707,-48.804799921827));
#36068=CARTESIAN_POINT('Ctrl Pts',(-6.44317547869334,2.06827917621507,-48.7960508405332));
#36069=CARTESIAN_POINT('Ctrl Pts',(-6.50002944235921,1.89116572423475,-48.7873009682183));
#36070=CARTESIAN_POINT('Ctrl Pts',(-6.54957634250384,1.71170683289251,-48.7785510959033));
#36071=CARTESIAN_POINT('Ctrl Pts',(-6.59164787708383,1.53051209225419,-48.7698012235883));
#36072=CARTESIAN_POINT('Ctrl Pts',(-6.63371649074997,1.3493299314809,-48.7610519587536));
#36073=CARTESIAN_POINT('Ctrl Pts',(-6.66831071257112,1.16641244174069,-48.7523026939188));
#36074=CARTESIAN_POINT('Ctrl Pts',(-6.69531304840323,0.982380875160711,
-48.743553429084));
#36075=CARTESIAN_POINT('Ctrl Pts',(-6.72231677033035,0.798339861796561,
-48.7348037151283));
#36076=CARTESIAN_POINT('Ctrl Pts',(-6.74172778477883,0.613184940730893,
-48.7260540011727));
#36077=CARTESIAN_POINT('Ctrl Pts',(-6.75348015835513,0.42754502769131,-48.717304287217));
#36078=CARTESIAN_POINT('Ctrl Pts',(-6.76249038365218,0.285219953547609,
-48.7105961194147));
#36079=CARTESIAN_POINT('Ctrl Pts',(-6.76699999999999,0.142609995758117,
-48.7038879516124));
#36080=CARTESIAN_POINT('Ctrl Pts',(-6.767,7.58693081418461E-13,-48.6971797838101));
#36081=CARTESIAN_POINT('Ctrl Pts',(-6.76699917014542,-0.0033513059037753,
-48.6971797838101));
#36082=CARTESIAN_POINT('Ctrl Pts',(-6.76690054123612,-0.202504044116444,
-48.6878331625662));
#36083=CARTESIAN_POINT('Ctrl Pts',(-6.7580062315747,-0.401386650076133,
-48.6784865413224));
#36084=CARTESIAN_POINT('Ctrl Pts',(-6.74041208644594,-0.599277819457265,
-48.6691399200785));
#36085=CARTESIAN_POINT('Ctrl Pts',(-6.72271805758446,-0.798292436924462,
-48.6597402371252));
#36086=CARTESIAN_POINT('Ctrl Pts',(-6.69622519243849,-0.996304175997024,
-48.6503405541718));
#36087=CARTESIAN_POINT('Ctrl Pts',(-6.66108160237869,-1.19259418347239,
-48.6409408712184));
#36088=CARTESIAN_POINT('Ctrl Pts',(-6.6258495783146,-1.38937812771784,-48.6315175352574));
#36089=CARTESIAN_POINT('Ctrl Pts',(-6.58192331598605,-1.58443152368695,
-48.6220941992965));
#36090=CARTESIAN_POINT('Ctrl Pts',(-6.52950170788515,-1.77704711437963,
-48.6126708633355));
#36091=CARTESIAN_POINT('Ctrl Pts',(-6.47693929460969,-1.97018007325028,
-48.603222216162));
#36092=CARTESIAN_POINT('Ctrl Pts',(-6.41583590556948,-2.16086197399059,
-48.5937735689885));
#36093=CARTESIAN_POINT('Ctrl Pts',(-6.34644080315507,-2.34839905724058,
-48.584324921815));
#36094=CARTESIAN_POINT('Ctrl Pts',(-6.30893860751651,-2.44974702187829,
-48.5792187255202));
#36095=CARTESIAN_POINT('Ctrl Pts',(-6.26901565813335,-2.55017688884191,
-48.5741125292255));
#36096=CARTESIAN_POINT('Ctrl Pts',(-6.22671709480138,-2.64958170685644,
-48.5690063329308));
#36097=CARTESIAN_POINT('Ctrl Pts',(-6.15845239278756,-2.81000891161144,
-48.560765557334));
#36098=CARTESIAN_POINT('Ctrl Pts',(-6.0838895322984,-2.96801773399273,-48.5525247817373));
#36099=CARTESIAN_POINT('Ctrl Pts',(-6.00322034728997,-3.12308092464537,
-48.5442840061405));
#36100=CARTESIAN_POINT('Ctrl Pts',(-5.92264051214965,-3.27797236600324,
-48.5360523580961));
#36101=CARTESIAN_POINT('Ctrl Pts',(-5.83596798244575,-3.42992435922279,
-48.5278207100518));
#36102=CARTESIAN_POINT('Ctrl Pts',(-5.7434429857839,-3.57842865920919,-48.5195890620074));
#36103=CARTESIAN_POINT('Ctrl Pts',(-5.65100398176838,-3.72679493943654,
-48.5113650644491));
#36104=CARTESIAN_POINT('Ctrl Pts',(-5.55272353032596,-3.87171960766436,
-48.5031410668909));
#36105=CARTESIAN_POINT('Ctrl Pts',(-5.44888823423283,-4.01271803281006,
-48.4949170693326));
#36106=CARTESIAN_POINT('Ctrl Pts',(-5.34514467702711,-4.15359188529947,
-48.4867003377081));
#36107=CARTESIAN_POINT('Ctrl Pts',(-5.23585626695808,-4.29054612310275,
-48.4784836060836));
#36108=CARTESIAN_POINT('Ctrl Pts',(-5.12135338170287,-4.4231242962097,-48.4702668744591));
#36109=CARTESIAN_POINT('Ctrl Pts',(-5.00690916051487,-4.55563454461031,
-48.4620543525704));
#36110=CARTESIAN_POINT('Ctrl Pts',(-4.88725601683277,-4.68377292493266,
-48.4538418306817));
#36111=CARTESIAN_POINT('Ctrl Pts',(-4.76276539569147,-4.80711501688943,
-48.445629308793));
#36112=CARTESIAN_POINT('Ctrl Pts',(-4.63831640481326,-4.9304158626568,-48.4374195332112));
#36113=CARTESIAN_POINT('Ctrl Pts',(-4.50903341154218,-5.04892336508585,
-48.4292097576294));
#36114=CARTESIAN_POINT('Ctrl Pts',(-4.37532566290722,-5.16224896179035,
-48.4209999820476));
#36115=CARTESIAN_POINT('Ctrl Pts',(-4.31692559205371,-5.21174663821244,
-48.4174141653648));
#36116=CARTESIAN_POINT('Ctrl Pts',(-4.25768187335778,-5.26025623384032,
-48.413828348682));
#36117=CARTESIAN_POINT('Ctrl Pts',(-4.19763070587936,-5.3077476821208,-48.4102425319993));
#36118=CARTESIAN_POINT('Ctrl Pts',(-4.04927500992292,-5.42507474098545,
-48.4013838144775));
#36119=CARTESIAN_POINT('Ctrl Pts',(-3.89614287579507,-5.53606354164227,
-48.3925250969557));
#36120=CARTESIAN_POINT('Ctrl Pts',(-3.73878837613257,-5.64036793821963,
-48.3836663794339));
#36121=CARTESIAN_POINT('Ctrl Pts',(-3.58113949147413,-5.74486747157052,
-48.3747910886745));
#36122=CARTESIAN_POINT('Ctrl Pts',(-3.41925267110229,-5.84265746627009,
-48.3659157979151));
#36123=CARTESIAN_POINT('Ctrl Pts',(-3.25370763711922,-5.93343708251398,
-48.3570405071556));
#36124=CARTESIAN_POINT('Ctrl Pts',(-3.08769241801749,-6.02447453327945,
-48.3481400085748));
#36125=CARTESIAN_POINT('Ctrl Pts',(-2.91799842216406,-6.10846163565813,
-48.3392395099941));
#36126=CARTESIAN_POINT('Ctrl Pts',(-2.74522928430887,-6.18514390912394,
-48.3303390114133));
#36127=CARTESIAN_POINT('Ctrl Pts',(-2.57222626864046,-6.26192998748601,
-48.3214264642156));
#36128=CARTESIAN_POINT('Ctrl Pts',(-2.39614003515011,-6.33139138475548,
-48.312513917018));
#36129=CARTESIAN_POINT('Ctrl Pts',(-2.21759187387818,-6.39332271052459,
-48.3036013698204));
#36130=CARTESIAN_POINT('Ctrl Pts',(-2.03864946082848,-6.45539078670944,
-48.2946691428481));
#36131=CARTESIAN_POINT('Ctrl Pts',(-1.85723449276926,-6.50989544904072,
-48.2857369158759));
#36132=CARTESIAN_POINT('Ctrl Pts',(-1.67398379057515,-6.55668111691362,
-48.2768046889036));
#36133=CARTESIAN_POINT('Ctrl Pts',(-1.50079071597112,-6.60089897566828,
-48.2683627029583));
#36134=CARTESIAN_POINT('Ctrl Pts',(-1.32595815882831,-6.63822229220504,
-48.259920717013));
#36135=CARTESIAN_POINT('Ctrl Pts',(-1.15002994236985,-6.66856207376469,
-48.2514787310677));
#36136=CARTESIAN_POINT('Ctrl Pts',(-0.978645014598349,-6.69811834038228,
-48.2432547566502));
#36137=CARTESIAN_POINT('Ctrl Pts',(-0.805892724177182,-6.72110254673465,
-48.2350307822326));
#36138=CARTESIAN_POINT('Ctrl Pts',(-0.632318095756071,-6.73739288046789,
-48.226806807815));
#36139=CARTESIAN_POINT('Ctrl Pts',(-0.45892677898349,-6.75366601002816,
-48.2185915187124));
#36140=CARTESIAN_POINT('Ctrl Pts',(-0.284715207696388,-6.76325931124833,
-48.2103762296097));
#36141=CARTESIAN_POINT('Ctrl Pts',(-0.110238333290158,-6.76610201740067,
-48.2021609405071));
#36142=CARTESIAN_POINT('Ctrl Pts',(0.0640892729504751,-6.76894229156577,
-48.1939526797349));
#36143=CARTESIAN_POINT('Ctrl Pts',(0.238681373748767,-6.76504346686485,
-48.1857444189627));
#36144=CARTESIAN_POINT('Ctrl Pts',(0.412978067854543,-6.75438658321177,
-48.1775361581905));
#36145=CARTESIAN_POINT('Ctrl Pts',(0.587160598188498,-6.74373667978307,
-48.1693332738027));
#36146=CARTESIAN_POINT('Ctrl Pts',(0.761047750594994,-6.7263375563464,-48.1611303894148));
#36147=CARTESIAN_POINT('Ctrl Pts',(0.934079702202542,-6.70222232620891,
-48.1529275050269));
#36148=CARTESIAN_POINT('Ctrl Pts',(1.10703300798866,-6.67811805683368,-48.1447283489827));
#36149=CARTESIAN_POINT('Ctrl Pts',(1.27913153294253,-6.64730381168794,-48.1365291929385));
#36150=CARTESIAN_POINT('Ctrl Pts',(1.44982056288041,-6.60986454743584,-48.1283300368943));
#36151=CARTESIAN_POINT('Ctrl Pts',(1.62049474702332,-6.57242853948932,-48.1201315939773));
#36152=CARTESIAN_POINT('Ctrl Pts',(1.78975932850531,-6.52836872860921,-48.1119331510603));
#36153=CARTESIAN_POINT('Ctrl Pts',(1.95706941294622,-6.47782126280977,-48.1037347081433));
#36154=CARTESIAN_POINT('Ctrl Pts',(2.12437783117674,-6.42727430040325,-48.095536346873));
#36155=CARTESIAN_POINT('Ctrl Pts',(2.28973144746005,-6.37023991449283,-48.0873379856028));
#36156=CARTESIAN_POINT('Ctrl Pts',(2.45260028837174,-6.30690421882867,-48.0791396243326));
#36157=CARTESIAN_POINT('Ctrl Pts',(2.61549709359384,-6.24355764853039,-48.0709398554173));
#36158=CARTESIAN_POINT('Ctrl Pts',(2.77590793915033,-6.17390774297557,-48.062740086502));
#36159=CARTESIAN_POINT('Ctrl Pts',(2.93332255514403,-6.09818889404742,-48.0545403175867));
#36160=CARTESIAN_POINT('Ctrl Pts',(3.09079279475686,-6.02244328930384,-48.0463376512225));
#36161=CARTESIAN_POINT('Ctrl Pts',(3.24526437273231,-5.9406246246854,-48.0381349848582));
#36162=CARTESIAN_POINT('Ctrl Pts',(3.39625131273346,-5.85301341368327,-48.0299323184939));
#36163=CARTESIAN_POINT('Ctrl Pts',(3.54740973615904,-5.76530269824399,-48.0217203359508));
#36164=CARTESIAN_POINT('Ctrl Pts',(3.6950753043787,-5.67178647330122,-48.0135083534078));
#36165=CARTESIAN_POINT('Ctrl Pts',(3.83878987097631,-5.57278936677942,-48.0052963708648));
#36166=CARTESIAN_POINT('Ctrl Pts',(3.98258920236766,-5.4737338704262,-47.9970795447835));
#36167=CARTESIAN_POINT('Ctrl Pts',(4.12243260009857,-5.36919126298458,-47.9888627187022));
#36168=CARTESIAN_POINT('Ctrl Pts',(4.25789487128543,-5.2595266198662,-47.9806458926209));
#36169=CARTESIAN_POINT('Ctrl Pts',(4.39356604485876,-5.1496928580297,-47.9724163950071));
#36170=CARTESIAN_POINT('Ctrl Pts',(4.52484232066105,-5.03472151177761,-47.9641868973932));
#36171=CARTESIAN_POINT('Ctrl Pts',(4.65133429783418,-4.91501558998457,-47.9559573997794));
#36172=CARTESIAN_POINT('Ctrl Pts',(4.76408385662894,-4.80831483181071,-47.9486219762545));
#36173=CARTESIAN_POINT('Ctrl Pts',(4.87303262295225,-4.69785300333945,-47.9412865527296));
#36174=CARTESIAN_POINT('Ctrl Pts',(4.97793230461094,-4.58393706007301,-47.9339511292047));
#36175=CARTESIAN_POINT('Ctrl Pts',(5.09334918686618,-4.45859994938706,-47.9258802590183));
#36176=CARTESIAN_POINT('Ctrl Pts',(5.20423996285354,-4.32867203111494,-47.9178093888319));
#36177=CARTESIAN_POINT('Ctrl Pts',(5.31020722916382,-4.19451882619881,-47.9097385186455));
#36178=CARTESIAN_POINT('Ctrl Pts',(5.41604262744776,-4.06053256451881,-47.9016776920297));
#36179=CARTESIAN_POINT('Ctrl Pts',(5.51696647882461,-3.92233176741359,-47.8936168654139));
#36180=CARTESIAN_POINT('Ctrl Pts',(5.61261742731917,-3.78031937996687,-47.8855560387981));
#36181=CARTESIAN_POINT('Ctrl Pts',(5.70817032043641,-3.63845257474862,-47.8775034756382));
#36182=CARTESIAN_POINT('Ctrl Pts',(5.79846086110304,-3.49278226184258,-47.8694509124784));
#36183=CARTESIAN_POINT('Ctrl Pts',(5.88316735776083,-3.34374503223219,-47.8613983493185));
#36184=CARTESIAN_POINT('Ctrl Pts',(5.96780556619126,-3.19482795265305,-47.8533522779306));
#36185=CARTESIAN_POINT('Ctrl Pts',(6.04686850722501,-3.04254968146831,-47.8453062065427));
#36186=CARTESIAN_POINT('Ctrl Pts',(6.12007736585327,-2.88737632392635,-47.8372601351548));
#36187=CARTESIAN_POINT('Ctrl Pts',(6.19324321896246,-2.73229412080086,-47.829218790319));
#36188=CARTESIAN_POINT('Ctrl Pts',(6.26056167680664,-2.57432055338884,-47.8211774454831));
#36189=CARTESIAN_POINT('Ctrl Pts',(6.32179957337942,-2.41394680016355,-47.8131361006472));
#36190=CARTESIAN_POINT('Ctrl Pts',(6.3842179481688,-2.25048153444691,-47.8049397434261));
#36191=CARTESIAN_POINT('Ctrl Pts',(6.44031874685477,-2.08452294774335,-47.7967433862051));
#36192=CARTESIAN_POINT('Ctrl Pts',(6.48990612972447,-1.91661353103979,-47.788547028984));
#36193=CARTESIAN_POINT('Ctrl Pts',(6.53854023421086,-1.7519320406359,-47.7805082402755));
#36194=CARTESIAN_POINT('Ctrl Pts',(6.5809089933205,-1.58537442334995,-47.772469451567));
#36195=CARTESIAN_POINT('Ctrl Pts',(6.61687786943182,-1.41746825750119,-47.7644306628585));
#36196=CARTESIAN_POINT('Ctrl Pts',(6.65285059453878,-1.24954412417139,-47.7563910139268));
#36197=CARTESIAN_POINT('Ctrl Pts',(6.68242199468255,-1.08027152013186,-47.748351364995));
#36198=CARTESIAN_POINT('Ctrl Pts',(6.70550864115327,-0.910188366998158,
-47.7403117160633));
#36199=CARTESIAN_POINT('Ctrl Pts',(6.72860232934845,-0.740053336312645,
-47.7322696149351));
#36200=CARTESIAN_POINT('Ctrl Pts',(6.74520727659557,-0.56910763429333,-47.724227513807));
#36201=CARTESIAN_POINT('Ctrl Pts',(6.75529193448963,-0.397894307347293,
-47.7161854126788));
#36202=CARTESIAN_POINT('Ctrl Pts',(6.76571690996615,-0.2209032032943,-47.707871922234));
#36203=CARTESIAN_POINT('Ctrl Pts',(6.76917380210623,-0.0436265318524084,
-47.6995584317893));
#36204=CARTESIAN_POINT('Ctrl Pts',(6.76568623699593,0.133336951082305,-47.6912449413445));
#36205=CARTESIAN_POINT('Ctrl Pts',(6.76230657835816,0.304825122558117,-47.6831886731737));
#36206=CARTESIAN_POINT('Ctrl Pts',(6.75240588539718,0.476018834040483,-47.675132405003));
#36207=CARTESIAN_POINT('Ctrl Pts',(6.73605833460217,0.646380006526059,-47.6670761368322));
#36208=CARTESIAN_POINT('Ctrl Pts',(6.71892786159665,0.824900171598416,-47.6586340352505));
#36209=CARTESIAN_POINT('Ctrl Pts',(6.69471790127608,1.00250561037161,-47.6501919336687));
#36210=CARTESIAN_POINT('Ctrl Pts',(6.66357341775822,1.17859166217401,-47.6417498320869));
#36211=CARTESIAN_POINT('Ctrl Pts',(6.63242893424036,1.35467771397639,-47.6333077305052));
#36212=CARTESIAN_POINT('Ctrl Pts',(6.5943501102287,1.52924394694912,-47.6248656289234));
#36213=CARTESIAN_POINT('Ctrl Pts',(6.54954059514586,1.70170708188466,-47.6164235273417));
#36214=CARTESIAN_POINT('Ctrl Pts',(6.50530051555239,1.87197857003586,-47.6080887072656));
#36215=CARTESIAN_POINT('Ctrl Pts',(6.45435972196866,2.0407416297399,-47.5997538871894));
#36216=CARTESIAN_POINT('Ctrl Pts',(6.39683554788043,2.2074383283284,-47.5914190671133));
#36217=CARTESIAN_POINT('Ctrl Pts',(6.33938031656763,2.37393524077068,-47.5830942363267));
#36218=CARTESIAN_POINT('Ctrl Pts',(6.27535753615828,2.53837039965132,-47.5747694055401));
#36219=CARTESIAN_POINT('Ctrl Pts',(6.20493511043231,2.70019800668846,-47.5664445747535));
#36220=CARTESIAN_POINT('Ctrl Pts',(6.13458417270687,2.861861337475,-47.5581281947623));
#36221=CARTESIAN_POINT('Ctrl Pts',(6.05784667168943,3.02092207337447,-47.549811814771));
#36222=CARTESIAN_POINT('Ctrl Pts',(5.97493975071795,3.17685126741723,-47.5414954347798));
#36223=CARTESIAN_POINT('Ctrl Pts',(5.89211498600623,3.33262594409017,-47.5331872958698));
#36224=CARTESIAN_POINT('Ctrl Pts',(5.80313315337678,3.485274960318,-47.5248791569598));
#36225=CARTESIAN_POINT('Ctrl Pts',(5.70825872939257,3.6342910282906,-47.5165710180499));
#36226=CARTESIAN_POINT('Ctrl Pts',(5.61343847697899,3.78322201079851,-47.5082676229361));
#36227=CARTESIAN_POINT('Ctrl Pts',(5.5127325222,3.92852388502452,-47.4999642278224));
#36228=CARTESIAN_POINT('Ctrl Pts',(5.40645064539748,4.06971502919813,-47.4916608327086));
#36229=CARTESIAN_POINT('Ctrl Pts',(5.30021180577,4.21084900023774,-47.4833607999242));
#36230=CARTESIAN_POINT('Ctrl Pts',(5.18840175188563,4.34787528060164,-47.4750607671397));
#36231=CARTESIAN_POINT('Ctrl Pts',(5.0713729614526,4.48034209473423,-47.4667607343553));
#36232=CARTESIAN_POINT('Ctrl Pts',(4.95437213213938,4.61277725921508,-47.4584626846573));
#36233=CARTESIAN_POINT('Ctrl Pts',(4.83215528170351,4.74065486843714,-47.4501646349593));
#36234=CARTESIAN_POINT('Ctrl Pts',(4.70511458584861,4.86355690149038,-47.4418665852614));
#36235=CARTESIAN_POINT('Ctrl Pts',(4.57805486031474,4.98647734428403,-47.433567292582));
#36236=CARTESIAN_POINT('Ctrl Pts',(4.44617009151387,5.10442047562056,-47.4252679999026));
#36237=CARTESIAN_POINT('Ctrl Pts',(4.3098890796138,5.21700537870393,-47.4169687072233));
#36238=CARTESIAN_POINT('Ctrl Pts',(4.17360043473173,5.32959658757068,-47.4086689497077));
#36239=CARTESIAN_POINT('Ctrl Pts',(4.03291532722172,5.43682875214606,-47.4003691921921));
#36240=CARTESIAN_POINT('Ctrl Pts',(3.88829517179141,5.53836164014446,-47.3920694346765));
#36241=CARTESIAN_POINT('Ctrl Pts',(3.74359164961655,5.63995305709625,-47.3837648927395));
#36242=CARTESIAN_POINT('Ctrl Pts',(3.59494883398991,5.73583843582138,-47.3754603508025));
#36243=CARTESIAN_POINT('Ctrl Pts',(3.44285727499436,5.82572079523371,-47.3671558088655));
#36244=CARTESIAN_POINT('Ctrl Pts',(3.33009239764871,5.89236205594276,-47.3609985923893));
#36245=CARTESIAN_POINT('Ctrl Pts',(3.21543230600807,5.95570426476123,-47.3548413759131));
#36246=CARTESIAN_POINT('Ctrl Pts',(3.0990855038472,6.01564277861013,-47.3486841594369));
#36247=CARTESIAN_POINT('Origin',(0.,0.,-63.6971797838103));
#36248=CARTESIAN_POINT('',(3.0990855038472,6.01564277861013,-44.9542932404068));
#36249=CARTESIAN_POINT('',(3.09908550384718,6.01564277861013,-45.3486032095739));
#36250=CARTESIAN_POINT('',(3.09908550384721,6.01564277861012,-63.6971797838103));
#36251=CARTESIAN_POINT('',(-6.76699445554588,0.00866248297634946,-46.3028202161574));
#36252=CARTESIAN_POINT('Ctrl Pts',(-6.76699445554588,0.00866248297634946,
-46.3028202161574));
#36253=CARTESIAN_POINT('Ctrl Pts',(-6.76721031445594,-0.159963077559033,
-46.2948874461289));
#36254=CARTESIAN_POINT('Ctrl Pts',(-6.76111922286706,-0.328826249995859,
-46.2869546761004));
#36255=CARTESIAN_POINT('Ctrl Pts',(-6.74869499058743,-0.497398154419779,
-46.2790219060718));
#36256=CARTESIAN_POINT('Ctrl Pts',(-6.73628023855867,-0.665841430860132,
-46.2710951891054));
#36257=CARTESIAN_POINT('Ctrl Pts',(-6.71754198738097,-0.833993501133486,
-46.263168472139));
#36258=CARTESIAN_POINT('Ctrl Pts',(-6.69250610205252,-1.00132465963334,
-46.2552417551727));
#36259=CARTESIAN_POINT('Ctrl Pts',(-6.66748360251499,-1.16856635215775,
-46.2473192763378));
#36260=CARTESIAN_POINT('Ctrl Pts',(-6.63617022537958,-1.33498762807606,
-46.239396797503));
#36261=CARTESIAN_POINT('Ctrl Pts',(-6.59864372361297,-1.50006333493727,
-46.2314743186682));
#36262=CARTESIAN_POINT('Ctrl Pts',(-6.56112284707921,-1.66511429690502,
-46.2235530274151));
#36263=CARTESIAN_POINT('Ctrl Pts',(-6.51739077483453,-1.82881971544845,
-46.2156317361621));
#36264=CARTESIAN_POINT('Ctrl Pts',(-6.46757647866796,-1.99066408331014,
-46.207710444909));
#36265=CARTESIAN_POINT('Ctrl Pts',(-6.41776374034483,-2.15250338980982,
-46.1997894013786));
#36266=CARTESIAN_POINT('Ctrl Pts',(-6.36186926856301,-2.31248139441357,
-46.1918683578482));
#36267=CARTESIAN_POINT('Ctrl Pts',(-6.30007195470136,-2.47009764292536,
-46.1839473143178));
#36268=CARTESIAN_POINT('Ctrl Pts',(-6.2382638160406,-2.62774150047253,-46.1760248832886));
#36269=CARTESIAN_POINT('Ctrl Pts',(-6.17055091868677,-2.78302242183815,
-46.1681024522593));
#36270=CARTESIAN_POINT('Ctrl Pts',(-6.09716023660602,-2.93546010859464,
-46.16018002123));
#36271=CARTESIAN_POINT('Ctrl Pts',(-6.02374153513716,-3.08795599362083,
-46.1522545655433));
#36272=CARTESIAN_POINT('Ctrl Pts',(-5.94464090369827,-3.23760613974861,
-46.1443291098566));
#36273=CARTESIAN_POINT('Ctrl Pts',(-5.86013102767455,-3.38395528021368,
-46.13640365417));
#36274=CARTESIAN_POINT('Ctrl Pts',(-5.77552340599045,-3.53047369075763,
-46.128469031757));
#36275=CARTESIAN_POINT('Ctrl Pts',(-5.68549424387489,-3.67368314307318,
-46.1205344093441));
#36276=CARTESIAN_POINT('Ctrl Pts',(-5.59035961032058,-3.81315727806975,
-46.1125997869311));
#36277=CARTESIAN_POINT('Ctrl Pts',(-5.49516237281654,-3.95272319490654,
-46.1046599430895));
#36278=CARTESIAN_POINT('Ctrl Pts',(-5.39485320534837,-4.08854859656338,
-46.0967200992479));
#36279=CARTESIAN_POINT('Ctrl Pts',(-5.28978760141626,-4.22024124096039,
-46.0887802554063));
#36280=CARTESIAN_POINT('Ctrl Pts',(-5.1845670780937,-4.35212806635891,-46.080828704253));
#36281=CARTESIAN_POINT('Ctrl Pts',(-5.07457637133191,-4.47986968581321,
-46.0728771530998));
#36282=CARTESIAN_POINT('Ctrl Pts',(-4.96020730033993,-4.60311118024043,
-46.0649256019465));
#36283=CARTESIAN_POINT('Ctrl Pts',(-4.90887553083546,-4.658425120718,-46.0613567420488));
#36284=CARTESIAN_POINT('Ctrl Pts',(-4.85666220303607,-4.71283308217111,
-46.0577878821511));
#36285=CARTESIAN_POINT('Ctrl Pts',(-4.80360476700314,-4.76630572271909,
-46.0542190222534));
#36286=CARTESIAN_POINT('Ctrl Pts',(-4.67970740531085,-4.89117265150364,
-46.0458851795607));
#36287=CARTESIAN_POINT('Ctrl Pts',(-4.55077972205122,-5.01136532619399,
-46.037551336868));
#36288=CARTESIAN_POINT('Ctrl Pts',(-4.41720372934772,-5.12646078824725,
-46.0292174941753));
#36289=CARTESIAN_POINT('Ctrl Pts',(-4.28378517285028,-5.24142059573779,
-46.0208934739706));
#36290=CARTESIAN_POINT('Ctrl Pts',(-4.14572948208992,-5.35129493336938,
-46.0125694537658));
#36291=CARTESIAN_POINT('Ctrl Pts',(-4.00345627242166,-5.45569673596395,
-46.0042454335611));
#36292=CARTESIAN_POINT('Ctrl Pts',(-3.86132466414372,-5.55999462974509,
-45.9959296980702));
#36293=CARTESIAN_POINT('Ctrl Pts',(-3.71498417868327,-5.6588306356081,-45.9876139625793));
#36294=CARTESIAN_POINT('Ctrl Pts',(-3.56488851785638,-5.75185699189885,
-45.9792982270884));
#36295=CARTESIAN_POINT('Ctrl Pts',(-3.41491474253282,-5.84480780593744,
-45.9709892444083));
#36296=CARTESIAN_POINT('Ctrl Pts',(-3.26119216244563,-5.93195818849206,
-45.9626802617283));
#36297=CARTESIAN_POINT('Ctrl Pts',(-3.10420473865019,-6.01300273910978,
-45.9543712790482));
#36298=CARTESIAN_POINT('Ctrl Pts',(-2.94731604847152,-6.09399631862798,
-45.9460675221111));
#36299=CARTESIAN_POINT('Ctrl Pts',(-2.78716691489952,-6.16889156005191,
-45.9377637651739));
#36300=CARTESIAN_POINT('Ctrl Pts',(-2.62426745602946,-6.23742810132708,
-45.9294600082367));
#36301=CARTESIAN_POINT('Ctrl Pts',(-2.46143413041278,-6.30593681841866,
-45.9211596224247));
#36302=CARTESIAN_POINT('Ctrl Pts',(-2.2958530244332,-6.36809184448666,-45.9128592366127));
#36303=CARTESIAN_POINT('Ctrl Pts',(-2.12805613808744,-6.42368010358147,
-45.9045588508006));
#36304=CARTESIAN_POINT('Ctrl Pts',(-1.96029463573881,-6.47925664055888,
-45.896260215324));
#36305=CARTESIAN_POINT('Ctrl Pts',(-1.79031861385656,-6.52826906003398,
-45.8879615798474));
#36306=CARTESIAN_POINT('Ctrl Pts',(-1.6186774427106,-6.57055342695422,-45.8796629443707));
#36307=CARTESIAN_POINT('Ctrl Pts',(-1.44704397575741,-6.61283589592124,
-45.8713646813821));
#36308=CARTESIAN_POINT('Ctrl Pts',(-1.27374584619206,-6.64839083111104,
-45.8630664183936));
#36309=CARTESIAN_POINT('Ctrl Pts',(-1.09934507768376,-6.67710486664486,
-45.854768155405));
#36310=CARTESIAN_POINT('Ctrl Pts',(-0.924923189986577,-6.70582237932586,
-45.8464688875322));
#36311=CARTESIAN_POINT('Ctrl Pts',(-0.749398740524253,-6.72769728575488,
-45.8381696196593));
#36312=CARTESIAN_POINT('Ctrl Pts',(-0.573341573289961,-6.74266775396337,
-45.8298703517865));
#36313=CARTESIAN_POINT('Ctrl Pts',(-0.397160785548049,-6.75764873385342,
-45.82156525649));
#36314=CARTESIAN_POINT('Ctrl Pts',(-0.220446879565258,-6.76571555880835,
-45.8132601611935));
#36315=CARTESIAN_POINT('Ctrl Pts',(-0.0437733295457148,-6.76685842142574,
-45.804955065897));
#36316=CARTESIAN_POINT('Ctrl Pts',(0.132964644837099,-6.76800170079027,
-45.7966469421309));
#36317=CARTESIAN_POINT('Ctrl Pts',(0.309661886153458,-6.76221599062028,
-45.7883388183648));
#36318=CARTESIAN_POINT('Ctrl Pts',(0.485747087053247,-6.74954359697152,
-45.7800306945987));
#36319=CARTESIAN_POINT('Ctrl Pts',(0.662019465504322,-6.73685773264153,
-45.771713739345));
#36320=CARTESIAN_POINT('Ctrl Pts',(0.837678157137102,-6.71727059098702,
-45.7633967840913));
#36321=CARTESIAN_POINT('Ctrl Pts',(1.01215803202879,-6.69087625936989,-45.7550798288376));
#36322=CARTESIAN_POINT('Ctrl Pts',(1.14074704517418,-6.67142403854851,-45.7489503593552));
#36323=CARTESIAN_POINT('Ctrl Pts',(1.26869593148752,-6.64827559605648,-45.7428208898728));
#36324=CARTESIAN_POINT('Ctrl Pts',(1.39578288781446,-6.62148617230938,-45.7366914203904));
#36325=CARTESIAN_POINT('Ctrl Pts',(1.57100439119975,-6.58455017793623,-45.7282403968652));
#36326=CARTESIAN_POINT('Ctrl Pts',(1.74490711405204,-6.54062348449208,-45.71978937334));
#36327=CARTESIAN_POINT('Ctrl Pts',(1.91691339630708,-6.48981756531403,-45.7113383498148));
#36328=CARTESIAN_POINT('Ctrl Pts',(2.08876823214282,-6.4390563792378,-45.7028947671647));
#36329=CARTESIAN_POINT('Ctrl Pts',(2.25872963909701,-6.38142813354898,-45.6944511845145));
#36330=CARTESIAN_POINT('Ctrl Pts',(2.42623146224893,-6.31709505165099,-45.6860076018643));
#36331=CARTESIAN_POINT('Ctrl Pts',(2.59360857507555,-6.25280986773656,-45.6775703057245));
#36332=CARTESIAN_POINT('Ctrl Pts',(2.75852944614736,-6.18182991731004,-45.6691330095847));
#36333=CARTESIAN_POINT('Ctrl Pts',(2.92044399381099,-6.10436695153669,-45.6606957134449));
#36334=CARTESIAN_POINT('Ctrl Pts',(3.08224302779018,-6.02695924968318,-45.6522644366725));
#36335=CARTESIAN_POINT('Ctrl Pts',(3.24103971818719,-5.94307790080715,-45.6438331599002));
#36336=CARTESIAN_POINT('Ctrl Pts',(3.39630465759495,-5.85298245963533,-45.6354018831278));
#36337=CARTESIAN_POINT('Ctrl Pts',(3.55150304482962,-5.76292563663075,-45.6269742203059));
#36338=CARTESIAN_POINT('Ctrl Pts',(3.70317241279008,-5.66666019737143,-45.6185465574839));
#36339=CARTESIAN_POINT('Ctrl Pts',(3.85080805053698,-5.56449156328946,-45.610118894662));
#36340=CARTESIAN_POINT('Ctrl Pts',(3.99839824019555,-5.46235438075386,-45.601693826208));
#36341=CARTESIAN_POINT('Ctrl Pts',(4.14195690372836,-5.35431781584026,-45.593268757754));
#36342=CARTESIAN_POINT('Ctrl Pts',(4.28100811183295,-5.24073072637972,-45.5848436893));
#36343=CARTESIAN_POINT('Ctrl Pts',(4.31905677861794,-5.20964982189229,-45.5825383326863));
#36344=CARTESIAN_POINT('Ctrl Pts',(4.35676813232352,-5.17815357257993,-45.5802329760726));
#36345=CARTESIAN_POINT('Ctrl Pts',(4.39413283355317,-5.14624966758221,-45.5779276194589));
#36346=CARTESIAN_POINT('Ctrl Pts',(4.53382746006166,-5.02697120566097,-45.5693086309344));
#36347=CARTESIAN_POINT('Ctrl Pts',(4.6686117013062,-4.90204487325264,-45.5606896424098));
#36348=CARTESIAN_POINT('Ctrl Pts',(4.79804525525148,-4.77190221280348,-45.5520706538853));
#36349=CARTESIAN_POINT('Ctrl Pts',(4.92755635144531,-4.6416815852877,-45.5434465018176));
#36350=CARTESIAN_POINT('Ctrl Pts',(5.05171014858183,-4.50623860874799,-45.5348223497499));
#36351=CARTESIAN_POINT('Ctrl Pts',(5.1701045948368,-4.36604025158352,-45.5261981976821));
#36352=CARTESIAN_POINT('Ctrl Pts',(5.29255408272797,-4.22104006296822,-45.5172786660859));
#36353=CARTESIAN_POINT('Ctrl Pts',(5.40884249144538,-4.07095325895653,-45.5083591344897));
#36354=CARTESIAN_POINT('Ctrl Pts',(5.51857210252305,-3.91633131249826,-45.4994396028934));
#36355=CARTESIAN_POINT('Ctrl Pts',(5.62486554799119,-3.76655132811095,-45.4907993850342));
#36356=CARTESIAN_POINT('Ctrl Pts',(5.72500462734414,-3.61251621795943,-45.4821591671749));
#36357=CARTESIAN_POINT('Ctrl Pts',(5.81867314823915,-3.45475495425663,-45.4735189493156));
#36358=CARTESIAN_POINT('Ctrl Pts',(5.91688372554382,-3.28934372926319,-45.4644597608509));
#36359=CARTESIAN_POINT('Ctrl Pts',(6.00798043531471,-3.11983634042863,-45.4554005723862));
#36360=CARTESIAN_POINT('Ctrl Pts',(6.09165394290615,-2.94686973581731,-45.4463413839214));
#36361=CARTESIAN_POINT('Ctrl Pts',(6.17532745049759,-2.77390313120598,-45.4372821954567));
#36362=CARTESIAN_POINT('Ctrl Pts',(6.25157763451954,-2.59747767518718,-45.428223006992));
#36363=CARTESIAN_POINT('Ctrl Pts',(6.32015363622209,-2.41825288473906,-45.4191638185273));
#36364=CARTESIAN_POINT('Ctrl Pts',(6.38861083481286,-2.23933858866626,-45.4101203244711));
#36365=CARTESIAN_POINT('Ctrl Pts',(6.44948427553468,-2.05747012730974,-45.4010768304148));
#36366=CARTESIAN_POINT('Ctrl Pts',(6.50254660692547,-1.87327964403664,-45.3920333363585));
#36367=CARTESIAN_POINT('Ctrl Pts',(6.55556040239563,-1.68925763912556,-45.3829981143532));
#36368=CARTESIAN_POINT('Ctrl Pts',(6.6007772872885,-1.50291808134845,-45.3739628923479));
#36369=CARTESIAN_POINT('Ctrl Pts',(6.63801961221435,-1.31490860057179,-45.3649276703426));
#36370=CARTESIAN_POINT('Ctrl Pts',(6.67519632427136,-1.12723035157049,-45.3559083664315));
#36371=CARTESIAN_POINT('Ctrl Pts',(6.70442648513945,-0.937888287704712,
-45.3468890625204));
#36372=CARTESIAN_POINT('Ctrl Pts',(6.72558342098193,-0.747540398515744,
-45.3378697586093));
#36373=CARTESIAN_POINT('Ctrl Pts',(6.74671381397062,-0.557431314049226,
-45.3288617700449));
#36374=CARTESIAN_POINT('Ctrl Pts',(6.75979116856504,-0.366319158461256,
-45.3198537814806));
#36375=CARTESIAN_POINT('Ctrl Pts',(6.76474017020583,-0.174869750396155,
-45.3108457929162));
#36376=CARTESIAN_POINT('Ctrl Pts',(6.76967799435306,0.0161472624749014,
-45.3018581492096));
#36377=CARTESIAN_POINT('Ctrl Pts',(6.76652410399345,0.2074997698381,-45.2928705055029));
#36378=CARTESIAN_POINT('Ctrl Pts',(6.75525506917884,0.398519698802507,-45.2838828617962));
#36379=CARTESIAN_POINT('Ctrl Pts',(6.74544052091391,0.564884817308657,-45.2760552470628));
#36380=CARTESIAN_POINT('Ctrl Pts',(6.72947123810675,0.730997469063674,-45.2682276323293));
#36381=CARTESIAN_POINT('Ctrl Pts',(6.7073639010008,0.896414245508953,-45.2604000175958));
#36382=CARTESIAN_POINT('Ctrl Pts',(6.68442186715912,1.06807658842258,-45.2522768591505));
#36383=CARTESIAN_POINT('Ctrl Pts',(6.65487812228032,1.2389125600411,-45.2441537007052));
#36384=CARTESIAN_POINT('Ctrl Pts',(6.61881905696717,1.40837611848831,-45.2360305422599));
#36385=CARTESIAN_POINT('Ctrl Pts',(6.58276253400699,1.57782772886709,-45.2279079565399));
#36386=CARTESIAN_POINT('Ctrl Pts',(6.54019168179962,1.74590676080617,-45.2197853708198));
#36387=CARTESIAN_POINT('Ctrl Pts',(6.49124394706447,1.91207767093778,-45.2116627850997));
#36388=CARTESIAN_POINT('Ctrl Pts',(6.44229033075539,2.07826854821392,-45.2035392233674));
#36389=CARTESIAN_POINT('Ctrl Pts',(6.38695841070977,2.2425504963687,-45.1954156616351));
#36390=CARTESIAN_POINT('Ctrl Pts',(6.32543539375741,2.40440347683183,-45.1872920999027));
#36391=CARTESIAN_POINT('Ctrl Pts',(6.26386756458739,2.56637434798613,-45.1791626211196));
#36392=CARTESIAN_POINT('Ctrl Pts',(6.19609976208033,2.72591237537359,-45.1710331423365));
#36393=CARTESIAN_POINT('Ctrl Pts',(6.12236745829981,2.88251725156182,-45.1629036635534));
#36394=CARTESIAN_POINT('Ctrl Pts',(6.04860509515681,3.03918597280169,-45.1547708705249));
#36395=CARTESIAN_POINT('Ctrl Pts',(5.96887355219253,3.1929188345764,-45.1466380774963));
#36396=CARTESIAN_POINT('Ctrl Pts',(5.88345397314894,3.34324069516958,-45.1385052844678));
#36397=CARTESIAN_POINT('Ctrl Pts',(5.79794151327188,3.49372600798129,-45.1303636482606));
#36398=CARTESIAN_POINT('Ctrl Pts',(5.70672885683142,3.6407926009944,-45.1222220120535));
#36399=CARTESIAN_POINT('Ctrl Pts',(5.61014052811366,3.78399421971237,-45.1140803758463));
#36400=CARTESIAN_POINT('Ctrl Pts',(5.56093008657976,3.85695349935859,-45.1099323227857));
#36401=CARTESIAN_POINT('Ctrl Pts',(5.51032490727817,3.92891003821627,-45.105784269725));
#36402=CARTESIAN_POINT('Ctrl Pts',(5.45837184762625,3.99980821703257,-45.1016362166643));
#36403=CARTESIAN_POINT('Ctrl Pts',(5.35265160826175,4.14408022882907,-45.09319526698));
#36404=CARTESIAN_POINT('Ctrl Pts',(5.24112980853916,4.28426478902159,-45.0847543172956));
#36405=CARTESIAN_POINT('Ctrl Pts',(5.12414896161536,4.41988534004857,-45.0763133676113));
#36406=CARTESIAN_POINT('Ctrl Pts',(5.00725445971155,4.55540578785783,-45.067878648297));
#36407=CARTESIAN_POINT('Ctrl Pts',(4.88490915937136,4.68636868978522,-45.0594439289827));
#36408=CARTESIAN_POINT('Ctrl Pts',(4.75749678072063,4.81232930932962,-45.0510092096685));
#36409=CARTESIAN_POINT('Ctrl Pts',(4.63017123614944,4.93820408419729,-45.0425802387838));
#36410=CARTESIAN_POINT('Ctrl Pts',(4.49778573702322,5.059083142006,-45.0341512678991));
#36411=CARTESIAN_POINT('Ctrl Pts',(4.36076205027886,5.17455730868329,-45.0257222970144));
#36412=CARTESIAN_POINT('Ctrl Pts',(4.22379593538374,5.28998295775409,-45.0172968676447));
#36413=CARTESIAN_POINT('Ctrl Pts',(4.08219577218,5.40000802818307,-45.008871438275));
#36414=CARTESIAN_POINT('Ctrl Pts',(3.93641814444968,5.50426209332799,-45.0004460089053));
#36415=CARTESIAN_POINT('Ctrl Pts',(3.79067326559698,5.60849273784468,-44.9920224723045));
#36416=CARTESIAN_POINT('Ctrl Pts',(3.64075306277067,5.70695476607202,-44.9835989357037));
#36417=CARTESIAN_POINT('Ctrl Pts',(3.48714535424184,5.79931946683312,-44.9751753991029));
#36418=CARTESIAN_POINT('Ctrl Pts',(3.36021289904917,5.8756442707966,-44.9682146795375));
#36419=CARTESIAN_POINT('Ctrl Pts',(3.23076311096976,5.94780627660475,-44.9612539599721));
#36420=CARTESIAN_POINT('Ctrl Pts',(3.0990855038472,6.01564277861013,-44.9542932404068));
#36421=CARTESIAN_POINT('Ctrl Pts',(3.0990855038472,6.01564277861013,-46.9540128207846));
#36422=CARTESIAN_POINT('Ctrl Pts',(2.9436651366959,6.09571086519164,-46.945789753969));
#36423=CARTESIAN_POINT('Ctrl Pts',(2.78499491016231,6.16982658704594,-46.9375666871535));
#36424=CARTESIAN_POINT('Ctrl Pts',(2.62356988515337,6.23772154377833,-46.929343620338));
#36425=CARTESIAN_POINT('Ctrl Pts',(2.4622820399152,6.30555880304654,-46.9211275415246));
#36426=CARTESIAN_POINT('Ctrl Pts',(2.29824438899914,6.36718569630545,-46.9129114627112));
#36427=CARTESIAN_POINT('Ctrl Pts',(2.1319750432217,6.42238050998848,-46.9046953838978));
#36428=CARTESIAN_POINT('Ctrl Pts',(1.96578725261032,6.47754825059814,-46.8964833350737));
#36429=CARTESIAN_POINT('Ctrl Pts',(1.79737028426355,6.526290083495,-46.8882712862495));
#36430=CARTESIAN_POINT('Ctrl Pts',(1.62726097812719,6.56843289598551,-46.8800592374253));
#36431=CARTESIAN_POINT('Ctrl Pts',(1.45720570249951,6.61056232297908,-46.871849796931));
#36432=CARTESIAN_POINT('Ctrl Pts',(1.28545950506018,6.64609682019459,-46.8636403564367));
#36433=CARTESIAN_POINT('Ctrl Pts',(1.11257317584935,6.67491347722055,-46.8554309159423));
#36434=CARTESIAN_POINT('Ctrl Pts',(1.06067644192987,6.6835636139257,-46.8529666195985));
#36435=CARTESIAN_POINT('Ctrl Pts',(1.00867705365995,6.69160877317709,-46.8505023232548));
#36436=CARTESIAN_POINT('Ctrl Pts',(0.956590091472105,6.69904652893958,-46.848038026911));
#36437=CARTESIAN_POINT('Ctrl Pts',(0.769346505385178,6.72578396961396,-46.8391793093892));
#36438=CARTESIAN_POINT('Ctrl Pts',(0.581164697193612,6.74464057162761,-46.8303205918675));
#36439=CARTESIAN_POINT('Ctrl Pts',(0.392697660495038,6.75559601718766,-46.8214618743457));
#36440=CARTESIAN_POINT('Ctrl Pts',(0.203878032240445,6.76657195862679,-46.8125865835862));
#36441=CARTESIAN_POINT('Ctrl Pts',(0.0147723679925125,6.76961718815369,
-46.8037112928268));
#36442=CARTESIAN_POINT('Ctrl Pts',(-0.173966971303869,6.76476344692816,
-46.7948360020673));
#36443=CARTESIAN_POINT('Ctrl Pts',(-0.36324237276091,6.75989591998622,-46.7859355034866));
#36444=CARTESIAN_POINT('Ctrl Pts',(-0.552149106327011,6.74708453411111,
-46.7770350049058));
#36445=CARTESIAN_POINT('Ctrl Pts',(-0.740037474591596,6.72641312559674,
-46.768134506325));
#36446=CARTESIAN_POINT('Ctrl Pts',(-0.928180187591721,6.705713734169,-46.7592219591274));
#36447=CARTESIAN_POINT('Ctrl Pts',(-1.11530152449871,6.67713310069943,-46.7503094119298));
#36448=CARTESIAN_POINT('Ctrl Pts',(-1.30076123301329,6.64080636780578,-46.7413968647322));
#36449=CARTESIAN_POINT('Ctrl Pts',(-1.48663045467715,6.60439942193806,-46.7324646377599));
#36450=CARTESIAN_POINT('Ctrl Pts',(-1.67083045371743,6.56021221558444,-46.7235324107876));
#36451=CARTESIAN_POINT('Ctrl Pts',(-1.85273262098156,6.50843075058426,-46.7146001838154));
#36452=CARTESIAN_POINT('Ctrl Pts',(-2.02465117435366,6.45949128665037,-46.7061581978701));
#36453=CARTESIAN_POINT('Ctrl Pts',(-2.19451716772574,6.40376878410272,-46.6977162119248));
#36454=CARTESIAN_POINT('Ctrl Pts',(-2.36181586475644,6.34145999127841,-46.6892742259795));
#36455=CARTESIAN_POINT('Ctrl Pts',(-2.52479412761867,6.28076030266288,-46.6810502515619));
#36456=CARTESIAN_POINT('Ctrl Pts',(-2.6856469466595,6.21369318557838,-46.6728262771444));
#36457=CARTESIAN_POINT('Ctrl Pts',(-2.84384203240731,6.14042763125773,-46.6646023027268));
#36458=CARTESIAN_POINT('Ctrl Pts',(-3.00187004879588,6.06723945247096,-46.6563870136241));
#36459=CARTESIAN_POINT('Ctrl Pts',(-3.15724559852198,5.98786602148833,-46.6481717245215));
#36460=CARTESIAN_POINT('Ctrl Pts',(-3.30945350000741,5.90252543673373,-46.6399564354188));
#36461=CARTESIAN_POINT('Ctrl Pts',(-3.46153118484209,5.81725786241428,-46.6317481746466));
#36462=CARTESIAN_POINT('Ctrl Pts',(-3.61044630761767,5.72603347585005,-46.6235399138744));
#36463=CARTESIAN_POINT('Ctrl Pts',(-3.75570547846719,5.62911763591875,-46.6153316531022));
#36464=CARTESIAN_POINT('Ctrl Pts',(-3.90086950502898,5.53226527554958,-46.6071287687143));
#36465=CARTESIAN_POINT('Ctrl Pts',(-4.0423820522995,5.42972908567718,-46.5989258843265));
#36466=CARTESIAN_POINT('Ctrl Pts',(-4.17977600159479,5.321819385933,-46.5907229999386));
#36467=CARTESIAN_POINT('Ctrl Pts',(-4.317107503117,5.2139587328934,-46.5825238438944));
#36468=CARTESIAN_POINT('Ctrl Pts',(-4.45032385468422,5.10072965681161,-46.5743246878501));
#36469=CARTESIAN_POINT('Ctrl Pts',(-4.57898844007612,4.98248470801961,-46.5661255318059));
#36470=CARTESIAN_POINT('Ctrl Pts',(-4.70764183477774,4.86425004366288,-46.5579270888889));
#36471=CARTESIAN_POINT('Ctrl Pts',(-4.83174398226159,4.7410006117415,-46.5497286459719));
#36472=CARTESIAN_POINT('Ctrl Pts',(-4.95089251187824,4.61312825919983,-46.5415302030549));
#36473=CARTESIAN_POINT('Ctrl Pts',(-5.07003985491662,4.48525718011537,-46.5333318417847));
#36474=CARTESIAN_POINT('Ctrl Pts',(-5.18423343304624,4.35276353382202,-46.5251334805144));
#36475=CARTESIAN_POINT('Ctrl Pts',(-5.29310891271248,4.21607483782769,-46.5169351192442));
#36476=CARTESIAN_POINT('Ctrl Pts',(-5.40200308611845,4.07936267261039,-46.5087353503289));
#36477=CARTESIAN_POINT('Ctrl Pts',(-5.50557711839364,3.93845430325552,-46.5005355814136));
#36478=CARTESIAN_POINT('Ctrl Pts',(-5.60350799682097,3.79380905286012,-46.4923358124983));
#36479=CARTESIAN_POINT('Ctrl Pts',(-5.7014734798485,3.6491126909957,-46.484133146134));
#36480=CARTESIAN_POINT('Ctrl Pts',(-5.79379163587259,3.50067711456468,-46.4759304797698));
#36481=CARTESIAN_POINT('Ctrl Pts',(-5.88018365440796,3.34898927893677,-46.4677278134055));
#36482=CARTESIAN_POINT('Ctrl Pts',(-5.9666737926827,3.19712916384197,-46.4595158308625));
#36483=CARTESIAN_POINT('Ctrl Pts',(-6.0472241693232,3.04200972215826,-46.4513038483194));
#36484=CARTESIAN_POINT('Ctrl Pts',(-6.12160222207306,2.88414202748585,-46.4430918657764));
#36485=CARTESIAN_POINT('Ctrl Pts',(-6.19602414400368,2.72618122031349,-46.4348750396951));
#36486=CARTESIAN_POINT('Ctrl Pts',(-6.26426634522733,2.56546925861872,-46.4266582136138));
#36487=CARTESIAN_POINT('Ctrl Pts',(-6.32614509416542,2.40253558715929,-46.4184413875325));
#36488=CARTESIAN_POINT('Ctrl Pts',(-6.38811926907129,2.23935064844657,-46.4102118899186));
#36489=CARTESIAN_POINT('Ctrl Pts',(-6.44371026686801,2.07393749294943,-46.4019823923048));
#36490=CARTESIAN_POINT('Ctrl Pts',(-6.49278437452873,1.90684033570607,-46.3937528946909));
#36491=CARTESIAN_POINT('Ctrl Pts',(-6.53652694311385,1.75789704953099,-46.3864174711661));
#36492=CARTESIAN_POINT('Ctrl Pts',(-6.57509240681827,1.60761613177491,-46.3790820476413));
#36493=CARTESIAN_POINT('Ctrl Pts',(-6.6084206600231,1.45638778495972,-46.3717466241164));
#36494=CARTESIAN_POINT('Ctrl Pts',(-6.66061480096339,1.21955468124653,-46.360258889462));
#36495=CARTESIAN_POINT('Ctrl Pts',(-6.70011427082052,0.979728298518272,
-46.3487711548076));
#36496=CARTESIAN_POINT('Ctrl Pts',(-6.72663108996774,0.738053642684177,
-46.3372834201532));
#36497=CARTESIAN_POINT('Ctrl Pts',(-6.75169631263707,0.509608857192325,
-46.326424552599));
#36498=CARTESIAN_POINT('Ctrl Pts',(-6.76516160254484,0.279512294337435,
-46.3155656850448));
#36499=CARTESIAN_POINT('Ctrl Pts',(-6.76682433008413,0.0487594686342606,
-46.3047068174906));
#36500=CARTESIAN_POINT('Ctrl Pts',(-6.76692062324185,0.035395933289899,
-46.3040779503904));
#36501=CARTESIAN_POINT('Ctrl Pts',(-6.7669773434168,0.0220302060269217,
-46.3034490832902));
#36502=CARTESIAN_POINT('Ctrl Pts',(-6.766994455545,0.00866248366889811,
-46.30282021619));
#36503=CARTESIAN_POINT('',(-6.767,7.08953227612601E-13,-46.6971797838101));
#36504=CARTESIAN_POINT('Ctrl Pts',(3.0990855038472,6.01564277861013,-47.3486841594369));
#36505=CARTESIAN_POINT('Ctrl Pts',(2.94193708164431,6.09660110926984,-47.340367670832));
#36506=CARTESIAN_POINT('Ctrl Pts',(2.78171095141422,6.17134796408445,-47.332051182227));
#36507=CARTESIAN_POINT('Ctrl Pts',(2.61893827740273,6.23966756319236,-47.3237346936221));
#36508=CARTESIAN_POINT('Ctrl Pts',(2.45688780546686,6.30768403675059,-47.3154551042409));
#36509=CARTESIAN_POINT('Ctrl Pts',(2.29231367972388,6.36933010932947,-47.3071755148598));
#36510=CARTESIAN_POINT('Ctrl Pts',(2.12575517203363,6.42444191728529,-47.2988959254787));
#36511=CARTESIAN_POINT('Ctrl Pts',(1.95574796491077,6.48069485014348,-47.2904449019535));
#36512=CARTESIAN_POINT('Ctrl Pts',(1.78336267081961,6.53024302663276,-47.2819938784283));
#36513=CARTESIAN_POINT('Ctrl Pts',(1.60915457911702,6.57289209865085,-47.2735428549031));
#36514=CARTESIAN_POINT('Ctrl Pts',(1.43509987246143,6.61550361942862,-47.265099272253));
#36515=CARTESIAN_POINT('Ctrl Pts',(1.2592258875842,6.65122806481807,-47.2566556896028));
#36516=CARTESIAN_POINT('Ctrl Pts',(1.08210350900727,6.67992073274782,-47.2482121069527));
#36517=CARTESIAN_POINT('Ctrl Pts',(0.905113003558764,6.70859203809249,-47.2397748108129));
#36518=CARTESIAN_POINT('Ctrl Pts',(0.726876283412527,6.73024194961993,-47.231337514673));
#36519=CARTESIAN_POINT('Ctrl Pts',(0.547975265559801,6.74477665370283,-47.2229002185332));
#36520=CARTESIAN_POINT('Ctrl Pts',(0.369201879942919,6.75930098838256,-47.2144689417608));
#36521=CARTESIAN_POINT('Ctrl Pts',(0.189765471540904,6.76672021408748,-47.2060376649885));
#36522=CARTESIAN_POINT('Ctrl Pts',(0.0102541461709204,6.76699223085754,
-47.1976063882161));
#36523=CARTESIAN_POINT('Ctrl Pts',(-0.169180234146751,6.76726413103137,
-47.1891787253942));
#36524=CARTESIAN_POINT('Ctrl Pts',(-0.348689136538506,6.76039492909866,
-47.1807510625723));
#36525=CARTESIAN_POINT('Ctrl Pts',(-0.527682716869333,6.74639458898732,
-47.1723233997504));
#36526=CARTESIAN_POINT('Ctrl Pts',(-0.706621195896954,6.73239855873438,
-47.1638983312964));
#36527=CARTESIAN_POINT('Ctrl Pts',(-0.885044339136366,6.71127579399997,
-47.1554732628424));
#36528=CARTESIAN_POINT('Ctrl Pts',(-1.06236531734555,6.68308827807185,-47.1470481943884));
#36529=CARTESIAN_POINT('Ctrl Pts',(-1.11088576464008,6.67537531091609,-47.1447428377747));
#36530=CARTESIAN_POINT('Ctrl Pts',(-1.15932371901165,6.66713367906998,-47.1424374811609));
#36531=CARTESIAN_POINT('Ctrl Pts',(-1.20766724045393,6.65836532764119,-47.1401321245471));
#36532=CARTESIAN_POINT('Ctrl Pts',(-1.38840815231793,6.62558327566189,-47.1315131360226));
#36533=CARTESIAN_POINT('Ctrl Pts',(-1.56774768451873,6.58544959396408,-47.1228941474982));
#36534=CARTESIAN_POINT('Ctrl Pts',(-1.74508818869424,6.53811564701022,-47.1142751589737));
#36535=CARTESIAN_POINT('Ctrl Pts',(-1.92253493565814,6.49075334279792,-47.1056510069059));
#36536=CARTESIAN_POINT('Ctrl Pts',(-2.09797997069514,6.43618224313281,-47.0970268548381));
#36537=CARTESIAN_POINT('Ctrl Pts',(-2.2708408736559,6.37460357406904,-47.0884027027703));
#36538=CARTESIAN_POINT('Ctrl Pts',(-2.44962230904706,6.31091581902359,-47.0794831711741));
#36539=CARTESIAN_POINT('Ctrl Pts',(-2.62563912946027,6.23973210127814,-47.0705636395779));
#36540=CARTESIAN_POINT('Ctrl Pts',(-2.79827013661542,6.16132885362617,-47.0616441079816));
#36541=CARTESIAN_POINT('Ctrl Pts',(-2.96549523077994,6.08538079141263,-47.0530038901224));
#36542=CARTESIAN_POINT('Ctrl Pts',(-3.12954310369647,6.00265869179961,-47.0443636722631));
#36543=CARTESIAN_POINT('Ctrl Pts',(-3.28987433182708,5.91346056728083,-47.0357234544039));
#36544=CARTESIAN_POINT('Ctrl Pts',(-3.45798014074014,5.81993715920501,-47.0266642659392));
#36545=CARTESIAN_POINT('Ctrl Pts',(-3.62199956735499,5.71929426033176,-47.0176050774744));
#36546=CARTESIAN_POINT('Ctrl Pts',(-3.78134478064512,5.61192664330958,-47.0085458890097));
#36547=CARTESIAN_POINT('Ctrl Pts',(-3.94068999393526,5.50455902628739,-46.999486700545));
#36548=CARTESIAN_POINT('Ctrl Pts',(-4.09536070564776,5.39046694490904,-46.9904275120803));
#36549=CARTESIAN_POINT('Ctrl Pts',(-4.24480826106308,5.27009410037531,-46.9813683236156));
#36550=CARTESIAN_POINT('Ctrl Pts',(-4.39399690907377,5.14992979334946,-46.9723248295593));
#36551=CARTESIAN_POINT('Ctrl Pts',(-4.53811845400273,5.02339642498788,-46.963281335503));
#36552=CARTESIAN_POINT('Ctrl Pts',(-4.67665832985533,4.89092586999586,-46.9542378414467));
#36553=CARTESIAN_POINT('Ctrl Pts',(-4.81507148379015,4.75857648533602,-46.9452026194414));
#36554=CARTESIAN_POINT('Ctrl Pts',(-4.94791298992995,4.62030092090447,-46.936167397436));
#36555=CARTESIAN_POINT('Ctrl Pts',(-5.07470344041103,4.4765694445502,-46.9271321754307));
#36556=CARTESIAN_POINT('Ctrl Pts',(-5.20127051372017,4.33309119176746,-46.9181128715196));
#36557=CARTESIAN_POINT('Ctrl Pts',(-5.32180766205109,4.18417639960211,-46.9090935676085));
#36558=CARTESIAN_POINT('Ctrl Pts',(-5.43587431600292,4.0303299394243,-46.9000742636973));
#36559=CARTESIAN_POINT('Ctrl Pts',(-5.54979786537001,3.87667649037666,-46.891066275133));
#36560=CARTESIAN_POINT('Ctrl Pts',(-5.65726697909139,3.71810391137042,-46.8820582865686));
#36561=CARTESIAN_POINT('Ctrl Pts',(-5.75788153122102,3.55514968354694,-46.8730502980042));
#36562=CARTESIAN_POINT('Ctrl Pts',(-5.85826884186048,3.39256349355473,-46.8640626542976));
#36563=CARTESIAN_POINT('Ctrl Pts',(-5.9518323680833,3.22561561049101,-46.8550750105909));
#36564=CARTESIAN_POINT('Ctrl Pts',(-6.0382156866559,3.05487157200145,-46.8460873668842));
#36565=CARTESIAN_POINT('Ctrl Pts',(-6.11344956988983,2.90616534877599,-46.8382597521508));
#36566=CARTESIAN_POINT('Ctrl Pts',(-6.18323768262847,2.75458022290258,-46.8304321374175));
#36567=CARTESIAN_POINT('Ctrl Pts',(-6.24737131521439,2.60050776769393,-46.8226045226841));
#36568=CARTESIAN_POINT('Ctrl Pts',(-6.31208327184665,2.44504596648796,-46.8147063225551));
#36569=CARTESIAN_POINT('Ctrl Pts',(-6.37102274600033,2.28708443549865,-46.8068081224262));
#36570=CARTESIAN_POINT('Ctrl Pts',(-6.4239928389839,2.12711189284522,-46.7989099222972));
#36571=CARTESIAN_POINT('Ctrl Pts',(-6.47695463193929,1.96716441672535,-46.7910129597588));
#36572=CARTESIAN_POINT('Ctrl Pts',(-6.52394878452144,1.8052069232848,-46.7831159972203));
#36573=CARTESIAN_POINT('Ctrl Pts',(-6.56482759592059,1.64174530175647,-46.7752190346819));
#36574=CARTESIAN_POINT('Ctrl Pts',(-6.60572002569664,1.47822922458494,-46.7673194413475));
#36575=CARTESIAN_POINT('Ctrl Pts',(-6.64049294982191,1.31320839355458,-46.7594198480131));
#36576=CARTESIAN_POINT('Ctrl Pts',(-6.669049312613,1.14720105732872,-46.7515202546787));
#36577=CARTESIAN_POINT('Ctrl Pts',(-6.69761136836199,0.981160626104589,
-46.743619086492));
#36578=CARTESIAN_POINT('Ctrl Pts',(-6.7199543417302,0.814133680992182,-46.7357179183053));
#36579=CARTESIAN_POINT('Ctrl Pts',(-6.73603290875121,0.646644919736252,
-46.7278167501186));
#36580=CARTESIAN_POINT('Ctrl Pts',(-6.7521232703795,0.479033295282363,-46.7199097859443));
#36581=CARTESIAN_POINT('Ctrl Pts',(-6.76194003144293,0.310959563961669,
-46.71200282177));
#36582=CARTESIAN_POINT('Ctrl Pts',(-6.76548995400033,0.142949929418268,
-46.7040958575957));
#36583=CARTESIAN_POINT('Ctrl Pts',(-6.76649701697076,0.0952879652797101,
-46.7018527633592));
#36584=CARTESIAN_POINT('Ctrl Pts',(-6.76700006046205,0.0476311417937134,
-46.6996096691227));
#36585=CARTESIAN_POINT('Ctrl Pts',(-6.76699999999455,-8.58912449818477E-6,
-46.6973665748862));
#36586=CARTESIAN_POINT('Ctrl Pts',(-6.767,7.08953217511608E-13,-46.6971797838101));
#36587=CARTESIAN_POINT('Ctrl Pts',(-6.76700000000002,-0.186007249559383,
-46.6884302719974));
#36588=CARTESIAN_POINT('Ctrl Pts',(-6.7593263729425,-0.37201435581565,-46.6796807601846));
#36589=CARTESIAN_POINT('Ctrl Pts',(-6.74400518263365,-0.557389537586108,
-46.6709312483719));
#36590=CARTESIAN_POINT('Ctrl Pts',(-6.72868405703731,-0.742763936382679,
-46.6621817735147));
#36591=CARTESIAN_POINT('Ctrl Pts',(-6.70571545643563,-0.927506130405085,
-46.6534322986575));
#36592=CARTESIAN_POINT('Ctrl Pts',(-6.67517739401571,-1.1109886400957,-46.6446828238003));
#36593=CARTESIAN_POINT('Ctrl Pts',(-6.64463945804384,-1.29447039004569,
-46.6359333851717));
#36594=CARTESIAN_POINT('Ctrl Pts',(-6.60653217002717,-1.4766921833931,-46.6271839465432));
#36595=CARTESIAN_POINT('Ctrl Pts',(-6.56098496085471,-1.65703510627818,
-46.6184345079147));
#36596=CARTESIAN_POINT('Ctrl Pts',(-6.51543793649543,-1.83737729740056,
-46.6096851047881));
#36597=CARTESIAN_POINT('Ctrl Pts',(-6.46245112156878,-2.01584035545012,
-46.6009357016614));
#36598=CARTESIAN_POINT('Ctrl Pts',(-6.40220448361693,-2.1918181379748,-46.5921862985348));
#36599=CARTESIAN_POINT('Ctrl Pts',(-6.34195808511946,-2.36779522106376,
-46.5834369301833));
#36600=CARTESIAN_POINT('Ctrl Pts',(-6.27445201416324,-2.54128677725818,
-46.5746875618317));
#36601=CARTESIAN_POINT('Ctrl Pts',(-6.19991555052692,-2.71170355428733,
-46.5659381934802));
#36602=CARTESIAN_POINT('Ctrl Pts',(-6.12537937695079,-2.88211966813605,
-46.557188859177));
#36603=CARTESIAN_POINT('Ctrl Pts',(-6.04381298028299,-3.04946076419972,
-46.5484395248738));
#36604=CARTESIAN_POINT('Ctrl Pts',(-5.95549339308817,-3.21315848424618,
-46.5396901905707));
#36605=CARTESIAN_POINT('Ctrl Pts',(-5.86717414225637,-3.37685558085381,
-46.5309408895891));
#36606=CARTESIAN_POINT('Ctrl Pts',(-5.77210188843887,-3.53690907700293,
-46.5221915886075));
#36607=CARTESIAN_POINT('Ctrl Pts',(-5.67059953311186,-3.69277537024277,
-46.513442287626));
#36608=CARTESIAN_POINT('Ctrl Pts',(-5.56909755592504,-3.84864108281321,
-46.5046930192394));
#36609=CARTESIAN_POINT('Ctrl Pts',(-5.46116568154745,-4.00031938355131,
-46.4959437508527));
#36610=CARTESIAN_POINT('Ctrl Pts',(-5.34717048488137,-4.14729511918474,
-46.4871944824661));
#36611=CARTESIAN_POINT('Ctrl Pts',(-5.23317570343069,-4.29427031947465,
-46.4784452459478));
#36612=CARTESIAN_POINT('Ctrl Pts',(-5.11311781951318,-4.43654276249819,
-46.4696960094294));
#36613=CARTESIAN_POINT('Ctrl Pts',(-4.98740458929022,-4.57362924412625,
-46.4609467729111));
#36614=CARTESIAN_POINT('Ctrl Pts',(-4.86169180652513,-4.71071523781502,
-46.4521975675344));
#36615=CARTESIAN_POINT('Ctrl Pts',(-4.7303239114134,-4.84261509584716,-46.4434483621577));
#36616=CARTESIAN_POINT('Ctrl Pts',(-4.59374706947091,-4.96888084599817,
-46.434699156781));
#36617=CARTESIAN_POINT('Ctrl Pts',(-4.45717070231289,-5.09514615720933,
-46.4259499818193));
#36618=CARTESIAN_POINT('Ctrl Pts',(-4.31538563497163,-5.21577720520747,
-46.4172008068576));
#36619=CARTESIAN_POINT('Ctrl Pts',(-4.16887340951861,-5.33036429293615,
-46.4084516318959));
#36620=CARTESIAN_POINT('Ctrl Pts',(-4.02236168122368,-5.44495099183791,
-46.3997024866226));
#36621=CARTESIAN_POINT('Ctrl Pts',(-3.87112305263094,-5.55349359497987,
-46.3909533413494));
#36622=CARTESIAN_POINT('Ctrl Pts',(-3.71567116928941,-5.65562346357247,
-46.3822041960762));
#36623=CARTESIAN_POINT('Ctrl Pts',(-3.56021980053267,-5.75775299408954,
-46.3734550797648));
#36624=CARTESIAN_POINT('Ctrl Pts',(-3.4005554444205,-5.85346967519898,-46.3647059634534));
#36625=CARTESIAN_POINT('Ctrl Pts',(-3.2372203588682,-5.94244843041395,-46.3559568471421));
#36626=CARTESIAN_POINT('Ctrl Pts',(-3.0738858004348,-6.03142689847455,-46.3472077590661));
#36627=CARTESIAN_POINT('Ctrl Pts',(-2.90688078789226,-6.113667347079,-46.3384586709901));
#36628=CARTESIAN_POINT('Ctrl Pts',(-2.7367725061041,-6.18889047001421,-46.3297095829141));
#36629=CARTESIAN_POINT('Ctrl Pts',(-2.56666475916939,-6.26411335643332,
-46.3209605223469));
#36630=CARTESIAN_POINT('Ctrl Pts',(-2.39345402457085,-6.33231884545259,
-46.3122114617797));
#36631=CARTESIAN_POINT('Ctrl Pts',(-2.21772855944043,-6.3932752980489,-46.3034624012125));
#36632=CARTESIAN_POINT('Ctrl Pts',(-2.04200363223579,-6.45423156404706,
-46.2947133674277));
#36633=CARTESIAN_POINT('Ctrl Pts',(-1.86376426061031,-6.50793874412453,
-46.2859643336429));
#36634=CARTESIAN_POINT('Ctrl Pts',(-1.68361577621695,-6.5542144394331,-46.2772152998581));
#36635=CARTESIAN_POINT('Ctrl Pts',(-1.5034678283323,-6.60048999692584,-46.2684662921292));
#36636=CARTESIAN_POINT('Ctrl Pts',(-1.32141105657409,-6.63933404265157,
-46.2597172844003));
#36637=CARTESIAN_POINT('Ctrl Pts',(-1.13806375346565,-6.67061465631524,
-46.2509682766715));
#36638=CARTESIAN_POINT('Ctrl Pts',(-0.954716981170515,-6.70189517941763,
-46.242219294272));
#36639=CARTESIAN_POINT('Ctrl Pts',(-0.770079967442999,-6.72561226608995,
-46.2334703118726));
#36640=CARTESIAN_POINT('Ctrl Pts',(-0.584779764073998,-6.74168536995977,
-46.2247213294732));
#36641=CARTESIAN_POINT('Ctrl Pts',(-0.391489587593831,-6.75845153117868,
-46.2155950990576));
#36642=CARTESIAN_POINT('Ctrl Pts',(-0.197478091806054,-6.76689985146392,
-46.2064688686419));
#36643=CARTESIAN_POINT('Ctrl Pts',(-0.00346214753179392,-6.76699911434415,
-46.1973426382263));
#36644=CARTESIAN_POINT('Ctrl Pts',(0.1844907984839,-6.76709527525937,-46.1885016025112));
#36645=CARTESIAN_POINT('Ctrl Pts',(0.372447602154062,-6.75935633790767,
-46.1796605667961));
#36646=CARTESIAN_POINT('Ctrl Pts',(0.559756448193523,-6.74380914014519,
-46.170819531081));
#36647=CARTESIAN_POINT('Ctrl Pts',(0.745136131042637,-6.72842206873162,
-46.1620695524676));
#36648=CARTESIAN_POINT('Ctrl Pts',(0.929880851944298,-6.70538686355734,
-46.1533195738543));
#36649=CARTESIAN_POINT('Ctrl Pts',(1.11336305057386,-6.67478177303325,-46.144569595241));
#36650=CARTESIAN_POINT('Ctrl Pts',(1.29684337090055,-6.64417699581274,-46.1358197062011));
#36651=CARTESIAN_POINT('Ctrl Pts',(1.4790609120513,-6.60600253548073,-46.1270698171611));
#36652=CARTESIAN_POINT('Ctrl Pts',(1.6593967109517,-6.56038806441225,-46.1183199281211));
#36653=CARTESIAN_POINT('Ctrl Pts',(1.83973072369116,-6.51477404513862,-46.1095701257456));
#36654=CARTESIAN_POINT('Ctrl Pts',(2.01818275356999,-6.46172023288673,-46.1008203233701));
#36655=CARTESIAN_POINT('Ctrl Pts',(2.19414664033296,-6.40140683918118,-46.0920705209946));
#36656=CARTESIAN_POINT('Ctrl Pts',(2.37010884271224,-6.3410940228151,-46.0833208023751));
#36657=CARTESIAN_POINT('Ctrl Pts',(2.54358267847766,-6.27352185699808,-46.0745710837555));
#36658=CARTESIAN_POINT('Ctrl Pts',(2.71397890841697,-6.19891986435281,-46.065821365136));
#36659=CARTESIAN_POINT('Ctrl Pts',(2.88437356388903,-6.12431856103262,-46.0570717273642));
#36660=CARTESIAN_POINT('Ctrl Pts',(3.05169040787139,-6.04268767582574,-46.0483220895923));
#36661=CARTESIAN_POINT('Ctrl Pts',(3.21536112512026,-5.9543044795396,-46.0395724518205));
#36662=CARTESIAN_POINT('Ctrl Pts',(3.37903038442812,-5.8659220705506,-46.0308228919884));
#36663=CARTESIAN_POINT('Ctrl Pts',(3.5390533297994,-5.77078760703397,-46.0220733321564));
#36664=CARTESIAN_POINT('Ctrl Pts',(3.69488643041856,-5.66922422085322,-46.0133237723243));
#36665=CARTESIAN_POINT('Ctrl Pts',(3.85071819468712,-5.56766170563179,-46.0045742875243));
#36666=CARTESIAN_POINT('Ctrl Pts',(4.00235994599199,-5.4596705345627,-45.9958248027243));
#36667=CARTESIAN_POINT('Ctrl Pts',(4.14929662974281,-5.34561750206699,-45.9870753179243));
#36668=CARTESIAN_POINT('Ctrl Pts',(4.29623210225016,-5.23156540974489,-45.978325905249));
#36669=CARTESIAN_POINT('Ctrl Pts',(4.4384623584208,-5.11145173172218,-45.9695764925736));
#36670=CARTESIAN_POINT('Ctrl Pts',(4.57550431797384,-4.98568443006602,-45.9608270798983));
#36671=CARTESIAN_POINT('Ctrl Pts',(4.71254519337452,-4.8599181233673,-45.9520777364404));
#36672=CARTESIAN_POINT('Ctrl Pts',(4.84439764314945,-4.72849847631141,-45.9433283929825));
#36673=CARTESIAN_POINT('Ctrl Pts',(4.9706138419665,-4.59187184425383,-45.9345790495246));
#36674=CARTESIAN_POINT('Ctrl Pts',(5.09682908420175,-4.45524624767783,-45.9258297723772));
#36675=CARTESIAN_POINT('Ctrl Pts',(5.21740796650144,-4.31341395556925,-45.9170804952299));
#36676=CARTESIAN_POINT('Ctrl Pts',(5.33194095942229,-4.16685668162884,-45.9083312180825));
#36677=CARTESIAN_POINT('Ctrl Pts',(5.44647312235122,-4.0203004697523,-45.8995820043389));
#36678=CARTESIAN_POINT('Ctrl Pts',(5.55495930712287,-3.8690195703555,-45.8908327905954));
#36679=CARTESIAN_POINT('Ctrl Pts',(5.65703106079802,-3.71352778058364,-45.8820835768519));
#36680=CARTESIAN_POINT('Ctrl Pts',(5.75910210868741,-3.55803706597595,-45.8733344236057));
#36681=CARTESIAN_POINT('Ctrl Pts',(5.85475865698552,-3.39833575880895,-45.8645852703595));
#36682=CARTESIAN_POINT('Ctrl Pts',(5.94367583069064,-3.23496624706719,-45.8558361171133));
#36683=CARTESIAN_POINT('Ctrl Pts',(6.03259241910078,-3.07159781070098,-45.8470870214582));
#36684=CARTESIAN_POINT('Ctrl Pts',(6.11476958470968,-2.90456146975833,-45.838337925803));
#36685=CARTESIAN_POINT('Ctrl Pts',(6.18992823574386,-2.73442451648256,-45.8295888301479));
#36686=CARTESIAN_POINT('Ctrl Pts',(6.26508641700941,-2.56428862662402,-45.8208397891778));
#36687=CARTESIAN_POINT('Ctrl Pts',(6.33322605570308,-2.39105242531249,-45.8120907482077));
#36688=CARTESIAN_POINT('Ctrl Pts',(6.39411573747782,-2.21530425353686,-45.8033417072375));
#36689=CARTESIAN_POINT('Ctrl Pts',(6.45500505889142,-2.03955712188509,-45.7945927180465));
#36690=CARTESIAN_POINT('Ctrl Pts',(6.50864441544947,-1.8612983202551,-45.7858437288555));
#36691=CARTESIAN_POINT('Ctrl Pts',(6.55485164049925,-1.68113324012237,-45.7770947396645));
#36692=CARTESIAN_POINT('Ctrl Pts',(6.60199852639128,-1.4973043591282,-45.7681678327876));
#36693=CARTESIAN_POINT('Ctrl Pts',(6.64140767441027,-1.31149113173566,-45.7592409259108));
#36694=CARTESIAN_POINT('Ctrl Pts',(6.67293975269618,-1.1243505044634,-45.7503140190339));
#36695=CARTESIAN_POINT('Ctrl Pts',(6.70384664831519,-0.940920291562845,
-45.7415641048499));
#36696=CARTESIAN_POINT('Ctrl Pts',(6.72718585889676,-0.756215114277056,
-45.7328141906659));
#36697=CARTESIAN_POINT('Ctrl Pts',(6.74287810451872,-0.570862389374271,
-45.7240642764819));
#36698=CARTESIAN_POINT('Ctrl Pts',(6.75857004154128,-0.385513309567318,
-45.7153145343713));
#36699=CARTESIAN_POINT('Ctrl Pts',(6.76661529035558,-0.199516993258512,
-45.7065647922607));
#36700=CARTESIAN_POINT('Ctrl Pts',(6.76698652348896,-0.013505218204444,
-45.6978150501501));
#36701=CARTESIAN_POINT('Ctrl Pts',(6.76735774981522,0.172503146038539,-45.6890654684795));
#36702=CARTESIAN_POINT('Ctrl Pts',(6.76005524147481,0.358526681833149,-45.6803158868089));
#36703=CARTESIAN_POINT('Ctrl Pts',(6.74510380214884,0.543933542114578,-45.6715663051382));
#36704=CARTESIAN_POINT('Ctrl Pts',(6.73015261710983,0.729337249084396,-45.6628168722763));
#36705=CARTESIAN_POINT('Ctrl Pts',(6.7075527844461,0.914124015854301,-45.6540674394144));
#36706=CARTESIAN_POINT('Ctrl Pts',(6.67738106408296,1.09766621749346,-45.6453180065524));
#36707=CARTESIAN_POINT('Ctrl Pts',(6.64720981677262,1.28120554143281,-45.6365687108701));
#36708=CARTESIAN_POINT('Ctrl Pts',(6.60946696581532,1.46350005650579,-45.6278194151877));
#36709=CARTESIAN_POINT('Ctrl Pts',(6.56428070011004,1.64393062206493,-45.6190701195054));
#36710=CARTESIAN_POINT('Ctrl Pts',(6.51909508282753,1.82435859844609,-45.6103209493754));
#36711=CARTESIAN_POINT('Ctrl Pts',(6.46646633415675,2.00292240086518,-45.6015717792454));
#36712=CARTESIAN_POINT('Ctrl Pts',(6.40657319597208,2.17901557696408,-45.5928226091154));
#36713=CARTESIAN_POINT('Ctrl Pts',(6.34668083768312,2.35510646007389,-45.5840735529124));
#36714=CARTESIAN_POINT('Ctrl Pts',(6.27952437143903,2.52872650996487,-45.5753244967093));
#36715=CARTESIAN_POINT('Ctrl Pts',(6.20533187335154,2.69928607997882,-45.5665754405062));
#36716=CARTESIAN_POINT('Ctrl Pts',(6.12831449784272,2.87633970115356,-45.5574932642173));
#36717=CARTESIAN_POINT('Ctrl Pts',(6.04371489463173,3.0500949056231,-45.5484110879285));
#36718=CARTESIAN_POINT('Ctrl Pts',(5.95184265120511,3.21991584599594,-45.5393289116397));
#36719=CARTESIAN_POINT('Ctrl Pts',(5.86333281335513,3.38352155905265,-45.5305791312852));
#36720=CARTESIAN_POINT('Ctrl Pts',(5.76807337235705,3.54347560903791,-45.5218293509308));
#36721=CARTESIAN_POINT('Ctrl Pts',(5.66638790086376,3.69923467178616,-45.5130795705764));
#36722=CARTESIAN_POINT('Ctrl Pts',(5.56470608502762,3.85498813489736,-45.5043301047821));
#36723=CARTESIAN_POINT('Ctrl Pts',(5.4565988576697,4.00654667256237,-45.4955806389879));
#36724=CARTESIAN_POINT('Ctrl Pts',(5.34243340580524,4.1533955150619,-45.4868311731936));
#36725=CARTESIAN_POINT('Ctrl Pts',(5.22827145140602,4.30023985883861,-45.4780819754397));
#36726=CARTESIAN_POINT('Ctrl Pts',(5.10805181978088,4.44237456993045,-45.4693327776858));
#36727=CARTESIAN_POINT('Ctrl Pts',(4.9821828128254,4.57931691626461,-45.460583579932));
#36728=CARTESIAN_POINT('Ctrl Pts',(4.85631699296224,4.71625579512166,-45.451834603714));
#36729=CARTESIAN_POINT('Ctrl Pts',(4.7248022779184,4.84800236135767,-45.443085627496));
#36730=CARTESIAN_POINT('Ctrl Pts',(4.58808530848123,4.974109186789,-45.434336651278));
#36731=CARTESIAN_POINT('Ctrl Pts',(4.45135945056974,5.10022421089005,-45.4255871062568));
#36732=CARTESIAN_POINT('Ctrl Pts',(4.30943087208039,5.22069856611988,-45.4168375612356));
#36733=CARTESIAN_POINT('Ctrl Pts',(4.16278164322461,5.33512305301689,-45.4080880162144));
#36734=CARTESIAN_POINT('Ctrl Pts',(4.01614103534387,5.44954081331429,-45.3993389855471));
#36735=CARTESIAN_POINT('Ctrl Pts',(3.86478055833414,5.55790924068337,-45.3905899548799));
#36736=CARTESIAN_POINT('Ctrl Pts',(3.70921425811957,5.65986029751287,-45.3818409242126));
#36737=CARTESIAN_POINT('Ctrl Pts',(3.55364584530133,5.76181273884646,-45.3730917747328));
#36738=CARTESIAN_POINT('Ctrl Pts',(3.39387173464365,5.85734747818051,-45.3643426252529));
#36739=CARTESIAN_POINT('Ctrl Pts',(3.23043456092434,5.94614005448792,-45.3555934757731));
#36740=CARTESIAN_POINT('Ctrl Pts',(3.1869076880641,5.96978744811272,-45.35326338704));
#36741=CARTESIAN_POINT('Ctrl Pts',(3.1431211498289,5.99295688499296,-45.350933298307));
#36742=CARTESIAN_POINT('Ctrl Pts',(3.09908550384718,6.01564277861014,-45.3486032095739));
#36743=CARTESIAN_POINT('Origin',(0.,0.,-63.6971797838103));
#36744=CARTESIAN_POINT('',(3.09908550384721,6.01564277861012,-42.9543661083715));
#36745=CARTESIAN_POINT('',(3.09908550384722,6.01564277861012,-43.3486032095739));
#36746=CARTESIAN_POINT('',(3.09908550384721,6.01564277861012,-63.6971797838103));
#36747=CARTESIAN_POINT('',(-6.76699974817481,-0.00184613164357677,-44.3028202161442));
#36748=CARTESIAN_POINT('Ctrl Pts',(-6.76699974817481,-0.00184613164357843,
-44.3028202161442));
#36749=CARTESIAN_POINT('Ctrl Pts',(-6.76694808985158,-0.191199833202375,
-44.2939578052881));
#36750=CARTESIAN_POINT('Ctrl Pts',(-6.75894451409944,-0.380318812548052,
-44.2850953944321));
#36751=CARTESIAN_POINT('Ctrl Pts',(-6.74307314779978,-0.568553887878346,
-44.276232983576));
#36752=CARTESIAN_POINT('Ctrl Pts',(-6.72716340080505,-0.75724415987488,
-44.2673491413269));
#36753=CARTESIAN_POINT('Ctrl Pts',(-6.70334785009519,-0.945046000564817,
-44.2584652990779));
#36754=CARTESIAN_POINT('Ctrl Pts',(-6.67176184369028,-1.13131909781393,
-44.2495814568288));
#36755=CARTESIAN_POINT('Ctrl Pts',(-6.64006191419913,-1.31826403707587,
-44.2406655727092));
#36756=CARTESIAN_POINT('Ctrl Pts',(-6.60053546746428,-1.50366894112442,
-44.2317496885897));
#36757=CARTESIAN_POINT('Ctrl Pts',(-6.55336891665049,-1.68690392206526,
-44.2228338044701));
#36758=CARTESIAN_POINT('Ctrl Pts',(-6.5061169547119,-1.87047071242522,-44.2139017751019));
#36759=CARTESIAN_POINT('Ctrl Pts',(-6.45119731553769,-2.05185948326789,
-44.2049697457337));
#36760=CARTESIAN_POINT('Ctrl Pts',(-6.38884548165277,-2.23045789280251,
-44.1960377163655));
#36761=CARTESIAN_POINT('Ctrl Pts',(-6.32631832791001,-2.40955848239852,
-44.1870805720645));
#36762=CARTESIAN_POINT('Ctrl Pts',(-6.25631725423912,-2.58585277136457,
-44.1781234277634));
#36763=CARTESIAN_POINT('Ctrl Pts',(-6.17912614081321,-2.75874774778681,
-44.1691662834624));
#36764=CARTESIAN_POINT('Ctrl Pts',(-6.12134972749879,-2.88815709524164,
-44.1624619926666));
#36765=CARTESIAN_POINT('Ctrl Pts',(-6.05954620669863,-3.01566253252796,
-44.1557577018709));
#36766=CARTESIAN_POINT('Ctrl Pts',(-5.99385085683238,-3.14102545453707,
-44.1490534110752));
#36767=CARTESIAN_POINT('Ctrl Pts',(-5.91476439462841,-3.29194191990997,
-44.1409825408888));
#36768=CARTESIAN_POINT('Ctrl Pts',(-5.82982994497036,-3.44014504877998,
-44.1329116707024));
#36769=CARTESIAN_POINT('Ctrl Pts',(-5.73925764505817,-3.58513747067549,
-44.124840800516));
#36770=CARTESIAN_POINT('Ctrl Pts',(-5.64879805533318,-3.72994946077196,
-44.1167799739002));
#36771=CARTESIAN_POINT('Ctrl Pts',(-5.55271477032055,-3.87155838153066,
-44.1087191472844));
#36772=CARTESIAN_POINT('Ctrl Pts',(-5.45126531353203,-4.00948818198565,
-44.1006583206686));
#36773=CARTESIAN_POINT('Ctrl Pts',(-5.34991985638948,-4.14727658542512,
-44.0926057575087));
#36774=CARTESIAN_POINT('Ctrl Pts',(-5.24321939394609,-4.28139307624674,
-44.0845531943488));
#36775=CARTESIAN_POINT('Ctrl Pts',(-5.13146649844571,-4.41138760202834,
-44.076500631189));
#36776=CARTESIAN_POINT('Ctrl Pts',(-5.01980369529258,-4.54127732952346,
-44.0684545598011));
#36777=CARTESIAN_POINT('Ctrl Pts',(-4.90309680799491,-4.6670514245402,-44.0604084884132));
#36778=CARTESIAN_POINT('Ctrl Pts',(-4.78169065075232,-4.78829025023628,
-44.0523624170253));
#36779=CARTESIAN_POINT('Ctrl Pts',(-4.66035581185737,-4.9094578558813,-44.0443210721894));
#36780=CARTESIAN_POINT('Ctrl Pts',(-4.53432746171645,-5.02609523294419,
-44.0362797273536));
#36781=CARTESIAN_POINT('Ctrl Pts',(-4.40398941018188,-5.13781726757636,
-44.0282383825177));
#36782=CARTESIAN_POINT('Ctrl Pts',(-4.27113884206445,-5.25169295926709,
-44.0200420252966));
#36783=CARTESIAN_POINT('Ctrl Pts',(-4.13381098147026,-5.36046157063303,
-44.0118456680756));
#36784=CARTESIAN_POINT('Ctrl Pts',(-3.99245053096405,-5.4637558288969,-44.0036493108545));
#36785=CARTESIAN_POINT('Ctrl Pts',(-3.85380762379097,-5.56506433639463,
-43.995610522146));
#36786=CARTESIAN_POINT('Ctrl Pts',(-3.71128609225324,-5.66110685131684,
-43.9875717334375));
#36787=CARTESIAN_POINT('Ctrl Pts',(-3.5653372671532,-5.75157884162676,-43.979532944729));
#36788=CARTESIAN_POINT('Ctrl Pts',(-3.41937282420635,-5.84206051325946,
-43.9714932957973));
#36789=CARTESIAN_POINT('Ctrl Pts',(-3.26998067483839,-5.92697027649108,
-43.9634536468655));
#36790=CARTESIAN_POINT('Ctrl Pts',(-3.11763911877259,-6.00604822866907,
-43.9554139979338));
#36791=CARTESIAN_POINT('Ctrl Pts',(-2.96525109657065,-6.08515030064068,
-43.9473718968056));
#36792=CARTESIAN_POINT('Ctrl Pts',(-2.80991220829138,-6.15841684894291,
-43.9393297956774));
#36793=CARTESIAN_POINT('Ctrl Pts',(-2.65212306967938,-6.22563508593898,
-43.9312876945493));
#36794=CARTESIAN_POINT('Ctrl Pts',(-2.48900916757461,-6.29512167434095,
-43.9229742041045));
#36795=CARTESIAN_POINT('Ctrl Pts',(-2.32327715088782,-6.35814442408832,
-43.9146607136597));
#36796=CARTESIAN_POINT('Ctrl Pts',(-2.15549868507928,-6.414523709413,-43.906347223215));
#36797=CARTESIAN_POINT('Ctrl Pts',(-1.99291134311829,-6.46915860012097,
-43.8982909550442));
#36798=CARTESIAN_POINT('Ctrl Pts',(-1.82840267569508,-6.51755497307224,
-43.8902346868735));
#36799=CARTESIAN_POINT('Ctrl Pts',(-1.66250426678463,-6.5596012502989,-43.8821784187027));
#36800=CARTESIAN_POINT('Ctrl Pts',(-1.48866059740945,-6.60366122148641,
-43.8737363171209));
#36801=CARTESIAN_POINT('Ctrl Pts',(-1.31329127299102,-6.64074779740795,
-43.8652942155392));
#36802=CARTESIAN_POINT('Ctrl Pts',(-1.13701442677451,-6.67079359546573,
-43.8568521139574));
#36803=CARTESIAN_POINT('Ctrl Pts',(-0.960737580557974,-6.70083939352352,
-43.8484100123757));
#36804=CARTESIAN_POINT('Ctrl Pts',(-0.783553680715682,-6.72384444012432,
-43.8399679107939));
#36805=CARTESIAN_POINT('Ctrl Pts',(-0.606080516427321,-6.73980381076536,
-43.8315258092121));
#36806=CARTESIAN_POINT('Ctrl Pts',(-0.430883212885349,-6.75555852339331,
-43.8231919665194));
#36807=CARTESIAN_POINT('Ctrl Pts',(-0.254847095583368,-6.76449787264988,
-43.8148581238268));
#36808=CARTESIAN_POINT('Ctrl Pts',(-0.0785367907614893,-6.76654424152365,
-43.8065242811341));
#36809=CARTESIAN_POINT('Ctrl Pts',(0.0975657100611083,-6.76858819849283,
-43.7982002609293));
#36810=CARTESIAN_POINT('Ctrl Pts',(0.273941409770814,-6.76375535531757,
-43.7898762407246));
#36811=CARTESIAN_POINT('Ctrl Pts',(0.450020024646737,-6.75201977021817,
-43.7815522205198));
#36812=CARTESIAN_POINT('Ctrl Pts',(0.625923392357247,-6.74029586528802,
-43.7732364850289));
#36813=CARTESIAN_POINT('Ctrl Pts',(0.801529919411688,-6.72168292904772,
-43.7649207495381));
#36814=CARTESIAN_POINT('Ctrl Pts',(0.976268551134108,-6.69620703951622,
-43.7566050140472));
#36815=CARTESIAN_POINT('Ctrl Pts',(1.15086528597577,-6.67075183773546,-43.7482960313672));
#36816=CARTESIAN_POINT('Ctrl Pts',(1.32459518710004,-6.63844483751473,-43.7399870486871));
#36817=CARTESIAN_POINT('Ctrl Pts',(1.49689132595528,-6.59936401165141,-43.7316780660071));
#36818=CARTESIAN_POINT('Ctrl Pts',(1.669079103131,-6.56030776477144,-43.72337430907));
#36819=CARTESIAN_POINT('Ctrl Pts',(1.83983457682786,-6.51448625918412,-43.7150705521328));
#36820=CARTESIAN_POINT('Ctrl Pts',(2.00859980708244,-6.46202876927892,-43.7067667951956));
#36821=CARTESIAN_POINT('Ctrl Pts',(2.17729652272206,-6.40959257584999,-43.6984664093836));
#36822=CARTESIAN_POINT('Ctrl Pts',(2.34400427328645,-6.3505258692829,-43.6901660235716));
#36823=CARTESIAN_POINT('Ctrl Pts',(2.50817882562078,-6.28500819241372,-43.6818656377596));
#36824=CARTESIAN_POINT('Ctrl Pts',(2.67231875781387,-6.21950433151781,-43.6735670022829));
#36825=CARTESIAN_POINT('Ctrl Pts',(2.83392623317169,-6.1475523392859,-43.6652683668063));
#36826=CARTESIAN_POINT('Ctrl Pts',(2.9924753714994,-6.06938054095882,-43.6569697313297));
#36827=CARTESIAN_POINT('Ctrl Pts',(3.15101739327636,-5.99121225140874,-43.6486714683411));
#36828=CARTESIAN_POINT('Ctrl Pts',(3.30650103974126,-5.90682486604122,-43.6403732053525));
#36829=CARTESIAN_POINT('Ctrl Pts',(3.45842331220062,-5.81649354797436,-43.6320749423639));
#36830=CARTESIAN_POINT('Ctrl Pts',(3.61036398179866,-5.72615129117047,-43.6237756744911));
#36831=CARTESIAN_POINT('Ctrl Pts',(3.75874211943104,-5.62986384565985,-43.6154764066183));
#36832=CARTESIAN_POINT('Ctrl Pts',(3.90308192686874,-5.52795083843467,-43.6071771387455));
#36833=CARTESIAN_POINT('Ctrl Pts',(4.0475230841156,-5.42596627185234,-43.598872043449));
#36834=CARTESIAN_POINT('Ctrl Pts',(4.18791996077287,-5.31834845149992,-43.5905669481525));
#36835=CARTESIAN_POINT('Ctrl Pts',(4.32382748084337,-5.2054591455417,-43.582261852856));
#36836=CARTESIAN_POINT('Ctrl Pts',(4.45978455986293,-5.09252867427223,-43.5739537290899));
#36837=CARTESIAN_POINT('Ctrl Pts',(4.59124875666223,-4.97432311395071,-43.5656456053238));
#36838=CARTESIAN_POINT('Ctrl Pts',(4.71781021000627,-4.85124270907575,-43.5573374815577));
#36839=CARTESIAN_POINT('Ctrl Pts',(4.84450619744388,-4.72803147044162,-43.549020526304));
#36840=CARTESIAN_POINT('Ctrl Pts',(4.96628878450176,-4.59993528176384,-43.5407035710503));
#36841=CARTESIAN_POINT('Ctrl Pts',(5.08278617928712,-4.46739002725841,-43.5323866157967));
#36842=CARTESIAN_POINT('Ctrl Pts',(5.16864298677856,-4.36970619131561,-43.5262571463141));
#36843=CARTESIAN_POINT('Ctrl Pts',(5.2516299655268,-4.2696065946261,-43.5201276768316));
#36844=CARTESIAN_POINT('Ctrl Pts',(5.33161298603271,-4.16727632479145,-43.5139982073491));
#36845=CARTESIAN_POINT('Ctrl Pts',(5.44188980360044,-4.02618817349592,-43.5055471838239));
#36846=CARTESIAN_POINT('Ctrl Pts',(5.54665617839165,-3.88060068047054,-43.4970961602988));
#36847=CARTESIAN_POINT('Ctrl Pts',(5.64554192698029,-3.73097110022413,-43.4886451367736));
#36848=CARTESIAN_POINT('Ctrl Pts',(5.74434060960638,-3.58147326437585,-43.4802015541234));
#36849=CARTESIAN_POINT('Ctrl Pts',(5.83726880428459,-3.42794071020951,-43.4717579714733));
#36850=CARTESIAN_POINT('Ctrl Pts',(5.9239978090905,-3.27086211233231,-43.4633143888231));
#36851=CARTESIAN_POINT('Ctrl Pts',(6.01066224145046,-3.1139004643647,-43.4548770926833));
#36852=CARTESIAN_POINT('Ctrl Pts',(6.09113652499687,-2.95339832492342,-43.4464397965435));
#36853=CARTESIAN_POINT('Ctrl Pts',(6.16513614727734,-2.78987191203006,-43.4380025004037));
#36854=CARTESIAN_POINT('Ctrl Pts',(6.23908297646957,-2.62646216276389,-43.4295712236313));
#36855=CARTESIAN_POINT('Ctrl Pts',(6.30656422178593,-2.46003274498916,-43.421139946859));
#36856=CARTESIAN_POINT('Ctrl Pts',(6.3673419701728,-2.29112313830488,-43.4127086700866));
#36857=CARTESIAN_POINT('Ctrl Pts',(6.42809366701662,-2.12228593239238,-43.4042810072647));
#36858=CARTESIAN_POINT('Ctrl Pts',(6.48214748308018,-1.95097096824125,-43.3958533444428));
#36859=CARTESIAN_POINT('Ctrl Pts',(6.52931393489892,-1.77773691516344,-43.3874256816209));
#36860=CARTESIAN_POINT('Ctrl Pts',(6.57646586701831,-1.60455619037872,-43.3790006131669));
#36861=CARTESIAN_POINT('Ctrl Pts',(6.61673457613478,-1.42945787428303,-43.3705755447129));
#36862=CARTESIAN_POINT('Ctrl Pts',(6.64998056898124,-1.25301533596841,-43.3621504762589));
#36863=CARTESIAN_POINT('Ctrl Pts',(6.65907769025789,-1.20473525671728,-43.3598451196452));
#36864=CARTESIAN_POINT('Ctrl Pts',(6.6676492868259,-1.15635460302723,-43.3575397630314));
#36865=CARTESIAN_POINT('Ctrl Pts',(6.6756931643768,-1.10788527162916,-43.3552344064176));
#36866=CARTESIAN_POINT('Ctrl Pts',(6.70576664103086,-0.9266739967168,-43.3466154178931));
#36867=CARTESIAN_POINT('Ctrl Pts',(6.72844643978489,-0.74430347567481,-43.3379964293687));
#36868=CARTESIAN_POINT('Ctrl Pts',(6.74367356783639,-0.561387397850085,
-43.3293774408442));
#36869=CARTESIAN_POINT('Ctrl Pts',(6.75890981829649,-0.378361736970917,
-43.3207532887764));
#36870=CARTESIAN_POINT('Ctrl Pts',(6.76668446241367,-0.194790170145841,
-43.3121291367086));
#36871=CARTESIAN_POINT('Ctrl Pts',(6.76699058382844,-0.0112888607616132,
-43.3035049846408));
#36872=CARTESIAN_POINT('Ctrl Pts',(6.76730718998401,0.178497417835661,-43.2945854530446));
#36873=CARTESIAN_POINT('Ctrl Pts',(6.75963462531111,0.368208183191211,-43.2856659214484));
#36874=CARTESIAN_POINT('Ctrl Pts',(6.74402370307352,0.557165408458398,-43.2767463898521));
#36875=CARTESIAN_POINT('Ctrl Pts',(6.72890163442433,0.74020546776821,-43.2681061719929));
#36876=CARTESIAN_POINT('Ctrl Pts',(6.70633094418731,0.922538170032766,-43.2594659541336));
#36877=CARTESIAN_POINT('Ctrl Pts',(6.67641033196807,1.10355519988358,-43.2508257362744));
#36878=CARTESIAN_POINT('Ctrl Pts',(6.64503884695588,1.29334988046378,-43.2417665478096));
#36879=CARTESIAN_POINT('Ctrl Pts',(6.60558699184346,1.48169774089452,-43.2327073593449));
#36880=CARTESIAN_POINT('Ctrl Pts',(6.5582282408616,1.66791227010457,-43.2236481708802));
#36881=CARTESIAN_POINT('Ctrl Pts',(6.51086948987974,1.85412679931461,-43.2145889824155));
#36882=CARTESIAN_POINT('Ctrl Pts',(6.45560398477864,2.03820764036222,-43.2055297939508));
#36883=CARTESIAN_POINT('Ctrl Pts',(6.39266447184202,2.21948866869125,-43.1964706054861));
#36884=CARTESIAN_POINT('Ctrl Pts',(6.32983399719578,2.4004556403572,-43.1874271114298));
#36885=CARTESIAN_POINT('Ctrl Pts',(6.25929899903813,2.57879948537713,-43.1783836173735));
#36886=CARTESIAN_POINT('Ctrl Pts',(6.18129258247601,2.75389015936132,-43.1693401233172));
#36887=CARTESIAN_POINT('Ctrl Pts',(6.10335751809788,2.92882067854624,-43.1603049013119));
#36888=CARTESIAN_POINT('Ctrl Pts',(6.01796477638797,3.10050375032539,-43.1512696793065));
#36889=CARTESIAN_POINT('Ctrl Pts',(5.92539546120855,3.26832948588252,-43.1422344573012));
#36890=CARTESIAN_POINT('Ctrl Pts',(5.83298923301035,3.43585954902888,-43.1332151533901));
#36891=CARTESIAN_POINT('Ctrl Pts',(5.73343179380139,3.59954563808829,-43.124195849479));
#36892=CARTESIAN_POINT('Ctrl Pts',(5.62704991926297,3.75880276233305,-43.1151765455679));
#36893=CARTESIAN_POINT('Ctrl Pts',(5.52080150821676,3.91786008739161,-43.1061685570035));
#36894=CARTESIAN_POINT('Ctrl Pts',(5.40774587996794,4.07249933900003,-43.0971605684391));
#36895=CARTESIAN_POINT('Ctrl Pts',(5.28825414611462,4.2221626077286,-43.0881525798747));
#36896=CARTESIAN_POINT('Ctrl Pts',(5.16903228852759,4.37148785672257,-43.0791649361681));
#36897=CARTESIAN_POINT('Ctrl Pts',(5.04340348913918,4.5158593700586,-43.0701772924614));
#36898=CARTESIAN_POINT('Ctrl Pts',(4.91178000762963,4.65475092315903,-43.0611896487547));
#36899=CARTESIAN_POINT('Ctrl Pts',(4.7971450780809,4.77571583931213,-43.0533620340213));
#36900=CARTESIAN_POINT('Ctrl Pts',(4.67796377580275,4.89252443596965,-43.0455344192879));
#36901=CARTESIAN_POINT('Ctrl Pts',(4.55453438253712,5.00484820531924,-43.0377068045545));
#36902=CARTESIAN_POINT('Ctrl Pts',(4.42644270366481,5.12141476870089,-43.0295835181457));
#36903=CARTESIAN_POINT('Ctrl Pts',(4.2938320800799,5.23309795129149,-43.0214602317368));
#36904=CARTESIAN_POINT('Ctrl Pts',(4.15712023609244,5.33953559241538,-43.013336945328));
#36905=CARTESIAN_POINT('Ctrl Pts',(4.02042557568307,5.44595985518475,-43.0052146799509));
#36906=CARTESIAN_POINT('Ctrl Pts',(3.8796310125444,5.54713966762463,-42.9970924145737));
#36907=CARTESIAN_POINT('Ctrl Pts',(3.73518650007377,5.64275383209889,-42.9889701491966));
#36908=CARTESIAN_POINT('Ctrl Pts',(3.59070430238548,5.73839294207324,-42.9808457647404));
#36909=CARTESIAN_POINT('Ctrl Pts',(3.44257055979513,5.82846330339839,-42.9727213802842));
#36910=CARTESIAN_POINT('Ctrl Pts',(3.29126351222216,5.91268750173008,-42.9645969958281));
#36911=CARTESIAN_POINT('Ctrl Pts',(3.22775078772149,5.94804149475773,-42.9611867000092));
#36912=CARTESIAN_POINT('Ctrl Pts',(3.16367924124438,5.98236594975342,-42.9577764041903));
#36913=CARTESIAN_POINT('Ctrl Pts',(3.09908550384721,6.01564277861012,-42.9543661083715));
#36914=CARTESIAN_POINT('Ctrl Pts',(3.0990855038472,6.01564277861013,-44.9542932404068));
#36915=CARTESIAN_POINT('Ctrl Pts',(2.93974035442061,6.09773279972179,-44.9458699638642));
#36916=CARTESIAN_POINT('Ctrl Pts',(2.77713243321382,6.17348729536887,-44.9374466873216));
#36917=CARTESIAN_POINT('Ctrl Pts',(2.61179635165935,6.24266039581354,-44.929023410779));
#36918=CARTESIAN_POINT('Ctrl Pts',(2.44643549540071,6.31184386146758,-44.9205988720547));
#36919=CARTESIAN_POINT('Ctrl Pts',(2.27834597141802,6.37444383702415,-44.9121743333303));
#36920=CARTESIAN_POINT('Ctrl Pts',(2.10808193716495,6.43026278982429,-44.903749794606));
#36921=CARTESIAN_POINT('Ctrl Pts',(1.93776863827557,6.4860978934247,-44.8953228183038));
#36922=CARTESIAN_POINT('Ctrl Pts',(1.76527989151013,6.53514795865822,-44.8868958420016));
#36923=CARTESIAN_POINT('Ctrl Pts',(1.59118491255707,6.57726535682199,-44.8784688656995));
#36924=CARTESIAN_POINT('Ctrl Pts',(1.41693492337219,6.61942025536454,-44.8700343862082));
#36925=CARTESIAN_POINT('Ctrl Pts',(1.24107616860051,6.65463007328726,-44.8615999067169));
#36926=CARTESIAN_POINT('Ctrl Pts',(1.06418911290291,6.68279810648047,-44.8531654272256));
#36927=CARTESIAN_POINT('Ctrl Pts',(0.887220494001733,6.71097912804649,-44.8447270585681));
#36928=CARTESIAN_POINT('Ctrl Pts',(0.709222958974084,6.73211184457387,-44.8362886899105));
#36929=CARTESIAN_POINT('Ctrl Pts',(0.53078253786795,6.74615141376878,-44.827850321253));
#36930=CARTESIAN_POINT('Ctrl Pts',(0.352136780759709,6.76020713865864,-44.8194022423467));
#36931=CARTESIAN_POINT('Ctrl Pts',(0.173047452317599,6.76715338594818,-44.8109541634403));
#36932=CARTESIAN_POINT('Ctrl Pts',(-0.00589763809075682,6.76699743001761,
-44.802506084534));
#36933=CARTESIAN_POINT('Ctrl Pts',(-0.135794502656443,6.76688422106427,
-44.7963735946231));
#36934=CARTESIAN_POINT('Ctrl Pts',(-0.265615351294428,6.76302969989654,
-44.7902411047122));
#36935=CARTESIAN_POINT('Ctrl Pts',(-0.395136940195535,6.75545378183383,
-44.7841086148013));
#36936=CARTESIAN_POINT('Ctrl Pts',(-0.569186692347734,6.74527334263192,
-44.7758678392045));
#36937=CARTESIAN_POINT('Ctrl Pts',(-0.743083056888376,6.72834813911043,
-44.7676270636077));
#36938=CARTESIAN_POINT('Ctrl Pts',(-0.916264977606776,6.70468101335263,
-44.759386288011));
#36939=CARTESIAN_POINT('Ctrl Pts',(-1.08925508057305,6.6810401015024,-44.7511546399666));
#36940=CARTESIAN_POINT('Ctrl Pts',(-1.26153196597617,6.65067218414367,-44.7429229919222));
#36941=CARTESIAN_POINT('Ctrl Pts',(-1.43253615344517,6.61363207088756,-44.7346913438778));
#36942=CARTESIAN_POINT('Ctrl Pts',(-1.6033814097802,6.57662638267853,-44.7264673463195));
#36943=CARTESIAN_POINT('Ctrl Pts',(-1.77295597817241,6.53296092320099,-44.7182433487612));
#36944=CARTESIAN_POINT('Ctrl Pts',(-1.94070697447512,6.48274212345545,-44.7100193512029));
#36945=CARTESIAN_POINT('Ctrl Pts',(-2.10830976212087,6.43256769221458,-44.7018026195784));
#36946=CARTESIAN_POINT('Ctrl Pts',(-2.274091849296,6.37585156223714,-44.6935858879539));
#36947=CARTESIAN_POINT('Ctrl Pts',(-2.4375121244189,6.31275087765317,-44.6853691563294));
#36948=CARTESIAN_POINT('Ctrl Pts',(-2.60084867328491,6.24968252188596,-44.6771566344407));
#36949=CARTESIAN_POINT('Ctrl Pts',(-2.76182548894159,6.18023625398197,-44.668944112552));
#36950=CARTESIAN_POINT('Ctrl Pts',(-2.91991776853191,6.10461867973845,-44.6607315906633));
#36951=CARTESIAN_POINT('Ctrl Pts',(-3.07795718130282,6.02902639237581,-44.6525218150815));
#36952=CARTESIAN_POINT('Ctrl Pts',(-3.2331136590022,5.94726706318852,-44.6443120394996));
#36953=CARTESIAN_POINT('Ctrl Pts',(-3.38488341245071,5.85959497611533,-44.6361022639178));
#36954=CARTESIAN_POINT('Ctrl Pts',(-3.45117249775066,5.82130208621886,-44.6325164472351));
#36955=CARTESIAN_POINT('Ctrl Pts',(-3.51681578541824,5.78188181406435,-44.6289306305525));
#36956=CARTESIAN_POINT('Ctrl Pts',(-3.58177276483859,5.74135810249287,-44.6253448138698));
#36957=CARTESIAN_POINT('Ctrl Pts',(-3.74224821092904,5.6412447544015,-44.6164860963481));
#36958=CARTESIAN_POINT('Ctrl Pts',(-3.89836685099313,5.53449769543603,-44.6076273788264));
#36959=CARTESIAN_POINT('Ctrl Pts',(-4.04961600148761,5.42152185649892,-44.5987686613047));
#36960=CARTESIAN_POINT('Ctrl Pts',(-4.20114811485178,5.30833465791128,-44.5898933705452));
#36961=CARTESIAN_POINT('Ctrl Pts',(-4.34779232508549,5.18889554673532,-44.5810180797858));
#36962=CARTESIAN_POINT('Ctrl Pts',(-4.48906995450461,5.06364887640958,-44.5721427890263));
#36963=CARTESIAN_POINT('Ctrl Pts',(-4.63074884415681,4.93804647737905,-44.5632422904455));
#36964=CARTESIAN_POINT('Ctrl Pts',(-4.76703045601414,4.8066036842549,-44.5543417918647));
#36965=CARTESIAN_POINT('Ctrl Pts',(-4.89747169536168,4.66980299296782,-44.545441293284));
#36966=CARTESIAN_POINT('Ctrl Pts',(-5.02808951319042,4.5328171144009,-44.5365287460863));
#36967=CARTESIAN_POINT('Ctrl Pts',(-5.15285099136919,4.3904590415754,-44.5276161988886));
#36968=CARTESIAN_POINT('Ctrl Pts',(-5.2713532987551,4.24324444260565,-44.5187036516909));
#36969=CARTESIAN_POINT('Ctrl Pts',(-5.39011727080803,4.09570477942518,-44.5097714247187));
#36970=CARTESIAN_POINT('Ctrl Pts',(-5.50259426477459,3.94328734380879,-44.5008391977464));
#36971=CARTESIAN_POINT('Ctrl Pts',(-5.60842310688594,3.78653921862007,-44.4919069707742));
#36972=CARTESIAN_POINT('Ctrl Pts',(-5.70844358335701,3.63839413969322,-44.4834649848289));
#36973=CARTESIAN_POINT('Ctrl Pts',(-5.80252592468991,3.48638109405627,-44.4750229988836));
#36974=CARTESIAN_POINT('Ctrl Pts',(-5.89040300023832,3.33098206161237,-44.4665810129382));
#36975=CARTESIAN_POINT('Ctrl Pts',(-5.97776970194635,3.17648555807587,-44.4581880564897));
#36976=CARTESIAN_POINT('Ctrl Pts',(-6.0591653667354,3.01835334963305,-44.4497951000411));
#36977=CARTESIAN_POINT('Ctrl Pts',(-6.13428132641641,2.85707570924869,-44.4414021435925));
#36978=CARTESIAN_POINT('Ctrl Pts',(-6.20930249335219,2.69600159352597,-44.4330197786532));
#36979=CARTESIAN_POINT('Ctrl Pts',(-6.27805960196019,2.53179025805266,-44.4246374137138));
#36980=CARTESIAN_POINT('Ctrl Pts',(-6.34028864572777,2.36495853850665,-44.4162550487745));
#36981=CARTESIAN_POINT('Ctrl Pts',(-6.40244851017053,2.1983122838982,-44.4078820024156));
#36982=CARTESIAN_POINT('Ctrl Pts',(-6.45809465261197,2.02905176457662,-44.3995089560566));
#36983=CARTESIAN_POINT('Ctrl Pts',(-6.50701004128297,1.85771615771696,-44.3911359096977));
#36984=CARTESIAN_POINT('Ctrl Pts',(-6.55586542985441,1.6865907128073,-44.3827731338002));
#36985=CARTESIAN_POINT('Ctrl Pts',(-6.59800643617382,1.51339557994791,-44.3744103579028));
#36986=CARTESIAN_POINT('Ctrl Pts',(-6.63326503441398,1.33868741057084,-44.3660475820053));
#36987=CARTESIAN_POINT('Ctrl Pts',(-6.66849827503971,1.16410488947872,-44.3576908205287));
#36988=CARTESIAN_POINT('Ctrl Pts',(-6.69685890240044,0.988011830130503,
-44.349334059052));
#36989=CARTESIAN_POINT('Ctrl Pts',(-6.71822916313347,0.810978366926595,
-44.3409772975753));
#36990=CARTESIAN_POINT('Ctrl Pts',(-6.7395845623884,0.634068017753489,-44.3326263476248));
#36991=CARTESIAN_POINT('Ctrl Pts',(-6.75395924728334,0.456218903690333,
-44.3242753976742));
#36992=CARTESIAN_POINT('Ctrl Pts',(-6.76128682932984,0.278009732798816,
-44.3159244477236));
#36993=CARTESIAN_POINT('Ctrl Pts',(-6.76511962010167,0.184795018679802,
-44.3115563705457));
#36994=CARTESIAN_POINT('Ctrl Pts',(-6.76702520935342,0.0914819259722868,
-44.3071882933678));
#36995=CARTESIAN_POINT('Ctrl Pts',(-6.76699974817508,-0.00184613066680469,
-44.3028202161899));
#36996=CARTESIAN_POINT('',(-6.767,6.6187019857333E-10,-44.6971797838412));
#36997=CARTESIAN_POINT('Ctrl Pts',(3.09908550384718,6.01564277861014,-45.3486032095739));
#36998=CARTESIAN_POINT('Ctrl Pts',(2.93373232018329,6.1008279655248,-45.3398537616746));
#36999=CARTESIAN_POINT('Ctrl Pts',(2.76486502144428,6.1791915818019,-45.3311043137754));
#37000=CARTESIAN_POINT('Ctrl Pts',(2.59305716434355,6.25046746591378,-45.3223548658761));
#37001=CARTESIAN_POINT('Ctrl Pts',(2.42125069459284,6.32174277447224,-45.3136054886287));
#37002=CARTESIAN_POINT('Ctrl Pts',(2.24650397871058,6.38593035557826,-45.3048561113812));
#37003=CARTESIAN_POINT('Ctrl Pts',(2.06941053323769,6.44281220003539,-45.2961067341338));
#37004=CARTESIAN_POINT('Ctrl Pts',(1.89231845896685,6.49969360406685,-45.2873574246312));
#37005=CARTESIAN_POINT('Ctrl Pts',(1.71287996431511,6.54926929700879,-45.2786081151286));
#37006=CARTESIAN_POINT('Ctrl Pts',(1.53170449173514,6.59137090065477,-45.269858805626));
#37007=CARTESIAN_POINT('Ctrl Pts',(1.35053036178178,6.63347219230082,-45.2611095609615));
#37008=CARTESIAN_POINT('Ctrl Pts',(1.1676195587885,6.66809944062453,-45.2523603162969));
#37009=CARTESIAN_POINT('Ctrl Pts',(0.983593309310526,6.69513503985391,-45.2436110716323));
#37010=CARTESIAN_POINT('Ctrl Pts',(0.799568362459917,6.72217044771215,-45.2348618888991));
#37011=CARTESIAN_POINT('Ctrl Pts',(0.614428268438427,6.74161427235979,-45.2261127061659));
#37012=CARTESIAN_POINT('Ctrl Pts',(0.428801816329997,6.75340047696804,-45.2173635234327));
#37013=CARTESIAN_POINT('Ctrl Pts',(0.243176616522541,6.76518660206243,-45.2086143997246));
#37014=CARTESIAN_POINT('Ctrl Pts',(0.0570653511652483,6.76931519233997,
-45.1998652760165));
#37015=CARTESIAN_POINT('Ctrl Pts',(-0.128899900800212,6.76577222610795,
-45.1911161523083));
#37016=CARTESIAN_POINT('Ctrl Pts',(-0.314863959942268,6.76222928260132,
-45.1823670847191));
#37017=CARTESIAN_POINT('Ctrl Pts',(-0.500681721080991,6.75101488651274,
-45.1736180171298));
#37018=CARTESIAN_POINT('Ctrl Pts',(-0.685722110173672,6.73216712415987,
-45.1648689495405));
#37019=CARTESIAN_POINT('Ctrl Pts',(-0.870761373827983,6.7133194764414,-45.1561199351642));
#37020=CARTESIAN_POINT('Ctrl Pts',(-1.0550229898438,6.6868385843999,-45.1473709207878));
#37021=CARTESIAN_POINT('Ctrl Pts',(-1.23788117676096,6.65281438131419,-45.1386219064115));
#37022=CARTESIAN_POINT('Ctrl Pts',(-1.43009641450478,6.61704912302621,-45.1294251955246));
#37023=CARTESIAN_POINT('Ctrl Pts',(-1.62076048990051,6.57294837083776,-45.1202284846377));
#37024=CARTESIAN_POINT('Ctrl Pts',(-1.80915798957194,6.52067760043142,-45.1110317737508));
#37025=CARTESIAN_POINT('Ctrl Pts',(-1.98840442999105,6.4709457857861,-45.1022817760443));
#37026=CARTESIAN_POINT('Ctrl Pts',(-2.16559895948318,6.41381888475783,-45.0935317783378));
#37027=CARTESIAN_POINT('Ctrl Pts',(-2.34013966238487,6.34949095286648,-45.0847817806313));
#37028=CARTESIAN_POINT('Ctrl Pts',(-2.51467682550215,6.28516432558205,-45.0760319603797));
#37029=CARTESIAN_POINT('Ctrl Pts',(-2.68656000075082,6.21363705881287,-45.0672821401281));
#37030=CARTESIAN_POINT('Ctrl Pts',(-2.85520533837172,6.13515211512589,-45.0585323198765));
#37031=CARTESIAN_POINT('Ctrl Pts',(-3.02384747994653,6.05666865882956,-45.0497826654453));
#37032=CARTESIAN_POINT('Ctrl Pts',(-3.18925164680909,5.97122791041781,-45.041033011014));
#37033=CARTESIAN_POINT('Ctrl Pts',(-3.35085601825581,5.87912008253947,-45.0322833565828));
#37034=CARTESIAN_POINT('Ctrl Pts',(-3.51245754187895,5.78701387780312,-45.0235338563396));
#37035=CARTESIAN_POINT('Ctrl Pts',(-3.67025915507472,5.68824097063218,-45.0147843560965));
#37036=CARTESIAN_POINT('Ctrl Pts',(-3.82372487925432,5.58313684659185,-45.0060348558534));
#37037=CARTESIAN_POINT('Ctrl Pts',(-3.97718810297457,5.47803443504199,-44.9972854981682));
#37038=CARTESIAN_POINT('Ctrl Pts',(-4.12631534259748,5.36660117498896,-44.9885361404831));
#37039=CARTESIAN_POINT('Ctrl Pts',(-4.27060009883016,5.24921554099961,-44.979786782798));
#37040=CARTESIAN_POINT('Ctrl Pts',(-4.41488269591073,5.13183166362993,-44.9710375560428));
#37041=CARTESIAN_POINT('Ctrl Pts',(-4.5543227323202,5.00849577142261,-44.9622883292877));
#37042=CARTESIAN_POINT('Ctrl Pts',(-4.68844662477214,4.87962675280218,-44.9535391025325));
#37043=CARTESIAN_POINT('Ctrl Pts',(-4.82256868832243,4.7507594914284,-44.944789995081));
#37044=CARTESIAN_POINT('Ctrl Pts',(-4.95137454635029,4.61635945315564,-44.9360408876295));
#37045=CARTESIAN_POINT('Ctrl Pts',(-5.07442674458329,4.47688309137706,-44.927291780178));
#37046=CARTESIAN_POINT('Ctrl Pts',(-5.19747742835866,4.33740844619554,-44.9185427804056));
#37047=CARTESIAN_POINT('Ctrl Pts',(-5.31477440448334,4.19285781739315,-44.9097937806333));
#37048=CARTESIAN_POINT('Ctrl Pts',(-5.42591931528644,4.04372212002773,-44.9010447808609));
#37049=CARTESIAN_POINT('Ctrl Pts',(-5.53707636460566,3.89457013504235,-44.8922948255803));
#37050=CARTESIAN_POINT('Ctrl Pts',(-5.64207983271152,3.74083230919918,-44.8835448702997));
#37051=CARTESIAN_POINT('Ctrl Pts',(-5.74057303466527,3.58303087255384,-44.8747949150192));
#37052=CARTESIAN_POINT('Ctrl Pts',(-5.83906243361643,3.42523552891048,-44.8660452975904));
#37053=CARTESIAN_POINT('Ctrl Pts',(-5.93104191766405,3.26337713160666,-44.8572956801615));
#37054=CARTESIAN_POINT('Ctrl Pts',(-6.01619906697738,3.09800545294881,-44.8485460627327));
#37055=CARTESIAN_POINT('Ctrl Pts',(-6.10135338093573,2.93263928043362,-44.8397967366273));
#37056=CARTESIAN_POINT('Ctrl Pts',(-6.17968568351138,2.76376031544027,-44.831047410522));
#37057=CARTESIAN_POINT('Ctrl Pts',(-6.25092992693296,2.59194213835376,-44.8222980844166));
#37058=CARTESIAN_POINT('Ctrl Pts',(-6.32217217689611,2.42012876884716,-44.8135490031228));
#37059=CARTESIAN_POINT('Ctrl Pts',(-6.38632665482459,2.24537661651625,-44.804799921829));
#37060=CARTESIAN_POINT('Ctrl Pts',(-6.44317547868063,2.06827917625466,-44.7960508405352));
#37061=CARTESIAN_POINT('Ctrl Pts',(-6.50002944234756,1.8911657242748,-44.7873009682202));
#37062=CARTESIAN_POINT('Ctrl Pts',(-6.54957634249327,1.71170683293297,-44.7785510959053));
#37063=CARTESIAN_POINT('Ctrl Pts',(-6.59164787707435,1.53051209229501,-44.7698012235903));
#37064=CARTESIAN_POINT('Ctrl Pts',(-6.63371649074161,1.34932993152199,-44.7610519587555));
#37065=CARTESIAN_POINT('Ctrl Pts',(-6.6683107125639,1.16641244178201,-44.7523026939207));
#37066=CARTESIAN_POINT('Ctrl Pts',(-6.69531304839714,0.982380875202212,
-44.7435534290859));
#37067=CARTESIAN_POINT('Ctrl Pts',(-6.72231677032539,0.798339861838338,
-44.7348037151303));
#37068=CARTESIAN_POINT('Ctrl Pts',(-6.74172778477501,0.613184940772896,
-44.7260540011747));
#37069=CARTESIAN_POINT('Ctrl Pts',(-6.75348015835246,0.427545027733496,
-44.717304287219));
#37070=CARTESIAN_POINT('Ctrl Pts',(-6.76249038363737,0.28521995379571,-44.7105961194264));
#37071=CARTESIAN_POINT('Ctrl Pts',(-6.76699999998605,0.142609996212931,
-44.7038879516338));
#37072=CARTESIAN_POINT('Ctrl Pts',(-6.767,6.61843980926672E-10,-44.6971797838412));
#37073=CARTESIAN_POINT('Ctrl Pts',(-6.767,6.63875942265778E-13,-44.6971797838101));
#37074=CARTESIAN_POINT('Ctrl Pts',(-6.76700000000002,-0.18600724955928,
-44.6884302719974));
#37075=CARTESIAN_POINT('Ctrl Pts',(-6.75932637294251,-0.372014355815401,
-44.6796807601846));
#37076=CARTESIAN_POINT('Ctrl Pts',(-6.74400518263369,-0.557389537585713,
-44.6709312483719));
#37077=CARTESIAN_POINT('Ctrl Pts',(-6.72868405703734,-0.742763936382393,
-44.6621817735147));
#37078=CARTESIAN_POINT('Ctrl Pts',(-6.70571545643566,-0.927506130404909,
-44.6534322986575));
#37079=CARTESIAN_POINT('Ctrl Pts',(-6.67517739401572,-1.11098864009563,
-44.6446828238003));
#37080=CARTESIAN_POINT('Ctrl Pts',(-6.64463945804385,-1.29447039004561,
-44.6359333851717));
#37081=CARTESIAN_POINT('Ctrl Pts',(-6.60653217002719,-1.47669218339299,
-44.6271839465432));
#37082=CARTESIAN_POINT('Ctrl Pts',(-6.56098496085474,-1.65703510627806,
-44.6184345079147));
#37083=CARTESIAN_POINT('Ctrl Pts',(-6.51543793649547,-1.83737729740041,
-44.6096851047881));
#37084=CARTESIAN_POINT('Ctrl Pts',(-6.46245112156884,-2.01584035544993,
-44.6009357016614));
#37085=CARTESIAN_POINT('Ctrl Pts',(-6.402204483617,-2.19181813797458,-44.5921862985348));
#37086=CARTESIAN_POINT('Ctrl Pts',(-6.34195808511952,-2.3677952210636,-44.5834369301833));
#37087=CARTESIAN_POINT('Ctrl Pts',(-6.27445201416329,-2.54128677725807,
-44.5746875618317));
#37088=CARTESIAN_POINT('Ctrl Pts',(-6.19991555052694,-2.71170355428728,
-44.5659381934802));
#37089=CARTESIAN_POINT('Ctrl Pts',(-6.12537937695079,-2.88211966813606,
-44.557188859177));
#37090=CARTESIAN_POINT('Ctrl Pts',(-6.04381298028296,-3.04946076419978,
-44.5484395248738));
#37091=CARTESIAN_POINT('Ctrl Pts',(-5.95549339308811,-3.21315848424629,
-44.5396901905706));
#37092=CARTESIAN_POINT('Ctrl Pts',(-5.86717414225626,-3.37685558085401,
-44.5309408895891));
#37093=CARTESIAN_POINT('Ctrl Pts',(-5.77210188843871,-3.5369090770032,-44.5221915886075));
#37094=CARTESIAN_POINT('Ctrl Pts',(-5.67059953311163,-3.69277537024311,
-44.513442287626));
#37095=CARTESIAN_POINT('Ctrl Pts',(-5.56909755592481,-3.84864108281355,
-44.5046930192393));
#37096=CARTESIAN_POINT('Ctrl Pts',(-5.46116568154721,-4.00031938355164,
-44.4959437508527));
#37097=CARTESIAN_POINT('Ctrl Pts',(-5.34717048488112,-4.14729511918505,
-44.4871944824661));
#37098=CARTESIAN_POINT('Ctrl Pts',(-5.2331757034303,-4.29427031947514,-44.4784452459477));
#37099=CARTESIAN_POINT('Ctrl Pts',(-5.11311781951263,-4.43654276249883,
-44.4696960094294));
#37100=CARTESIAN_POINT('Ctrl Pts',(-4.98740458928951,-4.57362924412703,
-44.460946772911));
#37101=CARTESIAN_POINT('Ctrl Pts',(-4.86169180652435,-4.71071523781583,
-44.4521975675343));
#37102=CARTESIAN_POINT('Ctrl Pts',(-4.73032391141256,-4.84261509584798,
-44.4434483621576));
#37103=CARTESIAN_POINT('Ctrl Pts',(-4.59374706947,-4.96888084599901,-44.4346991567809));
#37104=CARTESIAN_POINT('Ctrl Pts',(-4.45717070231214,-5.09514615720998,
-44.4259499818192));
#37105=CARTESIAN_POINT('Ctrl Pts',(-4.31538563497104,-5.21577720520795,
-44.4172008068575));
#37106=CARTESIAN_POINT('Ctrl Pts',(-4.16887340951821,-5.33036429293646,
-44.4084516318958));
#37107=CARTESIAN_POINT('Ctrl Pts',(-4.0223616812229,-5.4449509918385,-44.3997024866226));
#37108=CARTESIAN_POINT('Ctrl Pts',(-3.87112305262978,-5.5534935949807,-44.3909533413493));
#37109=CARTESIAN_POINT('Ctrl Pts',(-3.71567116928783,-5.65562346357351,
-44.3822041960761));
#37110=CARTESIAN_POINT('Ctrl Pts',(-3.56021980053102,-5.75775299409056,
-44.3734550797647));
#37111=CARTESIAN_POINT('Ctrl Pts',(-3.40055544441879,-5.85346967519998,
-44.3647059634533));
#37112=CARTESIAN_POINT('Ctrl Pts',(-3.23722035886642,-5.94244843041492,
-44.355956847142));
#37113=CARTESIAN_POINT('Ctrl Pts',(-3.07388580043271,-6.03142689847563,
-44.347207759066));
#37114=CARTESIAN_POINT('Ctrl Pts',(-2.90688078788986,-6.11366734708015,
-44.3384586709899));
#37115=CARTESIAN_POINT('Ctrl Pts',(-2.73677250610137,-6.18889047001541,
-44.3297095829139));
#37116=CARTESIAN_POINT('Ctrl Pts',(-2.56666475916652,-6.26411335643451,
-44.3209605223467));
#37117=CARTESIAN_POINT('Ctrl Pts',(-2.39345402456782,-6.33231884545374,
-44.3122114617796));
#37118=CARTESIAN_POINT('Ctrl Pts',(-2.21772855943726,-6.39327529805,-44.3034624012124));
#37119=CARTESIAN_POINT('Ctrl Pts',(-2.04200363223274,-6.45423156404802,
-44.2947133674276));
#37120=CARTESIAN_POINT('Ctrl Pts',(-1.8637642606074,-6.50793874412536,-44.2859643336428));
#37121=CARTESIAN_POINT('Ctrl Pts',(-1.68361577621418,-6.55421443943382,
-44.277215299858));
#37122=CARTESIAN_POINT('Ctrl Pts',(-1.50346782832924,-6.60048999692654,
-44.2684662921291));
#37123=CARTESIAN_POINT('Ctrl Pts',(-1.32141105657075,-6.63933404265224,
-44.2597172844002));
#37124=CARTESIAN_POINT('Ctrl Pts',(-1.13806375346203,-6.67061465631586,
-44.2509682766713));
#37125=CARTESIAN_POINT('Ctrl Pts',(-0.954716981166183,-6.70189517941827,
-44.2422192942718));
#37126=CARTESIAN_POINT('Ctrl Pts',(-0.770079967437952,-6.72561226609055,
-44.2334703118724));
#37127=CARTESIAN_POINT('Ctrl Pts',(-0.584779764068238,-6.74168536996027,
-44.2247213294729));
#37128=CARTESIAN_POINT('Ctrl Pts',(-0.391489587588108,-6.75845153117901,
-44.2155950990573));
#37129=CARTESIAN_POINT('Ctrl Pts',(-0.197478091800382,-6.76689985146408,
-44.2064688686417));
#37130=CARTESIAN_POINT('Ctrl Pts',(-0.00346214752617278,-6.76699911434415,
-44.1973426382261));
#37131=CARTESIAN_POINT('Ctrl Pts',(0.18449079848947,-6.76709527525922,-44.1885016025109));
#37132=CARTESIAN_POINT('Ctrl Pts',(0.372447602159575,-6.75935633790737,
-44.1796605667958));
#37133=CARTESIAN_POINT('Ctrl Pts',(0.559756448198972,-6.74380914014474,
-44.1708195310807));
#37134=CARTESIAN_POINT('Ctrl Pts',(0.74513613104807,-6.72842206873102,-44.1620695524674));
#37135=CARTESIAN_POINT('Ctrl Pts',(0.92988085194971,-6.70538686355659,-44.1533195738541));
#37136=CARTESIAN_POINT('Ctrl Pts',(1.11336305057924,-6.67478177303235,-44.1445695952408));
#37137=CARTESIAN_POINT('Ctrl Pts',(1.29684337090586,-6.6441769958117,-44.1358197062008));
#37138=CARTESIAN_POINT('Ctrl Pts',(1.47906091205653,-6.60600253547956,-44.1270698171608));
#37139=CARTESIAN_POINT('Ctrl Pts',(1.65939671095684,-6.56038806441095,-44.1183199281208));
#37140=CARTESIAN_POINT('Ctrl Pts',(1.83973072369626,-6.51477404513718,-44.1095701257453));
#37141=CARTESIAN_POINT('Ctrl Pts',(2.01818275357505,-6.46172023288515,-44.1008203233698));
#37142=CARTESIAN_POINT('Ctrl Pts',(2.19414664033797,-6.40140683917947,-44.0920705209943));
#37143=CARTESIAN_POINT('Ctrl Pts',(2.37010884271728,-6.34109402281323,-44.0833208023748));
#37144=CARTESIAN_POINT('Ctrl Pts',(2.54358267848271,-6.27352185699603,-44.0745710837553));
#37145=CARTESIAN_POINT('Ctrl Pts',(2.71397890842203,-6.19891986435059,-44.0658213651357));
#37146=CARTESIAN_POINT('Ctrl Pts',(2.88437356389396,-6.1243185610303,-44.0570717273639));
#37147=CARTESIAN_POINT('Ctrl Pts',(3.05169040787617,-6.04268767582332,-44.0483220895921));
#37148=CARTESIAN_POINT('Ctrl Pts',(3.2153611251249,-5.9543044795371,-44.0395724518203));
#37149=CARTESIAN_POINT('Ctrl Pts',(3.37903038443271,-5.86592207054796,-44.0308228919882));
#37150=CARTESIAN_POINT('Ctrl Pts',(3.53905332980392,-5.7707876070312,-44.0220733321561));
#37151=CARTESIAN_POINT('Ctrl Pts',(3.69488643042301,-5.66922422085032,-44.0133237723241));
#37152=CARTESIAN_POINT('Ctrl Pts',(3.8507181946915,-5.56766170562876,-44.0045742875241));
#37153=CARTESIAN_POINT('Ctrl Pts',(4.0023599459963,-5.45967053455954,-43.9958248027241));
#37154=CARTESIAN_POINT('Ctrl Pts',(4.14929662974704,-5.34561750206371,-43.9870753179241));
#37155=CARTESIAN_POINT('Ctrl Pts',(4.29623210225434,-5.23156540974145,-43.9783259052487));
#37156=CARTESIAN_POINT('Ctrl Pts',(4.43846235842494,-5.11145173171859,-43.9695764925734));
#37157=CARTESIAN_POINT('Ctrl Pts',(4.57550431797791,-4.98568443006228,-43.960827079898));
#37158=CARTESIAN_POINT('Ctrl Pts',(4.71254519337846,-4.85991812336348,-43.9520777364401));
#37159=CARTESIAN_POINT('Ctrl Pts',(4.84439764315324,-4.72849847630752,-43.9433283929822));
#37160=CARTESIAN_POINT('Ctrl Pts',(4.97061384197015,-4.59187184424988,-43.9345790495243));
#37161=CARTESIAN_POINT('Ctrl Pts',(5.09682908420519,-4.45524624767389,-43.925829772377));
#37162=CARTESIAN_POINT('Ctrl Pts',(5.21740796650468,-4.31341395556533,-43.9170804952296));
#37163=CARTESIAN_POINT('Ctrl Pts',(5.33194095942533,-4.16685668162496,-43.9083312180823));
#37164=CARTESIAN_POINT('Ctrl Pts',(5.44647312235404,-4.02030046974848,-43.8995820043387));
#37165=CARTESIAN_POINT('Ctrl Pts',(5.55495930712548,-3.86901957035174,-43.8908327905952));
#37166=CARTESIAN_POINT('Ctrl Pts',(5.65703106080043,-3.71352778057996,-43.8820835768516));
#37167=CARTESIAN_POINT('Ctrl Pts',(5.75910210868975,-3.55803706597215,-43.8733344236054));
#37168=CARTESIAN_POINT('Ctrl Pts',(5.85475865698779,-3.39833575880504,-43.8645852703592));
#37169=CARTESIAN_POINT('Ctrl Pts',(5.94367583069283,-3.23496624706317,-43.855836117113));
#37170=CARTESIAN_POINT('Ctrl Pts',(6.03259241910281,-3.07159781069699,-43.8470870214579));
#37171=CARTESIAN_POINT('Ctrl Pts',(6.11476958471156,-2.90456146975437,-43.8383379258028));
#37172=CARTESIAN_POINT('Ctrl Pts',(6.18992823574559,-2.73442451647865,-43.8295888301477));
#37173=CARTESIAN_POINT('Ctrl Pts',(6.26508641701097,-2.5642886266202,-43.8208397891776));
#37174=CARTESIAN_POINT('Ctrl Pts',(6.33322605570447,-2.39105242530879,-43.8120907482075));
#37175=CARTESIAN_POINT('Ctrl Pts',(6.39411573747906,-2.21530425353328,-43.8033417072373));
#37176=CARTESIAN_POINT('Ctrl Pts',(6.45500505889255,-2.03955712188152,-43.7945927180463));
#37177=CARTESIAN_POINT('Ctrl Pts',(6.50864441545048,-1.86129832025156,-43.7858437288553));
#37178=CARTESIAN_POINT('Ctrl Pts',(6.55485164050015,-1.68113324011885,-43.7770947396643));
#37179=CARTESIAN_POINT('Ctrl Pts',(6.60199852639206,-1.49730435912473,-43.7681678327875));
#37180=CARTESIAN_POINT('Ctrl Pts',(6.64140767441094,-1.31149113173226,-43.7592409259106));
#37181=CARTESIAN_POINT('Ctrl Pts',(6.67293975269674,-1.12435050446006,-43.7503140190337));
#37182=CARTESIAN_POINT('Ctrl Pts',(6.70384664831567,-0.940920291559479,
-43.7415641048497));
#37183=CARTESIAN_POINT('Ctrl Pts',(6.72718585889714,-0.756215114273666,
-43.7328141906657));
#37184=CARTESIAN_POINT('Ctrl Pts',(6.742878104519,-0.570862389370861,-43.7240642764817));
#37185=CARTESIAN_POINT('Ctrl Pts',(6.75857004154147,-0.38551330956387,-43.7153145343711));
#37186=CARTESIAN_POINT('Ctrl Pts',(6.76661529035568,-0.199516993255035,
-43.7065647922606));
#37187=CARTESIAN_POINT('Ctrl Pts',(6.76698652348897,-0.0135052182009377,
-43.69781505015));
#37188=CARTESIAN_POINT('Ctrl Pts',(6.76735774981513,0.172503146041962,-43.6890654684793));
#37189=CARTESIAN_POINT('Ctrl Pts',(6.76005524147463,0.358526681836487,-43.6803158868087));
#37190=CARTESIAN_POINT('Ctrl Pts',(6.74510380214858,0.543933542117825,-43.671566305138));
#37191=CARTESIAN_POINT('Ctrl Pts',(6.73015261710947,0.729337249087633,-43.6628168722761));
#37192=CARTESIAN_POINT('Ctrl Pts',(6.70755278444566,0.914124015857523,-43.6540674394142));
#37193=CARTESIAN_POINT('Ctrl Pts',(6.67738106408243,1.09766621749666,-43.6453180065523));
#37194=CARTESIAN_POINT('Ctrl Pts',(6.64720981677201,1.28120554143597,-43.6365687108699));
#37195=CARTESIAN_POINT('Ctrl Pts',(6.60946696581463,1.4635000565089,-43.6278194151876));
#37196=CARTESIAN_POINT('Ctrl Pts',(6.56428070010928,1.64393062206798,-43.6190701195052));
#37197=CARTESIAN_POINT('Ctrl Pts',(6.51909508282668,1.82435859844912,-43.6103209493752));
#37198=CARTESIAN_POINT('Ctrl Pts',(6.46646633415582,2.00292240086818,-43.6015717792452));
#37199=CARTESIAN_POINT('Ctrl Pts',(6.40657319597107,2.17901557696704,-43.5928226091153));
#37200=CARTESIAN_POINT('Ctrl Pts',(6.34668083768203,2.35510646007682,-43.5840735529122));
#37201=CARTESIAN_POINT('Ctrl Pts',(6.27952437143786,2.52872650996777,-43.5753244967091));
#37202=CARTESIAN_POINT('Ctrl Pts',(6.2053318733503,2.69928607998169,-43.566575440506));
#37203=CARTESIAN_POINT('Ctrl Pts',(6.12831449784144,2.87633970115627,-43.5574932642172));
#37204=CARTESIAN_POINT('Ctrl Pts',(6.04371489463044,3.05009490562565,-43.5484110879284));
#37205=CARTESIAN_POINT('Ctrl Pts',(5.95184265120381,3.21991584599834,-43.5393289116395));
#37206=CARTESIAN_POINT('Ctrl Pts',(5.86333281335374,3.38352155905506,-43.5305791312851));
#37207=CARTESIAN_POINT('Ctrl Pts',(5.76807337235558,3.54347560904031,-43.5218293509307));
#37208=CARTESIAN_POINT('Ctrl Pts',(5.66638790086219,3.69923467178856,-43.5130795705763));
#37209=CARTESIAN_POINT('Ctrl Pts',(5.56470608502597,3.85498813489974,-43.504330104782));
#37210=CARTESIAN_POINT('Ctrl Pts',(5.45659885766797,4.00654667256472,-43.4955806389877));
#37211=CARTESIAN_POINT('Ctrl Pts',(5.34243340580343,4.15339551506422,-43.4868311731935));
#37212=CARTESIAN_POINT('Ctrl Pts',(5.22827145140429,4.30023985884069,-43.4780819754396));
#37213=CARTESIAN_POINT('Ctrl Pts',(5.10805181977926,4.4423745699323,-43.4693327776857));
#37214=CARTESIAN_POINT('Ctrl Pts',(4.9821828128239,4.57931691626624,-43.4605835799319));
#37215=CARTESIAN_POINT('Ctrl Pts',(4.85631699296061,4.71625579512334,-43.4518346037139));
#37216=CARTESIAN_POINT('Ctrl Pts',(4.72480227791663,4.8480023613594,-43.4430856274958));
#37217=CARTESIAN_POINT('Ctrl Pts',(4.58808530847932,4.97410918679076,-43.4343366512778));
#37218=CARTESIAN_POINT('Ctrl Pts',(4.45135945056777,5.10022421089178,-43.4255871062566));
#37219=CARTESIAN_POINT('Ctrl Pts',(4.30943087207835,5.22069856612156,-43.4168375612354));
#37220=CARTESIAN_POINT('Ctrl Pts',(4.1627816432225,5.33512305301853,-43.4080880162142));
#37221=CARTESIAN_POINT('Ctrl Pts',(4.01614103534175,5.44954081331585,-43.399338985547));
#37222=CARTESIAN_POINT('Ctrl Pts',(3.864780558332,5.55790924068485,-43.3905899548797));
#37223=CARTESIAN_POINT('Ctrl Pts',(3.70921425811742,5.65986029751428,-43.3818409242125));
#37224=CARTESIAN_POINT('Ctrl Pts',(3.55364584529909,5.76181273884784,-43.3730917747326));
#37225=CARTESIAN_POINT('Ctrl Pts',(3.39387173464132,5.85734747818186,-43.3643426252528));
#37226=CARTESIAN_POINT('Ctrl Pts',(3.23043456092192,5.94614005448924,-43.3555934757729));
#37227=CARTESIAN_POINT('Ctrl Pts',(3.18690768806249,5.96978744811357,-43.3532633870399));
#37228=CARTESIAN_POINT('Ctrl Pts',(3.14312114982811,5.99295688499337,-43.3509332983069));
#37229=CARTESIAN_POINT('Ctrl Pts',(3.09908550384722,6.01564277861012,-43.3486032095739));
#37230=CARTESIAN_POINT('Origin',(0.,0.,-63.6971797838103));
#37231=CARTESIAN_POINT('',(3.09908550384721,6.01564277861012,-40.9541976313953));
#37232=CARTESIAN_POINT('',(3.09908550384719,6.01564277861013,-41.3487246499327));
#37233=CARTESIAN_POINT('',(3.09908550384721,6.01564277861012,-63.6971797838103));
#37234=CARTESIAN_POINT('',(-6.76699866356674,-0.00425291500162284,-42.3028202162243));
#37235=CARTESIAN_POINT('Ctrl Pts',(-6.76699866356628,-0.00425291572926541,
-42.30282021619));
#37236=CARTESIAN_POINT('Ctrl Pts',(-6.76684388596092,-0.250526276245932,
-42.2912054307044));
#37237=CARTESIAN_POINT('Ctrl Pts',(-6.75324119786962,-0.496385215031647,
-42.2795906452187));
#37238=CARTESIAN_POINT('Ctrl Pts',(-6.72634853459335,-0.740624325264789,
-42.2679758597331));
#37239=CARTESIAN_POINT('Ctrl Pts',(-6.70775751590284,-0.909467917163841,
-42.2599465064544));
#37240=CARTESIAN_POINT('Ctrl Pts',(-6.68281621829628,-1.07753799544482,
-42.2519171531757));
#37241=CARTESIAN_POINT('Ctrl Pts',(-6.65159041399686,-1.24444122578171,
-42.243887799897));
#37242=CARTESIAN_POINT('Ctrl Pts',(-6.61960773658645,-1.41538997456125,
-42.2356638254795));
#37243=CARTESIAN_POINT('Ctrl Pts',(-6.58098823809289,-1.58533161726112,
-42.2274398510619));
#37244=CARTESIAN_POINT('Ctrl Pts',(-6.5358075490959,-1.75371282745525,-42.2192158766443));
#37245=CARTESIAN_POINT('Ctrl Pts',(-6.49067457529011,-1.92191621075436,
-42.2110005875417));
#37246=CARTESIAN_POINT('Ctrl Pts',(-6.43899430161741,-2.08856209972778,
-42.202785298439));
#37247=CARTESIAN_POINT('Ctrl Pts',(-6.38089366570641,-2.2531056404323,-42.1945700093364));
#37248=CARTESIAN_POINT('Ctrl Pts',(-6.32284273595483,-2.41750841112046,
-42.1863617485642));
#37249=CARTESIAN_POINT('Ctrl Pts',(-6.25838250203016,-2.57981207940195,
-42.178153487792));
#37250=CARTESIAN_POINT('Ctrl Pts',(-6.18769018867022,-2.73948519416227,
-42.1699452270198));
#37251=CARTESIAN_POINT('Ctrl Pts',(-6.11704417854715,-2.89905372354829,
-42.1617423426319));
#37252=CARTESIAN_POINT('Ctrl Pts',(-6.04017436454052,-3.05599480473207,
-42.153539458244));
#37253=CARTESIAN_POINT('Ctrl Pts',(-5.957306757357,-3.20979519576384,-42.1453365738561));
#37254=CARTESIAN_POINT('Ctrl Pts',(-5.87447681484184,-3.36352568202923,
-42.1371374178119));
#37255=CARTESIAN_POINT('Ctrl Pts',(-5.78565467998213,-3.51411800704669,
-42.1289382617677));
#37256=CARTESIAN_POINT('Ctrl Pts',(-5.69111318190415,-3.66108177329554,
-42.1207391057235));
#37257=CARTESIAN_POINT('Ctrl Pts',(-5.59657990663755,-3.80803275727044,
-42.1125406628065));
#37258=CARTESIAN_POINT('Ctrl Pts',(-5.49632844567494,-3.95135550512971,
-42.1043422198895));
#37259=CARTESIAN_POINT('Ctrl Pts',(-5.39067619462646,-4.09058665287605,
-42.0961437769724));
#37260=CARTESIAN_POINT('Ctrl Pts',(-5.28502499574932,-4.22981641404497,
-42.0879454157022));
#37261=CARTESIAN_POINT('Ctrl Pts',(-5.17397332990384,-4.36495436987936,
-42.079747054432));
#37262=CARTESIAN_POINT('Ctrl Pts',(-5.05788023371376,-4.49556854484588,
-42.0715486931618));
#37263=CARTESIAN_POINT('Ctrl Pts',(-4.9417672045311,-4.62620514605017,-42.0633489242465));
#37264=CARTESIAN_POINT('Ctrl Pts',(-4.82061125876662,-4.75231615081152,
-42.0551491553312));
#37265=CARTESIAN_POINT('Ctrl Pts',(-4.69480982647489,-4.87350486746806,
-42.0469493864159));
#37266=CARTESIAN_POINT('Ctrl Pts',(-4.56896394131635,-4.9947364070542,-42.0387467200516));
#37267=CARTESIAN_POINT('Ctrl Pts',(-4.43846955787128,-5.11104194506308,
-42.0305440536873));
#37268=CARTESIAN_POINT('Ctrl Pts',(-4.3037588795333,-5.22206362531502,-42.0223413873229));
#37269=CARTESIAN_POINT('Ctrl Pts',(-4.168895203536,-5.33321139844559,-42.0141294047799));
#37270=CARTESIAN_POINT('Ctrl Pts',(-4.02980594293001,-5.43906309635014,
-42.0059174222369));
#37271=CARTESIAN_POINT('Ctrl Pts',(-3.88695496132079,-5.53930231425075,
-41.9977054396939));
#37272=CARTESIAN_POINT('Ctrl Pts',(-3.7440197242719,-5.63960065459687,-41.9894886136126));
#37273=CARTESIAN_POINT('Ctrl Pts',(-3.59731864440727,-5.73427972211552,
-41.9812717875313));
#37274=CARTESIAN_POINT('Ctrl Pts',(-3.44734202376301,-5.82306808917752,
-41.97305496145));
#37275=CARTESIAN_POINT('Ctrl Pts',(-3.29713411750919,-5.91199338072488,
-41.9648254638361));
#37276=CARTESIAN_POINT('Ctrl Pts',(-3.14364089131701,-5.99500964756865,
-41.9565959662223));
#37277=CARTESIAN_POINT('Ctrl Pts',(-2.98737574045601,-6.07189222444988,
-41.9483664686084));
#37278=CARTESIAN_POINT('Ctrl Pts',(-2.84808764323296,-6.1404220776154,-41.9410310450836));
#37279=CARTESIAN_POINT('Ctrl Pts',(-2.70659765149766,-6.20407921759945,
-41.9336956215588));
#37280=CARTESIAN_POINT('Ctrl Pts',(-2.56327997653755,-6.26273780082495,
-41.9263601980339));
#37281=CARTESIAN_POINT('Ctrl Pts',(-2.4055933281651,-6.32727747040638,-41.9182893278475));
#37282=CARTESIAN_POINT('Ctrl Pts',(-2.24517960117377,-6.38597554821436,
-41.9102184576611));
#37283=CARTESIAN_POINT('Ctrl Pts',(-2.08251983694756,-6.43858681146103,
-41.9021475874747));
#37284=CARTESIAN_POINT('Ctrl Pts',(-1.92006249015466,-6.49113260407997,
-41.8940867608589));
#37285=CARTESIAN_POINT('Ctrl Pts',(-1.75536501795551,-6.53760654030773,
-41.8860259342431));
#37286=CARTESIAN_POINT('Ctrl Pts',(-1.58893098858132,-6.57781022176271,
-41.8779651076273));
#37287=CARTESIAN_POINT('Ctrl Pts',(-1.42266757697749,-6.61797268891485,
-41.8699125444675));
#37288=CARTESIAN_POINT('Ctrl Pts',(-1.25467151040898,-6.65187760616159,
-41.8618599813076));
#37289=CARTESIAN_POINT('Ctrl Pts',(-1.08546408256142,-6.67937547420933,
-41.8538074181477));
#37290=CARTESIAN_POINT('Ctrl Pts',(-0.916393065446839,-6.70685117417389,
-41.8457613467598));
#37291=CARTESIAN_POINT('Ctrl Pts',(-0.746112997077899,-6.72793004596986,
-41.8377152753719));
#37292=CARTESIAN_POINT('Ctrl Pts',(-0.575157904931525,-6.74251306149234,
-41.8296692039841));
#37293=CARTESIAN_POINT('Ctrl Pts',(-0.404303237960745,-6.75708751042651,
-41.8216278591482));
#37294=CARTESIAN_POINT('Ctrl Pts',(-0.232774707315543,-6.76517366786207,
-41.8135865143123));
#37295=CARTESIAN_POINT('Ctrl Pts',(-0.0611139456945034,-6.76672402907357,
-41.8055451694764));
#37296=CARTESIAN_POINT('Ctrl Pts',(0.113855907209627,-6.76830427647876,
-41.7973488122554));
#37297=CARTESIAN_POINT('Ctrl Pts',(0.288962749829934,-6.76309411511982,
-41.7891524550343));
#37298=CARTESIAN_POINT('Ctrl Pts',(0.463629849140091,-6.75109890040032,
-41.7809560978132));
#37299=CARTESIAN_POINT('Ctrl Pts',(0.634939111024455,-6.73933428423701,
-41.7729173091047));
#37300=CARTESIAN_POINT('Ctrl Pts',(0.8058249993055,-6.72104317134424,-41.7648785203963));
#37301=CARTESIAN_POINT('Ctrl Pts',(0.975746109784252,-6.69628318765275,
-41.7568397316878));
#37302=CARTESIAN_POINT('Ctrl Pts',(1.14568540336148,-6.67152055441866,-41.748800082756));
#37303=CARTESIAN_POINT('Ctrl Pts',(1.31465934396178,-6.64028772581122,-41.7407604338243));
#37304=CARTESIAN_POINT('Ctrl Pts',(1.48213463143767,-6.60269383920632,-41.7327207848926));
#37305=CARTESIAN_POINT('Ctrl Pts',(1.64966100103271,-6.56508848598194,-41.7246786837644));
#37306=CARTESIAN_POINT('Ctrl Pts',(1.81568744343466,-6.5211182945414,-41.7166365826362));
#37307=CARTESIAN_POINT('Ctrl Pts',(1.97969392299502,-6.47094281934685,-41.708594481508));
#37308=CARTESIAN_POINT('Ctrl Pts',(2.14923497687789,-6.41907411899818,-41.7002809910633));
#37309=CARTESIAN_POINT('Ctrl Pts',(2.31661693306373,-6.36057412682575,-41.6919675006185));
#37310=CARTESIAN_POINT('Ctrl Pts',(2.48128674990314,-6.29567351954937,-41.6836540101738));
#37311=CARTESIAN_POINT('Ctrl Pts',(2.64086162557093,-6.2327809595425,-41.675597742003));
#37312=CARTESIAN_POINT('Ctrl Pts',(2.79788938413509,-6.16387817576336,-41.6675414738323));
#37313=CARTESIAN_POINT('Ctrl Pts',(2.95189146735603,-6.08922209850739,-41.6594852056615));
#37314=CARTESIAN_POINT('Ctrl Pts',(3.11326906834912,-6.01099056815958,-41.6510431040798));
#37315=CARTESIAN_POINT('Ctrl Pts',(3.27132362515598,-5.92644134502226,-41.642601002498));
#37316=CARTESIAN_POINT('Ctrl Pts',(3.42553881963984,-5.83592090377693,-41.6341589009162));
#37317=CARTESIAN_POINT('Ctrl Pts',(3.57975401412373,-5.74540046253157,-41.6257167993345));
#37318=CARTESIAN_POINT('Ctrl Pts',(3.73012950509335,-5.64890912484754,-41.6172746977527));
#37319=CARTESIAN_POINT('Ctrl Pts',(3.87618945569488,-5.54684093007541,-41.608832596171));
#37320=CARTESIAN_POINT('Ctrl Pts',(4.02037637884735,-5.44608162613678,-41.6004987534783));
#37321=CARTESIAN_POINT('Ctrl Pts',(4.16081652066068,-5.33956780953376,-41.5921649107856));
#37322=CARTESIAN_POINT('Ctrl Pts',(4.29702791065859,-5.2276036704231,-41.5838310680929));
#37323=CARTESIAN_POINT('Ctrl Pts',(4.43307875830125,-5.115771495215,-41.5755070478882));
#37324=CARTESIAN_POINT('Ctrl Pts',(4.56491051651839,-4.99850201347904,-41.5671830276834));
#37325=CARTESIAN_POINT('Ctrl Pts',(4.69207016107308,-4.87614259467129,-41.5588590074787));
#37326=CARTESIAN_POINT('Ctrl Pts',(4.81910324643551,-4.75390495749688,-41.5505432719878));
#37327=CARTESIAN_POINT('Ctrl Pts',(4.94147323349797,-4.62658771590757,-41.5422275364969));
#37328=CARTESIAN_POINT('Ctrl Pts',(5.05876000478071,-4.49457853575072,-41.5339118010061));
#37329=CARTESIAN_POINT('Ctrl Pts',(5.17595153308928,-4.36267655393176,-41.525602818326));
#37330=CARTESIAN_POINT('Ctrl Pts',(5.2880678406877,-4.22609048444294,-41.517293835646));
#37331=CARTESIAN_POINT('Ctrl Pts',(5.39472538306907,-4.08524504054166,-41.508984852966));
#37332=CARTESIAN_POINT('Ctrl Pts',(5.50131584565111,-3.94448817813124,-41.5006810960288));
#37333=CARTESIAN_POINT('Ctrl Pts',(5.6024541755498,-3.7994775564615,-41.4923773390917));
#37334=CARTESIAN_POINT('Ctrl Pts',(5.69779673950095,-3.65067135131778,-41.4840735821545));
#37335=CARTESIAN_POINT('Ctrl Pts',(5.79310059666959,-3.50192555790603,-41.4757731963425));
#37336=CARTESIAN_POINT('Ctrl Pts',(5.8826131889639,-3.34938754381223,-41.4674728105304));
#37337=CARTESIAN_POINT('Ctrl Pts',(5.96603373897391,-3.19354511873952,-41.4591724247184));
#37338=CARTESIAN_POINT('Ctrl Pts',(6.04943669776054,-3.0377355567792,-41.4508737892418));
#37339=CARTESIAN_POINT('Ctrl Pts',(6.12675000956663,-2.8786232785124,-41.4425751537651));
#37340=CARTESIAN_POINT('Ctrl Pts',(6.19771835067938,-2.7167215988489,-41.4342765182885));
#37341=CARTESIAN_POINT('Ctrl Pts',(6.26868350634561,-2.55482718621649,-41.4259782552999));
#37342=CARTESIAN_POINT('Ctrl Pts',(6.33330411939158,-2.39014394026607,-41.4176799923113));
#37343=CARTESIAN_POINT('Ctrl Pts',(6.39137253243378,-2.22320627735057,-41.4093817293228));
#37344=CARTESIAN_POINT('Ctrl Pts',(6.44944797731292,-2.05624839899674,-41.40108246145));
#37345=CARTESIAN_POINT('Ctrl Pts',(6.50096952747292,-1.88703588835013,-41.3927831935772));
#37346=CARTESIAN_POINT('Ctrl Pts',(6.5457789675968,-1.71611966580639,-41.3844839257044));
#37347=CARTESIAN_POINT('Ctrl Pts',(6.59061987116992,-1.54508343252655,-41.3761788304079));
#37348=CARTESIAN_POINT('Ctrl Pts',(6.628739159033,-1.37234143379624,-41.3678737351113));
#37349=CARTESIAN_POINT('Ctrl Pts',(6.66002925677816,-1.19845704923411,-41.3595686398148));
#37350=CARTESIAN_POINT('Ctrl Pts',(6.69133076452004,-1.02450925738344,-41.3512605160487));
#37351=CARTESIAN_POINT('Ctrl Pts',(6.71579806437575,-0.849418592958558,
-41.3429523922826));
#37352=CARTESIAN_POINT('Ctrl Pts',(6.73337530018403,-0.673755198029385,
-41.3346442685165));
#37353=CARTESIAN_POINT('Ctrl Pts',(6.75097122049243,-0.497905073926316,
-41.3263273132628));
#37354=CARTESIAN_POINT('Ctrl Pts',(6.7616624160892,-0.32148134989519,-41.3180103580091));
#37355=CARTESIAN_POINT('Ctrl Pts',(6.76544510652199,-0.14505692206052,-41.3096934027555));
#37356=CARTESIAN_POINT('Ctrl Pts',(6.7682328918187,-0.0150348029798014,
-41.303563933273));
#37357=CARTESIAN_POINT('Ctrl Pts',(6.76726943506968,0.114987655273514,-41.2974344637905));
#37358=CARTESIAN_POINT('Ctrl Pts',(6.7625712964825,0.244782474844537,-41.2913049943079));
#37359=CARTESIAN_POINT('Ctrl Pts',(6.75609372451022,0.423737452395306,-41.2828539707828));
#37360=CARTESIAN_POINT('Ctrl Pts',(6.74250293622476,0.602586556072336,-41.2744029472576));
#37361=CARTESIAN_POINT('Ctrl Pts',(6.7218101425669,0.780741575224981,-41.2659519237324));
#37362=CARTESIAN_POINT('Ctrl Pts',(6.70113556829883,0.958739734178298,-41.2575083410822));
#37363=CARTESIAN_POINT('Ctrl Pts',(6.67337149034784,1.13604469894378,-41.2490647584321));
#37364=CARTESIAN_POINT('Ctrl Pts',(6.63858108888244,1.31207093037401,-41.240621175782));
#37365=CARTESIAN_POINT('Ctrl Pts',(6.60381658995475,1.48796610479118,-41.2321838796421));
#37366=CARTESIAN_POINT('Ctrl Pts',(6.56203625995759,1.66258411962017,-41.2237465835023));
#37367=CARTESIAN_POINT('Ctrl Pts',(6.51335482385915,1.83534681695604,-41.2153092873625));
#37368=CARTESIAN_POINT('Ctrl Pts',(6.46470811825353,2.0079862612801,-41.2068780105902));
#37369=CARTESIAN_POINT('Ctrl Pts',(6.40917021680669,2.17877271001987,-41.1984467338178));
#37370=CARTESIAN_POINT('Ctrl Pts',(6.34690647594121,2.3471402143152,-41.1900154570455));
#37371=CARTESIAN_POINT('Ctrl Pts',(6.2846694235689,2.51543555020356,-41.1815877942236));
#37372=CARTESIAN_POINT('Ctrl Pts',(6.21571239381016,2.6813136983124,-41.1731601314016));
#37373=CARTESIAN_POINT('Ctrl Pts',(6.14025015285026,2.84422521267608,-41.1647324685797));
#37374=CARTESIAN_POINT('Ctrl Pts',(6.06481114215278,3.00708657643226,-41.1563074001257));
#37375=CARTESIAN_POINT('Ctrl Pts',(5.98287105303255,3.16698282725885,-41.1478823316718));
#37376=CARTESIAN_POINT('Ctrl Pts',(5.89469236428801,3.32338546220638,-41.1394572632178));
#37377=CARTESIAN_POINT('Ctrl Pts',(5.87056397596649,3.36618201049091,-41.137151906604));
#37378=CARTESIAN_POINT('Ctrl Pts',(5.8459687507013,3.40871711144768,-41.1348465499902));
#37379=CARTESIAN_POINT('Ctrl Pts',(5.82091267019111,3.45098025001718,-41.1325411933764));
#37380=CARTESIAN_POINT('Ctrl Pts',(5.72723602637226,3.60898856168555,-41.1239222048519));
#37381=CARTESIAN_POINT('Ctrl Pts',(5.62715607284524,3.76312286389861,-41.1153032163274));
#37382=CARTESIAN_POINT('Ctrl Pts',(5.52102284174427,3.9128756408731,-41.1066842278029));
#37383=CARTESIAN_POINT('Ctrl Pts',(5.41482602736629,4.06271813312529,-41.0980600757351));
#37384=CARTESIAN_POINT('Ctrl Pts',(5.30256887398964,4.20817361343996,-41.0894359236674));
#37385=CARTESIAN_POINT('Ctrl Pts',(5.18464285012906,4.34876620624811,-41.0808117715996));
#37386=CARTESIAN_POINT('Ctrl Pts',(5.06267782822622,4.49417413318286,-41.0718922400034));
#37387=CARTESIAN_POINT('Ctrl Pts',(4.93464897618203,4.63437989549188,-41.0629727084071));
#37388=CARTESIAN_POINT('Ctrl Pts',(4.80103176615619,4.76889745961885,-41.0540531768109));
#37389=CARTESIAN_POINT('Ctrl Pts',(4.67159875816515,4.89920262726316,-41.0454129589516));
#37390=CARTESIAN_POINT('Ctrl Pts',(4.53692234731059,5.02417028200731,-41.0367727410924));
#37391=CARTESIAN_POINT('Ctrl Pts',(4.39746975459071,5.14339856101585,-41.0281325232331));
#37392=CARTESIAN_POINT('Ctrl Pts',(4.25125500168537,5.26840830816039,-41.0190733347684));
#37393=CARTESIAN_POINT('Ctrl Pts',(4.09978965524161,5.38710798898233,-41.0100141463037));
#37394=CARTESIAN_POINT('Ctrl Pts',(3.9436484975699,5.49908406260667,-41.000954957839));
#37395=CARTESIAN_POINT('Ctrl Pts',(3.78750733989819,5.61106013623101,-40.9918957693743));
#37396=CARTESIAN_POINT('Ctrl Pts',(3.6266907092926,5.71631242084015,-40.9828365809096));
#37397=CARTESIAN_POINT('Ctrl Pts',(3.46180560937375,5.81448113961241,-40.9737773924449));
#37398=CARTESIAN_POINT('Ctrl Pts',(3.34301605592288,5.88520565184269,-40.9672508054284));
#37399=CARTESIAN_POINT('Ctrl Pts',(3.22203664576403,5.95230189956878,-40.9607242184118));
#37400=CARTESIAN_POINT('Ctrl Pts',(3.09908550384721,6.01564277861012,-40.9541976313953));
#37401=CARTESIAN_POINT('Ctrl Pts',(3.09908550384721,6.01564277861012,-42.9543661083715));
#37402=CARTESIAN_POINT('Ctrl Pts',(2.94508352360841,6.09498015319939,-42.9462354082376));
#37403=CARTESIAN_POINT('Ctrl Pts',(2.78811202322111,6.16835922330416,-42.9381047081037));
#37404=CARTESIAN_POINT('Ctrl Pts',(2.62868177603743,6.23556902939328,-42.9299740079697));
#37405=CARTESIAN_POINT('Ctrl Pts',(2.46190881464766,6.30587424809499,-42.9214688405786));
#37406=CARTESIAN_POINT('Ctrl Pts',(2.292445687093,6.36942830878534,-42.9129636731875));
#37407=CARTESIAN_POINT('Ctrl Pts',(2.12089558626553,6.42604784546142,-42.9044585057964));
#37408=CARTESIAN_POINT('Ctrl Pts',(1.94934548543806,6.48266738213751,-42.8959533384053));
#37409=CARTESIAN_POINT('Ctrl Pts',(1.77570886195601,6.5323523206861,-42.8874481710142));
#37410=CARTESIAN_POINT('Ctrl Pts',(1.60060127132296,6.57498019542564,-42.878943003623));
#37411=CARTESIAN_POINT('Ctrl Pts',(1.42682065125253,6.61728503485459,-42.870502288645));
#37412=CARTESIAN_POINT('Ctrl Pts',(1.25123339486017,6.65272723459906,-42.8620615736669));
#37413=CARTESIAN_POINT('Ctrl Pts',(1.07440837386975,6.68116274657028,-42.8536208586888));
#37414=CARTESIAN_POINT('Ctrl Pts',(0.897717005560992,6.70957676564187,-42.8451865236008));
#37415=CARTESIAN_POINT('Ctrl Pts',(0.71979006564518,6.73099460142001,-42.8367521885128));
#37416=CARTESIAN_POINT('Ctrl Pts',(0.541207430672698,6.74532308469985,-42.8283178534247));
#37417=CARTESIAN_POINT('Ctrl Pts',(0.362732353467413,6.75964293813911,-42.8198885982161));
#37418=CARTESIAN_POINT('Ctrl Pts',(0.183602700046286,6.76688192500108,-42.8114593430075));
#37419=CARTESIAN_POINT('Ctrl Pts',(0.00440469568970479,6.76699856647361,
-42.8030300877989));
#37420=CARTESIAN_POINT('Ctrl Pts',(-0.174712867895633,6.76711515558657,
-42.7946046164259));
#37421=CARTESIAN_POINT('Ctrl Pts',(-0.353898388377913,6.76011577391952,
-42.7861791450528));
#37422=CARTESIAN_POINT('Ctrl Pts',(-0.532564002869326,6.74601101265391,
-42.7777536736798));
#37423=CARTESIAN_POINT('Ctrl Pts',(-0.711176798621986,6.73191042116491,
-42.7693306931206));
#37424=CARTESIAN_POINT('Ctrl Pts',(-0.889269662869151,6.71070866527772,
-42.7609077125613));
#37425=CARTESIAN_POINT('Ctrl Pts',(-1.06625782114147,6.68246835075593,-42.7524847320021));
#37426=CARTESIAN_POINT('Ctrl Pts',(-1.24324890997032,6.65422756863314,-42.7440616119758));
#37427=CARTESIAN_POINT('Ctrl Pts',(-1.41913492607003,6.61894804101692,-42.7356384919494));
#37428=CARTESIAN_POINT('Ctrl Pts',(-1.59333860961469,6.57674395693729,-42.7272153719231));
#37429=CARTESIAN_POINT('Ctrl Pts',(-1.76754831741319,6.53453841337006,-42.7187919606113));
#37430=CARTESIAN_POINT('Ctrl Pts',(-1.94007525248876,6.48540791424459,-42.7103685492994));
#37431=CARTESIAN_POINT('Ctrl Pts',(-2.11035454792276,6.42951729774963,-42.7019451379875));
#37432=CARTESIAN_POINT('Ctrl Pts',(-2.28066347985192,6.37361695369513,-42.6935202606114));
#37433=CARTESIAN_POINT('Ctrl Pts',(-2.44872367536119,6.31095425053192,-42.6850953832353));
#37434=CARTESIAN_POINT('Ctrl Pts',(-2.61398722013432,6.24174333123162,-42.6766705058592));
#37435=CARTESIAN_POINT('Ctrl Pts',(-2.77930258397864,6.17251071055999,-42.6682429868278));
#37436=CARTESIAN_POINT('Ctrl Pts',(-2.9418192412985,6.09672590895556,-42.6598154677963));
#37437=CARTESIAN_POINT('Ctrl Pts',(-3.10101064488902,6.01465061165526,-42.6513879487649));
#37438=CARTESIAN_POINT('Ctrl Pts',(-3.26034480517789,5.93250171240037,-42.6429528722601));
#37439=CARTESIAN_POINT('Ctrl Pts',(-3.41634745666161,5.84405119874393,-42.6345177957553));
#37440=CARTESIAN_POINT('Ctrl Pts',(-3.56851698959077,5.74960655132176,-42.6260827192505));
#37441=CARTESIAN_POINT('Ctrl Pts',(-3.72076006705666,5.65511625817992,-42.6176435660178));
#37442=CARTESIAN_POINT('Ctrl Pts',(-3.86916605237184,5.55462623614353,-42.609204412785));
#37443=CARTESIAN_POINT('Ctrl Pts',(-4.01326315108692,5.4484867513951,-42.6007652595522));
#37444=CARTESIAN_POINT('Ctrl Pts',(-4.15752038207929,5.34222931592069,-42.5923167280541));
#37445=CARTESIAN_POINT('Ctrl Pts',(-4.29745889499402,5.2303100774344,-42.583868196556));
#37446=CARTESIAN_POINT('Ctrl Pts',(-4.43263981342177,5.11311972131185,-42.5754196650579));
#37447=CARTESIAN_POINT('Ctrl Pts',(-4.50733165680832,5.0483682473041,-42.5707515772919));
#37448=CARTESIAN_POINT('Ctrl Pts',(-4.58057167599017,4.98200821746615,-42.566083489526));
#37449=CARTESIAN_POINT('Ctrl Pts',(-4.65229075505635,4.91411026844303,-42.56141540176));
#37450=CARTESIAN_POINT('Ctrl Pts',(-4.77889952211963,4.79424710617333,-42.5531746261633));
#37451=CARTESIAN_POINT('Ctrl Pts',(-4.90104784218804,4.66932234474011,-42.5449338505665));
#37452=CARTESIAN_POINT('Ctrl Pts',(-5.01830828543984,4.53969943413503,-42.5366930749697));
#37453=CARTESIAN_POINT('Ctrl Pts',(-5.13543885003825,4.41022009495617,-42.5284614269253));
#37454=CARTESIAN_POINT('Ctrl Pts',(-5.24769208120687,4.27605322966876,-42.520229778881));
#37455=CARTESIAN_POINT('Ctrl Pts',(-5.354675217738,4.13760103351477,-42.5119981308366));
#37456=CARTESIAN_POINT('Ctrl Pts',(-5.4615589242409,3.99927751470395,-42.5037741332783));
#37457=CARTESIAN_POINT('Ctrl Pts',(-5.56318207440744,3.85667687674248,-42.49555013572));
#37458=CARTESIAN_POINT('Ctrl Pts',(-5.65919019381688,3.71023656256671,-42.4873261381617));
#37459=CARTESIAN_POINT('Ctrl Pts',(-5.75511348967983,3.56392562897745,-42.4791094065372));
#37460=CARTESIAN_POINT('Ctrl Pts',(-5.8454314480592,3.41378207692828,-42.4708926749127));
#37461=CARTESIAN_POINT('Ctrl Pts',(-5.92983125685374,3.26027456899575,-42.4626759432882));
#37462=CARTESIAN_POINT('Ctrl Pts',(-6.01418782450147,3.10684570864289,-42.4544634213995));
#37463=CARTESIAN_POINT('Ctrl Pts',(-6.09263211029324,2.9500566359011,-42.4462508995108));
#37464=CARTESIAN_POINT('Ctrl Pts',(-6.16489562918667,2.79040335457709,-42.4380383776221));
#37465=CARTESIAN_POINT('Ctrl Pts',(-6.23713498281156,2.6308034620788,-42.4298286020403));
#37466=CARTESIAN_POINT('Ctrl Pts',(-6.30319754045534,2.46834159283338,-42.4216188264584));
#37467=CARTESIAN_POINT('Ctrl Pts',(-6.36286159541037,2.30353669770027,-42.4134090508766));
#37468=CARTESIAN_POINT('Ctrl Pts',(-6.38892130453191,2.23155420116675,-42.4098232341939));
#37469=CARTESIAN_POINT('Ctrl Pts',(-6.41376097430492,2.15912499519095,-42.4062374175112));
#37470=CARTESIAN_POINT('Ctrl Pts',(-6.43736502764551,2.08629348387196,-42.4026516008285));
#37471=CARTESIAN_POINT('Ctrl Pts',(-6.49212766462547,1.9173205724184,-42.3943323187781));
#37472=CARTESIAN_POINT('Ctrl Pts',(-6.5402041605344,1.74627955095192,-42.3860130367278));
#37473=CARTESIAN_POINT('Ctrl Pts',(-6.5814623005094,1.57373536116259,-42.3776937546774));
#37474=CARTESIAN_POINT('Ctrl Pts',(-6.62263302592097,1.40155674468879,-42.36939209888));
#37475=CARTESIAN_POINT('Ctrl Pts',(-6.65701423575539,1.22788167181083,-42.3610904430825));
#37476=CARTESIAN_POINT('Ctrl Pts',(-6.6845263044129,1.05327920591459,-42.352788787285));
#37477=CARTESIAN_POINT('Ctrl Pts',(-6.71212599438798,0.878120660491798,
-42.3444606921082));
#37478=CARTESIAN_POINT('Ctrl Pts',(-6.73281268932431,0.702029154174227,
-42.3361325969314));
#37479=CARTESIAN_POINT('Ctrl Pts',(-6.74655859261206,0.525581731467544,
-42.3278045017547));
#37480=CARTESIAN_POINT('Ctrl Pts',(-6.76030449589981,0.349134308760862,
-42.3194764065779));
#37481=CARTESIAN_POINT('Ctrl Pts',(-6.76710964300839,0.172331317951537,
-42.3111483114011));
#37482=CARTESIAN_POINT('Ctrl Pts',(-6.76699866356674,-0.00425291500166258,
-42.3028202162243));
#37483=CARTESIAN_POINT('',(-6.767,7.13615364716924E-13,-42.6971797838101));
#37484=CARTESIAN_POINT('Ctrl Pts',(3.09908550384722,6.01564277861012,-43.3486032095739));
#37485=CARTESIAN_POINT('Ctrl Pts',(2.93373232018328,6.10082796552481,-43.3398537616746));
#37486=CARTESIAN_POINT('Ctrl Pts',(2.76486502144423,6.17919158180192,-43.3311043137753));
#37487=CARTESIAN_POINT('Ctrl Pts',(2.59305716434346,6.25046746591381,-43.3223548658761));
#37488=CARTESIAN_POINT('Ctrl Pts',(2.42125069459283,6.32174277447224,-43.3136054886286));
#37489=CARTESIAN_POINT('Ctrl Pts',(2.24650397871065,6.38593035557823,-43.3048561113812));
#37490=CARTESIAN_POINT('Ctrl Pts',(2.06941053323784,6.44281220003535,-43.2961067341338));
#37491=CARTESIAN_POINT('Ctrl Pts',(1.89231845896703,6.49969360406679,-43.2873574246312));
#37492=CARTESIAN_POINT('Ctrl Pts',(1.71287996431533,6.54926929700873,-43.2786081151286));
#37493=CARTESIAN_POINT('Ctrl Pts',(1.53170449173539,6.59137090065471,-43.269858805626));
#37494=CARTESIAN_POINT('Ctrl Pts',(1.35053036178204,6.63347219230076,-43.2611095609614));
#37495=CARTESIAN_POINT('Ctrl Pts',(1.16761955878877,6.66809944062448,-43.2523603162969));
#37496=CARTESIAN_POINT('Ctrl Pts',(0.983593309310796,6.69513503985387,-43.2436110716323));
#37497=CARTESIAN_POINT('Ctrl Pts',(0.799568362460319,6.7221704477121,-43.2348618888991));
#37498=CARTESIAN_POINT('Ctrl Pts',(0.614428268438959,6.74161427235974,-43.2261127061659));
#37499=CARTESIAN_POINT('Ctrl Pts',(0.428801816330661,6.75340047696799,-43.2173635234327));
#37500=CARTESIAN_POINT('Ctrl Pts',(0.243176616523146,6.76518660206241,-43.2086143997246));
#37501=CARTESIAN_POINT('Ctrl Pts',(0.0570653511657931,6.76931519233997,
-43.1998652760165));
#37502=CARTESIAN_POINT('Ctrl Pts',(-0.128899900799728,6.76577222610796,
-43.1911161523083));
#37503=CARTESIAN_POINT('Ctrl Pts',(-0.314863959941652,6.76222928260135,
-43.1823670847191));
#37504=CARTESIAN_POINT('Ctrl Pts',(-0.500681721080245,6.7510148865128,-43.1736180171298));
#37505=CARTESIAN_POINT('Ctrl Pts',(-0.685722110172797,6.73216712415996,
-43.1648689495406));
#37506=CARTESIAN_POINT('Ctrl Pts',(-0.870761373827028,6.71331947644152,
-43.1561199351642));
#37507=CARTESIAN_POINT('Ctrl Pts',(-1.05502298984277,6.68683858440007,-43.1473709207878));
#37508=CARTESIAN_POINT('Ctrl Pts',(-1.23788117675985,6.6528143813144,-43.1386219064115));
#37509=CARTESIAN_POINT('Ctrl Pts',(-1.43009641451724,6.61704912302392,-43.129425195524));
#37510=CARTESIAN_POINT('Ctrl Pts',(-1.62076048992632,6.57294837083181,-43.1202284846364));
#37511=CARTESIAN_POINT('Ctrl Pts',(-1.80915798961074,6.52067760042065,-43.1110317737489));
#37512=CARTESIAN_POINT('Ctrl Pts',(-1.98840443002955,6.47094578577426,-43.1022817760424));
#37513=CARTESIAN_POINT('Ctrl Pts',(-2.16559895952137,6.41381888474494,-43.0935317783359));
#37514=CARTESIAN_POINT('Ctrl Pts',(-2.34013966242268,6.34949095285254,-43.0847817806294));
#37515=CARTESIAN_POINT('Ctrl Pts',(-2.51467682553963,6.28516432556706,-43.0760319603778));
#37516=CARTESIAN_POINT('Ctrl Pts',(-2.68656000078793,6.21363705879682,-43.0672821401262));
#37517=CARTESIAN_POINT('Ctrl Pts',(-2.85520533840842,6.13515211510881,-43.0585323198746));
#37518=CARTESIAN_POINT('Ctrl Pts',(-3.02384747998287,6.05666865881142,-43.0497826654433));
#37519=CARTESIAN_POINT('Ctrl Pts',(-3.18925164684503,5.97122791039862,-43.0410330110121));
#37520=CARTESIAN_POINT('Ctrl Pts',(-3.3508560182913,5.87912008251924,-43.0322833565808));
#37521=CARTESIAN_POINT('Ctrl Pts',(-3.51245754191383,5.78701387778195,-43.0235338563377));
#37522=CARTESIAN_POINT('Ctrl Pts',(-3.67025915510894,5.68824097061009,-43.0147843560946));
#37523=CARTESIAN_POINT('Ctrl Pts',(-3.82372487928786,5.58313684656888,-43.0060348558514));
#37524=CARTESIAN_POINT('Ctrl Pts',(-3.97718810300738,5.47803443501816,-42.9972854981663));
#37525=CARTESIAN_POINT('Ctrl Pts',(-4.12631534262954,5.3666011749643,-42.9885361404812));
#37526=CARTESIAN_POINT('Ctrl Pts',(-4.27060009886143,5.24921554097417,-42.9797867827961));
#37527=CARTESIAN_POINT('Ctrl Pts',(-4.41488269594131,5.13183166360361,-42.9710375560409));
#37528=CARTESIAN_POINT('Ctrl Pts',(-4.55432273235007,5.00849577139544,-42.9622883292857));
#37529=CARTESIAN_POINT('Ctrl Pts',(-4.68844662480126,4.8796267527742,-42.9535391025306));
#37530=CARTESIAN_POINT('Ctrl Pts',(-4.82256868835087,4.75075949139953,-42.9447899950791));
#37531=CARTESIAN_POINT('Ctrl Pts',(-4.95137454637802,4.6163594531259,-42.9360408876276));
#37532=CARTESIAN_POINT('Ctrl Pts',(-5.07442674461026,4.47688309134649,-42.9272917801761));
#37533=CARTESIAN_POINT('Ctrl Pts',(-5.19747742838495,4.33740844616404,-42.9185427804037));
#37534=CARTESIAN_POINT('Ctrl Pts',(-5.3147744045089,4.19285781736076,-42.9097937806313));
#37535=CARTESIAN_POINT('Ctrl Pts',(-5.42591931531122,4.04372211999447,-42.9010447808589));
#37536=CARTESIAN_POINT('Ctrl Pts',(-5.53707636462956,3.89457013500838,-42.8922948255784));
#37537=CARTESIAN_POINT('Ctrl Pts',(-5.64207983273449,3.74083230916452,-42.8835448702978));
#37538=CARTESIAN_POINT('Ctrl Pts',(-5.7405730346873,3.58303087251854,-42.8747949150172));
#37539=CARTESIAN_POINT('Ctrl Pts',(-5.83906243363753,3.42523552887452,-42.8660452975884));
#37540=CARTESIAN_POINT('Ctrl Pts',(-5.93104191768417,3.26337713157008,-42.8572956801596));
#37541=CARTESIAN_POINT('Ctrl Pts',(-6.01619906699651,3.09800545291165,-42.8485460627308));
#37542=CARTESIAN_POINT('Ctrl Pts',(-6.10135338095378,2.93263928039605,-42.8397967366254));
#37543=CARTESIAN_POINT('Ctrl Pts',(-6.17968568352834,2.76376031540234,-42.83104741052));
#37544=CARTESIAN_POINT('Ctrl Pts',(-6.25092992694882,2.59194213831552,-42.8222980844146));
#37545=CARTESIAN_POINT('Ctrl Pts',(-6.32217217691111,2.42012876880803,-42.8135490031208));
#37546=CARTESIAN_POINT('Ctrl Pts',(-6.38632665483867,2.24537661647626,-42.804799921827));
#37547=CARTESIAN_POINT('Ctrl Pts',(-6.44317547869373,2.06827917621383,-42.7960508405332));
#37548=CARTESIAN_POINT('Ctrl Pts',(-6.50002944235956,1.89116572423353,-42.7873009682182));
#37549=CARTESIAN_POINT('Ctrl Pts',(-6.54957634250415,1.71170683289132,-42.7785510959033));
#37550=CARTESIAN_POINT('Ctrl Pts',(-6.5916478770841,1.53051209225302,-42.7698012235883));
#37551=CARTESIAN_POINT('Ctrl Pts',(-6.63371649075019,1.34932993147978,-42.7610519587535));
#37552=CARTESIAN_POINT('Ctrl Pts',(-6.66831071257131,1.16641244173963,-42.7523026939187));
#37553=CARTESIAN_POINT('Ctrl Pts',(-6.69531304840337,0.982380875159712,
-42.7435534290839));
#37554=CARTESIAN_POINT('Ctrl Pts',(-6.72231677033047,0.798339861795558,
-42.7348037151283));
#37555=CARTESIAN_POINT('Ctrl Pts',(-6.74172778477892,0.613184940729886,
-42.7260540011726));
#37556=CARTESIAN_POINT('Ctrl Pts',(-6.7534801583552,0.427545027690303,-42.717304287217));
#37557=CARTESIAN_POINT('Ctrl Pts',(-6.7624903836522,0.28521995354692,-42.7105961194147));
#37558=CARTESIAN_POINT('Ctrl Pts',(-6.76699999999999,0.142609995757751,
-42.7038879516124));
#37559=CARTESIAN_POINT('Ctrl Pts',(-6.767,7.1361580617263E-13,-42.6971797838101));
#37560=CARTESIAN_POINT('Ctrl Pts',(-6.76699988344647,-0.00125595997021738,
-42.6971797838101));
#37561=CARTESIAN_POINT('Ctrl Pts',(-6.76699667390786,-0.0185486666597619,
-42.6963684220283));
#37562=CARTESIAN_POINT('Ctrl Pts',(-6.76692717812646,-0.0358409891425261,
-42.6955570602465));
#37563=CARTESIAN_POINT('Ctrl Pts',(-6.76679140733531,-0.0531323781990722,
-42.6947456984647));
#37564=CARTESIAN_POINT('Ctrl Pts',(-6.76534913224035,-0.23681650923917,
-42.6861267099402));
#37565=CARTESIAN_POINT('Ctrl Pts',(-6.75642390721146,-0.420375002844922,
-42.6775077214157));
#37566=CARTESIAN_POINT('Ctrl Pts',(-6.740062835943,-0.603193142815786,-42.6688887328912));
#37567=CARTESIAN_POINT('Ctrl Pts',(-6.7236919629328,-0.786120807167066,
-42.6602645808235));
#37568=CARTESIAN_POINT('Ctrl Pts',(-6.69987638050173,-0.968306929775302,
-42.6516404287557));
#37569=CARTESIAN_POINT('Ctrl Pts',(-6.66871492179339,-1.14914328603976,
-42.6430162766879));
#37570=CARTESIAN_POINT('Ctrl Pts',(-6.63648617474091,-1.33617333615671,
-42.6340967450917));
#37571=CARTESIAN_POINT('Ctrl Pts',(-6.59639951463416,-1.52175917188238,
-42.6251772134955));
#37572=CARTESIAN_POINT('Ctrl Pts',(-6.54862125641083,-1.70524151957552,
-42.6162576818992));
#37573=CARTESIAN_POINT('Ctrl Pts',(-6.50233916687159,-1.88297814624599,
-42.60761746404));
#37574=CARTESIAN_POINT('Ctrl Pts',(-6.44884004425104,-2.05874075390657,
-42.5989772461807));
#37575=CARTESIAN_POINT('Ctrl Pts',(-6.38832542799106,-2.23194695861771,
-42.5903370283215));
#37576=CARTESIAN_POINT('Ctrl Pts',(-6.32487641287361,-2.41355206132448,
-42.5812778398568));
#37577=CARTESIAN_POINT('Ctrl Pts',(-6.25371475961217,-2.59234631320595,
-42.572218651392));
#37578=CARTESIAN_POINT('Ctrl Pts',(-6.17512908234659,-2.76768311342853,
-42.5631594629273));
#37579=CARTESIAN_POINT('Ctrl Pts',(-6.09654340508099,-2.94301991365113,
-42.5541002744626));
#37580=CARTESIAN_POINT('Ctrl Pts',(-6.01053390466334,-3.11489893486343,
-42.5450410859978));
#37581=CARTESIAN_POINT('Ctrl Pts',(-5.91744409407422,-3.28270382360427,
-42.5359818975331));
#37582=CARTESIAN_POINT('Ctrl Pts',(-5.82451555505095,-3.45021800214824,
-42.5269384034768));
#37583=CARTESIAN_POINT('Ctrl Pts',(-5.72444634757235,-3.61382688557528,
-42.5178949094205));
#37584=CARTESIAN_POINT('Ctrl Pts',(-5.61757415184038,-3.77294972780911,
-42.5088514153642));
#37585=CARTESIAN_POINT('Ctrl Pts',(-5.51079971171513,-3.93192702096089,
-42.4998161933589));
#37586=CARTESIAN_POINT('Ctrl Pts',(-5.39723483954908,-4.08642626782691,
-42.4907809713536));
#37587=CARTESIAN_POINT('Ctrl Pts',(-5.27726104762888,-4.23589480926745,
-42.4817457493482));
#37588=CARTESIAN_POINT('Ctrl Pts',(-5.15749862341199,-4.38510001967699,
-42.4727264454371));
#37589=CARTESIAN_POINT('Ctrl Pts',(-5.03134997524593,-4.52929203755353,
-42.463707141526));
#37590=CARTESIAN_POINT('Ctrl Pts',(-4.89923734187563,-4.66795056400252,
-42.4546878376149));
#37591=CARTESIAN_POINT('Ctrl Pts',(-4.76729045303197,-4.80643513364477,
-42.4456798490505));
#37592=CARTESIAN_POINT('Ctrl Pts',(-4.62939467470237,-4.93939989414737,
-42.4366718604862));
#37593=CARTESIAN_POINT('Ctrl Pts',(-4.48601128163889,-5.0663588286864,-42.4276638719218));
#37594=CARTESIAN_POINT('Ctrl Pts',(-4.34295172499068,-5.19303102202501,
-42.4186762282152));
#37595=CARTESIAN_POINT('Ctrl Pts',(-4.1944294710317,-5.31372430757826,-42.4096885845085));
#37596=CARTESIAN_POINT('Ctrl Pts',(-4.04094090057139,-5.42799093938902,
-42.4007009408018));
#37597=CARTESIAN_POINT('Ctrl Pts',(-3.90726299401948,-5.52750925585644,
-42.3928733260684));
#37598=CARTESIAN_POINT('Ctrl Pts',(-3.76981868177484,-5.62215328418074,
-42.385045711335));
#37599=CARTESIAN_POINT('Ctrl Pts',(-3.62895815416694,-5.71165052461242,
-42.3772180966016));
#37600=CARTESIAN_POINT('Ctrl Pts',(-3.48277921927813,-5.80452687190402,
-42.3690949381563));
#37601=CARTESIAN_POINT('Ctrl Pts',(-3.33298567607144,-5.89181751558342,
-42.360971779711));
#37602=CARTESIAN_POINT('Ctrl Pts',(-3.18005113614904,-5.97323729408745,
-42.3528486212657));
#37603=CARTESIAN_POINT('Ctrl Pts',(-3.02712737891212,-6.05465133207098,
-42.3447260355456));
#37604=CARTESIAN_POINT('Ctrl Pts',(-2.87106338916982,-6.13019515737294,
-42.3366034498255));
#37605=CARTESIAN_POINT('Ctrl Pts',(-2.71235758847528,-6.19962944959137,
-42.3284808641054));
#37606=CARTESIAN_POINT('Ctrl Pts',(-2.55363271764498,-6.2690720850548,-42.3203573023729));
#37607=CARTESIAN_POINT('Ctrl Pts',(-2.39226573957205,-6.33240358001369,
-42.3122337406405));
#37608=CARTESIAN_POINT('Ctrl Pts',(-2.22877521931706,-6.38943268387407,
-42.3041101789081));
#37609=CARTESIAN_POINT('Ctrl Pts',(-2.0651656156194,-6.446503326669,-42.295980700125));
#37610=CARTESIAN_POINT('Ctrl Pts',(-1.89942972642979,-6.49726228916622,
-42.2878512213419));
#37611=CARTESIAN_POINT('Ctrl Pts',(-1.73210206303117,-6.5415679651933,-42.2797217425588));
#37612=CARTESIAN_POINT('Ctrl Pts',(-1.56470618308922,-6.58589170386469,
-42.2715889495302));
#37613=CARTESIAN_POINT('Ctrl Pts',(-1.39571759232527,-6.62375683194439,
-42.2634561565017));
#37614=CARTESIAN_POINT('Ctrl Pts',(-1.22568091913084,-6.65507289850972,
-42.2553233634732));
#37615=CARTESIAN_POINT('Ctrl Pts',(-1.05545935685015,-6.68642301654657,
-42.247181727266));
#37616=CARTESIAN_POINT('Ctrl Pts',(-0.884187797736653,-6.71120979758355,
-42.2390400910589));
#37617=CARTESIAN_POINT('Ctrl Pts',(-0.712416664214558,-6.72939458618303,
-42.2308984548517));
#37618=CARTESIAN_POINT('Ctrl Pts',(-0.624901604834175,-6.7386594889724,
-42.2267504017912));
#37619=CARTESIAN_POINT('Ctrl Pts',(-0.537256897755374,-6.74621150705939,
-42.2226023487306));
#37620=CARTESIAN_POINT('Ctrl Pts',(-0.449555269251508,-6.75205072995518,
-42.2184542956701));
#37621=CARTESIAN_POINT('Ctrl Pts',(-0.271094570097564,-6.76393274193459,
-42.210013580692));
#37622=CARTESIAN_POINT('Ctrl Pts',(-0.0920306537212925,-6.76874397692548,
-42.2015728657139));
#37623=CARTESIAN_POINT('Ctrl Pts',(0.0870513340642555,-6.76644005849735,
-42.1931321507358));
#37624=CARTESIAN_POINT('Ctrl Pts',(0.265997963246156,-6.76413788147932,
-42.1846978156478));
#37625=CARTESIAN_POINT('Ctrl Pts',(0.444962304415066,-6.75473127597216,
-42.1762634805598));
#37626=CARTESIAN_POINT('Ctrl Pts',(0.623357093569214,-6.7382278778546,-42.1678291454718));
#37627=CARTESIAN_POINT('Ctrl Pts',(0.801644438093079,-6.72173441949772,
-42.1593998902631));
#37628=CARTESIAN_POINT('Ctrl Pts',(0.979362583322044,-6.69815272062077,
-42.1509706350545));
#37629=CARTESIAN_POINT('Ctrl Pts',(1.15592687335167,-6.66754243057091,-42.1425413798459));
#37630=CARTESIAN_POINT('Ctrl Pts',(1.33241190486665,-6.63694588127306,-42.1341159084729));
#37631=CARTESIAN_POINT('Ctrl Pts',(1.50774378596651,-6.59932708857285,-42.1256904370999));
#37632=CARTESIAN_POINT('Ctrl Pts',(1.68134517528666,-6.55479728149851,-42.1172649657268));
#37633=CARTESIAN_POINT('Ctrl Pts',(1.85489524299981,-6.51028063872699,-42.1088419851676));
#37634=CARTESIAN_POINT('Ctrl Pts',(2.02671551653271,-6.45885713873426,-42.1004190046083));
#37635=CARTESIAN_POINT('Ctrl Pts',(2.19624061559875,-6.40068872531655,-42.0919960240491));
#37636=CARTESIAN_POINT('Ctrl Pts',(2.36576852164858,-6.34251934875065,-42.0835729040228));
#37637=CARTESIAN_POINT('Ctrl Pts',(2.53300085986972,-6.27760493755164,-42.0751497839965));
#37638=CARTESIAN_POINT('Ctrl Pts',(2.69738849777813,-6.20615696643698,-42.0667266639701));
#37639=CARTESIAN_POINT('Ctrl Pts',(2.86178182048514,-6.13470652453235,-42.0583032526583));
#37640=CARTESIAN_POINT('Ctrl Pts',(3.0233299408013,-6.05672220499835,-42.0498798413464));
#37641=CARTESIAN_POINT('Ctrl Pts',(3.18150461990584,-5.97246325677419,-42.0414564300346));
#37642=CARTESIAN_POINT('Ctrl Pts',(3.33970682874089,-5.88818964358501,-42.0330315526585));
#37643=CARTESIAN_POINT('Ctrl Pts',(3.49453413146048,-5.79763938121708,-42.0246066752823));
#37644=CARTESIAN_POINT('Ctrl Pts',(3.64548344457245,-5.70111738656101,-42.0161817979062));
#37645=CARTESIAN_POINT('Ctrl Pts',(3.79648008846895,-5.60456512703233,-42.0077542788748));
#37646=CARTESIAN_POINT('Ctrl Pts',(3.94359603761136,-5.5020375816183,-41.9993267598434));
#37647=CARTESIAN_POINT('Ctrl Pts',(4.08635741077098,-5.39388284183455,-41.9908992408119));
#37648=CARTESIAN_POINT('Ctrl Pts',(4.22924680681245,-5.28563111306024,-41.9824641643072));
#37649=CARTESIAN_POINT('Ctrl Pts',(4.36777355801776,-5.17174230835793,-41.9740290878024));
#37650=CARTESIAN_POINT('Ctrl Pts',(4.50149620337621,-5.0526053607015,-41.9655940112976));
#37651=CARTESIAN_POINT('Ctrl Pts',(4.63528347776928,-4.93341083337415,-41.9571548580648));
#37652=CARTESIAN_POINT('Ctrl Pts',(4.76426177222556,-4.80896333213209,-41.948715704832));
#37653=CARTESIAN_POINT('Ctrl Pts',(4.88802633549392,-4.67968882977468,-41.9402765515993));
#37654=CARTESIAN_POINT('Ctrl Pts',(5.01192843589208,-4.55027066720032,-41.9318280201011));
#37655=CARTESIAN_POINT('Ctrl Pts',(5.13060500335559,-4.41601503165668,-41.923379488603));
#37656=CARTESIAN_POINT('Ctrl Pts',(5.24369064745112,-4.27738207246368,-41.9149309571049));
#37657=CARTESIAN_POINT('Ctrl Pts',(5.30617413488637,-4.20078286455247,-41.910262869339));
#37658=CARTESIAN_POINT('Ctrl Pts',(5.36695149572751,-4.12284785073278,-41.905594781573));
#37659=CARTESIAN_POINT('Ctrl Pts',(5.42596674891508,-4.04365847218431,-41.900926693807));
#37660=CARTESIAN_POINT('Ctrl Pts',(5.53014890715346,-3.90386206496541,-41.8926859182103));
#37661=CARTESIAN_POINT('Ctrl Pts',(5.62906881304512,-3.75984380107845,-41.8844451426135));
#37662=CARTESIAN_POINT('Ctrl Pts',(5.72236768346778,-3.61203503515728,-41.8762043670168));
#37663=CARTESIAN_POINT('Ctrl Pts',(5.8155632152766,-3.46438998346879,-41.8679727189724));
#37664=CARTESIAN_POINT('Ctrl Pts',(5.90314992029334,-3.31296308773015,-41.859741070928));
#37665=CARTESIAN_POINT('Ctrl Pts',(5.9848098138501,-3.15821792978945,-41.8515094228837));
#37666=CARTESIAN_POINT('Ctrl Pts',(6.06639381277728,-3.00361659185548,-41.8432854253254));
#37667=CARTESIAN_POINT('Ctrl Pts',(6.14206180527136,-2.84570344639689,-41.8350614277671));
#37668=CARTESIAN_POINT('Ctrl Pts',(6.21153957002151,-2.68497023634471,-41.8268374302088));
#37669=CARTESIAN_POINT('Ctrl Pts',(6.28095595089663,-2.52437903470798,-41.8186206985843));
#37670=CARTESIAN_POINT('Ctrl Pts',(6.34419286387446,-2.36097305971089,-41.8104039669598));
#37671=CARTESIAN_POINT('Ctrl Pts',(6.40102248589785,-2.19526766819678,-41.8021872353353));
#37672=CARTESIAN_POINT('Ctrl Pts',(6.45782299200198,-2.02964717368934,-41.7939747134466));
#37673=CARTESIAN_POINT('Ctrl Pts',(6.50822262984406,-1.86172994464453,-41.785762191558));
#37674=CARTESIAN_POINT('Ctrl Pts',(6.552041934908,-1.69205067394776,-41.7775496696693));
#37675=CARTESIAN_POINT('Ctrl Pts',(6.5958465865854,-1.52242814481584,-41.7693398940874));
#37676=CARTESIAN_POINT('Ctrl Pts',(6.63307520026661,-1.35104509196461,-41.7611301185056));
#37677=CARTESIAN_POINT('Ctrl Pts',(6.66359833152834,-1.17845079492218,-41.7529203429237));
#37678=CARTESIAN_POINT('Ctrl Pts',(6.67693004226706,-1.10306609000473,-41.749334526241));
#37679=CARTESIAN_POINT('Ctrl Pts',(6.68898318843072,-1.02745047825498,-41.7457487095583));
#37680=CARTESIAN_POINT('Ctrl Pts',(6.69975003711949,-0.951650377038417,
-41.7421628928756));
#37681=CARTESIAN_POINT('Ctrl Pts',(6.72634940891484,-0.764387127348094,
-41.7333041753538));
#37682=CARTESIAN_POINT('Ctrl Pts',(6.74506725240592,-0.576191466641557,
-41.7244454578321));
#37683=CARTESIAN_POINT('Ctrl Pts',(6.75588373128169,-0.387716403319989,
-41.7155867403103));
#37684=CARTESIAN_POINT('Ctrl Pts',(6.76672044605221,-0.198888733425766,
-41.7067114495509));
#37685=CARTESIAN_POINT('Ctrl Pts',(6.7696262401614,-0.00978087522273441,
-41.6978361587914));
#37686=CARTESIAN_POINT('Ctrl Pts',(6.76463333577029,0.178954833925484,-41.6889608680319));
#37687=CARTESIAN_POINT('Ctrl Pts',(6.75962625040808,0.368226594923957,-41.6800603694512));
#37688=CARTESIAN_POINT('Ctrl Pts',(6.74667558010456,0.55712383083115,-41.6711598708704));
#37689=CARTESIAN_POINT('Ctrl Pts',(6.72586564017671,0.744996906228688,-41.6622593722896));
#37690=CARTESIAN_POINT('Ctrl Pts',(6.70502752980533,0.933124305659871,-41.653346825092));
#37691=CARTESIAN_POINT('Ctrl Pts',(6.6763089326328,1.12022451814475,-41.6444342778944));
#37692=CARTESIAN_POINT('Ctrl Pts',(6.6398454633218,1.30565739120373,-41.6355217306967));
#37693=CARTESIAN_POINT('Ctrl Pts',(6.6033014791094,1.49149971815651,-41.6265895037245));
#37694=CARTESIAN_POINT('Ctrl Pts',(6.55897846730552,1.67566708626609,-41.6176572767522));
#37695=CARTESIAN_POINT('Ctrl Pts',(6.50706289319567,1.85753102369678,-41.6087250497799));
#37696=CARTESIAN_POINT('Ctrl Pts',(6.4579966806668,2.02941344546159,-41.6002830638347));
#37697=CARTESIAN_POINT('Ctrl Pts',(6.40214894479632,2.19923830639945,-41.5918410778894));
#37698=CARTESIAN_POINT('Ctrl Pts',(6.33971681340197,2.36649101537877,-41.5833990919441));
#37699=CARTESIAN_POINT('Ctrl Pts',(6.2788864724797,2.52945260390952,-41.5751736978778));
#37700=CARTESIAN_POINT('Ctrl Pts',(6.21168807255892,2.69028331838405,-41.5669483038116));
#37701=CARTESIAN_POINT('Ctrl Pts',(6.13829108938444,2.84845071959892,-41.5587229097454));
#37702=CARTESIAN_POINT('Ctrl Pts',(6.06497432842782,3.00644524531988,-41.5505065059581));
#37703=CARTESIAN_POINT('Ctrl Pts',(5.985472627089,3.16178193241649,-41.5422901021709));
#37704=CARTESIAN_POINT('Ctrl Pts',(5.90000456429368,3.31394555497126,-41.5340736983836));
#37705=CARTESIAN_POINT('Ctrl Pts',(5.81462748643463,3.46594719190184,-41.5258660413603));
#37706=CARTESIAN_POINT('Ctrl Pts',(5.72329688111432,3.61478218583412,-41.5176583843371));
#37707=CARTESIAN_POINT('Ctrl Pts',(5.62627842502757,3.75995745774727,-41.5094507273138));
#37708=CARTESIAN_POINT('Ctrl Pts',(5.52931891580423,3.90504452348535,-41.5012480571318));
#37709=CARTESIAN_POINT('Ctrl Pts',(5.42667863579515,4.04647599795403,-41.4930453869498));
#37710=CARTESIAN_POINT('Ctrl Pts',(5.31866823445393,4.18378503413007,-41.4848427167678));
#37711=CARTESIAN_POINT('Ctrl Pts',(5.21070383673897,4.32103558784976,-41.4766435402546));
#37712=CARTESIAN_POINT('Ctrl Pts',(5.09737409444621,4.45416691912772,-41.4684443637414));
#37713=CARTESIAN_POINT('Ctrl Pts',(4.97903189103809,4.58274267530107,-41.4602451872282));
#37714=CARTESIAN_POINT('Ctrl Pts',(4.8607185942922,4.7112870251304,-41.4520480134733));
#37715=CARTESIAN_POINT('Ctrl Pts',(4.73739551863087,4.83527775352706,-41.4438508397184));
#37716=CARTESIAN_POINT('Ctrl Pts',(4.60945463056433,4.95431297040962,-41.4356536659635));
#37717=CARTESIAN_POINT('Ctrl Pts',(4.48149343125921,5.07336708471214,-41.4274551908673));
#37718=CARTESIAN_POINT('Ctrl Pts',(4.3489132137002,5.18746386741849,-41.4192567157712));
#37719=CARTESIAN_POINT('Ctrl Pts',(4.21214178388496,5.29623928768805,-41.411058240675));
#37720=CARTESIAN_POINT('Ctrl Pts',(4.07535939164419,5.40502342646298,-41.4028591084594));
#37721=CARTESIAN_POINT('Ctrl Pts',(3.93438540207997,5.50848513434416,-41.3946599762438));
#37722=CARTESIAN_POINT('Ctrl Pts',(3.78967927024918,5.60630181390938,-41.3864608440281));
#37723=CARTESIAN_POINT('Ctrl Pts',(3.64488903257014,5.70417534631632,-41.378256946327));
#37724=CARTESIAN_POINT('Ctrl Pts',(3.49636262006873,5.79639710062467,-41.3700530486259));
#37725=CARTESIAN_POINT('Ctrl Pts',(3.34458741463909,5.88268850321329,-41.3618491509248));
#37726=CARTESIAN_POINT('Ctrl Pts',(3.26365133982806,5.92870450033015,-41.3574743172608));
#37727=CARTESIAN_POINT('Ctrl Pts',(3.18179184063274,5.97303486141136,-41.3530994835967));
#37728=CARTESIAN_POINT('Ctrl Pts',(3.09908550384719,6.01564277861013,-41.3487246499327));
#37729=CARTESIAN_POINT('Origin',(0.,0.,-63.6971797838103));
#37730=CARTESIAN_POINT('',(3.0990855038472,6.01564277861013,-38.9542099095282));
#37731=CARTESIAN_POINT('',(3.09908550384721,6.01564277861012,-39.3484860224351));
#37732=CARTESIAN_POINT('',(3.09908550384721,6.01564277861012,-63.6971797838103));
#37733=CARTESIAN_POINT('',(-6.76699799023945,0.00521537105487791,-40.3028202161432));
#37734=CARTESIAN_POINT('Ctrl Pts',(-6.76699799023945,0.00521537105492299,
-40.3028202161432));
#37735=CARTESIAN_POINT('Ctrl Pts',(-6.76712754022321,-0.162877075380806,
-40.2948963058703));
#37736=CARTESIAN_POINT('Ctrl Pts',(-6.76098983979437,-0.33122543153812,
-40.2869723955973));
#37737=CARTESIAN_POINT('Ctrl Pts',(-6.74855428627843,-0.499303560124519,
-40.2790484853244));
#37738=CARTESIAN_POINT('Ctrl Pts',(-6.73559519402501,-0.674457804070364,
-40.2707909771963));
#37739=CARTESIAN_POINT('Ctrl Pts',(-6.715796363107,-0.849318163805499,-40.2625334690682));
#37740=CARTESIAN_POINT('Ctrl Pts',(-6.6891833820932,-1.02328621642635,-40.2542759609401));
#37741=CARTESIAN_POINT('Ctrl Pts',(-6.66368313374093,-1.18998037762888,
-40.2463637128561));
#37742=CARTESIAN_POINT('Ctrl Pts',(-6.63192704679351,-1.35585490386659,
-40.238451464772));
#37743=CARTESIAN_POINT('Ctrl Pts',(-6.59399069768826,-1.52038668726107,
-40.230539216688));
#37744=CARTESIAN_POINT('Ctrl Pts',(-6.55606781177178,-1.68486008015379,
-40.2226297765729));
#37745=CARTESIAN_POINT('Ctrl Pts',(-6.51196911464742,-1.84799130365533,
-40.2147203364577));
#37746=CARTESIAN_POINT('Ctrl Pts',(-6.46182138259852,-2.00926688605388,
-40.2068108963426));
#37747=CARTESIAN_POINT('Ctrl Pts',(-6.41167809603406,-2.17052817173221,
-40.1989021573817));
#37748=CARTESIAN_POINT('Ctrl Pts',(-6.35548695491127,-2.32993377560291,
-40.1909934184208));
#37749=CARTESIAN_POINT('Ctrl Pts',(-6.29342468653699,-2.48698506527217,
-40.1830846794599));
#37750=CARTESIAN_POINT('Ctrl Pts',(-6.28524703420593,-2.50767897283795,
-40.1820425822357));
#37751=CARTESIAN_POINT('Ctrl Pts',(-6.27696751642473,-2.52833203012484,
-40.1810004850115));
#37752=CARTESIAN_POINT('Ctrl Pts',(-6.2685866004644,-2.5489431206832,-40.1799583877873));
#37753=CARTESIAN_POINT('Ctrl Pts',(-6.19734164812911,-2.72415501534487,
-40.1710996702656));
#37754=CARTESIAN_POINT('Ctrl Pts',(-6.11881653475247,-2.89620666730619,
-40.1622409527438));
#37755=CARTESIAN_POINT('Ctrl Pts',(-6.03332271373748,-3.06452378550069,
-40.1533822352221));
#37756=CARTESIAN_POINT('Ctrl Pts',(-5.94766894751403,-3.23315579799089,
-40.1445069444626));
#37757=CARTESIAN_POINT('Ctrl Pts',(-5.85502053688083,-3.39803908301622,
-40.1356316537032));
#37758=CARTESIAN_POINT('Ctrl Pts',(-5.75573358487283,-3.55862612534205,
-40.1267563629437));
#37759=CARTESIAN_POINT('Ctrl Pts',(-5.65616463559707,-3.71966927097509,
-40.1178558643629));
#37760=CARTESIAN_POINT('Ctrl Pts',(-5.54991955111832,-3.87639153365262,
-40.1089553657822));
#37761=CARTESIAN_POINT('Ctrl Pts',(-5.43739809211884,-4.02827394647166,
-40.1000548672014));
#37762=CARTESIAN_POINT('Ctrl Pts',(-5.32472431266944,-4.1803619627166,-40.0911423200038));
#37763=CARTESIAN_POINT('Ctrl Pts',(-5.20575734639003,-4.32759683721942,
-40.0822297728061));
#37764=CARTESIAN_POINT('Ctrl Pts',(-5.08093651341278,-4.46949361188365,
-40.0733172256085));
#37765=CARTESIAN_POINT('Ctrl Pts',(-4.95584006384608,-4.61170370848426,
-40.0643849986362));
#37766=CARTESIAN_POINT('Ctrl Pts',(-4.82486406561801,-4.74855193368263,
-40.0554527716639));
#37767=CARTESIAN_POINT('Ctrl Pts',(-4.68848590464814,-4.8795890115783,-40.0465205446917));
#37768=CARTESIAN_POINT('Ctrl Pts',(-4.55959279414736,-5.00343418180786,
-40.0380785587464));
#37769=CARTESIAN_POINT('Ctrl Pts',(-4.4258746730809,-5.12208879441507,-40.0296365728011));
#37770=CARTESIAN_POINT('Ctrl Pts',(-4.28776083656365,-5.23520735104456,
-40.0211945868558));
#37771=CARTESIAN_POINT('Ctrl Pts',(-4.15321374473151,-5.34540465792225,
-40.0129706124382));
#37772=CARTESIAN_POINT('Ctrl Pts',(-4.01423736702672,-5.45055785106176,
-40.0047466380206));
#37773=CARTESIAN_POINT('Ctrl Pts',(-3.87124586600751,-5.55029228463869,
-39.9965226636031));
#37774=CARTESIAN_POINT('Ctrl Pts',(-3.72840537788679,-5.64992138897727,
-39.9883073745004));
#37775=CARTESIAN_POINT('Ctrl Pts',(-3.58155850211936,-5.74414292619686,
-39.9800920853978));
#37776=CARTESIAN_POINT('Ctrl Pts',(-3.4311532002971,-5.83262177036116,-39.9718767962951));
#37777=CARTESIAN_POINT('Ctrl Pts',(-3.2808765729689,-5.92102491925163,-39.9636685355229));
#37778=CARTESIAN_POINT('Ctrl Pts',(-3.12704788995173,-6.00369497898534,
-39.9554602747507));
#37779=CARTESIAN_POINT('Ctrl Pts',(-2.97014495677272,-6.08033945892477,
-39.9472520139786));
#37780=CARTESIAN_POINT('Ctrl Pts',(-2.81334479450807,-6.15693373697744,
-39.9390491295907));
#37781=CARTESIAN_POINT('Ctrl Pts',(-2.65347471406588,-6.22751013988855,
-39.9308462452028));
#37782=CARTESIAN_POINT('Ctrl Pts',(-2.49103812149956,-6.29182152299602,
-39.9226433608149));
#37783=CARTESIAN_POINT('Ctrl Pts',(-2.32867535899208,-6.35610367553958,
-39.9144442047707));
#37784=CARTESIAN_POINT('Ctrl Pts',(-2.16374874110233,-6.41412634961514,
-39.9062450487264));
#37785=CARTESIAN_POINT('Ctrl Pts',(-1.99678278431146,-6.46569002599702,
-39.8980458926822));
#37786=CARTESIAN_POINT('Ctrl Pts',(-1.82983134949951,-6.51724921759269,
-39.8898474497652));
#37787=CARTESIAN_POINT('Ctrl Pts',(-1.66084126893709,-6.56235041658473,
-39.8816490068482));
#37788=CARTESIAN_POINT('Ctrl Pts',(-1.49035374915082,-6.60084348416111,
-39.8734505639312));
#37789=CARTESIAN_POINT('Ctrl Pts',(-1.3198679272181,-6.63933616839217,-39.865252202661));
#37790=CARTESIAN_POINT('Ctrl Pts',(-1.1478850454227,-6.67122077225602,-39.8570538413907));
#37791=CARTESIAN_POINT('Ctrl Pts',(-0.974957957846269,-6.69639798551671,
-39.8488554801205));
#37792=CARTESIAN_POINT('Ctrl Pts',(-0.802001178975093,-6.72157952166325,
-39.8406557112052));
#37793=CARTESIAN_POINT('Ctrl Pts',(-0.628100226299769,-6.74005132110533,
-39.8324559422899));
#37794=CARTESIAN_POINT('Ctrl Pts',(-0.453814608423492,-6.75176579134536,
-39.8242561733746));
#37795=CARTESIAN_POINT('Ctrl Pts',(-0.27946740543439,-6.76348440098014,
-39.8160535070103));
#37796=CARTESIAN_POINT('Ctrl Pts',(-0.104735624150543,-6.76844090092971,
-39.8078508406459));
#37797=CARTESIAN_POINT('Ctrl Pts',(0.06981962896297,-6.76663980269465,-39.7996481742816));
#37798=CARTESIAN_POINT('Ctrl Pts',(0.244573133213151,-6.76483665886219,
-39.7914361917386));
#37799=CARTESIAN_POINT('Ctrl Pts',(0.419149349707361,-6.75626058751377,
-39.7832242091956));
#37800=CARTESIAN_POINT('Ctrl Pts',(0.592989640392857,-6.74096820096244,
-39.7750122266526));
#37801=CARTESIAN_POINT('Ctrl Pts',(0.766932464431034,-6.72566679475486,
-39.7667954005713));
#37802=CARTESIAN_POINT('Ctrl Pts',(0.940138142190733,-6.70364122208695,
-39.75857857449));
#37803=CARTESIAN_POINT('Ctrl Pts',(1.11205676947754,-6.67499953119543,-39.7503617484087));
#37804=CARTESIAN_POINT('Ctrl Pts',(1.28424052011747,-6.64631367067989,-39.7421322507948));
#37805=CARTESIAN_POINT('Ctrl Pts',(1.4551329028892,-6.61099137519713,-39.733902753181));
#37806=CARTESIAN_POINT('Ctrl Pts',(1.62419645638245,-6.5691913407264,-39.7256732555671));
#37807=CARTESIAN_POINT('Ctrl Pts',(1.77489250438824,-6.53193257104429,-39.7183378320423));
#37808=CARTESIAN_POINT('Ctrl Pts',(1.9241355659828,-6.48952788029005,-39.7110024085175));
#37809=CARTESIAN_POINT('Ctrl Pts',(2.07155830167241,-6.44212194876596,-39.7036669849927));
#37810=CARTESIAN_POINT('Ctrl Pts',(2.23376158253994,-6.38996311729522,-39.6955961148063));
#37811=CARTESIAN_POINT('Ctrl Pts',(2.39428981073306,-6.3315789062554,-39.6875252446199));
#37812=CARTESIAN_POINT('Ctrl Pts',(2.55261704114451,-6.26709144988795,-39.6794543744335));
#37813=CARTESIAN_POINT('Ctrl Pts',(2.71074724562398,-6.20268424314755,-39.6713935478177));
#37814=CARTESIAN_POINT('Ctrl Pts',(2.86668156109682,-6.13218904221026,-39.663332721202));
#37815=CARTESIAN_POINT('Ctrl Pts',(3.01990695852402,-6.05577831181577,-39.6552718945862));
#37816=CARTESIAN_POINT('Ctrl Pts',(3.17297527884556,-5.97944591292879,-39.6472193314263));
#37817=CARTESIAN_POINT('Ctrl Pts',(3.32333987649275,-5.89721021769609,-39.6391667682664));
#37818=CARTESIAN_POINT('Ctrl Pts',(3.4705056479343,-5.80929251696419,-39.6311142051065));
#37819=CARTESIAN_POINT('Ctrl Pts',(3.61755277806687,-5.72144569325074,-39.6230681337186));
#37820=CARTESIAN_POINT('Ctrl Pts',(3.76140589614113,-5.62792617154377,-39.6150220623308));
#37821=CARTESIAN_POINT('Ctrl Pts',(3.90159265552522,-5.52900205736548,-39.6069759909429));
#37822=CARTESIAN_POINT('Ctrl Pts',(4.04169706415997,-5.43013605477323,-39.598934646107));
#37823=CARTESIAN_POINT('Ctrl Pts',(4.17813909763124,-5.32587199447616,-39.5908933012711));
#37824=CARTESIAN_POINT('Ctrl Pts',(4.31047376756382,-5.2165222993048,-39.5828519564352));
#37825=CARTESIAN_POINT('Ctrl Pts',(4.44535944273825,-5.10506467848009,-39.5746555992142));
#37826=CARTESIAN_POINT('Ctrl Pts',(4.57597744504392,-4.98832355638715,-39.5664592419931));
#37827=CARTESIAN_POINT('Ctrl Pts',(4.70188996882324,-4.86667440056137,-39.558262884772));
#37828=CARTESIAN_POINT('Ctrl Pts',(4.82538192349467,-4.74736385395217,-39.5502240960636));
#37829=CARTESIAN_POINT('Ctrl Pts',(4.94434741386688,-4.6233325525606,-39.5421853073551));
#37830=CARTESIAN_POINT('Ctrl Pts',(5.05840932216131,-4.49497320675792,-39.5341465186466));
#37831=CARTESIAN_POINT('Ctrl Pts',(5.17248343611352,-4.36660012534208,-39.5261068697149));
#37832=CARTESIAN_POINT('Ctrl Pts',(5.28165267500553,-4.23389835645969,-39.5180672207831));
#37833=CARTESIAN_POINT('Ctrl Pts',(5.38557929067777,-4.09729480313813,-39.5100275718514));
#37834=CARTESIAN_POINT('Ctrl Pts',(5.48953760530579,-3.9606495839741,-39.5019854707233));
#37835=CARTESIAN_POINT('Ctrl Pts',(5.58824988777376,-3.82010050855278,-39.4939433695951));
#37836=CARTESIAN_POINT('Ctrl Pts',(5.68142100308067,-3.6761045123546,-39.485901268467));
#37837=CARTESIAN_POINT('Ctrl Pts',(5.77773627747091,-3.52724921702795,-39.4775877780222));
#37838=CARTESIAN_POINT('Ctrl Pts',(5.86812961838286,-3.37471065711725,-39.4692742875774));
#37839=CARTESIAN_POINT('Ctrl Pts',(5.95232643524389,-3.21902143644568,-39.4609607971326));
#37840=CARTESIAN_POINT('Ctrl Pts',(6.03391817342702,-3.06814929418955,-39.4529045289619));
#37841=CARTESIAN_POINT('Ctrl Pts',(6.10969102577833,-2.91431891546404,-39.4448482607911));
#37842=CARTESIAN_POINT('Ctrl Pts',(6.17944429363589,-2.75803502911961,-39.4367919926203));
#37843=CARTESIAN_POINT('Ctrl Pts',(6.25253820764567,-2.59426634414703,-39.4283498910386));
#37844=CARTESIAN_POINT('Ctrl Pts',(6.31902159426447,-2.42780381573808,-39.4199077894568));
#37845=CARTESIAN_POINT('Ctrl Pts',(6.37872252447252,-2.25924499684892,-39.4114656878751));
#37846=CARTESIAN_POINT('Ctrl Pts',(6.43842345468058,-2.09068617795977,-39.4030235862933));
#37847=CARTESIAN_POINT('Ctrl Pts',(6.49134187456447,-1.92003153439721,-39.3945814847115));
#37848=CARTESIAN_POINT('Ctrl Pts',(6.53736745489061,-1.74788894376531,-39.3861393831297));
#37849=CARTESIAN_POINT('Ctrl Pts',(6.58280281746738,-1.57795385625877,-39.3778055404371));
#37850=CARTESIAN_POINT('Ctrl Pts',(6.62166609770372,-1.40602866319757,-39.3694716977444));
#37851=CARTESIAN_POINT('Ctrl Pts',(6.65378441784946,-1.23265644880628,-39.3611378550517));
#37852=CARTESIAN_POINT('Ctrl Pts',(6.68586488249151,-1.05948857550362,-39.352813834847));
#37853=CARTESIAN_POINT('Ctrl Pts',(6.71121616091981,-0.884877417489458,
-39.3444898146423));
#37854=CARTESIAN_POINT('Ctrl Pts',(6.72971532596606,-0.709380456072482,
-39.3361657944375));
#37855=CARTESIAN_POINT('Ctrl Pts',(6.74819607920109,-0.534058162912889,
-39.3278500589466));
#37856=CARTESIAN_POINT('Ctrl Pts',(6.75983827004864,-0.357852166613005,
-39.3195343234557));
#37857=CARTESIAN_POINT('Ctrl Pts',(6.76457009572151,-0.181329589616151,
-39.3112185879649));
#37858=CARTESIAN_POINT('Ctrl Pts',(6.76929807890517,-0.00495035815688297,
-39.3029096052848));
#37859=CARTESIAN_POINT('Ctrl Pts',(6.76712686923503,0.171744595524779,-39.2946006226048));
#37860=CARTESIAN_POINT('Ctrl Pts',(6.75803650121376,0.348183354373005,-39.2862916399247));
#37861=CARTESIAN_POINT('Ctrl Pts',(6.7489518503696,0.524511146137264,-39.2779878829875));
#37862=CARTESIAN_POINT('Ctrl Pts',(6.73295673138763,0.700582717780264,-39.2696841260503));
#37863=CARTESIAN_POINT('Ctrl Pts',(6.710083261767,0.875826249980194,-39.2613803691131));
#37864=CARTESIAN_POINT('Ctrl Pts',(6.68721907822373,1.05099863752983,-39.2530799833011));
#37865=CARTESIAN_POINT('Ctrl Pts',(6.65748215314951,1.22534331112235,-39.244779597489));
#37866=CARTESIAN_POINT('Ctrl Pts',(6.62095647461996,1.39829337450625,-39.236479211677));
#37867=CARTESIAN_POINT('Ctrl Pts',(6.58443849840557,1.57120696722212,-39.2281805762004));
#37868=CARTESIAN_POINT('Ctrl Pts',(6.5411346925989,1.74272619553313,-39.2198819407237));
#37869=CARTESIAN_POINT('Ctrl Pts',(6.49118024488089,1.91229391790805,-39.2115833052471));
#37870=CARTESIAN_POINT('Ctrl Pts',(6.44122803939115,2.08185402915806,-39.2032850422585));
#37871=CARTESIAN_POINT('Ctrl Pts',(6.38462588530303,2.24946247548421,-39.1949867792699));
#37872=CARTESIAN_POINT('Ctrl Pts',(6.3215590270979,2.41457666412088,-39.1866885162813));
#37873=CARTESIAN_POINT('Ctrl Pts',(6.25848453176547,2.57971084738092,-39.1783892484085));
#37874=CARTESIAN_POINT('Ctrl Pts',(6.18894389704812,2.74234984643531,-39.1700899805357));
#37875=CARTESIAN_POINT('Ctrl Pts',(6.11317082247102,2.90197027815397,-39.1617907126628));
#37876=CARTESIAN_POINT('Ctrl Pts',(6.03734454298267,3.06170278914287,-39.1534856173663));
#37877=CARTESIAN_POINT('Ctrl Pts',(5.95527722858991,3.21841218305704,-39.1451805220698));
#37878=CARTESIAN_POINT('Ctrl Pts',(5.86724934654525,3.37159815302245,-39.1368754267733));
#37879=CARTESIAN_POINT('Ctrl Pts',(5.77918936495744,3.52483998255801,-39.1285673030072));
#37880=CARTESIAN_POINT('Ctrl Pts',(5.68516466323755,3.67455552950446,-39.1202591792411));
#37881=CARTESIAN_POINT('Ctrl Pts',(5.58549963236082,3.82027261552067,-39.111951055475));
#37882=CARTESIAN_POINT('Ctrl Pts',(5.48572865813215,3.96614459795734,-39.1036341002213));
#37883=CARTESIAN_POINT('Ctrl Pts',(5.38030557814278,4.10800934435273,-39.0953171449676));
#37884=CARTESIAN_POINT('Ctrl Pts',(5.26959639949399,4.24542610187011,-39.0870001897139));
#37885=CARTESIAN_POINT('Ctrl Pts',(5.18800541923077,4.34670016141312,-39.0808707202315));
#37886=CARTESIAN_POINT('Ctrl Pts',(5.10354417342413,4.44555897920631,-39.0747412507491));
#37887=CARTESIAN_POINT('Ctrl Pts',(5.01637213175427,4.54183879455877,-39.0686117812667));
#37888=CARTESIAN_POINT('Ctrl Pts',(4.89616454163102,4.6746057271593,-39.0601594295596));
#37889=CARTESIAN_POINT('Ctrl Pts',(4.77058116702232,4.80270984526433,-39.0517070778525));
#37890=CARTESIAN_POINT('Ctrl Pts',(4.64000953199913,4.9257081260421,-39.0432547261455));
#37891=CARTESIAN_POINT('Ctrl Pts',(4.50958742826625,5.04856554857278,-39.0348120541139));
#37892=CARTESIAN_POINT('Ctrl Pts',(4.3741886985638,5.16632857020355,-39.0263693820823));
#37893=CARTESIAN_POINT('Ctrl Pts',(4.23423858843679,5.27859001781658,-39.0179267100508));
#37894=CARTESIAN_POINT('Ctrl Pts',(4.09438353268352,5.39077521724668,-39.0094897722977));
#37895=CARTESIAN_POINT('Ctrl Pts',(3.94998351461975,5.49746608262539,-39.0010528345446));
#37896=CARTESIAN_POINT('Ctrl Pts',(3.80149853946319,5.59829419148898,-38.9926158967915));
#37897=CARTESIAN_POINT('Ctrl Pts',(3.6531119608367,5.69905548459539,-38.9841845499434));
#37898=CARTESIAN_POINT('Ctrl Pts',(3.50064609711128,5.79396158332724,-38.9757532030954));
#37899=CARTESIAN_POINT('Ctrl Pts',(3.34459189983079,5.88268595316683,-38.9673218562474));
#37900=CARTESIAN_POINT('Ctrl Pts',(3.26369638942458,5.92867896911078,-38.962951207341));
#37901=CARTESIAN_POINT('Ctrl Pts',(3.18183712474675,5.97301153234306,-38.9585805584346));
#37902=CARTESIAN_POINT('Ctrl Pts',(3.0990855038472,6.01564277861013,-38.9542099095282));
#37903=CARTESIAN_POINT('Ctrl Pts',(3.09908550384721,6.01564277861012,-40.9541976313953));
#37904=CARTESIAN_POINT('Ctrl Pts',(2.92882846838773,6.10335428840864,-40.945159916578));
#37905=CARTESIAN_POINT('Ctrl Pts',(2.75478964636869,6.18386283890986,-40.9361222017608));
#37906=CARTESIAN_POINT('Ctrl Pts',(2.57757057627381,6.25686973848166,-40.9270844869435));
#37907=CARTESIAN_POINT('Ctrl Pts',(2.39443892302602,6.33231237684965,-40.9177452456576));
#37908=CARTESIAN_POINT('Ctrl Pts',(2.20791136910832,6.39974403881214,-40.9084060043718));
#37909=CARTESIAN_POINT('Ctrl Pts',(2.01867762557476,6.45888764757554,-40.8990667630859));
#37910=CARTESIAN_POINT('Ctrl Pts',(1.83609765572756,6.51595166852147,-40.8900559050829));
#37911=CARTESIAN_POINT('Ctrl Pts',(1.65099880494576,6.56530041468836,-40.8810450470798));
#37912=CARTESIAN_POINT('Ctrl Pts',(1.46402058189181,6.60673389321813,-40.8720341890768));
#37913=CARTESIAN_POINT('Ctrl Pts',(1.27729665572115,6.64811102077674,-40.8630355861539));
#37914=CARTESIAN_POINT('Ctrl Pts',(1.08869868941265,6.68159430937247,-40.854036983231));
#37915=CARTESIAN_POINT('Ctrl Pts',(0.898879886899542,6.70703391589214,-40.845038380308));
#37916=CARTESIAN_POINT('Ctrl Pts',(0.709452354237807,6.73242108423957,-40.8360583260325));
#37917=CARTESIAN_POINT('Ctrl Pts',(0.518809243438361,6.74979762800268,-40.8270782717569));
#37918=CARTESIAN_POINT('Ctrl Pts',(0.327612572950701,6.75906495027564,-40.8180982174814));
#37919=CARTESIAN_POINT('Ctrl Pts',(0.305720715110656,6.76012605087556,-40.8170700088253));
#37920=CARTESIAN_POINT('Ctrl Pts',(0.283821611724741,6.76108089412076,-40.8160418001693));
#37921=CARTESIAN_POINT('Ctrl Pts',(0.261916265177378,6.76192937481867,-40.8150135915133));
#37922=CARTESIAN_POINT('Ctrl Pts',(0.0888574217582246,6.76863262819677,
-40.806890433068));
#37923=CARTESIAN_POINT('Ctrl Pts',(-0.0845143140218471,6.76869001244394,
-40.7987672746227));
#37924=CARTESIAN_POINT('Ctrl Pts',(-0.257646167912469,6.76209342231827,
-40.7906441161774));
#37925=CARTESIAN_POINT('Ctrl Pts',(-0.430765815101109,6.75549729728674,
-40.7825215304573));
#37926=CARTESIAN_POINT('Ctrl Pts',(-0.603645248330071,6.74224814629945,
-40.7743989447372));
#37927=CARTESIAN_POINT('Ctrl Pts',(-0.77573332074428,6.72238996303302,-40.7662763590171));
#37928=CARTESIAN_POINT('Ctrl Pts',(-0.947842071311835,6.70252939360145,
-40.7581527972847));
#37929=CARTESIAN_POINT('Ctrl Pts',(-1.11915890825157,6.67605825371389,-40.7500292355523));
#37930=CARTESIAN_POINT('Ctrl Pts',(-1.28913946615814,6.64307221372713,-40.7419056738199));
#37931=CARTESIAN_POINT('Ctrl Pts',(-1.45924383473007,6.6100621473246,-40.7337761950368));
#37932=CARTESIAN_POINT('Ctrl Pts',(-1.62800962060493,6.57052777294826,-40.7256467162537));
#37933=CARTESIAN_POINT('Ctrl Pts',(-1.79490365933834,6.52461568628328,-40.7175172374706));
#37934=CARTESIAN_POINT('Ctrl Pts',(-1.96186573783402,6.47868488206861,-40.709384444442));
#37935=CARTESIAN_POINT('Ctrl Pts',(-2.1269541994697,6.42637129332055,-40.7012516514135));
#37936=CARTESIAN_POINT('Ctrl Pts',(-2.28965287835159,6.36787081343963,-40.693118858385));
#37937=CARTESIAN_POINT('Ctrl Pts',(-2.45252846736403,6.30930672316185,-40.6849772221778));
#37938=CARTESIAN_POINT('Ctrl Pts',(-2.61300874453222,6.24454244199253,-40.6768355859707));
#37939=CARTESIAN_POINT('Ctrl Pts',(-2.7705986005475,6.17382153893715,-40.6686939497635));
#37940=CARTESIAN_POINT('Ctrl Pts',(-2.85088849166117,6.13779019942487,-40.664545896703));
#37941=CARTESIAN_POINT('Ctrl Pts',(-2.93042849275127,6.10021339963102,-40.6603978436424));
#37942=CARTESIAN_POINT('Ctrl Pts',(-3.00915580109446,6.06112781293544,-40.6562497905818));
#37943=CARTESIAN_POINT('Ctrl Pts',(-3.16935499840773,5.98159404318106,-40.6478090756037));
#37944=CARTESIAN_POINT('Ctrl Pts',(-3.32651744598031,5.89564638932645,-40.6393683606257));
#37945=CARTESIAN_POINT('Ctrl Pts',(-3.48011514882274,5.80354094936311,-40.6309276456476));
#37946=CARTESIAN_POINT('Ctrl Pts',(-3.63359675528468,5.71150512703081,-40.6224933105596));
#37947=CARTESIAN_POINT('Ctrl Pts',(-3.78351870322428,5.61332096760009,-40.6140589754716));
#37948=CARTESIAN_POINT('Ctrl Pts',(-3.9293773398928,5.50929058234697,-40.6056246403836));
#37949=CARTESIAN_POINT('Ctrl Pts',(-4.07514812799051,5.40532285310705,-40.5971953851749));
#37950=CARTESIAN_POINT('Ctrl Pts',(-4.21686021305799,5.29551611100364,-40.5887661299663));
#37951=CARTESIAN_POINT('Ctrl Pts',(-4.35403836947873,5.18021610332107,-40.5803368747577));
#37952=CARTESIAN_POINT('Ctrl Pts',(-4.49115494755375,5.06496785303138,-40.5719114033847));
#37953=CARTESIAN_POINT('Ctrl Pts',(-4.62374140024711,4.9442314680578,-40.5634859320116));
#37954=CARTESIAN_POINT('Ctrl Pts',(-4.75135477795183,4.81839358853491,-40.5550604606386));
#37955=CARTESIAN_POINT('Ctrl Pts',(-4.8789304294401,4.69259291033971,-40.5466374800794));
#37956=CARTESIAN_POINT('Ctrl Pts',(-5.00153570067214,4.56169397904277,-40.5382144995201));
#37957=CARTESIAN_POINT('Ctrl Pts',(-5.1187634982169,4.42612124204956,-40.5297915189608));
#37958=CARTESIAN_POINT('Ctrl Pts',(-5.23599323681044,4.29054626025347,-40.5213683989345));
#37959=CARTESIAN_POINT('Ctrl Pts',(-5.34784510079353,4.15029756595743,-40.5129452789082));
#37960=CARTESIAN_POINT('Ctrl Pts',(-5.45395096164958,4.00583423370484,-40.5045221588818));
#37961=CARTESIAN_POINT('Ctrl Pts',(-5.56006049182318,3.86136590566939,-40.49609874757));
#37962=CARTESIAN_POINT('Ctrl Pts',(-5.66042342511529,3.71268291776603,-40.4876753362581));
#37963=CARTESIAN_POINT('Ctrl Pts',(-5.7547137287558,3.56027511578383,-40.4792519249463));
#37964=CARTESIAN_POINT('Ctrl Pts',(-5.84902044328238,3.40784078777531,-40.4708270475702));
#37965=CARTESIAN_POINT('Ctrl Pts',(-5.9372522455189,3.25168063678801,-40.462402170194));
#37966=CARTESIAN_POINT('Ctrl Pts',(-6.01912782135925,3.09231131520406,-40.4539772928179));
#37967=CARTESIAN_POINT('Ctrl Pts',(-6.10102906962677,2.9328920227068,-40.4455497737865));
#37968=CARTESIAN_POINT('Ctrl Pts',(-6.17656996561708,2.77026184994147,-40.4371222547551));
#37969=CARTESIAN_POINT('Ctrl Pts',(-6.24551615647476,2.6049600648019,-40.4286947357236));
#37970=CARTESIAN_POINT('Ctrl Pts',(-6.31452417561165,2.43951004341029,-40.4202596592188));
#37971=CARTESIAN_POINT('Ctrl Pts',(-6.37692554434306,2.27138393057703,-40.4118245827141));
#37972=CARTESIAN_POINT('Ctrl Pts',(-6.43253447786483,2.10113997417598,-40.4033895062093));
#37973=CARTESIAN_POINT('Ctrl Pts',(-6.48817028755014,1.93081373775044,-40.3949503529765));
#37974=CARTESIAN_POINT('Ctrl Pts',(-6.53700701903968,1.75836793564562,-40.3865111997438));
#37975=CARTESIAN_POINT('Ctrl Pts',(-6.57890924947765,1.58437435195645,-40.378072046511));
#37976=CARTESIAN_POINT('Ctrl Pts',(-6.62085804504184,1.41018741261292,-40.3696235150129));
#37977=CARTESIAN_POINT('Ctrl Pts',(-6.65585687139404,1.23444958090308,-40.3611749835148));
#37978=CARTESIAN_POINT('Ctrl Pts',(-6.68382151776658,1.05774236874601,-40.3527264520167));
#37979=CARTESIAN_POINT('Ctrl Pts',(-6.6992728922026,0.960105900749617,-40.3480583642507));
#37980=CARTESIAN_POINT('Ctrl Pts',(-6.7125777049321,0.862173597967542,-40.3433902764847));
#37981=CARTESIAN_POINT('Ctrl Pts',(-6.72372856026632,0.76404400911139,-40.3387221887187));
#37982=CARTESIAN_POINT('Ctrl Pts',(-6.74984068517333,0.534252481512515,
-40.327790857698));
#37983=CARTESIAN_POINT('Ctrl Pts',(-6.76418923897398,0.302940342222139,
-40.3168595266774));
#37984=CARTESIAN_POINT('Ctrl Pts',(-6.76662610837283,0.0711344465581041,
-40.3059281956566));
#37985=CARTESIAN_POINT('Ctrl Pts',(-6.76685705737744,0.0491655462588561,
-40.3048922025011));
#37986=CARTESIAN_POINT('Ctrl Pts',(-6.7669810525252,0.027192226654605,-40.3038562093455));
#37987=CARTESIAN_POINT('Ctrl Pts',(-6.76699799023869,0.00521537204463034,
-40.3028202161899));
#37988=CARTESIAN_POINT('',(-6.76699938789274,-0.00287823891704152,-40.6971797837711));
#37989=CARTESIAN_POINT('Ctrl Pts',(3.09908550384719,6.01564277861013,-41.3487246499327));
#37990=CARTESIAN_POINT('Ctrl Pts',(2.94379213113664,6.09564544132176,-41.3405102530541));
#37991=CARTESIAN_POINT('Ctrl Pts',(2.78551219358278,6.16957256320396,-41.3322958561754));
#37992=CARTESIAN_POINT('Ctrl Pts',(2.62476730733514,6.23721777576706,-41.3240814592968));
#37993=CARTESIAN_POINT('Ctrl Pts',(2.46391363966161,6.30490876610169,-41.3158615034618));
#37994=CARTESIAN_POINT('Ctrl Pts',(2.30059203317056,6.36630924838689,-41.3076415476268));
#37995=CARTESIAN_POINT('Ctrl Pts',(2.13533985033291,6.42126254903039,-41.2994215917918));
#37996=CARTESIAN_POINT('Ctrl Pts',(1.96985747544498,6.47629239821157,-41.2911901857692));
#37997=CARTESIAN_POINT('Ctrl Pts',(1.80243949674909,6.52485703144481,-41.2829587797467));
#37998=CARTESIAN_POINT('Ctrl Pts',(1.63363497364204,6.56685052158899,-41.2747273737242));
#37999=CARTESIAN_POINT('Ctrl Pts',(1.57309800053397,6.58191030041944,-41.2717754125098));
#38000=CARTESIAN_POINT('Ctrl Pts',(1.51238276679709,6.59612545097862,-41.2688234512953));
#38001=CARTESIAN_POINT('Ctrl Pts',(1.45151475646385,6.60949271213515,-41.2658714900809));
#38002=CARTESIAN_POINT('Ctrl Pts',(1.28509732268895,6.64603974704051,-41.2578006198945));
#38003=CARTESIAN_POINT('Ctrl Pts',(1.11699479168565,6.67636411374227,-41.2497297497081));
#38004=CARTESIAN_POINT('Ctrl Pts',(0.947723126957648,6.70030670004214,-41.2416588795217));
#38005=CARTESIAN_POINT('Ctrl Pts',(0.778662107659298,6.72421949165436,-41.2335980529059));
#38006=CARTESIAN_POINT('Ctrl Pts',(0.608435214196875,6.74176625316107,-41.2255372262901));
#38007=CARTESIAN_POINT('Ctrl Pts',(0.43757257483463,6.7528378657978,-41.2174763996744));
#38008=CARTESIAN_POINT('Ctrl Pts',(0.266885093176883,6.76389812850888,-41.2094238365145));
#38009=CARTESIAN_POINT('Ctrl Pts',(0.0955635316719927,6.76849642814417,
-41.2013712733546));
#38010=CARTESIAN_POINT('Ctrl Pts',(-0.0758529026689794,6.76657486008665,
-41.1933187101947));
#38011=CARTESIAN_POINT('Ctrl Pts',(-0.247131145431749,6.76465484114853,
-41.1852726388068));
#38012=CARTESIAN_POINT('Ctrl Pts',(-0.418503737707669,6.7562254202622,-41.177226567419));
#38013=CARTESIAN_POINT('Ctrl Pts',(-0.589427581032869,6.74128059990962,
-41.1691804960311));
#38014=CARTESIAN_POINT('Ctrl Pts',(-0.760251017539414,6.72634455868251,
-41.1611391511952));
#38015=CARTESIAN_POINT('Ctrl Pts',(-0.930625859224687,6.70490076964921,
-41.1530978063593));
#38016=CARTESIAN_POINT('Ctrl Pts',(-1.10001034920166,6.67699529965757,-41.1450564615235));
#38017=CARTESIAN_POINT('Ctrl Pts',(-1.27266005094853,6.64855189806975,-41.1368601043024));
#38018=CARTESIAN_POINT('Ctrl Pts',(-1.44428043351158,6.6133951575672,-41.1286637470813));
#38019=CARTESIAN_POINT('Ctrl Pts',(-1.61430422284346,6.57162924061528,-41.1204673898603));
#38020=CARTESIAN_POINT('Ctrl Pts',(-1.7810594387269,6.53066624052421,-41.1124286011518));
#38021=CARTESIAN_POINT('Ctrl Pts',(-1.94627852066613,6.48334598495039,-41.1043898124433));
#38022=CARTESIAN_POINT('Ctrl Pts',(-2.10943796254201,6.42981807535693,-41.0963510237348));
#38023=CARTESIAN_POINT('Ctrl Pts',(-2.27261486395664,6.37628443779209,-41.0883113748031));
#38024=CARTESIAN_POINT('Ctrl Pts',(-2.43373133154001,6.31654193986755,-41.0802717258714));
#38025=CARTESIAN_POINT('Ctrl Pts',(-2.59228067534066,6.25078954215029,-41.0722320769396));
#38026=CARTESIAN_POINT('Ctrl Pts',(-2.7508783787328,6.18501708910503,-41.0641899758115));
#38027=CARTESIAN_POINT('Ctrl Pts',(-2.90690705498651,6.1132312304802,-41.0561478746833));
#38028=CARTESIAN_POINT('Ctrl Pts',(-3.05988172670707,6.03567832298609,-41.0481057735551));
#38029=CARTESIAN_POINT('Ctrl Pts',(-3.21801869257826,5.95550830956053,-41.0397922831104));
#38030=CARTESIAN_POINT('Ctrl Pts',(-3.37289153634586,5.86917540387483,-41.0314787926656));
#38031=CARTESIAN_POINT('Ctrl Pts',(-3.52399495798297,5.77700169085233,-41.0231653022208));
#38032=CARTESIAN_POINT('Ctrl Pts',(-3.67042318741513,5.68767986443805,-41.0151090340501));
#38033=CARTESIAN_POINT('Ctrl Pts',(-3.81331150948368,5.59287354614307,-41.0070527658793));
#38034=CARTESIAN_POINT('Ctrl Pts',(-3.95223250598454,5.49291791479166,-40.9989964977086));
#38035=CARTESIAN_POINT('Ctrl Pts',(-4.09780675195578,5.38817517588919,-40.9905543961268));
#38036=CARTESIAN_POINT('Ctrl Pts',(-4.23902393556588,5.27777806943344,-40.982112294545));
#38037=CARTESIAN_POINT('Ctrl Pts',(-4.37543479113134,5.16215646688063,-40.9736701929633));
#38038=CARTESIAN_POINT('Ctrl Pts',(-4.51184564669678,5.04653486432783,-40.9652280913815));
#38039=CARTESIAN_POINT('Ctrl Pts',(-4.64344989323223,4.92568914108426,-40.9567859897997));
#38040=CARTESIAN_POINT('Ctrl Pts',(-4.76984630227191,4.80008908799649,-40.948343888218));
#38041=CARTESIAN_POINT('Ctrl Pts',(-4.89384004625725,4.67687656205977,-40.940062262259));
#38042=CARTESIAN_POINT('Ctrl Pts',(-5.01322680887011,4.54868741985101,-40.9317806363));
#38043=CARTESIAN_POINT('Ctrl Pts',(-5.12758617826025,4.41589730230612,-40.923499010341));
#38044=CARTESIAN_POINT('Ctrl Pts',(-5.24180727050531,4.28326774736704,-40.9152273980748));
#38045=CARTESIAN_POINT('Ctrl Pts',(-5.35101284864342,4.14604856369751,-40.9069557858086));
#38046=CARTESIAN_POINT('Ctrl Pts',(-5.45481820747363,4.00465320888267,-40.8986841735424));
#38047=CARTESIAN_POINT('Ctrl Pts',(-5.56018478539936,3.86113128632178,-40.8902881573035));
#38048=CARTESIAN_POINT('Ctrl Pts',(-5.6599871194426,3.71330679966699,-40.8818921410647));
#38049=CARTESIAN_POINT('Ctrl Pts',(-5.75386309753849,3.56164968164821,-40.8734961248258));
#38050=CARTESIAN_POINT('Ctrl Pts',(-5.84616337371679,3.41253811805693,-40.8652410351494));
#38051=CARTESIAN_POINT('Ctrl Pts',(-5.93273446191496,3.25972187539894,-40.856985945473));
#38052=CARTESIAN_POINT('Ctrl Pts',(-6.01327397138658,3.10367929159001,-40.8487308557966));
#38053=CARTESIAN_POINT('Ctrl Pts',(-6.09376909491767,2.94772270404419,-40.8404803155633));
#38054=CARTESIAN_POINT('Ctrl Pts',(-6.16823909902925,2.78854363023206,-40.83222977533));
#38055=CARTESIAN_POINT('Ctrl Pts',(-6.23642656767903,2.62664665799326,-40.8239792350968));
#38056=CARTESIAN_POINT('Ctrl Pts',(-6.30458838007217,2.46481060120347,-40.8157317992166));
#38057=CARTESIAN_POINT('Ctrl Pts',(-6.36647222962154,2.30025900876712,-40.8074843633364));
#38058=CARTESIAN_POINT('Ctrl Pts',(-6.42186800614757,2.13351829418411,-40.7992369274562));
#38059=CARTESIAN_POINT('Ctrl Pts',(-6.47899217181178,1.9615751461657,-40.7907321654857));
#38060=CARTESIAN_POINT('Ctrl Pts',(-6.52921667233642,1.78730441239828,-40.7822274035152));
#38061=CARTESIAN_POINT('Ctrl Pts',(-6.57236580696196,1.61130279571447,-40.7737226415447));
#38062=CARTESIAN_POINT('Ctrl Pts',(-6.61420760088614,1.44063370954358,-40.7654755584726));
#38063=CARTESIAN_POINT('Ctrl Pts',(-6.64939645595476,1.26833746207533,-40.7572284754005));
#38064=CARTESIAN_POINT('Ctrl Pts',(-6.67782361408341,1.09497067503655,-40.7489813923285));
#38065=CARTESIAN_POINT('Ctrl Pts',(-6.70758307577842,0.913478658327746,
-40.7403477909088));
#38066=CARTESIAN_POINT('Ctrl Pts',(-6.729931679293,0.730813754679236,-40.731714189489));
#38067=CARTESIAN_POINT('Ctrl Pts',(-6.7448052807437,0.547622794313622,-40.7230805880693));
#38068=CARTESIAN_POINT('Ctrl Pts',(-6.75967888219441,0.364431833948008,
-40.7144469866495));
#38069=CARTESIAN_POINT('Ctrl Pts',(-6.76707747653625,0.180715260589724,
-40.7058133852298));
#38070=CARTESIAN_POINT('Ctrl Pts',(-6.7669993878931,-0.0028782380871501,
-40.6971797838101));
#38071=CARTESIAN_POINT('Ctrl Pts',(-6.76699938789274,-0.00287823891708743,
-40.6971797837711));
#38072=CARTESIAN_POINT('Ctrl Pts',(-6.76689934781463,-0.238081488844765,
-40.6861192008684));
#38073=CARTESIAN_POINT('Ctrl Pts',(-6.75453223181383,-0.47288718151042,
-40.6750586179657));
#38074=CARTESIAN_POINT('Ctrl Pts',(-6.7300487737708,-0.706209956504527,
-40.663998035063));
#38075=CARTESIAN_POINT('Ctrl Pts',(-6.70556531572779,-0.939532731498602,
-40.6529374521603));
#38076=CARTESIAN_POINT('Ctrl Pts',(-6.66896560802827,-1.171372996591,-40.6418768692576));
#38077=CARTESIAN_POINT('Ctrl Pts',(-6.62045521010215,-1.40066477468068,
-40.6308162863549));
#38078=CARTESIAN_POINT('Ctrl Pts',(-6.58339002848412,-1.57585899616201,
-40.6223652628297));
#38079=CARTESIAN_POINT('Ctrl Pts',(-6.53933512208099,-1.74972928296825,
-40.6139142393046));
#38080=CARTESIAN_POINT('Ctrl Pts',(-6.48840239012968,-1.92169805738558,
-40.6054632157794));
#38081=CARTESIAN_POINT('Ctrl Pts',(-6.43751450293511,-2.09351541840799,
-40.5970196331292));
#38082=CARTESIAN_POINT('Ctrl Pts',(-6.37976095408972,-2.2634342877269,-40.5885760504791));
#38083=CARTESIAN_POINT('Ctrl Pts',(-6.31530438439976,-2.43088863018881,
-40.580132467829));
#38084=CARTESIAN_POINT('Ctrl Pts',(-6.25089580463375,-2.59821829767655,
-40.5716951716891));
#38085=CARTESIAN_POINT('Ctrl Pts',(-6.17979427125328,-2.76308678777859,
-40.5632578755493));
#38086=CARTESIAN_POINT('Ctrl Pts',(-6.10221194096156,-2.92494417512304,
-40.5548205794095));
#38087=CARTESIAN_POINT('Ctrl Pts',(-6.02468495974716,-3.08668608956259,
-40.5463893026372));
#38088=CARTESIAN_POINT('Ctrl Pts',(-5.9406865470088,-3.24542088797708,-40.5379580258648));
#38089=CARTESIAN_POINT('Ctrl Pts',(-5.85047664775428,-3.40061935448264,
-40.5295267490925));
#38090=CARTESIAN_POINT('Ctrl Pts',(-5.76030541572793,-3.5557512973077,-40.5210990862705));
#38091=CARTESIAN_POINT('Ctrl Pts',(-5.6639281712108,-3.70734964397582,-40.5126714234486));
#38092=CARTESIAN_POINT('Ctrl Pts',(-5.56165070769398,-3.85490990888336,
-40.5042437606267));
#38093=CARTESIAN_POINT('Ctrl Pts',(-5.45940472922576,-4.00242474890497,
-40.4958186921727));
#38094=CARTESIAN_POINT('Ctrl Pts',(-5.35126234257631,-4.14590371406427,
-40.4873936237187));
#38095=CARTESIAN_POINT('Ctrl Pts',(-5.23757275640213,-4.28487113241392,
-40.4789685552648));
#38096=CARTESIAN_POINT('Ctrl Pts',(-5.20646380567513,-4.32289687175891,
-40.476663198651));
#38097=CARTESIAN_POINT('Ctrl Pts',(-5.17493975894945,-4.36058499186709,
-40.4743578420372));
#38098=CARTESIAN_POINT('Ctrl Pts',(-5.14300831224887,-4.39792615901393,
-40.4720524854234));
#38099=CARTESIAN_POINT('Ctrl Pts',(-5.02362688074474,-4.53753279913351,
-40.4634334968989));
#38100=CARTESIAN_POINT('Ctrl Pts',(-4.89860120089721,-4.6722248909405,-40.4548145083744));
#38101=CARTESIAN_POINT('Ctrl Pts',(-4.7683631396862,-4.80156245071144,-40.4461955198499));
#38102=CARTESIAN_POINT('Ctrl Pts',(-4.63804705425388,-4.93097749522295,
-40.4375713677821));
#38103=CARTESIAN_POINT('Ctrl Pts',(-4.50251257135162,-5.05503139150259,
-40.4289472157144));
#38104=CARTESIAN_POINT('Ctrl Pts',(-4.36222695569932,-5.17332243214844,
-40.4203230636466));
#38105=CARTESIAN_POINT('Ctrl Pts',(-4.21713651997044,-5.29566497275978,
-40.4114035320504));
#38106=CARTESIAN_POINT('Ctrl Pts',(-4.06696401301909,-5.41184268532276,
-40.4024840004541));
#38107=CARTESIAN_POINT('Ctrl Pts',(-3.91226120089767,-5.52145825810091,
-40.3935644688579));
#38108=CARTESIAN_POINT('Ctrl Pts',(-3.76240288314324,-5.62764123636073,
-40.3849242509987));
#38109=CARTESIAN_POINT('Ctrl Pts',(-3.60829397862272,-5.72766671271702,
-40.3762840331394));
#38110=CARTESIAN_POINT('Ctrl Pts',(-3.45046369254555,-5.82121888494368,
-40.3676438152802));
#38111=CARTESIAN_POINT('Ctrl Pts',(-3.28498009823066,-5.91930747174675,
-40.3585846268154));
#38112=CARTESIAN_POINT('Ctrl Pts',(-3.11540558650537,-6.01027917269694,
-40.3495254383507));
#38113=CARTESIAN_POINT('Ctrl Pts',(-2.94237733334475,-6.093825122878,-40.340466249886));
#38114=CARTESIAN_POINT('Ctrl Pts',(-2.76934908018416,-6.17737107305904,
-40.3314070614213));
#38115=CARTESIAN_POINT('Ctrl Pts',(-2.59286745004693,-6.25349115134961,
-40.3223478729566));
#38116=CARTESIAN_POINT('Ctrl Pts',(-2.41359214469936,-6.32193498535421,
-40.3132886844919));
#38117=CARTESIAN_POINT('Ctrl Pts',(-2.23462742124062,-6.39026024521832,
-40.3042451904356));
#38118=CARTESIAN_POINT('Ctrl Pts',(-2.05271412508592,-6.45099957105981,
-40.2952016963793));
#38119=CARTESIAN_POINT('Ctrl Pts',(-1.86848456706522,-6.50392607758107,
-40.2861582023231));
#38120=CARTESIAN_POINT('Ctrl Pts',(-1.68442352314759,-6.55680417242035,
-40.2771229803177));
#38121=CARTESIAN_POINT('Ctrl Pts',(-1.49805067594403,-6.60188364998442,
-40.2680877583124));
#38122=CARTESIAN_POINT('Ctrl Pts',(-1.31001378613239,-6.63898733845329,
-40.2590525363071));
#38123=CARTESIAN_POINT('Ctrl Pts',(-1.1223081763854,-6.67602565830046,-40.2500332323959));
#38124=CARTESIAN_POINT('Ctrl Pts',(-0.932944611511852,-6.7051162023267,
-40.2410139284848));
#38125=CARTESIAN_POINT('Ctrl Pts',(-0.742581174275494,-6.72613278188973,
-40.2319946245737));
#38126=CARTESIAN_POINT('Ctrl Pts',(-0.552456561267698,-6.74712299468572,
-40.2229866360094));
#38127=CARTESIAN_POINT('Ctrl Pts',(-0.361334815213718,-6.76005943167516,
-40.213978647445));
#38128=CARTESIAN_POINT('Ctrl Pts',(-0.169881810109107,-6.76486726925178,
-40.2049706588806));
#38129=CARTESIAN_POINT('Ctrl Pts',(0.0211387916775638,-6.76966424815884,
-40.195983015174));
#38130=CARTESIAN_POINT('Ctrl Pts',(0.212488921545239,-6.76636926738616,
-40.1869953714673));
#38131=CARTESIAN_POINT('Ctrl Pts',(0.40350048950883,-6.75495938958675,-40.1780077277606));
#38132=CARTESIAN_POINT('Ctrl Pts',(0.569858326161454,-6.745022176844,-40.1701801130272));
#38133=CARTESIAN_POINT('Ctrl Pts',(0.735959158018499,-6.7289304173852,-40.1623524982937));
#38134=CARTESIAN_POINT('Ctrl Pts',(0.901359588940868,-6.7067011183908,-40.1545248835603));
#38135=CARTESIAN_POINT('Ctrl Pts',(1.0730049691823,-6.6836325178006,-40.146401725115));
#38136=CARTESIAN_POINT('Ctrl Pts',(1.24381911066791,-6.65396281728191,-40.1382785666697));
#38137=CARTESIAN_POINT('Ctrl Pts',(1.41325603536892,-6.61777881003085,-40.1301554082244));
#38138=CARTESIAN_POINT('Ctrl Pts',(1.58268101387985,-6.5815973539417,-40.1220328225043));
#38139=CARTESIAN_POINT('Ctrl Pts',(1.75072861106866,-6.53890258242891,-40.1139102367842));
#38140=CARTESIAN_POINT('Ctrl Pts',(1.91686338505769,-6.48983233705041,-40.1057876510641));
#38141=CARTESIAN_POINT('Ctrl Pts',(2.08301812184995,-6.44075619537681,-40.0976640893317));
#38142=CARTESIAN_POINT('Ctrl Pts',(2.24725922708082,-6.38530315922434,-40.0895405275993));
#38143=CARTESIAN_POINT('Ctrl Pts',(2.40906680035588,-6.32366081881556,-40.0814169658669));
#38144=CARTESIAN_POINT('Ctrl Pts',(2.57099223124696,-6.26197357927667,-40.0732874870838));
#38145=CARTESIAN_POINT('Ctrl Pts',(2.73048024756321,-6.19408816191164,-40.0651580083007));
#38146=CARTESIAN_POINT('Ctrl Pts',(2.88703071563051,-6.12024040761521,-40.0570285295176));
#38147=CARTESIAN_POINT('Ctrl Pts',(3.04364500656834,-6.04636254688909,-40.048895736489));
#38148=CARTESIAN_POINT('Ctrl Pts',(3.19731903754234,-5.96651767268191,-40.0407629434605));
#38149=CARTESIAN_POINT('Ctrl Pts',(3.34757787426296,-5.88098727899875,-40.032630150432));
#38150=CARTESIAN_POINT('Ctrl Pts',(3.49800009467293,-5.79536388398817,-40.0244885142248));
#38151=CARTESIAN_POINT('Ctrl Pts',(3.64499939324817,-5.70404281471206,-40.0163468780177));
#38152=CARTESIAN_POINT('Ctrl Pts',(3.78812975489722,-5.60734892440825,-40.0082052418105));
#38153=CARTESIAN_POINT('Ctrl Pts',(3.86105273003296,-5.55808470068126,-40.00405718875));
#38154=CARTESIAN_POINT('Ctrl Pts',(3.93297193626112,-5.50742647892359,-39.9999091356894));
#38155=CARTESIAN_POINT('Ctrl Pts',(4.0038317888937,-5.45542115755001,-39.9957610826288));
#38156=CARTESIAN_POINT('Ctrl Pts',(4.14802180062394,-5.34959751242089,-39.9873203676508));
#38157=CARTESIAN_POINT('Ctrl Pts',(4.28812031183531,-5.23797564500015,-39.9788796526727));
#38158=CARTESIAN_POINT('Ctrl Pts',(4.42365105696813,-5.12089839053508,-39.9704389376946));
#38159=CARTESIAN_POINT('Ctrl Pts',(4.55907936157832,-5.00390962857496,-39.9620046026066));
#38160=CARTESIAN_POINT('Ctrl Pts',(4.68994653111973,-4.88147391657323,-39.9535702675186));
#38161=CARTESIAN_POINT('Ctrl Pts',(4.81580817120893,-4.75397524794958,-39.9451359324305));
#38162=CARTESIAN_POINT('Ctrl Pts',(4.94159400663235,-4.6265533699506,-39.9367066772219));
#38163=CARTESIAN_POINT('Ctrl Pts',(5.0623800893322,-4.49407485134633,-39.9282774220133));
#38164=CARTESIAN_POINT('Ctrl Pts',(5.17775751289374,-4.35696180126387,-39.9198481668047));
#38165=CARTESIAN_POINT('Ctrl Pts',(5.29308314431078,-4.21991030030153,-39.9114226954317));
#38166=CARTESIAN_POINT('Ctrl Pts',(5.40300474327351,-4.07822867066769,-39.9029972240586));
#38167=CARTESIAN_POINT('Ctrl Pts',(5.50715221287519,-3.93237377473505,-39.8945717526856));
#38168=CARTESIAN_POINT('Ctrl Pts',(5.61126889346346,-3.78656199774099,-39.8861487721264));
#38169=CARTESIAN_POINT('Ctrl Pts',(5.70961465529431,-3.63657968585611,-39.8777257915671));
#38170=CARTESIAN_POINT('Ctrl Pts',(5.8018612090653,-3.48291480095959,-39.8693028110079));
#38171=CARTESIAN_POINT('Ctrl Pts',(5.89410929024782,-3.3292473716914,-39.8608796909816));
#38172=CARTESIAN_POINT('Ctrl Pts',(5.98025778436389,-3.17189752996982,-39.8524565709552));
#38173=CARTESIAN_POINT('Ctrl Pts',(6.06002272715309,-3.01138067111883,-39.8440334509289));
#38174=CARTESIAN_POINT('Ctrl Pts',(6.13979042834697,-2.85085826132728,-39.835610039617));
#38175=CARTESIAN_POINT('Ctrl Pts',(6.21317398949544,-2.68716891462428,-39.8271866283052));
#38176=CARTESIAN_POINT('Ctrl Pts',(6.27993619471869,-2.52085112417655,-39.8187632169933));
#38177=CARTESIAN_POINT('Ctrl Pts',(6.34671001966215,-2.35450438671927,-39.8103383396172));
#38178=CARTESIAN_POINT('Ctrl Pts',(6.40686006685966,-2.18552860293806,-39.8019134622411));
#38179=CARTESIAN_POINT('Ctrl Pts',(6.46019777310973,-2.01448100817756,-39.793488584865));
#38180=CARTESIAN_POINT('Ctrl Pts',(6.51355220361928,-1.84337978073281,-39.7850610658335));
#38181=CARTESIAN_POINT('Ctrl Pts',(6.56008993526042,-1.67020576537716,-39.7766335468021));
#38182=CARTESIAN_POINT('Ctrl Pts',(6.5996725482858,-1.495530426104,-39.7682060277707));
#38183=CARTESIAN_POINT('Ctrl Pts',(6.63929065746871,-1.32069844473765,-39.7597709512659));
#38184=CARTESIAN_POINT('Ctrl Pts',(6.67194111167981,-1.14436277484692,-39.7513358747611));
#38185=CARTESIAN_POINT('Ctrl Pts',(6.69753659428511,-0.967105251878937,
-39.7429007982563));
#38186=CARTESIAN_POINT('Ctrl Pts',(6.72314444735561,-0.789762059183462,
-39.7344616450235));
#38187=CARTESIAN_POINT('Ctrl Pts',(6.74169048893664,-0.611496455804941,
-39.7260224917908));
#38188=CARTESIAN_POINT('Ctrl Pts',(6.75313933945475,-0.432894977920331,
-39.717583338558));
#38189=CARTESIAN_POINT('Ctrl Pts',(6.76460091285572,-0.254095023719107,
-39.7091348070599));
#38190=CARTESIAN_POINT('Ctrl Pts',(6.7689495227256,-0.0749587824602956,
-39.7006862755618));
#38191=CARTESIAN_POINT('Ctrl Pts',(6.76620191111585,0.103926406712928,-39.6922377440637));
#38192=CARTESIAN_POINT('Ctrl Pts',(6.76468376655499,0.202766277674943,-39.6875696562977));
#38193=CARTESIAN_POINT('Ctrl Pts',(6.76100012467404,0.30152955400974,-39.6829015685317));
#38194=CARTESIAN_POINT('Ctrl Pts',(6.75516059642078,0.400117878336026,-39.6782334807658));
#38195=CARTESIAN_POINT('Ctrl Pts',(6.74485182667636,0.574160076761794,-39.669992705169));
#38196=CARTESIAN_POINT('Ctrl Pts',(6.72779840754416,0.748043914453889,-39.6617519295723));
#38197=CARTESIAN_POINT('Ctrl Pts',(6.70400359479417,0.921208337449707,-39.6535111539755));
#38198=CARTESIAN_POINT('Ctrl Pts',(6.68023513737897,1.09418096207374,-39.6452795059311));
#38199=CARTESIAN_POINT('Ctrl Pts',(6.64974020216558,1.2664354092589,-39.6370478578868));
#38200=CARTESIAN_POINT('Ctrl Pts',(6.61257401127576,1.43741223919948,-39.6288162098424));
#38201=CARTESIAN_POINT('Ctrl Pts',(6.5754423626094,1.60823016343237,-39.6205922122841));
#38202=CARTESIAN_POINT('Ctrl Pts',(6.53165188141004,1.77777248957256,-39.6123682147258));
#38203=CARTESIAN_POINT('Ctrl Pts',(6.48130940631116,1.94548641209917,-39.6041442171676));
#38204=CARTESIAN_POINT('Ctrl Pts',(6.43101140898456,2.11305215872381,-39.5959274855431));
#38205=CARTESIAN_POINT('Ctrl Pts',(6.37417305716934,2.27879238193669,-39.5877107539186));
#38206=CARTESIAN_POINT('Ctrl Pts',(6.31095189393438,2.44216608617147,-39.5794940222941));
#38207=CARTESIAN_POINT('Ctrl Pts',(6.2477631212419,2.60545608800921,-39.5712815004054));
#38208=CARTESIAN_POINT('Ctrl Pts',(6.17819817806482,2.76638165460895,-39.5630689785167));
#38209=CARTESIAN_POINT('Ctrl Pts',(6.10246405710077,2.92441813559437,-39.554856456628));
#38210=CARTESIAN_POINT('Ctrl Pts',(6.02675526199128,3.08240176841991,-39.5466466810461));
#38211=CARTESIAN_POINT('Ctrl Pts',(5.94488155242803,3.23749791976992,-39.5384369054643));
#38212=CARTESIAN_POINT('Ctrl Pts',(5.85709758374302,3.38920298809495,-39.5302271298824));
#38213=CARTESIAN_POINT('Ctrl Pts',(5.81875582686446,3.45546382061478,-39.5266413131997));
#38214=CARTESIAN_POINT('Ctrl Pts',(5.77928716420472,3.52107802441721,-39.523055496517));
#38215=CARTESIAN_POINT('Ctrl Pts',(5.73871556846833,3.5860051065523,-39.5194696798343));
#38216=CARTESIAN_POINT('Ctrl Pts',(5.63848392311761,3.74640669175261,-39.5106109623125));
#38217=CARTESIAN_POINT('Ctrl Pts',(5.53162178112995,3.90244658083081,-39.5017522447907));
#38218=CARTESIAN_POINT('Ctrl Pts',(5.41853445131823,4.05361238895353,-39.492893527269));
#38219=CARTESIAN_POINT('Ctrl Pts',(5.30523555327521,4.20506100402473,-39.4840182365095));
#38220=CARTESIAN_POINT('Ctrl Pts',(5.18568834837483,4.35161710752813,-39.4751429457501));
#38221=CARTESIAN_POINT('Ctrl Pts',(5.06033754288159,4.49280234954791,-39.4662676549906));
#38222=CARTESIAN_POINT('Ctrl Pts',(4.9346307129163,4.63438858939973,-39.4573671564098));
#38223=CARTESIAN_POINT('Ctrl Pts',(4.80308747005726,4.77057324658558,-39.448466657829));
#38224=CARTESIAN_POINT('Ctrl Pts',(4.66619063681407,4.90091358227307,-39.4395661592483));
#38225=CARTESIAN_POINT('Ctrl Pts',(4.52910848614448,5.03143035984746,-39.4306536120506));
#38226=CARTESIAN_POINT('Ctrl Pts',(4.38665846077222,5.15608683824668,-39.421741064853));
#38227=CARTESIAN_POINT('Ctrl Pts',(4.23935652569372,5.27448056665849,-39.4128285176554));
#38228=CARTESIAN_POINT('Ctrl Pts',(4.09172933355657,5.39313571998537,-39.4038962906831));
#38229=CARTESIAN_POINT('Ctrl Pts',(3.93922900593053,5.50550030037312,-39.3949640637109));
#38230=CARTESIAN_POINT('Ctrl Pts',(3.78240289183726,5.61121353753546,-39.3860318367386));
#38231=CARTESIAN_POINT('Ctrl Pts',(3.63418410439051,5.71112475397963,-39.3775898507933));
#38232=CARTESIAN_POINT('Ctrl Pts',(3.48210172969147,5.80509498490515,-39.3691478648481));
#38233=CARTESIAN_POINT('Ctrl Pts',(3.32663794447754,5.89285745511991,-39.3607058789028));
#38234=CARTESIAN_POINT('Ctrl Pts',(3.25162616590813,5.93520313050273,-39.3566325934135));
#38235=CARTESIAN_POINT('Ctrl Pts',(3.17575653689587,5.97614407567335,-39.3525593079243));
#38236=CARTESIAN_POINT('Ctrl Pts',(3.09908550384721,6.01564277861012,-39.3484860224351));
#38237=CARTESIAN_POINT('Origin',(0.,0.,-63.6971797838103));
#38238=CARTESIAN_POINT('',(3.09908550384718,6.01564277861013,-36.9542436419538));
#38239=CARTESIAN_POINT('',(3.09908550384721,6.01564277861012,-37.3484709211108));
#38240=CARTESIAN_POINT('',(3.09908550384721,6.01564277861012,-63.6971797838103));
#38241=CARTESIAN_POINT('',(-6.767,6.39834729252928E-13,-38.30282021619));
#38242=CARTESIAN_POINT('Ctrl Pts',(-6.767,6.39834728801335E-13,-38.30282021619));
#38243=CARTESIAN_POINT('Ctrl Pts',(-6.76700000000002,-0.186007249559384,
-38.2940707043773));
#38244=CARTESIAN_POINT('Ctrl Pts',(-6.7593263729425,-0.372014355815586,
-38.2853211925645));
#38245=CARTESIAN_POINT('Ctrl Pts',(-6.74400518263366,-0.557389537585977,
-38.2765716807518));
#38246=CARTESIAN_POINT('Ctrl Pts',(-6.72868405703732,-0.742763936382592,
-38.2678222058946));
#38247=CARTESIAN_POINT('Ctrl Pts',(-6.70571545643564,-0.927506130405041,
-38.2590727310374));
#38248=CARTESIAN_POINT('Ctrl Pts',(-6.67517739401571,-1.1109886400957,-38.2503232561802));
#38249=CARTESIAN_POINT('Ctrl Pts',(-6.64463945804385,-1.29447039004563,
-38.2415738175516));
#38250=CARTESIAN_POINT('Ctrl Pts',(-6.6065321700272,-1.47669218339296,-38.2328243789231));
#38251=CARTESIAN_POINT('Ctrl Pts',(-6.56098496085476,-1.65703510627798,
-38.2240749402946));
#38252=CARTESIAN_POINT('Ctrl Pts',(-6.51543793649547,-1.83737729740044,
-38.215325537168));
#38253=CARTESIAN_POINT('Ctrl Pts',(-6.4624511215688,-2.01584035545007,-38.2065761340413));
#38254=CARTESIAN_POINT('Ctrl Pts',(-6.40220448361692,-2.19181813797483,
-38.1978267309147));
#38255=CARTESIAN_POINT('Ctrl Pts',(-6.34195808511945,-2.36779522106378,
-38.1890773625632));
#38256=CARTESIAN_POINT('Ctrl Pts',(-6.27445201416324,-2.54128677725819,
-38.1803279942116));
#38257=CARTESIAN_POINT('Ctrl Pts',(-6.19991555052691,-2.71170355428734,
-38.1715786258601));
#38258=CARTESIAN_POINT('Ctrl Pts',(-6.12537937695073,-2.88211966813618,
-38.1628292915569));
#38259=CARTESIAN_POINT('Ctrl Pts',(-6.04381298028288,-3.04946076419995,
-38.1540799572537));
#38260=CARTESIAN_POINT('Ctrl Pts',(-5.95549339308798,-3.21315848424652,
-38.1453306229505));
#38261=CARTESIAN_POINT('Ctrl Pts',(-5.86717414225611,-3.37685558085427,
-38.136581321969));
#38262=CARTESIAN_POINT('Ctrl Pts',(-5.77210188843852,-3.5369090770035,-38.1278320209874));
#38263=CARTESIAN_POINT('Ctrl Pts',(-5.67059953311141,-3.69277537024345,
-38.1190827200058));
#38264=CARTESIAN_POINT('Ctrl Pts',(-5.56909755592451,-3.84864108281398,
-38.1103334516192));
#38265=CARTESIAN_POINT('Ctrl Pts',(-5.46116568154682,-4.00031938355217,
-38.1015841832326));
#38266=CARTESIAN_POINT('Ctrl Pts',(-5.34717048488064,-4.14729511918567,
-38.092834914846));
#38267=CARTESIAN_POINT('Ctrl Pts',(-5.23317570342969,-4.29427031947589,
-38.0840856783276));
#38268=CARTESIAN_POINT('Ctrl Pts',(-5.11311781951186,-4.43654276249972,
-38.0753364418092));
#38269=CARTESIAN_POINT('Ctrl Pts',(-4.98740458928858,-4.57362924412804,
-38.0665872052909));
#38270=CARTESIAN_POINT('Ctrl Pts',(-4.86169180652326,-4.71071523781696,
-38.0578379999142));
#38271=CARTESIAN_POINT('Ctrl Pts',(-4.73032391141129,-4.84261509584923,
-38.0490887945374));
#38272=CARTESIAN_POINT('Ctrl Pts',(-4.59374706946854,-4.96888084600036,
-38.0403395891607));
#38273=CARTESIAN_POINT('Ctrl Pts',(-4.45717070231063,-5.0951461572113,-38.031590414199));
#38274=CARTESIAN_POINT('Ctrl Pts',(-4.31538563496948,-5.21577720520924,
-38.0228412392373));
#38275=CARTESIAN_POINT('Ctrl Pts',(-4.1688734095166,-5.33036429293772,-38.0140920642756));
#38276=CARTESIAN_POINT('Ctrl Pts',(-4.02236168122134,-5.44495099183965,
-38.0053429190024));
#38277=CARTESIAN_POINT('Ctrl Pts',(-3.87112305262826,-5.55349359498176,
-37.9965937737292));
#38278=CARTESIAN_POINT('Ctrl Pts',(-3.71567116928637,-5.65562346357447,
-37.9878446284559));
#38279=CARTESIAN_POINT('Ctrl Pts',(-3.56021980052937,-5.75775299409159,
-37.9790955121445));
#38280=CARTESIAN_POINT('Ctrl Pts',(-3.40055544441694,-5.85346967520106,
-37.9703463958331));
#38281=CARTESIAN_POINT('Ctrl Pts',(-3.23722035886438,-5.94244843041603,
-37.9615972795218));
#38282=CARTESIAN_POINT('Ctrl Pts',(-3.07388580043084,-6.03142689847658,
-37.9528481914458));
#38283=CARTESIAN_POINT('Ctrl Pts',(-2.90688078788816,-6.11366734708095,
-37.9440991033697));
#38284=CARTESIAN_POINT('Ctrl Pts',(-2.73677250609987,-6.18889047001608,
-37.9353500152937));
#38285=CARTESIAN_POINT('Ctrl Pts',(-2.56666475916546,-6.26411335643492,
-37.9266009547266));
#38286=CARTESIAN_POINT('Ctrl Pts',(-2.39345402456724,-6.33231884545395,
-37.9178518941594));
#38287=CARTESIAN_POINT('Ctrl Pts',(-2.21772855943716,-6.39327529805004,
-37.9091028335923));
#38288=CARTESIAN_POINT('Ctrl Pts',(-2.04200363223247,-6.45423156404811,
-37.9003537998075));
#38289=CARTESIAN_POINT('Ctrl Pts',(-1.86376426060696,-6.5079387441255,-37.8916047660227));
#38290=CARTESIAN_POINT('Ctrl Pts',(-1.68361577621356,-6.55421443943398,
-37.8828557322379));
#38291=CARTESIAN_POINT('Ctrl Pts',(-1.50346782832887,-6.60048999692662,
-37.874106724509));
#38292=CARTESIAN_POINT('Ctrl Pts',(-1.32141105657063,-6.63933404265226,
-37.8653577167801));
#38293=CARTESIAN_POINT('Ctrl Pts',(-1.13806375346216,-6.67061465631584,
-37.8566087090512));
#38294=CARTESIAN_POINT('Ctrl Pts',(-0.954716981166758,-6.70189517941817,
-37.8478597266518));
#38295=CARTESIAN_POINT('Ctrl Pts',(-0.770079967438979,-6.72561226609042,
-37.8391107442523));
#38296=CARTESIAN_POINT('Ctrl Pts',(-0.584779764069715,-6.74168536996014,
-37.8303617618529));
#38297=CARTESIAN_POINT('Ctrl Pts',(-0.391489587589589,-6.75845153117892,
-37.8212355314373));
#38298=CARTESIAN_POINT('Ctrl Pts',(-0.197478091801861,-6.76689985146404,
-37.8121093010217));
#38299=CARTESIAN_POINT('Ctrl Pts',(-0.00346214752765282,-6.76699911434415,
-37.802983070606));
#38300=CARTESIAN_POINT('Ctrl Pts',(0.184490798488006,-6.76709527525926,
-37.7941420348909));
#38301=CARTESIAN_POINT('Ctrl Pts',(0.372447602158131,-6.75935633790745,
-37.7853009991758));
#38302=CARTESIAN_POINT('Ctrl Pts',(0.559756448197546,-6.74380914014485,
-37.7764599634607));
#38303=CARTESIAN_POINT('Ctrl Pts',(0.745136131046712,-6.72842206873117,
-37.7677099848474));
#38304=CARTESIAN_POINT('Ctrl Pts',(0.929880851948416,-6.70538686355677,
-37.758960006234));
#38305=CARTESIAN_POINT('Ctrl Pts',(1.11336305057802,-6.67478177303256,-37.7502100276207));
#38306=CARTESIAN_POINT('Ctrl Pts',(1.2968433709046,-6.64417699581195,-37.7414601385807));
#38307=CARTESIAN_POINT('Ctrl Pts',(1.47906091205525,-6.60600253547985,-37.7327102495408));
#38308=CARTESIAN_POINT('Ctrl Pts',(1.65939671095554,-6.56038806441128,-37.7239603605008));
#38309=CARTESIAN_POINT('Ctrl Pts',(1.83973072369499,-6.51477404513754,-37.7152105581253));
#38310=CARTESIAN_POINT('Ctrl Pts',(2.0181827535738,-6.46172023288554,-37.7064607557498));
#38311=CARTESIAN_POINT('Ctrl Pts',(2.19414664033674,-6.40140683917988,-37.6977109533743));
#38312=CARTESIAN_POINT('Ctrl Pts',(2.370108842716,-6.3410940228137,-37.6889612347548));
#38313=CARTESIAN_POINT('Ctrl Pts',(2.5435826784814,-6.27352185699656,-37.6802115161352));
#38314=CARTESIAN_POINT('Ctrl Pts',(2.71397890842068,-6.19891986435119,-37.6714617975157));
#38315=CARTESIAN_POINT('Ctrl Pts',(2.88437356389272,-6.12431856103088,-37.6627121597439));
#38316=CARTESIAN_POINT('Ctrl Pts',(3.05169040787505,-6.04268767582389,-37.653962521972));
#38317=CARTESIAN_POINT('Ctrl Pts',(3.21536112512389,-5.95430447953764,-37.6452128842002));
#38318=CARTESIAN_POINT('Ctrl Pts',(3.37903038443164,-5.86592207054857,-37.6364633243682));
#38319=CARTESIAN_POINT('Ctrl Pts',(3.5390533298028,-5.77078760703188,-37.6277137645361));
#38320=CARTESIAN_POINT('Ctrl Pts',(3.69488643042185,-5.66922422085108,-37.618964204704));
#38321=CARTESIAN_POINT('Ctrl Pts',(3.85071819469032,-5.56766170562958,-37.610214719904));
#38322=CARTESIAN_POINT('Ctrl Pts',(4.0023599459951,-5.45967053456042,-37.6014652351041));
#38323=CARTESIAN_POINT('Ctrl Pts',(4.14929662974583,-5.34561750206465,-37.5927157503041));
#38324=CARTESIAN_POINT('Ctrl Pts',(4.29623210225319,-5.2315654097424,-37.5839663376287));
#38325=CARTESIAN_POINT('Ctrl Pts',(4.43846235842385,-5.11145173171954,-37.5752169249533));
#38326=CARTESIAN_POINT('Ctrl Pts',(4.57550431797689,-4.98568443006322,-37.566467512278));
#38327=CARTESIAN_POINT('Ctrl Pts',(4.71254519337751,-4.85991812336441,-37.5577181688201));
#38328=CARTESIAN_POINT('Ctrl Pts',(4.84439764315236,-4.72849847630843,-37.5489688253622));
#38329=CARTESIAN_POINT('Ctrl Pts',(4.97061384196934,-4.59187184425076,-37.5402194819043));
#38330=CARTESIAN_POINT('Ctrl Pts',(5.09682908420447,-4.45524624767472,-37.5314702047569));
#38331=CARTESIAN_POINT('Ctrl Pts',(5.21740796650404,-4.3134139555661,-37.5227209276096));
#38332=CARTESIAN_POINT('Ctrl Pts',(5.33194095942477,-4.16685668162567,-37.5139716504622));
#38333=CARTESIAN_POINT('Ctrl Pts',(5.44647312235358,-4.02030046974909,-37.5052224367187));
#38334=CARTESIAN_POINT('Ctrl Pts',(5.55495930712513,-3.86901957035225,-37.4964732229751));
#38335=CARTESIAN_POINT('Ctrl Pts',(5.65703106080017,-3.71352778058036,-37.4877240092316));
#38336=CARTESIAN_POINT('Ctrl Pts',(5.75910210868956,-3.55803706597247,-37.4789748559854));
#38337=CARTESIAN_POINT('Ctrl Pts',(5.85475865698766,-3.39833575880526,-37.4702257027392));
#38338=CARTESIAN_POINT('Ctrl Pts',(5.94367583069276,-3.23496624706329,-37.461476549493));
#38339=CARTESIAN_POINT('Ctrl Pts',(6.03259241910284,-3.07159781069694,-37.4527274538378));
#38340=CARTESIAN_POINT('Ctrl Pts',(6.11476958471167,-2.90456146975415,-37.4439783581827));
#38341=CARTESIAN_POINT('Ctrl Pts',(6.18992823574577,-2.73442451647825,-37.4352292625276));
#38342=CARTESIAN_POINT('Ctrl Pts',(6.26508641701117,-2.56428862661971,-37.4264802215575));
#38343=CARTESIAN_POINT('Ctrl Pts',(6.33322605570469,-2.3910524253082,-37.4177311805873));
#38344=CARTESIAN_POINT('Ctrl Pts',(6.3941157374793,-2.21530425353259,-37.4089821396172));
#38345=CARTESIAN_POINT('Ctrl Pts',(6.45500505889272,-2.03955712188095,-37.4002331504262));
#38346=CARTESIAN_POINT('Ctrl Pts',(6.50864441545061,-1.86129832025111,-37.3914841612352));
#38347=CARTESIAN_POINT('Ctrl Pts',(6.55485164050023,-1.68113324011853,-37.3827351720442));
#38348=CARTESIAN_POINT('Ctrl Pts',(6.60199852639213,-1.49730435912441,-37.3738082651674));
#38349=CARTESIAN_POINT('Ctrl Pts',(6.641407674411,-1.31149113173193,-37.3648813582905));
#38350=CARTESIAN_POINT('Ctrl Pts',(6.67293975269679,-1.12435050445973,-37.3559544514136));
#38351=CARTESIAN_POINT('Ctrl Pts',(6.70384664831571,-0.940920291559148,
-37.3472045372296));
#38352=CARTESIAN_POINT('Ctrl Pts',(6.72718585889718,-0.756215114273333,
-37.3384546230456));
#38353=CARTESIAN_POINT('Ctrl Pts',(6.74287810451903,-0.570862389370528,
-37.3297047088616));
#38354=CARTESIAN_POINT('Ctrl Pts',(6.75857004154149,-0.385513309563553,
-37.320954966751));
#38355=CARTESIAN_POINT('Ctrl Pts',(6.76661529035569,-0.199516993254733,
-37.3122052246405));
#38356=CARTESIAN_POINT('Ctrl Pts',(6.76698652348897,-0.0135052182006522,
-37.3034554825299));
#38357=CARTESIAN_POINT('Ctrl Pts',(6.76735774981513,0.172503146042231,-37.2947059008592));
#38358=CARTESIAN_POINT('Ctrl Pts',(6.76005524147462,0.358526681836741,-37.2859563191886));
#38359=CARTESIAN_POINT('Ctrl Pts',(6.74510380214856,0.543933542118062,-37.2772067375179));
#38360=CARTESIAN_POINT('Ctrl Pts',(6.73015261710945,0.729337249087885,-37.268457304656));
#38361=CARTESIAN_POINT('Ctrl Pts',(6.70755278444563,0.914124015857789,-37.2597078717941));
#38362=CARTESIAN_POINT('Ctrl Pts',(6.67738106408238,1.09766621749694,-37.2509584389322));
#38363=CARTESIAN_POINT('Ctrl Pts',(6.64720981677196,1.2812055414362,-37.2422091432498));
#38364=CARTESIAN_POINT('Ctrl Pts',(6.60946696581459,1.46350005650908,-37.2334598475675));
#38365=CARTESIAN_POINT('Ctrl Pts',(6.56428070010925,1.64393062206811,-37.2247105518851));
#38366=CARTESIAN_POINT('Ctrl Pts',(6.51909508282663,1.82435859844928,-37.2159613817552));
#38367=CARTESIAN_POINT('Ctrl Pts',(6.46646633415577,2.00292240086837,-37.2072122116251));
#38368=CARTESIAN_POINT('Ctrl Pts',(6.406573195971,2.17901557696726,-37.1984630414952));
#38369=CARTESIAN_POINT('Ctrl Pts',(6.34668083768194,2.35510646007706,-37.1897139852921));
#38370=CARTESIAN_POINT('Ctrl Pts',(6.27952437143776,2.52872650996801,-37.180964929089));
#38371=CARTESIAN_POINT('Ctrl Pts',(6.20533187335019,2.69928607998195,-37.1722158728859));
#38372=CARTESIAN_POINT('Ctrl Pts',(6.12831449784133,2.87633970115651,-37.1631336965971));
#38373=CARTESIAN_POINT('Ctrl Pts',(6.04371489463032,3.05009490562587,-37.1540515203083));
#38374=CARTESIAN_POINT('Ctrl Pts',(5.9518426512037,3.21991584599854,-37.1449693440194));
#38375=CARTESIAN_POINT('Ctrl Pts',(5.86333281335362,3.38352155905526,-37.136219563665));
#38376=CARTESIAN_POINT('Ctrl Pts',(5.76807337235546,3.54347560904051,-37.1274697833106));
#38377=CARTESIAN_POINT('Ctrl Pts',(5.66638790086206,3.69923467178875,-37.1187200029562));
#38378=CARTESIAN_POINT('Ctrl Pts',(5.56470608502585,3.85498813489992,-37.1099705371619));
#38379=CARTESIAN_POINT('Ctrl Pts',(5.45659885766785,4.00654667256488,-37.1012210713676));
#38380=CARTESIAN_POINT('Ctrl Pts',(5.34243340580332,4.15339551506437,-37.0924716055734));
#38381=CARTESIAN_POINT('Ctrl Pts',(5.22827145140408,4.30023985884096,-37.0837224078195));
#38382=CARTESIAN_POINT('Ctrl Pts',(5.10805181977893,4.44237456993268,-37.0749732100656));
#38383=CARTESIAN_POINT('Ctrl Pts',(4.98218281282345,4.57931691626673,-37.0662240123117));
#38384=CARTESIAN_POINT('Ctrl Pts',(4.85631699296016,4.71625579512381,-37.0574750360937));
#38385=CARTESIAN_POINT('Ctrl Pts',(4.72480227791618,4.84800236135984,-37.0487260598757));
#38386=CARTESIAN_POINT('Ctrl Pts',(4.58808530847887,4.97410918679117,-37.0399770836577));
#38387=CARTESIAN_POINT('Ctrl Pts',(4.45135945056731,5.10022421089218,-37.0312275386365));
#38388=CARTESIAN_POINT('Ctrl Pts',(4.30943087207787,5.22069856612195,-37.0224779936153));
#38389=CARTESIAN_POINT('Ctrl Pts',(4.16278164322201,5.33512305301891,-37.0137284485941));
#38390=CARTESIAN_POINT('Ctrl Pts',(4.01614103534133,5.44954081331616,-37.0049794179269));
#38391=CARTESIAN_POINT('Ctrl Pts',(3.86478055833165,5.55790924068509,-36.9962303872596));
#38392=CARTESIAN_POINT('Ctrl Pts',(3.70921425811715,5.65986029751446,-36.9874813565924));
#38393=CARTESIAN_POINT('Ctrl Pts',(3.55364584529888,5.76181273884797,-36.9787322071125));
#38394=CARTESIAN_POINT('Ctrl Pts',(3.39387173464118,5.85734747818194,-36.9699830576327));
#38395=CARTESIAN_POINT('Ctrl Pts',(3.23043456092184,5.94614005448928,-36.9612339081528));
#38396=CARTESIAN_POINT('Ctrl Pts',(3.18690768806243,5.9697874481136,-36.9589038194198));
#38397=CARTESIAN_POINT('Ctrl Pts',(3.14312114982806,5.99295688499339,-36.9565737306868));
#38398=CARTESIAN_POINT('Ctrl Pts',(3.09908550384719,6.01564277861013,-36.9542436419538));
#38399=CARTESIAN_POINT('Ctrl Pts',(3.0990855038472,6.01564277861013,-38.9542099095282));
#38400=CARTESIAN_POINT('Ctrl Pts',(2.93954625881631,6.0978327921741,-38.9457836090008));
#38401=CARTESIAN_POINT('Ctrl Pts',(2.77668881039921,6.1736963075324,-38.9373573084735));
#38402=CARTESIAN_POINT('Ctrl Pts',(2.61104376445001,6.24297520899504,-38.9289310079462));
#38403=CARTESIAN_POINT('Ctrl Pts',(2.48599841881969,6.29527381007088,-38.9225699987425));
#38404=CARTESIAN_POINT('Ctrl Pts',(2.35936505171891,6.34382093289626,-38.9162089895389));
#38405=CARTESIAN_POINT('Ctrl Pts',(2.23138005412037,6.38852346431269,-38.9098479803352));
#38406=CARTESIAN_POINT('Ctrl Pts',(2.05796398281955,6.44909413682038,-38.9012289918107));
#38407=CARTESIAN_POINT('Ctrl Pts',(1.88214334099229,6.50257761206384,-38.8926100032862));
#38408=CARTESIAN_POINT('Ctrl Pts',(1.70451273536023,6.5488109863543,-38.8839910147617));
#38409=CARTESIAN_POINT('Ctrl Pts',(1.52677571314328,6.59507205856192,-38.8753668626939));
#38410=CARTESIAN_POINT('Ctrl Pts',(1.34722685747579,6.63407428498897,-38.8667427106261));
#38411=CARTESIAN_POINT('Ctrl Pts',(1.16647210396409,6.66570565136757,-38.8581185585584));
#38412=CARTESIAN_POINT('Ctrl Pts',(0.979526451516919,6.69842040055429,-38.8491990269621));
#38413=CARTESIAN_POINT('Ctrl Pts',(0.791291188010618,6.72325038873687,-38.8402794953659));
#38414=CARTESIAN_POINT('Ctrl Pts',(0.602443060545144,6.74012992150752,-38.8313599637697));
#38415=CARTESIAN_POINT('Ctrl Pts',(0.419508682656814,6.75648087434929,-38.8227197459104));
#38416=CARTESIAN_POINT('Ctrl Pts',(0.23599954997781,6.76537180209201,-38.8140795280512));
#38417=CARTESIAN_POINT('Ctrl Pts',(0.0525318974627829,6.76679609562376,
-38.805439310192));
#38418=CARTESIAN_POINT('Ctrl Pts',(-0.139832238302195,6.76828945421071,
-38.7963801217272));
#38419=CARTESIAN_POINT('Ctrl Pts',(-0.332150383408293,6.76157406414995,
-38.7873209332625));
#38420=CARTESIAN_POINT('Ctrl Pts',(-0.523716488820115,6.74670364247148,
-38.7782617447978));
#38421=CARTESIAN_POINT('Ctrl Pts',(-0.715282594231936,6.73183322079301,
-38.769202556333));
#38422=CARTESIAN_POINT('Ctrl Pts',(-0.906096284047167,6.708807846224,-38.7601433678683));
#38423=CARTESIAN_POINT('Ctrl Pts',(-1.09546147671801,6.67774311822691,-38.7510841794036));
#38424=CARTESIAN_POINT('Ctrl Pts',(-1.28449860747761,6.6467322076917,-38.7420406853473));
#38425=CARTESIAN_POINT('Ctrl Pts',(-1.47226654297517,6.60768204225785,-38.7329971912911));
#38426=CARTESIAN_POINT('Ctrl Pts',(-1.65810469081281,6.5607147350197,-38.7239536972348));
#38427=CARTESIAN_POINT('Ctrl Pts',(-1.84377285317746,6.5137903886054,-38.7149184752294));
#38428=CARTESIAN_POINT('Ctrl Pts',(-2.02751452141858,6.45896341691647,-38.7058832532241));
#38429=CARTESIAN_POINT('Ctrl Pts',(-2.20868076779968,6.39640666827492,-38.6968480312187));
#38430=CARTESIAN_POINT('Ctrl Pts',(-2.38952783869297,6.33396013100642,-38.6878287273076));
#38431=CARTESIAN_POINT('Ctrl Pts',(-2.56780832345928,6.26381108821348,-38.6788094233965));
#38432=CARTESIAN_POINT('Ctrl Pts',(-2.74289002919077,6.1861816403793,-38.6697901194854));
#38433=CARTESIAN_POINT('Ctrl Pts',(-2.91775208269464,6.10864958410909,-38.660782130921));
#38434=CARTESIAN_POINT('Ctrl Pts',(-3.08942314891028,6.0236559476321,-38.6517741423566));
#38435=CARTESIAN_POINT('Ctrl Pts',(-3.25729014899516,5.9314711400511,-38.6427661537921));
#38436=CARTESIAN_POINT('Ctrl Pts',(-3.42477801557925,5.83949453508765,-38.6337785100855));
#38437=CARTESIAN_POINT('Ctrl Pts',(-3.58847875738045,5.74035929295689,-38.6247908663788));
#38438=CARTESIAN_POINT('Ctrl Pts',(-3.74780348985188,5.63438177633128,-38.6158032226721));
#38439=CARTESIAN_POINT('Ctrl Pts',(-3.88656428900939,5.54208270467062,-38.6079756079388));
#38440=CARTESIAN_POINT('Ctrl Pts',(-4.02200601069406,5.44459439207581,-38.6001479932054));
#38441=CARTESIAN_POINT('Ctrl Pts',(-4.15375404391448,5.34215465357042,-38.5923203784721));
#38442=CARTESIAN_POINT('Ctrl Pts',(-4.29047642808377,5.2358471441543,-38.5841972200268));
#38443=CARTESIAN_POINT('Ctrl Pts',(-4.42315879319529,5.12425345235888,-38.5760740615816));
#38444=CARTESIAN_POINT('Ctrl Pts',(-4.55137299668703,5.00772331953635,-38.5679509031363));
#38445=CARTESIAN_POINT('Ctrl Pts',(-4.67957816040648,4.89120140269798,-38.5598283174162));
#38446=CARTESIAN_POINT('Ctrl Pts',(-4.80331551914681,4.76974398428607,-38.5517057316961));
#38447=CARTESIAN_POINT('Ctrl Pts',(-4.92219172300998,4.64373961823142,-38.543583145976));
#38448=CARTESIAN_POINT('Ctrl Pts',(-5.04108221107229,4.51772011145559,-38.5354595842437));
#38449=CARTESIAN_POINT('Ctrl Pts',(-5.15511013084091,4.3871528361571,-38.5273360225113));
#38450=CARTESIAN_POINT('Ctrl Pts',(-5.26392059652226,4.25246151699328,-38.519212460779));
#38451=CARTESIAN_POINT('Ctrl Pts',(-5.37281031771664,4.11767209118562,-38.5110829819959));
#38452=CARTESIAN_POINT('Ctrl Pts',(-5.4764747643854,3.97875290699445,-38.5029535032127));
#38453=CARTESIAN_POINT('Ctrl Pts',(-5.57460041236353,3.83615943913654,-38.4948240244296));
#38454=CARTESIAN_POINT('Ctrl Pts',(-5.6727660644412,3.69350783843162,-38.486691231401));
#38455=CARTESIAN_POINT('Ctrl Pts',(-5.76538822119881,3.54717927727347,-38.4785584383725));
#38456=CARTESIAN_POINT('Ctrl Pts',(-5.85219810773909,3.39765600197769,-38.4704256453439));
#38457=CARTESIAN_POINT('Ctrl Pts',(-5.9391023868613,3.24797014280378,-38.4622840091368));
#38458=CARTESIAN_POINT('Ctrl Pts',(-6.02018160151472,3.09508295424076,-38.4541423729296));
#38459=CARTESIAN_POINT('Ctrl Pts',(-6.09521378633161,2.93949960008725,-38.4460007367224));
#38460=CARTESIAN_POINT('Ctrl Pts',(-6.13344166534192,2.86023199441758,-38.4418526836618));
#38461=CARTESIAN_POINT('Ctrl Pts',(-6.17010065573144,2.78026483816001,-38.4377046306012));
#38462=CARTESIAN_POINT('Ctrl Pts',(-6.20516632234485,2.69966662979659,-38.4335565775406));
#38463=CARTESIAN_POINT('Ctrl Pts',(-6.2836902509147,2.51917988684769,-38.42426767892));
#38464=CARTESIAN_POINT('Ctrl Pts',(-6.35435036609351,2.33523149083991,-38.4149787802994));
#38465=CARTESIAN_POINT('Ctrl Pts',(-6.41687785198368,2.14848030773412,-38.4056898816789));
#38466=CARTESIAN_POINT('Ctrl Pts',(-6.47927456533099,1.96211970369527,-38.396420410241));
#38467=CARTESIAN_POINT('Ctrl Pts',(-6.53357255989753,1.77296819610722,-38.3871509388031));
#38468=CARTESIAN_POINT('Ctrl Pts',(-6.57955268183747,1.58170019501973,-38.3778814673653));
#38469=CARTESIAN_POINT('Ctrl Pts',(-6.62545405419011,1.39075977627676,-38.3686278716367));
#38470=CARTESIAN_POINT('Ctrl Pts',(-6.66306594648214,1.1977102803237,-38.3593742759082));
#38471=CARTESIAN_POINT('Ctrl Pts',(-6.69221929528,1.00323970409974,-38.3501206801796));
#38472=CARTESIAN_POINT('Ctrl Pts',(-6.72127264703585,0.809436168993859,
-38.3408988246195));
#38473=CARTESIAN_POINT('Ctrl Pts',(-6.74192532171844,0.614221465069455,
-38.3316769690594));
#38474=CARTESIAN_POINT('Ctrl Pts',(-6.75405965128696,0.41829084003543,-38.3224551134992));
#38475=CARTESIAN_POINT('Ctrl Pts',(-6.76267166772411,0.27923431006346,-38.3159101477295));
#38476=CARTESIAN_POINT('Ctrl Pts',(-6.76699396276897,0.139817469194059,
-38.3093651819597));
#38477=CARTESIAN_POINT('Ctrl Pts',(-6.76699999367839,0.000292500793738614,
-38.30282021619));
#38478=CARTESIAN_POINT('',(-6.76699993162883,0.00096194355167065,-38.6971797837635));
#38479=CARTESIAN_POINT('Ctrl Pts',(3.09908550384721,6.01564277861012,-39.3484860224351));
#38480=CARTESIAN_POINT('Ctrl Pts',(2.94437133429452,6.09534705257489,-39.3402665560113));
#38481=CARTESIAN_POINT('Ctrl Pts',(2.78639218245449,6.16917587646048,-39.3320470895876));
#38482=CARTESIAN_POINT('Ctrl Pts',(2.62563398538058,6.23685298646798,-39.3238276231638));
#38483=CARTESIAN_POINT('Ctrl Pts',(2.46502959728258,6.30446534489718,-39.3156160208971));
#38484=CARTESIAN_POINT('Ctrl Pts',(2.3016517873046,6.36593757261412,-39.3074044186305));
#38485=CARTESIAN_POINT('Ctrl Pts',(2.13601085070116,6.42103937425141,-39.2991928163638));
#38486=CARTESIAN_POINT('Ctrl Pts',(1.97049517578476,6.47609950657209,-39.2909874239096));
#38487=CARTESIAN_POINT('Ctrl Pts',(1.80272012168599,6.52479869529337,-39.2827820314554));
#38488=CARTESIAN_POINT('Ctrl Pts',(1.63321579930917,6.56695478535424,-39.2745766390012));
#38489=CARTESIAN_POINT('Ctrl Pts',(1.46380567465356,6.60908744823895,-39.2663758064854));
#38490=CARTESIAN_POINT('Ctrl Pts',(1.29266854312108,6.64468416961378,-39.2581749739696));
#38491=CARTESIAN_POINT('Ctrl Pts',(1.12034959639276,6.67361264847328,-39.2499741414538));
#38492=CARTESIAN_POINT('Ctrl Pts',(0.939296608403607,6.70400737659191,-39.2413576471032));
#38493=CARTESIAN_POINT('Ctrl Pts',(0.756939281898732,6.72704018589386,-39.2327411527526));
#38494=CARTESIAN_POINT('Ctrl Pts',(0.57392272231459,6.74261831255567,-39.224124658402));
#38495=CARTESIAN_POINT('Ctrl Pts',(0.399790550416843,6.7574402119285,-39.2159264446512));
#38496=CARTESIAN_POINT('Ctrl Pts',(0.225062026447252,6.7655140351368,-39.2077282309004));
#38497=CARTESIAN_POINT('Ctrl Pts',(0.0502982204209523,6.76681306739166,
-39.1995300171496));
#38498=CARTESIAN_POINT('Ctrl Pts',(-0.124481183155672,6.76811221558425,
-39.1913310717137));
#38499=CARTESIAN_POINT('Ctrl Pts',(-0.299295516341745,6.76263536508475,
-39.1831321262779));
#38500=CARTESIAN_POINT('Ctrl Pts',(-0.473583718648115,6.75040794777852,
-39.1749331808421));
#38501=CARTESIAN_POINT('Ctrl Pts',(-0.647919136903179,6.73817721797552,
-39.166732014252));
#38502=CARTESIAN_POINT('Ctrl Pts',(-0.821727782612122,6.71919230341321,
-39.158530847662));
#38503=CARTESIAN_POINT('Ctrl Pts',(-0.994453669868803,6.69353052570051,
-39.1503296810719));
#38504=CARTESIAN_POINT('Ctrl Pts',(-1.16725772738974,6.66785713428022,-39.1421248028936));
#38505=CARTESIAN_POINT('Ctrl Pts',(-1.33897769596545,6.63550091300536,-39.1339199247154));
#38506=CARTESIAN_POINT('Ctrl Pts',(-1.50906767778191,6.59659031196223,-39.1257150465371));
#38507=CARTESIAN_POINT('Ctrl Pts',(-1.67935628910185,6.55763427148003,-39.1175005867782));
#38508=CARTESIAN_POINT('Ctrl Pts',(-1.84801076260359,6.51210864508346,-39.1092861270193));
#38509=CARTESIAN_POINT('Ctrl Pts',(-2.01449935509248,6.46019205196966,-39.1010716672604));
#38510=CARTESIAN_POINT('Ctrl Pts',(-2.18110096466695,6.40824021642898,-39.0928516312978));
#38511=CARTESIAN_POINT('Ctrl Pts',(-2.34553342605553,6.34988888699901,-39.0846315953352));
#38512=CARTESIAN_POINT('Ctrl Pts',(-2.50728500844487,6.28536481729005,-39.0764115593726));
#38513=CARTESIAN_POINT('Ctrl Pts',(-2.66926134676726,6.22075109054481,-39.0681801015629));
#38514=CARTESIAN_POINT('Ctrl Pts',(-2.82854904072158,6.14994764018784,-39.0599486437531));
#38515=CARTESIAN_POINT('Ctrl Pts',(-2.98466015274912,6.07322754164469,-39.0517171859434));
#38516=CARTESIAN_POINT('Ctrl Pts',(-3.03864081228131,6.04669899114661,-39.0488708829755));
#38517=CARTESIAN_POINT('Ctrl Pts',(-3.09224190821867,6.01946339359807,-39.0460245800076));
#38518=CARTESIAN_POINT('Ctrl Pts',(-3.14544408829237,5.99153323344088,-39.0431782770398));
#38519=CARTESIAN_POINT('Ctrl Pts',(-3.29630219927205,5.91233551645193,-39.0351074068534));
#38520=CARTESIAN_POINT('Ctrl Pts',(-3.44444266254927,5.82729181424176,-39.0270365366669));
#38521=CARTESIAN_POINT('Ctrl Pts',(-3.58936826272957,5.73661263068282,-39.0189656664805));
#38522=CARTESIAN_POINT('Ctrl Pts',(-3.73411351426522,5.64604629031952,-39.0109048398647));
#38523=CARTESIAN_POINT('Ctrl Pts',(-3.87565155077558,5.54985861793858,-39.0028440132489));
#38524=CARTESIAN_POINT('Ctrl Pts',(-4.0135065113057,5.44830748799173,-38.9947831866331));
#38525=CARTESIAN_POINT('Ctrl Pts',(-4.15122015154176,5.34686046191965,-38.9867306234733));
#38526=CARTESIAN_POINT('Ctrl Pts',(-4.28525793171493,5.24006113943915,-38.9786780603134));
#38527=CARTESIAN_POINT('Ctrl Pts',(-4.41517002262306,5.12821242455212,-38.9706254971535));
#38528=CARTESIAN_POINT('Ctrl Pts',(-4.54497738170151,5.01645387925959,-38.9625794257656));
#38529=CARTESIAN_POINT('Ctrl Pts',(-4.67066539023081,4.89965428580147,-38.9545333543777));
#38530=CARTESIAN_POINT('Ctrl Pts',(-4.791814665727,4.77815876769741,-38.9464872829898));
#38531=CARTESIAN_POINT('Ctrl Pts',(-4.9128927737769,4.65673462043501,-38.9384459381539));
#38532=CARTESIAN_POINT('Ctrl Pts',(-5.02943719377697,4.53062030350734,-38.9304045933181));
#38533=CARTESIAN_POINT('Ctrl Pts',(-5.1410630949805,4.40019991062105,-38.9223632484822));
#38534=CARTESIAN_POINT('Ctrl Pts',(-5.25484080008599,4.26726541386387,-38.9141668912611));
#38535=CARTESIAN_POINT('Ctrl Pts',(-5.36350812498187,4.12985739148594,-38.9059705340401));
#38536=CARTESIAN_POINT('Ctrl Pts',(-5.46669812488634,3.98842081673489,-38.897774176819));
#38537=CARTESIAN_POINT('Ctrl Pts',(-5.56790437830955,3.84970324874557,-38.8897353881105));
#38538=CARTESIAN_POINT('Ctrl Pts',(-5.66384178073572,3.70711094025673,-38.881696599402));
#38539=CARTESIAN_POINT('Ctrl Pts',(-5.75420613299375,3.56109544649075,-38.8736578106935));
#38540=CARTESIAN_POINT('Ctrl Pts',(-5.84458015505619,3.415064327744,-38.8656181617618));
#38541=CARTESIAN_POINT('Ctrl Pts',(-5.92937974285766,3.26560961188173,-38.85757851283));
#38542=CARTESIAN_POINT('Ctrl Pts',(-6.00834534648432,3.11320979013305,-38.8495388638983));
#38543=CARTESIAN_POINT('Ctrl Pts',(-6.08733503563694,2.96076348447623,-38.8414967627701));
#38544=CARTESIAN_POINT('Ctrl Pts',(-6.16048702692392,2.80537061629134,-38.833454661642));
#38545=CARTESIAN_POINT('Ctrl Pts',(-6.22758890188882,2.64753195808307,-38.8254125605138));
#38546=CARTESIAN_POINT('Ctrl Pts',(-6.2969552014982,2.48436686529029,-38.817099070069));
#38547=CARTESIAN_POINT('Ctrl Pts',(-6.35985573377751,2.31858842465414,-38.8087855796243));
#38548=CARTESIAN_POINT('Ctrl Pts',(-6.41611129451752,2.1507684339242,-38.8004720891795));
#38549=CARTESIAN_POINT('Ctrl Pts',(-6.47062628872235,1.98814085183718,-38.7924158210088));
#38550=CARTESIAN_POINT('Ctrl Pts',(-6.5189013502021,1.82359654469976,-38.784359552838));
#38551=CARTESIAN_POINT('Ctrl Pts',(-6.56082529297568,1.65766717861295,-38.7763032846673));
#38552=CARTESIAN_POINT('Ctrl Pts',(-6.60475707082873,1.4837910694504,-38.7678611830855));
#38553=CARTESIAN_POINT('Ctrl Pts',(-6.64171433038961,1.30839444740119,-38.7594190815037));
#38554=CARTESIAN_POINT('Ctrl Pts',(-6.67163014485131,1.13209549522611,-38.750976979922));
#38555=CARTESIAN_POINT('Ctrl Pts',(-6.70154595931302,0.955796543051042,
-38.7425348783402));
#38556=CARTESIAN_POINT('Ctrl Pts',(-6.72442035542752,0.778595728902839,
-38.7340927767585));
#38557=CARTESIAN_POINT('Ctrl Pts',(-6.74024886421216,0.601110845424283,
-38.7256506751767));
#38558=CARTESIAN_POINT('Ctrl Pts',(-6.75804268603638,0.401588929867985,
-38.7161603780545));
#38559=CARTESIAN_POINT('Ctrl Pts',(-6.76697144454004,0.201360324820626,
-38.7066700809323));
#38560=CARTESIAN_POINT('Ctrl Pts',(-6.76699993162869,0.000961944536271024,
-38.6971797838101));
#38561=CARTESIAN_POINT('Ctrl Pts',(-6.76699993162883,0.000961943551675157,
-38.6971797837635));
#38562=CARTESIAN_POINT('Ctrl Pts',(-6.76702456299972,-0.17231276141232,
-38.6889739867329));
#38563=CARTESIAN_POINT('Ctrl Pts',(-6.76038966563165,-0.34584484753625,
-38.6807681897024));
#38564=CARTESIAN_POINT('Ctrl Pts',(-6.74706194009427,-0.519080125348007,
-38.6725623926718));
#38565=CARTESIAN_POINT('Ctrl Pts',(-6.73374985689133,-0.6921120823349,-38.6643662265285));
#38566=CARTESIAN_POINT('Ctrl Pts',(-6.71376061346842,-0.864847568095618,
-38.6561700603851));
#38567=CARTESIAN_POINT('Ctrl Pts',(-6.68711287393178,-1.0367306358432,-38.6479738942418));
#38568=CARTESIAN_POINT('Ctrl Pts',(-6.66049097002691,-1.20844705877502,
-38.6397856744809));
#38569=CARTESIAN_POINT('Ctrl Pts',(-6.62722348061152,-1.37931235505076,
-38.63159745472));
#38570=CARTESIAN_POINT('Ctrl Pts',(-6.58738100010477,-1.54877388906794,
-38.6234092349592));
#38571=CARTESIAN_POINT('Ctrl Pts',(-6.54756901736165,-1.71810570732088,
-38.6152272829404));
#38572=CARTESIAN_POINT('Ctrl Pts',(-6.50119214995199,-1.88603555350871,
-38.6070453309215));
#38573=CARTESIAN_POINT('Ctrl Pts',(-6.44837238636049,-2.05201914387354,
-38.5988633789027));
#38574=CARTESIAN_POINT('Ctrl Pts',(-6.3955819855785,-2.21791046300856,-38.590685975278));
#38575=CARTESIAN_POINT('Ctrl Pts',(-6.33635593265055,-2.38185733840268,
-38.5825085716532));
#38576=CARTESIAN_POINT('Ctrl Pts',(-6.27086657931742,-2.54332879203612,
-38.5743311680285));
#38577=CARTESIAN_POINT('Ctrl Pts',(-6.20539643680379,-2.70475287920779,
-38.5661561631848));
#38578=CARTESIAN_POINT('Ctrl Pts',(-6.13366678753111,-2.86370265619969,
-38.5579811583412));
#38579=CARTESIAN_POINT('Ctrl Pts',(-6.05589886771911,-3.01966519732873,
-38.5498061534976));
#38580=CARTESIAN_POINT('Ctrl Pts',(-5.97813938880849,-3.17561081034101,
-38.541632035966));
#38581=CARTESIAN_POINT('Ctrl Pts',(-5.89434310579912,-3.32856951025794,
-38.5334579184344));
#38582=CARTESIAN_POINT('Ctrl Pts',(-5.80477815147919,-3.4780511226993,-38.5252838009027));
#38583=CARTESIAN_POINT('Ctrl Pts',(-5.71520636675548,-3.62754413490944,
-38.5171090599965));
#38584=CARTESIAN_POINT('Ctrl Pts',(-5.61986522085826,-3.77355922230813,
-38.5089343190902));
#38585=CARTESIAN_POINT('Ctrl Pts',(-5.51906729291426,-3.91563343742543,
-38.5007595781839));
#38586=CARTESIAN_POINT('Ctrl Pts',(-5.41819964722992,-4.05780591937658,
-38.4925791831489));
#38587=CARTESIAN_POINT('Ctrl Pts',(-5.31186788789913,-4.19603178831862,
-38.4843987881138));
#38588=CARTESIAN_POINT('Ctrl Pts',(-5.20042661905157,-4.32987897981686,
-38.4762183930788));
#38589=CARTESIAN_POINT('Ctrl Pts',(-5.08894540440009,-4.46377414845788,
-38.4680350658046));
#38590=CARTESIAN_POINT('Ctrl Pts',(-4.97235126916519,-4.59328724112423,
-38.4598517385303));
#38591=CARTESIAN_POINT('Ctrl Pts',(-4.85103704135763,-4.718021685344,-38.4516684112561));
#38592=CARTESIAN_POINT('Ctrl Pts',(-4.72958736508698,-4.84289539673027,
-38.4434759472209));
#38593=CARTESIAN_POINT('Ctrl Pts',(-4.60340732654163,-4.9629795486941,-38.4352834831857));
#38594=CARTESIAN_POINT('Ctrl Pts',(-4.47292502481537,-5.07791598220967,
-38.4270910191505));
#38595=CARTESIAN_POINT('Ctrl Pts',(-4.37222348491334,-5.16661978106009,
-38.4207683705382));
#38596=CARTESIAN_POINT('Ctrl Pts',(-4.26896015810002,-5.25225827422651,
-38.4144457219259));
#38597=CARTESIAN_POINT('Ctrl Pts',(-4.16334399683779,-5.33468422345641,
-38.4081230733136));
#38598=CARTESIAN_POINT('Ctrl Pts',(-4.02217457272462,-5.44485698154289,
-38.3996720497885));
#38599=CARTESIAN_POINT('Ctrl Pts',(-3.87650987115763,-5.54951598081996,
-38.3912210262633));
#38600=CARTESIAN_POINT('Ctrl Pts',(-3.72680741947126,-5.64829137511283,
-38.3827700027381));
#38601=CARTESIAN_POINT('Ctrl Pts',(-3.57723677634384,-5.74697980060703,
-38.3743264200879));
#38602=CARTESIAN_POINT('Ctrl Pts',(-3.42363574452268,-5.83979476480231,
-38.3658828374378));
#38603=CARTESIAN_POINT('Ctrl Pts',(-3.26649324084622,-5.92640792618142,
-38.3574392547876));
#38604=CARTESIAN_POINT('Ctrl Pts',(-3.10946773465818,-6.01295660136419,
-38.3490019586477));
#38605=CARTESIAN_POINT('Ctrl Pts',(-2.94890630218418,-6.09331251888087,
-38.3405646625078));
#38606=CARTESIAN_POINT('Ctrl Pts',(-2.785325371087,-6.16719154698304,-38.3321273663679));
#38607=CARTESIAN_POINT('Ctrl Pts',(-2.62186114251269,-6.24101786803122,
-38.3236960895956));
#38608=CARTESIAN_POINT('Ctrl Pts',(-2.45538201356443,-6.30837638044795,
-38.3152648128232));
#38609=CARTESIAN_POINT('Ctrl Pts',(-2.28642763911666,-6.36902956902254,
-38.3068335360509));
#38610=CARTESIAN_POINT('Ctrl Pts',(-2.11754568463057,-6.42965675944463,
-38.298405873229));
#38611=CARTESIAN_POINT('Ctrl Pts',(-1.94619091117425,-6.48358424396456,
-38.2899782104071));
#38612=CARTESIAN_POINT('Ctrl Pts',(-1.77292212762096,-6.53062295109678,
-38.2815505475852));
#38613=CARTESIAN_POINT('Ctrl Pts',(-1.5997066830516,-6.57764717785468,-38.2731254791312));
#38614=CARTESIAN_POINT('Ctrl Pts',(-1.42457872294707,-6.61778676956985,
-38.2647004106772));
#38615=CARTESIAN_POINT('Ctrl Pts',(-1.24811171909707,-6.65090265577933,
-38.2562753422233));
#38616=CARTESIAN_POINT('Ctrl Pts',(-1.19982494532777,-6.65996417589743,
-38.2539699856096));
#38617=CARTESIAN_POINT('Ctrl Pts',(-1.15143798463569,-6.66850009729251,
-38.2516646289958));
#38618=CARTESIAN_POINT('Ctrl Pts',(-1.1029627353664,-6.67650823442861,-38.2493592723821));
#38619=CARTESIAN_POINT('Ctrl Pts',(-0.921729335428296,-6.70644808914259,
-38.2407402838577));
#38620=CARTESIAN_POINT('Ctrl Pts',(-0.739342141307451,-6.7289934132114,
-38.2321212953332));
#38621=CARTESIAN_POINT('Ctrl Pts',(-0.556414885681503,-6.74408566634441,
-38.2235023068087));
#38622=CARTESIAN_POINT('Ctrl Pts',(-0.373378040304804,-6.75918696108389,
-38.2148781547409));
#38623=CARTESIAN_POINT('Ctrl Pts',(-0.189800790848503,-6.76682624899216,
-38.2062540026732));
#38624=CARTESIAN_POINT('Ctrl Pts',(-0.00629930563155577,-6.76699706803162,
-38.1976298506054));
#38625=CARTESIAN_POINT('Ctrl Pts',(0.183487154821004,-6.76717373766914,
-38.1887103190092));
#38626=CARTESIAN_POINT('Ctrl Pts',(0.373192211341671,-6.75936129432861,
-38.1797907874129));
#38627=CARTESIAN_POINT('Ctrl Pts',(0.562137874734621,-6.74361105119422,
-38.1708712558167));
#38628=CARTESIAN_POINT('Ctrl Pts',(0.745166734228464,-6.72835402446034,
-38.1622310379575));
#38629=CARTESIAN_POINT('Ctrl Pts',(0.927482744725567,-6.70564889972387,
-38.1535908200982));
#38630=CARTESIAN_POINT('Ctrl Pts',(1.10847766379766,-6.67559482509699,-38.1449506022389));
#38631=CARTESIAN_POINT('Ctrl Pts',(1.29824916143105,-6.64408340598551,-38.1358914137742));
#38632=CARTESIAN_POINT('Ctrl Pts',(1.48656788135299,-6.60449268576423,-38.1268322253095));
#38633=CARTESIAN_POINT('Ctrl Pts',(1.67274744058781,-6.55699664480675,-38.1177730368448));
#38634=CARTESIAN_POINT('Ctrl Pts',(1.85892699982264,-6.50950060384926,-38.1087138483801));
#38635=CARTESIAN_POINT('Ctrl Pts',(2.04296704153323,-6.45409938416893,-38.0996546599154));
#38636=CARTESIAN_POINT('Ctrl Pts',(2.22420161295695,-6.39102622314443,-38.0905954714507));
#38637=CARTESIAN_POINT('Ctrl Pts',(2.40512220820077,-6.3280623319463,-38.0815519773944));
#38638=CARTESIAN_POINT('Ctrl Pts',(2.58341399668192,-6.25739585345925,-38.0725084833381));
#38639=CARTESIAN_POINT('Ctrl Pts',(2.75844710605893,-6.17926035728186,-38.0634649892818));
#38640=CARTESIAN_POINT('Ctrl Pts',(2.93332011329166,-6.10119633135673,-38.0544297672764));
#38641=CARTESIAN_POINT('Ctrl Pts',(3.10494017518044,-6.01567702458991,-38.0453945452711));
#38642=CARTESIAN_POINT('Ctrl Pts',(3.27269761034307,-5.92298399046078,-38.0363593232657));
#38643=CARTESIAN_POINT('Ctrl Pts',(3.44015949342455,-5.83045426127918,-38.0273400193546));
#38644=CARTESIAN_POINT('Ctrl Pts',(3.60377213061202,-5.73077615733481,-38.0183207154435));
#38645=CARTESIAN_POINT('Ctrl Pts',(3.76295077228059,-5.62427688555542,-38.0093014115324));
#38646=CARTESIAN_POINT('Ctrl Pts',(3.92192971322564,-5.51791122455072,-38.0002934229679));
#38647=CARTESIAN_POINT('Ctrl Pts',(4.07648556270885,-5.40474160580249,-37.9912854344035));
#38648=CARTESIAN_POINT('Ctrl Pts',(4.22606068508645,-5.2851395521752,-37.9822774458391));
#38649=CARTESIAN_POINT('Ctrl Pts',(4.37529798681038,-5.16580762397582,-37.9732898021324));
#38650=CARTESIAN_POINT('Ctrl Pts',(4.51957683014816,-5.04007240828892,-37.9643021584257));
#38651=CARTESIAN_POINT('Ctrl Pts',(4.65837129463945,-4.90834655268749,-37.9553145147191));
#38652=CARTESIAN_POINT('Ctrl Pts',(4.77925165334199,-4.79362246240146,-37.9474868999857));
#38653=CARTESIAN_POINT('Ctrl Pts',(4.89597234147034,-4.67435506522983,-37.9396592852524));
#38654=CARTESIAN_POINT('Ctrl Pts',(5.00820507123561,-4.55084288505437,-37.9318316705191));
#38655=CARTESIAN_POINT('Ctrl Pts',(5.12467532145758,-4.42266731131056,-37.9237085120738));
#38656=CARTESIAN_POINT('Ctrl Pts',(5.23625901429123,-4.28997653712542,-37.9155853536285));
#38657=CARTESIAN_POINT('Ctrl Pts',(5.3425943139521,-4.15318853370838,-37.9074621951833));
#38658=CARTESIAN_POINT('Ctrl Pts',(5.44892211641825,-4.01641017456092,-37.8993396094631));
#38659=CARTESIAN_POINT('Ctrl Pts',(5.55000203814904,-3.87553545057345,-37.891217023743));
#38660=CARTESIAN_POINT('Ctrl Pts',(5.64551317557136,-3.73101460523142,-37.8830944380229));
#38661=CARTESIAN_POINT('Ctrl Pts',(5.74103578964029,-3.58647639422174,-37.8749708762904));
#38662=CARTESIAN_POINT('Ctrl Pts',(5.83098808616751,-3.43829149547754,-37.866847314558));
#38663=CARTESIAN_POINT('Ctrl Pts',(5.91509308643174,-3.28693820733633,-37.8587237528255));
#38664=CARTESIAN_POINT('Ctrl Pts',(5.99925934720783,-3.13547467628599,-37.8505942740424));
#38665=CARTESIAN_POINT('Ctrl Pts',(6.07756962728576,-2.98083846683454,-37.8424647952593));
#38666=CARTESIAN_POINT('Ctrl Pts',(6.14979314090534,-2.82353206535248,-37.8343353164761));
#38667=CARTESIAN_POINT('Ctrl Pts',(6.22204609878018,-2.66616153281938,-37.8262025234476));
#38668=CARTESIAN_POINT('Ctrl Pts',(6.28820720415832,-2.50611897639113,-37.818069730419));
#38669=CARTESIAN_POINT('Ctrl Pts',(6.34809434810833,-2.3439255848928,-37.8099369373905));
#38670=CARTESIAN_POINT('Ctrl Pts',(6.40804661024213,-2.18155583268699,-37.8017953011833));
#38671=CARTESIAN_POINT('Ctrl Pts',(6.46171117191644,-2.01703092182005,-37.7936536649762));
#38672=CARTESIAN_POINT('Ctrl Pts',(6.50895596995547,-1.8508865932793,-37.785512028769));
#38673=CARTESIAN_POINT('Ctrl Pts',(6.53302655283478,-1.76623831461031,-37.7813639757086));
#38674=CARTESIAN_POINT('Ctrl Pts',(6.55543153589605,-1.68116984577571,-37.7772159226481));
#38675=CARTESIAN_POINT('Ctrl Pts',(6.57615859055716,-1.59575286051483,-37.7730678695876));
#38676=CARTESIAN_POINT('Ctrl Pts',(6.61833528361732,-1.42194109476349,-37.7646271546095));
#38677=CARTESIAN_POINT('Ctrl Pts',(6.65364800675882,-1.24632775325899,-37.7561864396314));
#38678=CARTESIAN_POINT('Ctrl Pts',(6.6819531313822,-1.06948181378257,-37.7477457246534));
#38679=CARTESIAN_POINT('Ctrl Pts',(6.71023686165885,-0.892769542798911,
-37.7393113895654));
#38680=CARTESIAN_POINT('Ctrl Pts',(6.73152349951128,-0.714826859088382,
-37.7308770544773));
#38681=CARTESIAN_POINT('Ctrl Pts',(6.74572030332436,-0.536233707740832,
-37.7224427193893));
#38682=CARTESIAN_POINT('Ctrl Pts',(6.75990855660553,-0.357748120494308,
-37.7140134641807));
#38683=CARTESIAN_POINT('Ctrl Pts',(6.76701546259102,-0.17861317819431,-37.7055842089721));
#38684=CARTESIAN_POINT('Ctrl Pts',(6.76699997472549,0.000584863454290374,
-37.6971549537635));
#38685=CARTESIAN_POINT('Ctrl Pts',(6.76698449381236,0.179702464314105,-37.6887294823905));
#38686=CARTESIAN_POINT('Ctrl Pts',(6.75985299394651,0.358882775184343,-37.6803040110175));
#38687=CARTESIAN_POINT('Ctrl Pts',(6.74561649975955,0.537537941146272,-37.6718785396446));
#38688=CARTESIAN_POINT('Ctrl Pts',(6.73138421429322,0.716140291458942,-37.6634555590853));
#38689=CARTESIAN_POINT('Ctrl Pts',(6.71005114972376,0.894217474456715,-37.6550325785261));
#38690=CARTESIAN_POINT('Ctrl Pts',(6.68168034297353,1.07118476199073,-37.6466095979669));
#38691=CARTESIAN_POINT('Ctrl Pts',(6.65330906646156,1.24815497973616,-37.6381864779405));
#38692=CARTESIAN_POINT('Ctrl Pts',(6.61789986118044,1.42401493512585,-37.6297633579142));
#38693=CARTESIAN_POINT('Ctrl Pts',(6.57556734176414,1.59818745268662,-37.6213402378879));
#38694=CARTESIAN_POINT('Ctrl Pts',(6.53323335841875,1.77236599342335,-37.612916826576));
#38695=CARTESIAN_POINT('Ctrl Pts',(6.48397566216803,1.94485665586912,-37.6044934152642));
#38696=CARTESIAN_POINT('Ctrl Pts',(6.42795950765314,2.11509469480013,-37.5960700039523));
#38697=CARTESIAN_POINT('Ctrl Pts',(6.37193360372924,2.28536236304583,-37.5876451265762));
#38698=CARTESIAN_POINT('Ctrl Pts',(6.30914700061127,2.45337630934582,-37.5792202492001));
#38699=CARTESIAN_POINT('Ctrl Pts',(6.23981424521007,2.61858877742831,-37.5707953718239));
#38700=CARTESIAN_POINT('Ctrl Pts',(6.17045975023532,2.78385304856668,-37.5623678527925));
#38701=CARTESIAN_POINT('Ctrl Pts',(6.09455513969854,2.9463137827764,-37.5539403337611));
#38702=CARTESIAN_POINT('Ctrl Pts',(6.01236248700822,3.10544462594591,-37.5455128147296));
#38703=CARTESIAN_POINT('Ctrl Pts',(5.93009612712363,3.26471817150532,-37.5370777382249));
#38704=CARTESIAN_POINT('Ctrl Pts',(5.84153061099496,3.42065556275218,-37.5286426617201));
#38705=CARTESIAN_POINT('Ctrl Pts',(5.74697378902983,3.57275541679027,-37.5202075852153));
#38706=CARTESIAN_POINT('Ctrl Pts',(5.6523712671303,3.72492878168888,-37.5117684319825));
#38707=CARTESIAN_POINT('Ctrl Pts',(5.55177184719688,3.87326063165815,-37.5033292787497));
#38708=CARTESIAN_POINT('Ctrl Pts',(5.44552614318835,4.01727943064112,-37.494890125517));
#38709=CARTESIAN_POINT('Ctrl Pts',(5.33916237041437,4.16145827488856,-37.4864415940188));
#38710=CARTESIAN_POINT('Ctrl Pts',(5.2271399805179,4.30131422757586,-37.4779930625207));
#38711=CARTESIAN_POINT('Ctrl Pts',(5.10984998236812,4.43640870047976,-37.4695445310226));
#38712=CARTESIAN_POINT('Ctrl Pts',(5.04504345290673,4.51105277991045,-37.4648764432566));
#38713=CARTESIAN_POINT('Ctrl Pts',(4.97862943853597,4.58424384948346,-37.4602083554906));
#38714=CARTESIAN_POINT('Ctrl Pts',(4.91067862684337,4.65591284538958,-37.4555402677246));
#38715=CARTESIAN_POINT('Ctrl Pts',(4.79069238073492,4.78246459020229,-37.447297447461));
#38716=CARTESIAN_POINT('Ctrl Pts',(4.66564531357555,4.90454994027631,-37.4390546271974));
#38717=CARTESIAN_POINT('Ctrl Pts',(4.53590146638694,5.02174141978944,-37.4308118069338));
#38718=CARTESIAN_POINT('Ctrl Pts',(4.40634680531483,5.13876201643316,-37.4225810059465));
#38719=CARTESIAN_POINT('Ctrl Pts',(4.2721092754121,5.25090272790146,-37.4143502049592));
#38720=CARTESIAN_POINT('Ctrl Pts',(4.13359124472159,5.35777121773233,-37.406119403972));
#38721=CARTESIAN_POINT('Ctrl Pts',(3.99519018441227,5.4645494633695,-37.3978955534151));
#38722=CARTESIAN_POINT('Ctrl Pts',(3.85251609900339,5.56606413430345,-37.3896717028583));
#38723=CARTESIAN_POINT('Ctrl Pts',(3.70600667392114,5.6619611030854,-37.3814478523014));
#38724=CARTESIAN_POINT('Ctrl Pts',(3.55961814680442,5.75777893874386,-37.3732307879755));
#38725=CARTESIAN_POINT('Ctrl Pts',(3.40940088306261,5.84798811539616,-37.3650137236496));
#38726=CARTESIAN_POINT('Ctrl Pts',(3.25582383722723,5.93227613492014,-37.3567966593237));
#38727=CARTESIAN_POINT('Ctrl Pts',(3.20395444979805,5.96074372209468,-37.3540214132527));
#38728=CARTESIAN_POINT('Ctrl Pts',(3.15170206751786,5.988536243908,-37.3512461671817));
#38729=CARTESIAN_POINT('Ctrl Pts',(3.09908550384721,6.01564277861012,-37.3484709211107));
#38730=CARTESIAN_POINT('Origin',(0.,0.,-63.6971797838103));
#38731=CARTESIAN_POINT('',(3.09908550384724,6.01564277861011,-34.9544861942313));
#38732=CARTESIAN_POINT('',(3.0990855038472,6.01564277861013,-35.3486949847746));
#38733=CARTESIAN_POINT('',(3.09908550384721,6.01564277861012,-63.6971797838103));
#38734=CARTESIAN_POINT('',(-6.76699965717165,-0.00196728107387918,-36.30282021619));
#38735=CARTESIAN_POINT('Ctrl Pts',(-6.76699958899529,-0.00235850324450193,
-36.30282021619));
#38736=CARTESIAN_POINT('Ctrl Pts',(-6.76693518406772,-0.187148632078428,
-36.2941557813363));
#38737=CARTESIAN_POINT('Ctrl Pts',(-6.75929728402724,-0.371773878308019,
-36.2854913464826));
#38738=CARTESIAN_POINT('Ctrl Pts',(-6.744151692339,-0.555614030349293,-36.276826911629));
#38739=CARTESIAN_POINT('Ctrl Pts',(-6.72898809559704,-0.739672731251764,
-36.2681521765098));
#38740=CARTESIAN_POINT('Ctrl Pts',(-6.70629902098999,-0.922944181880305,
-36.2594774413907));
#38741=CARTESIAN_POINT('Ctrl Pts',(-6.67620166752469,-1.10481686018114,
-36.2508027062715));
#38742=CARTESIAN_POINT('Ctrl Pts',(-6.64604452067217,-1.28705085873868,
-36.2421107373515));
#38743=CARTESIAN_POINT('Ctrl Pts',(-6.60844972316436,-1.46788023873274,
-36.2334187684315));
#38744=CARTESIAN_POINT('Ctrl Pts',(-6.56358525718865,-1.64670506515762,
-36.2247267995115));
#38745=CARTESIAN_POINT('Ctrl Pts',(-6.53973275556198,-1.7417785129392,-36.2201056545075));
#38746=CARTESIAN_POINT('Ctrl Pts',(-6.51382625408026,-1.83628563886716,
-36.2154845095034));
#38747=CARTESIAN_POINT('Ctrl Pts',(-6.48589658976399,-1.93013844759589,
-36.2108633644994));
#38748=CARTESIAN_POINT('Ctrl Pts',(-6.43488188762416,-2.10156453521602,
-36.2024226495213));
#38749=CARTESIAN_POINT('Ctrl Pts',(-6.37702900081694,-2.27109352276146,
-36.1939819345432));
#38750=CARTESIAN_POINT('Ctrl Pts',(-6.3125001209302,-2.43816144323058,-36.1855412195651));
#38751=CARTESIAN_POINT('Ctrl Pts',(-6.24802001501109,-2.60510308589419,
-36.1771068844771));
#38752=CARTESIAN_POINT('Ctrl Pts',(-6.17687409466979,-2.76958705975169,
-36.1686725493891));
#38753=CARTESIAN_POINT('Ctrl Pts',(-6.0992740452056,-2.93106552664407,-36.1602382143011));
#38754=CARTESIAN_POINT('Ctrl Pts',(-6.0217207331413,-3.09244673736546,-36.1518089590924));
#38755=CARTESIAN_POINT('Ctrl Pts',(-5.93772118578649,-3.25082575021071,
-36.1433797038838));
#38756=CARTESIAN_POINT('Ctrl Pts',(-5.8475349372065,-3.40567528665746,-36.1349504486752));
#38757=CARTESIAN_POINT('Ctrl Pts',(-5.75738917262334,-3.56045531219494,
-36.1265249773022));
#38758=CARTESIAN_POINT('Ctrl Pts',(-5.66106241171812,-3.71170873274347,
-36.1180995059292));
#38759=CARTESIAN_POINT('Ctrl Pts',(-5.55885999157159,-3.85893309013057,
-36.1096740345562));
#38760=CARTESIAN_POINT('Ctrl Pts',(-5.45668778542541,-4.00611392372658,
-36.1012510539969));
#38761=CARTESIAN_POINT('Ctrl Pts',(-5.34864357397227,-4.14926779590544,
-36.0928280734377));
#38762=CARTESIAN_POINT('Ctrl Pts',(-5.23507606828636,-4.28792112325489,
-36.0844050928785));
#38763=CARTESIAN_POINT('Ctrl Pts',(-5.12150668215806,-4.42657674641591,
-36.0759819728521));
#38764=CARTESIAN_POINT('Ctrl Pts',(-5.00241402517405,-4.56073141379927,
-36.0675588528258));
#38765=CARTESIAN_POINT('Ctrl Pts',(-4.87818757972632,-4.68994402280068,
-36.0591357327995));
#38766=CARTESIAN_POINT('Ctrl Pts',(-4.75395683832092,-4.81916110018963,
-36.0507123214876));
#38767=CARTESIAN_POINT('Ctrl Pts',(-4.62459218548861,-4.94343553790109,
-36.0422889101758));
#38768=CARTESIAN_POINT('Ctrl Pts',(-4.49052061019821,-5.06236245733009,
-36.0338654988639));
#38769=CARTESIAN_POINT('Ctrl Pts',(-4.35642570023534,-5.18131007555901,
-36.0254406214878));
#38770=CARTESIAN_POINT('Ctrl Pts',(-4.21762248400595,-5.29490809863485,
-36.0170157441117));
#38771=CARTESIAN_POINT('Ctrl Pts',(-4.07457199843356,-5.40279113325522,
-36.0085908667356));
#38772=CARTESIAN_POINT('Ctrl Pts',(-3.93147665878687,-5.51070799504947,
-36.0001633477041));
#38773=CARTESIAN_POINT('Ctrl Pts',(-3.78413166080402,-5.61290609498366,
-35.9917358286727));
#38774=CARTESIAN_POINT('Ctrl Pts',(-3.63302834270189,-5.70906245027367,
-35.9833083096412));
#38775=CARTESIAN_POINT('Ctrl Pts',(-3.48178952098421,-5.80530503486666,
-35.9748732331365));
#38776=CARTESIAN_POINT('Ctrl Pts',(-3.32678592639158,-5.89549486965611,
-35.9664381566317));
#38777=CARTESIAN_POINT('Ctrl Pts',(-3.16853589061581,-5.97935358629003,
-35.9580030801269));
#38778=CARTESIAN_POINT('Ctrl Pts',(-3.01020937155624,-6.06325283239362,
-35.9495639268941));
#38779=CARTESIAN_POINT('Ctrl Pts',(-2.84863358030992,-6.14081470891375,
-35.9411247736614));
#38780=CARTESIAN_POINT('Ctrl Pts',(-2.68434878449117,-6.21180815891804,
-35.9326856204286));
#38781=CARTESIAN_POINT('Ctrl Pts',(-2.51988142220354,-6.28288050254982,
-35.9242370889305));
#38782=CARTESIAN_POINT('Ctrl Pts',(-2.35269934930984,-6.3473697097327,-35.9157885574324));
#38783=CARTESIAN_POINT('Ctrl Pts',(-2.18336116201439,-6.40509352283065,
-35.9073400259343));
#38784=CARTESIAN_POINT('Ctrl Pts',(-2.08979631934266,-6.43698780242099,
-35.9026719381683));
#38785=CARTESIAN_POINT('Ctrl Pts',(-1.99557349648872,-6.46681754635892,
-35.8980038504023));
#38786=CARTESIAN_POINT('Ctrl Pts',(-1.90078853251652,-6.49455864202131,
-35.8933357626363));
#38787=CARTESIAN_POINT('Ctrl Pts',(-1.73346056929066,-6.543531188302,-35.8850949870396));
#38788=CARTESIAN_POINT('Ctrl Pts',(-1.56400775857775,-6.58610057937274,
-35.8768542114428));
#38789=CARTESIAN_POINT('Ctrl Pts',(-1.39295940348758,-6.6220807228722,-35.8686134358461));
#38790=CARTESIAN_POINT('Ctrl Pts',(-1.22210050299461,-6.658021014462,-35.8603817878017));
#38791=CARTESIAN_POINT('Ctrl Pts',(-1.04964992212572,-6.68738651814767,
-35.8521501397573));
#38792=CARTESIAN_POINT('Ctrl Pts',(-0.876152964625214,-6.71004060960725,
-35.8439184917129));
#38793=CARTESIAN_POINT('Ctrl Pts',(-0.702817255036443,-6.73267364637519,
-35.8356944941546));
#38794=CARTESIAN_POINT('Ctrl Pts',(-0.528437456303542,-6.7486076474621,
-35.8274704965963));
#38795=CARTESIAN_POINT('Ctrl Pts',(-0.353570028647881,-6.75775681974736,
-35.8192464990381));
#38796=CARTESIAN_POINT('Ctrl Pts',(-0.178857097044056,-6.76689790870336,
-35.8110297674136));
#38797=CARTESIAN_POINT('Ctrl Pts',(-0.00365774913480038,-6.76926609785636,
-35.8028130357891));
#38798=CARTESIAN_POINT('Ctrl Pts',(0.171465578530179,-6.76482731157118,
-35.7945963041645));
#38799=CARTESIAN_POINT('Ctrl Pts',(0.346499184031142,-6.76039079944054,
-35.7863837822759));
#38800=CARTESIAN_POINT('Ctrl Pts',(0.521456492059731,-6.7491542665203,-35.7781712603872));
#38801=CARTESIAN_POINT('Ctrl Pts',(0.695773782498911,-6.73113570236013,
-35.7699587384985));
#38802=CARTESIAN_POINT('Ctrl Pts',(0.870032780397239,-6.71312316369452,
-35.7617489629166));
#38803=CARTESIAN_POINT('Ctrl Pts',(1.04365183355713,-6.6883331483432,-35.7535391873348));
#38804=CARTESIAN_POINT('Ctrl Pts',(1.21607096902238,-6.65683561448688,-35.7453294117529));
#38805=CARTESIAN_POINT('Ctrl Pts',(1.29137916791349,-6.64307831001003,-35.7417435950702));
#38806=CARTESIAN_POINT('Ctrl Pts',(1.36645852944062,-6.6280420689442,-35.7381577783875));
#38807=CARTESIAN_POINT('Ctrl Pts',(1.44126284911144,-6.61173580837674,-35.7345719617048));
#38808=CARTESIAN_POINT('Ctrl Pts',(1.62606603232124,-6.57145138533304,-35.7257132441831));
#38809=CARTESIAN_POINT('Ctrl Pts',(1.80899833781516,-6.52345413561644,-35.7168545266613));
#38810=CARTESIAN_POINT('Ctrl Pts',(1.98944073126631,-6.46795288918979,-35.7079958091395));
#38811=CARTESIAN_POINT('Ctrl Pts',(2.1702207034546,-6.41234780884518,-35.6991205183801));
#38812=CARTESIAN_POINT('Ctrl Pts',(2.34850120656789,-6.34921075250704,-35.6902452276207));
#38813=CARTESIAN_POINT('Ctrl Pts',(2.523681965802,-6.27879911571359,-35.6813699368612));
#38814=CARTESIAN_POINT('Ctrl Pts',(2.69936027778126,-6.20818749403979,-35.6724694382804));
#38815=CARTESIAN_POINT('Ctrl Pts',(2.87192098591952,-6.1302600431543,-35.6635689396997));
#38816=CARTESIAN_POINT('Ctrl Pts',(3.04078449077462,-6.04532204937542,-35.6546684411189));
#38817=CARTESIAN_POINT('Ctrl Pts',(3.20987658638236,-5.96026907492061,-35.6457558939213));
#38818=CARTESIAN_POINT('Ctrl Pts',(3.37526125240075,-5.86818672274897,-35.6368433467236));
#38819=CARTESIAN_POINT('Ctrl Pts',(3.53638564474794,-5.76942506421747,-35.627930799526));
#38820=CARTESIAN_POINT('Ctrl Pts',(3.6978658154893,-5.67044533029858,-35.6189985725537));
#38821=CARTESIAN_POINT('Ctrl Pts',(3.8550666747862,-5.56475692654458,-35.6100663455815));
#38822=CARTESIAN_POINT('Ctrl Pts',(4.00746403775423,-5.45275352332256,-35.6011341186092));
#38823=CARTESIAN_POINT('Ctrl Pts',(4.15149714397457,-5.34689737358918,-35.5926921326639));
#38824=CARTESIAN_POINT('Ctrl Pts',(4.29123969267153,-5.23540085759743,-35.5842501467186));
#38825=CARTESIAN_POINT('Ctrl Pts',(4.42627796346352,-5.11862797926918,-35.5758081607733));
#38826=CARTESIAN_POINT('Ctrl Pts',(4.55782891504988,-5.00487072235626,-35.5675841863557));
#38827=CARTESIAN_POINT('Ctrl Pts',(4.68516603952161,-4.88588801639151,-35.5593602119381));
#38828=CARTESIAN_POINT('Ctrl Pts',(4.80784948061873,-4.76202397849006,-35.5511362375206));
#38829=CARTESIAN_POINT('Ctrl Pts',(4.93040335609873,-4.63829075303049,-35.5429209484179));
#38830=CARTESIAN_POINT('Ctrl Pts',(5.04831308484545,-4.50968671395908,-35.5347056593153));
#38831=CARTESIAN_POINT('Ctrl Pts',(5.16117197961678,-4.37659602851561,-35.5264903702126));
#38832=CARTESIAN_POINT('Ctrl Pts',(5.27393432153411,-4.24361920459406,-35.5182821094404));
#38833=CARTESIAN_POINT('Ctrl Pts',(5.38165420473158,-4.10616365083521,-35.5100738486682));
#38834=CARTESIAN_POINT('Ctrl Pts',(5.48396185591917,-3.9646502194801,-35.5018655878961));
#38835=CARTESIAN_POINT('Ctrl Pts',(5.58620249592566,-3.82322947896547,-35.4936627035082));
#38836=CARTESIAN_POINT('Ctrl Pts',(5.68303775583713,-3.67775644467268,-35.4854598191203));
#38837=CARTESIAN_POINT('Ctrl Pts',(5.77413817168248,-3.52868493554176,-35.4772569347324));
#38838=CARTESIAN_POINT('Ctrl Pts',(5.86519718091487,-3.37968118182362,-35.4690577786882));
#38839=CARTESIAN_POINT('Ctrl Pts',(5.95052635246151,-3.22708251709033,-35.460858622644));
#38840=CARTESIAN_POINT('Ctrl Pts',(6.02983954427082,-3.07137169198843,-35.4526594665998));
#38841=CARTESIAN_POINT('Ctrl Pts',(6.10914583776106,-2.91567440994198,-35.4444610236827));
#38842=CARTESIAN_POINT('Ctrl Pts',(6.18243702350282,-2.75686582210234,-35.4362625807657));
#38843=CARTESIAN_POINT('Ctrl Pts',(6.24947276527891,-2.59545355497592,-35.4280641378487));
#38844=CARTESIAN_POINT('Ctrl Pts',(6.31650783945839,-2.43404289532458,-35.4198657765785));
#38845=CARTESIAN_POINT('Ctrl Pts',(6.37728745520165,-2.27002893889326,-35.4116674153083));
#38846=CARTESIAN_POINT('Ctrl Pts',(6.43161936994523,-2.10393946684437,-35.403469054038));
#38847=CARTESIAN_POINT('Ctrl Pts',(6.48596061338865,-1.937821477508,-35.3952692851228));
#38848=CARTESIAN_POINT('Ctrl Pts',(6.53385183871864,-1.76962760350437,-35.3870695162075));
#38849=CARTESIAN_POINT('Ctrl Pts',(6.57515062560832,-1.59990101273879,-35.3788697472922));
#38850=CARTESIAN_POINT('Ctrl Pts',(6.61646400572987,-1.43011444782673,-35.3706670809279));
#38851=CARTESIAN_POINT('Ctrl Pts',(6.65118022228053,-1.25879443559642,-35.3624644145636));
#38852=CARTESIAN_POINT('Ctrl Pts',(6.67920792109747,-1.08649461422909,-35.3542617481993));
#38853=CARTESIAN_POINT('Ctrl Pts',(6.70726745237469,-0.91399910333133,-35.3460497656563));
#38854=CARTESIAN_POINT('Ctrl Pts',(6.72862323197611,-0.740521914505824,
-35.3378377831133));
#38855=CARTESIAN_POINT('Ctrl Pts',(6.74323566301143,-0.566623149095401,
-35.3296258005702));
#38856=CARTESIAN_POINT('Ctrl Pts',(6.75785671265607,-0.392621815842825,
-35.3214089744889));
#38857=CARTESIAN_POINT('Ctrl Pts',(6.76572646938014,-0.218198768086149,
-35.3131921484076));
#38858=CARTESIAN_POINT('Ctrl Pts',(6.76685750815821,-0.043914283358825,
-35.3049753223263));
#38859=CARTESIAN_POINT('Ctrl Pts',(6.76799029116142,0.130638973215197,-35.2967458247125));
#38860=CARTESIAN_POINT('Ctrl Pts',(6.76236360065717,0.305052881495234,-35.2885163270986));
#38861=CARTESIAN_POINT('Ctrl Pts',(6.7500420401126,0.478770776794607,-35.2802868294848));
#38862=CARTESIAN_POINT('Ctrl Pts',(6.73905912604876,0.633615506772126,-35.2729514059599));
#38863=CARTESIAN_POINT('Ctrl Pts',(6.72275777400732,0.78790716291095,-35.2656159824351));
#38864=CARTESIAN_POINT('Ctrl Pts',(6.70121782300113,0.941259097534815,-35.2582805589102));
#38865=CARTESIAN_POINT('Ctrl Pts',(6.67751751762014,1.10999149995793,-35.250209427384));
#38866=CARTESIAN_POINT('Ctrl Pts',(6.64739683500269,1.27813628400426,-35.2421382958579));
#38867=CARTESIAN_POINT('Ctrl Pts',(6.61088632372678,1.44515432212698,-35.2340671643317));
#38868=CARTESIAN_POINT('Ctrl Pts',(6.57442149695097,1.61196337562268,-35.2260061319687));
#38869=CARTESIAN_POINT('Ctrl Pts',(6.53158282944332,1.77764812867464,-35.2179450996057));
#38870=CARTESIAN_POINT('Ctrl Pts',(6.48245267133049,1.94167359871843,-35.2098840672426));
#38871=CARTESIAN_POINT('Ctrl Pts',(6.43337321381493,2.10552980023922,-35.2018313535818));
#38872=CARTESIAN_POINT('Ctrl Pts',(6.37801529274396,2.26772977208575,-35.193778639921));
#38873=CARTESIAN_POINT('Ctrl Pts',(6.31651243020506,2.4277478697478,-35.1857259262602));
#38874=CARTESIAN_POINT('Ctrl Pts',(6.25505956869748,2.5876358747673,-35.1776797593514));
#38875=CARTESIAN_POINT('Ctrl Pts',(6.18747184257628,2.74534518985611,-35.1696335924426));
#38876=CARTESIAN_POINT('Ctrl Pts',(6.11393278631222,2.90036461233007,-35.1615874255338));
#38877=CARTESIAN_POINT('Ctrl Pts',(6.04043742973722,3.05529191639912,-35.1535460399617));
#38878=CARTESIAN_POINT('Ctrl Pts',(5.96099794307738,3.20753217389843,-35.1455046543896));
#38879=CARTESIAN_POINT('Ctrl Pts',(5.87584619560389,3.35659358362124,-35.1374632688175));
#38880=CARTESIAN_POINT('Ctrl Pts',(5.79071677786396,3.50561590428644,-35.1294239919749));
#38881=CARTESIAN_POINT('Ctrl Pts',(5.69987826131055,3.65146071018358,-35.1213847151323));
#38882=CARTESIAN_POINT('Ctrl Pts',(5.60360876930624,3.79366020625916,-35.1133454382897));
#38883=CARTESIAN_POINT('Ctrl Pts',(5.50734934030068,3.9358448382971,-35.1053070017884));
#38884=CARTESIAN_POINT('Ctrl Pts',(5.40566027432216,4.0743846093166,-35.0972685652871));
#38885=CARTESIAN_POINT('Ctrl Pts',(5.29886326791086,4.20884034717225,-35.0892301287858));
#38886=CARTESIAN_POINT('Ctrl Pts',(5.19205628380869,4.34330864678251,-35.08119094128));
#38887=CARTESIAN_POINT('Ctrl Pts',(5.08014064171457,4.47369186142722,-35.0731517537742));
#38888=CARTESIAN_POINT('Ctrl Pts',(4.96347849765918,4.59958369890961,-35.0651125662683));
#38889=CARTESIAN_POINT('Ctrl Pts',(4.84678235582765,4.72551222389283,-35.057071035976));
#38890=CARTESIAN_POINT('Ctrl Pts',(4.72533721287457,4.84694649318234,-35.0490295056837));
#38891=CARTESIAN_POINT('Ctrl Pts',(4.59954214525066,4.96351700451031,-35.0409879753914));
#38892=CARTESIAN_POINT('Ctrl Pts',(4.4736185205672,5.08020664580457,-35.0329382270067));
#38893=CARTESIAN_POINT('Ctrl Pts',(4.34333636856366,5.19202235009193,-35.0248884786219));
#38894=CARTESIAN_POINT('Ctrl Pts',(4.20912845914178,5.29863441034034,-35.0168387302372));
#38895=CARTESIAN_POINT('Ctrl Pts',(4.07484461333391,5.40530679292441,-35.0087844272118));
#38896=CARTESIAN_POINT('Ctrl Pts',(3.93663088636786,5.50676944735738,-35.0007301241865));
#38897=CARTESIAN_POINT('Ctrl Pts',(3.7949486641671,5.60273626332138,-34.9926758211611));
#38898=CARTESIAN_POINT('Ctrl Pts',(3.65307088193487,5.69883553961285,-34.9846104010052));
#38899=CARTESIAN_POINT('Ctrl Pts',(3.50771536059478,5.78942363358591,-34.9765449808494));
#38900=CARTESIAN_POINT('Ctrl Pts',(3.35936841129851,5.87426019828623,-34.9684795606935));
#38901=CARTESIAN_POINT('Ctrl Pts',(3.27357526868321,5.92332352940866,-34.9638151052061));
#38902=CARTESIAN_POINT('Ctrl Pts',(3.18678200517044,5.97046407269439,-34.9591506497187));
#38903=CARTESIAN_POINT('Ctrl Pts',(3.09908550384724,6.01564277861011,-34.9544861942313));
#38904=CARTESIAN_POINT('Ctrl Pts',(3.09908550384719,6.01564277861013,-36.9542436419538));
#38905=CARTESIAN_POINT('Ctrl Pts',(2.93373232018322,6.10082796552483,-36.9454941940545));
#38906=CARTESIAN_POINT('Ctrl Pts',(2.76486502144414,6.17919158180196,-36.9367447461552));
#38907=CARTESIAN_POINT('Ctrl Pts',(2.59305716434334,6.25046746591386,-36.927995298256));
#38908=CARTESIAN_POINT('Ctrl Pts',(2.42125069459268,6.3217427744723,-36.9192459210085));
#38909=CARTESIAN_POINT('Ctrl Pts',(2.24650397871046,6.3859303555783,-36.9104965437611));
#38910=CARTESIAN_POINT('Ctrl Pts',(2.06941053323762,6.44281220003542,-36.9017471665137));
#38911=CARTESIAN_POINT('Ctrl Pts',(1.89231845896672,6.49969360406689,-36.8929978570111));
#38912=CARTESIAN_POINT('Ctrl Pts',(1.71287996431492,6.54926929700884,-36.8842485475085));
#38913=CARTESIAN_POINT('Ctrl Pts',(1.53170449173489,6.59137090065482,-36.8754992380059));
#38914=CARTESIAN_POINT('Ctrl Pts',(1.3505303617816,6.63347219230085,-36.8667499933413));
#38915=CARTESIAN_POINT('Ctrl Pts',(1.16761955878839,6.66809944062455,-36.8580007486767));
#38916=CARTESIAN_POINT('Ctrl Pts',(0.983593309310475,6.69513503985392,-36.8492515040122));
#38917=CARTESIAN_POINT('Ctrl Pts',(0.799568362459997,6.72217044771214,-36.840502321279));
#38918=CARTESIAN_POINT('Ctrl Pts',(0.61442826843864,6.74161427235977,-36.8317531385458));
#38919=CARTESIAN_POINT('Ctrl Pts',(0.428801816330342,6.75340047696802,-36.8230039558126));
#38920=CARTESIAN_POINT('Ctrl Pts',(0.243176616522986,6.76518660206241,-36.8142548321045));
#38921=CARTESIAN_POINT('Ctrl Pts',(0.0570653511657919,6.76931519233996,
-36.8055057083964));
#38922=CARTESIAN_POINT('Ctrl Pts',(-0.128899900799569,6.76577222610796,
-36.7967565846883));
#38923=CARTESIAN_POINT('Ctrl Pts',(-0.314863959941717,6.76222928260135,
-36.788007517099));
#38924=CARTESIAN_POINT('Ctrl Pts',(-0.500681721080533,6.75101488651278,
-36.7792584495097));
#38925=CARTESIAN_POINT('Ctrl Pts',(-0.685722110173307,6.73216712415991,
-36.7705093819204));
#38926=CARTESIAN_POINT('Ctrl Pts',(-0.870761373827663,6.71331947644145,
-36.7617603675441));
#38927=CARTESIAN_POINT('Ctrl Pts',(-1.05502298984352,6.68683858439995,-36.7530113531677));
#38928=CARTESIAN_POINT('Ctrl Pts',(-1.23788117676073,6.65281438131423,-36.7442623387914));
#38929=CARTESIAN_POINT('Ctrl Pts',(-1.43009641451808,6.61704912302374,-36.7350656279038));
#38930=CARTESIAN_POINT('Ctrl Pts',(-1.62076048992713,6.57294837083161,-36.7258689170163));
#38931=CARTESIAN_POINT('Ctrl Pts',(-1.80915798961151,6.52067760042044,-36.7166722061288));
#38932=CARTESIAN_POINT('Ctrl Pts',(-1.98840443003026,6.47094578577405,-36.7079222084223));
#38933=CARTESIAN_POINT('Ctrl Pts',(-2.165598959522,6.41381888474472,-36.6991722107158));
#38934=CARTESIAN_POINT('Ctrl Pts',(-2.34013966242325,6.34949095285233,-36.6904222130093));
#38935=CARTESIAN_POINT('Ctrl Pts',(-2.51467682554014,6.28516432556685,-36.6816723927577));
#38936=CARTESIAN_POINT('Ctrl Pts',(-2.68656000078837,6.21363705879663,-36.6729225725061));
#38937=CARTESIAN_POINT('Ctrl Pts',(-2.85520533840879,6.13515211510863,-36.6641727522545));
#38938=CARTESIAN_POINT('Ctrl Pts',(-3.02384747998321,6.05666865881124,-36.6554230978232));
#38939=CARTESIAN_POINT('Ctrl Pts',(-3.18925164684534,5.97122791039846,-36.646673443392));
#38940=CARTESIAN_POINT('Ctrl Pts',(-3.35085601829158,5.87912008251908,-36.6379237889607));
#38941=CARTESIAN_POINT('Ctrl Pts',(-3.51245754191427,5.78701387778169,-36.6291742887176));
#38942=CARTESIAN_POINT('Ctrl Pts',(-3.67025915510954,5.68824097060971,-36.6204247884744));
#38943=CARTESIAN_POINT('Ctrl Pts',(-3.8237248792886,5.58313684656837,-36.6116752882313));
#38944=CARTESIAN_POINT('Ctrl Pts',(-3.97718810300834,5.47803443501747,-36.6029259305462));
#38945=CARTESIAN_POINT('Ctrl Pts',(-4.12631534263071,5.36660117496341,-36.5941765728611));
#38946=CARTESIAN_POINT('Ctrl Pts',(-4.27060009886279,5.24921554097306,-36.5854272151759));
#38947=CARTESIAN_POINT('Ctrl Pts',(-4.41488269594255,5.13183166360255,-36.5766779884208));
#38948=CARTESIAN_POINT('Ctrl Pts',(-4.55432273235118,5.00849577139443,-36.5679287616656));
#38949=CARTESIAN_POINT('Ctrl Pts',(-4.68844662480226,4.87962675277325,-36.5591795349104));
#38950=CARTESIAN_POINT('Ctrl Pts',(-4.8225686883517,4.75075949139869,-36.5504304274589));
#38951=CARTESIAN_POINT('Ctrl Pts',(-4.95137454637869,4.61635945312518,-36.5416813200074));
#38952=CARTESIAN_POINT('Ctrl Pts',(-5.07442674461079,4.47688309134589,-36.5329322125559));
#38953=CARTESIAN_POINT('Ctrl Pts',(-5.19747742838539,4.33740844616351,-36.5241832127836));
#38954=CARTESIAN_POINT('Ctrl Pts',(-5.31477440450927,4.19285781736029,-36.5154342130112));
#38955=CARTESIAN_POINT('Ctrl Pts',(-5.42591931531152,4.04372211999407,-36.5066852132388));
#38956=CARTESIAN_POINT('Ctrl Pts',(-5.53707636462979,3.89457013500804,-36.4979352579582));
#38957=CARTESIAN_POINT('Ctrl Pts',(-5.64207983273467,3.74083230916426,-36.4891853026777));
#38958=CARTESIAN_POINT('Ctrl Pts',(-5.74057303468742,3.58303087251836,-36.4804353473971));
#38959=CARTESIAN_POINT('Ctrl Pts',(-5.83906243363762,3.42523552887436,-36.4716857299683));
#38960=CARTESIAN_POINT('Ctrl Pts',(-5.93104191768424,3.26337713156995,-36.4629361125395));
#38961=CARTESIAN_POINT('Ctrl Pts',(-6.01619906699656,3.09800545291155,-36.4541864951107));
#38962=CARTESIAN_POINT('Ctrl Pts',(-6.10135338095374,2.93263928039612,-36.4454371690053));
#38963=CARTESIAN_POINT('Ctrl Pts',(-6.17968568352823,2.76376031540258,-36.4366878428999));
#38964=CARTESIAN_POINT('Ctrl Pts',(-6.25092992694864,2.59194213831594,-36.4279385167945));
#38965=CARTESIAN_POINT('Ctrl Pts',(-6.32217217691082,2.42012876880875,-36.4191894355007));
#38966=CARTESIAN_POINT('Ctrl Pts',(-6.3863266548383,2.24537661647729,-36.4104403542069));
#38967=CARTESIAN_POINT('Ctrl Pts',(-6.4431754786933,2.06827917621518,-36.4016912729131));
#38968=CARTESIAN_POINT('Ctrl Pts',(-6.5000294423592,1.8911657242348,-36.3929414005982));
#38969=CARTESIAN_POINT('Ctrl Pts',(-6.54957634250385,1.7117068328925,-36.3841915282832));
#38970=CARTESIAN_POINT('Ctrl Pts',(-6.59164787708384,1.53051209225411,-36.3754416559682));
#38971=CARTESIAN_POINT('Ctrl Pts',(-6.63371649075002,1.34932993148067,-36.3666923911334));
#38972=CARTESIAN_POINT('Ctrl Pts',(-6.6683107125712,1.1664124417403,-36.3579431262987));
#38973=CARTESIAN_POINT('Ctrl Pts',(-6.69531304840331,0.982380875160164,
-36.3491938614639));
#38974=CARTESIAN_POINT('Ctrl Pts',(-6.72231677033043,0.798339861795949,
-36.3404441475082));
#38975=CARTESIAN_POINT('Ctrl Pts',(-6.74172778477889,0.613184940730217,
-36.3316944335525));
#38976=CARTESIAN_POINT('Ctrl Pts',(-6.75348015835518,0.42754502769057,-36.3229447195969));
#38977=CARTESIAN_POINT('Ctrl Pts',(-6.7624903836522,0.285219953547091,-36.3162365517946));
#38978=CARTESIAN_POINT('Ctrl Pts',(-6.76699999999999,0.142609995757826,
-36.3095283839923));
#38979=CARTESIAN_POINT('Ctrl Pts',(-6.767,6.92579744391243E-13,-36.30282021619));
#38980=CARTESIAN_POINT('',(-6.766998182033,0.00496027842551228,-36.697179783844));
#38981=CARTESIAN_POINT('Ctrl Pts',(3.09908550384721,6.01564277861012,-37.3484709211107));
#38982=CARTESIAN_POINT('Ctrl Pts',(2.93573755334438,6.09979492728598,-37.3398551787245));
#38983=CARTESIAN_POINT('Ctrl Pts',(2.76887746110941,6.17733142416523,-37.3312394363382));
#38984=CARTESIAN_POINT('Ctrl Pts',(2.59908859426785,6.24796186601253,-37.3226236939519));
#38985=CARTESIAN_POINT('Ctrl Pts',(2.42929972742626,6.31859230785985,-37.3140079515656));
#38986=CARTESIAN_POINT('Ctrl Pts',(2.25658249603023,6.38231650272491,-37.3053922091793));
#38987=CARTESIAN_POINT('Ctrl Pts',(2.08154640978273,6.43890157899006,-37.296776466793));
#38988=CARTESIAN_POINT('Ctrl Pts',(1.90157407836224,6.49708242796451,-37.2879177492713));
#38989=CARTESIAN_POINT('Ctrl Pts',(1.71933738879032,6.54765666396894,-37.2790590317495));
#38990=CARTESIAN_POINT('Ctrl Pts',(1.53547637484139,6.59049325182144,-37.2702003142278));
#38991=CARTESIAN_POINT('Ctrl Pts',(1.35127138646322,6.63340998005031,-37.2613250234683));
#38992=CARTESIAN_POINT('Ctrl Pts',(1.16543625335621,6.66856007218692,-37.2524497327088));
#38993=CARTESIAN_POINT('Ctrl Pts',(0.978619236211917,6.69586390173188,-37.2435744419492));
#38994=CARTESIAN_POINT('Ctrl Pts',(0.791271616735659,6.72324528029164,-37.2346739433685));
#38995=CARTESIAN_POINT('Ctrl Pts',(0.602936790772713,6.74273576320412,-37.2257734447877));
#38996=CARTESIAN_POINT('Ctrl Pts',(0.414269250765005,6.75430751357018,-37.2168729462069));
#38997=CARTESIAN_POINT('Ctrl Pts',(0.225346311255239,6.76589492863024,-37.2079603990093));
#38998=CARTESIAN_POINT('Ctrl Pts',(0.0360900172276769,6.76954218877923,
-37.1990478518116));
#38999=CARTESIAN_POINT('Ctrl Pts',(-0.152845724085443,6.76527362230301,
-37.190135304614));
#39000=CARTESIAN_POINT('Ctrl Pts',(-0.342198653966852,6.76099563041514,
-37.1812030776417));
#39001=CARTESIAN_POINT('Ctrl Pts',(-0.531229355054916,6.74876685705625,
-37.1722708506695));
#39002=CARTESIAN_POINT('Ctrl Pts',(-0.719286747375817,6.72866372878371,
-37.1633386236972));
#39003=CARTESIAN_POINT('Ctrl Pts',(-0.897022699205253,6.70966395114046,
-37.154896637752));
#39004=CARTESIAN_POINT('Ctrl Pts',(-1.07388913092905,6.68363092743483,-37.1464546518068));
#39005=CARTESIAN_POINT('Ctrl Pts',(-1.24934535075696,6.65067103340272,-37.1380126658615));
#39006=CARTESIAN_POINT('Ctrl Pts',(-1.42027047105775,6.61856231786066,-37.129788691444));
#39007=CARTESIAN_POINT('Ctrl Pts',(-1.59018359197934,6.57981752561607,-37.1215647170264));
#39008=CARTESIAN_POINT('Ctrl Pts',(-1.75853144301131,6.53451269521611,-37.1133407426088));
#39009=CARTESIAN_POINT('Ctrl Pts',(-1.92670150237886,6.4892557111127,-37.1051254535062));
#39010=CARTESIAN_POINT('Ctrl Pts',(-2.09330924027813,6.43745257732025,-37.0969101644035));
#39011=CARTESIAN_POINT('Ctrl Pts',(-2.25780989650979,6.37923063317376,-37.0886948753009));
#39012=CARTESIAN_POINT('Ctrl Pts',(-2.42216981941357,6.32105849896811,-37.0804866145287));
#39013=CARTESIAN_POINT('Ctrl Pts',(-2.58442591466463,6.25647861007735,-37.0722783537565));
#39014=CARTESIAN_POINT('Ctrl Pts',(-2.74404686196727,6.18566858304966,-37.0640700929843));
#39015=CARTESIAN_POINT('Ctrl Pts',(-2.90356325806401,6.1149049363614,-37.0558672085965));
#39016=CARTESIAN_POINT('Ctrl Pts',(-3.06044761763232,6.0379194247961,-37.0476643242087));
#39017=CARTESIAN_POINT('Ctrl Pts',(-3.21418686550801,5.95493843743122,-37.0394614398208));
#39018=CARTESIAN_POINT('Ctrl Pts',(-3.36785623640807,5.87199516626771,-37.0312622837766));
#39019=CARTESIAN_POINT('Ctrl Pts',(-3.51838302864861,5.78306201827077,-37.0230631277325));
#39020=CARTESIAN_POINT('Ctrl Pts',(-3.6652770460092,5.68841218408073,-37.0148639716883));
#39021=CARTESIAN_POINT('Ctrl Pts',(-3.81215828716303,5.59377058212419,-37.0066655287713));
#39022=CARTESIAN_POINT('Ctrl Pts',(-3.95540707695803,5.49341347125853,-36.9984670858543));
#39023=CARTESIAN_POINT('Ctrl Pts',(-4.09456028555036,5.38765858866296,-36.9902686429373));
#39024=CARTESIAN_POINT('Ctrl Pts',(-4.23371210834143,5.28190475926086,-36.9820702816671));
#39025=CARTESIAN_POINT('Ctrl Pts',(-4.36876814494653,5.17075348139762,-36.9738719203968));
#39026=CARTESIAN_POINT('Ctrl Pts',(-4.49929668468071,5.0545641101109,-36.9656735591266));
#39027=CARTESIAN_POINT('Ctrl Pts',(-4.62984763594943,4.93835478930116,-36.9574737902113));
#39028=CARTESIAN_POINT('Ctrl Pts',(-4.75586927367679,4.8171058901698,-36.949274021296));
#39029=CARTESIAN_POINT('Ctrl Pts',(-4.87696519934859,4.69121513515878,-36.9410742523807));
#39030=CARTESIAN_POINT('Ctrl Pts',(-4.99810391516209,4.56527989571762,-36.9328715860164));
#39031=CARTESIAN_POINT('Ctrl Pts',(-5.11431320322787,4.43469979137637,-36.924668919652));
#39032=CARTESIAN_POINT('Ctrl Pts',(-5.22523552614307,4.29990728927175,-36.9164662532877));
#39033=CARTESIAN_POINT('Ctrl Pts',(-5.3362838290913,4.16496169657707,-36.9082542707447));
#39034=CARTESIAN_POINT('Ctrl Pts',(-5.44203294257358,4.0257944254142,-36.9000422882016));
#39035=CARTESIAN_POINT('Ctrl Pts',(-5.54216680392175,3.88286957255942,-36.8918303056586));
#39036=CARTESIAN_POINT('Ctrl Pts',(-5.64235972557483,3.73986042069455,-36.8836134795773));
#39037=CARTESIAN_POINT('Ctrl Pts',(-5.73693059923295,3.593089570335,-36.875396653496));
#39038=CARTESIAN_POINT('Ctrl Pts',(-5.82560835885852,3.44304752351718,-36.8671798274147));
#39039=CARTESIAN_POINT('Ctrl Pts',(-5.91442287239662,3.29277409019349,-36.8589503298008));
#39040=CARTESIAN_POINT('Ctrl Pts',(-5.99732594044969,3.13921969476663,-36.850720832187));
#39041=CARTESIAN_POINT('Ctrl Pts',(-6.07409327636515,2.98289789802059,-36.8424913345731));
#39042=CARTESIAN_POINT('Ctrl Pts',(-6.14252040864462,2.84355930906805,-36.8351559110483));
#39043=CARTESIAN_POINT('Ctrl Pts',(-6.20607320552896,2.70202241903317,-36.8278204875234));
#39044=CARTESIAN_POINT('Ctrl Pts',(-6.26462609939512,2.55866153189076,-36.8204850639985));
#39045=CARTESIAN_POINT('Ctrl Pts',(-6.3371380022418,2.38112341149918,-36.8114008756202));
#39046=CARTESIAN_POINT('Ctrl Pts',(-6.40218349129019,2.20029400097097,-36.8023166872419));
#39047=CARTESIAN_POINT('Ctrl Pts',(-6.45947873997281,2.01678541442548,-36.7932324988636));
#39048=CARTESIAN_POINT('Ctrl Pts',(-6.51649563618737,1.834168351508,-36.7841924433988));
#39049=CARTESIAN_POINT('Ctrl Pts',(-6.56583729367326,1.64889827935473,-36.7751523879341));
#39050=CARTESIAN_POINT('Ctrl Pts',(-6.60726903101154,1.46160355494775,-36.7661123324693));
#39051=CARTESIAN_POINT('Ctrl Pts',(-6.64857467197834,1.27487885696642,-36.7570997901687));
#39052=CARTESIAN_POINT('Ctrl Pts',(-6.68201834175108,1.08614201070574,-36.7480872478681));
#39053=CARTESIAN_POINT('Ctrl Pts',(-6.70741420988106,0.896037731954226,
-36.7390747055675));
#39054=CARTESIAN_POINT('Ctrl Pts',(-6.73268694761279,0.706855162806453,
-36.7301058600572));
#39055=CARTESIAN_POINT('Ctrl Pts',(-6.74998963237898,0.516318601169058,
-36.7211370145468));
#39056=CARTESIAN_POINT('Ctrl Pts',(-6.75918712047647,0.325082251722556,
-36.7121681690365));
#39057=CARTESIAN_POINT('Ctrl Pts',(-6.76431061506854,0.218553339501031,
-36.707172040639));
#39058=CARTESIAN_POINT('Ctrl Pts',(-6.76691986186397,0.111807595444429,
-36.7021759122415));
#39059=CARTESIAN_POINT('Ctrl Pts',(-6.766998182033,0.00496027842553114,
-36.697179783844));
#39060=CARTESIAN_POINT('Ctrl Pts',(-6.76699818203353,0.00496027770000192,
-36.6971797838101));
#39061=CARTESIAN_POINT('Ctrl Pts',(-6.76712516176854,-0.168270272665018,
-36.6890796078194));
#39062=CARTESIAN_POINT('Ctrl Pts',(-6.76059593780152,-0.341532716517958,
-36.6809794318287));
#39063=CARTESIAN_POINT('Ctrl Pts',(-6.74742994385826,-0.514274394389723,
-36.672879255838));
#39064=CARTESIAN_POINT('Ctrl Pts',(-6.73426271426744,-0.687032284317682,
-36.6647783196341));
#39065=CARTESIAN_POINT('Ctrl Pts',(-6.71445750083666,-0.85926894536719,
-36.6566773834301));
#39066=CARTESIAN_POINT('Ctrl Pts',(-6.68808571516971,-1.03043605650368,
-36.6485764472262));
#39067=CARTESIAN_POINT('Ctrl Pts',(-6.66170642162143,-1.20165189783899,
-36.6404732047368));
#39068=CARTESIAN_POINT('Ctrl Pts',(-6.62875688817058,-1.37179722067042,
-36.6323699622473));
#39069=CARTESIAN_POINT('Ctrl Pts',(-6.58935981068275,-1.54033317349169,
-36.6242667197578));
#39070=CARTESIAN_POINT('Ctrl Pts',(-6.54994399759125,-1.70894927496912,
-36.6161596237049));
#39071=CARTESIAN_POINT('Ctrl Pts',(-6.50407461742164,-1.87595412586907,
-36.6080525276519));
#39072=CARTESIAN_POINT('Ctrl Pts',(-6.45192443716212,-2.04082337725494,
-36.599945431599));
#39073=CARTESIAN_POINT('Ctrl Pts',(-6.39970252262244,-2.20591941169334,
-36.59182718397));
#39074=CARTESIAN_POINT('Ctrl Pts',(-6.34118266034671,-2.36887362892636,
-36.5837089363411));
#39075=CARTESIAN_POINT('Ctrl Pts',(-6.27658645573511,-2.52917999827663,
-36.5755906887121));
#39076=CARTESIAN_POINT('Ctrl Pts',(-6.2119444340683,-2.68960007037182,-36.5674666829399));
#39077=CARTESIAN_POINT('Ctrl Pts',(-6.14121763327434,-2.8473682199109,-36.5593426771676));
#39078=CARTESIAN_POINT('Ctrl Pts',(-6.06467380902991,-3.00200276316772,
-36.5512186713954));
#39079=CARTESIAN_POINT('Ctrl Pts',(-5.9879908607999,-3.15691836598982,-36.5430798996499));
#39080=CARTESIAN_POINT('Ctrl Pts',(-5.90546993777691,-3.30868866097301,
-36.5349411279045));
#39081=CARTESIAN_POINT('Ctrl Pts',(-5.81742309480156,-3.45685949035675,
-36.526802356159));
#39082=CARTESIAN_POINT('Ctrl Pts',(-5.73143683440478,-3.60156264027164,
-36.5188540581511));
#39083=CARTESIAN_POINT('Ctrl Pts',(-5.64018065764468,-3.74283271596098,
-36.5109057601433));
#39084=CARTESIAN_POINT('Ctrl Pts',(-5.54398136462814,-3.88027829268159,
-36.5029574621355));
#39085=CARTESIAN_POINT('Ctrl Pts',(-5.44311577373594,-4.02439088308348,
-36.4946236194428));
#39086=CARTESIAN_POINT('Ctrl Pts',(-5.33649843438387,-4.16475245015001,
-36.4862897767501));
#39087=CARTESIAN_POINT('Ctrl Pts',(-5.22443389202061,-4.30088124782659,
-36.4779559340574));
#39088=CARTESIAN_POINT('Ctrl Pts',(-5.11250143189811,-4.43684960049309,
-36.4696319138527));
#39089=CARTESIAN_POINT('Ctrl Pts',(-4.99513477761626,-4.56859485575408,
-36.4613078936479));
#39090=CARTESIAN_POINT('Ctrl Pts',(-4.87268163256819,-4.6956642456241,-36.4529838734432));
#39091=CARTESIAN_POINT('Ctrl Pts',(-4.75035036243681,-4.8226071661307,-36.4446681379523));
#39092=CARTESIAN_POINT('Ctrl Pts',(-4.6229429275459,-4.94488324422499,-36.4363524024615));
#39093=CARTESIAN_POINT('Ctrl Pts',(-4.49084730340559,-5.06207264838177,
-36.4280366669706));
#39094=CARTESIAN_POINT('Ctrl Pts',(-4.35885894779976,-5.17916688863193,
-36.4197276842905));
#39095=CARTESIAN_POINT('Ctrl Pts',(-4.22219024794498,-5.2911824558007,-36.4114187016105));
#39096=CARTESIAN_POINT('Ctrl Pts',(-4.08126619978474,-5.39773611864221,
-36.4031097189304));
#39097=CARTESIAN_POINT('Ctrl Pts',(-3.9404307825521,-5.5042227670167,-36.3948059619933));
#39098=CARTESIAN_POINT('Ctrl Pts',(-3.79534562727522,-5.60525414773612,
-36.3865022050561));
#39099=CARTESIAN_POINT('Ctrl Pts',(-3.64646916298839,-5.7004869654596,-36.3781984481189));
#39100=CARTESIAN_POINT('Ctrl Pts',(-3.49765313895715,-5.79568112095482,
-36.3698980623069));
#39101=CARTESIAN_POINT('Ctrl Pts',(-3.34504916538819,-5.88508121700561,
-36.3615976764949));
#39102=CARTESIAN_POINT('Ctrl Pts',(-3.18914527362632,-5.96838683596388,
-36.3532972906829));
#39103=CARTESIAN_POINT('Ctrl Pts',(-3.03327425793842,-6.05167488793481,
-36.3449986552062));
#39104=CARTESIAN_POINT('Ctrl Pts',(-2.87410501696344,-6.12887085936584,
-36.3367000197296));
#39105=CARTESIAN_POINT('Ctrl Pts',(-2.7121510537312,-6.19971980509964,-36.3284013842529));
#39106=CARTESIAN_POINT('Ctrl Pts',(-2.5502043598772,-6.27056557074588,-36.3201031212644));
#39107=CARTESIAN_POINT('Ctrl Pts',(-2.38547351152884,-6.33506473918674,
-36.3118048582758));
#39108=CARTESIAN_POINT('Ctrl Pts',(-2.21849307800729,-6.39301004714006,
-36.3035065952872));
#39109=CARTESIAN_POINT('Ctrl Pts',(-2.0514924238677,-6.45096237202294,-36.2952073274144));
#39110=CARTESIAN_POINT('Ctrl Pts',(-1.88224197047683,-6.50235914154458,
-36.2869080595416));
#39111=CARTESIAN_POINT('Ctrl Pts',(-1.71129275473856,-6.54704254664496,
-36.2786087916688));
#39112=CARTESIAN_POINT('Ctrl Pts',(-1.54022350509793,-6.59175732669761,
-36.2703036963723));
#39113=CARTESIAN_POINT('Ctrl Pts',(-1.36745344656601,-6.62974923514353,
-36.2619986010758));
#39114=CARTESIAN_POINT('Ctrl Pts',(-1.19354603792688,-6.66091111300467,
-36.2536935057793));
#39115=CARTESIAN_POINT('Ctrl Pts',(-1.01957521360319,-6.69208435410693,
-36.2453853820132));
#39116=CARTESIAN_POINT('Ctrl Pts',(-0.844466556129819,-6.71642254649862,
-36.237077258247));
#39117=CARTESIAN_POINT('Ctrl Pts',(-0.668790248606514,-6.73387025442047,
-36.2287691344809));
#39118=CARTESIAN_POINT('Ctrl Pts',(-0.49292719818365,-6.75133650915501,
-36.2204521792273));
#39119=CARTESIAN_POINT('Ctrl Pts',(-0.316495639097168,-6.76189761811846,
-36.2121352239736));
#39120=CARTESIAN_POINT('Ctrl Pts',(-0.140068470103331,-6.76555022327696,
-36.2038182687199));
#39121=CARTESIAN_POINT('Ctrl Pts',(-0.0100443308303591,-6.76824213770571,
-36.1976887992374));
#39122=CARTESIAN_POINT('Ctrl Pts',(0.11997738168582,-6.7671828108584,-36.191559329755));
#39123=CARTESIAN_POINT('Ctrl Pts',(0.24976870186275,-6.76238897103456,-36.1854298602725));
#39124=CARTESIAN_POINT('Ctrl Pts',(0.428718854614736,-6.75577945070935,
-36.1769788367473));
#39125=CARTESIAN_POINT('Ctrl Pts',(0.607557888684686,-6.74205679406928,
-36.1685278132221));
#39126=CARTESIAN_POINT('Ctrl Pts',(0.785697601848088,-6.7212326457615,-36.1600767896969));
#39127=CARTESIAN_POINT('Ctrl Pts',(0.963680468288821,-6.70042683249737,
-36.1516332070468));
#39128=CARTESIAN_POINT('Ctrl Pts',(1.14096491337727,-6.67253202859512,-36.1431896243966));
#39129=CARTESIAN_POINT('Ctrl Pts',(1.31696544471025,-6.63761184594573,-36.1347460417465));
#39130=CARTESIAN_POINT('Ctrl Pts',(1.49283493816366,-6.6027176624604,-36.1263087456067));
#39131=CARTESIAN_POINT('Ctrl Pts',(1.66742209934474,-6.56080859150973,-36.1178714494669));
#39132=CARTESIAN_POINT('Ctrl Pts',(1.84014885509666,-6.51199978432789,-36.1094341533271));
#39133=CARTESIAN_POINT('Ctrl Pts',(2.01275238347909,-6.46322579850821,-36.1010028765548));
#39134=CARTESIAN_POINT('Ctrl Pts',(2.18349783564774,-6.40756198500263,-36.0925715997824));
#39135=CARTESIAN_POINT('Ctrl Pts',(2.35181938481972,-6.34517411748379,-36.0841403230101));
#39136=CARTESIAN_POINT('Ctrl Pts',(2.5200687852818,-6.28281299166367,-36.0757126601882));
#39137=CARTESIAN_POINT('Ctrl Pts',(2.68589604373395,-6.21373367256571,-36.0672849973664));
#39138=CARTESIAN_POINT('Ctrl Pts',(2.84875187271498,-6.13815133144361,-36.0588573345445));
#39139=CARTESIAN_POINT('Ctrl Pts',(3.01155756823131,-6.06259225755519,-36.0504322660905));
#39140=CARTESIAN_POINT('Ctrl Pts',(3.1713933581389,-5.98053429329852,-36.0420071976366));
#39141=CARTESIAN_POINT('Ctrl Pts',(3.32773093316721,-5.89224030708542,-36.0335821291826));
#39142=CARTESIAN_POINT('Ctrl Pts',(3.37050967906797,-5.86808036984646,-36.0312767725687));
#39143=CARTESIAN_POINT('Ctrl Pts',(3.4130266334959,-5.84345378856547,-36.0289714159548));
#39144=CARTESIAN_POINT('Ctrl Pts',(3.45527128580487,-5.81836655269264,-36.026666059341));
#39145=CARTESIAN_POINT('Ctrl Pts',(3.61321048327226,-5.72457342897485,-36.0180470708165));
#39146=CARTESIAN_POINT('Ctrl Pts',(3.76727095094069,-5.62437985373978,-36.009428082292));
#39147=CARTESIAN_POINT('Ctrl Pts',(3.91694543125652,-5.51813623323661,-36.0008090937675));
#39148=CARTESIAN_POINT('Ctrl Pts',(4.06670957994318,-5.41182896332346,-35.9921849416998));
#39149=CARTESIAN_POINT('Ctrl Pts',(4.21208224937313,-5.29946459076497,-35.983560789632));
#39150=CARTESIAN_POINT('Ctrl Pts',(4.35258785275091,-5.18143493485012,-35.9749366375642));
#39151=CARTESIAN_POINT('Ctrl Pts',(4.49790581084434,-5.05936273146688,-35.966017105968));
#39152=CARTESIAN_POINT('Ctrl Pts',(4.63801713464026,-4.93123053533874,-35.9570975743717));
#39153=CARTESIAN_POINT('Ctrl Pts',(4.77243614129764,-4.79751417686661,-35.9481780427755));
#39154=CARTESIAN_POINT('Ctrl Pts',(4.90264583778416,-4.66798512524732,-35.9395378249162));
#39155=CARTESIAN_POINT('Ctrl Pts',(5.02751415666685,-4.53321660773519,-35.930897607057));
#39156=CARTESIAN_POINT('Ctrl Pts',(5.14663957971879,-4.39367614150975,-35.9222573891977));
#39157=CARTESIAN_POINT('Ctrl Pts',(5.27154148334465,-4.24736925404713,-35.913198200733));
#39158=CARTESIAN_POINT('Ctrl Pts',(5.39012945090665,-4.09581642711831,-35.9041390122683));
#39159=CARTESIAN_POINT('Ctrl Pts',(5.50199036545045,-3.93959274779646,-35.8950798238035));
#39160=CARTESIAN_POINT('Ctrl Pts',(5.61385127999425,-3.7833690684746,-35.8860206353388));
#39161=CARTESIAN_POINT('Ctrl Pts',(5.71898495995174,-3.62247487518775,-35.8769614468741));
#39162=CARTESIAN_POINT('Ctrl Pts',(5.81703207616521,-3.45751743666826,-35.8679022584094));
#39163=CARTESIAN_POINT('Ctrl Pts',(5.91490933262873,-3.29284577533776,-35.8588587643532));
#39164=CARTESIAN_POINT('Ctrl Pts',(6.00581545573631,-3.12397366454647,-35.8498152702969));
#39165=CARTESIAN_POINT('Ctrl Pts',(6.08941893511293,-2.95148539428676,-35.8407717762406));
#39166=CARTESIAN_POINT('Ctrl Pts',(6.17294594269256,-2.77915489841738,-35.8317365542353));
#39167=CARTESIAN_POINT('Ctrl Pts',(6.24918353883517,-2.60321506095434,-35.82270133223));
#39168=CARTESIAN_POINT('Ctrl Pts',(6.31784655891654,-2.4242738826268,-35.8136661102246));
#39169=CARTESIAN_POINT('Ctrl Pts',(6.38638860970443,-2.24564795970009,-35.8046468063135));
#39170=CARTESIAN_POINT('Ctrl Pts',(6.44738264706108,-2.06403147680182,-35.7956275024024));
#39171=CARTESIAN_POINT('Ctrl Pts',(6.50059197864906,-1.88005130970501,-35.7866081984913));
#39172=CARTESIAN_POINT('Ctrl Pts',(6.55373455541437,-1.6963019585772,-35.7776002099269));
#39173=CARTESIAN_POINT('Ctrl Pts',(6.59911185095206,-1.51019506921802,-35.7685922213624));
#39174=CARTESIAN_POINT('Ctrl Pts',(6.63653645356359,-1.32237396394578,-35.759584232798));
#39175=CARTESIAN_POINT('Ctrl Pts',(6.67387653139898,-1.13497705921994,-35.7505965890913));
#39176=CARTESIAN_POINT('Ctrl Pts',(6.7032997225382,-0.9458738997491,-35.7416089453847));
#39177=CARTESIAN_POINT('Ctrl Pts',(6.72466936137,-0.755718850004144,-35.732621301678));
#39178=CARTESIAN_POINT('Ctrl Pts',(6.74328083565911,-0.590106981355902,
-35.7247936869446));
#39179=CARTESIAN_POINT('Ctrl Pts',(6.75578424925169,-0.42369755940464,-35.7169660722113));
#39180=CARTESIAN_POINT('Ctrl Pts',(6.76212065723859,-0.256930373734165,
-35.7091384574779));
#39181=CARTESIAN_POINT('Ctrl Pts',(6.76869630611822,-0.0838666348017703,
-35.7010152990326));
#39182=CARTESIAN_POINT('Ctrl Pts',(6.76862585696639,0.0895050961617428,
-35.6928921405873));
#39183=CARTESIAN_POINT('Ctrl Pts',(6.76190161212426,0.262632039079982,-35.684768982142));
#39184=CARTESIAN_POINT('Ctrl Pts',(6.7551778413766,0.435746775642425,-35.6766463964219));
#39185=CARTESIAN_POINT('Ctrl Pts',(6.74180122360032,0.60861639278875,-35.6685238107018));
#39186=CARTESIAN_POINT('Ctrl Pts',(6.72181615884099,0.780689776251874,-35.6604012249817));
#39187=CARTESIAN_POINT('Ctrl Pts',(6.70182869267044,0.952783836103028,-35.6522776632493));
#39188=CARTESIAN_POINT('Ctrl Pts',(6.67523124174807,1.12408110832392,-35.6441541015169));
#39189=CARTESIAN_POINT('Ctrl Pts',(6.64211987778535,1.29403729819843,-35.6360305397846));
#39190=CARTESIAN_POINT('Ctrl Pts',(6.60898439612312,1.46411728098961,-35.6279010610014));
#39191=CARTESIAN_POINT('Ctrl Pts',(6.56932559524705,1.63285387083436,-35.6197715822183));
#39192=CARTESIAN_POINT('Ctrl Pts',(6.52329046392428,1.79971401152366,-35.6116421034352));
#39193=CARTESIAN_POINT('Ctrl Pts',(6.47723656488886,1.96664217815496,-35.6035093104067));
#39194=CARTESIAN_POINT('Ctrl Pts',(6.42480126454203,2.13169202217281,-35.5953765173782));
#39195=CARTESIAN_POINT('Ctrl Pts',(6.36618083681926,2.2943475222632,-35.5872437243496));
#39196=CARTESIAN_POINT('Ctrl Pts',(6.30749666827451,2.45717988553384,-35.5791020881425));
#39197=CARTESIAN_POINT('Ctrl Pts',(6.24261407667555,2.61761236598165,-35.5709604519354));
#39198=CARTESIAN_POINT('Ctrl Pts',(6.17177699602401,2.77515003402498,-35.5628188157283));
#39199=CARTESIAN_POINT('Ctrl Pts',(6.13568646560412,2.8554133360767,-35.5586707626677));
#39200=CARTESIAN_POINT('Ctrl Pts',(6.09805102824434,2.93492560878375,-35.554522709607));
#39201=CARTESIAN_POINT('Ctrl Pts',(6.05890740362131,3.01362407648048,-35.5503746565464));
#39202=CARTESIAN_POINT('Ctrl Pts',(5.97926234502005,3.17375089488067,-35.5419346632583));
#39203=CARTESIAN_POINT('Ctrl Pts',(5.89320674020421,3.33083675555393,-35.5334946699701));
#39204=CARTESIAN_POINT('Ctrl Pts',(5.80099700859093,3.48435398694206,-35.5250546766819));
#39205=CARTESIAN_POINT('Ctrl Pts',(5.70885313141505,3.63776157924195,-35.5166207110765));
#39206=CARTESIAN_POINT('Ctrl Pts',(5.61056405831751,3.78760533720003,-35.5081867454711));
#39207=CARTESIAN_POINT('Ctrl Pts',(5.50643222722078,3.93338189437848,-35.4997527798657));
#39208=CARTESIAN_POINT('Ctrl Pts',(5.40236020939849,4.07907471757155,-35.4913236587261));
#39209=CARTESIAN_POINT('Ctrl Pts',(5.29245231666745,4.22070472623775,-35.4828945375865));
#39210=CARTESIAN_POINT('Ctrl Pts',(5.17705462422063,4.35779696840454,-35.474465416447));
#39211=CARTESIAN_POINT('Ctrl Pts',(5.06170710095617,4.49482960967679,-35.4660399598704));
#39212=CARTESIAN_POINT('Ctrl Pts',(4.94087475063419,4.62732816293984,-35.4576145032938));
#39213=CARTESIAN_POINT('Ctrl Pts',(4.81494453202444,4.75484996120046,-35.4491890467173));
#39214=CARTESIAN_POINT('Ctrl Pts',(4.6890396650411,4.88234608742599,-35.4407652863105));
#39215=CARTESIAN_POINT('Ctrl Pts',(4.55803920736126,5.00486721656025,-35.4323415259037));
#39216=CARTESIAN_POINT('Ctrl Pts',(4.42236802073555,5.12200645149687,-35.4239177654969));
#39217=CARTESIAN_POINT('Ctrl Pts',(4.28671878876183,5.23912673066845,-35.4154953682441));
#39218=CARTESIAN_POINT('Ctrl Pts',(4.14640058850214,5.35086663585823,-35.4070729709914));
#39219=CARTESIAN_POINT('Ctrl Pts',(4.00187264440221,5.45685846783525,-35.3986505737386));
#39220=CARTESIAN_POINT('Ctrl Pts',(3.85731176433453,5.5628744539202,-35.3902262571352));
#39221=CARTESIAN_POINT('Ctrl Pts',(3.70853949033344,5.66313954913234,-35.3818019405318));
#39222=CARTESIAN_POINT('Ctrl Pts',(3.55604606397443,5.75732797319138,-35.3733776239284));
#39223=CARTESIAN_POINT('Ctrl Pts',(3.4071144891321,5.84931639959086,-35.3651500775438));
#39224=CARTESIAN_POINT('Ctrl Pts',(3.25463392784788,5.93550872083648,-35.3569225311592));
#39225=CARTESIAN_POINT('Ctrl Pts',(3.0990855038472,6.01564277861013,-35.3486949847746));
#39226=CARTESIAN_POINT('Origin',(0.,0.,-63.6971797838103));
#39227=CARTESIAN_POINT('',(3.09908550384723,6.01564277861011,-32.9539663901326));
#39228=CARTESIAN_POINT('',(3.09908550384718,6.01564277861014,-33.3487628447403));
#39229=CARTESIAN_POINT('',(3.09908550384721,6.01564277861012,-63.6971797838103));
#39230=CARTESIAN_POINT('',(-6.76699999651487,-0.00021718149412733,-34.30282021619));
#39231=CARTESIAN_POINT('Ctrl Pts',(-6.76699999651487,-0.000217181494128159,
-34.30282021619));
#39232=CARTESIAN_POINT('Ctrl Pts',(-6.7669938648465,-0.191269370176862,
-34.2938005713136));
#39233=CARTESIAN_POINT('Ctrl Pts',(-6.7588924502058,-0.38237811217807,-34.2847809264371));
#39234=CARTESIAN_POINT('Ctrl Pts',(-6.74270737712069,-0.572875402266653,
-34.2757612815607));
#39235=CARTESIAN_POINT('Ctrl Pts',(-6.72653787596974,-0.763189411671673,
-34.266750314638));
#39236=CARTESIAN_POINT('Ctrl Pts',(-6.70230026323093,-0.952892902147142,
-34.2577393477154));
#39237=CARTESIAN_POINT('Ctrl Pts',(-6.67005812475392,-1.14132099446397,
-34.2487283807927));
#39238=CARTESIAN_POINT('Ctrl Pts',(-6.63787300301086,-1.3294158720837,-34.2397333487903));
#39239=CARTESIAN_POINT('Ctrl Pts',(-6.59771166086158,-1.51623961630588,
-34.2307383167878));
#39240=CARTESIAN_POINT('Ctrl Pts',(-6.5496890263464,-1.70113569657378,-34.2217432847854));
#39241=CARTESIAN_POINT('Ctrl Pts',(-6.50172615196388,-1.88580168920914,
-34.2127594463443));
#39242=CARTESIAN_POINT('Ctrl Pts',(-6.44592156777571,-2.06854457076069,
-34.2037756079032));
#39243=CARTESIAN_POINT('Ctrl Pts',(-6.38244100642491,-2.24871870172901,
-34.1947917694621));
#39244=CARTESIAN_POINT('Ctrl Pts',(-6.31909761565152,-2.42850350738176,
-34.1858273435511));
#39245=CARTESIAN_POINT('Ctrl Pts',(-6.24811143560728,-2.60573041346402,
-34.17686291764));
#39246=CARTESIAN_POINT('Ctrl Pts',(-6.16969755941112,-2.77976995907873,
-34.167898491729));
#39247=CARTESIAN_POINT('Ctrl Pts',(-6.10857035845828,-2.91544174058734,
-34.1609103119492));
#39248=CARTESIAN_POINT('Ctrl Pts',(-6.0429304192004,-3.0491767919573,-34.1539221321694));
#39249=CARTESIAN_POINT('Ctrl Pts',(-5.97290064038415,-3.18068340771267,
-34.1469339523896));
#39250=CARTESIAN_POINT('Ctrl Pts',(-5.89149704071466,-3.33354854714038,
-34.1388107939443));
#39251=CARTESIAN_POINT('Ctrl Pts',(-5.80419510917805,-3.48333551189467,
-34.130687635499));
#39252=CARTESIAN_POINT('Ctrl Pts',(-5.71126635389772,-3.62956273328288,
-34.1225644770537));
#39253=CARTESIAN_POINT('Ctrl Pts',(-5.61834415058117,-3.7757796448864,-34.1144418913336));
#39254=CARTESIAN_POINT('Ctrl Pts',(-5.51979611007115,-3.91843700413229,
-34.1063193056135));
#39255=CARTESIAN_POINT('Ctrl Pts',(-5.41593792345498,-4.05708089755211,
-34.0981967198934));
#39256=CARTESIAN_POINT('Ctrl Pts',(-5.3120672572083,-4.19574145046328,-34.090073158161));
#39257=CARTESIAN_POINT('Ctrl Pts',(-5.20288539471126,-4.3303872850359,-34.0819495964286));
#39258=CARTESIAN_POINT('Ctrl Pts',(-5.08874924847139,-4.46059638234417,
-34.0738260346962));
#39259=CARTESIAN_POINT('Ctrl Pts',(-4.97452996759335,-4.5909003215281,-34.0656965559131));
#39260=CARTESIAN_POINT('Ctrl Pts',(-4.85534943715149,-4.71676079349159,
-34.05756707713));
#39261=CARTESIAN_POINT('Ctrl Pts',(-4.73160291533413,-4.83779111285322,
-34.0494375983469));
#39262=CARTESIAN_POINT('Ctrl Pts',(-4.60780594423763,-4.95887077414605,
-34.0413048053183));
#39263=CARTESIAN_POINT('Ctrl Pts',(-4.47943954241164,-5.07511611218259,
-34.0331720122898));
#39264=CARTESIAN_POINT('Ctrl Pts',(-4.3469329867438,-5.1861799630131,-34.0250392192612));
#39265=CARTESIAN_POINT('Ctrl Pts',(-4.21428235029912,-5.29736457893201,
-34.0168975830541));
#39266=CARTESIAN_POINT('Ctrl Pts',(-4.07748285748908,-5.40335623068946,
-34.0087559468469));
#39267=CARTESIAN_POINT('Ctrl Pts',(-3.93699435812846,-5.50384996380395,
-34.0006143106398));
#39268=CARTESIAN_POINT('Ctrl Pts',(-3.86541737594449,-5.55505015583014,
-33.9964662575792));
#39269=CARTESIAN_POINT('Ctrl Pts',(-3.79288325329798,-5.60482393113451,
-33.9923182045186));
#39270=CARTESIAN_POINT('Ctrl Pts',(-3.71945531104089,-5.65313551838002,
-33.9881701514581));
#39271=CARTESIAN_POINT('Ctrl Pts',(-3.57003959167336,-5.75144292480034,
-33.97972943648));
#39272=CARTESIAN_POINT('Ctrl Pts',(-3.4166136099478,-5.84389562763648,-33.9712887215019));
#39273=CARTESIAN_POINT('Ctrl Pts',(-3.25966460728389,-5.93016657843781,
-33.9628480065238));
#39274=CARTESIAN_POINT('Ctrl Pts',(-3.10283423407095,-6.0163723215898,-33.9544136714358));
#39275=CARTESIAN_POINT('Ctrl Pts',(-2.94248643931854,-6.09640546694306,
-33.9459793363478));
#39276=CARTESIAN_POINT('Ctrl Pts',(-2.77913594602292,-6.16998317611347,
-33.9375450012598));
#39277=CARTESIAN_POINT('Ctrl Pts',(-2.61588383639307,-6.24351657048201,
-33.9291157460512));
#39278=CARTESIAN_POINT('Ctrl Pts',(-2.44963293694206,-6.31060214342651,
-33.9206864908425));
#39279=CARTESIAN_POINT('Ctrl Pts',(-2.28092134062876,-6.37100359738278,
-33.9122572356339));
#39280=CARTESIAN_POINT('Ctrl Pts',(-2.11228547780905,-6.43137793753522,
-33.9038317642609));
#39281=CARTESIAN_POINT('Ctrl Pts',(-1.94119143394642,-6.48507402909674,
-33.8954062928879));
#39282=CARTESIAN_POINT('Ctrl Pts',(-1.76819636321376,-6.53190405786227,
-33.8869808215149));
#39283=CARTESIAN_POINT('Ctrl Pts',(-1.59525243484278,-6.57872024231272,
-33.8785578409556));
#39284=CARTESIAN_POINT('Ctrl Pts',(-1.42040892184351,-6.61867432483879,
-33.8701348603964));
#39285=CARTESIAN_POINT('Ctrl Pts',(-1.24423757045886,-6.65162851249667,
-33.8617118798371));
#39286=CARTESIAN_POINT('Ctrl Pts',(-1.06806330204222,-6.68458324580751,
-33.8532887598108));
#39287=CARTESIAN_POINT('Ctrl Pts',(-0.890561477743755,-6.7105377848897,
-33.8448656397845));
#39288=CARTESIAN_POINT('Ctrl Pts',(-0.71231412258111,-6.72940544110485,
-33.8364425197582));
#39289=CARTESIAN_POINT('Ctrl Pts',(-0.534060603327663,-6.74827374979501,
-33.8280191084463));
#39290=CARTESIAN_POINT('Ctrl Pts',(-0.35506183343988,-6.76005465169477,
-33.8195956971344));
#39291=CARTESIAN_POINT('Ctrl Pts',(-0.175905208564063,-6.76471332412542,
-33.8111722858226));
#39292=CARTESIAN_POINT('Ctrl Pts',(0.00328259787393709,-6.76937280738116,
-33.8027474084465));
#39293=CARTESIAN_POINT('Ctrl Pts',(0.18262798070206,-6.7669075811072,-33.7943225310703));
#39294=CARTESIAN_POINT('Ctrl Pts',(0.361542919830847,-6.75733495670595,
-33.7858976536942));
#39295=CARTESIAN_POINT('Ctrl Pts',(0.540513958482216,-6.74775933076854,
-33.7774701346628));
#39296=CARTESIAN_POINT('Ctrl Pts',(0.719053951462811,-6.73107188137891,
-33.7690426156314));
#39297=CARTESIAN_POINT('Ctrl Pts',(0.896579004388525,-6.70734187952945,
-33.7606150966));
#39298=CARTESIAN_POINT('Ctrl Pts',(1.07426325492059,-6.68359059753147,-33.7521800200952));
#39299=CARTESIAN_POINT('Ctrl Pts',(1.25093041590619,-6.65278418804784,-33.7437449435904));
#39300=CARTESIAN_POINT('Ctrl Pts',(1.42600466859868,-6.61504343788722,-33.7353098670856));
#39301=CARTESIAN_POINT('Ctrl Pts',(1.60116353582971,-6.57728444737367,-33.7268707138529));
#39302=CARTESIAN_POINT('Ctrl Pts',(1.77472763532533,-6.53258451032157,-33.7184315606201));
#39303=CARTESIAN_POINT('Ctrl Pts',(1.94613483011703,-6.48111473613956,-33.7099924073873));
#39304=CARTESIAN_POINT('Ctrl Pts',(2.11773250635989,-6.42958776460776,-33.7015438758892));
#39305=CARTESIAN_POINT('Ctrl Pts',(2.2871681715165,-6.37127602725521,-33.6930953443911));
#39306=CARTESIAN_POINT('Ctrl Pts',(2.45389708841369,-6.30639977161889,-33.684646812893));
#39307=CARTESIAN_POINT('Ctrl Pts',(2.54602022453233,-6.27055353546456,-33.679978725127));
#39308=CARTESIAN_POINT('Ctrl Pts',(2.63731737974505,-6.23270405171612,-33.675310637361));
#39309=CARTESIAN_POINT('Ctrl Pts',(2.72769970169339,-6.19289458471415,-33.6706425495951));
#39310=CARTESIAN_POINT('Ctrl Pts',(2.88725549207892,-6.12261722476807,-33.6624017739983));
#39311=CARTESIAN_POINT('Ctrl Pts',(3.04431386512154,-6.04607262618752,-33.6541609984016));
#39312=CARTESIAN_POINT('Ctrl Pts',(3.1983500263171,-5.96345924016903,-33.6459202228048));
#39313=CARTESIAN_POINT('Ctrl Pts',(3.35221557576458,-5.88093735743194,-33.6376885747604));
#39314=CARTESIAN_POINT('Ctrl Pts',(3.50306526792112,-5.79236023834901,-33.6294569267161));
#39315=CARTESIAN_POINT('Ctrl Pts',(3.65039391979644,-5.69797448487734,-33.6212252786717));
#39316=CARTESIAN_POINT('Ctrl Pts',(3.797585644559,-5.60367645343764,-33.6130012811134));
#39317=CARTESIAN_POINT('Ctrl Pts',(3.94126254841058,-5.5035807297708,-33.6047772835551));
#39318=CARTESIAN_POINT('Ctrl Pts',(4.08094364387114,-5.39797999028783,-33.5965532859968));
#39319=CARTESIAN_POINT('Ctrl Pts',(4.22050133054114,-5.29247254946849,-33.5883365543723));
#39320=CARTESIAN_POINT('Ctrl Pts',(4.35606996238116,-5.18147000044937,-33.5801198227478));
#39321=CARTESIAN_POINT('Ctrl Pts',(4.48719728141066,-5.06530843658121,-33.5719030911233));
#39322=CARTESIAN_POINT('Ctrl Pts',(4.61825741906009,-4.9492063865827,-33.5636905692346));
#39323=CARTESIAN_POINT('Ctrl Pts',(4.7448805100339,-4.82795082119743,-33.5554780473459));
#39324=CARTESIAN_POINT('Ctrl Pts',(4.86664684013806,-4.70191849497354,-33.5472655254572));
#39325=CARTESIAN_POINT('Ctrl Pts',(4.98837245099535,-4.57592831456616,-33.5390557498754));
#39326=CARTESIAN_POINT('Ctrl Pts',(5.10524428949107,-4.44516481106522,-33.5308459742936));
#39327=CARTESIAN_POINT('Ctrl Pts',(5.21687897201709,-4.3100420869553,-33.5226361987117));
#39328=CARTESIAN_POINT('Ctrl Pts',(5.26563810105552,-4.25102399157652,-33.519050382029));
#39329=CARTESIAN_POINT('Ctrl Pts',(5.31339861499413,-4.19117474445455,-33.5154645653463));
#39330=CARTESIAN_POINT('Ctrl Pts',(5.36013090501688,-4.13053092000083,-33.5118787486636));
#39331=CARTESIAN_POINT('Ctrl Pts',(5.47558247242473,-3.98071107202465,-33.5030200311418));
#39332=CARTESIAN_POINT('Ctrl Pts',(5.58463619895538,-3.82619489454296,-33.49416131362));
#39333=CARTESIAN_POINT('Ctrl Pts',(5.6869529359615,-3.66754077061985,-33.4853025960983));
#39334=CARTESIAN_POINT('Ctrl Pts',(5.78946109114947,-3.50858983031233,-33.4764273053388));
#39335=CARTESIAN_POINT('Ctrl Pts',(5.88520692836807,-3.34548569079147,-33.4675520145794));
#39336=CARTESIAN_POINT('Ctrl Pts',(5.97389692410437,-3.17881181263949,-33.4586767238199));
#39337=CARTESIAN_POINT('Ctrl Pts',(6.06283881937008,-3.01166454319774,-33.4497762252391));
#39338=CARTESIAN_POINT('Ctrl Pts',(6.14468464771538,-2.8409274764045,-33.4408757266584));
#39339=CARTESIAN_POINT('Ctrl Pts',(6.21918754204155,-2.66720740043125,-33.4319752280776));
#39340=CARTESIAN_POINT('Ctrl Pts',(6.29379129103547,-2.49325215935867,-33.42306268088));
#39341=CARTESIAN_POINT('Ctrl Pts',(6.36103215381326,-2.31630608365107,-33.4141501336823));
#39342=CARTESIAN_POINT('Ctrl Pts',(6.42071257160129,-2.13699299785496,-33.4052375864847));
#39343=CARTESIAN_POINT('Ctrl Pts',(6.48052476958043,-1.95728397125298,-33.3963053595125));
#39344=CARTESIAN_POINT('Ctrl Pts',(6.53274304917183,-1.77519772759828,-33.3873731325402));
#39345=CARTESIAN_POINT('Ctrl Pts',(6.57721985283051,-1.5913729944712,-33.3784409055679));
#39346=CARTESIAN_POINT('Ctrl Pts',(6.61925556828464,-1.4176373943489,-33.3699989196226));
#39347=CARTESIAN_POINT('Ctrl Pts',(6.65437666351834,-1.24234916980446,-33.3615569336774));
#39348=CARTESIAN_POINT('Ctrl Pts',(6.68250099371985,-1.06605322049759,-33.3531149477321));
#39349=CARTESIAN_POINT('Ctrl Pts',(6.70989902228651,-0.894310056458122,
-33.3448909733145));
#39350=CARTESIAN_POINT('Ctrl Pts',(6.73070831014295,-0.721282309763172,
-33.3366669988969));
#39351=CARTESIAN_POINT('Ctrl Pts',(6.74481391059258,-0.547516494250918,
-33.3284430244794));
#39352=CARTESIAN_POINT('Ctrl Pts',(6.75890461415955,-0.373934192299406,
-33.3202277353767));
#39353=CARTESIAN_POINT('Ctrl Pts',(6.76630569969628,-0.1996157281842,-33.3120124462741));
#39354=CARTESIAN_POINT('Ctrl Pts',(6.76695338696486,-0.0251168995863532,
-33.3037971571714));
#39355=CARTESIAN_POINT('Ctrl Pts',(6.76760052012511,0.149232642063764,-33.2955888963992));
#39356=CARTESIAN_POINT('Ctrl Pts',(6.76150576048054,0.323761884313008,-33.2873806356271));
#39357=CARTESIAN_POINT('Ctrl Pts',(6.74865719260139,0.497910731707596,-33.2791723748549));
#39358=CARTESIAN_POINT('Ctrl Pts',(6.73581704049269,0.67194551216964,-33.270969490467));
#39359=CARTESIAN_POINT('Ctrl Pts',(6.7162319180324,0.845600037727389,-33.2627666060791));
#39360=CARTESIAN_POINT('Ctrl Pts',(6.68994197807794,1.01831494634549,-33.2545637216912));
#39361=CARTESIAN_POINT('Ctrl Pts',(6.66366398732654,1.1909513532432,-33.246364565647));
#39362=CARTESIAN_POINT('Ctrl Pts',(6.63068730424331,1.36264864025744,-33.2381654096028));
#39363=CARTESIAN_POINT('Ctrl Pts',(6.59110385667708,1.53285320578864,-33.2299662535586));
#39364=CARTESIAN_POINT('Ctrl Pts',(6.55152385190826,1.70304296766142,-33.2217678106416));
#39365=CARTESIAN_POINT('Ctrl Pts',(6.50533830008708,1.87173991571334,-33.2135693677246));
#39366=CARTESIAN_POINT('Ctrl Pts',(6.45269019283601,2.03840091132192,-33.2053709248076));
#39367=CARTESIAN_POINT('Ctrl Pts',(6.40004260989775,2.2050602471843,-33.1971725635373));
#39368=CARTESIAN_POINT('Ctrl Pts',(6.34093270676223,2.36968332863238,-33.1889742022671));
#39369=CARTESIAN_POINT('Ctrl Pts',(6.27555324913947,2.53174256535198,-33.1807758409969));
#39370=CARTESIAN_POINT('Ctrl Pts',(6.21016256597204,2.69382962737433,-33.1725760720816));
#39371=CARTESIAN_POINT('Ctrl Pts',(6.13850031787242,2.85335163498853,-33.1643763031663));
#39372=CARTESIAN_POINT('Ctrl Pts',(6.06080729700758,3.00980130715297,-33.156176534251));
#39373=CARTESIAN_POINT('Ctrl Pts',(5.983086822739,3.16630626196657,-33.1479738678867));
#39374=CARTESIAN_POINT('Ctrl Pts',(5.89933149012313,3.31973639766562,-33.1397712015224));
#39375=CARTESIAN_POINT('Ctrl Pts',(5.80982790369007,3.46960930502329,-33.1315685351581));
#39376=CARTESIAN_POINT('Ctrl Pts',(5.72022266355448,3.61965243054262,-33.1233565526151));
#39377=CARTESIAN_POINT('Ctrl Pts',(5.62485631087446,3.7661299480724,-33.1151445700721));
#39378=CARTESIAN_POINT('Ctrl Pts',(5.52405921104255,3.90858783103258,-33.106932587529));
#39379=CARTESIAN_POINT('Ctrl Pts',(5.42320265971882,4.05112973757754,-33.0987157614477));
#39380=CARTESIAN_POINT('Ctrl Pts',(5.31690919426824,4.189646999542,-33.0904989353664));
#39381=CARTESIAN_POINT('Ctrl Pts',(5.2055492098384,4.32371905007146,-33.0822821092851));
#39382=CARTESIAN_POINT('Ctrl Pts',(5.09401749222929,4.45799785906633,-33.0740526116713));
#39383=CARTESIAN_POINT('Ctrl Pts',(4.9774038813645,4.58781749089686,-33.0658231140574));
#39384=CARTESIAN_POINT('Ctrl Pts',(4.85611625261524,4.71279364507784,-33.0575936164436));
#39385=CARTESIAN_POINT('Ctrl Pts',(4.74800562825541,4.82419206384428,-33.0502581929187));
#39386=CARTESIAN_POINT('Ctrl Pts',(4.6361820424265,4.93174267929951,-33.0429227693939));
#39387=CARTESIAN_POINT('Ctrl Pts',(4.52095554968146,5.03520108017589,-33.035587345869));
#39388=CARTESIAN_POINT('Ctrl Pts',(4.39417909650282,5.14902984300791,-33.0275166413384));
#39389=CARTESIAN_POINT('Ctrl Pts',(4.26286932038105,5.25827529688711,-33.0194459368078));
#39390=CARTESIAN_POINT('Ctrl Pts',(4.12739668916492,5.36254469168048,-33.0113752322772));
#39391=CARTESIAN_POINT('Ctrl Pts',(3.99207256961981,5.46669978130447,-33.0033133752444));
#39392=CARTESIAN_POINT('Ctrl Pts',(3.85259496140558,5.56588943448039,-32.9952515182117));
#39393=CARTESIAN_POINT('Ctrl Pts',(3.70937148115886,5.65975725758317,-32.9871896611789));
#39394=CARTESIAN_POINT('Ctrl Pts',(3.56631248760859,5.75351727707652,-32.9791370628811));
#39395=CARTESIAN_POINT('Ctrl Pts',(3.41951649686986,5.84196743257849,-32.9710844645832));
#39396=CARTESIAN_POINT('Ctrl Pts',(3.26942412133972,5.92479155032496,-32.9630318662853));
#39397=CARTESIAN_POINT('Ctrl Pts',(3.21310031955796,5.95587220431704,-32.9600100409011));
#39398=CARTESIAN_POINT('Ctrl Pts',(3.15631264399957,5.98616100799977,-32.9569882155169));
#39399=CARTESIAN_POINT('Ctrl Pts',(3.09908550384723,6.01564277861011,-32.9539663901326));
#39400=CARTESIAN_POINT('Ctrl Pts',(3.09908550384724,6.01564277861011,-34.9544861942313));
#39401=CARTESIAN_POINT('Ctrl Pts',(3.01301923408008,6.05998163628863,-34.9499084485033));
#39402=CARTESIAN_POINT('Ctrl Pts',(2.92608302260693,6.10243092898755,-34.9453307027752));
#39403=CARTESIAN_POINT('Ctrl Pts',(2.83836998641864,6.14295896292641,-34.9407529570472));
#39404=CARTESIAN_POINT('Ctrl Pts',(2.67868731963912,6.21674074976132,-34.9324191143545));
#39405=CARTESIAN_POINT('Ctrl Pts',(2.51592169567249,6.28438672683791,-34.9240852716618));
#39406=CARTESIAN_POINT('Ctrl Pts',(2.35057870886505,6.34563383228424,-34.9157514289691));
#39407=CARTESIAN_POINT('Ctrl Pts',(2.18543059968516,6.40680875026841,-34.9074274087644));
#39408=CARTESIAN_POINT('Ctrl Pts',(2.01771150254169,6.46159970093205,-34.8991033885596));
#39409=CARTESIAN_POINT('Ctrl Pts',(1.8479497256929,6.50979038151856,-34.8907793683549));
#39410=CARTESIAN_POINT('Ctrl Pts',(1.67835690900003,6.55793309898252,-34.882463632864));
#39411=CARTESIAN_POINT('Ctrl Pts',(1.50672579562963,6.59948853981487,-34.8741478973731));
#39412=CARTESIAN_POINT('Ctrl Pts',(1.33360292203884,6.63428912893684,-34.8658321618823));
#39413=CARTESIAN_POINT('Ctrl Pts',(1.1606206332488,6.66906145816577,-34.8575231792023));
#39414=CARTESIAN_POINT('Ctrl Pts',(0.986149337592733,6.69708979739558,-34.8492141965222));
#39415=CARTESIAN_POINT('Ctrl Pts',(0.810749146081458,6.71825682912824,-34.8409052138422));
#39416=CARTESIAN_POINT('Ctrl Pts',(0.635459268471964,6.73941054834487,-34.832601456905));
#39417=CARTESIAN_POINT('Ctrl Pts',(0.459242003630512,6.75371151836466,-34.8242976999679));
#39418=CARTESIAN_POINT('Ctrl Pts',(0.282666258558173,6.76109375665452,-34.8159939430307));
#39419=CARTESIAN_POINT('Ctrl Pts',(0.106162198981455,6.76847299793361,-34.8076935572187));
#39420=CARTESIAN_POINT('Ctrl Pts',(-0.0706997038729907,6.7689390898049,
-34.7993931714067));
#39421=CARTESIAN_POINT('Ctrl Pts',(-0.247346537768416,6.76247799924362,
-34.7910927855947));
#39422=CARTESIAN_POINT('Ctrl Pts',(-0.423956121442899,6.75601827115822,
-34.782794150118));
#39423=CARTESIAN_POINT('Ctrl Pts',(-0.600350379152984,6.74263428354,-34.7744955146414));
#39424=CARTESIAN_POINT('Ctrl Pts',(-0.775957268691582,6.72236411667538,
-34.7661968791648));
#39425=CARTESIAN_POINT('Ctrl Pts',(-0.951556276034575,6.70209485964647,
-34.7578986161762));
#39426=CARTESIAN_POINT('Ctrl Pts',(-1.12636764018125,6.67494007935993,-34.7496003531876));
#39427=CARTESIAN_POINT('Ctrl Pts',(-1.29982510772464,6.64098966188991,-34.741302090199));
#39428=CARTESIAN_POINT('Ctrl Pts',(-1.473303580227,6.60703513316924,-34.7330028223262));
#39429=CARTESIAN_POINT('Ctrl Pts',(-1.64542748826131,6.56628339488382,-34.7247035544534));
#39430=CARTESIAN_POINT('Ctrl Pts',(-1.81564123312953,6.51887535642153,-34.7164042865806));
#39431=CARTESIAN_POINT('Ctrl Pts',(-1.98597449548109,6.47143402987518,-34.7080991912841));
#39432=CARTESIAN_POINT('Ctrl Pts',(-2.15439457918814,6.41732715751474,-34.6997940959876));
#39433=CARTESIAN_POINT('Ctrl Pts',(-2.32036063819031,6.35674566965968,-34.6914890006911));
#39434=CARTESIAN_POINT('Ctrl Pts',(-2.48638721704772,6.29614209064395,-34.683180876925));
#39435=CARTESIAN_POINT('Ctrl Pts',(-2.64995766349802,6.22905931655855,-34.6748727531588));
#39436=CARTESIAN_POINT('Ctrl Pts',(-2.81055134778003,6.15573635899816,-34.6665646293927));
#39437=CARTESIAN_POINT('Ctrl Pts',(-2.97131574222061,6.0823354595575,-34.6582476741391));
#39438=CARTESIAN_POINT('Ctrl Pts',(-3.12909673887959,6.00268127474854,-34.6499307188854));
#39439=CARTESIAN_POINT('Ctrl Pts',(-3.28339756684109,5.91705918662827,-34.6416137636317));
#39440=CARTESIAN_POINT('Ctrl Pts',(-3.39711492941807,5.85395701039238,-34.6354842941492));
#39441=CARTESIAN_POINT('Ctrl Pts',(-3.50894256167725,5.78761435019159,-34.6293548246667));
#39442=CARTESIAN_POINT('Ctrl Pts',(-3.61869188062726,5.71816037490051,-34.6232253551841));
#39443=CARTESIAN_POINT('Ctrl Pts',(-3.77000906704334,5.62240050844298,-34.614774331659));
#39444=CARTESIAN_POINT('Ctrl Pts',(-3.91765088171373,5.52054960774435,-34.6063233081338));
#39445=CARTESIAN_POINT('Ctrl Pts',(-4.06111487832845,5.41291372044847,-34.5978722846086));
#39446=CARTESIAN_POINT('Ctrl Pts',(-4.20445255915799,5.30537260335235,-34.5894287019585));
#39447=CARTESIAN_POINT('Ctrl Pts',(-4.34361948984515,5.19205684999914,-34.5809851193084));
#39448=CARTESIAN_POINT('Ctrl Pts',(-4.47814171585854,5.07331605290737,-34.5725415366582));
#39449=CARTESIAN_POINT('Ctrl Pts',(-4.61256378588424,4.95466366203785,-34.5641042405184));
#39450=CARTESIAN_POINT('Ctrl Pts',(-4.74234779714123,4.83059449786061,-34.5556669443786));
#39451=CARTESIAN_POINT('Ctrl Pts',(-4.86705214129365,4.70149895819716,-34.5472296482387));
#39452=CARTESIAN_POINT('Ctrl Pts',(-4.99166751840477,4.57249551835818,-34.5387983714664));
#39453=CARTESIAN_POINT('Ctrl Pts',(-5.11121022724892,4.43847309362074,-34.5303670946941));
#39454=CARTESIAN_POINT('Ctrl Pts',(-5.22527471574947,4.29985966572739,-34.5219358179217));
#39455=CARTESIAN_POINT('Ctrl Pts',(-5.33929031208093,4.16130565256728,-34.5135081550998));
#39456=CARTESIAN_POINT('Ctrl Pts',(-5.44783215899378,4.01816481478249,-34.5050804922779));
#39457=CARTESIAN_POINT('Ctrl Pts',(-5.5505338541505,3.87089949933206,-34.496652829456));
#39458=CARTESIAN_POINT('Ctrl Pts',(-5.65320393366362,3.72367951797005,-34.4882277610021));
#39459=CARTESIAN_POINT('Ctrl Pts',(-5.75003725735343,3.57233786257888,-34.4798026925481));
#39460=CARTESIAN_POINT('Ctrl Pts',(-5.84070955289625,3.41736754223284,-34.4713776240941));
#39461=CARTESIAN_POINT('Ctrl Pts',(-5.86552026836535,3.37496291906495,-34.4690722674803));
#39462=CARTESIAN_POINT('Ctrl Pts',(-5.88986993550112,3.33228677081255,-34.4667669108665));
#39463=CARTESIAN_POINT('Ctrl Pts',(-5.91375248523771,3.28934956235192,-34.4644615542527));
#39464=CARTESIAN_POINT('Ctrl Pts',(-6.00304167411293,3.12882111968981,-34.4558425657282));
#39465=CARTESIAN_POINT('Ctrl Pts',(-6.08575826444504,2.96471339317893,-34.4472235772037));
#39466=CARTESIAN_POINT('Ctrl Pts',(-6.16164022538411,2.79758444607638,-34.4386045886792));
#39467=CARTESIAN_POINT('Ctrl Pts',(-6.23756764638927,2.63035537382041,-34.4299804366115));
#39468=CARTESIAN_POINT('Ctrl Pts',(-6.30665214078173,2.46010174574732,-34.4213562845437));
#39469=CARTESIAN_POINT('Ctrl Pts',(-6.3686798857243,2.28740147616695,-34.4127321324759));
#39470=CARTESIAN_POINT('Ctrl Pts',(-6.4328320976185,2.10878617589184,-34.4038126008797));
#39471=CARTESIAN_POINT('Ctrl Pts',(-6.489435497163,1.92755401014723,-34.3948930692835));
#39472=CARTESIAN_POINT('Ctrl Pts',(-6.53830981141823,1.74436057336554,-34.3859735376872));
#39473=CARTESIAN_POINT('Ctrl Pts',(-6.58565363416623,1.56690381040624,-34.377333319828));
#39474=CARTESIAN_POINT('Ctrl Pts',(-6.62574509461208,1.38760705870056,-34.3686931019687));
#39475=CARTESIAN_POINT('Ctrl Pts',(-6.65847246900525,1.20707637682922,-34.3600528841095));
#39476=CARTESIAN_POINT('Ctrl Pts',(-6.69278681818168,1.01779162760461,-34.3509936956447));
#39477=CARTESIAN_POINT('Ctrl Pts',(-6.71900509300623,0.827150689016133,
-34.34193450718));
#39478=CARTESIAN_POINT('Ctrl Pts',(-6.73705967588828,0.635858414680623,
-34.3328753187153));
#39479=CARTESIAN_POINT('Ctrl Pts',(-6.75511425877033,0.444566140345081,
-34.3238161302506));
#39480=CARTESIAN_POINT('Ctrl Pts',(-6.76500516310217,0.252622914086894,
-34.3147569417859));
#39481=CARTESIAN_POINT('Ctrl Pts',(-6.76672744690538,0.0607343337615893,
-34.3056977533212));
#39482=CARTESIAN_POINT('Ctrl Pts',(-6.76690980082569,0.04041733674841,-34.3047385742774));
#39483=CARTESIAN_POINT('Ctrl Pts',(-6.76700064857688,0.0200999438642893,
-34.3037793952337));
#39484=CARTESIAN_POINT('Ctrl Pts',(-6.76699999651487,-0.000217181494126501,
-34.30282021619));
#39485=CARTESIAN_POINT('',(-6.76699750788529,-0.00580760486991878,-34.69717978378));
#39486=CARTESIAN_POINT('Ctrl Pts',(3.0990855038472,6.01564277861013,-35.3486949847746));
#39487=CARTESIAN_POINT('Ctrl Pts',(2.9397578610707,6.09772378080103,-35.3402675411684));
#39488=CARTESIAN_POINT('Ctrl Pts',(2.77721167747412,6.17344824237863,-35.3318400975623));
#39489=CARTESIAN_POINT('Ctrl Pts',(2.6119859135409,6.24258108377168,-35.3234126539561));
#39490=CARTESIAN_POINT('Ctrl Pts',(2.44661212069491,6.31177586259569,-35.3149776600425));
#39491=CARTESIAN_POINT('Ctrl Pts',(2.27855425848195,6.37436709208856,-35.3065426661289));
#39492=CARTESIAN_POINT('Ctrl Pts',(2.10837033981459,6.43016823342828,-35.2981076722153));
#39493=CARTESIAN_POINT('Ctrl Pts',(1.93810468087938,6.48599617636167,-35.289668626928));
#39494=CARTESIAN_POINT('Ctrl Pts',(1.76571124808744,6.53502743067727,-35.2812295816406));
#39495=CARTESIAN_POINT('Ctrl Pts',(1.59176166204321,6.57712580168948,-35.2727905363533));
#39496=CARTESIAN_POINT('Ctrl Pts',(1.41761785380289,6.61927117734398,-35.2643420685088));
#39497=CARTESIAN_POINT('Ctrl Pts',(1.24191474644245,6.65446813147599,-35.2558936006643));
#39498=CARTESIAN_POINT('Ctrl Pts',(1.06523377548364,6.68263166750711,-35.2474451328199));
#39499=CARTESIAN_POINT('Ctrl Pts',(0.963471630884538,6.69885289274981,-35.2425791067744));
#39500=CARTESIAN_POINT('Ctrl Pts',(0.861385212995945,6.7127418374066,-35.2377130807289));
#39501=CARTESIAN_POINT('Ctrl Pts',(0.759086148044961,6.7242900903996,-35.2328470546834));
#39502=CARTESIAN_POINT('Ctrl Pts',(0.585839307576767,6.74384743772162,-35.2246062790866));
#39503=CARTESIAN_POINT('Ctrl Pts',(0.411596968069216,6.75673212776572,-35.2163655034899));
#39504=CARTESIAN_POINT('Ctrl Pts',(0.23691250157723,6.76285157803988,-35.2081247278931));
#39505=CARTESIAN_POINT('Ctrl Pts',(0.0624215170694169,6.76896425035944,
-35.1998930798487));
#39506=CARTESIAN_POINT('Ctrl Pts',(-0.112510266890498,6.76832659096517,
-35.1916614318043));
#39507=CARTESIAN_POINT('Ctrl Pts',(-0.287322196330214,6.76089749630151,
-35.18342978376));
#39508=CARTESIAN_POINT('Ctrl Pts',(-0.461971655723405,6.7534753062316,-35.1752057862017));
#39509=CARTESIAN_POINT('Ctrl Pts',(-0.636501129060441,6.73927426636674,
-35.1669817886434));
#39510=CARTESIAN_POINT('Ctrl Pts',(-0.810347686599929,6.71830526448614,
-35.1587577910852));
#39511=CARTESIAN_POINT('Ctrl Pts',(-0.984040650031187,6.69735478880007,
-35.1505410594607));
#39512=CARTESIAN_POINT('Ctrl Pts',(-1.15705154834542,6.66964831135703,-35.1423243278361));
#39513=CARTESIAN_POINT('Ctrl Pts',(-1.32882043143063,6.63524869624436,-35.1341075962116));
#39514=CARTESIAN_POINT('Ctrl Pts',(-1.50050131095741,6.60086670532814,-35.125895074323));
#39515=CARTESIAN_POINT('Ctrl Pts',(-1.67094109457323,6.55979847593406,-35.1176825524343));
#39516=CARTESIAN_POINT('Ctrl Pts',(-1.83958749467868,6.5121583863894,-35.1094700305456));
#39517=CARTESIAN_POINT('Ctrl Pts',(-2.00817749861661,6.46453422791988,-35.1012602549637));
#39518=CARTESIAN_POINT('Ctrl Pts',(-2.17497497173797,6.41034268391535,-35.0930504793819));
#39519=CARTESIAN_POINT('Ctrl Pts',(-2.33944022862973,6.3497486892529,-35.0848407038001));
#39520=CARTESIAN_POINT('Ctrl Pts',(-2.41127438000354,6.32328280662706,-35.0812548871173));
#39521=CARTESIAN_POINT('Ctrl Pts',(-2.48266379697164,6.29559616331778,-35.0776690704346));
#39522=CARTESIAN_POINT('Ctrl Pts',(-2.55356448819593,6.26670546656093,-35.0740832537519));
#39523=CARTESIAN_POINT('Ctrl Pts',(-2.72872380369538,6.19533134339162,-35.0652245362301));
#39524=CARTESIAN_POINT('Ctrl Pts',(-2.90071750942194,6.11667939132356,-35.0563658187084));
#39525=CARTESIAN_POINT('Ctrl Pts',(-3.06897154411131,6.03106148712108,-35.0475071011866));
#39526=CARTESIAN_POINT('Ctrl Pts',(-3.23754035507439,5.9452834055719,-35.0386318104273));
#39527=CARTESIAN_POINT('Ctrl Pts',(-3.40235528218208,5.85251344558974,-35.0297565196679));
#39528=CARTESIAN_POINT('Ctrl Pts',(-3.56286907291655,5.75310811381594,-35.0208812289086));
#39529=CARTESIAN_POINT('Ctrl Pts',(-3.72383875890983,5.65342044854762,-35.0119807303278));
#39530=CARTESIAN_POINT('Ctrl Pts',(-3.88048264056111,5.54705983583765,-35.003080231747));
#39531=CARTESIAN_POINT('Ctrl Pts',(-4.03228204586679,5.43442641891307,-34.9941797331662));
#39532=CARTESIAN_POINT('Ctrl Pts',(-4.18428694223035,5.32164052998145,-34.9852671859686));
#39533=CARTESIAN_POINT('Ctrl Pts',(-4.33143405797199,5.20256503433119,-34.9763546387709));
#39534=CARTESIAN_POINT('Ctrl Pts',(-4.47323875905405,5.07763960955252,-34.9674420915733));
#39535=CARTESIAN_POINT('Ctrl Pts',(-4.61535657876507,4.95243833723544,-34.9585098646011));
#39536=CARTESIAN_POINT('Ctrl Pts',(-4.75210819332307,4.82136147136103,-34.9495776376288));
#39537=CARTESIAN_POINT('Ctrl Pts',(-4.88304467894395,4.68488672898686,-34.9406454106566));
#39538=CARTESIAN_POINT('Ctrl Pts',(-5.00679477785951,4.55590233790446,-34.9322034247112));
#39539=CARTESIAN_POINT('Ctrl Pts',(-5.1253507629051,4.42209676475768,-34.9237614387658));
#39540=CARTESIAN_POINT('Ctrl Pts',(-5.23836745235438,4.28389955929342,-34.9153194528204));
#39541=CARTESIAN_POINT('Ctrl Pts',(-5.34670294374354,4.15142653928605,-34.9072271374274));
#39542=CARTESIAN_POINT('Ctrl Pts',(-5.45018002904958,4.01463327173237,-34.8991348220344));
#39543=CARTESIAN_POINT('Ctrl Pts',(-5.54842804094167,3.87391730351749,-34.8910425066414));
#39544=CARTESIAN_POINT('Ctrl Pts',(-5.64654032475745,3.73339573218966,-34.8829613706542));
#39545=CARTESIAN_POINT('Ctrl Pts',(-5.73943771506141,3.588962557331,-34.8748802346671));
#39546=CARTESIAN_POINT('Ctrl Pts',(-5.82678883261555,3.44104938937335,-34.86679909868));
#39547=CARTESIAN_POINT('Ctrl Pts',(-5.91407045960886,3.29325389099205,-34.8587243914906));
#39548=CARTESIAN_POINT('Ctrl Pts',(-5.9958144054164,3.14198422553593,-34.8506496843013));
#39549=CARTESIAN_POINT('Ctrl Pts',(-6.07173145988988,2.98770247497698,-34.842574977112));
#39550=CARTESIAN_POINT('Ctrl Pts',(-6.14760302267668,2.83351317448876,-34.8345051085199));
#39551=CARTESIAN_POINT('Ctrl Pts',(-6.21765447963233,2.67631571287037,-34.8264352399278));
#39552=CARTESIAN_POINT('Ctrl Pts',(-6.28164167632996,2.51659826952863,-34.8183653713357));
#39553=CARTESIAN_POINT('Ctrl Pts',(-6.34560308667609,2.35694519109657,-34.810298754839));
#39554=CARTESIAN_POINT('Ctrl Pts',(-6.40350496398756,2.19477449671422,-34.8022321383423));
#39555=CARTESIAN_POINT('Ctrl Pts',(-6.4551506293771,2.03059581208385,-34.7941655218456));
#39556=CARTESIAN_POINT('Ctrl Pts',(-6.50689571333092,1.8661010813925,-34.7860833770093));
#39557=CARTESIAN_POINT('Ctrl Pts',(-6.55236033583749,1.69959096963597,-34.778001232173));
#39558=CARTESIAN_POINT('Ctrl Pts',(-6.59139632965033,1.53159505923469,-34.7699190873367));
#39559=CARTESIAN_POINT('Ctrl Pts',(-6.6303565999565,1.36392503369507,-34.7618526205526));
#39560=CARTESIAN_POINT('Ctrl Pts',(-6.6629130929852,1.19477533563551,-34.7537861537685));
#39561=CARTESIAN_POINT('Ctrl Pts',(-6.6889694020591,1.02468401876733,-34.7457196869844));
#39562=CARTESIAN_POINT('Ctrl Pts',(-6.71510167602282,0.854096815543634,
-34.737629703122));
#39563=CARTESIAN_POINT('Ctrl Pts',(-6.7346957445689,0.682562865173304,-34.7295397192596));
#39564=CARTESIAN_POINT('Ctrl Pts',(-6.74770664325823,0.510631037569024,
-34.7214497353973));
#39565=CARTESIAN_POINT('Ctrl Pts',(-6.76071754194755,0.338699209964744,
-34.7133597515349));
#39566=CARTESIAN_POINT('Ctrl Pts',(-6.76714527485211,0.166369881176929,
-34.7052697676725));
#39567=CARTESIAN_POINT('Ctrl Pts',(-6.76699750788584,-0.0058076042296127,
-34.6971797838101));
#39568=CARTESIAN_POINT('Ctrl Pts',(-6.76699750788529,-0.00580760486992044,
-34.69717978378));
#39569=CARTESIAN_POINT('Ctrl Pts',(-6.76681016756483,-0.224095782195824,
-34.6869232288782));
#39570=CARTESIAN_POINT('Ctrl Pts',(-6.75605708735273,-0.441891872896532,
-34.6766666739764));
#39571=CARTESIAN_POINT('Ctrl Pts',(-6.73490233367366,-0.658315696210507,
-34.6664101190746));
#39572=CARTESIAN_POINT('Ctrl Pts',(-6.71347909904819,-0.877486215316188,
-34.6560233953413));
#39573=CARTESIAN_POINT('Ctrl Pts',(-6.68138856748068,-1.09524956911206,
-34.645636671608));
#39574=CARTESIAN_POINT('Ctrl Pts',(-6.63884856683888,-1.31071686743604,
-34.6352499478748));
#39575=CARTESIAN_POINT('Ctrl Pts',(-6.59578266898006,-1.52884786230068,
-34.6247348191339));
#39576=CARTESIAN_POINT('Ctrl Pts',(-6.54200733234682,-1.74462585407272,
-34.614219690393));
#39577=CARTESIAN_POINT('Ctrl Pts',(-6.47779638330922,-1.95715176120453,
-34.6037045616522));
#39578=CARTESIAN_POINT('Ctrl Pts',(-6.4657610015762,-1.99698656288283,-34.6017336580872));
#39579=CARTESIAN_POINT('Ctrl Pts',(-6.45335913126745,-2.03670717311506,
-34.5997627545222));
#39580=CARTESIAN_POINT('Ctrl Pts',(-6.44059276114684,-2.07630775297472,
-34.5977918509573));
#39581=CARTESIAN_POINT('Ctrl Pts',(-6.38831434538541,-2.23847253111752,
-34.5897209807709));
#39582=CARTESIAN_POINT('Ctrl Pts',(-6.32981178682534,-2.39895766683898,
-34.5816501105845));
#39583=CARTESIAN_POINT('Ctrl Pts',(-6.26520760747365,-2.55723730522889,
-34.5735792403981));
#39584=CARTESIAN_POINT('Ctrl Pts',(-6.20068382300171,-2.71531997691133,
-34.5655184137823));
#39585=CARTESIAN_POINT('Ctrl Pts',(-6.13007366509786,-2.87120227128112,
-34.5574575871665));
#39586=CARTESIAN_POINT('Ctrl Pts',(-6.05354997673014,-3.0243712866033,-34.5493967605507));
#39587=CARTESIAN_POINT('Ctrl Pts',(-5.97710473566744,-3.17738328261918,
-34.5413441973908));
#39588=CARTESIAN_POINT('Ctrl Pts',(-5.89475819341828,-3.32768720397726,
-34.5332916342309));
#39589=CARTESIAN_POINT('Ctrl Pts',(-5.80673200582719,-3.47478811044676,
-34.5252390710711));
#39590=CARTESIAN_POINT('Ctrl Pts',(-5.71877678271408,-3.62177042789947,
-34.5171929996832));
#39591=CARTESIAN_POINT('Ctrl Pts',(-5.62515121821254,-3.76555455147239,
-34.5091469282953));
#39592=CARTESIAN_POINT('Ctrl Pts',(-5.52612376605051,-3.90566833234617,
-34.5011008569075));
#39593=CARTESIAN_POINT('Ctrl Pts',(-5.42715448617896,-4.04569980534085,
-34.4930595120716));
#39594=CARTESIAN_POINT('Ctrl Pts',(-5.32278985047443,-4.18206492398033,
-34.4850181672357));
#39595=CARTESIAN_POINT('Ctrl Pts',(-5.21334260978889,-4.31431893037123,
-34.4769768223999));
#39596=CARTESIAN_POINT('Ctrl Pts',(-5.1017855630724,-4.44912238705942,-34.4687804651788));
#39597=CARTESIAN_POINT('Ctrl Pts',(-4.98494816323669,-4.57965427631834,
-34.4605841079577));
#39598=CARTESIAN_POINT('Ctrl Pts',(-4.86320620052541,-4.70547706945547,
-34.4523877507367));
#39599=CARTESIAN_POINT('Ctrl Pts',(-4.74380463116985,-4.82888101848579,
-34.4443489620282));
#39600=CARTESIAN_POINT('Ctrl Pts',(-4.61968564584448,-4.94775502366046,
-34.4363101733197));
#39601=CARTESIAN_POINT('Ctrl Pts',(-4.49124223287662,-5.06172225686332,
-34.4282713846112));
#39602=CARTESIAN_POINT('Ctrl Pts',(-4.36278507529989,-5.17570168559266,
-34.4202317356794));
#39603=CARTESIAN_POINT('Ctrl Pts',(-4.23000284797881,-5.28477304889399,
-34.4121920867477));
#39604=CARTESIAN_POINT('Ctrl Pts',(-4.09332270285892,-5.3885989134709,-34.404152437816));
#39605=CARTESIAN_POINT('Ctrl Pts',(-3.95660086853438,-5.49245644627374,
-34.3961103366878));
#39606=CARTESIAN_POINT('Ctrl Pts',(-3.81597904710695,-5.59106506988513,
-34.3880682355596));
#39607=CARTESIAN_POINT('Ctrl Pts',(-3.6719143915468,-5.6841299862997,-34.3800261344314));
#39608=CARTESIAN_POINT('Ctrl Pts',(-3.52298811987531,-5.78033547800169,
-34.3717126439867));
#39609=CARTESIAN_POINT('Ctrl Pts',(-3.37038295108125,-5.87061632202818,
-34.3633991535419));
#39610=CARTESIAN_POINT('Ctrl Pts',(-3.2146316913088,-5.95469832058964,-34.3550856630971));
#39611=CARTESIAN_POINT('Ctrl Pts',(-3.06369942946313,-6.03617879299113,
-34.3470293949264));
#39612=CARTESIAN_POINT('Ctrl Pts',(-2.90981322243165,-6.11183819992559,
-34.3389731267556));
#39613=CARTESIAN_POINT('Ctrl Pts',(-2.75347794691015,-6.18147621494085,
-34.3309168585849));
#39614=CARTESIAN_POINT('Ctrl Pts',(-2.58965541161322,-6.25444935638185,
-34.3224747570031));
#39615=CARTESIAN_POINT('Ctrl Pts',(-2.42314390779816,-6.32080998595858,
-34.3140326554214));
#39616=CARTESIAN_POINT('Ctrl Pts',(-2.25454111502833,-6.38038661529588,
-34.3055905538396));
#39617=CARTESIAN_POINT('Ctrl Pts',(-2.0859383222585,-6.43996324463319,-34.2971484522578));
#39618=CARTESIAN_POINT('Ctrl Pts',(-1.91524470638034,-6.49275582016111,
-34.2887063506761));
#39619=CARTESIAN_POINT('Ctrl Pts',(-1.74306822618245,-6.53865446088667,
-34.2802642490943));
#39620=CARTESIAN_POINT('Ctrl Pts',(-1.57309968369904,-6.58396451169691,
-34.2719304064016));
#39621=CARTESIAN_POINT('Ctrl Pts',(-1.40114588204097,-6.62270101457491,
-34.2635965637089));
#39622=CARTESIAN_POINT('Ctrl Pts',(-1.22775003275432,-6.65469149225355,
-34.2552627210162));
#39623=CARTESIAN_POINT('Ctrl Pts',(-1.05455855241248,-6.68664426510711,
-34.2469387008115));
#39624=CARTESIAN_POINT('Ctrl Pts',(-0.879928749428964,-6.71186678938897,
-34.2386146806067));
#39625=CARTESIAN_POINT('Ctrl Pts',(-0.704418195599665,-6.7302365490158,
-34.230290660402));
#39626=CARTESIAN_POINT('Ctrl Pts',(-0.529082323557154,-6.74858802562566,
-34.2219749249111));
#39627=CARTESIAN_POINT('Ctrl Pts',(-0.352867790939159,-6.76010029012006,
-34.2136591894203));
#39628=CARTESIAN_POINT('Ctrl Pts',(-0.176341772977713,-6.76470195789165,
-34.2053434539294));
#39629=CARTESIAN_POINT('Ctrl Pts',(4.08966522569276E-5,-6.76929988886905,
-34.1970344712494));
#39630=CARTESIAN_POINT('Ctrl Pts',(0.176734201389097,-6.76699839607443,
-34.1887254885693));
#39631=CARTESIAN_POINT('Ctrl Pts',(0.353166209611189,-6.75777793571148,
-34.1804165058893));
#39632=CARTESIAN_POINT('Ctrl Pts',(0.529487254994421,-6.74856327434422,
-34.1721127489521));
#39633=CARTESIAN_POINT('Ctrl Pts',(0.705546984982687,-6.73243833563828,
-34.163808992015));
#39634=CARTESIAN_POINT('Ctrl Pts',(0.880773604091035,-6.70943565870756,
-34.1555052350778));
#39635=CARTESIAN_POINT('Ctrl Pts',(1.05592908541612,-6.68644232030915,-34.1472048492658));
#39636=CARTESIAN_POINT('Ctrl Pts',(1.23025178548296,-6.65657685255211,-34.1389044634537));
#39637=CARTESIAN_POINT('Ctrl Pts',(1.40317487012166,-6.61992366148274,-34.1306040776417));
#39638=CARTESIAN_POINT('Ctrl Pts',(1.57606148978124,-6.58327819961766,-34.1223054421651));
#39639=CARTESIAN_POINT('Ctrl Pts',(1.74754874197225,-6.5398479381213,-34.1140068066884));
#39640=CARTESIAN_POINT('Ctrl Pts',(1.91707958499378,-6.48976847543886,-34.1057081712118));
#39641=CARTESIAN_POINT('Ctrl Pts',(2.08660281854565,-6.43969126059609,-34.0974099082232));
#39642=CARTESIAN_POINT('Ctrl Pts',(2.25416948445153,-6.38296553799724,-34.0891116452347));
#39643=CARTESIAN_POINT('Ctrl Pts',(2.41923712668085,-6.31977695214704,-34.0808133822461));
#39644=CARTESIAN_POINT('Ctrl Pts',(2.58432475789711,-6.2565807144288,-34.0725141143733));
#39645=CARTESIAN_POINT('Ctrl Pts',(2.74691243786262,-6.18692017887483,-34.0642148465005));
#39646=CARTESIAN_POINT('Ctrl Pts',(2.90647695590489,-6.11102943085646,-34.0559155786277));
#39647=CARTESIAN_POINT('Ctrl Pts',(3.066153513957,-6.03508539530113,-34.0476104833311));
#39648=CARTESIAN_POINT('Ctrl Pts',(3.22280235401065,-5.95290255559377,-34.0393053880346));
#39649=CARTESIAN_POINT('Ctrl Pts',(3.37592337612668,-5.8647617478054,-34.0310002927381));
#39650=CARTESIAN_POINT('Ctrl Pts',(3.52910023412966,-5.77658879929519,-34.022692168972));
#39651=CARTESIAN_POINT('Ctrl Pts',(3.67874641249367,-5.68245373233268,-34.0143840452059));
#39652=CARTESIAN_POINT('Ctrl Pts',(3.82438997219138,-5.58268128595947,-34.0060759214398));
#39653=CARTESIAN_POINT('Ctrl Pts',(3.97018835015152,-5.48280278205224,-33.9977589661861));
#39654=CARTESIAN_POINT('Ctrl Pts',(4.11197532565338,-5.37727512860384,-33.9894420109324));
#39655=CARTESIAN_POINT('Ctrl Pts',(4.24931041585057,-5.26646465759943,-33.9811250556788));
#39656=CARTESIAN_POINT('Ctrl Pts',(4.35052428782257,-5.18479902641009,-33.9749955861963));
#39657=CARTESIAN_POINT('Ctrl Pts',(4.44932080234844,-5.10026491130442,-33.9688661167137));
#39658=CARTESIAN_POINT('Ctrl Pts',(4.54553631636467,-5.01302190266609,-33.9627366472312));
#39659=CARTESIAN_POINT('Ctrl Pts',(4.67819373064139,-4.89273535576128,-33.954285623706));
#39660=CARTESIAN_POINT('Ctrl Pts',(4.8061858353245,-4.76707815321763,-33.9458346001809));
#39661=CARTESIAN_POINT('Ctrl Pts',(4.92907009953112,-4.63643795967424,-33.9373835766557));
#39662=CARTESIAN_POINT('Ctrl Pts',(5.05184616779529,-4.50591279093858,-33.9289399940055));
#39663=CARTESIAN_POINT('Ctrl Pts',(5.16952313349309,-4.37041361640582,-33.9204964113554));
#39664=CARTESIAN_POINT('Ctrl Pts',(5.28169400177359,-4.23036611555417,-33.9120528287053));
#39665=CARTESIAN_POINT('Ctrl Pts',(5.39378135534839,-4.09042288442956,-33.9036155325654));
#39666=CARTESIAN_POINT('Ctrl Pts',(5.50037057703699,-3.94593833543775,-33.8951782364256));
#39667=CARTESIAN_POINT('Ctrl Pts',(5.60109353563225,-3.79737280301772,-33.8867409402858));
#39668=CARTESIAN_POINT('Ctrl Pts',(5.70174463607636,-3.64891326077741,-33.8783096635134));
#39669=CARTESIAN_POINT('Ctrl Pts',(5.79653763580677,-3.49637881623328,-33.8698783867411));
#39670=CARTESIAN_POINT('Ctrl Pts',(5.88514637004556,-3.34026064898229,-33.8614471099688));
#39671=CARTESIAN_POINT('Ctrl Pts',(5.97371712337331,-3.18420939962909,-33.8530194471468));
#39672=CARTESIAN_POINT('Ctrl Pts',(6.05610873237419,-3.02457777763841,-33.8445917843249));
#39673=CARTESIAN_POINT('Ctrl Pts',(6.13203949449097,-2.86188410631929,-33.836164121503));
#39674=CARTESIAN_POINT('Ctrl Pts',(6.20794688211602,-2.69924051854693,-33.827739053049));
#39675=CARTESIAN_POINT('Ctrl Pts',(6.27739724921018,-2.53353706129902,-33.819313984595));
#39676=CARTESIAN_POINT('Ctrl Pts',(6.34015565664528,-2.36531504233766,-33.8108889161411));
#39677=CARTESIAN_POINT('Ctrl Pts',(6.35732827790547,-2.31928434880494,-33.8085835595273));
#39678=CARTESIAN_POINT('Ctrl Pts',(6.37400012285963,-2.27306520228473,-33.8062782029135));
#39679=CARTESIAN_POINT('Ctrl Pts',(6.39016700662039,-2.2266689532798,-33.8039728462997));
#39680=CARTESIAN_POINT('Ctrl Pts',(6.45060979658932,-2.05320826812559,-33.7953538577752));
#39681=CARTESIAN_POINT('Ctrl Pts',(6.50396361824192,-1.87734823875085,-33.7867348692508));
#39682=CARTESIAN_POINT('Ctrl Pts',(6.55006600635919,-1.6996835918305,-33.7781158807263));
#39683=CARTESIAN_POINT('Ctrl Pts',(6.59619601392121,-1.52191250793146,-33.7694917286585));
#39684=CARTESIAN_POINT('Ctrl Pts',(6.63506584174416,-1.34233494328947,-33.7608675765907));
#39685=CARTESIAN_POINT('Ctrl Pts',(6.66656392236928,-1.16155691593838,-33.7522434245229));
#39686=CARTESIAN_POINT('Ctrl Pts',(6.69914082072965,-0.974587192516405,
-33.7433238929267));
#39687=CARTESIAN_POINT('Ctrl Pts',(6.72383200935134,-0.786333672111318,
-33.7344043613305));
#39688=CARTESIAN_POINT('Ctrl Pts',(6.74057229283507,-0.597473150078047,
-33.7254848297342));
#39689=CARTESIAN_POINT('Ctrl Pts',(6.75678835695958,-0.414526765755616,
-33.716844611875));
#39690=CARTESIAN_POINT('Ctrl Pts',(6.76554397422496,-0.231011127350753,
-33.7082043940157));
#39691=CARTESIAN_POINT('Ctrl Pts',(6.76683298989388,-0.0475424745237331,
-33.6995641761565));
#39692=CARTESIAN_POINT('Ctrl Pts',(6.76818451089358,0.14482271005868,-33.6905049876918));
#39693=CARTESIAN_POINT('Ctrl Pts',(6.76132731938759,0.337135851381192,-33.6814457992271));
#39694=CARTESIAN_POINT('Ctrl Pts',(6.74631565298735,0.528690940207873,-33.6723866107623));
#39695=CARTESIAN_POINT('Ctrl Pts',(6.7313039865871,0.720246029034587,-33.6633274222976));
#39696=CARTESIAN_POINT('Ctrl Pts',(6.70813792429692,0.911042689521306,-33.6542682338329));
#39697=CARTESIAN_POINT('Ctrl Pts',(6.67693357879445,1.10038492554522,-33.6452090453682));
#39698=CARTESIAN_POINT('Ctrl Pts',(6.64578329263131,1.28939913942923,-33.6361655513119));
#39699=CARTESIAN_POINT('Ctrl Pts',(6.60659468957936,1.47713823075668,-33.6271220572556));
#39700=CARTESIAN_POINT('Ctrl Pts',(6.55949036977891,1.66294169734775,-33.6180785631993));
#39701=CARTESIAN_POINT('Ctrl Pts',(6.51242913612754,1.8485752101873,-33.609043341194));
#39702=CARTESIAN_POINT('Ctrl Pts',(6.45746669982507,2.03227640252955,-33.6000081191887));
#39703=CARTESIAN_POINT('Ctrl Pts',(6.3947763876249,2.21339647426191,-33.5909728971833));
#39704=CARTESIAN_POINT('Ctrl Pts',(6.33219652210728,2.39419745185733,-33.5819535932722));
#39705=CARTESIAN_POINT('Ctrl Pts',(6.26191604559772,2.57242616468167,-33.5729342893611));
#39706=CARTESIAN_POINT('Ctrl Pts',(6.18415752465822,2.74745058376182,-33.56391498545));
#39707=CARTESIAN_POINT('Ctrl Pts',(6.1064965572145,2.92225542248314,-33.5549069968856));
#39708=CARTESIAN_POINT('Ctrl Pts',(6.02137636442516,3.09386377308503,-33.5458990083212));
#39709=CARTESIAN_POINT('Ctrl Pts',(5.92906780736512,3.26166275627426,-33.5368910197569));
#39710=CARTESIAN_POINT('Ctrl Pts',(5.83696773241452,3.42908275958242,-33.5279033760502));
#39711=CARTESIAN_POINT('Ctrl Pts',(5.73771181462949,3.59271036080958,-33.5189157323435));
#39712=CARTESIAN_POINT('Ctrl Pts',(5.63161685080284,3.75195690883485,-33.5099280886368));
#39713=CARTESIAN_POINT('Ctrl Pts',(5.53921549077015,3.89064961475902,-33.5021004739035));
#39714=CARTESIAN_POINT('Ctrl Pts',(5.44162733849227,4.0260194178936,-33.4942728591701));
#39715=CARTESIAN_POINT('Ctrl Pts',(5.33909048514265,4.15769188269877,-33.4864452444367));
#39716=CARTESIAN_POINT('Ctrl Pts',(5.23268593916626,4.29433103611042,-33.4783223718833));
#39717=CARTESIAN_POINT('Ctrl Pts',(5.12099856321383,4.42692655870261,-33.47019949933));
#39718=CARTESIAN_POINT('Ctrl Pts',(5.0043783765593,4.55505061050102,-33.4620766267766));
#39719=CARTESIAN_POINT('Ctrl Pts',(4.88776807567165,4.68316380136237,-33.4539544427903));
#39720=CARTESIAN_POINT('Ctrl Pts',(4.76622604397042,4.80680600640928,-33.4458322588041));
#39721=CARTESIAN_POINT('Ctrl Pts',(4.64014106541251,4.92558421845292,-33.4377100748178));
#39722=CARTESIAN_POINT('Ctrl Pts',(4.51400044247048,5.04441485022595,-33.4295843063131));
#39723=CARTESIAN_POINT('Ctrl Pts',(4.38331313241626,5.15837694765739,-33.4214585378084));
#39724=CARTESIAN_POINT('Ctrl Pts',(4.2485034687129,5.26711565055624,-33.4133327693038));
#39725=CARTESIAN_POINT('Ctrl Pts',(4.11366266659085,5.37587946998729,-33.4052051239041));
#39726=CARTESIAN_POINT('Ctrl Pts',(3.97469790425233,5.47941726831582,-33.3970774785045));
#39727=CARTESIAN_POINT('Ctrl Pts',(3.83206458138181,5.57741607235099,-33.3889498331048));
#39728=CARTESIAN_POINT('Ctrl Pts',(3.68930618332906,5.67550081155212,-33.3808150605717));
#39729=CARTESIAN_POINT('Ctrl Pts',(3.54287310595884,5.76803665496158,-33.3726802880385));
#39730=CARTESIAN_POINT('Ctrl Pts',(3.39324814791047,5.85475499117616,-33.3645455155054));
#39731=CARTESIAN_POINT('Ctrl Pts',(3.29648324385166,5.91083715549818,-33.3592846252504));
#39732=CARTESIAN_POINT('Ctrl Pts',(3.19838388179903,5.96448712077082,-33.3540237349953));
#39733=CARTESIAN_POINT('Ctrl Pts',(3.09908550384718,6.01564277861014,-33.3487628447403));
#39734=CARTESIAN_POINT('Origin',(0.,0.,-63.6971797838103));
#39735=CARTESIAN_POINT('',(3.09908550384721,6.01564277861012,-30.9542680870819));
#39736=CARTESIAN_POINT('',(3.0990855038472,6.01564277861013,-31.3484270467647));
#39737=CARTESIAN_POINT('',(3.09908550384721,6.01564277861012,-63.6971797838103));
#39738=CARTESIAN_POINT('',(-6.76699974407564,0.00186109651007785,-32.3028202161598));
#39739=CARTESIAN_POINT('Ctrl Pts',(-6.76699974407564,0.00186109651002826,
-32.3028202161599));
#39740=CARTESIAN_POINT('Ctrl Pts',(-6.76704658566934,-0.168456267928749,
-32.2948236154397));
#39741=CARTESIAN_POINT('Ctrl Pts',(-6.76065907798607,-0.338861495845034,
-32.2868270147195));
#39742=CARTESIAN_POINT('Ctrl Pts',(-6.74784363645294,-0.508817509507621,
-32.2788304139993));
#39743=CARTESIAN_POINT('Ctrl Pts',(-6.73502917781086,-0.678760488251144,
-32.2708344265852));
#39744=CARTESIAN_POINT('Ctrl Pts',(-6.7157877893052,-0.848253943265322,
-32.262838439171));
#39745=CARTESIAN_POINT('Ctrl Pts',(-6.69017792726411,-1.01676364094518,
-32.2548424517568));
#39746=CARTESIAN_POINT('Ctrl Pts',(-6.67621983595172,-1.10860614066129,
-32.2504844149084));
#39747=CARTESIAN_POINT('Ctrl Pts',(-6.66037085973537,-1.20015649082171,
-32.2461263780599));
#39748=CARTESIAN_POINT('Ctrl Pts',(-6.64264691453626,-1.2913291481268,-32.2417683412114));
#39749=CARTESIAN_POINT('Ctrl Pts',(-6.607593865287,-1.47164338464694,-32.2331493526869));
#39750=CARTESIAN_POINT('Ctrl Pts',(-6.56520739634836,-1.6504638741543,-32.2245303641624));
#39751=CARTESIAN_POINT('Ctrl Pts',(-6.51564637819431,-1.82719491963047,
-32.2159113756379));
#39752=CARTESIAN_POINT('Ctrl Pts',(-6.46605566856741,-2.00403184277489,
-32.2072872235701));
#39753=CARTESIAN_POINT('Ctrl Pts',(-6.40928191396484,-2.17877653089512,
-32.1986630715023));
#39754=CARTESIAN_POINT('Ctrl Pts',(-6.34553365094708,-2.35084914120371,
-32.1900389194345));
#39755=CARTESIAN_POINT('Ctrl Pts',(-6.27960199277124,-2.52881528470679,
-32.1811193878383));
#39756=CARTESIAN_POINT('Ctrl Pts',(-6.2062097418672,-2.70392273813924,-32.1721998562421));
#39757=CARTESIAN_POINT('Ctrl Pts',(-6.12564112338535,-2.87555382969791,
-32.1632803246459));
#39758=CARTESIAN_POINT('Ctrl Pts',(-6.04759549859063,-3.04181032046688,
-32.1546401067866));
#39759=CARTESIAN_POINT('Ctrl Pts',(-5.9628163395388,-3.20480462884413,-32.1459998889273));
#39760=CARTESIAN_POINT('Ctrl Pts',(-5.87160842070543,-3.36400112275562,
-32.1373596710681));
#39761=CARTESIAN_POINT('Ctrl Pts',(-5.7759777618907,-3.53091717334071,-32.1283004826034));
#39762=CARTESIAN_POINT('Ctrl Pts',(-5.67327957934809,-3.69365760686278,
-32.1192412941387));
#39763=CARTESIAN_POINT('Ctrl Pts',(-5.56391600898354,-3.85163960476272,
-32.110182105674));
#39764=CARTESIAN_POINT('Ctrl Pts',(-5.454552438619,-4.00962160266263,-32.1011229172093));
#39765=CARTESIAN_POINT('Ctrl Pts',(-5.33852373783123,-4.16284487990282,
-32.0920637287446));
#39766=CARTESIAN_POINT('Ctrl Pts',(-5.21628047439728,-4.31076640661748,
-32.0830045402799));
#39767=CARTESIAN_POINT('Ctrl Pts',(-5.09424898884043,-4.45843166966553,
-32.0739610462236));
#39768=CARTESIAN_POINT('Ctrl Pts',(-4.96591268640582,-4.60095011232842,
-32.0649175521673));
#39769=CARTESIAN_POINT('Ctrl Pts',(-4.83170988049905,-4.73781264199925,
-32.055874058111));
#39770=CARTESIAN_POINT('Ctrl Pts',(-4.69762982940854,-4.8745499840142,-32.0468388361057));
#39771=CARTESIAN_POINT('Ctrl Pts',(-4.55769415477322,-5.00564157198395,
-32.0378036141004));
#39772=CARTESIAN_POINT('Ctrl Pts',(-4.41237911784053,-5.13061395160899,
-32.0287683920951));
#39773=CARTESIAN_POINT('Ctrl Pts',(-4.2673200943678,-5.25536615710765,-32.019749088184));
#39774=CARTESIAN_POINT('Ctrl Pts',(-4.11690081379617,-5.3740205269628,-32.0107297842729));
#39775=CARTESIAN_POINT('Ctrl Pts',(-3.96163164959631,-5.48614287755221,
-32.0017104803618));
#39776=CARTESIAN_POINT('Ctrl Pts',(-3.80655728140831,-5.59812456282119,
-31.9927024917974));
#39777=CARTESIAN_POINT('Ctrl Pts',(-3.64664536464657,-5.70359044400696,
-31.983694503233));
#39778=CARTESIAN_POINT('Ctrl Pts',(-3.48243837122316,-5.8021471879497,-31.9746865146687));
#39779=CARTESIAN_POINT('Ctrl Pts',(-3.31860224504604,-5.90048133803412,
-31.965698870962));
#39780=CARTESIAN_POINT('Ctrl Pts',(-3.15049060921926,-5.99193737664443,
-31.9567112272553));
#39781=CARTESIAN_POINT('Ctrl Pts',(-2.97867344019052,-6.07616602280613,
-31.9477235835487));
#39782=CARTESIAN_POINT('Ctrl Pts',(-2.82903259464324,-6.14952333571139,
-31.9398959688152));
#39783=CARTESIAN_POINT('Ctrl Pts',(-2.67658157812106,-6.21739909447239,
-31.9320683540818));
#39784=CARTESIAN_POINT('Ctrl Pts',(-2.52171455837233,-6.27958953165675,
-31.9242407393484));
#39785=CARTESIAN_POINT('Ctrl Pts',(-2.36100029455,-6.34412806507136,-31.9161175809031));
#39786=CARTESIAN_POINT('Ctrl Pts',(-2.19775536071387,-6.40251345397151,
-31.9079944224579));
#39787=CARTESIAN_POINT('Ctrl Pts',(-2.03249757759334,-6.45455208338094,
-31.8998712640126));
#39788=CARTESIAN_POINT('Ctrl Pts',(-1.86725144601121,-6.50658704379471,
-31.8917486782925));
#39789=CARTESIAN_POINT('Ctrl Pts',(-1.69999309695263,-6.55227602611667,
-31.8836260925724));
#39790=CARTESIAN_POINT('Ctrl Pts',(-1.53125634743834,-6.59147502448654,
-31.8755035068523));
#39791=CARTESIAN_POINT('Ctrl Pts',(-1.3624993224679,-6.63067873301928,-31.8673799451199));
#39792=CARTESIAN_POINT('Ctrl Pts',(-1.19226390010267,-6.66339082310288,
-31.8592563833876));
#39793=CARTESIAN_POINT('Ctrl Pts',(-1.02109489801628,-6.6895182344654,-31.8511328216553));
#39794=CARTESIAN_POINT('Ctrl Pts',(-0.849801219622619,-6.71566467654685,
-31.8430033428722));
#39795=CARTESIAN_POINT('Ctrl Pts',(-0.677572965566393,-6.73521680543398,
-31.8348738640891));
#39796=CARTESIAN_POINT('Ctrl Pts',(-0.504961539524183,-6.74813328585035,
-31.8267443853059));
#39797=CARTESIAN_POINT('Ctrl Pts',(-0.332279742841576,-6.76105503208845,
-31.8186115922774));
#39798=CARTESIAN_POINT('Ctrl Pts',(-0.159214828318478,-6.76733572424922,
-31.8104787992489));
#39799=CARTESIAN_POINT('Ctrl Pts',(0.0136812215726762,-6.76698616994126,
-31.8023460062203));
#39800=CARTESIAN_POINT('Ctrl Pts',(0.18676526968823,-6.76663623554602,-31.7942043700132));
#39801=CARTESIAN_POINT('Ctrl Pts',(0.359679721161646,-6.7596416700172,-31.7860627338061));
#39802=CARTESIAN_POINT('Ctrl Pts',(0.531876381940679,-6.74606526164206,
-31.7779210975989));
#39803=CARTESIAN_POINT('Ctrl Pts',(0.619608241681404,-6.73914826598162,
-31.7737730445382));
#39804=CARTESIAN_POINT('Ctrl Pts',(0.707153903593955,-6.73052360732793,
-31.7696249914775));
#39805=CARTESIAN_POINT('Ctrl Pts',(0.794441887476215,-6.72020469088727,
-31.7654769384169));
#39806=CARTESIAN_POINT('Ctrl Pts',(0.972060876959575,-6.69920712135667,
-31.7570362234388));
#39807=CARTESIAN_POINT('Ctrl Pts',(1.14897812505722,-6.67114787233272,-31.7485955084607));
#39808=CARTESIAN_POINT('Ctrl Pts',(1.32461025384826,-6.63609046618565,-31.7401547934826));
#39809=CARTESIAN_POINT('Ctrl Pts',(1.50010963160125,-6.60105955807791,-31.7317204583946));
#39810=CARTESIAN_POINT('Ctrl Pts',(1.67432550058884,-6.55904110225151,-31.7232861233066));
#39811=CARTESIAN_POINT('Ctrl Pts',(1.84668192470545,-6.51015014181441,-31.7148517882185));
#39812=CARTESIAN_POINT('Ctrl Pts',(2.01893454101275,-6.46128862770358,-31.7064225330099));
#39813=CARTESIAN_POINT('Ctrl Pts',(2.18932962521364,-6.40556295188272,-31.6979932778013));
#39814=CARTESIAN_POINT('Ctrl Pts',(2.35730332960249,-6.34313881388741,-31.6895640225927));
#39815=CARTESIAN_POINT('Ctrl Pts',(2.52520163173223,-6.28074269766518,-31.6811385512197));
#39816=CARTESIAN_POINT('Ctrl Pts',(2.69068040928394,-6.21165423065285,-31.6727130798467));
#39817=CARTESIAN_POINT('Ctrl Pts',(2.8531924503838,-6.13608848054466,-31.6642876084737));
#39818=CARTESIAN_POINT('Ctrl Pts',(3.01565644820917,-6.06054506986468,-31.6558646279145));
#39819=CARTESIAN_POINT('Ctrl Pts',(3.17515515662037,-5.9785283352109,-31.6474416473553));
#39820=CARTESIAN_POINT('Ctrl Pts',(3.3311624091704,-5.8903010113007,-31.6390186667961));
#39821=CARTESIAN_POINT('Ctrl Pts',(3.48717224487779,-5.80207222652854,-31.6305955467697));
#39822=CARTESIAN_POINT('Ctrl Pts',(3.63969021581832,-5.70763280537124,-31.6221724267434));
#39823=CARTESIAN_POINT('Ctrl Pts',(3.78821519843597,-5.60729120077946,-31.6137493067171));
#39824=CARTESIAN_POINT('Ctrl Pts',(3.93674531729517,-5.50694612620767,-31.6053258954052));
#39825=CARTESIAN_POINT('Ctrl Pts',(4.08128189606481,-5.40069864779729,-31.5969024840933));
#39826=CARTESIAN_POINT('Ctrl Pts',(4.22135309971023,-5.28890035901291,-31.5884790727814));
#39827=CARTESIAN_POINT('Ctrl Pts',(4.36144868224157,-5.17708261214109,-31.5800541954053));
#39828=CARTESIAN_POINT('Ctrl Pts',(4.49707707953395,-5.0597123368144,-31.5716293180292));
#39829=CARTESIAN_POINT('Ctrl Pts',(4.62779954899389,-4.93718141598341,-31.5632044406531));
#39830=CARTESIAN_POINT('Ctrl Pts',(4.75856300702829,-4.81461207507213,-31.5547769216216));
#39831=CARTESIAN_POINT('Ctrl Pts',(4.88441722710938,-4.68687909049526,-31.5463494025901));
#39832=CARTESIAN_POINT('Ctrl Pts',(5.00496008102947,-4.55441144246998,-31.5379218835586));
#39833=CARTESIAN_POINT('Ctrl Pts',(5.12561103312129,-4.42182500257858,-31.5294868070538));
#39834=CARTESIAN_POINT('Ctrl Pts',(5.24094087717673,-4.28449566228239,-31.521051730549));
#39835=CARTESIAN_POINT('Ctrl Pts',(5.35058683568231,-4.1428866160955,-31.5126166540442));
#39836=CARTESIAN_POINT('Ctrl Pts',(5.4602857868012,-4.00120912932467,-31.5041775008115));
#39837=CARTESIAN_POINT('Ctrl Pts',(5.56429517607593,-3.85524807990081,-31.4957383475787));
#39838=CARTESIAN_POINT('Ctrl Pts',(5.66229509756711,-3.70549635380572,-31.4872991943459));
#39839=CARTESIAN_POINT('Ctrl Pts',(5.76040392444774,-3.55557821155638,-31.4788506628478));
#39840=CARTESIAN_POINT('Ctrl Pts',(5.85248976380151,-3.40186125891017,-31.4704021313497));
#39841=CARTESIAN_POINT('Ctrl Pts',(5.93827766318478,-3.2448647729791,-31.4619535998515));
#39842=CARTESIAN_POINT('Ctrl Pts',(5.98567826098805,-3.15811912074092,-31.4572855120856));
#39843=CARTESIAN_POINT('Ctrl Pts',(6.03115697502175,-3.0703726647477,-31.4526174243198));
#39844=CARTESIAN_POINT('Ctrl Pts',(6.07467368380423,-2.98171572006728,-31.4479493365539));
#39845=CARTESIAN_POINT('Ctrl Pts',(6.15149559670978,-2.82520581218904,-31.4397085609571));
#39846=CARTESIAN_POINT('Ctrl Pts',(6.22237115158676,-2.66550902500934,-31.4314677853604));
#39847=CARTESIAN_POINT('Ctrl Pts',(6.28702661886985,-2.50311511793245,-31.4232270097636));
#39848=CARTESIAN_POINT('Ctrl Pts',(6.35161047321313,-2.34090107971402,-31.4149953617193));
#39849=CARTESIAN_POINT('Ctrl Pts',(6.40998782761032,-2.17599619760905,-31.406763713675));
#39850=CARTESIAN_POINT('Ctrl Pts',(6.46193096237487,-2.00891444255374,-31.3985320656306));
#39851=CARTESIAN_POINT('Ctrl Pts',(6.51382582123821,-1.8419879731264,-31.3903080680723));
#39852=CARTESIAN_POINT('Ctrl Pts',(6.55929826474335,-1.67288899773513,-31.382084070514));
#39853=CARTESIAN_POINT('Ctrl Pts',(6.59816875328745,-1.50215115855267,-31.3738600729558));
#39854=CARTESIAN_POINT('Ctrl Pts',(6.63700489960395,-1.3315641669143,-31.3656433413313));
#39855=CARTESIAN_POINT('Ctrl Pts',(6.6692506377745,-1.15934154297199,-31.3574266097067));
#39856=CARTESIAN_POINT('Ctrl Pts',(6.69477636597363,-0.98603164736275,-31.3492098780822));
#39857=CARTESIAN_POINT('Ctrl Pts',(6.72028901639722,-0.812810544829176,
-31.3409973561935));
#39858=CARTESIAN_POINT('Ctrl Pts',(6.7390884620531,-0.638503631174716,-31.3327848343048));
#39859=CARTESIAN_POINT('Ctrl Pts',(6.75109618269687,-0.463669421005698,
-31.3245723124161));
#39860=CARTESIAN_POINT('Ctrl Pts',(6.7630998879011,-0.288893676237496,-31.3163625368343));
#39861=CARTESIAN_POINT('Ctrl Pts',(6.76831636821242,-0.113591340786384,
-31.3081527612524));
#39862=CARTESIAN_POINT('Ctrl Pts',(6.76671894874299,0.0616738901205327,
-31.2999429856705));
#39863=CARTESIAN_POINT('Ctrl Pts',(6.76602123741997,0.138225189559716,-31.2963571689877));
#39864=CARTESIAN_POINT('Ctrl Pts',(6.76402429762049,0.214769368334944,-31.292771352305));
#39865=CARTESIAN_POINT('Ctrl Pts',(6.76072902687091,0.291259377918038,-31.2891855356222));
#39866=CARTESIAN_POINT('Ctrl Pts',(6.75258809962594,0.48022703802957,-31.2803268181004));
#39867=CARTESIAN_POINT('Ctrl Pts',(6.73652816999348,0.668668124403733,-31.2714681005787));
#39868=CARTESIAN_POINT('Ctrl Pts',(6.7126493121296,0.855937037617868,-31.2626093830569));
#39869=CARTESIAN_POINT('Ctrl Pts',(6.68872578075796,1.04355630089041,-31.2537340922975));
#39870=CARTESIAN_POINT('Ctrl Pts',(6.65695412098099,1.22999875128215,-31.2448588015381));
#39871=CARTESIAN_POINT('Ctrl Pts',(6.61748546232807,1.41462898170394,-31.2359835107787));
#39872=CARTESIAN_POINT('Ctrl Pts',(6.57790470380997,1.59978360349453,-31.227083012198));
#39873=CARTESIAN_POINT('Ctrl Pts',(6.53058325401584,1.78311545011171,-31.2181825136172));
#39874=CARTESIAN_POINT('Ctrl Pts',(6.47572296005789,1.96400130971929,-31.2092820150364));
#39875=CARTESIAN_POINT('Ctrl Pts',(6.4207884016467,2.14513203475675,-31.2003694678388));
#39876=CARTESIAN_POINT('Ctrl Pts',(6.35829469482546,2.32380991235501,-31.1914569206412));
#39877=CARTESIAN_POINT('Ctrl Pts',(6.28849238220523,2.49943044691122,-31.1825443734436));
#39878=CARTESIAN_POINT('Ctrl Pts',(6.21853593926143,2.67543876875986,-31.1736121464713));
#39879=CARTESIAN_POINT('Ctrl Pts',(6.14123870780059,2.84837600263461,-31.1646799194991));
#39880=CARTESIAN_POINT('Ctrl Pts',(6.05689908236603,3.01765844754398,-31.1557476925268));
#39881=CARTESIAN_POINT('Ctrl Pts',(5.97718839714009,3.17764990601824,-31.1473057065815));
#39882=CARTESIAN_POINT('Ctrl Pts',(5.89118762133789,3.33437680082602,-31.1388637206362));
#39883=CARTESIAN_POINT('Ctrl Pts',(5.79918477858274,3.48736933860672,-31.1304217346908));
#39884=CARTESIAN_POINT('Ctrl Pts',(5.70956342756009,3.63640166762703,-31.1221982693817));
#39885=CARTESIAN_POINT('Ctrl Pts',(5.61407463849383,3.78217460051554,-31.1139748040727));
#39886=CARTESIAN_POINT('Ctrl Pts',(5.51298232745837,3.92419607781412,-31.1057513387636));
#39887=CARTESIAN_POINT('Ctrl Pts',(5.41199195061199,4.06607435090683,-31.0975361654033));
#39888=CARTESIAN_POINT('Ctrl Pts',(5.305409507286,4.20420840997081,-31.089320992043));
#39889=CARTESIAN_POINT('Ctrl Pts',(5.19354407300965,4.33813196683853,-31.0811058186827));
#39890=CARTESIAN_POINT('Ctrl Pts',(5.08177110580615,4.47194482356577,-31.072897435919));
#39891=CARTESIAN_POINT('Ctrl Pts',(4.96472407208927,4.60155383497081,-31.0646890531553));
#39892=CARTESIAN_POINT('Ctrl Pts',(4.84275452513964,4.7265227820502,-31.0564806703916));
#39893=CARTESIAN_POINT('Ctrl Pts',(4.71618856164337,4.85620117792674,-31.0479629551158));
#39894=CARTESIAN_POINT('Ctrl Pts',(4.58432206138568,4.98088264727668,-31.03944523984));
#39895=CARTESIAN_POINT('Ctrl Pts',(4.44759350135276,5.10011774831961,-31.0309275245641));
#39896=CARTESIAN_POINT('Ctrl Pts',(4.31597847507724,5.21489355633625,-31.0227283647137));
#39897=CARTESIAN_POINT('Ctrl Pts',(4.17985876899612,5.32462273389042,-31.0145292048632));
#39898=CARTESIAN_POINT('Ctrl Pts',(4.03966251238306,5.42894241874484,-31.0063300450128));
#39899=CARTESIAN_POINT('Ctrl Pts',(3.89950189218883,5.53323558662888,-30.9981329693028));
#39900=CARTESIAN_POINT('Ctrl Pts',(3.75526707419318,5.63212178862292,-30.9899358935928));
#39901=CARTESIAN_POINT('Ctrl Pts',(3.60741812487521,5.72527933574615,-30.9817388178829));
#39902=CARTESIAN_POINT('Ctrl Pts',(3.45956971450485,5.81843654328605,-30.9735417720534));
#39903=CARTESIAN_POINT('Ctrl Pts',(3.30810750176141,5.90586494564656,-30.9653447262238));
#39904=CARTESIAN_POINT('Ctrl Pts',(3.15351944059881,5.98728687618736,-30.9571476803943));
#39905=CARTESIAN_POINT('Ctrl Pts',(3.13541736023296,5.99682128860645,-30.9561878159569));
#39906=CARTESIAN_POINT('Ctrl Pts',(3.11727244616411,6.00627339093736,-30.9552279515194));
#39907=CARTESIAN_POINT('Ctrl Pts',(3.09908550384721,6.01564277861012,-30.9542680870819));
#39908=CARTESIAN_POINT('Ctrl Pts',(3.09908550384723,6.01564277861011,-32.9539663901326));
#39909=CARTESIAN_POINT('Ctrl Pts',(2.94674704149251,6.09412315680687,-32.9459223007143));
#39910=CARTESIAN_POINT('Ctrl Pts',(2.79129257097801,6.16688148165184,-32.937878211296));
#39911=CARTESIAN_POINT('Ctrl Pts',(2.63320140856036,6.23366179239424,-32.9298341218777));
#39912=CARTESIAN_POINT('Ctrl Pts',(2.47519013293361,6.30040835764044,-32.921794097307));
#39913=CARTESIAN_POINT('Ctrl Pts',(2.31454516101582,6.36118277802486,-32.9137540727364));
#39914=CARTESIAN_POINT('Ctrl Pts',(2.15176855625465,6.41577595309513,-32.9057140481657));
#39915=CARTESIAN_POINT('Ctrl Pts',(1.9890111333849,6.47036269480628,-32.8976749710462));
#39916=CARTESIAN_POINT('Ctrl Pts',(1.82412292827275,6.51876951353359,-32.8896358939267));
#39917=CARTESIAN_POINT('Ctrl Pts',(1.65762420155657,6.56083615146834,-32.8815968168071));
#39918=CARTESIAN_POINT('Ctrl Pts',(1.49112888342494,6.60290192820918,-32.8735579042647));
#39919=CARTESIAN_POINT('Ctrl Pts',(1.32302347111279,6.63862768989094,-32.8655189917222));
#39920=CARTESIAN_POINT('Ctrl Pts',(1.15384124118038,6.66790367283086,-32.8574800791798));
#39921=CARTESIAN_POINT('Ctrl Pts',(0.984628981384295,6.69718485226085,-32.8494397397295));
#39922=CARTESIAN_POINT('Ctrl Pts',(0.814339891447124,6.72001391017923,-32.8413994002792));
#39923=CARTESIAN_POINT('Ctrl Pts',(0.643515094834652,6.73633263153772,-32.833359060829));
#39924=CARTESIAN_POINT('Ctrl Pts',(0.472626148960312,6.75265748101081,-32.825315702017));
#39925=CARTESIAN_POINT('Ctrl Pts',(0.301201467382972,6.76246709214905,-32.8172723432051));
#39926=CARTESIAN_POINT('Ctrl Pts',(0.129784770481594,6.76575530989342,-32.8092289843932));
#39927=CARTESIAN_POINT('Ctrl Pts',(-0.0418364582406628,6.76904745108968,
-32.8011760283666));
#39928=CARTESIAN_POINT('Ctrl Pts',(-0.21344930978222,6.76580265238947,-32.7931230723401));
#39929=CARTESIAN_POINT('Ctrl Pts',(-0.384511736156809,6.75606688279192,
-32.7850701163136));
#39930=CARTESIAN_POINT('Ctrl Pts',(-0.555683056889247,6.74632491563012,
-32.7770120339628));
#39931=CARTESIAN_POINT('Ctrl Pts',(-0.726302884308395,6.7300837842317,-32.7689539516119));
#39932=CARTESIAN_POINT('Ctrl Pts',(-0.895837323044223,6.70744097928867,
-32.7608958692611));
#39933=CARTESIAN_POINT('Ctrl Pts',(-1.06564251148265,6.68476201335824,-32.7528249180005));
#39934=CARTESIAN_POINT('Ctrl Pts',(-1.23435848265583,6.65566101806081,-32.7447539667399));
#39935=CARTESIAN_POINT('Ctrl Pts',(-1.40146345646603,6.6202861856713,-32.7366830154792));
#39936=CARTESIAN_POINT('Ctrl Pts',(-1.52999193641433,6.59307769910277,-32.7304752583215));
#39937=CARTESIAN_POINT('Ctrl Pts',(-1.65756762294372,6.56215871816995,-32.7242675011637));
#39938=CARTESIAN_POINT('Ctrl Pts',(-1.78396096288756,6.52761612557703,-32.718059744006));
#39939=CARTESIAN_POINT('Ctrl Pts',(-1.95364257022628,6.48124309171767,-32.7097259013133));
#39940=CARTESIAN_POINT('Ctrl Pts',(-2.12173195195283,6.4281904168494,-32.7013920586206));
#39941=CARTESIAN_POINT('Ctrl Pts',(-2.28767289072268,6.36858239681741,-32.6930582159279));
#39942=CARTESIAN_POINT('Ctrl Pts',(-2.45341824710276,6.30904463237813,-32.6847341957232));
#39943=CARTESIAN_POINT('Ctrl Pts',(-2.61701988034437,6.24296703086413,-32.6764101755184));
#39944=CARTESIAN_POINT('Ctrl Pts',(-2.77793430400726,6.17052428911999,-32.6680861553137));
#39945=CARTESIAN_POINT('Ctrl Pts',(-2.93868857309032,6.09815364804029,-32.6597704198228));
#39946=CARTESIAN_POINT('Ctrl Pts',(-3.09676064591749,6.01943063023907,-32.6514546843319));
#39947=CARTESIAN_POINT('Ctrl Pts',(-3.25162446653574,5.93457895125056,-32.6431389488411));
#39948=CARTESIAN_POINT('Ctrl Pts',(-3.40636252965612,5.84979617625006,-32.634829966161));
#39949=CARTESIAN_POINT('Ctrl Pts',(-3.55789722807418,5.75889482321709,-32.626520983481));
#39950=CARTESIAN_POINT('Ctrl Pts',(-3.70572448192878,5.66214580031578,-32.618212000801));
#39951=CARTESIAN_POINT('Ctrl Pts',(-3.85345876324445,5.56545762547912,-32.6099082438638));
#39952=CARTESIAN_POINT('Ctrl Pts',(-3.9974899566244,5.46292930009872,-32.6016044869267));
#39953=CARTESIAN_POINT('Ctrl Pts',(-4.13734030809213,5.3548766722527,-32.5933007299895));
#39954=CARTESIAN_POINT('Ctrl Pts',(-4.2771338836885,5.24686791116878,-32.5850003441775));
#39955=CARTESIAN_POINT('Ctrl Pts',(-4.41274972461563,5.13333952875915,-32.5766999583655));
#39956=CARTESIAN_POINT('Ctrl Pts',(-4.54374046386894,5.01464969833389,-32.5683995725534));
#39957=CARTESIAN_POINT('Ctrl Pts',(-4.67470358058384,4.89598489650543,-32.5601009370768));
#39958=CARTESIAN_POINT('Ctrl Pts',(-4.80104328110679,4.77216104844101,-32.5518023016001));
#39959=CARTESIAN_POINT('Ctrl Pts',(-4.92234642091017,4.6435756387242,-32.5435036661235));
#39960=CARTESIAN_POINT('Ctrl Pts',(-5.04364411596642,4.51499600062255,-32.5352054031349));
#39961=CARTESIAN_POINT('Ctrl Pts',(-5.15990546228823,4.38165547985473,-32.5269071401463));
#39962=CARTESIAN_POINT('Ctrl Pts',(-5.27075510311867,4.24398746969739,-32.5186088771578));
#39963=CARTESIAN_POINT('Ctrl Pts',(-5.38161816736721,4.10630278853197,-32.510309609285));
#39964=CARTESIAN_POINT('Ctrl Pts',(-5.48706800265771,3.96428984501167,-32.5020103414122));
#39965=CARTESIAN_POINT('Ctrl Pts',(-5.58677025902328,3.81841420918331,-32.4937110735394));
#39966=CARTESIAN_POINT('Ctrl Pts',(-5.68654252244277,3.67243614514644,-32.4854059782429));
#39967=CARTESIAN_POINT('Ctrl Pts',(-5.78055894636304,3.52259025676187,-32.4771008829464));
#39968=CARTESIAN_POINT('Ctrl Pts',(-5.86852867744744,3.36937088519162,-32.4687957876499));
#39969=CARTESIAN_POINT('Ctrl Pts',(-5.95653048687016,3.2160956418712,-32.4604876638838));
#39970=CARTESIAN_POINT('Ctrl Pts',(-6.0384810419881,3.05944476875903,-32.4521795401177));
#39971=CARTESIAN_POINT('Ctrl Pts',(-6.11413591731701,2.89993637595277,-32.4438714163516));
#39972=CARTESIAN_POINT('Ctrl Pts',(-6.18987121334135,2.74025842664641,-32.4355544610979));
#39973=CARTESIAN_POINT('Ctrl Pts',(-6.25929731614242,2.57771720629242,-32.4272375058442));
#39974=CARTESIAN_POINT('Ctrl Pts',(-6.32221791334578,2.41285093948418,-32.4189205505905));
#39975=CARTESIAN_POINT('Ctrl Pts',(-6.36858943617088,2.29134700922621,-32.412791081108));
#39976=CARTESIAN_POINT('Ctrl Pts',(-6.41142852680388,2.16858064488716,-32.4066616116255));
#39977=CARTESIAN_POINT('Ctrl Pts',(-6.4506740762854,2.04477210503751,-32.4005321421429));
#39978=CARTESIAN_POINT('Ctrl Pts',(-6.50830866478331,1.86295138036853,-32.3915306258945));
#39979=CARTESIAN_POINT('Ctrl Pts',(-6.55828335742479,1.67859318478716,-32.3825291096461));
#39980=CARTESIAN_POINT('Ctrl Pts',(-6.60039647752542,1.49233218134237,-32.3735275933976));
#39981=CARTESIAN_POINT('Ctrl Pts',(-6.64245259760231,1.30632328179281,-32.3645382606834));
#39982=CARTESIAN_POINT('Ctrl Pts',(-6.67666832357005,1.11841694940868,-32.3555489279692));
#39983=CARTESIAN_POINT('Ctrl Pts',(-6.70289203373836,0.929261741409192,
-32.346559595255));
#39984=CARTESIAN_POINT('Ctrl Pts',(-6.7290565298193,0.740533652720438,-32.3375905607796));
#39985=CARTESIAN_POINT('Ctrl Pts',(-6.74726499411421,0.550562556810063,
-32.3286215263043));
#39986=CARTESIAN_POINT('Ctrl Pts',(-6.75741703542808,0.360005568438032,
-32.3196524918289));
#39987=CARTESIAN_POINT('Ctrl Pts',(-6.76376784751614,0.240798840667619,
-32.3140417332826));
#39988=CARTESIAN_POINT('Ctrl Pts',(-6.76696687798998,0.121363075749445,
-32.3084309747363));
#39989=CARTESIAN_POINT('Ctrl Pts',(-6.76699974407546,0.00186109715245153,
-32.30282021619));
#39990=CARTESIAN_POINT('',(-6.76699995539293,0.000776989150092258,-32.6971797837746));
#39991=CARTESIAN_POINT('Ctrl Pts',(3.09908550384718,6.01564277861014,-33.3487628447403));
#39992=CARTESIAN_POINT('Ctrl Pts',(2.96644959077812,6.08397297217539,-33.3417357109953));
#39993=CARTESIAN_POINT('Ctrl Pts',(2.8316741744699,6.14785184684299,-33.3347085772502));
#39994=CARTESIAN_POINT('Ctrl Pts',(2.69509059765216,6.20715519948123,-33.3276814435052));
#39995=CARTESIAN_POINT('Ctrl Pts',(2.53103181003941,6.27838803992871,-33.3192407285271));
#39996=CARTESIAN_POINT('Ctrl Pts',(2.36402599205973,6.34316528046175,-33.310800013549));
#39997=CARTESIAN_POINT('Ctrl Pts',(2.19460924522626,6.40124825801714,-33.3023592985709));
#39998=CARTESIAN_POINT('Ctrl Pts',(2.02532055155202,6.45928733372154,-33.2939249634829));
#39999=CARTESIAN_POINT('Ctrl Pts',(1.85362487592134,6.51064212519106,-33.2854906283949));
#40000=CARTESIAN_POINT('Ctrl Pts',(1.68007781421692,6.55512223670742,-33.2770562933069));
#40001=CARTESIAN_POINT('Ctrl Pts',(1.50663527742571,6.59957555848877,-33.2686270380982));
#40002=CARTESIAN_POINT('Ctrl Pts',(1.33134389977629,6.63716237249768,-33.2601977828896));
#40003=CARTESIAN_POINT('Ctrl Pts',(1.15477432116531,6.66774214162314,-33.251768527681));
#40004=CARTESIAN_POINT('Ctrl Pts',(0.978284003443115,6.69830818369721,-33.2433430563079));
#40005=CARTESIAN_POINT('Ctrl Pts',(0.800516956786865,6.72187339571259,-33.2349175849349));
#40006=CARTESIAN_POINT('Ctrl Pts',(0.622054287099278,6.73834827416196,-33.2264921135619));
#40007=CARTESIAN_POINT('Ctrl Pts',(0.443644376154458,6.75481828215928,-33.2180691330027));
#40008=CARTESIAN_POINT('Ctrl Pts',(0.264539583932974,6.76420210609244,-33.2096461524435));
#40009=CARTESIAN_POINT('Ctrl Pts',(0.0853268156944474,6.7664620249081,-33.2012231718842));
#40010=CARTESIAN_POINT('Ctrl Pts',(-0.0938889199359123,6.76872198114334,
-33.1928000518579));
#40011=CARTESIAN_POINT('Ctrl Pts',(-0.273212301935094,6.76385778577173,
-33.1843769318316));
#40012=CARTESIAN_POINT('Ctrl Pts',(-0.452055060805209,6.75188382764399,
-33.1759538118053));
#40013=CARTESIAN_POINT('Ctrl Pts',(-0.630904004356051,6.73990945543681,
-33.1675304004934));
#40014=CARTESIAN_POINT('Ctrl Pts',(-0.80927195886621,6.72082485235693,-33.1591069891815));
#40015=CARTESIAN_POINT('Ctrl Pts',(-0.986574256654533,6.69469642598576,
-33.1506835778697));
#40016=CARTESIAN_POINT('Ctrl Pts',(-1.16390741326628,6.66856345205653,-33.1422587004936));
#40017=CARTESIAN_POINT('Ctrl Pts',(-1.34017421345398,6.63538425927048,-33.1338338231174));
#40018=CARTESIAN_POINT('Ctrl Pts',(-1.51479831322526,6.59527672431187,-33.1254089457413));
#40019=CARTESIAN_POINT('Ctrl Pts',(-1.68947716710864,6.55515661346902,-33.1169814267099));
#40020=CARTESIAN_POINT('Ctrl Pts',(-1.86251196875455,6.50810390387631,-33.1085539076785));
#40021=CARTESIAN_POINT('Ctrl Pts',(-2.03333934774553,6.45428695495558,-33.100126388647));
#40022=CARTESIAN_POINT('Ctrl Pts',(-2.2043199181278,6.40042174507499,-33.0916913121423));
#40023=CARTESIAN_POINT('Ctrl Pts',(-2.37308879208708,6.33978027561281,-33.0832562356375));
#40024=CARTESIAN_POINT('Ctrl Pts',(-2.53909938812987,6.27258027427298,-33.0748211591327));
#40025=CARTESIAN_POINT('Ctrl Pts',(-2.70519021818626,6.20534779473026,-33.0663820058999));
#40026=CARTESIAN_POINT('Ctrl Pts',(-2.86851980578215,6.13155059409251,-33.0579428526671));
#40027=CARTESIAN_POINT('Ctrl Pts',(-3.0285636768799,6.05145363157347,-33.0495036994344));
#40028=CARTESIAN_POINT('Ctrl Pts',(-3.18878540159028,5.9712676588721,-33.0410551679362));
#40029=CARTESIAN_POINT('Ctrl Pts',(-3.34571381937356,5.88476809221298,-33.0326066364382));
#40030=CARTESIAN_POINT('Ctrl Pts',(-3.49885002351674,5.79226531789911,-33.02415810494));
#40031=CARTESIAN_POINT('Ctrl Pts',(-3.5834627448222,5.74115453383082,-33.0194900171741));
#40032=CARTESIAN_POINT('Ctrl Pts',(-3.66691824116116,5.68821179022224,-33.0148219294081));
#40033=CARTESIAN_POINT('Ctrl Pts',(-3.74913639405821,5.63349494530244,-33.0101538416421));
#40034=CARTESIAN_POINT('Ctrl Pts',(-3.8942796265701,5.53690095158362,-33.0019130660453));
#40035=CARTESIAN_POINT('Ctrl Pts',(-4.03588784783809,5.43456073571528,-32.9936722904486));
#40036=CARTESIAN_POINT('Ctrl Pts',(-4.1734780613004,5.3267597910779,-32.9854315148518));
#40037=CARTESIAN_POINT('Ctrl Pts',(-4.31091587868448,5.21907824767393,-32.9771998668075));
#40038=CARTESIAN_POINT('Ctrl Pts',(-4.44434427217922,5.105948236368,-32.9689682187631));
#40039=CARTESIAN_POINT('Ctrl Pts',(-4.57330782221945,4.98769932566373,-32.9607365707188));
#40040=CARTESIAN_POINT('Ctrl Pts',(-4.70215151365581,4.86956031538746,-32.9525125731605));
#40041=CARTESIAN_POINT('Ctrl Pts',(-4.82653836504406,4.74631211946352,-32.9442885756022));
#40042=CARTESIAN_POINT('Ctrl Pts',(-4.94604469392578,4.61832554998981,-32.9360645780439));
#40043=CARTESIAN_POINT('Ctrl Pts',(-5.06544543850151,4.4904520571476,-32.9278478464194));
#40044=CARTESIAN_POINT('Ctrl Pts',(-5.17997401287459,4.3578487936894,-32.9196311147949));
#40045=CARTESIAN_POINT('Ctrl Pts',(-5.28924248288343,4.22092441975229,-32.9114143831704));
#40046=CARTESIAN_POINT('Ctrl Pts',(-5.39845497060967,4.08407019724126,-32.9032018612817));
#40047=CARTESIAN_POINT('Ctrl Pts',(-5.50241249986528,3.94289955080353,-32.894989339393));
#40048=CARTESIAN_POINT('Ctrl Pts',(-5.60076617008913,3.79785561968661,-32.8867768175043));
#40049=CARTESIAN_POINT('Ctrl Pts',(-5.69908695037244,3.65286019195811,-32.8785670419225));
#40050=CARTESIAN_POINT('Ctrl Pts',(-5.79180740530984,3.50399435397829,-32.8703572663407));
#40051=CARTESIAN_POINT('Ctrl Pts',(-5.8786208305718,3.35173181062675,-32.8621474907588));
#40052=CARTESIAN_POINT('Ctrl Pts',(-5.91653867929808,3.28522748749861,-32.8585616740761));
#40053=CARTESIAN_POINT('Ctrl Pts',(-5.95333019236971,3.21807554308386,-32.8549758573934));
#40054=CARTESIAN_POINT('Ctrl Pts',(-5.98897247047381,3.15031708688297,-32.8513900407106));
#40055=CARTESIAN_POINT('Ctrl Pts',(-6.07640315339711,2.98410526164082,-32.8425940148087));
#40056=CARTESIAN_POINT('Ctrl Pts',(-6.15682981791816,2.81440555629455,-32.8337979889067));
#40057=CARTESIAN_POINT('Ctrl Pts',(-6.23001551085722,2.6418167488451,-32.8250019630047));
#40058=CARTESIAN_POINT('Ctrl Pts',(-6.30332443844021,2.46893732557474,-32.8161911258046));
#40059=CARTESIAN_POINT('Ctrl Pts',(-6.36936792808263,2.29315932964415,-32.8073802886045));
#40060=CARTESIAN_POINT('Ctrl Pts',(-6.42795827965447,2.11509842679285,-32.7985694514043));
#40061=CARTESIAN_POINT('Ctrl Pts',(-6.48670226317345,1.93657062380388,-32.7897355109792));
#40062=CARTESIAN_POINT('Ctrl Pts',(-6.53795392300957,1.75574819589847,-32.7809015705541));
#40063=CARTESIAN_POINT('Ctrl Pts',(-6.58157557974711,1.57326154471419,-32.7720676301289));
#40064=CARTESIAN_POINT('Ctrl Pts',(-6.62525363021519,1.39053897624012,-32.7632222692559));
#40065=CARTESIAN_POINT('Ctrl Pts',(-6.6612819206485,1.20614815230693,-32.754376908383));
#40066=CARTESIAN_POINT('Ctrl Pts',(-6.68957426973306,1.0207277255593,-32.74553154751));
#40067=CARTESIAN_POINT('Ctrl Pts',(-6.71792717479372,0.834910431273443,
-32.7366672543292));
#40068=CARTESIAN_POINT('Ctrl Pts',(-6.73851098454875,0.648059395695866,
-32.7278029611484));
#40069=CARTESIAN_POINT('Ctrl Pts',(-6.75129134058409,0.460819090917759,
-32.7189386679676));
#40070=CARTESIAN_POINT('Ctrl Pts',(-6.76174851149789,0.307614918545673,
-32.7116857065818));
#40071=CARTESIAN_POINT('Ctrl Pts',(-6.76698234500998,0.154150231762921,
-32.7044327451959));
#40072=CARTESIAN_POINT('Ctrl Pts',(-6.76699995539284,0.000776989901219398,
-32.6971797838101));
#40073=CARTESIAN_POINT('Ctrl Pts',(-6.76699995539293,0.000776989150042673,
-32.6971797837746));
#40074=CARTESIAN_POINT('Ctrl Pts',(-6.76700364076461,-0.0313198683675472,
-32.695661935776));
#40075=CARTESIAN_POINT('Ctrl Pts',(-6.76677896688004,-0.0634170283982404,
-32.6941440877775));
#40076=CARTESIAN_POINT('Ctrl Pts',(-6.76632591716142,-0.0955122125681283,
-32.692626239779));
#40077=CARTESIAN_POINT('Ctrl Pts',(-6.76387121201341,-0.269409713373156,
-32.6844022653615));
#40078=CARTESIAN_POINT('Ctrl Pts',(-6.75470508379871,-0.44344307132773,
-32.6761782909439));
#40079=CARTESIAN_POINT('Ctrl Pts',(-6.73880799304889,-0.617054157121077,
-32.6679543165263));
#40080=CARTESIAN_POINT('Ctrl Pts',(-6.72292769116931,-0.790481892763339,
-32.6597390274237));
#40081=CARTESIAN_POINT('Ctrl Pts',(-6.70033061469403,-0.963487890154671,
-32.651523738321));
#40082=CARTESIAN_POINT('Ctrl Pts',(-6.67104922470096,-1.13551364660086,
-32.6433084492184));
#40083=CARTESIAN_POINT('Ctrl Pts',(-6.64179288547393,-1.30739223185811,
-32.6351001884462));
#40084=CARTESIAN_POINT('Ctrl Pts',(-6.60586368163906,-1.47829189483929,
-32.626891927674));
#40085=CARTESIAN_POINT('Ctrl Pts',(-6.56334590791908,-1.6476587914377,-32.6186836669018));
#40086=CARTESIAN_POINT('Ctrl Pts',(-6.52085598320365,-1.81691475326548,
-32.6104807825139));
#40087=CARTESIAN_POINT('Ctrl Pts',(-6.47178617161156,-1.98463960192755,
-32.6022778981261));
#40088=CARTESIAN_POINT('Ctrl Pts',(-6.41627193933049,-2.15028914347818,
-32.5940750137382));
#40089=CARTESIAN_POINT('Ctrl Pts',(-6.36078293916598,-2.31586339463268,
-32.585875857694));
#40090=CARTESIAN_POINT('Ctrl Pts',(-6.29885546754327,-2.47936387858849,
-32.5776767016497));
#40091=CARTESIAN_POINT('Ctrl Pts',(-6.23067501123257,-2.64026095384566,
-32.5694775456055));
#40092=CARTESIAN_POINT('Ctrl Pts',(-6.1625004849638,-2.80114403496942,-32.5612791026885));
#40093=CARTESIAN_POINT('Ctrl Pts',(-6.0880741892412,-2.9594238251642,-32.5530806597715));
#40094=CARTESIAN_POINT('Ctrl Pts',(-6.00763012443662,-3.11458974633285,
-32.5448822168545));
#40095=CARTESIAN_POINT('Ctrl Pts',(-5.92718686075979,-3.2697541222324,-32.5366838555843));
#40096=CARTESIAN_POINT('Ctrl Pts',(-5.8407261115259,-3.42180437193956,-32.528485494314));
#40097=CARTESIAN_POINT('Ctrl Pts',(-5.74852824819261,-3.57025376965442,
-32.5202871330438));
#40098=CARTESIAN_POINT('Ctrl Pts',(-5.6563145546388,-3.71872865588514,-32.5120873641285));
#40099=CARTESIAN_POINT('Ctrl Pts',(-5.55836197372408,-3.86360115364792,
-32.5038875952133));
#40100=CARTESIAN_POINT('Ctrl Pts',(-5.45499470992903,-4.00441278025209,
-32.495687826298));
#40101=CARTESIAN_POINT('Ctrl Pts',(-5.35159092054627,-4.14527416368671,
-32.4874851599337));
#40102=CARTESIAN_POINT('Ctrl Pts',(-5.24276884905177,-4.28207152856614,
-32.4792824935694));
#40103=CARTESIAN_POINT('Ctrl Pts',(-5.12889356935204,-4.41437875065782,
-32.4710798272051));
#40104=CARTESIAN_POINT('Ctrl Pts',(-5.01488895579823,-4.54683624068299,
-32.4628678446621));
#40105=CARTESIAN_POINT('Ctrl Pts',(-4.89581990250523,-4.67479312761385,
-32.454655862119));
#40106=CARTESIAN_POINT('Ctrl Pts',(-4.77208972971953,-4.79785875276725,
-32.446443879576));
#40107=CARTESIAN_POINT('Ctrl Pts',(-4.64828657920569,-4.92099696368963,
-32.4382270534947));
#40108=CARTESIAN_POINT('Ctrl Pts',(-4.51981709256398,-5.0392379196295,-32.4300102274134));
#40109=CARTESIAN_POINT('Ctrl Pts',(-4.38711829001342,-5.15223078961237,
-32.4217934013322));
#40110=CARTESIAN_POINT('Ctrl Pts',(-4.254214846744,-5.26539791092002,-32.4135639037183));
#40111=CARTESIAN_POINT('Ctrl Pts',(-4.11706933552169,-5.3733005512914,-32.4053344061045));
#40112=CARTESIAN_POINT('Ctrl Pts',(-3.97614948353633,-5.47563003539993,
-32.3971049084906));
#40113=CARTESIAN_POINT('Ctrl Pts',(-3.85053953188731,-5.56684217740868,
-32.3897694849658));
#40114=CARTESIAN_POINT('Ctrl Pts',(-3.72193134591881,-5.65362687499,-32.3824340614409));
#40115=CARTESIAN_POINT('Ctrl Pts',(-3.59067229527631,-5.7357964981278,-32.3750986379161));
#40116=CARTESIAN_POINT('Ctrl Pts',(-3.44625326412708,-5.82620441518474,
-32.3670277677297));
#40117=CARTESIAN_POINT('Ctrl Pts',(-3.29815374402904,-5.91131939795726,
-32.3589568975433));
#40118=CARTESIAN_POINT('Ctrl Pts',(-3.14680608435033,-5.99081801321787,
-32.3508860273568));
#40119=CARTESIAN_POINT('Ctrl Pts',(-2.9956467650705,-6.07021769863087,-32.3428252007411));
#40120=CARTESIAN_POINT('Ctrl Pts',(-2.84124767496596,-6.14401475190585,
-32.3347643741253));
#40121=CARTESIAN_POINT('Ctrl Pts',(-2.68407132278089,-6.21192805288545,
-32.3267035475095));
#40122=CARTESIAN_POINT('Ctrl Pts',(-2.52705609797334,-6.27977173339141,
-32.3186509843496));
#40123=CARTESIAN_POINT('Ctrl Pts',(-2.36726961640093,-6.34174351812268,
-32.3105984211897));
#40124=CARTESIAN_POINT('Ctrl Pts',(-2.20520016739459,-6.39760746074053,
-32.3025458580298));
#40125=CARTESIAN_POINT('Ctrl Pts',(-2.04326137466428,-6.45342636726582,
-32.2944997866419));
#40126=CARTESIAN_POINT('Ctrl Pts',(-1.87904362853917,-6.50314711120076,
-32.2864537152541));
#40127=CARTESIAN_POINT('Ctrl Pts',(-1.71305634720513,-6.54658131785593,
-32.2784076438662));
#40128=CARTESIAN_POINT('Ctrl Pts',(-1.54716657277489,-6.58999000969468,
-32.2703662990303));
#40129=CARTESIAN_POINT('Ctrl Pts',(-1.37950969241191,-6.62711942168255,
-32.2623249541944));
#40130=CARTESIAN_POINT('Ctrl Pts',(-1.21061137812345,-6.65783065954355,
-32.2542836093585));
#40131=CARTESIAN_POINT('Ctrl Pts',(-1.03845722403718,-6.68913391557174,
-32.2460872521374));
#40132=CARTESIAN_POINT('Ctrl Pts',(-0.865013660771462,-6.71376890035964,
-32.2378908949164));
#40133=CARTESIAN_POINT('Ctrl Pts',(-0.690849936269294,-6.73164284298838,
-32.2296945376953));
#40134=CARTESIAN_POINT('Ctrl Pts',(-0.520034372208636,-6.74917317314665,
-32.2216557489868));
#40135=CARTESIAN_POINT('Ctrl Pts',(-0.348526471807505,-6.76020003690927,
-32.2136169602783));
#40136=CARTESIAN_POINT('Ctrl Pts',(-0.176869554794799,-6.76468817910972,
-32.2055781715698));
#40137=CARTESIAN_POINT('Ctrl Pts',(-0.00519426893594305,-6.76917680158205,
-32.197538522638));
#40138=CARTESIAN_POINT('Ctrl Pts',(0.166629691918991,-6.76712529941602,
-32.1894988737063));
#40139=CARTESIAN_POINT('Ctrl Pts',(0.338058236840963,-6.7585505567765,-32.1814592247745));
#40140=CARTESIAN_POINT('Ctrl Pts',(0.509539069676452,-6.74997319873007,
-32.1734171236463));
#40141=CARTESIAN_POINT('Ctrl Pts',(0.680623873718714,-6.73486865842038,
-32.1653750225181));
#40142=CARTESIAN_POINT('Ctrl Pts',(0.850773058213182,-6.71330575822512,
-32.1573329213899));
#40143=CARTESIAN_POINT('Ctrl Pts',(1.02666410918672,-6.69101519486657,-32.1490194309452));
#40144=CARTESIAN_POINT('Ctrl Pts',(1.20155485529246,-6.66182281114754,-32.1407059405004));
#40145=CARTESIAN_POINT('Ctrl Pts',(1.37486108899908,-6.6258619051378,-32.1323924500557));
#40146=CARTESIAN_POINT('Ctrl Pts',(1.54280516780542,-6.59101364201605,-32.1243361818849));
#40147=CARTESIAN_POINT('Ctrl Pts',(1.70926098515278,-6.54980961983952,-32.1162799137142));
#40148=CARTESIAN_POINT('Ctrl Pts',(1.87371326938176,-6.50242167074258,-32.1082236455434));
#40149=CARTESIAN_POINT('Ctrl Pts',(2.04604155580157,-6.45276420260152,-32.0997815439617));
#40150=CARTESIAN_POINT('Ctrl Pts',(2.21616922062781,-6.39631606958526,-32.0913394423799));
#40151=CARTESIAN_POINT('Ctrl Pts',(2.38352855884928,-6.33333092528331,-32.0828973407982));
#40152=CARTESIAN_POINT('Ctrl Pts',(2.55088789707078,-6.27034578098134,-32.0744552392165));
#40153=CARTESIAN_POINT('Ctrl Pts',(2.71547851777711,-6.20082388437573,-32.0660131376348));
#40154=CARTESIAN_POINT('Ctrl Pts',(2.87676452164858,-6.12507264340465,-32.057571036053));
#40155=CARTESIAN_POINT('Ctrl Pts',(3.03598224389287,-6.05029281282366,-32.0492371933604));
#40156=CARTESIAN_POINT('Ctrl Pts',(3.19248603147525,-5.96920526117568,-32.0409033506677));
#40157=CARTESIAN_POINT('Ctrl Pts',(3.34574921568815,-5.88202781238938,-32.032569507975));
#40158=CARTESIAN_POINT('Ctrl Pts',(3.49883175984881,-5.79495311325547,-32.0242454877702));
#40159=CARTESIAN_POINT('Ctrl Pts',(3.64868100957273,-5.70180298615775,-32.0159214675655));
#40160=CARTESIAN_POINT('Ctrl Pts',(3.79479148025796,-5.60284272680945,-32.0075974473608));
#40161=CARTESIAN_POINT('Ctrl Pts',(3.94075653041124,-5.50398096042671,-31.9992817118699));
#40162=CARTESIAN_POINT('Ctrl Pts',(4.08298992903231,-5.3993207767074,-31.9909659763791));
#40163=CARTESIAN_POINT('Ctrl Pts',(4.22101176860237,-5.28917277552174,-31.9826502408882));
#40164=CARTESIAN_POINT('Ctrl Pts',(4.35892152724194,-5.17911422025639,-31.9743412582082));
#40165=CARTESIAN_POINT('Ctrl Pts',(4.4926262708117,-5.06357694335015,-31.9660322755281));
#40166=CARTESIAN_POINT('Ctrl Pts',(4.62167583407019,-4.94291427042505,-31.9577232928481));
#40167=CARTESIAN_POINT('Ctrl Pts',(4.75064423458499,-4.82232748550259,-31.9494195359109));
#40168=CARTESIAN_POINT('Ctrl Pts',(4.87496303615949,-4.69662196554811,-31.9411157789737));
#40169=CARTESIAN_POINT('Ctrl Pts',(4.99421571495734,-4.56619079676629,-31.9328120220365));
#40170=CARTESIAN_POINT('Ctrl Pts',(5.11341998004209,-4.43581257989507,-31.9245116362245));
#40171=CARTESIAN_POINT('Ctrl Pts',(5.22756198620456,-4.30071279324783,-31.9162112504125));
#40172=CARTESIAN_POINT('Ctrl Pts',(5.33626240364882,-4.16132101133813,-31.9079108646005));
#40173=CARTESIAN_POINT('Ctrl Pts',(5.4449398990034,-4.02195862352828,-31.8996122291238));
#40174=CARTESIAN_POINT('Ctrl Pts',(5.5481778779696,-3.87830631767617,-31.8913135936472));
#40175=CARTESIAN_POINT('Ctrl Pts',(5.64563746672557,-3.73082652964521,-31.8830149581705));
#40176=CARTESIAN_POINT('Ctrl Pts',(5.7430926809631,-3.58335336131232,-31.874716695182));
#40177=CARTESIAN_POINT('Ctrl Pts',(5.83476983025493,-3.43205334338494,-31.8664184321934));
#40178=CARTESIAN_POINT('Ctrl Pts',(5.9203734258444,-3.2774178095805,-31.8581201692048));
#40179=CARTESIAN_POINT('Ctrl Pts',(6.00598738766399,-3.12276355007282,-31.849820901332));
#40180=CARTESIAN_POINT('Ctrl Pts',(6.08552616234302,-2.9647732743823,-31.8415216334592));
#40181=CARTESIAN_POINT('Ctrl Pts',(6.15874017766571,-2.80396298549145,-31.8332223655864));
#40182=CARTESIAN_POINT('Ctrl Pts',(6.23200560102765,-2.64303978185873,-31.8249172702899));
#40183=CARTESIAN_POINT('Ctrl Pts',(6.29893724685141,-2.47929292533969,-31.8166121749934));
#40184=CARTESIAN_POINT('Ctrl Pts',(6.35933332849873,-2.31325930605396,-31.8083070796969));
#40185=CARTESIAN_POINT('Ctrl Pts',(6.41975143369796,-2.14716514227706,-31.7999989559308));
#40186=CARTESIAN_POINT('Ctrl Pts',(6.47362911274582,-1.9787828830234,-31.7916908321647));
#40187=CARTESIAN_POINT('Ctrl Pts',(6.52081439472444,-1.80866487486061,-31.7833827083986));
#40188=CARTESIAN_POINT('Ctrl Pts',(6.56804983438527,-1.63836603223771,-31.7750657531449));
#40189=CARTESIAN_POINT('Ctrl Pts',(6.60857857753647,-1.46632809152995,-31.7667487978912));
#40190=CARTESIAN_POINT('Ctrl Pts',(6.64229950269269,-1.29311496647761,-31.7584318426375));
#40191=CARTESIAN_POINT('Ctrl Pts',(6.66715131148143,-1.16545952868767,-31.752302373155));
#40192=CARTESIAN_POINT('Ctrl Pts',(6.68830654293802,-1.03716602112991,-31.7461729036724));
#40193=CARTESIAN_POINT('Ctrl Pts',(6.7057427584848,-0.908461918315057,-31.7400434341898));
#40194=CARTESIAN_POINT('Ctrl Pts',(6.72978299038332,-0.731010769603445,
-31.7315924106647));
#40195=CARTESIAN_POINT('Ctrl Pts',(6.74679555423204,-0.552454660540933,
-31.7231413871395));
#40196=CARTESIAN_POINT('Ctrl Pts',(6.75669149813917,-0.37337514509378,-31.7146903636143));
#40197=CARTESIAN_POINT('Ctrl Pts',(6.76657872896178,-0.19445330383817,-31.7062467809642));
#40198=CARTESIAN_POINT('Ctrl Pts',(6.76936181090752,-0.0150093041905303,
-31.6978031983141));
#40199=CARTESIAN_POINT('Ctrl Pts',(6.76500345896609,0.164369097390344,-31.689359615664));
#40200=CARTESIAN_POINT('Ctrl Pts',(6.76064835195343,0.343613946164104,-31.6809223195242));
#40201=CARTESIAN_POINT('Ctrl Pts',(6.74916241830657,0.522792963925201,-31.6724850233844));
#40202=CARTESIAN_POINT('Ctrl Pts',(6.73056042233343,0.701316905057112,-31.6640477272445));
#40203=CARTESIAN_POINT('Ctrl Pts',(6.71197169746612,0.879713482968431,-31.6556164504722));
#40204=CARTESIAN_POINT('Ctrl Pts',(6.68627707100798,1.05745558755062,-31.6471851736999));
#40205=CARTESIAN_POINT('Ctrl Pts',(6.65354327729324,1.23395739682776,-31.6387538969276));
#40206=CARTESIAN_POINT('Ctrl Pts',(6.62082351446716,1.41038355104167,-31.6303262341056));
#40207=CARTESIAN_POINT('Ctrl Pts',(6.58107065972707,1.58557014445998,-31.6218985712836));
#40208=CARTESIAN_POINT('Ctrl Pts',(6.5344029435084,1.75893921778688,-31.6134709084617));
#40209=CARTESIAN_POINT('Ctrl Pts',(6.48774959345892,1.93225492125471,-31.6050458400077));
#40210=CARTESIAN_POINT('Ctrl Pts',(6.43418571309681,2.10375390070893,-31.5966207715538));
#40211=CARTESIAN_POINT('Ctrl Pts',(6.3738801113642,2.27287072354674,-31.5881957030998));
#40212=CARTESIAN_POINT('Ctrl Pts',(6.35737865282271,2.31914626280926,-31.585890346486));
#40213=CARTESIAN_POINT('Ctrl Pts',(6.34037270536527,2.3652435259633,-31.5835849898723));
#40214=CARTESIAN_POINT('Ctrl Pts',(6.32286637598616,2.41115113409002,-31.5812796332585));
#40215=CARTESIAN_POINT('Ctrl Pts',(6.25741582871609,2.58278494782026,-31.572660644734));
#40216=CARTESIAN_POINT('Ctrl Pts',(6.18499657830533,2.75168975055454,-31.5640416562095));
#40217=CARTESIAN_POINT('Ctrl Pts',(6.10586728046743,2.91730590670867,-31.555422667685));
#40218=CARTESIAN_POINT('Ctrl Pts',(6.0266905771185,3.08302128172017,-31.5467985156172));
#40219=CARTESIAN_POINT('Ctrl Pts',(5.94079593493681,3.24544380381087,-31.5381743635494));
#40220=CARTESIAN_POINT('Ctrl Pts',(5.84848822186665,3.40403797256833,-31.5295502114816));
#40221=CARTESIAN_POINT('Ctrl Pts',(5.75301894479092,3.56806403427124,-31.5206306798854));
#40222=CARTESIAN_POINT('Ctrl Pts',(5.65068970730467,3.72799455010796,-31.5117111482892));
#40223=CARTESIAN_POINT('Ctrl Pts',(5.54188643122727,3.88326972838342,-31.5027916166929));
#40224=CARTESIAN_POINT('Ctrl Pts',(5.43649031272387,4.03368248873555,-31.4941513988337));
#40225=CARTESIAN_POINT('Ctrl Pts',(5.32501970799295,4.17972684724951,-31.4855111809744));
#40226=CARTESIAN_POINT('Ctrl Pts',(5.2078667173747,4.32092736042402,-31.4768709631152));
#40227=CARTESIAN_POINT('Ctrl Pts',(5.08503289090163,4.46897479174999,-31.4678117746505));
#40228=CARTESIAN_POINT('Ctrl Pts',(4.95595215179736,4.61169664779443,-31.4587525861858));
#40229=CARTESIAN_POINT('Ctrl Pts',(4.82112061059534,4.74858769089219,-31.4496933977211));
#40230=CARTESIAN_POINT('Ctrl Pts',(4.68628906939334,4.88547873398993,-31.4406342092564));
#40231=CARTESIAN_POINT('Ctrl Pts',(4.54570702855292,5.01653872745792,-31.4315750207917));
#40232=CARTESIAN_POINT('Ctrl Pts',(4.39991149110873,5.14130993720563,-31.422515832327));
#40233=CARTESIAN_POINT('Ctrl Pts',(4.25436304851726,5.26586968421424,-31.4134719974107));
#40234=CARTESIAN_POINT('Ctrl Pts',(4.10348522547124,5.38427734437918,-31.4044281624944));
#40235=CARTESIAN_POINT('Ctrl Pts',(3.94779719257886,5.49610646969894,-31.3953843275781));
#40236=CARTESIAN_POINT('Ctrl Pts',(3.79229985677368,5.6077986192469,-31.3863515701541));
#40237=CARTESIAN_POINT('Ctrl Pts',(3.63200427101384,5.71292818765523,-31.37731881273));
#40238=CARTESIAN_POINT('Ctrl Pts',(3.46746036859561,5.81111070211357,-31.368286055306));
#40239=CARTESIAN_POINT('Ctrl Pts',(3.34687412860517,5.88306390169944,-31.3616663857922));
#40240=CARTESIAN_POINT('Ctrl Pts',(3.2240069292606,5.95128686638822,-31.3550467162785));
#40241=CARTESIAN_POINT('Ctrl Pts',(3.0990855038472,6.01564277861013,-31.3484270467647));
#40242=CARTESIAN_POINT('Origin',(0.,0.,-63.6971797838103));
#40243=CARTESIAN_POINT('',(3.09908550384723,6.01564277861011,-28.9543744409077));
#40244=CARTESIAN_POINT('',(3.09908550384723,6.01564277861011,-29.348603209574));
#40245=CARTESIAN_POINT('',(3.09908550384721,6.01564277861012,-63.6971797838103));
#40246=CARTESIAN_POINT('',(-6.76699999859312,0.000137987943152793,-30.3028202161642));
#40247=CARTESIAN_POINT('Ctrl Pts',(-6.76699999859312,0.000137987943145954,
-30.3028202161641));
#40248=CARTESIAN_POINT('Ctrl Pts',(-6.76700388479958,-0.190443583885455,
-30.2938915872868));
#40249=CARTESIAN_POINT('Ctrl Pts',(-6.75895235621057,-0.380837284568577,
-30.2849629584095));
#40250=CARTESIAN_POINT('Ctrl Pts',(-6.74291859928137,-0.570383873777514,
-30.2760343295323));
#40251=CARTESIAN_POINT('Ctrl Pts',(-6.72683535805985,-0.760515452447654,
-30.2670781446128));
#40252=CARTESIAN_POINT('Ctrl Pts',(-6.70272060340288,-0.949794440188979,
-30.2581219596934));
#40253=CARTESIAN_POINT('Ctrl Pts',(-6.67069935526168,-1.13756718997665,
-30.249165774774));
#40254=CARTESIAN_POINT('Ctrl Pts',(-6.63863002257894,-1.32562190774221,
-30.2401961408459));
#40255=CARTESIAN_POINT('Ctrl Pts',(-6.59863052172635,-1.51216562698233,
-30.2312265069177));
#40256=CARTESIAN_POINT('Ctrl Pts',(-6.55087651698734,-1.69655706039727,
-30.2222568729896));
#40257=CARTESIAN_POINT('Ctrl Pts',(-6.50301856834516,-1.88134985000013,
-30.2132677152798));
#40258=CARTESIAN_POINT('Ctrl Pts',(-6.44737241789432,-2.06398074481492,
-30.20427855757));
#40259=CARTESIAN_POINT('Ctrl Pts',(-6.38416375623423,-2.24382310657175,
-30.1952893998603));
#40260=CARTESIAN_POINT('Ctrl Pts',(-6.34326185575947,-2.36019789111124,
-30.1894725762741));
#40261=CARTESIAN_POINT('Ctrl Pts',(-6.29919429622271,-2.47540542601184,
-30.1836557526879));
#40262=CARTESIAN_POINT('Ctrl Pts',(-6.25203279118684,-2.58928078390979,
-30.1778389291016));
#40263=CARTESIAN_POINT('Ctrl Pts',(-6.18351378203424,-2.75472560345341,
-30.1693879055764));
#40264=CARTESIAN_POINT('Ctrl Pts',(-6.10836566388483,-2.91758895645562,
-30.1609368820512));
#40265=CARTESIAN_POINT('Ctrl Pts',(-6.0268042065883,-3.07732352141428,-30.152485858526));
#40266=CARTESIAN_POINT('Ctrl Pts',(-5.94531456173106,-3.23691744483554,
-30.1440422758759));
#40267=CARTESIAN_POINT('Ctrl Pts',(-5.8574229828226,-3.39338777720544,-30.1355986932257));
#40268=CARTESIAN_POINT('Ctrl Pts',(-5.76339300972036,-3.54620783591522,
-30.1271551105756));
#40269=CARTESIAN_POINT('Ctrl Pts',(-5.66943304486209,-3.69891411533101,
-30.1187178144358));
#40270=CARTESIAN_POINT('Ctrl Pts',(-5.56934396948447,-3.84797525737609,
-30.1102805182959));
#40271=CARTESIAN_POINT('Ctrl Pts',(-5.46343505218162,-3.99288948389424,
-30.101843222156));
#40272=CARTESIAN_POINT('Ctrl Pts',(-5.35760169281609,-4.13770032516097,
-30.0934119453837));
#40273=CARTESIAN_POINT('Ctrl Pts',(-5.24595696853239,-4.27836988515905,
-30.0849806686113));
#40274=CARTESIAN_POINT('Ctrl Pts',(-5.12885333600842,-4.41442549577126,
-30.076549391839));
#40275=CARTESIAN_POINT('Ctrl Pts',(-5.01179989834027,-4.55042278802381,
-30.068121729017));
#40276=CARTESIAN_POINT('Ctrl Pts',(-4.88929243294571,-4.68180982275689,
-30.0596940661951));
#40277=CARTESIAN_POINT('Ctrl Pts',(-4.76172394130033,-4.80814663949086,
-30.0512664033731));
#40278=CARTESIAN_POINT('Ctrl Pts',(-4.63419472028228,-4.93444456475575,
-30.0428413349191));
#40279=CARTESIAN_POINT('Ctrl Pts',(-4.50160781528299,-5.05569513941955,
-30.0344162664651));
#40280=CARTESIAN_POINT('Ctrl Pts',(-4.36439363267744,-5.17149467939827,
-30.0259911980111));
#40281=CARTESIAN_POINT('Ctrl Pts',(-4.32684763230044,-5.20318097806753,
-30.0236858413975));
#40282=CARTESIAN_POINT('Ctrl Pts',(-4.28895537736297,-5.23445935613614,
-30.0213804847839));
#40283=CARTESIAN_POINT('Ctrl Pts',(-4.25072614289869,-5.26532204694809,
-30.0190751281703));
#40284=CARTESIAN_POINT('Ctrl Pts',(-4.10779930407347,-5.38070774318834,
-30.0104561396458));
#40285=CARTESIAN_POINT('Ctrl Pts',(-3.96022357502899,-5.49022844631624,
-30.0018371511213));
#40286=CARTESIAN_POINT('Ctrl Pts',(-3.80850408783043,-5.59353069295047,
-29.9932181625969));
#40287=CARTESIAN_POINT('Ctrl Pts',(-3.65669370711997,-5.69689482684885,
-29.9845940105291));
#40288=CARTESIAN_POINT('Ctrl Pts',(-3.50073486539035,-5.79403289829253,
-29.9759698584614));
#40289=CARTESIAN_POINT('Ctrl Pts',(-3.34116048499428,-5.88463555485918,
-29.9673457063936));
#40290=CARTESIAN_POINT('Ctrl Pts',(-3.17612063913872,-5.97834137678842,
-29.9584261747974));
#40291=CARTESIAN_POINT('Ctrl Pts',(-3.0072135185948,-6.06505600859998,-29.9495066432011));
#40292=CARTESIAN_POINT('Ctrl Pts',(-2.8350543133621,-6.1444898926019,-29.9405871116049));
#40293=CARTESIAN_POINT('Ctrl Pts',(-2.66828624671713,-6.22143631694905,
-29.9319468937456));
#40294=CARTESIAN_POINT('Ctrl Pts',(-2.49846698929844,-6.2915510100068,-29.9233066758864));
#40295=CARTESIAN_POINT('Ctrl Pts',(-2.32617462618558,-6.35462041419394,
-29.9146664580271));
#40296=CARTESIAN_POINT('Ctrl Pts',(-2.14552767793693,-6.42074810081001,
-29.9056072695623));
#40297=CARTESIAN_POINT('Ctrl Pts',(-1.96216218528791,-6.47913013149219,
-29.8965480810976));
#40298=CARTESIAN_POINT('Ctrl Pts',(-1.77676110815794,-6.52957953964399,
-29.8874888926328));
#40299=CARTESIAN_POINT('Ctrl Pts',(-1.59136003102797,-6.58002894779578,
-29.8784297041681));
#40300=CARTESIAN_POINT('Ctrl Pts',(-1.40392374989238,-6.62254568108135,
-29.8693705157033));
#40301=CARTESIAN_POINT('Ctrl Pts',(-1.21514665878078,-6.65700440120434,
-29.8603113272386));
#40302=CARTESIAN_POINT('Ctrl Pts',(-1.02669661073589,-6.69140342401216,
-29.8512678331823));
#40303=CARTESIAN_POINT('Ctrl Pts',(-0.836736937202911,-6.71780485300529,
-29.842224339126));
#40304=CARTESIAN_POINT('Ctrl Pts',(-0.645930803590734,-6.73610142418986,
-29.8331808450697));
#40305=CARTESIAN_POINT('Ctrl Pts',(-0.455299199650862,-6.75438125956771,
-29.8241456230643));
#40306=CARTESIAN_POINT('Ctrl Pts',(-0.263822918229505,-6.76457101547801,
-29.815110401059));
#40307=CARTESIAN_POINT('Ctrl Pts',(-0.0721712101117952,-6.76661512991769,
-29.8060751790536));
#40308=CARTESIAN_POINT('Ctrl Pts',(0.11914284941797,-6.76865564307273,-29.7970558751425));
#40309=CARTESIAN_POINT('Ctrl Pts',(0.310631480718239,-6.76257916907742,
-29.7880365712314));
#40310=CARTESIAN_POINT('Ctrl Pts',(0.501624621187765,-6.7483821571854,-29.7790172673203));
#40311=CARTESIAN_POINT('Ctrl Pts',(0.692378147423253,-6.73420295643634,
-29.7700092787558));
#40312=CARTESIAN_POINT('Ctrl Pts',(0.882637186657034,-6.71192356669804,
-29.7610012901914));
#40313=CARTESIAN_POINT('Ctrl Pts',(1.07173342245696,-6.68159236044737,-29.7519933016269));
#40314=CARTESIAN_POINT('Ctrl Pts',(1.2604025777839,-6.65132965828859,-29.7430056579202));
#40315=CARTESIAN_POINT('Ctrl Pts',(1.44791393722817,-6.61305147679858,-29.7340180142136));
#40316=CARTESIAN_POINT('Ctrl Pts',(1.63360650694425,-6.56685760318201,-29.7250303705069));
#40317=CARTESIAN_POINT('Ctrl Pts',(1.79533186477981,-6.5266259409681,-29.7172027557736));
#40318=CARTESIAN_POINT('Ctrl Pts',(1.95567757885048,-6.48039085641162,-29.7093751410404));
#40319=CARTESIAN_POINT('Ctrl Pts',(2.11421086436455,-6.42825026122995,-29.7015475263071));
#40320=CARTESIAN_POINT('Ctrl Pts',(2.27872981949548,-6.37414101715936,-29.6934243678618));
#40321=CARTESIAN_POINT('Ctrl Pts',(2.44122283603883,-6.3136944983611,-29.6853012094166));
#40322=CARTESIAN_POINT('Ctrl Pts',(2.6011690606084,-6.24709600679657,-29.6771780509713));
#40323=CARTESIAN_POINT('Ctrl Pts',(2.76110400813265,-6.18050221077398,-29.6690554652512));
#40324=CARTESIAN_POINT('Ctrl Pts',(2.91849218345026,-6.10775744666156,-29.660932879531));
#40325=CARTESIAN_POINT('Ctrl Pts',(3.07283243885395,-6.02909527232129,-29.6528102938109));
#40326=CARTESIAN_POINT('Ctrl Pts',(3.22719123982684,-5.95042364591167,-29.6446867320786));
#40327=CARTESIAN_POINT('Ctrl Pts',(3.37850106605793,-5.86583336070378,-29.6365631703462));
#40328=CARTESIAN_POINT('Ctrl Pts',(3.52628515822614,-5.77560403619171,-29.6284396086139));
#40329=CARTESIAN_POINT('Ctrl Pts',(3.67417689356898,-5.68530899032364,-29.6203101298308));
#40330=CARTESIAN_POINT('Ctrl Pts',(3.8185374530025,-5.58936689258128,-29.6121806510477));
#40331=CARTESIAN_POINT('Ctrl Pts',(3.95891834508355,-5.48810117772632,-29.6040511722646));
#40332=CARTESIAN_POINT('Ctrl Pts',(4.09935646798361,-5.38679417862166,-29.5959183792361));
#40333=CARTESIAN_POINT('Ctrl Pts',(4.23581140132458,-5.28015946148076,-29.5877855862076));
#40334=CARTESIAN_POINT('Ctrl Pts',(4.36786778669794,-5.16856072789383,-29.579652793179));
#40335=CARTESIAN_POINT('Ctrl Pts',(4.50006776335609,-5.0568406476148,-29.5715111569719));
#40336=CARTESIAN_POINT('Ctrl Pts',(4.6278593694121,-4.94014601664691,-29.5633695207648));
#40337=CARTESIAN_POINT('Ctrl Pts',(4.75086361636828,-4.8188778671666,-29.5552278845577));
#40338=CARTESIAN_POINT('Ctrl Pts',(4.81353260944063,-4.75709339217701,-29.551079831497));
#40339=CARTESIAN_POINT('Ctrl Pts',(4.87495954492782,-4.6941222936225,-29.5469317784364));
#40340=CARTESIAN_POINT('Ctrl Pts',(4.93509836574921,-4.63002085528559,-29.5427837253757));
#40341=CARTESIAN_POINT('Ctrl Pts',(5.05747255871364,-4.49958328306187,-29.5343430103976));
#40342=CARTESIAN_POINT('Ctrl Pts',(5.17476269518204,-4.36419473843019,-29.5259022954195));
#40343=CARTESIAN_POINT('Ctrl Pts',(5.28656334043379,-4.22427947081884,-29.5174615804414));
#40344=CARTESIAN_POINT('Ctrl Pts',(5.39827948149022,-4.08446995775906,-29.5090272453534));
#40345=CARTESIAN_POINT('Ctrl Pts',(5.50451419515488,-3.94014080183503,-29.5005929102654));
#40346=CARTESIAN_POINT('Ctrl Pts',(5.60490091563784,-3.79175087866834,-29.4921585751774));
#40347=CARTESIAN_POINT('Ctrl Pts',(5.70522717463469,-3.64345032863024,-29.4837293199688));
#40348=CARTESIAN_POINT('Ctrl Pts',(5.79971227605554,-3.49109416277208,-29.4753000647601));
#40349=CARTESIAN_POINT('Ctrl Pts',(5.88803152156129,-3.33517222960084,-29.4668708095515));
#40350=CARTESIAN_POINT('Ctrl Pts',(5.97631112115577,-3.17932028872962,-29.4584453381785));
#40351=CARTESIAN_POINT('Ctrl Pts',(6.05843021950572,-3.01990606169661,-29.4500198668055));
#40352=CARTESIAN_POINT('Ctrl Pts',(6.13410863538623,-2.85744645606528,-29.4415943954324));
#40353=CARTESIAN_POINT('Ctrl Pts',(6.20976467853105,-2.69503487820748,-29.4331714148732));
#40354=CARTESIAN_POINT('Ctrl Pts',(6.27898369568356,-2.5295800190689,-29.424748434314));
#40355=CARTESIAN_POINT('Ctrl Pts',(6.34153230108522,-2.36162170431523,-29.4163254537548));
#40356=CARTESIAN_POINT('Ctrl Pts',(6.40408194216229,-2.1936606085196,-29.4079023337285));
#40357=CARTESIAN_POINT('Ctrl Pts',(6.45996082829072,-2.02319628435379,-29.3994792137021));
#40358=CARTESIAN_POINT('Ctrl Pts',(6.50898417274263,-1.8507874105326,-29.3910560936758));
#40359=CARTESIAN_POINT('Ctrl Pts',(6.55800921250346,-1.67837257452531,-29.382632682364));
#40360=CARTESIAN_POINT('Ctrl Pts',(6.60017814651254,-1.50401337552693,-29.3742092710521));
#40361=CARTESIAN_POINT('Ctrl Pts',(6.6353563755266,-1.32828263925963,-29.3657858597403));
#40362=CARTESIAN_POINT('Ctrl Pts',(6.67054072718416,-1.15252131769337,-29.3573609823642));
#40363=CARTESIAN_POINT('Ctrl Pts',(6.69873188263415,-0.97538830993719,-29.348936104988));
#40364=CARTESIAN_POINT('Ctrl Pts',(6.71984650463333,-0.797465957998982,
-29.3405112276119));
#40365=CARTESIAN_POINT('Ctrl Pts',(6.74096774720992,-0.619487817768444,
-29.3320837085805));
#40366=CARTESIAN_POINT('Ctrl Pts',(6.75500799321,-0.440720170939507,-29.3236561895491));
#40367=CARTESIAN_POINT('Ctrl Pts',(6.76193580646864,-0.261750165610784,
-29.3152286705177));
#40368=CARTESIAN_POINT('Ctrl Pts',(6.76886983232248,-0.0826196668977874,
-29.3067935940129));
#40369=CARTESIAN_POINT('Ctrl Pts',(6.76867866805481,0.0967132193563114,
-29.2983585175081));
#40370=CARTESIAN_POINT('Ctrl Pts',(6.76138301570507,0.275660506665534,-29.2899234410033));
#40371=CARTESIAN_POINT('Ctrl Pts',(6.75408383731852,0.454694280376415,-29.2814842877706));
#40372=CARTESIAN_POINT('Ctrl Pts',(6.7396733445118,0.633341750840649,-29.2730451345378));
#40373=CARTESIAN_POINT('Ctrl Pts',(6.71822415898553,0.811019820733883,-29.264605981305));
#40374=CARTESIAN_POINT('Ctrl Pts',(6.69675113740043,0.988895340778397,-29.2561574498069));
#40375=CARTESIAN_POINT('Ctrl Pts',(6.66822384176986,1.16579897766599,-29.2477089183088));
#40376=CARTESIAN_POINT('Ctrl Pts',(6.63276628116368,1.34115638888911,-29.2392603868107));
#40377=CARTESIAN_POINT('Ctrl Pts',(6.61317482850513,1.43804704807635,-29.2345922990447));
#40378=CARTESIAN_POINT('Ctrl Pts',(6.59146851904817,1.5344658745573,-29.2299242112787));
#40379=CARTESIAN_POINT('Ctrl Pts',(6.56767481186212,1.630317933911,-29.2252561235126));
#40380=CARTESIAN_POINT('Ctrl Pts',(6.52567075980433,1.79952968639066,-29.2170153479159));
#40381=CARTESIAN_POINT('Ctrl Pts',(6.477065097266,1.96735071512019,-29.2087745723191));
#40382=CARTESIAN_POINT('Ctrl Pts',(6.42196376187807,2.13323004880508,-29.2005337967224));
#40383=CARTESIAN_POINT('Ctrl Pts',(6.36692345719267,2.29892565314476,-29.192302148678));
#40384=CARTESIAN_POINT('Ctrl Pts',(6.30540191671621,2.46268351007463,-29.1840705006336));
#40385=CARTESIAN_POINT('Ctrl Pts',(6.23755587019177,2.62396375093792,-29.1758388525892));
#40386=CARTESIAN_POINT('Ctrl Pts',(6.16977287971997,2.78509409809512,-29.1676148550309));
#40387=CARTESIAN_POINT('Ctrl Pts',(6.0956772265536,2.94375108905025,-29.1593908574725));
#40388=CARTESIAN_POINT('Ctrl Pts',(6.01547516936666,3.09941082896946,-29.1511668599142));
#40389=CARTESIAN_POINT('Ctrl Pts',(5.9353439710092,3.25493304290299,-29.1429501282897));
#40390=CARTESIAN_POINT('Ctrl Pts',(5.84911728383338,3.40746296864367,-29.1347333966652));
#40391=CARTESIAN_POINT('Ctrl Pts',(5.75704905105121,3.55649760632429,-29.1265166650407));
#40392=CARTESIAN_POINT('Ctrl Pts',(5.66502798823345,3.70545588804214,-29.118304143152));
#40393=CARTESIAN_POINT('Ctrl Pts',(5.56717152689508,3.85092214625655,-29.1100916212633));
#40394=CARTESIAN_POINT('Ctrl Pts',(5.46377923073043,3.99241850484625,-29.1018790993747));
#40395=CARTESIAN_POINT('Ctrl Pts',(5.36042150944697,4.13386754637301,-29.0936693237928));
#40396=CARTESIAN_POINT('Ctrl Pts',(5.25153185084407,4.27134904596709,-29.0854595482109));
#40397=CARTESIAN_POINT('Ctrl Pts',(5.13745282101675,4.40441454813543,-29.0772497726291));
#40398=CARTESIAN_POINT('Ctrl Pts',(5.08762606458192,4.46253410241685,-29.0736639559464));
#40399=CARTESIAN_POINT('Ctrl Pts',(5.03680986332872,4.51981160902196,-29.0700781392637));
#40400=CARTESIAN_POINT('Ctrl Pts',(4.98503519945453,4.57621164941039,-29.066492322581));
#40401=CARTESIAN_POINT('Ctrl Pts',(4.85719369768314,4.71547408635725,-29.0576382585371));
#40402=CARTESIAN_POINT('Ctrl Pts',(4.72363850840139,4.8492402212088,-29.0487841944932));
#40403=CARTESIAN_POINT('Ctrl Pts',(4.58486112874115,4.97708121594961,-29.0399301304493));
#40404=CARTESIAN_POINT('Ctrl Pts',(4.44569336719082,5.10528182844138,-29.0310511598517));
#40405=CARTESIAN_POINT('Ctrl Pts',(4.30127421369035,5.22752377461368,-29.0221721892541));
#40406=CARTESIAN_POINT('Ctrl Pts',(4.15212909194728,5.3434177268678,-29.0132932186565));
#40407=CARTESIAN_POINT('Ctrl Pts',(4.00276279421828,5.45948354501236,-29.0044010809164));
#40408=CARTESIAN_POINT('Ctrl Pts',(3.84865673546643,5.56918240899693,-28.9955089431762));
#40409=CARTESIAN_POINT('Ctrl Pts',(3.69036506749606,5.67216842738338,-28.9866168054361));
#40410=CARTESIAN_POINT('Ctrl Pts',(3.53175314594796,5.77536280569974,-28.9777066772423));
#40411=CARTESIAN_POINT('Ctrl Pts',(3.36893890085892,5.87181704189946,-28.9687965490484));
#40412=CARTESIAN_POINT('Ctrl Pts',(3.20250276976003,5.96123015909295,-28.9598864208546));
#40413=CARTESIAN_POINT('Ctrl Pts',(3.16818255209653,5.97966772804983,-28.9580490942056));
#40414=CARTESIAN_POINT('Ctrl Pts',(3.13370839824824,5.99780606288608,-28.9562117675566));
#40415=CARTESIAN_POINT('Ctrl Pts',(3.09908550384723,6.01564277861011,-28.9543744409077));
#40416=CARTESIAN_POINT('Ctrl Pts',(3.09908550384721,6.01564277861012,-30.9542680870819));
#40417=CARTESIAN_POINT('Ctrl Pts',(2.94371447950243,6.09568544520211,-30.9460679664523));
#40418=CARTESIAN_POINT('Ctrl Pts',(2.78527441477496,6.16968742560315,-30.9378678458226));
#40419=CARTESIAN_POINT('Ctrl Pts',(2.6242794472051,6.23742305627708,-30.929667725193));
#40420=CARTESIAN_POINT('Ctrl Pts',(2.46322305524189,6.30518453011918,-30.9214644759722));
#40421=CARTESIAN_POINT('Ctrl Pts',(2.2996101490492,6.36667475273516,-30.9132612267514));
#40422=CARTESIAN_POINT('Ctrl Pts',(2.1339731655378,6.42171686768925,-30.9050579775305));
#40423=CARTESIAN_POINT('Ctrl Pts',(1.96814645873079,6.47682202877727,-30.8968453321746));
#40424=CARTESIAN_POINT('Ctrl Pts',(1.80029138397078,6.52546421516487,-30.8886326868187));
#40425=CARTESIAN_POINT('Ctrl Pts',(1.6309547958345,6.56751668851663,-30.8804200414627));
#40426=CARTESIAN_POINT('Ctrl Pts',(1.46151405033017,6.60959502795553,-30.8722023445847));
#40427=CARTESIAN_POINT('Ctrl Pts',(1.29059032549375,6.64507550236139,-30.8639846477066));
#40428=CARTESIAN_POINT('Ctrl Pts',(1.11873877346133,6.67388286957108,-30.8557669508285));
#40429=CARTESIAN_POINT('Ctrl Pts',(0.94662984775507,6.70273338016728,-30.8475369467073));
#40430=CARTESIAN_POINT('Ctrl Pts',(0.773590673694652,6.72489077018064,-30.8393069425861));
#40431=CARTESIAN_POINT('Ctrl Pts',(0.600180819029017,6.74033174142562,-30.8310769384649));
#40432=CARTESIAN_POINT('Ctrl Pts',(0.472474212952908,6.75170314840832,-30.8250160032525));
#40433=CARTESIAN_POINT('Ctrl Pts',(0.344566632330296,6.75943299989573,-30.8189550680401));
#40434=CARTESIAN_POINT('Ctrl Pts',(0.216680517030194,6.76353003641882,-30.8128941328278));
#40435=CARTESIAN_POINT('Ctrl Pts',(0.0463846469923235,6.76898573735741,
-30.8048232626414));
#40436=CARTESIAN_POINT('Ctrl Pts',(-0.124428369577882,6.76801541995605,
-30.7967523924549));
#40437=CARTESIAN_POINT('Ctrl Pts',(-0.295222157570116,6.76055714254969,
-30.7886815222685));
#40438=CARTESIAN_POINT('Ctrl Pts',(-0.465803405968926,6.75310814638984,
-30.7806206956527));
#40439=CARTESIAN_POINT('Ctrl Pts',(-0.636365105444776,6.73918727108163,
-30.7725598690369));
#40440=CARTESIAN_POINT('Ctrl Pts',(-0.806366110133777,6.71878431685582,
-30.7644990424211));
#40441=CARTESIAN_POINT('Ctrl Pts',(-0.976192840410988,6.69840227846432,
-30.7564464792612));
#40442=CARTESIAN_POINT('Ctrl Pts',(-1.14545965252415,6.67155142907742,-30.7483939161014));
#40443=CARTESIAN_POINT('Ctrl Pts',(-1.31362585340333,6.63827357957401,-30.7403413529415));
#40444=CARTESIAN_POINT('Ctrl Pts',(-1.48165648296141,6.60502255782789,-30.7322952815536));
#40445=CARTESIAN_POINT('Ctrl Pts',(-1.64858790323685,6.56535492057922,-30.7242492101657));
#40446=CARTESIAN_POINT('Ctrl Pts',(-1.81388510042842,6.51936422072304,-30.7162031387778));
#40447=CARTESIAN_POINT('Ctrl Pts',(-1.97908519609627,6.47340053745946,-30.7081617939419));
#40448=CARTESIAN_POINT('Ctrl Pts',(-2.14265262133072,6.42112128564826,-30.7001204491059));
#40449=CARTESIAN_POINT('Ctrl Pts',(-2.30406321494482,6.36267095656676,-30.69207910427));
#40450=CARTESIAN_POINT('Ctrl Pts',(-2.46858530814144,6.30309388499294,-30.683882747049));
#40451=CARTESIAN_POINT('Ctrl Pts',(-2.63086617898871,6.23710546880609,-30.6756863898279));
#40452=CARTESIAN_POINT('Ctrl Pts',(-2.79036721872086,6.1649119851534,-30.6674900326068));
#40453=CARTESIAN_POINT('Ctrl Pts',(-2.94680197657918,6.09410636436796,-30.6594512438983));
#40454=CARTESIAN_POINT('Ctrl Pts',(-3.1005624706329,6.01733226656811,-30.6514124551898));
#40455=CARTESIAN_POINT('Ctrl Pts',(-3.25116144052422,5.93483262507448,-30.6433736664813));
#40456=CARTESIAN_POINT('Ctrl Pts',(-3.40177652586958,5.85232415537186,-30.6353340175495));
#40457=CARTESIAN_POINT('Ctrl Pts',(-3.54922908580803,5.76408910138276,-30.6272943686178));
#40458=CARTESIAN_POINT('Ctrl Pts',(-3.69305743016558,5.67041584167324,-30.6192547196861));
#40459=CARTESIAN_POINT('Ctrl Pts',(-3.83692964402033,5.57671401041321,-30.6112126185579));
#40460=CARTESIAN_POINT('Ctrl Pts',(-3.97717512916192,5.47757087545426,-30.6031705174297));
#40461=CARTESIAN_POINT('Ctrl Pts',(-4.11336221975358,5.37331743423967,-30.5951284163015));
#40462=CARTESIAN_POINT('Ctrl Pts',(-4.25414508958853,5.26554584898444,-30.5868149258568));
#40463=CARTESIAN_POINT('Ctrl Pts',(-4.39059051552245,5.15231328263402,-30.578501435412));
#40464=CARTESIAN_POINT('Ctrl Pts',(-4.52226071961451,5.03402890176762,-30.5701879449673));
#40465=CARTESIAN_POINT('Ctrl Pts',(-4.64985700198412,4.91940428061649,-30.5621316767965));
#40466=CARTESIAN_POINT('Ctrl Pts',(-4.77296894296149,4.80003610830509,-30.5540754086258));
#40467=CARTESIAN_POINT('Ctrl Pts',(-4.89123772725468,4.67633216265488,-30.546019140455));
#40468=CARTESIAN_POINT('Ctrl Pts',(-5.01517067856516,4.54670374747496,-30.5375770388733));
#40469=CARTESIAN_POINT('Ctrl Pts',(-5.13378484358296,4.4123144104076,-30.5291349372916));
#40470=CARTESIAN_POINT('Ctrl Pts',(-5.24671726850061,4.27366902139339,-30.5206928357099));
#40471=CARTESIAN_POINT('Ctrl Pts',(-5.35964969341829,4.13502363237914,-30.5122507341281));
#40472=CARTESIAN_POINT('Ctrl Pts',(-5.46690017074366,3.99212261192921,-30.5038086325464));
#40473=CARTESIAN_POINT('Ctrl Pts',(-5.56816028146203,3.84550127811039,-30.4953665309647));
#40474=CARTESIAN_POINT('Ctrl Pts',(-5.67116896999752,3.69634806070966,-30.4867786496534));
#40475=CARTESIAN_POINT('Ctrl Pts',(-5.7682881196305,3.54289853264869,-30.4781907683421));
#40476=CARTESIAN_POINT('Ctrl Pts',(-5.85915963143274,3.38563692876083,-30.4696028870308));
#40477=CARTESIAN_POINT('Ctrl Pts',(-5.94991018504773,3.2285846542673,-30.461026436965));
#40478=CARTESIAN_POINT('Ctrl Pts',(-6.03442952272235,3.06773069020775,-30.4524499868992));
#40479=CARTESIAN_POINT('Ctrl Pts',(-6.11240217391094,2.90358892826943,-30.4438735368333));
#40480=CARTESIAN_POINT('Ctrl Pts',(-6.19027876786987,2.73964937829496,-30.4353076523956));
#40481=CARTESIAN_POINT('Ctrl Pts',(-6.26162461990626,2.57243038834527,-30.4267417679578));
#40482=CARTESIAN_POINT('Ctrl Pts',(-6.32616936136809,2.40247168792633,-30.4181758835201));
#40483=CARTESIAN_POINT('Ctrl Pts',(-6.39064096204112,2.23270558125139,-30.4096197057684));
#40484=CARTESIAN_POINT('Ctrl Pts',(-6.44832670671636,2.06020624724369,-30.4010635280168));
#40485=CARTESIAN_POINT('Ctrl Pts',(-6.49900345467092,1.88553522803883,-30.3925073502651));
#40486=CARTESIAN_POINT('Ctrl Pts',(-6.54961033477658,1.71110502713566,-30.3839629688848));
#40487=CARTESIAN_POINT('Ctrl Pts',(-6.59322741040896,1.53450941620116,-30.3754185875044));
#40488=CARTESIAN_POINT('Ctrl Pts',(-6.62968070160935,1.35632694978333,-30.3668742061241));
#40489=CARTESIAN_POINT('Ctrl Pts',(-6.66610360228398,1.1782930312375,-30.3583369480578));
#40490=CARTESIAN_POINT('Ctrl Pts',(-6.69537456119865,0.998675201964652,
-30.3497996899915));
#40491=CARTESIAN_POINT('Ctrl Pts',(-6.71736986548872,0.818065455953325,
-30.3412624319252));
#40492=CARTESIAN_POINT('Ctrl Pts',(-6.73934393126139,0.637630105493947,
-30.3327334173777));
#40493=CARTESIAN_POINT('Ctrl Pts',(-6.75405631961916,0.45620506097962,-30.3242044028302));
#40494=CARTESIAN_POINT('Ctrl Pts',(-6.76143465766259,0.274390907573759,
-30.3156753882827));
#40495=CARTESIAN_POINT('Ctrl Pts',(-6.76514160429665,0.183045761820821,
-30.3113903309184));
#40496=CARTESIAN_POINT('Ctrl Pts',(-6.76699813350448,0.0916025323879388,
-30.3071052735542));
#40497=CARTESIAN_POINT('Ctrl Pts',(-6.76699999859311,0.000137988494950558,
-30.30282021619));
#40498=CARTESIAN_POINT('',(-6.767,3.39320585518443E-13,-30.6971797838101));
#40499=CARTESIAN_POINT('Ctrl Pts',(3.0990855038472,6.01564277861013,-31.3484270467647));
#40500=CARTESIAN_POINT('Ctrl Pts',(2.92903432523677,6.10324823690256,-31.3394159215786));
#40501=CARTESIAN_POINT('Ctrl Pts',(2.75517565391701,6.18368609644757,-31.3304047963925));
#40502=CARTESIAN_POINT('Ctrl Pts',(2.57810514217839,6.2566494928095,-31.3213936712064));
#40503=CARTESIAN_POINT('Ctrl Pts',(2.40127488857691,6.32951388878159,-31.3123947727662));
#40504=CARTESIAN_POINT('Ctrl Pts',(2.22124171000805,6.39492396748568,-31.303395874326));
#40505=CARTESIAN_POINT('Ctrl Pts',(2.03862336042999,6.4526199170809,-31.2943969758858));
#40506=CARTESIAN_POINT('Ctrl Pts',(1.85638271667096,6.51019653531677,-31.2854166896842));
#40507=CARTESIAN_POINT('Ctrl Pts',(1.67156779962697,6.56009079414926,-31.2764364034827));
#40508=CARTESIAN_POINT('Ctrl Pts',(1.48481382549683,6.60209185816234,-31.2674561172811));
#40509=CARTESIAN_POINT('Ctrl Pts',(1.45913711007258,6.60786656455455,-31.2662214219859));
#40510=CARTESIAN_POINT('Ctrl Pts',(1.43342376993098,6.61349213775955,-31.2649867266906));
#40511=CARTESIAN_POINT('Ctrl Pts',(1.40767548398599,6.61896810173495,-31.2637520313954));
#40512=CARTESIAN_POINT('Ctrl Pts',(1.23827546502397,6.65499490380053,-31.2556288729501));
#40513=CARTESIAN_POINT('Ctrl Pts',(1.06743726754016,6.68452577478008,-31.2475057145048));
#40514=CARTESIAN_POINT('Ctrl Pts',(0.895704241073713,6.70745875220434,-31.2393825560595));
#40515=CARTESIAN_POINT('Ctrl Pts',(0.723983322684397,6.73039011273366,-31.2312599703394));
#40516=CARTESIAN_POINT('Ctrl Pts',(0.55136806378577,6.7467244578645,-31.2231373846193));
#40517=CARTESIAN_POINT('Ctrl Pts',(0.378409067366565,6.75641144230684,-31.2150147988991));
#40518=CARTESIAN_POINT('Ctrl Pts',(0.205429288144462,6.76609959074002,-31.2068912371668));
#40519=CARTESIAN_POINT('Ctrl Pts',(0.0321060546674524,6.76913876871745,
-31.1987676754344));
#40520=CARTESIAN_POINT('Ctrl Pts',(-0.14100792743591,6.76553070825935,-31.1906441137021));
#40521=CARTESIAN_POINT('Ctrl Pts',(-0.314248002533276,6.76192001975734,
-31.182514634919));
#40522=CARTESIAN_POINT('Ctrl Pts',(-0.487278155527502,6.75165243025827,
-31.1743851561358));
#40523=CARTESIAN_POINT('Ctrl Pts',(-0.65954806106113,6.73478176002389,-31.1662556773527));
#40524=CARTESIAN_POINT('Ctrl Pts',(-0.831888198002263,6.71790421191428,
-31.1581228843242));
#40525=CARTESIAN_POINT('Ctrl Pts',(-1.00346710729642,6.69441826679735,-31.1499900912957));
#40526=CARTESIAN_POINT('Ctrl Pts',(-1.17374283375576,6.66442921488457,-31.1418572982672));
#40527=CARTESIAN_POINT('Ctrl Pts',(-1.34420370923653,6.63440755442723,-31.1337156620601));
#40528=CARTESIAN_POINT('Ctrl Pts',(-1.51335821432473,6.59786874103933,-31.1255740258529));
#40529=CARTESIAN_POINT('Ctrl Pts',(-1.68067703873291,6.55496862627702,-31.1174323896457));
#40530=CARTESIAN_POINT('Ctrl Pts',(-1.76592370709553,6.5331116005132,-31.1132843365851));
#40531=CARTESIAN_POINT('Ctrl Pts',(-1.85069413992202,6.50960412564579,-31.1091362835246));
#40532=CARTESIAN_POINT('Ctrl Pts',(-1.93492021399903,6.48447166432686,-31.104988230464));
#40533=CARTESIAN_POINT('Ctrl Pts',(-2.10630863999641,6.43333057726927,-31.0965475154859));
#40534=CARTESIAN_POINT('Ctrl Pts',(-2.2757949243887,6.37535270620505,-31.0881068005078));
#40535=CARTESIAN_POINT('Ctrl Pts',(-2.44281521991742,6.31070065851169,-31.0796660855297));
#40536=CARTESIAN_POINT('Ctrl Pts',(-2.60970927363744,6.24609747788211,-31.0712317504417));
#40537=CARTESIAN_POINT('Ctrl Pts',(-2.7741407442683,6.17483029677232,-31.0627974153536));
#40538=CARTESIAN_POINT('Ctrl Pts',(-2.93556194988327,6.09711120436535,-31.0543630802656));
#40539=CARTESIAN_POINT('Ctrl Pts',(-3.09688593381462,6.01943892105627,-31.045933825057));
#40540=CARTESIAN_POINT('Ctrl Pts',(-3.2552029676386,5.93532261784037,-31.0375045698484));
#40541=CARTESIAN_POINT('Ctrl Pts',(-3.40998596434023,5.84502221749436,-31.0290753146398));
#40542=CARTESIAN_POINT('Ctrl Pts',(-3.56469948000213,5.75476235238695,-31.0206498432668));
#40543=CARTESIAN_POINT('Ctrl Pts',(-3.71588183415688,5.65832409293377,-31.0122243718938));
#40544=CARTESIAN_POINT('Ctrl Pts',(-3.86303079390488,5.55601314661356,-31.0037989005208));
#40545=CARTESIAN_POINT('Ctrl Pts',(-4.01013625214949,5.45373244637857,-30.9953759199617));
#40546=CARTESIAN_POINT('Ctrl Pts',(-4.15321042042536,5.34558271166036,-30.9869529394025));
#40547=CARTESIAN_POINT('Ctrl Pts',(-4.29177997256654,5.23191300262885,-30.9785299588434));
#40548=CARTESIAN_POINT('Ctrl Pts',(-4.43035181913392,5.11824141146121,-30.9701068388171));
#40549=CARTESIAN_POINT('Ctrl Pts',(-4.56441863863559,4.99904986966019,-30.9616837187908));
#40550=CARTESIAN_POINT('Ctrl Pts',(-4.69353961576692,4.87472818475312,-30.9532605987645));
#40551=CARTESIAN_POINT('Ctrl Pts',(-4.82266505811647,4.75040220059536,-30.9448371874526));
#40552=CARTESIAN_POINT('Ctrl Pts',(-4.94684407670967,4.62094595079707,-30.9364137761408));
#40553=CARTESIAN_POINT('Ctrl Pts',(-5.06567210788635,4.48678672274294,-30.927990364829));
#40554=CARTESIAN_POINT('Ctrl Pts',(-5.18452082065161,4.3526041447609,-30.9195654874529));
#40555=CARTESIAN_POINT('Ctrl Pts',(-5.29801646810998,4.21371720624633,-30.9111406100769));
#40556=CARTESIAN_POINT('Ctrl Pts',(-5.40579399699795,4.07058721341541,-30.9027157327008));
#40557=CARTESIAN_POINT('Ctrl Pts',(-5.51360531997894,3.92741234157914,-30.8942882136694));
#40558=CARTESIAN_POINT('Ctrl Pts',(-5.61569474922438,3.77999202921619,-30.8858606946379));
#40559=CARTESIAN_POINT('Ctrl Pts',(-5.71173966431975,3.62881785255703,-30.8774331756064));
#40560=CARTESIAN_POINT('Ctrl Pts',(-5.80787070878275,3.47750810873923,-30.8689980991017));
#40561=CARTESIAN_POINT('Ctrl Pts',(-5.89794622918145,3.32243805598583,-30.8605630225969));
#40562=CARTESIAN_POINT('Ctrl Pts',(-5.98168823942467,3.16412623109898,-30.8521279460921));
#40563=CARTESIAN_POINT('Ctrl Pts',(-6.06547072273255,3.00573789306529,-30.8436887928593));
#40564=CARTESIAN_POINT('Ctrl Pts',(-6.14291344237129,2.84410495650474,-30.8352496396265));
#40565=CARTESIAN_POINT('Ctrl Pts',(-6.21378573983061,2.67976785925159,-30.8268104863938));
#40566=CARTESIAN_POINT('Ctrl Pts',(-6.28473679628267,2.51524813740863,-30.8183619548957));
#40567=CARTESIAN_POINT('Ctrl Pts',(-6.34910271641903,2.34801855968716,-30.8099134233976));
#40568=CARTESIAN_POINT('Ctrl Pts',(-6.40670165452679,2.17863785652497,-30.8014648918995));
#40569=CARTESIAN_POINT('Ctrl Pts',(-6.43852693663505,2.08504952245279,-30.7967968041333));
#40570=CARTESIAN_POINT('Ctrl Pts',(-6.46828719849882,1.99080473063557,-30.7921287163671));
#40571=CARTESIAN_POINT('Ctrl Pts',(-6.49595839816723,1.89599933789036,-30.7874606286009));
#40572=CARTESIAN_POINT('Ctrl Pts',(-6.54949111980473,1.71258876081452,-30.7784297428438));
#40573=CARTESIAN_POINT('Ctrl Pts',(-6.59530470013533,1.52672903902217,-30.7693988570867));
#40574=CARTESIAN_POINT('Ctrl Pts',(-6.63319070558781,1.33905566101768,-30.7603679713296));
#40575=CARTESIAN_POINT('Ctrl Pts',(-6.67098922671683,1.1518156482706,-30.7513579392075));
#40576=CARTESIAN_POINT('Ctrl Pts',(-6.70089663607218,0.962770559905612,
-30.7423479070855));
#40577=CARTESIAN_POINT('Ctrl Pts',(-6.72275420312697,0.772570336175757,
-30.7333378749634));
#40578=CARTESIAN_POINT('Ctrl Pts',(-6.74453441785932,0.58304321705057,-30.7243597286824));
#40579=CARTESIAN_POINT('Ctrl Pts',(-6.75832158011288,0.392369348153801,
-30.7153815824015));
#40580=CARTESIAN_POINT('Ctrl Pts',(-6.76400803109756,0.201207244520965,
-30.7064034361205));
#40581=CARTESIAN_POINT('Ctrl Pts',(-6.76595534646838,0.135744110533633,
-30.7033288853504));
#40582=CARTESIAN_POINT('Ctrl Pts',(-6.76695311776644,0.0702238391348725,
-30.7002543345802));
#40583=CARTESIAN_POINT('Ctrl Pts',(-6.76699838636073,0.00467322065976275,
-30.6971797838101));
#40584=CARTESIAN_POINT('Ctrl Pts',(-6.767,4.3548441435357E-13,-30.6971797838101));
#40585=CARTESIAN_POINT('Ctrl Pts',(-6.76700000000001,-0.186007249559608,
-30.6884302719974));
#40586=CARTESIAN_POINT('Ctrl Pts',(-6.75932637294249,-0.372014355815825,
-30.6796807601846));
#40587=CARTESIAN_POINT('Ctrl Pts',(-6.74400518263364,-0.557389537586234,
-30.6709312483719));
#40588=CARTESIAN_POINT('Ctrl Pts',(-6.7286840570373,-0.742763936382708,
-30.6621817735147));
#40589=CARTESIAN_POINT('Ctrl Pts',(-6.70571545643564,-0.92750613040502,
-30.6534322986575));
#40590=CARTESIAN_POINT('Ctrl Pts',(-6.67517739401573,-1.11098864009554,
-30.6446828238003));
#40591=CARTESIAN_POINT('Ctrl Pts',(-6.64463945804386,-1.29447039004561,
-30.6359333851718));
#40592=CARTESIAN_POINT('Ctrl Pts',(-6.60653217002717,-1.47669218339309,
-30.6271839465432));
#40593=CARTESIAN_POINT('Ctrl Pts',(-6.56098496085469,-1.65703510627825,
-30.6184345079147));
#40594=CARTESIAN_POINT('Ctrl Pts',(-6.51543793649544,-1.83737729740051,
-30.6096851047881));
#40595=CARTESIAN_POINT('Ctrl Pts',(-6.46245112156883,-2.01584035544994,
-30.6009357016615));
#40596=CARTESIAN_POINT('Ctrl Pts',(-6.40220448361703,-2.19181813797451,
-30.5921862985348));
#40597=CARTESIAN_POINT('Ctrl Pts',(-6.34195808511956,-2.36779522106348,
-30.5834369301833));
#40598=CARTESIAN_POINT('Ctrl Pts',(-6.27445201416335,-2.54128677725791,
-30.5746875618318));
#40599=CARTESIAN_POINT('Ctrl Pts',(-6.19991555052702,-2.71170355428708,
-30.5659381934802));
#40600=CARTESIAN_POINT('Ctrl Pts',(-6.12537937695088,-2.88211966813585,
-30.557188859177));
#40601=CARTESIAN_POINT('Ctrl Pts',(-6.04381298028307,-3.04946076419956,
-30.5484395248739));
#40602=CARTESIAN_POINT('Ctrl Pts',(-5.95549339308823,-3.21315848424607,
-30.5396901905707));
#40603=CARTESIAN_POINT('Ctrl Pts',(-5.86717414225637,-3.37685558085382,
-30.5309408895891));
#40604=CARTESIAN_POINT('Ctrl Pts',(-5.7721018884388,-3.53690907700304,-30.5221915886076));
#40605=CARTESIAN_POINT('Ctrl Pts',(-5.67059953311171,-3.69277537024299,
-30.513442287626));
#40606=CARTESIAN_POINT('Ctrl Pts',(-5.56909755592487,-3.84864108281347,
-30.5046930192394));
#40607=CARTESIAN_POINT('Ctrl Pts',(-5.46116568154724,-4.0003193835516,-30.4959437508527));
#40608=CARTESIAN_POINT('Ctrl Pts',(-5.34717048488112,-4.14729511918506,
-30.4871944824661));
#40609=CARTESIAN_POINT('Ctrl Pts',(-5.23317570343023,-4.29427031947523,
-30.4784452459478));
#40610=CARTESIAN_POINT('Ctrl Pts',(-5.11311781951248,-4.43654276249901,
-30.4696960094294));
#40611=CARTESIAN_POINT('Ctrl Pts',(-4.98740458928927,-4.57362924412729,
-30.460946772911));
#40612=CARTESIAN_POINT('Ctrl Pts',(-4.86169180652415,-4.71071523781603,
-30.4521975675343));
#40613=CARTESIAN_POINT('Ctrl Pts',(-4.7303239114124,-4.84261509584814,-30.4434483621576));
#40614=CARTESIAN_POINT('Ctrl Pts',(-4.59374706946988,-4.96888084599912,
-30.4346991567809));
#40615=CARTESIAN_POINT('Ctrl Pts',(-4.45717070231215,-5.09514615720996,
-30.4259499818192));
#40616=CARTESIAN_POINT('Ctrl Pts',(-4.3153856349712,-5.21577720520781,-30.4172008068575));
#40617=CARTESIAN_POINT('Ctrl Pts',(-4.16887340951853,-5.33036429293622,
-30.4084516318959));
#40618=CARTESIAN_POINT('Ctrl Pts',(-4.02236168122339,-5.44495099183813,
-30.3997024866226));
#40619=CARTESIAN_POINT('Ctrl Pts',(-3.87112305263044,-5.55349359498023,
-30.3909533413494));
#40620=CARTESIAN_POINT('Ctrl Pts',(-3.71567116928868,-5.65562346357295,
-30.3822041960761));
#40621=CARTESIAN_POINT('Ctrl Pts',(-3.56021980053185,-5.75775299409006,
-30.3734550797648));
#40622=CARTESIAN_POINT('Ctrl Pts',(-3.40055544441958,-5.85346967519952,
-30.3647059634534));
#40623=CARTESIAN_POINT('Ctrl Pts',(-3.23722035886718,-5.94244843041451,
-30.355956847142));
#40624=CARTESIAN_POINT('Ctrl Pts',(-3.07388580043369,-6.03142689847512,
-30.347207759066));
#40625=CARTESIAN_POINT('Ctrl Pts',(-2.90688078789107,-6.11366734707957,
-30.33845867099));
#40626=CARTESIAN_POINT('Ctrl Pts',(-2.73677250610282,-6.18889047001478,
-30.329709582914));
#40627=CARTESIAN_POINT('Ctrl Pts',(-2.56666475916808,-6.26411335643386,
-30.3209605223468));
#40628=CARTESIAN_POINT('Ctrl Pts',(-2.39345402456951,-6.3323188454531,-30.3122114617796));
#40629=CARTESIAN_POINT('Ctrl Pts',(-2.21772855943907,-6.39327529804938,
-30.3034624012125));
#40630=CARTESIAN_POINT('Ctrl Pts',(-2.04200363223441,-6.4542315640475,-30.2947133674277));
#40631=CARTESIAN_POINT('Ctrl Pts',(-1.86376426060892,-6.50793874412493,
-30.2859643336429));
#40632=CARTESIAN_POINT('Ctrl Pts',(-1.68361577621555,-6.55421443943346,
-30.2772152998581));
#40633=CARTESIAN_POINT('Ctrl Pts',(-1.50346782833073,-6.6004899969262,-30.2684662921292));
#40634=CARTESIAN_POINT('Ctrl Pts',(-1.32141105657236,-6.63933404265192,
-30.2597172844003));
#40635=CARTESIAN_POINT('Ctrl Pts',(-1.13806375346375,-6.67061465631556,
-30.2509682766714));
#40636=CARTESIAN_POINT('Ctrl Pts',(-0.954716981167896,-6.70189517941802,
-30.2422192942719));
#40637=CARTESIAN_POINT('Ctrl Pts',(-0.770079967439657,-6.72561226609035,
-30.2334703118725));
#40638=CARTESIAN_POINT('Ctrl Pts',(-0.584779764069928,-6.74168536996012,
-30.224721329473));
#40639=CARTESIAN_POINT('Ctrl Pts',(-0.391489587589783,-6.75845153117891,
-30.2155950990574));
#40640=CARTESIAN_POINT('Ctrl Pts',(-0.197478091802034,-6.76689985146403,
-30.2064688686418));
#40641=CARTESIAN_POINT('Ctrl Pts',(-0.00346214752780608,-6.76699911434415,
-30.1973426382262));
#40642=CARTESIAN_POINT('Ctrl Pts',(0.18449079848784,-6.76709527525926,-30.188501602511));
#40643=CARTESIAN_POINT('Ctrl Pts',(0.372447602157948,-6.75935633790746,
-30.1796605667959));
#40644=CARTESIAN_POINT('Ctrl Pts',(0.559756448197352,-6.74380914014487,
-30.1708195310808));
#40645=CARTESIAN_POINT('Ctrl Pts',(0.745136131046472,-6.7284220687312,-30.1620695524675));
#40646=CARTESIAN_POINT('Ctrl Pts',(0.929880851948136,-6.7053868635568,-30.1533195738542));
#40647=CARTESIAN_POINT('Ctrl Pts',(1.11336305057769,-6.67478177303261,-30.1445695952409));
#40648=CARTESIAN_POINT('Ctrl Pts',(1.29684337090427,-6.64417699581201,-30.1358197062009));
#40649=CARTESIAN_POINT('Ctrl Pts',(1.47906091205491,-6.60600253547992,-30.1270698171609));
#40650=CARTESIAN_POINT('Ctrl Pts',(1.65939671095518,-6.56038806441137,-30.1183199281209));
#40651=CARTESIAN_POINT('Ctrl Pts',(1.83973072369456,-6.51477404513766,-30.1095701257454));
#40652=CARTESIAN_POINT('Ctrl Pts',(2.0181827535733,-6.46172023288569,-30.1008203233699));
#40653=CARTESIAN_POINT('Ctrl Pts',(2.19414664033618,-6.40140683918008,-30.0920705209944));
#40654=CARTESIAN_POINT('Ctrl Pts',(2.37010884271549,-6.34109402281389,-30.0833208023749));
#40655=CARTESIAN_POINT('Ctrl Pts',(2.54358267848093,-6.27352185699675,-30.0745710837554));
#40656=CARTESIAN_POINT('Ctrl Pts',(2.71397890842027,-6.19891986435137,-30.0658213651358));
#40657=CARTESIAN_POINT('Ctrl Pts',(2.8843735638923,-6.12431856103108,-30.057071727364));
#40658=CARTESIAN_POINT('Ctrl Pts',(3.05169040787463,-6.0426876758241,-30.0483220895922));
#40659=CARTESIAN_POINT('Ctrl Pts',(3.21536112512347,-5.95430447953787,-30.0395724518204));
#40660=CARTESIAN_POINT('Ctrl Pts',(3.37903038443129,-5.86592207054877,-30.0308228919883));
#40661=CARTESIAN_POINT('Ctrl Pts',(3.53905332980253,-5.77078760703205,-30.0220733321562));
#40662=CARTESIAN_POINT('Ctrl Pts',(3.69488643042165,-5.66922422085121,-30.0133237723242));
#40663=CARTESIAN_POINT('Ctrl Pts',(3.85071819469009,-5.56766170562974,-30.0045742875242));
#40664=CARTESIAN_POINT('Ctrl Pts',(4.00235994599484,-5.45967053456061,-29.9958248027242));
#40665=CARTESIAN_POINT('Ctrl Pts',(4.14929662974553,-5.34561750206488,-29.9870753179242));
#40666=CARTESIAN_POINT('Ctrl Pts',(4.29623210225295,-5.2315654097426,-29.9783259052488));
#40667=CARTESIAN_POINT('Ctrl Pts',(4.43846235842365,-5.11145173171971,-29.9695764925735));
#40668=CARTESIAN_POINT('Ctrl Pts',(4.57550431797673,-4.98568443006337,-29.9608270798981));
#40669=CARTESIAN_POINT('Ctrl Pts',(4.71254519337739,-4.85991812336452,-29.9520777364402));
#40670=CARTESIAN_POINT('Ctrl Pts',(4.84439764315228,-4.72849847630851,-29.9433283929823));
#40671=CARTESIAN_POINT('Ctrl Pts',(4.97061384196929,-4.59187184425081,-29.9345790495244));
#40672=CARTESIAN_POINT('Ctrl Pts',(5.09682908420441,-4.45524624767478,-29.925829772377));
#40673=CARTESIAN_POINT('Ctrl Pts',(5.21740796650398,-4.31341395556618,-29.9170804952297));
#40674=CARTESIAN_POINT('Ctrl Pts',(5.3319409594247,-4.16685668162576,-29.9083312180823));
#40675=CARTESIAN_POINT('Ctrl Pts',(5.44647312235341,-4.02030046974932,-29.8995820043388));
#40676=CARTESIAN_POINT('Ctrl Pts',(5.55495930712486,-3.86901957035262,-29.8908327905952));
#40677=CARTESIAN_POINT('Ctrl Pts',(5.65703106079983,-3.71352778058088,-29.8820835768517));
#40678=CARTESIAN_POINT('Ctrl Pts',(5.75910210868914,-3.55803706597315,-29.8733344236055));
#40679=CARTESIAN_POINT('Ctrl Pts',(5.85475865698717,-3.3983357588061,-29.8645852703593));
#40680=CARTESIAN_POINT('Ctrl Pts',(5.94367583069221,-3.2349662470643,-29.8558361171131));
#40681=CARTESIAN_POINT('Ctrl Pts',(6.03259241910233,-3.07159781069795,-29.847087021458));
#40682=CARTESIAN_POINT('Ctrl Pts',(6.11476958471119,-2.90456146975516,-29.8383379258029));
#40683=CARTESIAN_POINT('Ctrl Pts',(6.18992823574533,-2.73442451647925,-29.8295888301477));
#40684=CARTESIAN_POINT('Ctrl Pts',(6.26508641701078,-2.56428862662068,-29.8208397891776));
#40685=CARTESIAN_POINT('Ctrl Pts',(6.33322605570435,-2.39105242530913,-29.8120907482075));
#40686=CARTESIAN_POINT('Ctrl Pts',(6.39411573747899,-2.21530425353348,-29.8033417072374));
#40687=CARTESIAN_POINT('Ctrl Pts',(6.45500505889245,-2.03955712188183,-29.7945927180464));
#40688=CARTESIAN_POINT('Ctrl Pts',(6.50864441545036,-1.86129832025197,-29.7858437288554));
#40689=CARTESIAN_POINT('Ctrl Pts',(6.55485164050002,-1.68113324011938,-29.7770947396644));
#40690=CARTESIAN_POINT('Ctrl Pts',(6.60199852639195,-1.49730435912525,-29.7681678327875));
#40691=CARTESIAN_POINT('Ctrl Pts',(6.64140767441084,-1.31149113173276,-29.7592409259106));
#40692=CARTESIAN_POINT('Ctrl Pts',(6.67293975269666,-1.12435050446054,-29.7503140190337));
#40693=CARTESIAN_POINT('Ctrl Pts',(6.7038466483156,-0.940920291559975,-29.7415641048497));
#40694=CARTESIAN_POINT('Ctrl Pts',(6.72718585889708,-0.756215114274175,
-29.7328141906657));
#40695=CARTESIAN_POINT('Ctrl Pts',(6.74287810451896,-0.570862389371384,
-29.7240642764818));
#40696=CARTESIAN_POINT('Ctrl Pts',(6.75857004154145,-0.385513309564392,
-29.7153145343712));
#40697=CARTESIAN_POINT('Ctrl Pts',(6.76661529035567,-0.199516993255554,
-29.7065647922606));
#40698=CARTESIAN_POINT('Ctrl Pts',(6.76698652348897,-0.0135052182014546,
-29.69781505015));
#40699=CARTESIAN_POINT('Ctrl Pts',(6.76735774981515,0.17250314604148,-29.6890654684794));
#40700=CARTESIAN_POINT('Ctrl Pts',(6.76005524147466,0.358526681836041,-29.6803158868087));
#40701=CARTESIAN_POINT('Ctrl Pts',(6.74510380214861,0.543933542117414,-29.6715663051381));
#40702=CARTESIAN_POINT('Ctrl Pts',(6.73015261710951,0.72933724908729,-29.6628168722762));
#40703=CARTESIAN_POINT('Ctrl Pts',(6.7075527844457,0.914124015857248,-29.6540674394142));
#40704=CARTESIAN_POINT('Ctrl Pts',(6.67738106408246,1.09766621749645,-29.6453180065523));
#40705=CARTESIAN_POINT('Ctrl Pts',(6.64720981677204,1.28120554143583,-29.6365687108699));
#40706=CARTESIAN_POINT('Ctrl Pts',(6.60946696581465,1.46350005650882,-29.6278194151876));
#40707=CARTESIAN_POINT('Ctrl Pts',(6.56428070010928,1.64393062206797,-29.6190701195053));
#40708=CARTESIAN_POINT('Ctrl Pts',(6.51909508282669,1.82435859844906,-29.6103209493753));
#40709=CARTESIAN_POINT('Ctrl Pts',(6.46646633415585,2.00292240086808,-29.6015717792453));
#40710=CARTESIAN_POINT('Ctrl Pts',(6.40657319597112,2.1790155769669,-29.5928226091153));
#40711=CARTESIAN_POINT('Ctrl Pts',(6.34668083768208,2.35510646007669,-29.5840735529122));
#40712=CARTESIAN_POINT('Ctrl Pts',(6.27952437143792,2.52872650996763,-29.5753244967091));
#40713=CARTESIAN_POINT('Ctrl Pts',(6.20533187335035,2.69928607998156,-29.5665754405061));
#40714=CARTESIAN_POINT('Ctrl Pts',(6.1283144978415,2.87633970115614,-29.5574932642172));
#40715=CARTESIAN_POINT('Ctrl Pts',(6.0437148946305,3.05009490562553,-29.5484110879284));
#40716=CARTESIAN_POINT('Ctrl Pts',(5.95184265120387,3.21991584599822,-29.5393289116395));
#40717=CARTESIAN_POINT('Ctrl Pts',(5.86333281335381,3.38352155905493,-29.5305791312851));
#40718=CARTESIAN_POINT('Ctrl Pts',(5.76807337235566,3.54347560904018,-29.5218293509307));
#40719=CARTESIAN_POINT('Ctrl Pts',(5.66638790086228,3.69923467178841,-29.5130795705763));
#40720=CARTESIAN_POINT('Ctrl Pts',(5.5647060850261,3.85498813489955,-29.504330104782));
#40721=CARTESIAN_POINT('Ctrl Pts',(5.45659885766815,4.00654667256449,-29.4955806389878));
#40722=CARTESIAN_POINT('Ctrl Pts',(5.34243340580365,4.15339551506394,-29.4868311731935));
#40723=CARTESIAN_POINT('Ctrl Pts',(5.22827145140433,4.30023985884067,-29.4780819754396));
#40724=CARTESIAN_POINT('Ctrl Pts',(5.1080518197791,4.4423745699325,-29.4693327776857));
#40725=CARTESIAN_POINT('Ctrl Pts',(4.98218281282352,4.57931691626666,-29.4605835799319));
#40726=CARTESIAN_POINT('Ctrl Pts',(4.85631699296011,4.71625579512387,-29.4518346037138));
#40727=CARTESIAN_POINT('Ctrl Pts',(4.724802277916,4.84800236136002,-29.4430856274958));
#40728=CARTESIAN_POINT('Ctrl Pts',(4.58808530847855,4.97410918679147,-29.4343366512778));
#40729=CARTESIAN_POINT('Ctrl Pts',(4.45135945056701,5.10022421089244,-29.4255871062566));
#40730=CARTESIAN_POINT('Ctrl Pts',(4.3094308720776,5.22069856612218,-29.4168375612354));
#40731=CARTESIAN_POINT('Ctrl Pts',(4.16278164322177,5.3351230530191,-29.4080880162142));
#40732=CARTESIAN_POINT('Ctrl Pts',(4.01614103534092,5.44954081331647,-29.399338985547));
#40733=CARTESIAN_POINT('Ctrl Pts',(3.86478055833106,5.55790924068551,-29.3905899548797));
#40734=CARTESIAN_POINT('Ctrl Pts',(3.70921425811636,5.65986029751498,-29.3818409242124));
#40735=CARTESIAN_POINT('Ctrl Pts',(3.55364584529798,5.76181273884852,-29.3730917747326));
#40736=CARTESIAN_POINT('Ctrl Pts',(3.39387173464017,5.85734747818253,-29.3643426252527));
#40737=CARTESIAN_POINT('Ctrl Pts',(3.23043456092071,5.94614005448989,-29.3555934757729));
#40738=CARTESIAN_POINT('Ctrl Pts',(3.18690768806169,5.969787448114,-29.3532633870399));
#40739=CARTESIAN_POINT('Ctrl Pts',(3.14312114982771,5.99295688499357,-29.3509332983069));
#40740=CARTESIAN_POINT('Ctrl Pts',(3.09908550384723,6.01564277861011,-29.348603209574));
#40741=CARTESIAN_POINT('Origin',(0.,0.,-63.6971797838103));
#40742=CARTESIAN_POINT('',(3.09908550384719,6.01564277861013,-26.9540130953596));
#40743=CARTESIAN_POINT('',(3.09908550384723,6.01564277861011,-27.3486843298454));
#40744=CARTESIAN_POINT('',(3.09908550384721,6.01564277861012,-63.6971797838103));
#40745=CARTESIAN_POINT('',(-6.76699602342832,-0.00733613694335467,-28.3028202162144));
#40746=CARTESIAN_POINT('Ctrl Pts',(-6.76699602342776,-0.00733613746203318,
-28.3028202161899));
#40747=CARTESIAN_POINT('Ctrl Pts',(-6.76676555142464,-0.219928000235072,
-28.2927712501011));
#40748=CARTESIAN_POINT('Ctrl Pts',(-6.75651764005179,-0.432142597509886,
-28.2827222840123));
#40749=CARTESIAN_POINT('Ctrl Pts',(-6.73635434321315,-0.643287775939668,
-28.2726733179236));
#40750=CARTESIAN_POINT('Ctrl Pts',(-6.71963244938501,-0.818395412566786,
-28.2643394752309));
#40751=CARTESIAN_POINT('Ctrl Pts',(-6.6960571440256,-0.993074637253249,
-28.2560056325382));
#40752=CARTESIAN_POINT('Ctrl Pts',(-6.66565593329613,-1.16675617800557,
-28.2476717898455));
#40753=CARTESIAN_POINT('Ctrl Pts',(-6.63529055423959,-1.34023301308947,
-28.2393477696408));
#40754=CARTESIAN_POINT('Ctrl Pts',(-6.59811535603069,-1.51271416701442,
-28.2310237494361));
#40755=CARTESIAN_POINT('Ctrl Pts',(-6.55420967939453,-1.68363430665067,
-28.2226997292313));
#40756=CARTESIAN_POINT('Ctrl Pts',(-6.51034770111078,-1.85438433323848,
-28.2143839937404));
#40757=CARTESIAN_POINT('Ctrl Pts',(-6.45976867644582,-2.02357610609857,
-28.2060682582496));
#40758=CARTESIAN_POINT('Ctrl Pts',(-6.40260322104912,-2.19065309755139,
-28.1977525227587));
#40759=CARTESIAN_POINT('Ctrl Pts',(-6.3454841869831,-2.35759441377488,-28.1894435400787));
#40760=CARTESIAN_POINT('Ctrl Pts',(-6.28178949175138,-2.52242404280815,
-28.1811345573986));
#40761=CARTESIAN_POINT('Ctrl Pts',(-6.21170000276441,-2.68459905305365,
-28.1728255747186));
#40762=CARTESIAN_POINT('Ctrl Pts',(-6.14165459494374,-2.84667206706981,
-28.1645218177815));
#40763=CARTESIAN_POINT('Ctrl Pts',(-6.065222546109,-3.00609347116171,-28.1562180608443));
#40764=CARTESIAN_POINT('Ctrl Pts',(-5.98263349844512,-3.16233860035296,
-28.1479143039072));
#40765=CARTESIAN_POINT('Ctrl Pts',(-5.9000779799436,-3.3185202977884,-28.1396139180951));
#40766=CARTESIAN_POINT('Ctrl Pts',(-5.81137060553026,-3.47152798271818,
-28.1313135322831));
#40767=CARTESIAN_POINT('Ctrl Pts',(-5.71678790923481,-3.62085970465948,
-28.1230131464711));
#40768=CARTESIAN_POINT('Ctrl Pts',(-5.62222515796898,-3.77015993642621,
-28.1147145109945));
#40769=CARTESIAN_POINT('Ctrl Pts',(-5.52178973910362,-3.91578545587575,
-28.1064158755178));
#40770=CARTESIAN_POINT('Ctrl Pts',(-5.4158027636553,-4.05726132079061,-28.0981172400412));
#40771=CARTESIAN_POINT('Ctrl Pts',(-5.30982054548079,-4.19873083549666,
-28.0898189770526));
#40772=CARTESIAN_POINT('Ctrl Pts',(-5.19828747593302,-4.33605078861525,
-28.0815207140641));
#40773=CARTESIAN_POINT('Ctrl Pts',(-5.08156649910743,-4.4687773400729,-28.0732224510755));
#40774=CARTESIAN_POINT('Ctrl Pts',(-4.96483138786964,-4.60151996414955,
-28.0649231832026));
#40775=CARTESIAN_POINT('Ctrl Pts',(-4.84290734763171,-4.7296678174379,-28.0566239153298));
#40776=CARTESIAN_POINT('Ctrl Pts',(-4.71619602803271,-4.8528119709266,-28.048324647457));
#40777=CARTESIAN_POINT('Ctrl Pts',(-4.58939573666474,-4.97604259145872,
-28.0400195521605));
#40778=CARTESIAN_POINT('Ctrl Pts',(-4.45780169889509,-5.09426224911316,
-28.031714456864));
#40779=CARTESIAN_POINT('Ctrl Pts',(-4.32185133935365,-5.20709996068129,
-28.0234093615675));
#40780=CARTESIAN_POINT('Ctrl Pts',(-4.1858514052418,-5.31997881874654,-28.0151012378014));
#40781=CARTESIAN_POINT('Ctrl Pts',(-4.04549225547649,-5.42747160272777,
-28.0067931140353));
#40782=CARTESIAN_POINT('Ctrl Pts',(-3.9012426614008,-5.52924901744047,-27.9984849902692));
#40783=CARTESIAN_POINT('Ctrl Pts',(-3.75683973083989,-5.63113462095708,
-27.9901680350156));
#40784=CARTESIAN_POINT('Ctrl Pts',(-3.60853838187039,-5.7272925221305,-27.9818510797619));
#40785=CARTESIAN_POINT('Ctrl Pts',(-3.45683541949477,-5.81743739824731,
-27.9735341245082));
#40786=CARTESIAN_POINT('Ctrl Pts',(-3.34503264432766,-5.88387280042489,
-27.9674046550256));
#40787=CARTESIAN_POINT('Ctrl Pts',(-3.2313828680445,-5.94704317520922,-27.961275185543));
#40788=CARTESIAN_POINT('Ctrl Pts',(-3.11609268191041,-6.00685070546492,
-27.9551457160604));
#40789=CARTESIAN_POINT('Ctrl Pts',(-2.95713600906782,-6.08931050832551,
-27.9466946925352));
#40790=CARTESIAN_POINT('Ctrl Pts',(-2.79476971361754,-6.16552663204085,
-27.93824366901));
#40791=CARTESIAN_POINT('Ctrl Pts',(-2.6295113109288,-6.23521926364242,-27.9297926454848));
#40792=CARTESIAN_POINT('Ctrl Pts',(-2.4643984133519,-6.30485053295324,-27.9213490628347));
#40793=CARTESIAN_POINT('Ctrl Pts',(-2.29639878804057,-6.36796963030381,
-27.9129054801845));
#40794=CARTESIAN_POINT('Ctrl Pts',(-2.12605320903425,-6.42434329347017,
-27.9044618975343));
#40795=CARTESIAN_POINT('Ctrl Pts',(-1.95583445761778,-6.48067498468827,
-27.8960246013945));
#40796=CARTESIAN_POINT('Ctrl Pts',(-1.78327354801447,-6.53027114940594,
-27.8875873052546));
#40797=CARTESIAN_POINT('Ctrl Pts',(-1.60893020449224,-6.57294702527508,
-27.8791500091148));
#40798=CARTESIAN_POINT('Ctrl Pts',(-1.43471124165274,-6.61559245516063,
-27.8707187323424));
#40799=CARTESIAN_POINT('Ctrl Pts',(-1.25871270257502,-6.65132736544411,
-27.86228745557));
#40800=CARTESIAN_POINT('Ctrl Pts',(-1.08150860985812,-6.68001707533767,
-27.8538561787977));
#40801=CARTESIAN_POINT('Ctrl Pts',(-0.904380473229808,-6.70869448778305,
-27.8454285159757));
#40802=CARTESIAN_POINT('Ctrl Pts',(-0.726048139738801,-6.73033266712018,
-27.8370008531538));
#40803=CARTESIAN_POINT('Ctrl Pts',(-0.547095591389842,-6.74484806455133,
-27.8285731903318));
#40804=CARTESIAN_POINT('Ctrl Pts',(-0.368198131713365,-6.75935899356902,
-27.8201481218778));
#40805=CARTESIAN_POINT('Ctrl Pts',(-0.188681167948277,-6.76675148666101,
-27.8117230534238));
#40806=CARTESIAN_POINT('Ctrl Pts',(-0.00913394119624452,-6.76699383560516,
-27.8032979849698));
#40807=CARTESIAN_POINT('Ctrl Pts',(0.0399956758395798,-6.76706014969439,
-27.8009926283563));
#40808=CARTESIAN_POINT('Ctrl Pts',(0.0891275412486155,-6.76659140642043,
-27.7986872717427));
#40809=CARTESIAN_POINT('Ctrl Pts',(0.138249557663999,-6.76558763595637,
-27.7963819151291));
#40810=CARTESIAN_POINT('Ctrl Pts',(0.321901012404443,-6.76183486032942,
-27.7877629266046));
#40811=CARTESIAN_POINT('Ctrl Pts',(0.505332709507144,-6.7506013072657,-27.7791439380802));
#40812=CARTESIAN_POINT('Ctrl Pts',(0.687930573940023,-6.7319418094216,-27.7705249495557));
#40813=CARTESIAN_POINT('Ctrl Pts',(0.870637830788935,-6.71327113287309,
-27.761900797488));
#40814=CARTESIAN_POINT('Ctrl Pts',(1.05250995546141,-6.68716566400971,-27.7532766454202));
#40815=CARTESIAN_POINT('Ctrl Pts',(1.23294001473092,-6.65373187918444,-27.7446524933525));
#40816=CARTESIAN_POINT('Ctrl Pts',(1.4195498520723,-6.61915297823408,-27.7357329617562));
#40817=CARTESIAN_POINT('Ctrl Pts',(1.60461674238068,-6.57673495314702,-27.7268134301599));
#40818=CARTESIAN_POINT('Ctrl Pts',(1.78748355630071,-6.52665239889138,-27.7178938985637));
#40819=CARTESIAN_POINT('Ctrl Pts',(1.96462392454099,-6.47813817198995,-27.7092536807044));
#40820=CARTESIAN_POINT('Ctrl Pts',(2.13969964485953,-6.42243231477914,-27.7006134628452));
#40821=CARTESIAN_POINT('Ctrl Pts',(2.31213091461799,-6.3597436767269,-27.691973244986));
#40822=CARTESIAN_POINT('Ctrl Pts',(2.49292350519993,-6.29401521987917,-27.6829140565212));
#40823=CARTESIAN_POINT('Ctrl Pts',(2.67080844790044,-6.22061009361683,-27.6738548680564));
#40824=CARTESIAN_POINT('Ctrl Pts',(2.84514282360538,-6.13982502301872,-27.6647956795917));
#40825=CARTESIAN_POINT('Ctrl Pts',(3.01947719931033,-6.0590399524206,-27.6557364911269));
#40826=CARTESIAN_POINT('Ctrl Pts',(3.19026068322077,-5.97087514244076,-27.6466773026621));
#40827=CARTESIAN_POINT('Ctrl Pts',(3.35688129178983,-5.8756818321648,-27.6376181141973));
#40828=CARTESIAN_POINT('Ctrl Pts',(3.52321324184415,-5.7806534376204,-27.628574620141));
#40829=CARTESIAN_POINT('Ctrl Pts',(3.6855503812889,-5.67853406541888,-27.6195311260847));
#40830=CARTESIAN_POINT('Ctrl Pts',(3.84331625777254,-5.56966867441335,-27.6104876320284));
#40831=CARTESIAN_POINT('Ctrl Pts',(4.00093782638581,-5.46090286218291,-27.601452410023));
#40832=CARTESIAN_POINT('Ctrl Pts',(4.153996284261,-5.34540348579733,-27.5924171880176));
#40833=CARTESIAN_POINT('Ctrl Pts',(4.30194381513703,-5.22355897941282,-27.5833819660122));
#40834=CARTESIAN_POINT('Ctrl Pts',(4.4496306946715,-5.10192913652328,-27.5743626621011));
#40835=CARTESIAN_POINT('Ctrl Pts',(4.59222444421059,-4.97397663734442,-27.5653433581899));
#40836=CARTESIAN_POINT('Ctrl Pts',(4.7292101174876,-4.84013023219964,-27.5563240542788));
#40837=CARTESIAN_POINT('Ctrl Pts',(4.86602393266931,-4.70645174671902,-27.5473160657144));
#40838=CARTESIAN_POINT('Ctrl Pts',(4.99724354268756,-4.56689427768299,-27.5383080771499));
#40839=CARTESIAN_POINT('Ctrl Pts',(5.12238877167882,-4.42192517708959,-27.5293000885855));
#40840=CARTESIAN_POINT('Ctrl Pts',(5.24725135578692,-4.27728349428773,-27.5203124448788));
#40841=CARTESIAN_POINT('Ctrl Pts',(5.36606678835974,-4.12725475676875,-27.5113248011721));
#40842=CARTESIAN_POINT('Ctrl Pts',(5.47839360298146,-3.97234093839034,-27.5023371574654));
#40843=CARTESIAN_POINT('Ctrl Pts',(5.57622247312257,-3.83742173969105,-27.4945095427323));
#40844=CARTESIAN_POINT('Ctrl Pts',(5.66913006210312,-3.69879774835549,-27.4866819279991));
#40845=CARTESIAN_POINT('Ctrl Pts',(5.75684829687764,-3.55682255485666,-27.478854313266));
#40846=CARTESIAN_POINT('Ctrl Pts',(5.84787846940244,-3.40948686813585,-27.4707311548207));
#40847=CARTESIAN_POINT('Ctrl Pts',(5.93327791108822,-3.25860712323924,-27.4626079963754));
#40848=CARTESIAN_POINT('Ctrl Pts',(6.01276744062879,-3.10466048142374,-27.4544848379301));
#40849=CARTESIAN_POINT('Ctrl Pts',(6.09225136574148,-2.95072469365226,-27.44636225221));
#40850=CARTESIAN_POINT('Ctrl Pts',(6.16582604076437,-2.79372276490383,-27.4382396664899));
#40851=CARTESIAN_POINT('Ctrl Pts',(6.23325843401677,-2.63415608777438,-27.4301170807698));
#40852=CARTESIAN_POINT('Ctrl Pts',(6.30069892996536,-2.47457023706612,-27.4219935190374));
#40853=CARTESIAN_POINT('Ctrl Pts',(6.36199553312253,-2.31241936193011,-27.413869957305));
#40854=CARTESIAN_POINT('Ctrl Pts',(6.41696353120311,-2.14822439219215,-27.4057463955726));
#40855=CARTESIAN_POINT('Ctrl Pts',(6.47197156694739,-1.9839098259033,-27.3976169167895));
#40856=CARTESIAN_POINT('Ctrl Pts',(6.52064167464196,-1.81754853877116,-27.3894874380064));
#40857=CARTESIAN_POINT('Ctrl Pts',(6.56283898308723,-1.64967678109096,-27.3813579592233));
#40858=CARTESIAN_POINT('Ctrl Pts',(6.60505349463245,-1.48173658504981,-27.3732251661947));
#40859=CARTESIAN_POINT('Ctrl Pts',(6.64078987144616,-1.31228504889536,-27.3650923731662));
#40860=CARTESIAN_POINT('Ctrl Pts',(6.66996452079699,-1.14186789573464,-27.3569595801377));
#40861=CARTESIAN_POINT('Ctrl Pts',(6.69917089315295,-0.971265439773515,
-27.3488179439305));
#40862=CARTESIAN_POINT('Ctrl Pts',(6.72180123960825,-0.799695632130619,
-27.3406763077234));
#40863=CARTESIAN_POINT('Ctrl Pts',(6.73782383170312,-0.627709337937163,
-27.3325346715163));
#40864=CARTESIAN_POINT('Ctrl Pts',(6.74598712474247,-0.540084657115235,
-27.3283866184556));
#40865=CARTESIAN_POINT('Ctrl Pts',(6.75243603773168,-0.452351885714152,
-27.324238565395));
#40866=CARTESIAN_POINT('Ctrl Pts',(6.7571715750192,-0.364583743127011,-27.3200905123343));
#40867=CARTESIAN_POINT('Ctrl Pts',(6.76680773924558,-0.1859876970055,-27.3116497973562));
#40868=CARTESIAN_POINT('Ctrl Pts',(6.76936609789953,-0.00687742669364791,
-27.3032090823781));
#40869=CARTESIAN_POINT('Ctrl Pts',(6.76480963877645,0.172161410069907,-27.2947683674001));
#40870=CARTESIAN_POINT('Ctrl Pts',(6.76025662363985,0.351064920845359,-27.286334032312));
#40871=CARTESIAN_POINT('Ctrl Pts',(6.74859951932881,0.52989677359061,-27.277899697224));
#40872=CARTESIAN_POINT('Ctrl Pts',(6.72985334847792,0.708069846823457,-27.269465362136));
#40873=CARTESIAN_POINT('Ctrl Pts',(6.71111846817762,0.886135608962445,-27.2610361069273));
#40874=CARTESIAN_POINT('Ctrl Pts',(6.68530306831416,1.06354305186015,-27.2526068517187));
#40875=CARTESIAN_POINT('Ctrl Pts',(6.65247414806712,1.23970831621745,-27.2441775965101));
#40876=CARTESIAN_POINT('Ctrl Pts',(6.61965996450019,1.41579450117988,-27.2357521251371));
#40877=CARTESIAN_POINT('Ctrl Pts',(6.57983859895231,1.59063929218077,-27.2273266537641));
#40878=CARTESIAN_POINT('Ctrl Pts',(6.53312853419137,1.76366679271754,-27.218901182391));
#40879=CARTESIAN_POINT('Ctrl Pts',(6.48643227828065,1.93664314130556,-27.2104782018318));
#40880=CARTESIAN_POINT('Ctrl Pts',(6.43285147120553,2.10780294926773,-27.2020552212725));
#40881=CARTESIAN_POINT('Ctrl Pts',(6.37255515602749,2.27658291818844,-27.1936322407133));
#40882=CARTESIAN_POINT('Ctrl Pts',(6.31225784246759,2.44536568175523,-27.185209120687));
#40883=CARTESIAN_POINT('Ctrl Pts',(6.2452449045544,2.61176821142514,-27.1767860006606));
#40884=CARTESIAN_POINT('Ctrl Pts',(6.17173470796589,2.77524407836306,-27.1683628806343));
#40885=CARTESIAN_POINT('Ctrl Pts',(6.09822196927221,2.93872559856902,-27.1599394693224));
#40886=CARTESIAN_POINT('Ctrl Pts',(6.01821166053042,3.09927995000798,-27.1515160580106));
#40887=CARTESIAN_POINT('Ctrl Pts',(5.9319696550329,3.2563821968204,-27.1430926466987));
#40888=CARTESIAN_POINT('Ctrl Pts',(5.84571263942648,3.41351178671026,-27.1346677693226));
#40889=CARTESIAN_POINT('Ctrl Pts',(5.75322192516306,3.56718778176935,-27.1262428919465));
#40890=CARTESIAN_POINT('Ctrl Pts',(5.65480873343709,3.71691097394646,-27.1178180145703));
#40891=CARTESIAN_POINT('Ctrl Pts',(5.55636468384588,3.86668111245268,-27.1093904955389));
#40892=CARTESIAN_POINT('Ctrl Pts',(5.45199463750489,4.01249569844281,-27.1009629765075));
#40893=CARTESIAN_POINT('Ctrl Pts',(5.34205261947399,4.15388526692434,-27.092535457476));
#40894=CARTESIAN_POINT('Ctrl Pts',(5.2320120096904,4.29540162810642,-27.0841003809713));
#40895=CARTESIAN_POINT('Ctrl Pts',(5.11638964894084,4.43248477926204,-27.0756653044665));
#40896=CARTESIAN_POINT('Ctrl Pts',(4.99557999268886,4.56469818680784,-27.0672302279617));
#40897=CARTESIAN_POINT('Ctrl Pts',(4.87471194833497,4.6969754939636,-27.0587910747289));
#40898=CARTESIAN_POINT('Ctrl Pts',(4.74865183921287,4.82437812303524,-27.0503519214961));
#40899=CARTESIAN_POINT('Ctrl Pts',(4.61783069589847,4.94650671322883,-27.0419127682634));
#40900=CARTESIAN_POINT('Ctrl Pts',(4.48686417361529,5.06877102252754,-27.0334642367652));
#40901=CARTESIAN_POINT('Ctrl Pts',(4.35112629457193,5.18574936040683,-27.0250157052671));
#40902=CARTESIAN_POINT('Ctrl Pts',(4.21108176802987,5.29708215369239,-27.016567173769));
#40903=CARTESIAN_POINT('Ctrl Pts',(4.13370262336073,5.35859713418308,-27.0118990860031));
#40904=CARTESIAN_POINT('Ctrl Pts',(4.05500924032428,5.41838931959196,-27.0072309982372));
#40905=CARTESIAN_POINT('Ctrl Pts',(3.97508375785797,5.47640375776054,-27.0025629104713));
#40906=CARTESIAN_POINT('Ctrl Pts',(3.83400746665901,5.57880491344033,-26.9943232791461));
#40907=CARTESIAN_POINT('Ctrl Pts',(3.68877700289684,5.67589260201036,-26.986083647821));
#40908=CARTESIAN_POINT('Ctrl Pts',(3.53982801636344,5.76731363934445,-26.9778440164958));
#40909=CARTESIAN_POINT('Ctrl Pts',(3.39622970023635,5.85545057350763,-26.9699003761171));
#40910=CARTESIAN_POINT('Ctrl Pts',(3.24917563626411,5.938320675094,-26.9619567357384));
#40911=CARTESIAN_POINT('Ctrl Pts',(3.09908550384719,6.01564277861013,-26.9540130953596));
#40912=CARTESIAN_POINT('Ctrl Pts',(3.09908550384723,6.01564277861011,-28.9543744409077));
#40913=CARTESIAN_POINT('Ctrl Pts',(2.93074066342593,6.10236918072498,-28.9454409168082));
#40914=CARTESIAN_POINT('Ctrl Pts',(2.75887803291552,6.18196094278929,-28.9365073927087));
#40915=CARTESIAN_POINT('Ctrl Pts',(2.58410552795895,6.25417361610405,-28.9275738686092));
#40916=CARTESIAN_POINT('Ctrl Pts',(2.4546895975365,6.30764581590827,-28.920958752956));
#40917=CARTESIAN_POINT('Ctrl Pts',(2.32367854641631,6.35707296890079,-28.9143436373028));
#40918=CARTESIAN_POINT('Ctrl Pts',(2.19132453108998,6.40237345048251,-28.9077285216496));
#40919=CARTESIAN_POINT('Ctrl Pts',(2.02678076599642,6.45869143812821,-28.8995045472321));
#40920=CARTESIAN_POINT('Ctrl Pts',(1.85984636351425,6.5087367461534,-28.8912805728145));
#40921=CARTESIAN_POINT('Ctrl Pts',(1.69104018799337,6.55230280760828,-28.8830565983969));
#40922=CARTESIAN_POINT('Ctrl Pts',(1.52241228817216,6.5958228590753,-28.8748413092943));
#40923=CARTESIAN_POINT('Ctrl Pts',(1.35191689607876,6.63287720124364,-28.8666260201916));
#40924=CARTESIAN_POINT('Ctrl Pts',(1.18009075940021,6.66330809730259,-28.858410731089));
#40925=CARTESIAN_POINT('Ctrl Pts',(1.00841162313236,6.69371295917195,-28.8502024703168));
#40926=CARTESIAN_POINT('Ctrl Pts',(0.835404360778233,6.71750559811737,-28.8419942095446));
#40927=CARTESIAN_POINT('Ctrl Pts',(0.66161880973207,6.73457864685006,-28.8337859487724));
#40928=CARTESIAN_POINT('Ctrl Pts',(0.48794708766042,6.75164051279098,-28.8255830643845));
#40929=CARTESIAN_POINT('Ctrl Pts',(0.313498447920012,6.76199152053251,-28.8173801799966));
#40930=CARTESIAN_POINT('Ctrl Pts',(0.138830895033099,6.76557573178989,-28.8091772956087));
#40931=CARTESIAN_POINT('Ctrl Pts',(-0.0357572686251395,6.76915831396527,
-28.8009781395645));
#40932=CARTESIAN_POINT('Ctrl Pts',(-0.210563789420254,6.76598021974895,
-28.7927789835203));
#40933=CARTESIAN_POINT('Ctrl Pts',(-0.385027498984551,6.75603750914881,
-28.784579827476));
#40934=CARTESIAN_POINT('Ctrl Pts',(-0.559476034448037,6.74609566332276,
-28.776381384559));
#40935=CARTESIAN_POINT('Ctrl Pts',(-0.733581459842993,6.7293903849033,-28.768182941642));
#40936=CARTESIAN_POINT('Ctrl Pts',(-0.906784197880069,6.70596983429504,
-28.759984498725));
#40937=CARTESIAN_POINT('Ctrl Pts',(-1.07998521102291,6.68254951692774,-28.7517861374548));
#40938=CARTESIAN_POINT('Ctrl Pts',(-1.25228319910867,6.65241410759397,-28.7435877761846));
#40939=CARTESIAN_POINT('Ctrl Pts',(-1.42312540678331,6.61566346457918,-28.7353894149143));
#40940=CARTESIAN_POINT('Ctrl Pts',(-1.59399694778214,6.57890651153984,-28.7271896459991));
#40941=CARTESIAN_POINT('Ctrl Pts',(-1.76341185970093,6.53553213736093,-28.7189898770838));
#40942=CARTESIAN_POINT('Ctrl Pts',(-1.93082919855987,6.48569098909196,-28.7107901081685));
#40943=CARTESIAN_POINT('Ctrl Pts',(-2.09830569557285,6.43583222908489,-28.7025874418043));
#40944=CARTESIAN_POINT('Ctrl Pts',(-2.26378286987201,6.37950224534938,-28.6943847754401));
#40945=CARTESIAN_POINT('Ctrl Pts',(-2.42673646242253,6.31690107109087,-28.6861821090758));
#40946=CARTESIAN_POINT('Ctrl Pts',(-2.58987512952515,6.25422879754511,-28.6779701265328));
#40947=CARTESIAN_POINT('Ctrl Pts',(-2.75048415367643,6.18527123286659,-28.6697581439898));
#40948=CARTESIAN_POINT('Ctrl Pts',(-2.90805977032927,6.11027637445251,-28.6615461614468));
#40949=CARTESIAN_POINT('Ctrl Pts',(-3.0657283272101,6.03523728305754,-28.6533293353655));
#40950=CARTESIAN_POINT('Ctrl Pts',(-3.22035959304848,5.95415396612532,-28.6451125092842));
#40951=CARTESIAN_POINT('Ctrl Pts',(-3.3714759373419,5.86731957574535,-28.6368956832029));
#40952=CARTESIAN_POINT('Ctrl Pts',(-3.52282532486363,5.7803512741941,-28.628666185589));
#40953=CARTESIAN_POINT('Ctrl Pts',(-3.6706486550626,5.68761436624255,-28.6204366879752));
#40954=CARTESIAN_POINT('Ctrl Pts',(-3.814497632205,5.58944512576181,-28.6122071903614));
#40955=CARTESIAN_POINT('Ctrl Pts',(-3.94271848121428,5.50194124765932,-28.6048717668364));
#40956=CARTESIAN_POINT('Ctrl Pts',(-4.06778194823807,5.41012197708436,-28.5975363433115));
#40957=CARTESIAN_POINT('Ctrl Pts',(-4.18939427405906,5.31425108707532,-28.5902009197866));
#40958=CARTESIAN_POINT('Ctrl Pts',(-4.32169451661494,5.20995457011769,-28.5822208215108));
#40959=CARTESIAN_POINT('Ctrl Pts',(-4.45036072809953,5.10050658472618,-28.574240723235));
#40960=CARTESIAN_POINT('Ctrl Pts',(-4.57494775252778,4.98619514877237,-28.5662606249592));
#40961=CARTESIAN_POINT('Ctrl Pts',(-4.6993801079693,4.87202562514088,-28.5582904336037));
#40962=CARTESIAN_POINT('Ctrl Pts',(-4.81974307204676,4.75300491405228,-28.5503202422481));
#40963=CARTESIAN_POINT('Ctrl Pts',(-4.93562074350316,4.62946399449238,-28.5423500508926));
#40964=CARTESIAN_POINT('Ctrl Pts',(-5.05138093085121,4.50604832852617,-28.5343879402209));
#40965=CARTESIAN_POINT('Ctrl Pts',(-5.16266461369269,4.37812184624029,-28.5264258295491));
#40966=CARTESIAN_POINT('Ctrl Pts',(-5.2690894278619,4.24605529888554,-28.5184637188774));
#40967=CARTESIAN_POINT('Ctrl Pts',(-5.37543048518111,4.1140926885504,-28.5105078744258));
#40968=CARTESIAN_POINT('Ctrl Pts',(-5.47692004453577,3.97799679110307,-28.5025520299742));
#40969=CARTESIAN_POINT('Ctrl Pts',(-5.5732132071822,3.83817450714398,-28.4945961855226));
#40970=CARTESIAN_POINT('Ctrl Pts',(-5.66992782327639,3.69774025259395,-28.4866055201347));
#40971=CARTESIAN_POINT('Ctrl Pts',(-5.76140017579024,3.55354719239718,-28.4786148547469));
#40972=CARTESIAN_POINT('Ctrl Pts',(-5.84732194109161,3.40604097409715,-28.470624189359));
#40973=CARTESIAN_POINT('Ctrl Pts',(-5.93280275843591,3.25929175334467,-28.4626745318295));
#40974=CARTESIAN_POINT('Ctrl Pts',(-6.01278963937287,3.10926363788242,-28.4547248743));
#40975=CARTESIAN_POINT('Ctrl Pts',(-6.08702289982685,2.95642372081263,-28.4467752167705));
#40976=CARTESIAN_POINT('Ctrl Pts',(-6.16125164055588,2.80359310946888,-28.4388260432594));
#40977=CARTESIAN_POINT('Ctrl Pts',(-6.2297272909782,2.64795137992276,-28.4308768697483));
#40978=CARTESIAN_POINT('Ctrl Pts',(-6.29223687319425,2.48998878142345,-28.4229276962372));
#40979=CARTESIAN_POINT('Ctrl Pts',(-6.35475543993098,2.33200347891328,-28.4149773801891));
#40980=CARTESIAN_POINT('Ctrl Pts',(-6.41130609288055,2.17169699852571,-28.4070270641409));
#40981=CARTESIAN_POINT('Ctrl Pts',(-6.46172469727903,2.0095778005776,-28.3990767480928));
#40982=CARTESIAN_POINT('Ctrl Pts',(-6.51259395384014,1.84600954690824,-28.3910553704362));
#40983=CARTESIAN_POINT('Ctrl Pts',(-6.55722088757064,1.68059638973622,-28.3830339927797));
#40984=CARTESIAN_POINT('Ctrl Pts',(-6.59548907831681,1.51387344841095,-28.3750126151232));
#40985=CARTESIAN_POINT('Ctrl Pts',(-6.63346996163374,1.34840221872225,-28.3670514598432));
#40986=CARTESIAN_POINT('Ctrl Pts',(-6.66518724716878,1.18164119134741,-28.3590903045632));
#40987=CARTESIAN_POINT('Ctrl Pts',(-6.69057910139988,1.0141204503959,-28.3511291492833));
#40988=CARTESIAN_POINT('Ctrl Pts',(-6.71625907169329,0.844698886613637,
-28.3430776604385));
#40989=CARTESIAN_POINT('Ctrl Pts',(-6.73546915322974,0.674500664825639,
-28.3350261715937));
#40990=CARTESIAN_POINT('Ctrl Pts',(-6.74819954296709,0.504075320065096,
-28.3269746827488));
#40991=CARTESIAN_POINT('Ctrl Pts',(-6.76092993270445,0.333649975304522,
-28.318923193904));
#40992=CARTESIAN_POINT('Ctrl Pts',(-6.76718068348335,0.162997905035864,
-28.3108717050592));
#40993=CARTESIAN_POINT('Ctrl Pts',(-6.76699602342832,-0.00733613694335302,
-28.3028202162144));
#40994=CARTESIAN_POINT('',(-6.76716557178108,-0.00065835778244856,-28.6968932965683));
#40995=CARTESIAN_POINT('Ctrl Pts',(3.09908550384723,6.01564277861011,-29.348603209574));
#40996=CARTESIAN_POINT('Ctrl Pts',(2.9337323201833,6.10082796552479,-29.3398537616747));
#40997=CARTESIAN_POINT('Ctrl Pts',(2.76486502144426,6.1791915818019,-29.3311043137754));
#40998=CARTESIAN_POINT('Ctrl Pts',(2.59305716434351,6.25046746591379,-29.3223548658761));
#40999=CARTESIAN_POINT('Ctrl Pts',(2.42125069459283,6.32174277447224,-29.3136054886287));
#41000=CARTESIAN_POINT('Ctrl Pts',(2.2465039787106,6.38593035557825,-29.3048561113812));
#41001=CARTESIAN_POINT('Ctrl Pts',(2.06941053323774,6.44281220003538,-29.2961067341338));
#41002=CARTESIAN_POINT('Ctrl Pts',(1.89231845896683,6.49969360406686,-29.2873574246312));
#41003=CARTESIAN_POINT('Ctrl Pts',(1.71287996431501,6.54926929700882,-29.2786081151286));
#41004=CARTESIAN_POINT('Ctrl Pts',(1.53170449173496,6.59137090065481,-29.269858805626));
#41005=CARTESIAN_POINT('Ctrl Pts',(1.35053036178162,6.63347219230085,-29.2611095609614));
#41006=CARTESIAN_POINT('Ctrl Pts',(1.16761955878835,6.66809944062456,-29.2523603162969));
#41007=CARTESIAN_POINT('Ctrl Pts',(0.983593309310392,6.69513503985393,-29.2436110716323));
#41008=CARTESIAN_POINT('Ctrl Pts',(0.799568362459799,6.72217044771217,-29.2348618888991));
#41009=CARTESIAN_POINT('Ctrl Pts',(0.614428268438325,6.7416142723598,-29.2261127061659));
#41010=CARTESIAN_POINT('Ctrl Pts',(0.428801816329911,6.75340047696804,-29.2173635234327));
#41011=CARTESIAN_POINT('Ctrl Pts',(0.243176616522344,6.76518660206244,-29.2086143997246));
#41012=CARTESIAN_POINT('Ctrl Pts',(0.0570653511649389,6.76931519233997,
-29.1998652760165));
#41013=CARTESIAN_POINT('Ctrl Pts',(-0.128899900800633,6.76577222610794,
-29.1911161523083));
#41014=CARTESIAN_POINT('Ctrl Pts',(-0.314863959942703,6.7622292826013,-29.1823670847191));
#41015=CARTESIAN_POINT('Ctrl Pts',(-0.500681721081441,6.75101488651271,
-29.1736180171298));
#41016=CARTESIAN_POINT('Ctrl Pts',(-0.685722110174135,6.73216712415982,
-29.1648689495405));
#41017=CARTESIAN_POINT('Ctrl Pts',(-0.870761373828476,6.71331947644134,
-29.1561199351642));
#41018=CARTESIAN_POINT('Ctrl Pts',(-1.05502298984432,6.68683858439982,-29.1473709207878));
#41019=CARTESIAN_POINT('Ctrl Pts',(-1.23788117676151,6.65281438131409,-29.1386219064114));
#41020=CARTESIAN_POINT('Ctrl Pts',(-1.43009641451888,6.61704912302357,-29.1294251955239));
#41021=CARTESIAN_POINT('Ctrl Pts',(-1.62076048992794,6.57294837083141,-29.1202284846364));
#41022=CARTESIAN_POINT('Ctrl Pts',(-1.80915798961233,6.52067760042021,-29.1110317737488));
#41023=CARTESIAN_POINT('Ctrl Pts',(-1.98840443003115,6.47094578577377,-29.1022817760423));
#41024=CARTESIAN_POINT('Ctrl Pts',(-2.16559895952297,6.4138188847444,-29.0935317783358));
#41025=CARTESIAN_POINT('Ctrl Pts',(-2.34013966242429,6.34949095285195,-29.0847817806293));
#41026=CARTESIAN_POINT('Ctrl Pts',(-2.51467682554121,6.28516432556642,-29.0760319603777));
#41027=CARTESIAN_POINT('Ctrl Pts',(-2.68656000078947,6.21363705879615,-29.0672821401261));
#41028=CARTESIAN_POINT('Ctrl Pts',(-2.85520533840993,6.13515211510811,-29.0585323198745));
#41029=CARTESIAN_POINT('Ctrl Pts',(-3.02384747998429,6.0566686588107,-29.0497826654433));
#41030=CARTESIAN_POINT('Ctrl Pts',(-3.18925164684636,5.97122791039791,-29.041033011012));
#41031=CARTESIAN_POINT('Ctrl Pts',(-3.35085601829255,5.87912008251853,-29.0322833565808));
#41032=CARTESIAN_POINT('Ctrl Pts',(-3.51245754191513,5.78701387778117,-29.0235338563377));
#41033=CARTESIAN_POINT('Ctrl Pts',(-3.67025915511029,5.68824097060923,-29.0147843560945));
#41034=CARTESIAN_POINT('Ctrl Pts',(-3.82372487928925,5.58313684656793,-29.0060348558514));
#41035=CARTESIAN_POINT('Ctrl Pts',(-3.97718810300878,5.47803443501715,-28.9972854981663));
#41036=CARTESIAN_POINT('Ctrl Pts',(-4.12631534263096,5.36660117496322,-28.9885361404812));
#41037=CARTESIAN_POINT('Ctrl Pts',(-4.27060009886285,5.24921554097301,-28.979786782796));
#41038=CARTESIAN_POINT('Ctrl Pts',(-4.41488269594267,5.13183166360245,-28.9710375560409));
#41039=CARTESIAN_POINT('Ctrl Pts',(-4.55432273235136,5.00849577139427,-28.9622883292857));
#41040=CARTESIAN_POINT('Ctrl Pts',(-4.68844662480249,4.87962675277302,-28.9535391025305));
#41041=CARTESIAN_POINT('Ctrl Pts',(-4.82256868835199,4.7507594913984,-28.944789995079));
#41042=CARTESIAN_POINT('Ctrl Pts',(-4.95137454637903,4.61635945312482,-28.9360408876275));
#41043=CARTESIAN_POINT('Ctrl Pts',(-5.07442674461117,4.47688309134546,-28.927291780176));
#41044=CARTESIAN_POINT('Ctrl Pts',(-5.19747742838597,4.33740844616283,-28.9185427804037));
#41045=CARTESIAN_POINT('Ctrl Pts',(-5.31477440451002,4.19285781735936,-28.9097937806313));
#41046=CARTESIAN_POINT('Ctrl Pts',(-5.42591931531242,4.04372211999286,-28.9010447808589));
#41047=CARTESIAN_POINT('Ctrl Pts',(-5.53707636463076,3.89457013500667,-28.8922948255783));
#41048=CARTESIAN_POINT('Ctrl Pts',(-5.6420798327357,3.74083230916271,-28.8835448702977));
#41049=CARTESIAN_POINT('Ctrl Pts',(-5.7405730346885,3.58303087251663,-28.8747949150171));
#41050=CARTESIAN_POINT('Ctrl Pts',(-5.83906243363864,3.42523552887262,-28.8660452975883));
#41051=CARTESIAN_POINT('Ctrl Pts',(-5.93104191768521,3.26337713156819,-28.8572956801595));
#41052=CARTESIAN_POINT('Ctrl Pts',(-6.01619906699748,3.09800545290977,-28.8485460627307));
#41053=CARTESIAN_POINT('Ctrl Pts',(-6.10135338095468,2.93263928039419,-28.8397967366253));
#41054=CARTESIAN_POINT('Ctrl Pts',(-6.17968568352917,2.76376031540049,-28.8310474105199));
#41055=CARTESIAN_POINT('Ctrl Pts',(-6.25092992694958,2.59194213831369,-28.8222980844145));
#41056=CARTESIAN_POINT('Ctrl Pts',(-6.32217217691175,2.42012876880634,-28.8135490031207));
#41057=CARTESIAN_POINT('Ctrl Pts',(-6.38632665483921,2.24537661647471,-28.8047999218269));
#41058=CARTESIAN_POINT('Ctrl Pts',(-6.44317547869418,2.06827917621244,-28.7960508405331));
#41059=CARTESIAN_POINT('Ctrl Pts',(-6.50002944236,1.89116572423205,-28.7873009682182));
#41060=CARTESIAN_POINT('Ctrl Pts',(-6.54957634250457,1.71170683288974,-28.7785510959032));
#41061=CARTESIAN_POINT('Ctrl Pts',(-6.59164787708449,1.53051209225135,-28.7698012235882));
#41062=CARTESIAN_POINT('Ctrl Pts',(-6.63371649075056,1.34932993147799,-28.7610519587534));
#41063=CARTESIAN_POINT('Ctrl Pts',(-6.66831071257165,1.16641244173772,-28.7523026939186));
#41064=CARTESIAN_POINT('Ctrl Pts',(-6.69531304840367,0.982380875157681,
-28.7435534290839));
#41065=CARTESIAN_POINT('Ctrl Pts',(-6.72231677033071,0.798339861793501,
-28.7348037151282));
#41066=CARTESIAN_POINT('Ctrl Pts',(-6.74172778477911,0.613184940727803,
-28.7260540011725));
#41067=CARTESIAN_POINT('Ctrl Pts',(-6.75348015835533,0.427545027688197,
-28.7173042872169));
#41068=CARTESIAN_POINT('Ctrl Pts',(-6.76249038365226,0.285219953545373,
-28.7105961194146));
#41069=CARTESIAN_POINT('Ctrl Pts',(-6.767,0.142609995756768,-28.7038879516124));
#41070=CARTESIAN_POINT('Ctrl Pts',(-6.767,2.92894570544878E-13,-28.6971797838101));
#41071=CARTESIAN_POINT('Ctrl Pts',(-6.7669992726319,-0.00313754671095234,
-28.6971797838101));
#41072=CARTESIAN_POINT('Ctrl Pts',(-6.76690773148581,-0.200571697034152,
-28.6879156319988));
#41073=CARTESIAN_POINT('Ctrl Pts',(-6.75817155794658,-0.397750728450315,
-28.6786514801875));
#41074=CARTESIAN_POINT('Ctrl Pts',(-6.74088222003617,-0.593966241128391,
-28.6693873283761));
#41075=CARTESIAN_POINT('Ctrl Pts',(-6.72350447558709,-0.79118507356343,
-28.6600758056591));
#41076=CARTESIAN_POINT('Ctrl Pts',(-6.69748593276225,-0.987430335429607,
-28.6507642829421));
#41077=CARTESIAN_POINT('Ctrl Pts',(-6.66297023084457,-1.18199691322738,
-28.6414527602251));
#41078=CARTESIAN_POINT('Ctrl Pts',(-6.62837627730316,-1.37700459897866,
-28.6321201270647));
#41079=CARTESIAN_POINT('Ctrl Pts',(-6.58524667423045,-1.57032581884113,
-28.6227874939043));
#41080=CARTESIAN_POINT('Ctrl Pts',(-6.53377579614006,-1.76126739757889,
-28.6134548607439));
#41081=CARTESIAN_POINT('Ctrl Pts',(-6.48216851314583,-1.95271499775349,
-28.6040974948225));
#41082=CARTESIAN_POINT('Ctrl Pts',(-6.4221757607285,-2.14177016752003,-28.594740128901));
#41083=CARTESIAN_POINT('Ctrl Pts',(-6.35404225119917,-2.32775343839845,
-28.5853827629796));
#41084=CARTESIAN_POINT('Ctrl Pts',(-6.30400694633252,-2.46433424456539,
-28.5785109805063));
#41085=CARTESIAN_POINT('Ctrl Pts',(-6.24958233640898,-2.59925876060361,
-28.571639198033));
#41086=CARTESIAN_POINT('Ctrl Pts',(-6.19088166755803,-2.73226521009471,
-28.5647674155597));
#41087=CARTESIAN_POINT('Ctrl Pts',(-6.12048668033918,-2.89176913901457,
-28.5565266399629));
#41088=CARTESIAN_POINT('Ctrl Pts',(-6.04382629762756,-3.04877103020393,
-28.5482858643662));
#41089=CARTESIAN_POINT('Ctrl Pts',(-5.96109935751612,-3.2027462356267,-28.5400450887695));
#41090=CARTESIAN_POINT('Ctrl Pts',(-5.87846404645946,-3.35655089681664,
-28.5318134407251));
#41091=CARTESIAN_POINT('Ctrl Pts',(-5.78977572440595,-3.50733523678609,
-28.5235817926807));
#41092=CARTESIAN_POINT('Ctrl Pts',(-5.69528136573571,-3.65459425451083,
-28.5153501446364));
#41093=CARTESIAN_POINT('Ctrl Pts',(-5.60087483003553,-3.80171640983991,
-28.5071261470781));
#41094=CARTESIAN_POINT('Ctrl Pts',(-5.50067319529155,-3.94531947036094,
-28.4989021495199));
#41095=CARTESIAN_POINT('Ctrl Pts',(-5.39496949248503,-4.08492266452571,
-28.4906781519617));
#41096=CARTESIAN_POINT('Ctrl Pts',(-5.28935917931002,-4.22440251872684,
-28.4824614203372));
#41097=CARTESIAN_POINT('Ctrl Pts',(-5.17825670070644,-4.35988926743616,
-28.4742446887127));
#41098=CARTESIAN_POINT('Ctrl Pts',(-5.06199848340014,-4.4909309006101,-28.4660279570882));
#41099=CARTESIAN_POINT('Ctrl Pts',(-4.9457998294826,-4.62190539630404,-28.4578154351995));
#41100=CARTESIAN_POINT('Ctrl Pts',(-4.82445093317755,-4.7484390466513,-28.4496029133108));
#41101=CARTESIAN_POINT('Ctrl Pts',(-4.69832885840152,-4.87011241536697,
-28.4413903914221));
#41102=CARTESIAN_POINT('Ctrl Pts',(-4.57224895945459,-4.99174509592226,
-28.4331806158403));
#41103=CARTESIAN_POINT('Ctrl Pts',(-4.44139931757727,-5.10852048588802,
-28.4249708402585));
#41104=CARTESIAN_POINT('Ctrl Pts',(-4.30619431782448,-5.22005550709341,
-28.4167610646766));
#41105=CARTESIAN_POINT('Ctrl Pts',(-4.24714028657992,-5.26877110665828,
-28.4131752479938));
#41106=CARTESIAN_POINT('Ctrl Pts',(-4.18725584013383,-5.31648747855582,
-28.4095894313109));
#41107=CARTESIAN_POINT('Ctrl Pts',(-4.12657757471939,-5.36317504094571,
-28.4060036146281));
#41108=CARTESIAN_POINT('Ctrl Pts',(-3.97667264076494,-5.47851610926318,
-28.3971448971063));
#41109=CARTESIAN_POINT('Ctrl Pts',(-3.82207609594595,-5.58745587566541,
-28.3882861795845));
#41110=CARTESIAN_POINT('Ctrl Pts',(-3.66334657324155,-5.68965560331373,
-28.3794274620628));
#41111=CARTESIAN_POINT('Ctrl Pts',(-3.50432009309359,-5.79204653023827,
-28.3705521713033));
#41112=CARTESIAN_POINT('Ctrl Pts',(-3.34114540096804,-5.8876720787245,-28.3616768805438));
#41113=CARTESIAN_POINT('Ctrl Pts',(-3.17440617371424,-5.97623915554632,
-28.3528015897844));
#41114=CARTESIAN_POINT('Ctrl Pts',(-3.0071933695647,-6.06505778278009,-28.3439010912036));
#41115=CARTESIAN_POINT('Ctrl Pts',(-2.83639600123169,-6.14677769813225,
-28.3350005926228));
#41116=CARTESIAN_POINT('Ctrl Pts',(-2.66262103874598,-6.2211524819785,-28.3261000940421));
#41117=CARTESIAN_POINT('Ctrl Pts',(-2.48861083686074,-6.29562794706929,
-28.3171875468444));
#41118=CARTESIAN_POINT('Ctrl Pts',(-2.31161523008141,-6.36273832269259,
-28.3082749996468));
#41119=CARTESIAN_POINT('Ctrl Pts',(-2.13225818845227,-6.42228651009734,
-28.2993624524492));
#41120=CARTESIAN_POINT('Ctrl Pts',(-1.95250510895869,-6.48196618571553,
-28.2904302254769));
#41121=CARTESIAN_POINT('Ctrl Pts',(-1.77038041233506,-6.53405019220034,
-28.2814979985046));
#41122=CARTESIAN_POINT('Ctrl Pts',(-1.58652293478772,-6.57839144300433,
-28.2725657715324));
#41123=CARTESIAN_POINT('Ctrl Pts',(-1.41275638740813,-6.62029904535745,
-28.2641237855871));
#41124=CARTESIAN_POINT('Ctrl Pts',(-1.23744231443331,-6.65529088456251,
-28.2556817996419));
#41125=CARTESIAN_POINT('Ctrl Pts',(-1.06112567594325,-6.68328521760474,
-28.2472398136967));
#41126=CARTESIAN_POINT('Ctrl Pts',(-0.889362357011027,-6.71055660614642,
-28.2390158392791));
#41127=CARTESIAN_POINT('Ctrl Pts',(-0.716319313894368,-6.73123830859869,
-28.2307918648615));
#41128=CARTESIAN_POINT('Ctrl Pts',(-0.542543145037324,-6.74521578126104,
-28.222567890444));
#41129=CARTESIAN_POINT('Ctrl Pts',(-0.368950500675128,-6.75917849235611,
-28.2143526013413));
#41130=CARTESIAN_POINT('Ctrl Pts',(-0.194626626851767,-6.76645104443985,
-28.2061373122387));
#41131=CARTESIAN_POINT('Ctrl Pts',(-0.0201273681247383,-6.76697006710185,
-28.197922023136));
#41132=CARTESIAN_POINT('Ctrl Pts',(0.154222603286449,-6.76748864573044,
-28.1897137623638));
#41133=CARTESIAN_POINT('Ctrl Pts',(0.328747304201376,-6.76126520088701,
-28.1815055015917));
#41134=CARTESIAN_POINT('Ctrl Pts',(0.502886630532824,-6.74828823012409,
-28.1732972408195));
#41135=CARTESIAN_POINT('Ctrl Pts',(0.676911896168154,-6.73531975923509,
-28.1650943564316));
#41136=CARTESIAN_POINT('Ctrl Pts',(0.850551933686825,-6.71560660020399,
-28.1568914720437));
#41137=CARTESIAN_POINT('Ctrl Pts',(1.02324741081172,-6.68918931831557,-28.1486885876558));
#41138=CARTESIAN_POINT('Ctrl Pts',(1.19586439504825,-6.66278404350917,-28.1404894316116));
#41139=CARTESIAN_POINT('Ctrl Pts',(1.36753732046336,-6.62968077063963,-28.1322902755674));
#41140=CARTESIAN_POINT('Ctrl Pts',(1.53771265338977,-6.58997183572168,-28.1240911195232));
#41141=CARTESIAN_POINT('Ctrl Pts',(1.70787318520008,-6.55026635451554,-28.1158926766062));
#41142=CARTESIAN_POINT('Ctrl Pts',(1.87653603308155,-6.50395642875941,-28.1076942336892));
#41143=CARTESIAN_POINT('Ctrl Pts',(2.04315816399235,-6.45118545051306,-28.0994957907722));
#41144=CARTESIAN_POINT('Ctrl Pts',(2.20977863554397,-6.39841499780319,-28.0912974295019));
#41145=CARTESIAN_POINT('Ctrl Pts',(2.37435808832747,-6.3391837280583,-28.0830990682317));
#41146=CARTESIAN_POINT('Ctrl Pts',(2.53636907430538,-6.27368479594786,-28.0749007069615));
#41147=CARTESIAN_POINT('Ctrl Pts',(2.69840787730143,-6.20817461777918,-28.0667009380462));
#41148=CARTESIAN_POINT('Ctrl Pts',(2.85787700233019,-6.13639476769248,-28.0585011691309));
#41149=CARTESIAN_POINT('Ctrl Pts',(3.01426934603287,-6.05858641182633,-28.0503014002157));
#41150=CARTESIAN_POINT('Ctrl Pts',(3.17071695212731,-5.98075056180194,-28.0420987338514));
#41151=CARTESIAN_POINT('Ctrl Pts',(3.3240852902191,-5.89688212224843,-28.0338960674871));
#41152=CARTESIAN_POINT('Ctrl Pts',(3.47389216253669,-5.80726805331614,-28.0256934011228));
#41153=CARTESIAN_POINT('Ctrl Pts',(3.62386917801668,-5.71755220520076,-28.0174814185798));
#41154=CARTESIAN_POINT('Ctrl Pts',(3.77027633859534,-5.62207787516147,-28.0092694360368));
#41155=CARTESIAN_POINT('Ctrl Pts',(3.91265986140665,-5.52117576327156,-28.0010574534937));
#41156=CARTESIAN_POINT('Ctrl Pts',(4.05512736394403,-5.42021413795236,-27.9928406274124));
#41157=CARTESIAN_POINT('Ctrl Pts',(4.19356621415738,-5.31381856750332,-27.9846238013311));
#41158=CARTESIAN_POINT('Ctrl Pts',(4.32755611841255,-5.20235975707083,-27.9764069752499));
#41159=CARTESIAN_POINT('Ctrl Pts',(4.46175265445181,-5.09072906105502,-27.968177477636));
#41160=CARTESIAN_POINT('Ctrl Pts',(4.59148626747131,-4.97401976108095,-27.9599479800222));
#41161=CARTESIAN_POINT('Ctrl Pts',(4.7163729578319,-4.85264001576791,-27.9517184824083));
#41162=CARTESIAN_POINT('Ctrl Pts',(4.82769163236163,-4.74444728262724,-27.9443830588834));
#41163=CARTESIAN_POINT('Ctrl Pts',(4.93515976692244,-4.63254442615424,-27.9370476353585));
#41164=CARTESIAN_POINT('Ctrl Pts',(5.03853317892781,-4.51724168103099,-27.9297122118336));
#41165=CARTESIAN_POINT('Ctrl Pts',(5.15227076833743,-4.39037872828305,-27.9216413416472));
#41166=CARTESIAN_POINT('Ctrl Pts',(5.26142151905001,-4.25898564716953,-27.9135704714608));
#41167=CARTESIAN_POINT('Ctrl Pts',(5.36559293037466,-4.12343321826769,-27.9054996012744));
#41168=CARTESIAN_POINT('Ctrl Pts',(5.46963470847495,-3.98804947382741,-27.8974387746586));
#41169=CARTESIAN_POINT('Ctrl Pts',(5.5687092520658,-3.84851697256138,-27.8893779480428));
#41170=CARTESIAN_POINT('Ctrl Pts',(5.6624606030548,-3.70524343584227,-27.881317121427));
#41171=CARTESIAN_POINT('Ctrl Pts',(5.75611584601515,-3.56211677420312,-27.8732645582671));
#41172=CARTESIAN_POINT('Ctrl Pts',(5.84445855350297,-3.41525701855249,-27.8652119951072));
#41173=CARTESIAN_POINT('Ctrl Pts',(5.92717287637335,-3.26510500498592,-27.8571594319473));
#41174=CARTESIAN_POINT('Ctrl Pts',(6.00982051705628,-3.11507404016117,-27.8491133605594));
#41175=CARTESIAN_POINT('Ctrl Pts',(6.08684862519433,-2.96175642513735,-27.8410672891715));
#41176=CARTESIAN_POINT('Ctrl Pts',(6.15798461741865,-2.80562193668985,-27.8330212177837));
#41177=CARTESIAN_POINT('Ctrl Pts',(6.22907882180025,-2.64957916726169,-27.8249798729478));
#41178=CARTESIAN_POINT('Ctrl Pts',(6.2942876463808,-2.49072315710083,-27.8169385281119));
#41179=CARTESIAN_POINT('Ctrl Pts',(6.35338448663524,-2.32954814609673,-27.808897183276));
#41180=CARTESIAN_POINT('Ctrl Pts',(6.4136205321285,-2.16526617681682,-27.8007008260549));
#41181=CARTESIAN_POINT('Ctrl Pts',(6.46750635923963,-1.99857523600003,-27.7925044688339));
#41182=CARTESIAN_POINT('Ctrl Pts',(6.51485336973347,-1.83002037444189,-27.7843081116128));
#41183=CARTESIAN_POINT('Ctrl Pts',(6.56129017123856,-1.66470584735237,-27.7762693229043));
#41184=CARTESIAN_POINT('Ctrl Pts',(6.60143719935804,-1.49759879257117,-27.7682305341958));
#41185=CARTESIAN_POINT('Ctrl Pts',(6.63516695392705,-1.32922853321558,-27.7601917454873));
#41186=CARTESIAN_POINT('Ctrl Pts',(6.66890031788542,-1.16084025671666,-27.7521520965556));
#41187=CARTESIAN_POINT('Ctrl Pts',(6.69621496749303,-0.991188872691557,
-27.7441124476238));
#41188=CARTESIAN_POINT('Ctrl Pts',(6.717034644702,-0.820813366041932,-27.7360727986921));
#41189=CARTESIAN_POINT('Ctrl Pts',(6.73786067218061,-0.650385892668927,
-27.7280306975639));
#41190=CARTESIAN_POINT('Ctrl Pts',(6.75218773871132,-0.479234227539398,
-27.7199885964358));
#41191=CARTESIAN_POINT('Ctrl Pts',(6.75999153019552,-0.307901789025053,
-27.7119464953076));
#41192=CARTESIAN_POINT('Ctrl Pts',(6.7680586689821,-0.130787553856494,-27.7036330048628));
#41193=CARTESIAN_POINT('Ctrl Pts',(6.76915453951254,0.0465194324935302,
-27.6953195144181));
#41194=CARTESIAN_POINT('Ctrl Pts',(6.76331073914564,0.223420781838351,-27.6870060239733));
#41195=CARTESIAN_POINT('Ctrl Pts',(6.75764774798627,0.394848742159236,-27.6789497558026));
#41196=CARTESIAN_POINT('Ctrl Pts',(6.74546822191276,0.565895430864003,-27.6708934876318));
#41197=CARTESIAN_POINT('Ctrl Pts',(6.72685349619744,0.736023804435914,-27.662837219461));
#41198=CARTESIAN_POINT('Ctrl Pts',(6.70734726799422,0.914300021313188,-27.6543951178793));
#41199=CARTESIAN_POINT('Ctrl Pts',(6.68077436121496,1.09156731859551,-27.6459530162975));
#41200=CARTESIAN_POINT('Ctrl Pts',(6.64728777912249,1.26722301964917,-27.6375109147158));
#41201=CARTESIAN_POINT('Ctrl Pts',(6.61380119703002,1.44287872070286,-27.629068813134));
#41202=CARTESIAN_POINT('Ctrl Pts',(6.57340112806252,1.6169223961403,-27.6206267115523));
#41203=CARTESIAN_POINT('Ctrl Pts',(6.52629897085658,1.78877353038229,-27.6121846099705));
#41204=CARTESIAN_POINT('Ctrl Pts',(6.47979489459287,1.95844258010019,-27.6038497022068));
#41205=CARTESIAN_POINT('Ctrl Pts',(6.42661064491424,2.12651407104573,-27.5955147944431));
#41206=CARTESIAN_POINT('Ctrl Pts',(6.3668709788531,2.29243166498767,-27.5871798866793));
#41207=CARTESIAN_POINT('Ctrl Pts',(6.30720301190912,2.45815012582775,-27.5788549824119));
#41208=CARTESIAN_POINT('Ctrl Pts',(6.24099541972999,2.62171951501863,-27.5705300781445));
#41209=CARTESIAN_POINT('Ctrl Pts',(6.16842336475276,2.78259630438413,-27.5622051738771));
#41210=CARTESIAN_POINT('Ctrl Pts',(6.09592510257987,2.94330951081894,-27.5538887345488));
#41211=CARTESIAN_POINT('Ctrl Pts',(6.01707541419289,3.10133525735415,-27.5455722952206));
#41212=CARTESIAN_POINT('Ctrl Pts',(5.9320984733461,3.25614752468694,-27.5372558558923));
#41213=CARTESIAN_POINT('Ctrl Pts',(5.84720606510457,3.41080578924965,-27.5289476895176));
#41214=CARTESIAN_POINT('Ctrl Pts',(5.75619872405018,3.56225664467217,-27.5206395231429));
#41215=CARTESIAN_POINT('Ctrl Pts',(5.65934766262805,3.7099963656999,-27.5123313567682));
#41216=CARTESIAN_POINT('Ctrl Pts',(5.56255213255724,3.85765137742003,-27.5040279540347));
#41217=CARTESIAN_POINT('Ctrl Pts',(5.45991974729519,4.00159920387351,-27.4957245513012));
#41218=CARTESIAN_POINT('Ctrl Pts',(5.3517666754693,4.14136239072799,-27.4874211485676));
#41219=CARTESIAN_POINT('Ctrl Pts',(5.24365765656705,4.28106864922257,-27.4791211279772));
#41220=CARTESIAN_POINT('Ctrl Pts',(5.13003264432549,4.41659338990774,-27.4708211073868));
#41221=CARTESIAN_POINT('Ctrl Pts',(5.01125010095246,4.54748957400717,-27.4625210867964));
#41222=CARTESIAN_POINT('Ctrl Pts',(4.8924962210701,4.67835417146564,-27.4542230690892));
#41223=CARTESIAN_POINT('Ctrl Pts',(4.76858752439499,4.80459218139696,-27.445925051382));
#41224=CARTESIAN_POINT('Ctrl Pts',(4.63992171489285,4.92579084814467,-27.4376270336748));
#41225=CARTESIAN_POINT('Ctrl Pts',(4.51123961457061,5.0470048602719,-27.4293279653271));
#41226=CARTESIAN_POINT('Ctrl Pts',(4.37779944747247,5.16317801195076,-27.4210288969794));
#41227=CARTESIAN_POINT('Ctrl Pts',(4.24003501347875,5.27393516119361,-27.4127298286317));
#41228=CARTESIAN_POINT('Ctrl Pts',(4.10226297319145,5.38469842559528,-27.4044303020732));
#41229=CARTESIAN_POINT('Ctrl Pts',(3.96016646425015,5.4900448773709,-27.3961307755147));
#41230=CARTESIAN_POINT('Ctrl Pts',(3.81421135182252,5.58964048608032,-27.3878312489562));
#41231=CARTESIAN_POINT('Ctrl Pts',(3.66818024325294,5.68928795239097,-27.3795274009869));
#41232=CARTESIAN_POINT('Ctrl Pts',(3.51828680711016,5.78317840071868,-27.3712235530176));
#41233=CARTESIAN_POINT('Ctrl Pts',(3.36502537900307,5.87102147830045,-27.3629197050483));
#41234=CARTESIAN_POINT('Ctrl Pts',(3.27744614500196,5.92121825345732,-27.3581745799806));
#41235=CARTESIAN_POINT('Ctrl Pts',(3.18876761150909,5.96944114562792,-27.353429454913));
#41236=CARTESIAN_POINT('Ctrl Pts',(3.09908550384723,6.01564277861011,-27.3486843298453));
#41237=CARTESIAN_POINT('Origin',(0.,0.,-63.6971797838103));
#41238=CARTESIAN_POINT('',(3.09908550384718,6.01564277861014,-24.9542890874699));
#41239=CARTESIAN_POINT('',(3.0990855038472,6.01564277861013,-25.348603209574));
#41240=CARTESIAN_POINT('',(3.09908550384721,6.01564277861012,-63.6971797838103));
#41241=CARTESIAN_POINT('',(-6.76699450066406,0.0086271653731468,-26.302820216166));
#41242=CARTESIAN_POINT('Ctrl Pts',(-6.76699450066406,0.00862716537319188,
-26.302820216166));
#41243=CARTESIAN_POINT('Ctrl Pts',(-6.76720929633067,-0.159854720834625,
-26.2948897094655));
#41244=CARTESIAN_POINT('Ctrl Pts',(-6.76112789536669,-0.328586091746019,
-26.286959202765));
#41245=CARTESIAN_POINT('Ctrl Pts',(-6.74872146581008,-0.497038808257709,
-26.2790286960646));
#41246=CARTESIAN_POINT('Ctrl Pts',(-6.73632507264396,-0.665355252102513,
-26.2711046048812));
#41247=CARTESIAN_POINT('Ctrl Pts',(-6.71761385734345,-0.833393109637448,
-26.263180513698));
#41248=CARTESIAN_POINT('Ctrl Pts',(-6.69261103071651,-1.00062310163805,
-26.2552564225147));
#41249=CARTESIAN_POINT('Ctrl Pts',(-6.66762271089184,-1.16775606571198,
-26.2473369289405));
#41250=CARTESIAN_POINT('Ctrl Pts',(-6.63635009950524,-1.33408171855351,
-26.2394174353663));
#41251=CARTESIAN_POINT('Ctrl Pts',(-6.59886831744837,-1.49907502446546,
-26.2314979417921));
#41252=CARTESIAN_POINT('Ctrl Pts',(-6.56139431247054,-1.66403409598644,
-26.2235800914303));
#41253=CARTESIAN_POINT('Ctrl Pts',(-6.51771377670204,-1.82766099490035,
-26.2156622410685));
#41254=CARTESIAN_POINT('Ctrl Pts',(-6.46795309912641,-1.98944004873259,
-26.2077443907067));
#41255=CARTESIAN_POINT('Ctrl Pts',(-6.41819600781018,-2.15120744312447,
-26.1998271109856));
#41256=CARTESIAN_POINT('Ctrl Pts',(-6.36235975821465,-2.31112689000894,
-26.1919098312644));
#41257=CARTESIAN_POINT('Ctrl Pts',(-6.30062074567853,-2.4686974742008,-26.1839925515432));
#41258=CARTESIAN_POINT('Ctrl Pts',(-6.23887342452758,-2.62628926367661,
-26.176074206343));
#41259=CARTESIAN_POINT('Ctrl Pts',(-6.17122190041459,-2.7815312041177,-26.1681558611427));
#41260=CARTESIAN_POINT('Ctrl Pts',(-6.09789076943403,-2.93394225642756,
-26.1602375159425));
#41261=CARTESIAN_POINT('Ctrl Pts',(-6.02453460447058,-3.08640533924105,
-26.1523164675558));
#41262=CARTESIAN_POINT('Ctrl Pts',(-5.94549514263107,-3.23603526611232,
-26.1443954191691));
#41263=CARTESIAN_POINT('Ctrl Pts',(-5.86104283849494,-3.38237576938565,
-26.1364743707824));
#41264=CARTESIAN_POINT('Ctrl Pts',(-5.77649437220515,-3.52888290420454,
-26.1285443030435));
#41265=CARTESIAN_POINT('Ctrl Pts',(-5.68652095174598,-3.67209280581836,
-26.1206142353046));
#41266=CARTESIAN_POINT('Ctrl Pts',(-5.59143660638892,-3.81157784608081,
-26.1126841675658));
#41267=CARTESIAN_POINT('Ctrl Pts',(-5.49629311215779,-3.95114965544335,
-26.1047491667901));
#41268=CARTESIAN_POINT('Ctrl Pts',(-5.39603259352157,-4.08699168530267,
-26.0968141660144));
#41269=CARTESIAN_POINT('Ctrl Pts',(-5.29100870928579,-4.21871021027303,
-26.0888791652387));
#41270=CARTESIAN_POINT('Ctrl Pts',(-5.18582476707317,-4.35062947625361,
-26.0809320714026));
#41271=CARTESIAN_POINT('Ctrl Pts',(-5.07586321740119,-4.47841240388381,
-26.0729849775666));
#41272=CARTESIAN_POINT('Ctrl Pts',(-4.961514367973,-4.60170231288352,-26.0650378837305));
#41273=CARTESIAN_POINT('Ctrl Pts',(-4.88929343112213,-4.67957028249356,
-26.0600186241145));
#41274=CARTESIAN_POINT('Ctrl Pts',(-4.81532309359165,-4.75564678488783,
-26.0549993644984));
#41275=CARTESIAN_POINT('Ctrl Pts',(-4.73970804784808,-4.82985057958983,
-26.0499801048823));
#41276=CARTESIAN_POINT('Ctrl Pts',(-4.61415887433898,-4.95305655010088,
-26.0416462621896));
#41277=CARTESIAN_POINT('Ctrl Pts',(-4.48364207027366,-5.07152169441127,
-26.0333124194969));
#41278=CARTESIAN_POINT('Ctrl Pts',(-4.34854524625484,-5.18482817856816,
-26.0249785768042));
#41279=CARTESIAN_POINT('Ctrl Pts',(-4.21360765093424,-5.29800111669907,
-26.0166545565995));
#41280=CARTESIAN_POINT('Ctrl Pts',(-4.07410105347681,-5.40602728522836,
-26.0083305363947));
#41281=CARTESIAN_POINT('Ctrl Pts',(-3.93045018640649,-5.50852524113099,
-26.0000065161899));
#41282=CARTESIAN_POINT('Ctrl Pts',(-3.78694229187903,-5.61092118307651,
-25.9916907806991));
#41283=CARTESIAN_POINT('Ctrl Pts',(-3.63929862691486,-5.70779967364826,
-25.9833750452082));
#41284=CARTESIAN_POINT('Ctrl Pts',(-3.48797748408892,-5.79881902377448,
-25.9750593097174));
#41285=CARTESIAN_POINT('Ctrl Pts',(-3.33677922192115,-5.88976446144245,
-25.9667503270373));
#41286=CARTESIAN_POINT('Ctrl Pts',(-3.1819097291763,-5.97486006077029,-25.9584413443573));
#41287=CARTESIAN_POINT('Ctrl Pts',(-3.02385699088013,-6.0538068930802,-25.9501323616772));
#41288=CARTESIAN_POINT('Ctrl Pts',(-2.8659036562055,-6.13270407360221,-25.9418286047401));
#41289=CARTESIAN_POINT('Ctrl Pts',(-2.70477137611208,-6.20546003888148,
-25.9335248478029));
#41290=CARTESIAN_POINT('Ctrl Pts',(-2.54097369058976,-6.27182124296688,
-25.9252210908657));
#41291=CARTESIAN_POINT('Ctrl Pts',(-2.37724250297927,-6.33815550600313,
-25.9169207050537));
#41292=CARTESIAN_POINT('Ctrl Pts',(-2.21084838794507,-6.39810005041631,
-25.9086203192417));
#41293=CARTESIAN_POINT('Ctrl Pts',(-2.04232613575009,-6.45144890355896,
-25.9003199334296));
#41294=CARTESIAN_POINT('Ctrl Pts',(-1.87383942051301,-6.50478650681666,
-25.892021297953));
#41295=CARTESIAN_POINT('Ctrl Pts',(-1.70322579355409,-6.55153108482973,
-25.8837226624764));
#41296=CARTESIAN_POINT('Ctrl Pts',(-1.53103675948158,-6.59152603280273,
-25.8754240269997));
#41297=CARTESIAN_POINT('Ctrl Pts',(-1.35885545419271,-6.63151918558419,
-25.8671257640111));
#41298=CARTESIAN_POINT('Ctrl Pts',(-1.18509922149033,-6.66476323353771,
-25.8588275010225));
#41299=CARTESIAN_POINT('Ctrl Pts',(-1.01033154485271,-6.69115230505744,
-25.8505292380339));
#41300=CARTESIAN_POINT('Ctrl Pts',(-0.83554270459548,-6.71754457218109,
-25.8422299701611));
#41301=CARTESIAN_POINT('Ctrl Pts',(-0.659742520299974,-6.73708015745405,
-25.8339307022883));
#41302=CARTESIAN_POINT('Ctrl Pts',(-0.483501608820698,-6.74970482275098,
-25.8256314344155));
#41303=CARTESIAN_POINT('Ctrl Pts',(-0.307136947815695,-6.76233835259774,
-25.817326339119));
#41304=CARTESIAN_POINT('Ctrl Pts',(-0.130331288586724,-6.76805124128259,
-25.8090212438225));
#41305=CARTESIAN_POINT('Ctrl Pts',(0.0463418149108182,-6.76684131897526,
-25.800716148526));
#41306=CARTESIAN_POINT('Ctrl Pts',(0.223079342608453,-6.76563095546734,
-25.7924080247599));
#41307=CARTESIAN_POINT('Ctrl Pts',(0.399683870559923,-6.75749275923777,
-25.7840999009938));
#41308=CARTESIAN_POINT('Ctrl Pts',(0.575584705443573,-6.74247664043855,
-25.7757917772277));
#41309=CARTESIAN_POINT('Ctrl Pts',(0.751672521898899,-6.72744455959176,
-25.767474821974));
#41310=CARTESIAN_POINT('Ctrl Pts',(0.927054804690868,-6.70551998554797,
-25.7591578667203));
#41311=CARTESIAN_POINT('Ctrl Pts',(1.10116772692618,-6.67680452291186,-25.7508409114667));
#41312=CARTESIAN_POINT('Ctrl Pts',(1.22948630154825,-6.65564166384445,-25.7447114419842));
#41313=CARTESIAN_POINT('Ctrl Pts',(1.35711558514734,-6.6307914351338,-25.7385819725017));
#41314=CARTESIAN_POINT('Ctrl Pts',(1.48383452984843,-6.60231202595193,-25.7324525030192));
#41315=CARTESIAN_POINT('Ctrl Pts',(1.65854863615358,-6.56304595934251,-25.724001479494));
#41316=CARTESIAN_POINT('Ctrl Pts',(1.83185098681095,-6.51680737513996,-25.7155504559688));
#41317=CARTESIAN_POINT('Ctrl Pts',(2.00316545741816,-6.46371542924089,-25.7070994324436));
#41318=CARTESIAN_POINT('Ctrl Pts',(2.17432909072547,-6.41067022922229,-25.6986558497935));
#41319=CARTESIAN_POINT('Ctrl Pts',(2.34350801744213,-6.35078379244406,-25.6902122671433));
#41320=CARTESIAN_POINT('Ctrl Pts',(2.51013829310537,-6.28422586716026,-25.6817686844932));
#41321=CARTESIAN_POINT('Ctrl Pts',(2.67664450733739,-6.21771749632529,-25.6733313883534));
#41322=CARTESIAN_POINT('Ctrl Pts',(2.84060554636083,-6.1445476612844,-25.6648940922135));
#41323=CARTESIAN_POINT('Ctrl Pts',(3.00147419709432,-6.0649354196213,-25.6564567960737));
#41324=CARTESIAN_POINT('Ctrl Pts',(3.16222808031167,-5.98537997522224,-25.6480255193014));
#41325=CARTESIAN_POINT('Ctrl Pts',(3.31989367946601,-5.89939143869697,-25.639594242529));
#41326=CARTESIAN_POINT('Ctrl Pts',(3.47394509046804,-5.80723639164216,-25.6311629657566));
#41327=CARTESIAN_POINT('Ctrl Pts',(3.62793046945956,-5.71512084557599,-25.6227353029346));
#41328=CARTESIAN_POINT('Ctrl Pts',(3.77830446469358,-5.61684422815872,-25.6143076401127));
#41329=CARTESIAN_POINT('Ctrl Pts',(3.92456647714537,-5.51271865475346,-25.6058799772907));
#41330=CARTESIAN_POINT('Ctrl Pts',(4.07078346436403,-5.40862513531859,-25.5974549088367));
#41331=CARTESIAN_POINT('Ctrl Pts',(4.21289072346152,-5.29868644265154,-25.5890298403827));
#41332=CARTESIAN_POINT('Ctrl Pts',(4.35041701292123,-5.1832577413906,-25.5806047719287));
#41333=CARTESIAN_POINT('Ctrl Pts',(4.38804841528869,-5.15167291554407,-25.578299415315));
#41334=CARTESIAN_POINT('Ctrl Pts',(4.42533700352259,-5.11967727355014,-25.5759940587013));
#41335=CARTESIAN_POINT('Ctrl Pts',(4.46227354144736,-5.08727862823522,-25.5736887020876));
#41336=CARTESIAN_POINT('Ctrl Pts',(4.60036740276721,-4.96615049104538,-25.5650697135631));
#41337=CARTESIAN_POINT('Ctrl Pts',(4.73347610402824,-4.83944037359167,-25.5564507250387));
#41338=CARTESIAN_POINT('Ctrl Pts',(4.86116512889644,-4.70758564336341,-25.5478317365142));
#41339=CARTESIAN_POINT('Ctrl Pts',(4.98893065088635,-4.57565192038416,-25.5392075844464));
#41340=CARTESIAN_POINT('Ctrl Pts',(5.11126980513273,-4.43856765222686,-25.5305834323786));
#41341=CARTESIAN_POINT('Ctrl Pts',(5.22778679387279,-4.29680511983139,-25.5219592803108));
#41342=CARTESIAN_POINT('Ctrl Pts',(5.34829452082279,-4.15018718256418,-25.5130397487146));
#41343=CARTESIAN_POINT('Ctrl Pts',(5.46257397868827,-3.99856512529576,-25.5041202171183));
#41344=CARTESIAN_POINT('Ctrl Pts',(5.57023482799024,-3.84249566831826,-25.4952006855221));
#41345=CARTESIAN_POINT('Ctrl Pts',(5.67452429463413,-3.69131350197723,-25.4865604676629));
#41346=CARTESIAN_POINT('Ctrl Pts',(5.77260327723682,-3.53595854214474,-25.4779202498036));
#41347=CARTESIAN_POINT('Ctrl Pts',(5.86416265558127,-3.37696392472381,-25.4692800319443));
#41348=CARTESIAN_POINT('Ctrl Pts',(5.9601618164407,-3.21025953977097,-25.4602208434796));
#41349=CARTESIAN_POINT('Ctrl Pts',(6.04899319374431,-3.03955408641109,-25.4511616550149));
#41350=CARTESIAN_POINT('Ctrl Pts',(6.1303559622308,-2.86548857550354,-25.4421024665503));
#41351=CARTESIAN_POINT('Ctrl Pts',(6.21171873071729,-2.691423064596,-25.4330432780856));
#41352=CARTESIAN_POINT('Ctrl Pts',(6.28561277385952,-2.51399786209427,-25.4239840896209));
#41353=CARTESIAN_POINT('Ctrl Pts',(6.35179603764721,-2.33387576707272,-25.4149249011562));
#41354=CARTESIAN_POINT('Ctrl Pts',(6.41786464357386,-2.15406572094324,-25.4058814070999));
#41355=CARTESIAN_POINT('Ctrl Pts',(6.47631082476443,-1.97140276102581,-25.3968379130436));
#41356=CARTESIAN_POINT('Ctrl Pts',(6.5269156678898,-1.78652200217481,-25.3877944189874));
#41357=CARTESIAN_POINT('Ctrl Pts',(6.5774742229503,-1.60181035307754,-25.378759196982));
#41358=CARTESIAN_POINT('Ctrl Pts',(6.62020569695263,-1.41488518462245,-25.3697239749767));
#41359=CARTESIAN_POINT('Ctrl Pts',(6.65494108045985,-1.22639643492954,-25.3606887529713));
#41360=CARTESIAN_POINT('Ctrl Pts',(6.68961526778301,-1.03823976138075,-25.3516694490602));
#41361=CARTESIAN_POINT('Ctrl Pts',(6.71632145224507,-0.8485252412071,-25.3426501451492));
#41362=CARTESIAN_POINT('Ctrl Pts',(6.73494173339735,-0.65791249246595,-25.3336308412381));
#41363=CARTESIAN_POINT('Ctrl Pts',(6.75353865410628,-0.467538880732505,
-25.3246228526737));
#41364=CARTESIAN_POINT('Ctrl Pts',(6.76406989302338,-0.276269525572618,
-25.3156148641094));
#41365=CARTESIAN_POINT('Ctrl Pts',(6.76646900867999,-0.0847711895236639,
-25.3066068755451));
#41366=CARTESIAN_POINT('Ctrl Pts',(6.76886270584986,0.106294640826465,-25.2976192318384));
#41367=CARTESIAN_POINT('Ctrl Pts',(6.76316093836758,0.297588182134574,-25.2886315881317));
#41368=CARTESIAN_POINT('Ctrl Pts',(6.74934917479396,0.488441108741004,-25.2796439444251));
#41369=CARTESIAN_POINT('Ctrl Pts',(6.73732008601697,0.654660779766946,-25.2718163296916));
#41370=CARTESIAN_POINT('Ctrl Pts',(6.71914017042194,0.820546046547857,-25.2639887149582));
#41371=CARTESIAN_POINT('Ctrl Pts',(6.6948320114491,0.985653761965331,-25.2561611002248));
#41372=CARTESIAN_POINT('Ctrl Pts',(6.66960606030373,1.15699537477519,-25.2480379417795));
#41373=CARTESIAN_POINT('Ctrl Pts',(6.63778998791161,1.32742277749532,-25.2399147833342));
#41374=CARTESIAN_POINT('Ctrl Pts',(6.59947744861363,1.49639112709215,-25.2317916248889));
#41375=CARTESIAN_POINT('Ctrl Pts',(6.56116761055032,1.66534756353546,-25.2236690391688));
#41376=CARTESIAN_POINT('Ctrl Pts',(6.51636229888125,1.83284479480095,-25.2155464534487));
#41377=CARTESIAN_POINT('Ctrl Pts',(6.46520607973286,1.99834915532427,-25.2074238677286));
#41378=CARTESIAN_POINT('Ctrl Pts',(6.4140437136376,2.16387340290199,-25.1993003059961));
#41379=CARTESIAN_POINT('Ctrl Pts',(6.35652902973073,2.32740395356957,-25.1911767442637));
#41380=CARTESIAN_POINT('Ctrl Pts',(6.2928561433664,2.48842330781878,-25.1830531825312));
#41381=CARTESIAN_POINT('Ctrl Pts',(6.2291368788607,2.64955994555867,-25.1749237037481));
#41382=CARTESIAN_POINT('Ctrl Pts',(6.15925058787047,2.80818139294527,-25.1667942249649));
#41383=CARTESIAN_POINT('Ctrl Pts',(6.08343938395315,2.96379052258551,-25.1586647461818));
#41384=CARTESIAN_POINT('Ctrl Pts',(6.0075972731426,3.11946309132851,-25.1505319531533));
#41385=CARTESIAN_POINT('Ctrl Pts',(5.92582560733681,3.27212057199723,-25.1423991601248));
#41386=CARTESIAN_POINT('Ctrl Pts',(5.83841183260115,3.42129160887273,-25.1342663670963));
#41387=CARTESIAN_POINT('Ctrl Pts',(5.75090300864663,3.57062484662074,-25.1261247308891));
#41388=CARTESIAN_POINT('Ctrl Pts',(5.65774001914182,3.71646376070708,-25.117983094682));
#41389=CARTESIAN_POINT('Ctrl Pts',(5.55925330217142,3.85836645775076,-25.1098414584748));
#41390=CARTESIAN_POINT('Ctrl Pts',(5.50907565760953,3.93066395444538,-25.1056934054142));
#41391=CARTESIAN_POINT('Ctrl Pts',(5.45751675200637,4.00194022615733,-25.1015453523537));
#41392=CARTESIAN_POINT('Ctrl Pts',(5.40462417928148,4.07214028254504,-25.0973972992931));
#41393=CARTESIAN_POINT('Ctrl Pts',(5.2969909396395,4.21499322205623,-25.0889562580256));
#41394=CARTESIAN_POINT('Ctrl Pts',(5.18361096006823,4.35368172516,-25.0805152167581));
#41395=CARTESIAN_POINT('Ctrl Pts',(5.06483308104717,4.4877338224465,-25.0720741754906));
#41396=CARTESIAN_POINT('Ctrl Pts',(4.94614309501864,4.62168672415816,-25.0636393804061));
#41397=CARTESIAN_POINT('Ctrl Pts',(4.82206339181756,4.75100981004534,-25.0552045853217));
#41398=CARTESIAN_POINT('Ctrl Pts',(4.69298359101839,4.87526348153945,-25.0467697902372));
#41399=CARTESIAN_POINT('Ctrl Pts',(4.56399276583258,4.99943150410502,-25.0383408093163));
#41400=CARTESIAN_POINT('Ctrl Pts',(4.43000895672942,5.11853685095818,-25.0299118283954));
#41401=CARTESIAN_POINT('Ctrl Pts',(4.29145934431418,5.23217600010727,-25.0214828474744));
#41402=CARTESIAN_POINT('Ctrl Pts',(4.15296797633668,5.34576737685027,-25.0130574099864));
#41403=CARTESIAN_POINT('Ctrl Pts',(4.00991488863878,5.45389692561738,-25.0046319724983));
#41404=CARTESIAN_POINT('Ctrl Pts',(3.86276155936935,5.55620033255268,-24.9962065350103));
#41405=CARTESIAN_POINT('Ctrl Pts',(3.71564479254461,5.65847832067702,-24.9877831909481));
#41406=CARTESIAN_POINT('Ctrl Pts',(3.56443008805123,5.75493286188631,-24.979359846886));
#41407=CARTESIAN_POINT('Ctrl Pts',(3.40960956477191,5.84524179275896,-24.9709365028239));
#41408=CARTESIAN_POINT('Ctrl Pts',(3.30761675616245,5.90473559440178,-24.9653873643726));
#41409=CARTESIAN_POINT('Ctrl Pts',(3.20405967863177,5.96156311408783,-24.9598382259212));
#41410=CARTESIAN_POINT('Ctrl Pts',(3.09908550384718,6.01564277861014,-24.9542890874699));
#41411=CARTESIAN_POINT('Ctrl Pts',(3.09908550384719,6.01564277861013,-26.9540130953596));
#41412=CARTESIAN_POINT('Ctrl Pts',(2.94369358937914,6.09569620719059,-26.9457888539227));
#41413=CARTESIAN_POINT('Ctrl Pts',(2.78504743618393,6.16980231941268,-26.9375646124858));
#41414=CARTESIAN_POINT('Ctrl Pts',(2.62364130021567,6.23769150630284,-26.9293403710488));
#41415=CARTESIAN_POINT('Ctrl Pts',(2.46237917532573,6.3055201205577,-26.9211234675106));
#41416=CARTESIAN_POINT('Ctrl Pts',(2.29836230241852,6.36714272762714,-26.9129065639724));
#41417=CARTESIAN_POINT('Ctrl Pts',(2.13210812002705,6.42233633224816,-26.9046896604342));
#41418=CARTESIAN_POINT('Ctrl Pts',(1.96594004975562,6.47750134908727,-26.896477012879));
#41419=CARTESIAN_POINT('Ctrl Pts',(1.79753731470756,6.52624388348932,-26.8882643653239));
#41420=CARTESIAN_POINT('Ctrl Pts',(1.62743624522011,6.56838947290307,-26.8800517177687));
#41421=CARTESIAN_POINT('Ctrl Pts',(1.45739277347126,6.61052079144451,-26.8718418510892));
#41422=CARTESIAN_POINT('Ctrl Pts',(1.285652457804,6.64605952932386,-26.8636319844097));
#41423=CARTESIAN_POINT('Ctrl Pts',(1.11276575848564,6.67488137473183,-26.8554221177303));
#41424=CARTESIAN_POINT('Ctrl Pts',(1.03117841971235,6.68848275456407,-26.8515477816668));
#41425=CARTESIAN_POINT('Ctrl Pts',(0.949335959981298,6.70058900574323,-26.8476734456033));
#41426=CARTESIAN_POINT('Ctrl Pts',(0.867297029201273,6.71119101673754,-26.8437991095399));
#41427=CARTESIAN_POINT('Ctrl Pts',(0.679713995189303,6.7354326465349,-26.8349403920181));
#41428=CARTESIAN_POINT('Ctrl Pts',(0.49129776790984,6.7517816425708,-26.8260816744964));
#41429=CARTESIAN_POINT('Ctrl Pts',(0.302701553623098,6.76022638448108,-26.8172229569746));
#41430=CARTESIAN_POINT('Ctrl Pts',(0.11375250610948,6.76868692514719,-26.8083476662152));
#41431=CARTESIAN_POINT('Ctrl Pts',(-0.0753769422491641,6.76921364809673,
-26.7994723754557));
#41432=CARTESIAN_POINT('Ctrl Pts',(-0.264034911035329,6.76184697887749,
-26.7905970846963));
#41433=CARTESIAN_POINT('Ctrl Pts',(-0.453228710871385,6.75445938666131,
-26.7816965861155));
#41434=CARTESIAN_POINT('Ctrl Pts',(-0.641948090647254,6.7391335492757,-26.7727960875347));
#41435=CARTESIAN_POINT('Ctrl Pts',(-0.829544526971442,6.71596194731416,
-26.763895588954));
#41436=CARTESIAN_POINT('Ctrl Pts',(-1.01739491284253,6.69275897792402,-26.7549830417564));
#41437=CARTESIAN_POINT('Ctrl Pts',(-1.20411906216787,6.66168906653027,-26.7460704945588));
#41438=CARTESIAN_POINT('Ctrl Pts',(-1.38907857905345,6.62289586972458,-26.7371579473612));
#41439=CARTESIAN_POINT('Ctrl Pts',(-1.57444650461624,6.58401701375163,-26.7282257203889));
#41440=CARTESIAN_POINT('Ctrl Pts',(-1.75804174927372,6.53738081546298,-26.7192934934167));
#41441=CARTESIAN_POINT('Ctrl Pts',(-1.93923823651591,6.4831816311156,-26.7103612664444));
#41442=CARTESIAN_POINT('Ctrl Pts',(-2.11048984077922,6.43195714321012,-26.7019192804991));
#41443=CARTESIAN_POINT('Ctrl Pts',(-2.27959874031394,6.37397755117248,-26.6934772945537));
#41444=CARTESIAN_POINT('Ctrl Pts',(-2.44605286443069,6.30944644041064,-26.6850353086084));
#41445=CARTESIAN_POINT('Ctrl Pts',(-2.60820836519787,6.24658182449214,-26.6768113341908));
#41446=CARTESIAN_POINT('Ctrl Pts',(-2.7681538183743,6.1773786482961,-26.6685873597733));
#41447=CARTESIAN_POINT('Ctrl Pts',(-2.92535923206763,6.10201297633467,-26.6603633853557));
#41448=CARTESIAN_POINT('Ctrl Pts',(-3.08239862159142,6.02672689783511,-26.652148096253));
#41449=CARTESIAN_POINT('Ctrl Pts',(-3.23670341337504,5.94529143730795,-26.6439328071504));
#41450=CARTESIAN_POINT('Ctrl Pts',(-3.38776137584139,5.85793153428386,-26.6357175180477));
#41451=CARTESIAN_POINT('Ctrl Pts',(-3.53869010545076,5.77064636925881,-26.6275092572755));
#41452=CARTESIAN_POINT('Ctrl Pts',(-3.686377229187,5.67744703461661,-26.6193009965034));
#41453=CARTESIAN_POINT('Ctrl Pts',(-3.83033293459859,5.57860543596062,-26.6110927357312));
#41454=CARTESIAN_POINT('Ctrl Pts',(-3.97419434948814,5.47982857823247,-26.6028898513433));
#41455=CARTESIAN_POINT('Ctrl Pts',(-4.11432891981485,5.37541702011825,-26.5946869669554));
#41456=CARTESIAN_POINT('Ctrl Pts',(-4.25027370070327,5.26568727414666,-26.5864840825675));
#41457=CARTESIAN_POINT('Ctrl Pts',(-4.38615669248902,5.15600740212019,-26.5782849265233));
#41458=CARTESIAN_POINT('Ctrl Pts',(-4.51785341029003,5.04101438269913,-26.5700857704791));
#41459=CARTESIAN_POINT('Ctrl Pts',(-4.6449319713574,4.92106654918035,-26.5618866144349));
#41460=CARTESIAN_POINT('Ctrl Pts',(-4.77199947968023,4.80112914820623,-26.5536881715179));
#41461=CARTESIAN_POINT('Ctrl Pts',(-4.89444936489766,4.67623803127121,-26.5454897286009));
#41462=CARTESIAN_POINT('Ctrl Pts',(-5.0118845100908,4.54679036876696,-26.5372912856839));
#41463=CARTESIAN_POINT('Ctrl Pts',(-5.12931848576894,4.41734399540814,-26.5290929244137));
#41464=CARTESIAN_POINT('Ctrl Pts',(-5.24173757910049,4.28334143181827,-26.5208945631435));
#41465=CARTESIAN_POINT('Ctrl Pts',(-5.34878318189772,4.14521500926648,-26.5126962018732));
#41466=CARTESIAN_POINT('Ctrl Pts',(-5.45584716424772,4.00706487063664,-26.504496432958));
#41467=CARTESIAN_POINT('Ctrl Pts',(-5.55753559820403,3.86478974591198,-26.4962966640427));
#41468=CARTESIAN_POINT('Ctrl Pts',(-5.65353161629358,3.7188532188793,-26.4880968951274));
#41469=CARTESIAN_POINT('Ctrl Pts',(-5.74956155528621,3.57286512409529,-26.4798942287631));
#41470=CARTESIAN_POINT('Ctrl Pts',(-5.83989487455199,3.42321334925615,-26.4716915623988));
#41471=CARTESIAN_POINT('Ctrl Pts',(-5.92425927289701,3.27038851934963,-26.4634888960346));
#41472=CARTESIAN_POINT('Ctrl Pts',(-6.00871948811169,3.11739011863485,-26.4552769134915));
#41473=CARTESIAN_POINT('Ctrl Pts',(-6.0871970653548,2.96121177751405,-26.4470649309485));
#41474=CARTESIAN_POINT('Ctrl Pts',(-6.15946626873234,2.80236762119971,-26.4388529484055));
#41475=CARTESIAN_POINT('Ctrl Pts',(-6.23177809746274,2.64342977645521,-26.4306361223242));
#41476=CARTESIAN_POINT('Ctrl Pts',(-6.29787411752868,2.48182331374087,-26.4224192962429));
#41477=CARTESIAN_POINT('Ctrl Pts',(-6.35757766402478,2.31808007754117,-26.4142024701616));
#41478=CARTESIAN_POINT('Ctrl Pts',(-6.41737328201233,2.15408432562242,-26.4059729725477));
#41479=CARTESIAN_POINT('Ctrl Pts',(-6.47075661670434,1.98794555644227,-26.3977434749339));
#41480=CARTESIAN_POINT('Ctrl Pts',(-6.51760121400132,1.82020971738107,-26.38951397732));
#41481=CARTESIAN_POINT('Ctrl Pts',(-6.55935649204513,1.6706971374456,-26.3821785537951));
#41482=CARTESIAN_POINT('Ctrl Pts',(-6.59591731160973,1.51991598575371,-26.3748431302702));
#41483=CARTESIAN_POINT('Ctrl Pts',(-6.62722876856031,1.36825723062829,-26.3675077067453));
#41484=CARTESIAN_POINT('Ctrl Pts',(-6.67579691731258,1.13301474446292,-26.3561295092542));
#41485=CARTESIAN_POINT('Ctrl Pts',(-6.71187188657008,0.895012061568704,
-26.3447513117631));
#41486=CARTESIAN_POINT('Ctrl Pts',(-6.73519158237264,0.655349791131986,
-26.333373114272));
#41487=CARTESIAN_POINT('Ctrl Pts',(-6.7560643755579,0.440834942932958,-26.3231888149113));
#41488=CARTESIAN_POINT('Ctrl Pts',(-6.76671866160522,0.22499038588721,-26.3130045155506));
#41489=CARTESIAN_POINT('Ctrl Pts',(-6.76699450066341,0.00862716588261877,
-26.30282021619));
#41490=CARTESIAN_POINT('',(-6.767,2.46159836221269E-13,-26.6971797838101));
#41491=CARTESIAN_POINT('Ctrl Pts',(3.09908550384723,6.01564277861011,-27.3486843298453));
#41492=CARTESIAN_POINT('Ctrl Pts',(2.94202003450173,6.09655837435233,-27.3403739174868));
#41493=CARTESIAN_POINT('Ctrl Pts',(2.78187539054827,6.17127148352116,-27.3320635051283));
#41494=CARTESIAN_POINT('Ctrl Pts',(2.61918139267093,6.23956551630692,-27.3237530927698));
#41495=CARTESIAN_POINT('Ctrl Pts',(2.45633190967738,6.30792481705439,-27.3154347382287));
#41496=CARTESIAN_POINT('Ctrl Pts',(2.29092853147358,6.36985266617452,-27.3071163836876));
#41497=CARTESIAN_POINT('Ctrl Pts',(2.12351817934484,6.4251816738511,-27.2987980291465));
#41498=CARTESIAN_POINT('Ctrl Pts',(2.09573825456533,6.43436292012312,-27.2974176888002));
#41499=CARTESIAN_POINT('Ctrl Pts',(2.06790309431458,6.44336257498331,-27.2960373484538));
#41500=CARTESIAN_POINT('Ctrl Pts',(2.04001522898076,6.45218000876654,-27.2946570081075));
#41501=CARTESIAN_POINT('Ctrl Pts',(1.86927400082929,6.50616404287139,-27.2862059845823));
#41502=CARTESIAN_POINT('Ctrl Pts',(1.69624418085032,6.5534122471801,-27.2777549610571));
#41503=CARTESIAN_POINT('Ctrl Pts',(1.52148359721141,6.59373768536606,-27.2693039375319));
#41504=CARTESIAN_POINT('Ctrl Pts',(1.34687688507213,6.63402761820227,-27.2608603548818));
#41505=CARTESIAN_POINT('Ctrl Pts',(1.17054276816465,6.66740685979813,-27.2524167722316));
#41506=CARTESIAN_POINT('Ctrl Pts',(0.993054007324512,6.69373832312982,-27.2439731895814));
#41507=CARTESIAN_POINT('Ctrl Pts',(0.815697392395926,6.72005018186677,-27.2355358934416));
#41508=CARTESIAN_POINT('Ctrl Pts',(0.637188174069064,6.73932467407811,-27.2270985973017));
#41509=CARTESIAN_POINT('Ctrl Pts',(0.458109467011628,6.75147574358631,-27.2186613011619));
#41510=CARTESIAN_POINT('Ctrl Pts',(0.27915851895759,6.76361814423289,-27.2102300243896));
#41511=CARTESIAN_POINT('Ctrl Pts',(0.0996392225044273,6.76864723672818,
-27.2017987476172));
#41512=CARTESIAN_POINT('Ctrl Pts',(-0.0798598080510627,6.76652875639039,
-27.1933674708448));
#41513=CARTESIAN_POINT('Ctrl Pts',(-0.259281898824211,6.76441118410996,
-27.1849398080229));
#41514=CARTESIAN_POINT('Ctrl Pts',(-0.438683410162749,6.75515215054191,
-27.176512145201));
#41515=CARTESIAN_POINT('Ctrl Pts',(-0.617474682917946,6.73876947342431,
-27.1680844823791));
#41516=CARTESIAN_POINT('Ctrl Pts',(-0.796210916648085,6.72239183954268,
-27.1596594139251));
#41517=CARTESIAN_POINT('Ctrl Pts',(-0.974336956710911,6.69889496560102,
-27.1512343454711));
#41518=CARTESIAN_POINT('Ctrl Pts',(-1.15126685130219,6.66834864393673,-27.1428092770171));
#41519=CARTESIAN_POINT('Ctrl Pts',(-1.19968028614615,6.65999023533069,-27.1405039204034));
#41520=CARTESIAN_POINT('Ctrl Pts',(-1.24800419538771,6.65110430743247,-27.1381985637898));
#41521=CARTESIAN_POINT('Ctrl Pts',(-1.29622666598137,6.64169296417704,-27.1358932071761));
#41522=CARTESIAN_POINT('Ctrl Pts',(-1.47651500757769,6.60650697211099,-27.1272742186516));
#41523=CARTESIAN_POINT('Ctrl Pts',(-1.65530419536613,6.56398866374391,-27.1186552301272));
#41524=CARTESIAN_POINT('Ctrl Pts',(-1.83199864963129,6.51429734873602,-27.1100362416027));
#41525=CARTESIAN_POINT('Ctrl Pts',(-2.00879895964344,6.4645762641958,-27.1014120895349));
#41526=CARTESIAN_POINT('Ctrl Pts',(-2.18350173887581,6.40767367931469,-27.0927879374672));
#41527=CARTESIAN_POINT('Ctrl Pts',(-2.35552729846031,6.34379855813599,-27.0841637853994));
#41528=CARTESIAN_POINT('Ctrl Pts',(-2.53344477974066,6.27773569687258,-27.0752442538031));
#41529=CARTESIAN_POINT('Ctrl Pts',(-2.70849807075692,6.2042143527267,-27.0663247222069));
#41530=CARTESIAN_POINT('Ctrl Pts',(-2.88006970944353,6.12351920620373,-27.0574051906106));
#41531=CARTESIAN_POINT('Ctrl Pts',(-3.04626860909665,6.04535101557425,-27.0487649727514));
#41532=CARTESIAN_POINT('Ctrl Pts',(-3.20920036236136,5.96045169784565,-27.0401247548921));
#41533=CARTESIAN_POINT('Ctrl Pts',(-3.36832956203072,5.86912642235196,-27.0314845370329));
#41534=CARTESIAN_POINT('Ctrl Pts',(-3.53517505522743,5.77337271616397,-27.0224253485681));
#41535=CARTESIAN_POINT('Ctrl Pts',(-3.69783972134989,5.67055456700585,-27.0133661601034));
#41536=CARTESIAN_POINT('Ctrl Pts',(-3.85574103850704,5.56107454040788,-27.0043069716386));
#41537=CARTESIAN_POINT('Ctrl Pts',(-4.01364235566422,5.45159451380989,-26.9952477831738));
#41538=CARTESIAN_POINT('Ctrl Pts',(-4.16678003900837,5.33545286738085,-26.9861885947091));
#41539=CARTESIAN_POINT('Ctrl Pts',(-4.31461139104156,5.21310056917133,-26.9771294062443));
#41540=CARTESIAN_POINT('Ctrl Pts',(-4.46218663562887,5.09096023773449,-26.968085912188));
#41541=CARTESIAN_POINT('Ctrl Pts',(-4.60461041245573,4.96251888607445,-26.9590424181317));
#41542=CARTESIAN_POINT('Ctrl Pts',(-4.74137395223829,4.82821520285046,-26.9499989240754));
#41543=CARTESIAN_POINT('Ctrl Pts',(-4.87801239491148,4.69403436671404,-26.94096370207));
#41544=CARTESIAN_POINT('Ctrl Pts',(-5.00900076750657,4.5540020714474,-26.9319284800646));
#41545=CARTESIAN_POINT('Ctrl Pts',(-5.13386596701775,4.40859492726389,-26.9228932580592));
#41546=CARTESIAN_POINT('Ctrl Pts',(-5.25851118122987,4.26344395881409,-26.913873954148));
#41547=CARTESIAN_POINT('Ctrl Pts',(-5.3770546091405,4.11293723088186,-26.9048546502369));
#41548=CARTESIAN_POINT('Ctrl Pts',(-5.48906244356266,3.95758543693878,-26.8958353463258));
#41549=CARTESIAN_POINT('Ctrl Pts',(-5.60092975633303,3.80242854267219,-26.8868273577614));
#41550=CARTESIAN_POINT('Ctrl Pts',(-5.70627769988811,3.6424389054898,-26.877819369197));
#41551=CARTESIAN_POINT('Ctrl Pts',(-5.8047133411596,3.4781592871753,-26.8688113806326));
#41552=CARTESIAN_POINT('Ctrl Pts',(-5.90292666208736,3.314250700133,-26.8598237369259));
#41553=CARTESIAN_POINT('Ctrl Pts',(-5.99425872091947,3.14607167608885,-26.8508360932191));
#41554=CARTESIAN_POINT('Ctrl Pts',(-6.07836065704107,2.97419244887335,-26.8418484495124));
#41555=CARTESIAN_POINT('Ctrl Pts',(-6.15160761428083,2.82449755495256,-26.8340208347793));
#41556=CARTESIAN_POINT('Ctrl Pts',(-6.21937094682393,2.67199653257325,-26.8261932200462));
#41557=CARTESIAN_POINT('Ctrl Pts',(-6.28144717792786,2.51708369962187,-26.818365605313));
#41558=CARTESIAN_POINT('Ctrl Pts',(-6.34392048509957,2.36117995312011,-26.8104879205543));
#41559=CARTESIAN_POINT('Ctrl Pts',(-6.40061979527873,2.20286322566247,-26.8026102357956));
#41560=CARTESIAN_POINT('Ctrl Pts',(-6.45135507265898,2.04262251198729,-26.7947325510369));
#41561=CARTESIAN_POINT('Ctrl Pts',(-6.50360939287892,1.87758410090503,-26.7866190039503));
#41562=CARTESIAN_POINT('Ctrl Pts',(-6.54953679513948,1.71050508572804,-26.7785054568638));
#41563=CARTESIAN_POINT('Ctrl Pts',(-6.58898439250822,1.54193828517327,-26.7703919097773));
#41564=CARTESIAN_POINT('Ctrl Pts',(-6.62729075844782,1.37824817530526,-26.762513090166));
#41565=CARTESIAN_POINT('Ctrl Pts',(-6.65948699384009,1.21315557237102,-26.7546342705548));
#41566=CARTESIAN_POINT('Ctrl Pts',(-6.68548482724296,1.0471779336408,-26.7467554509435));
#41567=CARTESIAN_POINT('Ctrl Pts',(-6.71264446014735,0.873783033058348,
-26.7385245401193));
#41568=CARTESIAN_POINT('Ctrl Pts',(-6.73303885051885,0.699422635723901,
-26.7302936292952));
#41569=CARTESIAN_POINT('Ctrl Pts',(-6.74662778723258,0.524692767761558,
-26.722062718471));
#41570=CARTESIAN_POINT('Ctrl Pts',(-6.7602167239463,0.349962899799214,-26.7138318076468));
#41571=CARTESIAN_POINT('Ctrl Pts',(-6.76700022565576,0.174864042719825,
-26.7056008968226));
#41572=CARTESIAN_POINT('Ctrl Pts',(-6.76699999999437,-8.73235207390737E-6,
-26.6973699859984));
#41573=CARTESIAN_POINT('Ctrl Pts',(-6.767,2.46159858321081E-13,-26.6971797838101));
#41574=CARTESIAN_POINT('Ctrl Pts',(-6.76700000000001,-0.186007249559863,
-26.6884302719974));
#41575=CARTESIAN_POINT('Ctrl Pts',(-6.75932637294247,-0.372014355816143,
-26.6796807601846));
#41576=CARTESIAN_POINT('Ctrl Pts',(-6.74400518263361,-0.557389537586617,
-26.6709312483719));
#41577=CARTESIAN_POINT('Ctrl Pts',(-6.72868405703726,-0.742763936383156,
-26.6621817735147));
#41578=CARTESIAN_POINT('Ctrl Pts',(-6.70571545643557,-0.927506130405536,
-26.6534322986574));
#41579=CARTESIAN_POINT('Ctrl Pts',(-6.67517739401564,-1.11098864009612,
-26.6446828238002));
#41580=CARTESIAN_POINT('Ctrl Pts',(-6.64463945804373,-1.29447039004625,
-26.6359333851717));
#41581=CARTESIAN_POINT('Ctrl Pts',(-6.60653217002702,-1.47669218339379,
-26.6271839465432));
#41582=CARTESIAN_POINT('Ctrl Pts',(-6.5609849608545,-1.65703510627901,-26.6184345079147));
#41583=CARTESIAN_POINT('Ctrl Pts',(-6.51543793649521,-1.83737729740133,
-26.6096851047881));
#41584=CARTESIAN_POINT('Ctrl Pts',(-6.46245112156856,-2.01584035545082,
-26.6009357016614));
#41585=CARTESIAN_POINT('Ctrl Pts',(-6.40220448361671,-2.19181813797544,
-26.5921862985348));
#41586=CARTESIAN_POINT('Ctrl Pts',(-6.34195808511921,-2.36779522106443,
-26.5834369301833));
#41587=CARTESIAN_POINT('Ctrl Pts',(-6.27445201416296,-2.54128677725889,
-26.5746875618317));
#41588=CARTESIAN_POINT('Ctrl Pts',(-6.19991555052659,-2.71170355428807,
-26.5659381934802));
#41589=CARTESIAN_POINT('Ctrl Pts',(-6.12537937695036,-2.88211966813698,
-26.557188859177));
#41590=CARTESIAN_POINT('Ctrl Pts',(-6.04381298028244,-3.04946076420082,
-26.5484395248738));
#41591=CARTESIAN_POINT('Ctrl Pts',(-5.95549339308748,-3.21315848424745,
-26.5396901905706));
#41592=CARTESIAN_POINT('Ctrl Pts',(-5.86717414225566,-3.37685558085504,
-26.5309408895891));
#41593=CARTESIAN_POINT('Ctrl Pts',(-5.77210188843815,-3.5369090770041,-26.5221915886075));
#41594=CARTESIAN_POINT('Ctrl Pts',(-5.67059953311112,-3.6927753702439,-26.5134422876259));
#41595=CARTESIAN_POINT('Ctrl Pts',(-5.56909755592427,-3.84864108281434,
-26.5046930192393));
#41596=CARTESIAN_POINT('Ctrl Pts',(-5.46116568154663,-4.00031938355243,
-26.4959437508527));
#41597=CARTESIAN_POINT('Ctrl Pts',(-5.34717048488051,-4.14729511918585,
-26.4871944824661));
#41598=CARTESIAN_POINT('Ctrl Pts',(-5.23317570342956,-4.29427031947606,
-26.4784452459477));
#41599=CARTESIAN_POINT('Ctrl Pts',(-5.11311781951174,-4.43654276249987,
-26.4696960094293));
#41600=CARTESIAN_POINT('Ctrl Pts',(-4.98740458928846,-4.57362924412817,
-26.460946772911));
#41601=CARTESIAN_POINT('Ctrl Pts',(-4.86169180652338,-4.71071523781682,
-26.4521975675343));
#41602=CARTESIAN_POINT('Ctrl Pts',(-4.73032391141167,-4.84261509584885,
-26.4434483621576));
#41603=CARTESIAN_POINT('Ctrl Pts',(-4.59374706946921,-4.96888084599974,
-26.4346991567809));
#41604=CARTESIAN_POINT('Ctrl Pts',(-4.45717070231118,-5.09514615721082,
-26.4259499818192));
#41605=CARTESIAN_POINT('Ctrl Pts',(-4.31538563496991,-5.21577720520889,
-26.4172008068575));
#41606=CARTESIAN_POINT('Ctrl Pts',(-4.16887340951689,-5.33036429293749,
-26.4084516318958));
#41607=CARTESIAN_POINT('Ctrl Pts',(-4.02236168122185,-5.44495099183926,
-26.3997024866225));
#41608=CARTESIAN_POINT('Ctrl Pts',(-3.87112305262899,-5.55349359498124,
-26.3909533413493));
#41609=CARTESIAN_POINT('Ctrl Pts',(-3.71567116928734,-5.65562346357383,
-26.3822041960761));
#41610=CARTESIAN_POINT('Ctrl Pts',(-3.56021980053056,-5.75775299409085,
-26.3734550797647));
#41611=CARTESIAN_POINT('Ctrl Pts',(-3.40055544441836,-5.85346967520023,
-26.3647059634533));
#41612=CARTESIAN_POINT('Ctrl Pts',(-3.23722035886603,-5.94244843041514,
-26.355956847142));
#41613=CARTESIAN_POINT('Ctrl Pts',(-3.0738858004326,-6.03142689847567,-26.347207759066));
#41614=CARTESIAN_POINT('Ctrl Pts',(-2.90688078789005,-6.11366734708005,
-26.33845867099));
#41615=CARTESIAN_POINT('Ctrl Pts',(-2.73677250610188,-6.18889047001519,
-26.329709582914));
#41616=CARTESIAN_POINT('Ctrl Pts',(-2.56666475916736,-6.26411335643415,
-26.3209605223468));
#41617=CARTESIAN_POINT('Ctrl Pts',(-2.39345402456902,-6.33231884545328,
-26.3122114617796));
#41618=CARTESIAN_POINT('Ctrl Pts',(-2.21772855943881,-6.39327529804946,
-26.3034624012125));
#41619=CARTESIAN_POINT('Ctrl Pts',(-2.042003632234,-6.45423156404763,-26.2947133674277));
#41620=CARTESIAN_POINT('Ctrl Pts',(-1.86376426060836,-6.5079387441251,-26.2859643336428));
#41621=CARTESIAN_POINT('Ctrl Pts',(-1.68361577621482,-6.55421443943365,
-26.277215299858));
#41622=CARTESIAN_POINT('Ctrl Pts',(-1.50346782833009,-6.60048999692635,
-26.2684662921291));
#41623=CARTESIAN_POINT('Ctrl Pts',(-1.32141105657181,-6.63933404265203,
-26.2597172844003));
#41624=CARTESIAN_POINT('Ctrl Pts',(-1.13806375346329,-6.67061465631564,
-26.2509682766714));
#41625=CARTESIAN_POINT('Ctrl Pts',(-0.954716981168126,-6.70189517941797,
-26.2422192942719));
#41626=CARTESIAN_POINT('Ctrl Pts',(-0.770079967440584,-6.72561226609023,
-26.2334703118725));
#41627=CARTESIAN_POINT('Ctrl Pts',(-0.584779764071559,-6.74168536995998,
-26.2247213294731));
#41628=CARTESIAN_POINT('Ctrl Pts',(-0.391489587591418,-6.75845153117881,
-26.2155950990575));
#41629=CARTESIAN_POINT('Ctrl Pts',(-0.197478091803673,-6.76689985146399,
-26.2064688686419));
#41630=CARTESIAN_POINT('Ctrl Pts',(-0.00346214752944389,-6.76699911434415,
-26.1973426382262));
#41631=CARTESIAN_POINT('Ctrl Pts',(0.184490798486235,-6.76709527525931,
-26.1885016025111));
#41632=CARTESIAN_POINT('Ctrl Pts',(0.372447602156381,-6.75935633790754,
-26.179660566796));
#41633=CARTESIAN_POINT('Ctrl Pts',(0.559756448195821,-6.743809140145,-26.1708195310809));
#41634=CARTESIAN_POINT('Ctrl Pts',(0.745136131044979,-6.72842206873137,
-26.1620695524675));
#41635=CARTESIAN_POINT('Ctrl Pts',(0.929880851946681,-6.70538686355701,
-26.1533195738542));
#41636=CARTESIAN_POINT('Ctrl Pts',(1.11336305057628,-6.67478177303285,-26.1445695952409));
#41637=CARTESIAN_POINT('Ctrl Pts',(1.29684337090296,-6.64417699581227,-26.1358197062009));
#41638=CARTESIAN_POINT('Ctrl Pts',(1.4790609120537,-6.6060025354802,-26.127069817161));
#41639=CARTESIAN_POINT('Ctrl Pts',(1.65939671095408,-6.56038806441165,-26.118319928121));
#41640=CARTESIAN_POINT('Ctrl Pts',(1.83973072369346,-6.51477404513797,-26.1095701257455));
#41641=CARTESIAN_POINT('Ctrl Pts',(2.01818275357222,-6.46172023288603,-26.10082032337));
#41642=CARTESIAN_POINT('Ctrl Pts',(2.1941466403351,-6.40140683918045,-26.0920705209945));
#41643=CARTESIAN_POINT('Ctrl Pts',(2.37010884271446,-6.34109402281428,-26.083320802375));
#41644=CARTESIAN_POINT('Ctrl Pts',(2.54358267847994,-6.27352185699716,-26.0745710837554));
#41645=CARTESIAN_POINT('Ctrl Pts',(2.71397890841932,-6.19891986435178,-26.0658213651359));
#41646=CARTESIAN_POINT('Ctrl Pts',(2.88437356389133,-6.12431856103153,-26.0570717273641));
#41647=CARTESIAN_POINT('Ctrl Pts',(3.05169040787365,-6.0426876758246,-26.0483220895922));
#41648=CARTESIAN_POINT('Ctrl Pts',(3.21536112512248,-5.95430447953841,-26.0395724518204));
#41649=CARTESIAN_POINT('Ctrl Pts',(3.37903038443035,-5.86592207054932,-26.0308228919884));
#41650=CARTESIAN_POINT('Ctrl Pts',(3.53905332980163,-5.77078760703261,-26.0220733321563));
#41651=CARTESIAN_POINT('Ctrl Pts',(3.69488643042079,-5.66922422085177,-26.0133237723242));
#41652=CARTESIAN_POINT('Ctrl Pts',(3.8507181946893,-5.56766170563029,-26.0045742875242));
#41653=CARTESIAN_POINT('Ctrl Pts',(4.00235994599412,-5.45967053456114,-25.9958248027242));
#41654=CARTESIAN_POINT('Ctrl Pts',(4.14929662974488,-5.34561750206539,-25.9870753179242));
#41655=CARTESIAN_POINT('Ctrl Pts',(4.29623210225234,-5.23156540974311,-25.9783259052489));
#41656=CARTESIAN_POINT('Ctrl Pts',(4.43846235842308,-5.11145173172021,-25.9695764925735));
#41657=CARTESIAN_POINT('Ctrl Pts',(4.5755043179762,-4.98568443006386,-25.9608270798981));
#41658=CARTESIAN_POINT('Ctrl Pts',(4.7125451933768,-4.85991812336509,-25.9520777364402));
#41659=CARTESIAN_POINT('Ctrl Pts',(4.84439764315164,-4.72849847630916,-25.9433283929823));
#41660=CARTESIAN_POINT('Ctrl Pts',(4.97061384196861,-4.59187184425155,-25.9345790495245));
#41661=CARTESIAN_POINT('Ctrl Pts',(5.09682908420371,-4.45524624767559,-25.9258297723771));
#41662=CARTESIAN_POINT('Ctrl Pts',(5.21740796650326,-4.31341395556705,-25.9170804952297));
#41663=CARTESIAN_POINT('Ctrl Pts',(5.33194095942397,-4.1668566816267,-25.9083312180824));
#41664=CARTESIAN_POINT('Ctrl Pts',(5.44647312235278,-4.02030046975018,-25.8995820043388));
#41665=CARTESIAN_POINT('Ctrl Pts',(5.55495930712433,-3.86901957035339,-25.8908327905953));
#41666=CARTESIAN_POINT('Ctrl Pts',(5.65703106079939,-3.71352778058156,-25.8820835768518));
#41667=CARTESIAN_POINT('Ctrl Pts',(5.75910210868871,-3.55803706597383,-25.8733344236056));
#41668=CARTESIAN_POINT('Ctrl Pts',(5.85475865698677,-3.39833575880679,-25.8645852703594));
#41669=CARTESIAN_POINT('Ctrl Pts',(5.94367583069183,-3.234966247065,-25.8558361171132));
#41670=CARTESIAN_POINT('Ctrl Pts',(6.03259241910196,-3.07159781069866,-25.847087021458));
#41671=CARTESIAN_POINT('Ctrl Pts',(6.11476958471085,-2.90456146975588,-25.8383379258029));
#41672=CARTESIAN_POINT('Ctrl Pts',(6.189928235745,-2.73442451647998,-25.8295888301478));
#41673=CARTESIAN_POINT('Ctrl Pts',(6.26508641701035,-2.5642886266217,-25.8208397891777));
#41674=CARTESIAN_POINT('Ctrl Pts',(6.33322605570383,-2.39105242531046,-25.8120907482076));
#41675=CARTESIAN_POINT('Ctrl Pts',(6.39411573747842,-2.21530425353513,-25.8033417072375));
#41676=CARTESIAN_POINT('Ctrl Pts',(6.45500505889196,-2.03955712188338,-25.7945927180465));
#41677=CARTESIAN_POINT('Ctrl Pts',(6.50864441544996,-1.86129832025341,-25.7858437288555));
#41678=CARTESIAN_POINT('Ctrl Pts',(6.55485164049968,-1.6811332401207,-25.7770947396645));
#41679=CARTESIAN_POINT('Ctrl Pts',(6.60199852639165,-1.49730435912654,-25.7681678327876));
#41680=CARTESIAN_POINT('Ctrl Pts',(6.64140767441059,-1.31149113173403,-25.7592409259107));
#41681=CARTESIAN_POINT('Ctrl Pts',(6.67293975269645,-1.12435050446178,-25.7503140190338));
#41682=CARTESIAN_POINT('Ctrl Pts',(6.70384664831542,-0.940920291561222,
-25.7415641048498));
#41683=CARTESIAN_POINT('Ctrl Pts',(6.72718585889694,-0.756215114275426,
-25.7328141906658));
#41684=CARTESIAN_POINT('Ctrl Pts',(6.74287810451885,-0.570862389372636,
-25.7240642764818));
#41685=CARTESIAN_POINT('Ctrl Pts',(6.75857004154137,-0.385513309565678,
-25.7153145343712));
#41686=CARTESIAN_POINT('Ctrl Pts',(6.76661529035563,-0.199516993256871,
-25.7065647922607));
#41687=CARTESIAN_POINT('Ctrl Pts',(6.76698652348897,-0.0135052182028017,
-25.6978150501501));
#41688=CARTESIAN_POINT('Ctrl Pts',(6.76735774981518,0.172503146040102,-25.6890654684794));
#41689=CARTESIAN_POINT('Ctrl Pts',(6.76005524147473,0.358526681834634,-25.6803158868088));
#41690=CARTESIAN_POINT('Ctrl Pts',(6.74510380214872,0.543933542115981,-25.6715663051382));
#41691=CARTESIAN_POINT('Ctrl Pts',(6.73015261710967,0.729337249085829,-25.6628168722762));
#41692=CARTESIAN_POINT('Ctrl Pts',(6.7075527844459,0.91412401585576,-25.6540674394143));
#41693=CARTESIAN_POINT('Ctrl Pts',(6.67738106408271,1.09766621749494,-25.6453180065524));
#41694=CARTESIAN_POINT('Ctrl Pts',(6.64720981677234,1.28120554143423,-25.63656871087));
#41695=CARTESIAN_POINT('Ctrl Pts',(6.60946696581502,1.46350005650714,-25.6278194151877));
#41696=CARTESIAN_POINT('Ctrl Pts',(6.56428070010972,1.64393062206621,-25.6190701195053));
#41697=CARTESIAN_POINT('Ctrl Pts',(6.51909508282717,1.82435859844738,-25.6103209493753));
#41698=CARTESIAN_POINT('Ctrl Pts',(6.46646633415635,2.00292240086648,-25.6015717792454));
#41699=CARTESIAN_POINT('Ctrl Pts',(6.40657319597164,2.17901557696537,-25.5928226091154));
#41700=CARTESIAN_POINT('Ctrl Pts',(6.34668083768264,2.35510646007518,-25.5840735529123));
#41701=CARTESIAN_POINT('Ctrl Pts',(6.27952437143852,2.52872650996614,-25.5753244967092));
#41702=CARTESIAN_POINT('Ctrl Pts',(6.205331873351,2.69928607998008,-25.5665754405061));
#41703=CARTESIAN_POINT('Ctrl Pts',(6.12831449784216,2.87633970115475,-25.5574932642173));
#41704=CARTESIAN_POINT('Ctrl Pts',(6.04371489463117,3.05009490562421,-25.5484110879285));
#41705=CARTESIAN_POINT('Ctrl Pts',(5.95184265120455,3.21991584599698,-25.5393289116396));
#41706=CARTESIAN_POINT('Ctrl Pts',(5.8633328133545,3.38352155905374,-25.5305791312852));
#41707=CARTESIAN_POINT('Ctrl Pts',(5.76807337235636,3.54347560903903,-25.5218293509308));
#41708=CARTESIAN_POINT('Ctrl Pts',(5.666387900863,3.69923467178731,-25.5130795705764));
#41709=CARTESIAN_POINT('Ctrl Pts',(5.56470608502682,3.85498813489852,-25.5043301047821));
#41710=CARTESIAN_POINT('Ctrl Pts',(5.45659885766885,4.00654667256353,-25.4955806389878));
#41711=CARTESIAN_POINT('Ctrl Pts',(5.34243340580433,4.15339551506306,-25.4868311731936));
#41712=CARTESIAN_POINT('Ctrl Pts',(5.22827145140514,4.30023985883968,-25.4780819754397));
#41713=CARTESIAN_POINT('Ctrl Pts',(5.10805181978004,4.44237456993141,-25.4693327776858));
#41714=CARTESIAN_POINT('Ctrl Pts',(4.9821828128246,4.57931691626549,-25.4605835799319));
#41715=CARTESIAN_POINT('Ctrl Pts',(4.8563169929615,4.71625579512242,-25.451834603714));
#41716=CARTESIAN_POINT('Ctrl Pts',(4.72480227791772,4.84800236135833,-25.443085627496));
#41717=CARTESIAN_POINT('Ctrl Pts',(4.58808530848063,4.97410918678955,-25.434336651278));
#41718=CARTESIAN_POINT('Ctrl Pts',(4.45135945056915,5.10022421089058,-25.4255871062568));
#41719=CARTESIAN_POINT('Ctrl Pts',(4.30943087207979,5.22069856612037,-25.4168375612356));
#41720=CARTESIAN_POINT('Ctrl Pts',(4.16278164322401,5.33512305301736,-25.4080880162144));
#41721=CARTESIAN_POINT('Ctrl Pts',(4.0161410353432,5.44954081331479,-25.3993389855471));
#41722=CARTESIAN_POINT('Ctrl Pts',(3.86478055833338,5.5579092406839,-25.3905899548798));
#41723=CARTESIAN_POINT('Ctrl Pts',(3.70921425811872,5.65986029751343,-25.3818409242126));
#41724=CARTESIAN_POINT('Ctrl Pts',(3.55364584530041,5.76181273884702,-25.3730917747327));
#41725=CARTESIAN_POINT('Ctrl Pts',(3.39387173464266,5.85734747818108,-25.3643426252529));
#41726=CARTESIAN_POINT('Ctrl Pts',(3.23043456092328,5.9461400544885,-25.355593475773));
#41727=CARTESIAN_POINT('Ctrl Pts',(3.1869076880634,5.96978744811309,-25.35326338704));
#41728=CARTESIAN_POINT('Ctrl Pts',(3.14312114982855,5.99295688499314,-25.350933298307));
#41729=CARTESIAN_POINT('Ctrl Pts',(3.09908550384719,6.01564277861013,-25.348603209574));
#41730=CARTESIAN_POINT('Origin',(0.,0.,-63.6971797838103));
#41731=CARTESIAN_POINT('',(3.09908550384719,6.01564277861013,-22.9543563216829));
#41732=CARTESIAN_POINT('',(3.09908550384722,6.01564277861011,-23.348603209574));
#41733=CARTESIAN_POINT('',(3.09908550384721,6.01564277861012,-63.6971797838103));
#41734=CARTESIAN_POINT('',(-6.76699985752918,-0.0013885964259113,-24.302820216155));
#41735=CARTESIAN_POINT('Ctrl Pts',(-6.76699985752918,-0.00138859642590996,
-24.302820216155));
#41736=CARTESIAN_POINT('Ctrl Pts',(-6.76696126318091,-0.189469124644247,
-24.2940182998959));
#41737=CARTESIAN_POINT('Ctrl Pts',(-6.75907723606001,-0.377334540807269,
-24.2852163836369));
#41738=CARTESIAN_POINT('Ctrl Pts',(-6.74342679625424,-0.564343905398435,
-24.2764144673779));
#41739=CARTESIAN_POINT('Ctrl Pts',(-6.72774331109054,-0.751748133741929,
-24.2675939661796));
#41740=CARTESIAN_POINT('Ctrl Pts',(-6.70426066358534,-0.938292432248802,
-24.2587734649813));
#41741=CARTESIAN_POINT('Ctrl Pts',(-6.67310915788618,-1.12334463408856,
-24.249952963783));
#41742=CARTESIAN_POINT('Ctrl Pts',(-6.6418545809807,-1.30900911945202,-24.2411032781303));
#41743=CARTESIAN_POINT('Ctrl Pts',(-6.60288040506713,-1.49317136165447,
-24.2322535924775));
#41744=CARTESIAN_POINT('Ctrl Pts',(-6.55636800887928,-1.67520969796153,
-24.2234039068248));
#41745=CARTESIAN_POINT('Ctrl Pts',(-6.50977942525895,-1.85754621356254,
-24.2145397253626));
#41746=CARTESIAN_POINT('Ctrl Pts',(-6.45562802879989,-2.03775161692499,
-24.2056755439005));
#41747=CARTESIAN_POINT('Ctrl Pts',(-6.39414431751011,-2.21522176019765,
-24.1968113624384));
#41748=CARTESIAN_POINT('Ctrl Pts',(-6.33249091550744,-2.39318170856659,
-24.1879227164598));
#41749=CARTESIAN_POINT('Ctrl Pts',(-6.26346480114711,-2.56839104029644,
-24.1790340704812));
#41750=CARTESIAN_POINT('Ctrl Pts',(-6.18734493758006,-2.7402648819781,-24.1701454245025));
#41751=CARTESIAN_POINT('Ctrl Pts',(-6.11503594919804,-2.90353400831308,
-24.161701780903));
#41752=CARTESIAN_POINT('Ctrl Pts',(-6.03632618151536,-3.06379328561213,
-24.1532581373035));
#41753=CARTESIAN_POINT('Ctrl Pts',(-5.95149173846921,-3.22056440502791,
-24.144814493704));
#41754=CARTESIAN_POINT('Ctrl Pts',(-5.87040260093117,-3.37041432927839,
-24.1367436235176));
#41755=CARTESIAN_POINT('Ctrl Pts',(-5.78350212677905,-3.51747328255109,
-24.1286727533313));
#41756=CARTESIAN_POINT('Ctrl Pts',(-5.69100705784284,-3.66124673678011,
-24.1206018831449));
#41757=CARTESIAN_POINT('Ctrl Pts',(-5.59862709183042,-3.80484127612065,
-24.1125410565291));
#41758=CARTESIAN_POINT('Ctrl Pts',(-5.50066658303825,-3.94515814187245,
-24.1044802299133));
#41759=CARTESIAN_POINT('Ctrl Pts',(-5.39738937150403,-4.08172475460747,
-24.0964194032975));
#41760=CARTESIAN_POINT('Ctrl Pts',(-5.29421803331549,-4.21815136778222,
-24.0883668401376));
#41761=CARTESIAN_POINT('Ctrl Pts',(-5.18574106188821,-4.35083508368595,
-24.0803142769777));
#41762=CARTESIAN_POINT('Ctrl Pts',(-5.07226699578639,-4.47932991902317,
-24.0722617138178));
#41763=CARTESIAN_POINT('Ctrl Pts',(-4.95888440959649,-4.60772116508556,
-24.06421564243));
#41764=CARTESIAN_POINT('Ctrl Pts',(-4.84051299257633,-4.7319299737604,-24.0561695710421));
#41765=CARTESIAN_POINT('Ctrl Pts',(-4.71750311646949,-4.85154133715262,
-24.0481234996542));
#41766=CARTESIAN_POINT('Ctrl Pts',(-4.59456550079222,-4.97108243652399,
-24.0400821548184));
#41767=CARTESIAN_POINT('Ctrl Pts',(-4.46699511709127,-5.08603120759034,
-24.0320408099825));
#41768=CARTESIAN_POINT('Ctrl Pts',(-4.33518086957777,-5.19600768167706,
-24.0239994651466));
#41769=CARTESIAN_POINT('Ctrl Pts',(-4.20082564896488,-5.30810416378636,
-24.0158031079256));
#41770=CARTESIAN_POINT('Ctrl Pts',(-4.06206154160527,-5.41503439628679,
-24.0076067507045));
#41771=CARTESIAN_POINT('Ctrl Pts',(-3.9193381014415,-5.51643706087444,-23.9994103934834));
#41772=CARTESIAN_POINT('Ctrl Pts',(-3.77935840701377,-5.61589033909452,
-23.9913716047749));
#41773=CARTESIAN_POINT('Ctrl Pts',(-3.63557055703218,-5.71002644174433,
-23.9833328160664));
#41774=CARTESIAN_POINT('Ctrl Pts',(-3.48842989759845,-5.79854687396259,
-23.9752940273579));
#41775=CARTESIAN_POINT('Ctrl Pts',(-3.341273492781,-5.88707677866912,-23.9672543784262));
#41776=CARTESIAN_POINT('Ctrl Pts',(-3.19076388411651,-5.96998962378017,
-23.9592147294945));
#41777=CARTESIAN_POINT('Ctrl Pts',(-3.03738278992653,-6.04703189899459,
-23.9511750805628));
#41778=CARTESIAN_POINT('Ctrl Pts',(-2.8839549125279,-6.12409767309495,-23.9431329794346));
#41779=CARTESIAN_POINT('Ctrl Pts',(-2.72765413979294,-6.19528914557821,
-23.9350908783065));
#41780=CARTESIAN_POINT('Ctrl Pts',(-2.56898387667595,-6.26040021415397,
-23.9270487771783));
#41781=CARTESIAN_POINT('Ctrl Pts',(-2.40495911557534,-6.32770852548052,
-23.9187352867335));
#41782=CARTESIAN_POINT('Ctrl Pts',(-2.23840254812185,-6.38851870702157,
-23.9104217962887));
#41783=CARTESIAN_POINT('Ctrl Pts',(-2.06988818108355,-6.44265876155261,
-23.9021083058439));
#41784=CARTESIAN_POINT('Ctrl Pts',(-1.90658770693222,-6.49512370404318,
-23.8940520376732));
#41785=CARTESIAN_POINT('Ctrl Pts',(-1.7414491532652,-6.54132509649991,-23.8859957695024));
#41786=CARTESIAN_POINT('Ctrl Pts',(-1.57500554275679,-6.5811584497173,-23.8779395013317));
#41787=CARTESIAN_POINT('Ctrl Pts',(-1.40059056081101,-6.62289951482055,
-23.8694973997499));
#41788=CARTESIAN_POINT('Ctrl Pts',(-1.22474292072371,-6.65764748650981,
-23.8610552981681));
#41789=CARTESIAN_POINT('Ctrl Pts',(-1.04808159823491,-6.68534321956931,
-23.8526131965863));
#41790=CARTESIAN_POINT('Ctrl Pts',(-0.871420275746075,-6.71303895262882,
-23.8441710950045));
#41791=CARTESIAN_POINT('Ctrl Pts',(-0.693945738634898,-6.73368247969746,
-23.8357289934227));
#41792=CARTESIAN_POINT('Ctrl Pts',(-0.516275786879578,-6.74727710353457,
-23.8272868918409));
#41793=CARTESIAN_POINT('Ctrl Pts',(-0.340884219412577,-6.76069739413723,
-23.8189530491482));
#41794=CARTESIAN_POINT('Ctrl Pts',(-0.164744669744684,-6.76729175556978,
-23.8106192064555));
#41795=CARTESIAN_POINT('Ctrl Pts',(0.0115772523575617,-6.76699009658119,
-23.8022853637629));
#41796=CARTESIAN_POINT('Ctrl Pts',(0.187691356767948,-6.76668879313588,
-23.7939613435581));
#41797=CARTESIAN_POINT('Ctrl Pts',(0.36398706053264,-6.75950766123828,-23.7856373233533));
#41798=CARTESIAN_POINT('Ctrl Pts',(0.539893785042186,-6.74542835562523,
-23.7773133031486));
#41799=CARTESIAN_POINT('Ctrl Pts',(0.715625433464996,-6.7313630628348,-23.7689975676577));
#41800=CARTESIAN_POINT('Ctrl Pts',(0.89096852936691,-6.71041330247559,-23.7606818321669));
#41801=CARTESIAN_POINT('Ctrl Pts',(1.06535241597644,-6.68261275473697,-23.752366096676));
#41802=CARTESIAN_POINT('Ctrl Pts',(1.23959469377682,-6.65483478249276,-23.744057113996));
#41803=CARTESIAN_POINT('Ctrl Pts',(1.41287897234954,-6.62021716259422,-23.735748131316));
#41804=CARTESIAN_POINT('Ctrl Pts',(1.58463941174141,-6.57884541046192,-23.7274391486359));
#41805=CARTESIAN_POINT('Ctrl Pts',(1.75629182636982,-6.5374996781381,-23.7191353916988));
#41806=CARTESIAN_POINT('Ctrl Pts',(1.92642197456027,-6.48940836033004,-23.7108316347616));
#41807=CARTESIAN_POINT('Ctrl Pts',(2.09447368731141,-6.43470814980448,-23.7025278778244));
#41808=CARTESIAN_POINT('Ctrl Pts',(2.26245717511828,-6.38003014624577,-23.6942274920124));
#41809=CARTESIAN_POINT('Ctrl Pts',(2.42836357859681,-6.3187487036407,-23.6859271062004));
#41810=CARTESIAN_POINT('Ctrl Pts',(2.59165110374154,-6.25105059621783,-23.6776267203883));
#41811=CARTESIAN_POINT('Ctrl Pts',(2.75490419579602,-6.18336676456428,-23.6693280849117));
#41812=CARTESIAN_POINT('Ctrl Pts',(2.91553918865101,-6.10926909693446,-23.6610294494351));
#41813=CARTESIAN_POINT('Ctrl Pts',(3.07303328924743,-6.02899290123791,-23.6527308139584));
#41814=CARTESIAN_POINT('Ctrl Pts',(3.23052032064901,-5.94872030877518,-23.6444325509699));
#41815=CARTESIAN_POINT('Ctrl Pts',(3.38486643097191,-5.86226989897023,-23.6361342879813));
#41816=CARTESIAN_POINT('Ctrl Pts',(3.53557233034882,-5.76992350875398,-23.6278360249927));
#41817=CARTESIAN_POINT('Ctrl Pts',(3.68629647956674,-5.67756593578412,-23.6195367571199));
#41818=CARTESIAN_POINT('Ctrl Pts',(3.83337924325554,-5.57931114192698,-23.6112374892471));
#41819=CARTESIAN_POINT('Ctrl Pts',(3.97634912170628,-5.47548506182838,-23.6029382213743));
#41820=CARTESIAN_POINT('Ctrl Pts',(4.11941938805517,-5.37158607908716,-23.5946331260778));
#41821=CARTESIAN_POINT('Ctrl Pts',(4.25837071686701,-5.2621081979698,-23.5863280307812));
#41822=CARTESIAN_POINT('Ctrl Pts',(4.39276288911597,-5.1474190814432,-23.5780229354847));
#41823=CARTESIAN_POINT('Ctrl Pts',(4.52720406773925,-5.03268814330094,-23.5697148117186));
#41824=CARTESIAN_POINT('Ctrl Pts',(4.65708251649328,-4.91274241357201,-23.5614066879525));
#41825=CARTESIAN_POINT('Ctrl Pts',(4.78199374036426,-4.78798755920658,-23.5530985641864));
#41826=CARTESIAN_POINT('Ctrl Pts',(4.90703774414458,-4.66310009115171,-23.5447816089327));
#41827=CARTESIAN_POINT('Ctrl Pts',(5.02710373249196,-4.5333935357797,-23.5364646536791));
#41828=CARTESIAN_POINT('Ctrl Pts',(5.14182575095762,-4.39930868964535,-23.5281476984254));
#41829=CARTESIAN_POINT('Ctrl Pts',(5.22637413311174,-4.30049019809801,-23.522018228943));
#41830=CARTESIAN_POINT('Ctrl Pts',(5.30802077137017,-4.19929437624894,-23.5158887594606));
#41831=CARTESIAN_POINT('Ctrl Pts',(5.38663401285674,-4.09590808143138,-23.5097592899781));
#41832=CARTESIAN_POINT('Ctrl Pts',(5.49502224369749,-3.9533639326779,-23.501308266453));
#41833=CARTESIAN_POINT('Ctrl Pts',(5.59784060462339,-3.80639422127925,-23.4928572429278));
#41834=CARTESIAN_POINT('Ctrl Pts',(5.69472503408853,-3.65546109076891,-23.4844062194027));
#41835=CARTESIAN_POINT('Ctrl Pts',(5.79152415969299,-3.50466085239416,-23.4759626367526));
#41836=CARTESIAN_POINT('Ctrl Pts',(5.88239958932085,-3.34990442815064,-23.4675190541025));
#41837=CARTESIAN_POINT('Ctrl Pts',(5.96702915765726,-3.19168482649338,-23.4590754714524));
#41838=CARTESIAN_POINT('Ctrl Pts',(6.05159571664363,-3.03358302425849,-23.4506381753126));
#41839=CARTESIAN_POINT('Ctrl Pts',(6.12992552853229,-2.87202347595894,-23.4422008791728));
#41840=CARTESIAN_POINT('Ctrl Pts',(6.20174098034566,-2.70752614257025,-23.433763583033));
#41841=CARTESIAN_POINT('Ctrl Pts',(6.27350519730995,-2.54314616548629,-23.4253323062607));
#41842=CARTESIAN_POINT('Ctrl Pts',(6.33876419210611,-2.37583288696878,-23.4169010294884));
#41843=CARTESIAN_POINT('Ctrl Pts',(6.39728725678751,-2.20612890696444,-23.408469752716));
#41844=CARTESIAN_POINT('Ctrl Pts',(6.45578523636488,-2.03649766822914,-23.4000420898941));
#41845=CARTESIAN_POINT('Ctrl Pts',(6.50755293384692,-1.86447808367463,-23.3916144270723));
#41846=CARTESIAN_POINT('Ctrl Pts',(6.55240832212275,-1.69063129634361,-23.3831867642504));
#41847=CARTESIAN_POINT('Ctrl Pts',(6.59724990213602,-1.51683802592948,-23.3747616957964));
#41848=CARTESIAN_POINT('Ctrl Pts',(6.63518333376086,-1.34121899507468,-23.3663366273425));
#41849=CARTESIAN_POINT('Ctrl Pts',(6.66607677140178,-1.16434937960118,-23.3579115588885));
#41850=CARTESIAN_POINT('Ctrl Pts',(6.67453016156533,-1.1159524389611,-23.3556062022745));
#41851=CARTESIAN_POINT('Ctrl Pts',(6.68245673431267,-1.06746193098025,-23.3533008456605));
#41852=CARTESIAN_POINT('Ctrl Pts',(6.68985445395339,-1.01888978055528,-23.3509954890464));
#41853=CARTESIAN_POINT('Ctrl Pts',(6.71751215354869,-0.837294098318812,
-23.3423765005219));
#41854=CARTESIAN_POINT('Ctrl Pts',(6.73776139366763,-0.654637731083349,
-23.3337575119974));
#41855=CARTESIAN_POINT('Ctrl Pts',(6.75055135896841,-0.471535099361469,
-23.3251385234728));
#41856=CARTESIAN_POINT('Ctrl Pts',(6.76334898659981,-0.288322772822682,
-23.316514371405));
#41857=CARTESIAN_POINT('Ctrl Pts',(6.7686783999153,-0.10466395165724,-23.3078902193371));
#41858=CARTESIAN_POINT('Ctrl Pts',(6.76654088834419,0.078825163280762,-23.2992660672693));
#41859=CARTESIAN_POINT('Ctrl Pts',(6.76433016642674,0.268598829766734,-23.2903465356731));
#41860=CARTESIAN_POINT('Ctrl Pts',(6.75413198765148,0.458190601449416,-23.2814270040769));
#41861=CARTESIAN_POINT('Ctrl Pts',(6.73600618976047,0.64692318826012,-23.2725074724807));
#41862=CARTESIAN_POINT('Ctrl Pts',(6.71844799839546,0.82974564363355,-23.2638672546214));
#41863=CARTESIAN_POINT('Ctrl Pts',(6.69345126546767,1.01176161468065,-23.2552270367621));
#41864=CARTESIAN_POINT('Ctrl Pts',(6.66112278249805,1.19236415431085,-23.2465868189028));
#41865=CARTESIAN_POINT('Ctrl Pts',(6.62722666728823,1.38172424572757,-23.2375276304382));
#41866=CARTESIAN_POINT('Ctrl Pts',(6.58527016512356,1.56953004256572,-23.2284684419736));
#41867=CARTESIAN_POINT('Ctrl Pts',(6.53543587681752,1.75509740470619,-23.2194092535089));
#41868=CARTESIAN_POINT('Ctrl Pts',(6.48560158851148,1.9406647668467,-23.2103500650443));
#41869=CARTESIAN_POINT('Ctrl Pts',(6.42788966055494,2.12399333926707,-23.2012908765797));
#41870=CARTESIAN_POINT('Ctrl Pts',(6.36254168908051,2.30442015585539,-23.1922316881151));
#41871=CARTESIAN_POINT('Ctrl Pts',(6.29730692838156,2.48453439564347,-23.1831881940588));
#41872=CARTESIAN_POINT('Ctrl Pts',(6.2244032583442,2.66192314364162,-23.1741447000026));
#41873=CARTESIAN_POINT('Ctrl Pts',(6.1440721534288,2.8359595154834,-23.1651012059463));
#41874=CARTESIAN_POINT('Ctrl Pts',(6.06381452708134,3.00983669689219,-23.156065983941));
#41875=CARTESIAN_POINT('Ctrl Pts',(5.97614312949107,3.18036740825088,-23.1470307619357));
#41876=CARTESIAN_POINT('Ctrl Pts',(5.88134716121483,3.34694555815752,-23.1379955399304));
#41877=CARTESIAN_POINT('Ctrl Pts',(5.78671820279783,3.51323023362767,-23.1289762360194));
#41878=CARTESIAN_POINT('Ctrl Pts',(5.68498985596708,3.67557604633669,-23.1199569321083));
#41879=CARTESIAN_POINT('Ctrl Pts',(5.57649665749191,3.83340240895494,-23.1109376281972));
#41880=CARTESIAN_POINT('Ctrl Pts',(5.46813957131234,3.99103076737732,-23.1019296396329));
#41881=CARTESIAN_POINT('Ctrl Pts',(5.35303470505299,4.14415079539388,-23.0929216510686));
#41882=CARTESIAN_POINT('Ctrl Pts',(5.23156056683908,4.29220957497352,-23.0839136625042));
#41883=CARTESIAN_POINT('Ctrl Pts',(5.11036078222108,4.43993395861358,-23.0749260187976));
#41884=CARTESIAN_POINT('Ctrl Pts',(4.98282059060928,4.58261972742745,-23.065938375091));
#41885=CARTESIAN_POINT('Ctrl Pts',(4.84935922262927,4.7197461933774,-23.0569507313843));
#41886=CARTESIAN_POINT('Ctrl Pts',(4.73312362134445,4.8391738409656,-23.0491231166506));
#41887=CARTESIAN_POINT('Ctrl Pts',(4.61239739832344,4.95438499555938,-23.041295501917));
#41888=CARTESIAN_POINT('Ctrl Pts',(4.48748318345316,5.06505515056106,-23.0334678871833));
#41889=CARTESIAN_POINT('Ctrl Pts',(4.35785277193138,5.17990371083857,-23.0253447370661));
#41890=CARTESIAN_POINT('Ctrl Pts',(4.22376899574635,5.28980931252195,-23.017221586949));
#41891=CARTESIAN_POINT('Ctrl Pts',(4.0856543433547,5.39441540731031,-23.0090984368318));
#41892=CARTESIAN_POINT('Ctrl Pts',(3.94755721279876,5.49900823130679,-23.0009763172534));
#41893=CARTESIAN_POINT('Ctrl Pts',(3.80543051846155,5.59830266940212,-22.992854197675));
#41894=CARTESIAN_POINT('Ctrl Pts',(3.65972842587266,5.6919835601361,-22.9847320780966));
#41895=CARTESIAN_POINT('Ctrl Pts',(3.51399481055972,5.78568471877986,-22.9766082012934));
#41896=CARTESIAN_POINT('Ctrl Pts',(3.36468456166332,5.87376970914436,-22.9684843244901));
#41897=CARTESIAN_POINT('Ctrl Pts',(3.21227947894243,5.95596755776636,-22.9603604476869));
#41898=CARTESIAN_POINT('Ctrl Pts',(3.17473339339418,5.97621758749729,-22.9583590723522));
#41899=CARTESIAN_POINT('Ctrl Pts',(3.13699959370374,5.99611053399551,-22.9563576970175));
#41900=CARTESIAN_POINT('Ctrl Pts',(3.09908550384719,6.01564277861013,-22.9543563216829));
#41901=CARTESIAN_POINT('Ctrl Pts',(3.09908550384718,6.01564277861014,-24.9542890874699));
#41902=CARTESIAN_POINT('Ctrl Pts',(2.93974250446997,6.09773169207842,-24.9458659075154));
#41903=CARTESIAN_POINT('Ctrl Pts',(2.77713343362295,6.17348699570386,-24.9374427275608));
#41904=CARTESIAN_POINT('Ctrl Pts',(2.61179253161539,6.24266199403733,-24.9290195476063));
#41905=CARTESIAN_POINT('Ctrl Pts',(2.44643071877461,6.31184574100368,-24.9205953023635));
#41906=CARTESIAN_POINT('Ctrl Pts',(2.27833669360101,6.37444739472453,-24.9121710571208));
#41907=CARTESIAN_POINT('Ctrl Pts',(2.10806433798888,6.43026855946931,-24.9037468118781));
#41908=CARTESIAN_POINT('Ctrl Pts',(1.93774669663451,6.48610457044599,-24.8953203261178));
#41909=CARTESIAN_POINT('Ctrl Pts',(1.76524988660969,6.53515639324064,-24.8868938403575));
#41910=CARTESIAN_POINT('Ctrl Pts',(1.59114294713281,6.57727550903788,-24.8784673545972));
#41911=CARTESIAN_POINT('Ctrl Pts',(1.41688211841228,6.61943185298291,-24.870033420854));
#41912=CARTESIAN_POINT('Ctrl Pts',(1.24100864062694,6.65464316526037,-24.8615994871107));
#41913=CARTESIAN_POINT('Ctrl Pts',(1.06410293293535,6.68281182947106,-24.8531655533675));
#41914=CARTESIAN_POINT('Ctrl Pts',(0.887119446636669,6.71099287835546,-24.8447279115493));
#41915=CARTESIAN_POINT('Ctrl Pts',(0.709103155837299,6.73212505908049,-24.8362902697311));
#41916=CARTESIAN_POINT('Ctrl Pts',(0.530640151997714,6.74616261507888,-24.8278526279129));
#41917=CARTESIAN_POINT('Ctrl Pts',(0.351964788015918,6.76021687491685,-24.8194049458131));
#41918=CARTESIAN_POINT('Ctrl Pts',(0.172841981973288,6.76715961762895,-24.8109572637133));
#41919=CARTESIAN_POINT('Ctrl Pts',(-0.00614018145540926,6.76699721428727,
-24.8025095816135));
#41920=CARTESIAN_POINT('Ctrl Pts',(-0.166031593208453,6.76685213335252,
-24.7949629535524));
#41921=CARTESIAN_POINT('Ctrl Pts',(-0.325810607070901,6.76103750980862,
-24.7874163254912));
#41922=CARTESIAN_POINT('Ctrl Pts',(-0.485061296249177,6.74959291653068,
-24.7798696974301));
#41923=CARTESIAN_POINT('Ctrl Pts',(-0.658960047123738,6.73709563638972,
-24.7716289218333));
#41924=CARTESIAN_POINT('Ctrl Pts',(-0.832615606941793,6.71785623257765,
-24.7633881462365));
#41925=CARTESIAN_POINT('Ctrl Pts',(-1.00546700708788,6.69188501826337,-24.7551473706398));
#41926=CARTESIAN_POINT('Ctrl Pts',(-1.17812695556864,6.66594256988461,-24.7469157225954));
#41927=CARTESIAN_POINT('Ctrl Pts',(-1.34998416916725,6.63328321007928,-24.738684074551));
#41928=CARTESIAN_POINT('Ctrl Pts',(-1.52047994699688,6.59396919395142,-24.7304524265066));
#41929=CARTESIAN_POINT('Ctrl Pts',(-1.69081726620803,6.55469171623385,-24.7222284289483));
#41930=CARTESIAN_POINT('Ctrl Pts',(-1.85979532491654,6.50877197895478,-24.7140044313901));
#41931=CARTESIAN_POINT('Ctrl Pts',(-2.0268627052942,6.45632376619137,-24.7057804338318));
#41932=CARTESIAN_POINT('Ctrl Pts',(-2.19378248099232,6.40392189162767,-24.6975637022073));
#41933=CARTESIAN_POINT('Ctrl Pts',(-2.35879460474896,6.34500314383873,-24.6893469705828));
#41934=CARTESIAN_POINT('Ctrl Pts',(-2.5213601055814,6.27973185876456,-24.6811302389583));
#41935=CARTESIAN_POINT('Ctrl Pts',(-2.68384231808897,6.21449401458632,-24.6729177170696));
#41936=CARTESIAN_POINT('Ctrl Pts',(-2.8438800747858,6.14291024732061,-24.6647051951809));
#41937=CARTESIAN_POINT('Ctrl Pts',(-3.00095137062681,6.06519413301281,-24.6564926732923));
#41938=CARTESIAN_POINT('Ctrl Pts',(-3.157970141071,5.98750400734744,-24.6482828977104));
#41939=CARTESIAN_POINT('Ctrl Pts',(-3.3120241083009,5.90368577745693,-24.6400731221286));
#41940=CARTESIAN_POINT('Ctrl Pts',(-3.46261291399464,5.81400041347071,-24.6318633465467));
#41941=CARTESIAN_POINT('Ctrl Pts',(-3.52838619199684,5.77482817652375,-24.6282775298641));
#41942=CARTESIAN_POINT('Ctrl Pts',(-3.5934987167778,5.7345372570846,-24.6246917131814));
#41943=CARTESIAN_POINT('Ctrl Pts',(-3.65791030015089,5.69315213533329,-24.6211058964987));
#41944=CARTESIAN_POINT('Ctrl Pts',(-3.81703835178444,5.59091068362489,-24.612247178977));
#41945=CARTESIAN_POINT('Ctrl Pts',(-3.97172164551044,5.48209412690925,-24.6033884614553));
#41946=CARTESIAN_POINT('Ctrl Pts',(-4.12145293553082,5.36711418736405,-24.5945297439335));
#41947=CARTESIAN_POINT('Ctrl Pts',(-4.27146434874709,5.25191913881842,-24.5856544531741));
#41948=CARTESIAN_POINT('Ctrl Pts',(-4.4165050382828,5.13053782208303,-24.5767791624147));
#41949=CARTESIAN_POINT('Ctrl Pts',(-4.55610228615621,5.00342092553506,-24.5679038716552));
#41950=CARTESIAN_POINT('Ctrl Pts',(-4.69609602160113,4.87594298841948,-24.5590033730745));
#41951=CARTESIAN_POINT('Ctrl Pts',(-4.83061518387692,4.74269704823708,-24.5501028744937));
#41952=CARTESIAN_POINT('Ctrl Pts',(-4.95922314274264,4.60417145863247,-24.541202375913));
#41953=CARTESIAN_POINT('Ctrl Pts',(-5.08800519837498,4.46545834675119,-24.5322898287153));
#41954=CARTESIAN_POINT('Ctrl Pts',(-5.21085989449811,4.32145150324707,-24.5233772815177));
#41955=CARTESIAN_POINT('Ctrl Pts',(-5.32739130261227,4.1726719148348,-24.5144647343201));
#41956=CARTESIAN_POINT('Ctrl Pts',(-5.44418002345574,4.02356380656185,-24.5055325073479));
#41957=CARTESIAN_POINT('Ctrl Pts',(-5.5546173685349,3.86966207927037,-24.4966002803756));
#41958=CARTESIAN_POINT('Ctrl Pts',(-5.6583494813666,3.711518576906,-24.4876680534034));
#41959=CARTESIAN_POINT('Ctrl Pts',(-5.75638830654893,3.56205470541254,-24.479226067458));
#41960=CARTESIAN_POINT('Ctrl Pts',(-5.84843801511981,3.40880228570009,-24.4707840815125));
#41961=CARTESIAN_POINT('Ctrl Pts',(-5.93423791843253,3.25224681219577,-24.462342095567));
#41962=CARTESIAN_POINT('Ctrl Pts',(-6.01993194663376,3.09588452455265,-24.4539105268385));
#41963=CARTESIAN_POINT('Ctrl Pts',(-6.09954851351526,2.93593918572723,-24.4454789581099));
#41964=CARTESIAN_POINT('Ctrl Pts',(-6.17278380768894,2.77290985492374,-24.4370473893814));
#41965=CARTESIAN_POINT('Ctrl Pts',(-6.24592343696218,2.61009348407181,-24.4286268345388));
#41966=CARTESIAN_POINT('Ctrl Pts',(-6.31269826743987,2.4442014499328,-24.4202062796963));
#41967=CARTESIAN_POINT('Ctrl Pts',(-6.37284955307715,2.27575868093354,-24.4117857248537));
#41968=CARTESIAN_POINT('Ctrl Pts',(-6.43293074713882,2.10751219068301,-24.4033749821033));
#41969=CARTESIAN_POINT('Ctrl Pts',(-6.48640366561141,1.93672120074102,-24.3949642393529));
#41970=CARTESIAN_POINT('Ctrl Pts',(-6.53305685168915,1.76393230385905,-24.3865534966025));
#41971=CARTESIAN_POINT('Ctrl Pts',(-6.57964837773527,1.59137177656423,-24.3781538700632));
#41972=CARTESIAN_POINT('Ctrl Pts',(-6.61943806093463,1.41681892897331,-24.3697542435239));
#41973=CARTESIAN_POINT('Ctrl Pts',(-6.65226369345949,1.24083711770753,-24.3613546169845));
#41974=CARTESIAN_POINT('Ctrl Pts',(-6.68506370311208,1.0649926734664,-24.3529615469848));
#41975=CARTESIAN_POINT('Ctrl Pts',(-6.71091043242371,0.887721814446482,
-24.344568476985));
#41976=CARTESIAN_POINT('Ctrl Pts',(-6.72969209734646,0.709600785591848,
-24.3361754069852));
#41977=CARTESIAN_POINT('Ctrl Pts',(-6.74845868258237,0.531622769049905,
-24.3277890757313));
#41978=CARTESIAN_POINT('Ctrl Pts',(-6.76017148011533,0.352796274545456,
-24.3194027444774));
#41979=CARTESIAN_POINT('Ctrl Pts',(-6.764770165924,0.173705504301365,-24.3110164132235));
#41980=CARTESIAN_POINT('Ctrl Pts',(-6.76626830751665,0.115362024680058,
-24.3082843475457));
#41981=CARTESIAN_POINT('Ctrl Pts',(-6.76701183699318,0.0569905504860054,
-24.3055522818678));
#41982=CARTESIAN_POINT('Ctrl Pts',(-6.76699985752934,-0.0013885956796133,
-24.3028202161899));
#41983=CARTESIAN_POINT('',(-6.767,5.12853742065664E-10,-24.6971797838342));
#41984=CARTESIAN_POINT('Ctrl Pts',(3.09908550384719,6.01564277861013,-25.348603209574));
#41985=CARTESIAN_POINT('Ctrl Pts',(2.93373232018326,6.10082796552481,-25.3398537616747));
#41986=CARTESIAN_POINT('Ctrl Pts',(2.76486502144422,6.17919158180192,-25.3311043137754));
#41987=CARTESIAN_POINT('Ctrl Pts',(2.59305716434347,6.25046746591381,-25.3223548658761));
#41988=CARTESIAN_POINT('Ctrl Pts',(2.42125069459279,6.32174277447226,-25.3136054886287));
#41989=CARTESIAN_POINT('Ctrl Pts',(2.24650397871055,6.38593035557827,-25.3048561113813));
#41990=CARTESIAN_POINT('Ctrl Pts',(2.06941053323769,6.44281220003539,-25.2961067341338));
#41991=CARTESIAN_POINT('Ctrl Pts',(1.89231845896684,6.49969360406685,-25.2873574246312));
#41992=CARTESIAN_POINT('Ctrl Pts',(1.71287996431508,6.5492692970088,-25.2786081151286));
#41993=CARTESIAN_POINT('Ctrl Pts',(1.53170449173509,6.59137090065478,-25.269858805626));
#41994=CARTESIAN_POINT('Ctrl Pts',(1.35053036178181,6.63347219230081,-25.2611095609615));
#41995=CARTESIAN_POINT('Ctrl Pts',(1.16761955878861,6.66809944062451,-25.2523603162969));
#41996=CARTESIAN_POINT('Ctrl Pts',(0.983593309310713,6.69513503985388,-25.2436110716323));
#41997=CARTESIAN_POINT('Ctrl Pts',(0.799568362460183,6.72217044771212,-25.2348618888991));
#41998=CARTESIAN_POINT('Ctrl Pts',(0.614428268438772,6.74161427235975,-25.2261127061659));
#41999=CARTESIAN_POINT('Ctrl Pts',(0.428801816330421,6.75340047696801,-25.2173635234328));
#42000=CARTESIAN_POINT('Ctrl Pts',(0.243176616522949,6.76518660206241,-25.2086143997246));
#42001=CARTESIAN_POINT('Ctrl Pts',(0.0570653511656382,6.76931519233997,
-25.1998652760165));
#42002=CARTESIAN_POINT('Ctrl Pts',(-0.12889990079984,6.76577222610796,-25.1911161523084));
#42003=CARTESIAN_POINT('Ctrl Pts',(-0.314863959942008,6.76222928260134,
-25.1823670847191));
#42004=CARTESIAN_POINT('Ctrl Pts',(-0.500681721080844,6.75101488651276,
-25.1736180171298));
#42005=CARTESIAN_POINT('Ctrl Pts',(-0.685722110173637,6.73216712415987,
-25.1648689495405));
#42006=CARTESIAN_POINT('Ctrl Pts',(-0.870761373827949,6.71331947644141,
-25.1561199351642));
#42007=CARTESIAN_POINT('Ctrl Pts',(-1.05502298984377,6.68683858439991,-25.1473709207878));
#42008=CARTESIAN_POINT('Ctrl Pts',(-1.23788117676093,6.6528143813142,-25.1386219064115));
#42009=CARTESIAN_POINT('Ctrl Pts',(-1.43009641450781,6.61704912302565,-25.1294251955244));
#42010=CARTESIAN_POINT('Ctrl Pts',(-1.62076048990655,6.57294837083637,-25.1202284846374));
#42011=CARTESIAN_POINT('Ctrl Pts',(-1.8091579895809,6.52067760042893,-25.1110317737504));
#42012=CARTESIAN_POINT('Ctrl Pts',(-1.98840442999994,6.47094578578336,-25.1022817760439));
#42013=CARTESIAN_POINT('Ctrl Pts',(-2.165598959492,6.41381888475486,-25.0935317783374));
#42014=CARTESIAN_POINT('Ctrl Pts',(-2.3401396623936,6.34949095286326,-25.0847817806309));
#42015=CARTESIAN_POINT('Ctrl Pts',(-2.51467682551077,6.2851643255786,-25.0760319603793));
#42016=CARTESIAN_POINT('Ctrl Pts',(-2.68656000075933,6.21363705880919,-25.0672821401277));
#42017=CARTESIAN_POINT('Ctrl Pts',(-2.85520533838011,6.13515211512198,-25.0585323198761));
#42018=CARTESIAN_POINT('Ctrl Pts',(-3.02384747995483,6.05666865882541,-25.0497826654448));
#42019=CARTESIAN_POINT('Ctrl Pts',(-3.18925164681729,5.97122791041344,-25.0410330110136));
#42020=CARTESIAN_POINT('Ctrl Pts',(-3.35085601826389,5.87912008253486,-25.0322833565824));
#42021=CARTESIAN_POINT('Ctrl Pts',(-3.51245754188701,5.78701387779823,-25.0235338563392));
#42022=CARTESIAN_POINT('Ctrl Pts',(-3.67025915508273,5.68824097062701,-25.0147843560961));
#42023=CARTESIAN_POINT('Ctrl Pts',(-3.82372487926228,5.58313684658639,-25.0060348558529));
#42024=CARTESIAN_POINT('Ctrl Pts',(-3.97718810298238,5.47803443503632,-24.9972854981678));
#42025=CARTESIAN_POINT('Ctrl Pts',(-4.12631534260514,5.36660117498307,-24.9885361404827));
#42026=CARTESIAN_POINT('Ctrl Pts',(-4.27060009883765,5.24921554099352,-24.9797867827976));
#42027=CARTESIAN_POINT('Ctrl Pts',(-4.41488269591803,5.13183166362364,-24.9710375560424));
#42028=CARTESIAN_POINT('Ctrl Pts',(-4.55432273232732,5.00849577141613,-24.9622883292872));
#42029=CARTESIAN_POINT('Ctrl Pts',(-4.68844662477907,4.87962675279552,-24.953539102532));
#42030=CARTESIAN_POINT('Ctrl Pts',(-4.82256868832932,4.75075949142141,-24.9447899950805));
#42031=CARTESIAN_POINT('Ctrl Pts',(-4.95137454635713,4.61635945314831,-24.936040887629));
#42032=CARTESIAN_POINT('Ctrl Pts',(-5.07442674459007,4.47688309136938,-24.9272917801775));
#42033=CARTESIAN_POINT('Ctrl Pts',(-5.19747742836518,4.33740844618772,-24.9185427804052));
#42034=CARTESIAN_POINT('Ctrl Pts',(-5.3147744044896,4.19285781738521,-24.9097937806328));
#42035=CARTESIAN_POINT('Ctrl Pts',(-5.42591931529244,4.04372212001968,-24.9010447808604));
#42036=CARTESIAN_POINT('Ctrl Pts',(-5.5370763646114,3.89457013503419,-24.8922948255799));
#42037=CARTESIAN_POINT('Ctrl Pts',(-5.642079832717,3.74083230919091,-24.8835448702993));
#42038=CARTESIAN_POINT('Ctrl Pts',(-5.74057303467049,3.58303087254548,-24.8747949150187));
#42039=CARTESIAN_POINT('Ctrl Pts',(-5.83906243362146,3.42523552890191,-24.8660452975899));
#42040=CARTESIAN_POINT('Ctrl Pts',(-5.93104191766888,3.26337713159788,-24.8572956801611));
#42041=CARTESIAN_POINT('Ctrl Pts',(-6.016199066982,3.09800545293983,-24.8485460627323));
#42042=CARTESIAN_POINT('Ctrl Pts',(-6.10135338094014,2.93263928042444,-24.8397967366269));
#42043=CARTESIAN_POINT('Ctrl Pts',(-6.17968568351558,2.7637603154309,-24.8310474105215));
#42044=CARTESIAN_POINT('Ctrl Pts',(-6.25092992693692,2.59194213834421,-24.8222980844161));
#42045=CARTESIAN_POINT('Ctrl Pts',(-6.32217217689992,2.42012876883723,-24.8135490031223));
#42046=CARTESIAN_POINT('Ctrl Pts',(-6.38632665482822,2.24537661650595,-24.8047999218285));
#42047=CARTESIAN_POINT('Ctrl Pts',(-6.44317547868406,2.06827917624398,-24.7960508405347));
#42048=CARTESIAN_POINT('Ctrl Pts',(-6.50002944235073,1.8911657242639,-24.7873009682197));
#42049=CARTESIAN_POINT('Ctrl Pts',(-6.54957634249617,1.71170683292186,-24.7785510959048));
#42050=CARTESIAN_POINT('Ctrl Pts',(-6.59164787707697,1.53051209228371,-24.7698012235898));
#42051=CARTESIAN_POINT('Ctrl Pts',(-6.63371649074386,1.34932993151087,-24.761051958755));
#42052=CARTESIAN_POINT('Ctrl Pts',(-6.6683107125658,1.16641244177108,-24.7523026939202));
#42053=CARTESIAN_POINT('Ctrl Pts',(-6.69531304839871,0.982380875191491,
-24.7435534290855));
#42054=CARTESIAN_POINT('Ctrl Pts',(-6.72231677032668,0.798339861827445,
-24.7348037151298));
#42055=CARTESIAN_POINT('Ctrl Pts',(-6.74172778477602,0.613184940761843,
-24.7260540011742));
#42056=CARTESIAN_POINT('Ctrl Pts',(-6.75348015835317,0.427545027722295,
-24.7173042872185));
#42057=CARTESIAN_POINT('Ctrl Pts',(-6.76249038364074,0.285219953738662,
-24.7105961194237));
#42058=CARTESIAN_POINT('Ctrl Pts',(-6.76699999998919,0.142609996109865,
-24.703887951629));
#42059=CARTESIAN_POINT('Ctrl Pts',(-6.767,5.12854570784153E-10,-24.6971797838342));
#42060=CARTESIAN_POINT('Ctrl Pts',(-6.767,2.94242285249967E-13,-24.6971797838101));
#42061=CARTESIAN_POINT('Ctrl Pts',(-6.76700000000001,-0.186007249559716,
-24.6884302719974));
#42062=CARTESIAN_POINT('Ctrl Pts',(-6.75932637294248,-0.3720143558159,-24.6796807601846));
#42063=CARTESIAN_POINT('Ctrl Pts',(-6.74400518263364,-0.557389537586276,
-24.6709312483719));
#42064=CARTESIAN_POINT('Ctrl Pts',(-6.7286840570373,-0.742763936382717,
-24.6621817735147));
#42065=CARTESIAN_POINT('Ctrl Pts',(-6.70571545643564,-0.927506130404996,
-24.6534322986575));
#42066=CARTESIAN_POINT('Ctrl Pts',(-6.67517739401574,-1.11098864009548,
-24.6446828238003));
#42067=CARTESIAN_POINT('Ctrl Pts',(-6.64463945804389,-1.2944703900454,-24.6359333851718));
#42068=CARTESIAN_POINT('Ctrl Pts',(-6.60653217002725,-1.47669218339272,
-24.6271839465433));
#42069=CARTESIAN_POINT('Ctrl Pts',(-6.56098496085482,-1.65703510627773,
-24.6184345079148));
#42070=CARTESIAN_POINT('Ctrl Pts',(-6.51543793649556,-1.83737729740012,
-24.6096851047881));
#42071=CARTESIAN_POINT('Ctrl Pts',(-6.46245112156892,-2.01584035544967,
-24.6009357016615));
#42072=CARTESIAN_POINT('Ctrl Pts',(-6.40220448361708,-2.19181813797436,
-24.5921862985348));
#42073=CARTESIAN_POINT('Ctrl Pts',(-6.34195808511964,-2.36779522106327,
-24.5834369301833));
#42074=CARTESIAN_POINT('Ctrl Pts',(-6.27445201416346,-2.54128677725765,
-24.5746875618318));
#42075=CARTESIAN_POINT('Ctrl Pts',(-6.19991555052717,-2.71170355428676,
-24.5659381934802));
#42076=CARTESIAN_POINT('Ctrl Pts',(-6.12537937695099,-2.88211966813562,
-24.5571888591771));
#42077=CARTESIAN_POINT('Ctrl Pts',(-6.04381298028314,-3.04946076419942,
-24.5484395248739));
#42078=CARTESIAN_POINT('Ctrl Pts',(-5.95549339308826,-3.21315848424601,
-24.5396901905707));
#42079=CARTESIAN_POINT('Ctrl Pts',(-5.86717414225632,-3.3768555808539,-24.5309408895891));
#42080=CARTESIAN_POINT('Ctrl Pts',(-5.77210188843868,-3.53690907700326,
-24.5221915886075));
#42081=CARTESIAN_POINT('Ctrl Pts',(-5.67059953311149,-3.69277537024333,
-24.513442287626));
#42082=CARTESIAN_POINT('Ctrl Pts',(-5.56909755592458,-3.84864108281388,
-24.5046930192393));
#42083=CARTESIAN_POINT('Ctrl Pts',(-5.46116568154688,-4.00031938355209,
-24.4959437508527));
#42084=CARTESIAN_POINT('Ctrl Pts',(-5.3471704848807,-4.14729511918561,-24.4871944824661));
#42085=CARTESIAN_POINT('Ctrl Pts',(-5.23317570342983,-4.29427031947572,
-24.4784452459477));
#42086=CARTESIAN_POINT('Ctrl Pts',(-5.1131178195121,-4.43654276249944,-24.4696960094294));
#42087=CARTESIAN_POINT('Ctrl Pts',(-4.98740458928893,-4.57362924412766,
-24.460946772911));
#42088=CARTESIAN_POINT('Ctrl Pts',(-4.8616918065238,-4.71071523781639,-24.4521975675343));
#42089=CARTESIAN_POINT('Ctrl Pts',(-4.73032391141204,-4.84261509584849,
-24.4434483621576));
#42090=CARTESIAN_POINT('Ctrl Pts',(-4.59374706946951,-4.96888084599946,
-24.4346991567809));
#42091=CARTESIAN_POINT('Ctrl Pts',(-4.45717070231163,-5.09514615721042,
-24.4259499818192));
#42092=CARTESIAN_POINT('Ctrl Pts',(-4.31538563497053,-5.21577720520838,
-24.4172008068575));
#42093=CARTESIAN_POINT('Ctrl Pts',(-4.16887340951768,-5.33036429293688,
-24.4084516318958));
#42094=CARTESIAN_POINT('Ctrl Pts',(-4.0223616812227,-5.44495099183863,-24.3997024866226));
#42095=CARTESIAN_POINT('Ctrl Pts',(-3.87112305262993,-5.55349359498058,
-24.3909533413494));
#42096=CARTESIAN_POINT('Ctrl Pts',(-3.71567116928835,-5.65562346357317,
-24.3822041960761));
#42097=CARTESIAN_POINT('Ctrl Pts',(-3.5602198005318,-5.75775299409007,-24.3734550797648));
#42098=CARTESIAN_POINT('Ctrl Pts',(-3.40055544441984,-5.85346967519936,
-24.3647059634534));
#42099=CARTESIAN_POINT('Ctrl Pts',(-3.23722035886776,-5.94244843041419,
-24.3559568471421));
#42100=CARTESIAN_POINT('Ctrl Pts',(-3.07388580043406,-6.03142689847494,
-24.347207759066));
#42101=CARTESIAN_POINT('Ctrl Pts',(-2.90688078789121,-6.11366734707951,
-24.33845867099));
#42102=CARTESIAN_POINT('Ctrl Pts',(-2.73677250610272,-6.18889047001482,
-24.329709582914));
#42103=CARTESIAN_POINT('Ctrl Pts',(-2.56666475916807,-6.26411335643386,
-24.3209605223468));
#42104=CARTESIAN_POINT('Ctrl Pts',(-2.39345402456959,-6.33231884545306,
-24.3122114617797));
#42105=CARTESIAN_POINT('Ctrl Pts',(-2.21772855943924,-6.39327529804931,
-24.3034624012125));
#42106=CARTESIAN_POINT('Ctrl Pts',(-2.04200363223474,-6.45423156404739,
-24.2947133674277));
#42107=CARTESIAN_POINT('Ctrl Pts',(-1.86376426060941,-6.50793874412479,
-24.2859643336429));
#42108=CARTESIAN_POINT('Ctrl Pts',(-1.6836157762162,-6.5542144394333,-24.2772152998581));
#42109=CARTESIAN_POINT('Ctrl Pts',(-1.50346782833139,-6.60048999692605,
-24.2684662921292));
#42110=CARTESIAN_POINT('Ctrl Pts',(-1.32141105657302,-6.63933404265179,
-24.2597172844003));
#42111=CARTESIAN_POINT('Ctrl Pts',(-1.13806375346441,-6.67061465631545,
-24.2509682766714));
#42112=CARTESIAN_POINT('Ctrl Pts',(-0.95471698116888,-6.70189517941787,
-24.242219294272));
#42113=CARTESIAN_POINT('Ctrl Pts',(-0.770079967440963,-6.7256122660902,
-24.2334703118725));
#42114=CARTESIAN_POINT('Ctrl Pts',(-0.584779764071558,-6.74168536995998,
-24.2247213294731));
#42115=CARTESIAN_POINT('Ctrl Pts',(-0.391489587591418,-6.75845153117881,
-24.2155950990575));
#42116=CARTESIAN_POINT('Ctrl Pts',(-0.19747809180367,-6.76689985146399,
-24.2064688686419));
#42117=CARTESIAN_POINT('Ctrl Pts',(-0.00346214752944239,-6.76699911434415,
-24.1973426382262));
#42118=CARTESIAN_POINT('Ctrl Pts',(0.184490798486235,-6.76709527525931,
-24.1885016025111));
#42119=CARTESIAN_POINT('Ctrl Pts',(0.372447602156376,-6.75935633790754,
-24.179660566796));
#42120=CARTESIAN_POINT('Ctrl Pts',(0.559756448195814,-6.743809140145,-24.1708195310809));
#42121=CARTESIAN_POINT('Ctrl Pts',(0.745136131044969,-6.72842206873137,
-24.1620695524675));
#42122=CARTESIAN_POINT('Ctrl Pts',(0.929880851946669,-6.70538686355701,
-24.1533195738542));
#42123=CARTESIAN_POINT('Ctrl Pts',(1.11336305057626,-6.67478177303285,-24.1445695952409));
#42124=CARTESIAN_POINT('Ctrl Pts',(1.29684337090294,-6.64417699581227,-24.1358197062009));
#42125=CARTESIAN_POINT('Ctrl Pts',(1.47906091205368,-6.6060025354802,-24.127069817161));
#42126=CARTESIAN_POINT('Ctrl Pts',(1.65939671095406,-6.56038806441165,-24.118319928121));
#42127=CARTESIAN_POINT('Ctrl Pts',(1.83973072369344,-6.51477404513798,-24.1095701257455));
#42128=CARTESIAN_POINT('Ctrl Pts',(2.01818275357219,-6.46172023288604,-24.10082032337));
#42129=CARTESIAN_POINT('Ctrl Pts',(2.19414664033507,-6.40140683918046,-24.0920705209945));
#42130=CARTESIAN_POINT('Ctrl Pts',(2.37010884271446,-6.34109402281428,-24.083320802375));
#42131=CARTESIAN_POINT('Ctrl Pts',(2.54358267847997,-6.27352185699714,-24.0745710837554));
#42132=CARTESIAN_POINT('Ctrl Pts',(2.71397890841937,-6.19891986435176,-24.0658213651359));
#42133=CARTESIAN_POINT('Ctrl Pts',(2.88437356389145,-6.12431856103148,-24.0570717273641));
#42134=CARTESIAN_POINT('Ctrl Pts',(3.05169040787381,-6.04268767582452,-24.0483220895922));
#42135=CARTESIAN_POINT('Ctrl Pts',(3.21536112512269,-5.95430447953829,-24.0395724518204));
#42136=CARTESIAN_POINT('Ctrl Pts',(3.37903038443055,-5.8659220705492,-24.0308228919883));
#42137=CARTESIAN_POINT('Ctrl Pts',(3.53905332980183,-5.77078760703248,-24.0220733321563));
#42138=CARTESIAN_POINT('Ctrl Pts',(3.69488643042099,-5.66922422085164,-24.0133237723242));
#42139=CARTESIAN_POINT('Ctrl Pts',(3.85071819468949,-5.56766170563015,-24.0045742875242));
#42140=CARTESIAN_POINT('Ctrl Pts',(4.0023599459943,-5.459670534561,-23.9958248027242));
#42141=CARTESIAN_POINT('Ctrl Pts',(4.14929662974506,-5.34561750206525,-23.9870753179242));
#42142=CARTESIAN_POINT('Ctrl Pts',(4.29623210225248,-5.23156540974299,-23.9783259052488));
#42143=CARTESIAN_POINT('Ctrl Pts',(4.43846235842319,-5.11145173172011,-23.9695764925735));
#42144=CARTESIAN_POINT('Ctrl Pts',(4.57550431797629,-4.98568443006378,-23.9608270798981));
#42145=CARTESIAN_POINT('Ctrl Pts',(4.71254519337698,-4.85991812336492,-23.9520777364402));
#42146=CARTESIAN_POINT('Ctrl Pts',(4.8443976431519,-4.7284984763089,-23.9433283929823));
#42147=CARTESIAN_POINT('Ctrl Pts',(4.97061384196894,-4.59187184425118,-23.9345790495244));
#42148=CARTESIAN_POINT('Ctrl Pts',(5.09682908420408,-4.45524624767517,-23.9258297723771));
#42149=CARTESIAN_POINT('Ctrl Pts',(5.21740796650366,-4.31341395556657,-23.9170804952297));
#42150=CARTESIAN_POINT('Ctrl Pts',(5.33194095942439,-4.16685668162616,-23.9083312180823));
#42151=CARTESIAN_POINT('Ctrl Pts',(5.44647312235317,-4.02030046974965,-23.8995820043388));
#42152=CARTESIAN_POINT('Ctrl Pts',(5.55495930712468,-3.86901957035289,-23.8908327905953));
#42153=CARTESIAN_POINT('Ctrl Pts',(5.6570310607997,-3.71352778058107,-23.8820835768517));
#42154=CARTESIAN_POINT('Ctrl Pts',(5.75910210868896,-3.55803706597342,-23.8733344236055));
#42155=CARTESIAN_POINT('Ctrl Pts',(5.85475865698696,-3.39833575880646,-23.8645852703593));
#42156=CARTESIAN_POINT('Ctrl Pts',(5.94367583069196,-3.23496624706475,-23.8558361171131));
#42157=CARTESIAN_POINT('Ctrl Pts',(6.032592419102,-3.07159781069858,-23.847087021458));
#42158=CARTESIAN_POINT('Ctrl Pts',(6.1147695847108,-2.90456146975597,-23.8383379258029));
#42159=CARTESIAN_POINT('Ctrl Pts',(6.18992823574488,-2.73442451648025,-23.8295888301478));
#42160=CARTESIAN_POINT('Ctrl Pts',(6.26508641701032,-2.56428862662178,-23.8208397891777));
#42161=CARTESIAN_POINT('Ctrl Pts',(6.33322605570389,-2.39105242531033,-23.8120907482076));
#42162=CARTESIAN_POINT('Ctrl Pts',(6.39411573747854,-2.21530425353479,-23.8033417072374));
#42163=CARTESIAN_POINT('Ctrl Pts',(6.45500505889202,-2.03955712188319,-23.7945927180464));
#42164=CARTESIAN_POINT('Ctrl Pts',(6.50864441544996,-1.86129832025337,-23.7858437288555));
#42165=CARTESIAN_POINT('Ctrl Pts',(6.55485164049965,-1.68113324012082,-23.7770947396645));
#42166=CARTESIAN_POINT('Ctrl Pts',(6.60199852639162,-1.49730435912667,-23.7681678327876));
#42167=CARTESIAN_POINT('Ctrl Pts',(6.64140767441057,-1.31149113173415,-23.7592409259107));
#42168=CARTESIAN_POINT('Ctrl Pts',(6.67293975269643,-1.12435050446191,-23.7503140190338));
#42169=CARTESIAN_POINT('Ctrl Pts',(6.7038466483154,-0.940920291561387,-23.7415641048498));
#42170=CARTESIAN_POINT('Ctrl Pts',(6.72718585889692,-0.756215114275625,
-23.7328141906658));
#42171=CARTESIAN_POINT('Ctrl Pts',(6.74287810451883,-0.570862389372871,
-23.7240642764818));
#42172=CARTESIAN_POINT('Ctrl Pts',(6.75857004154136,-0.385513309565883,
-23.7153145343713));
#42173=CARTESIAN_POINT('Ctrl Pts',(6.76661529035562,-0.199516993257048,
-23.7065647922607));
#42174=CARTESIAN_POINT('Ctrl Pts',(6.76698652348897,-0.0135052182029489,
-23.6978150501501));
#42175=CARTESIAN_POINT('Ctrl Pts',(6.76735774981518,0.172503146039984,-23.6890654684794));
#42176=CARTESIAN_POINT('Ctrl Pts',(6.76005524147474,0.358526681834546,-23.6803158868088));
#42177=CARTESIAN_POINT('Ctrl Pts',(6.74510380214873,0.543933542115922,-23.6715663051382));
#42178=CARTESIAN_POINT('Ctrl Pts',(6.73015261710968,0.729337249085736,-23.6628168722762));
#42179=CARTESIAN_POINT('Ctrl Pts',(6.70755278444592,0.914124015855634,-23.6540674394143));
#42180=CARTESIAN_POINT('Ctrl Pts',(6.67738106408274,1.09766621749478,-23.6453180065524));
#42181=CARTESIAN_POINT('Ctrl Pts',(6.64720981677236,1.28120554143416,-23.63656871087));
#42182=CARTESIAN_POINT('Ctrl Pts',(6.60946696581501,1.46350005650716,-23.6278194151877));
#42183=CARTESIAN_POINT('Ctrl Pts',(6.5642807001097,1.64393062206632,-23.6190701195053));
#42184=CARTESIAN_POINT('Ctrl Pts',(6.51909508282715,1.82435859844743,-23.6103209493753));
#42185=CARTESIAN_POINT('Ctrl Pts',(6.46646633415636,2.00292240086646,-23.6015717792454));
#42186=CARTESIAN_POINT('Ctrl Pts',(6.40657319597167,2.17901557696529,-23.5928226091154));
#42187=CARTESIAN_POINT('Ctrl Pts',(6.34668083768268,2.35510646007506,-23.5840735529123));
#42188=CARTESIAN_POINT('Ctrl Pts',(6.27952437143857,2.528726509966,-23.5753244967092));
#42189=CARTESIAN_POINT('Ctrl Pts',(6.20533187335107,2.69928607997991,-23.5665754405061));
#42190=CARTESIAN_POINT('Ctrl Pts',(6.12831449784224,2.87633970115458,-23.5574932642173));
#42191=CARTESIAN_POINT('Ctrl Pts',(6.04371489463125,3.05009490562404,-23.5484110879285));
#42192=CARTESIAN_POINT('Ctrl Pts',(5.95184265120464,3.21991584599681,-23.5393289116396));
#42193=CARTESIAN_POINT('Ctrl Pts',(5.8633328133546,3.38352155905357,-23.5305791312852));
#42194=CARTESIAN_POINT('Ctrl Pts',(5.76807337235647,3.54347560903886,-23.5218293509308));
#42195=CARTESIAN_POINT('Ctrl Pts',(5.66638790086311,3.69923467178715,-23.5130795705764));
#42196=CARTESIAN_POINT('Ctrl Pts',(5.56470608502697,3.85498813489831,-23.5043301047821));
#42197=CARTESIAN_POINT('Ctrl Pts',(5.45659885766904,4.00654667256326,-23.4955806389878));
#42198=CARTESIAN_POINT('Ctrl Pts',(5.34243340580458,4.15339551506275,-23.4868311731936));
#42199=CARTESIAN_POINT('Ctrl Pts',(5.22827145140539,4.30023985883937,-23.4780819754397));
#42200=CARTESIAN_POINT('Ctrl Pts',(5.1080518197803,4.44237456993111,-23.4693327776858));
#42201=CARTESIAN_POINT('Ctrl Pts',(4.98218281282487,4.57931691626519,-23.460583579932));
#42202=CARTESIAN_POINT('Ctrl Pts',(4.8563169929617,4.71625579512222,-23.451834603714));
#42203=CARTESIAN_POINT('Ctrl Pts',(4.72480227791784,4.84800236135822,-23.443085627496));
#42204=CARTESIAN_POINT('Ctrl Pts',(4.58808530848065,4.97410918678953,-23.434336651278));
#42205=CARTESIAN_POINT('Ctrl Pts',(4.45135945056915,5.10022421089058,-23.4255871062568));
#42206=CARTESIAN_POINT('Ctrl Pts',(4.30943087207976,5.22069856612039,-23.4168375612356));
#42207=CARTESIAN_POINT('Ctrl Pts',(4.16278164322396,5.3351230530174,-23.4080880162144));
#42208=CARTESIAN_POINT('Ctrl Pts',(4.01614103534315,5.44954081331483,-23.3993389855471));
#42209=CARTESIAN_POINT('Ctrl Pts',(3.86478055833334,5.55790924068393,-23.3905899548798));
#42210=CARTESIAN_POINT('Ctrl Pts',(3.70921425811868,5.65986029751345,-23.3818409242126));
#42211=CARTESIAN_POINT('Ctrl Pts',(3.5536458453004,5.76181273884703,-23.3730917747327));
#42212=CARTESIAN_POINT('Ctrl Pts',(3.39387173464268,5.85734747818107,-23.3643426252529));
#42213=CARTESIAN_POINT('Ctrl Pts',(3.23043456092332,5.94614005448847,-23.355593475773));
#42214=CARTESIAN_POINT('Ctrl Pts',(3.18690768806344,5.96978744811307,-23.35326338704));
#42215=CARTESIAN_POINT('Ctrl Pts',(3.14312114982858,5.99295688499312,-23.350933298307));
#42216=CARTESIAN_POINT('Ctrl Pts',(3.09908550384722,6.01564277861012,-23.348603209574));
#42217=CARTESIAN_POINT('Origin',(0.,0.,-63.6971797838103));
#42218=CARTESIAN_POINT('',(3.09908550384717,6.01564277861014,-20.9542113918581));
#42219=CARTESIAN_POINT('',(3.09908550384722,6.01564277861012,-21.3487227114526));
#42220=CARTESIAN_POINT('',(3.09908550384721,6.01564277861012,-63.6971797838103));
#42221=CARTESIAN_POINT('',(-6.7669985214907,-0.00447326979864322,-22.3028202162209));
#42222=CARTESIAN_POINT('Ctrl Pts',(-6.76699852149027,-0.00447327045386464,
-22.30282021619));
#42223=CARTESIAN_POINT('Ctrl Pts',(-6.76683979782902,-0.244584569803976,
-22.2915000487806));
#42224=CARTESIAN_POINT('Ctrl Pts',(-6.75389750641668,-0.484287776517787,
-22.2801798813713));
#42225=CARTESIAN_POINT('Ctrl Pts',(-6.72832438920961,-0.722454090975468,
-22.2688597139619));
#42226=CARTESIAN_POINT('Ctrl Pts',(-6.70632789425158,-0.927310780628065,
-22.2591227701499));
#42227=CARTESIAN_POINT('Ctrl Pts',(-6.67498738865535,-1.13103108037173,
-22.2493858263378));
#42228=CARTESIAN_POINT('Ctrl Pts',(-6.63442894834782,-1.33290717205828,
-22.2396488825258));
#42229=CARTESIAN_POINT('Ctrl Pts',(-6.60017265787884,-1.50341486375258,
-22.2314249081082));
#42230=CARTESIAN_POINT('Ctrl Pts',(-6.55929354599552,-1.67282715905326,
-22.2232009336907));
#42231=CARTESIAN_POINT('Ctrl Pts',(-6.51187460497495,-1.8405917877363,-22.2149769592731));
#42232=CARTESIAN_POINT('Ctrl Pts',(-6.46450574295683,-2.00817924069444,
-22.2067616701705));
#42233=CARTESIAN_POINT('Ctrl Pts',(-6.41061090207985,-2.17412214992992,
-22.1985463810678));
#42234=CARTESIAN_POINT('Ctrl Pts',(-6.35032426429631,-2.33787740018367,
-22.1903310919651));
#42235=CARTESIAN_POINT('Ctrl Pts',(-6.29008920283704,-2.50149255481757,
-22.1821228311929));
#42236=CARTESIAN_POINT('Ctrl Pts',(-6.22347335833223,-2.66292344329954,
-22.1739145704208));
#42237=CARTESIAN_POINT('Ctrl Pts',(-6.15066101690496,-2.82164102166197,
-22.1657063096486));
#42238=CARTESIAN_POINT('Ctrl Pts',(-6.07789636732612,-2.98025464052329,
-22.1575034252607));
#42239=CARTESIAN_POINT('Ctrl Pts',(-5.99894345429057,-3.13615816451053,
-22.1493005408728));
#42240=CARTESIAN_POINT('Ctrl Pts',(-5.91403510308101,-3.28884140686741,
-22.141097656485));
#42241=CARTESIAN_POINT('Ctrl Pts',(-5.82916534409085,-3.44145525222029,
-22.1328985004407));
#42242=CARTESIAN_POINT('Ctrl Pts',(-5.73834571358609,-3.59085141920646,
-22.1246993443966));
#42243=CARTESIAN_POINT('Ctrl Pts',(-5.64185554690849,-3.73654318693334,
-22.1165001883523));
#42244=CARTESIAN_POINT('Ctrl Pts',(-5.54537377252907,-3.88222228301916,
-22.1083017454353));
#42245=CARTESIAN_POINT('Ctrl Pts',(-5.44322263509805,-4.02419731815061,
-22.1001033025183));
#42246=CARTESIAN_POINT('Ctrl Pts',(-5.33572567249588,-4.16200919603362,
-22.0919048596013));
#42247=CARTESIAN_POINT('Ctrl Pts',(-5.2282297804362,-4.29981970147346,-22.0837064983311));
#42248=CARTESIAN_POINT('Ctrl Pts',(-5.1153883890271,-4.43346684876428,-22.0755081370609));
#42249=CARTESIAN_POINT('Ctrl Pts',(-4.99756625548406,-4.56252348180774,
-22.0673097757907));
#42250=CARTESIAN_POINT('Ctrl Pts',(-4.87972389207549,-4.69160227366172,
-22.0591100068754));
#42251=CARTESIAN_POINT('Ctrl Pts',(-4.75689932460476,-4.81608871606268,
-22.0509102379601));
#42252=CARTESIAN_POINT('Ctrl Pts',(-4.62949523045415,-4.93559144492353,
-22.0427104690448));
#42253=CARTESIAN_POINT('Ctrl Pts',(-4.50204611712428,-5.05513640095774,
-22.0345078026805));
#42254=CARTESIAN_POINT('Ctrl Pts',(-4.37001451507296,-5.16969389020239,
-22.0263051363162));
#42255=CARTESIAN_POINT('Ctrl Pts',(-4.23383735478326,-5.27891184367024,
-22.0181024699518));
#42256=CARTESIAN_POINT('Ctrl Pts',(-4.09750553127736,-5.38825384143387,
-22.0098904874088));
#42257=CARTESIAN_POINT('Ctrl Pts',(-3.95701902333565,-5.49224396332791,
-22.0016785048658));
#42258=CARTESIAN_POINT('Ctrl Pts',(-3.81284586685571,-5.59057200969645,
-21.9934665223228));
#42259=CARTESIAN_POINT('Ctrl Pts',(-3.66858767509963,-5.6889580512756,-21.9852496962415));
#42260=CARTESIAN_POINT('Ctrl Pts',(-3.52063880381534,-5.7816751702197,-21.9770328701602));
#42261=CARTESIAN_POINT('Ctrl Pts',(-3.369493126046,-5.8684584921024,-21.9688160440789));
#42262=CARTESIAN_POINT('Ctrl Pts',(-3.2181143598121,-5.95537564640125,-21.960586546465));
#42263=CARTESIAN_POINT('Ctrl Pts',(-3.06352925281743,-6.03634055079179,
-21.9523570488512));
#42264=CARTESIAN_POINT('Ctrl Pts',(-2.9062541465771,-6.11113539659395,-21.9441275512373));
#42265=CARTESIAN_POINT('Ctrl Pts',(-2.76606581816127,-6.17780433523132,
-21.9367921277125));
#42266=CARTESIAN_POINT('Ctrl Pts',(-2.62374067824165,-6.23957167109107,
-21.9294567041876));
#42267=CARTESIAN_POINT('Ctrl Pts',(-2.47965458072791,-6.29631655496093,
-21.9221212806628));
#42268=CARTESIAN_POINT('Ctrl Pts',(-2.32112246806096,-6.35875065844598,
-21.9140504104764));
#42269=CARTESIAN_POINT('Ctrl Pts',(-2.15994130847932,-6.41530737282659,
-21.90597954029));
#42270=CARTESIAN_POINT('Ctrl Pts',(-1.99659536623688,-6.46574790287415,
-21.8979086701036));
#42271=CARTESIAN_POINT('Ctrl Pts',(-1.83345269532306,-6.51612566360269,
-21.8898478434878));
#42272=CARTESIAN_POINT('Ctrl Pts',(-1.66815095386152,-6.56040227556719,
-21.881787016872));
#42273=CARTESIAN_POINT('Ctrl Pts',(-1.50119630741602,-6.59838606377351,
-21.8737261902562));
#42274=CARTESIAN_POINT('Ctrl Pts',(-1.33441281244487,-6.63633091337291,
-21.8656736270963));
#42275=CARTESIAN_POINT('Ctrl Pts',(-1.16598014516901,-6.66799569491895,
-21.8576210639364));
#42276=CARTESIAN_POINT('Ctrl Pts',(-0.996421543867331,-6.69323786421169,
-21.8495685007765));
#42277=CARTESIAN_POINT('Ctrl Pts',(-0.826999636405796,-6.71845968390831,
-21.8415224293886));
#42278=CARTESIAN_POINT('Ctrl Pts',(-0.656453968629374,-6.73726914223733,
-21.8334763580008));
#42279=CARTESIAN_POINT('Ctrl Pts',(-0.48531983937667,-6.74957433128249,
-21.8254302866129));
#42280=CARTESIAN_POINT('Ctrl Pts',(-0.314286240472433,-6.7618722918166,
-21.817388941777));
#42281=CARTESIAN_POINT('Ctrl Pts',(-0.142665239355296,-6.76767356261957,
-21.8093475969411));
#42282=CARTESIAN_POINT('Ctrl Pts',(0.0290009467029128,-6.76693785586142,
-21.8013062521052));
#42283=CARTESIAN_POINT('Ctrl Pts',(0.203976328610638,-6.76618796694074,
-21.7931098948842));
#42284=CARTESIAN_POINT('Ctrl Pts',(0.378998263215142,-6.75864644712516,
-21.7849135376631));
#42285=CARTESIAN_POINT('Ctrl Pts',(0.553490139944152,-6.7443263314422,-21.7767171804421));
#42286=CARTESIAN_POINT('Ctrl Pts',(0.724627547763495,-6.73028150870549,
-21.7686783917336));
#42287=CARTESIAN_POINT('Ctrl Pts',(0.895254709047074,-6.70971640581834,
-21.7606396030251));
#42288=CARTESIAN_POINT('Ctrl Pts',(1.0648310349809,-6.68269585324228,-21.7526008143166));
#42289=CARTESIAN_POINT('Ctrl Pts',(1.234425507118,-6.65567240922228,-21.7445611653848));
#42290=CARTESIAN_POINT('Ctrl Pts',(1.40296855114293,-6.62219219871555,-21.7365215164531));
#42291=CARTESIAN_POINT('Ctrl Pts',(1.56992836752977,-6.58237145114322,-21.7284818675214));
#42292=CARTESIAN_POINT('Ctrl Pts',(1.73693910881058,-6.54253855773011,-21.7204397663932));
#42293=CARTESIAN_POINT('Ctrl Pts',(1.90236529815806,-6.4963613643341,-21.7123976652651));
#42294=CARTESIAN_POINT('Ctrl Pts',(2.06568907075119,-6.44400633635467,-21.7043555641369));
#42295=CARTESIAN_POINT('Ctrl Pts',(2.23452437898895,-6.38988453187784,-21.6960420736921));
#42296=CARTESIAN_POINT('Ctrl Pts',(2.40111247499271,-6.32916077531904,-21.6877285832474));
#42297=CARTESIAN_POINT('Ctrl Pts',(2.56490343797082,-6.26207308755539,-21.6794150928026));
#42298=CARTESIAN_POINT('Ctrl Pts',(2.72362665182019,-6.19706111608909,-21.6713588246319));
#42299=CARTESIAN_POINT('Ctrl Pts',(2.87972293892313,-6.12607337260562,-21.6633025564611));
#42300=CARTESIAN_POINT('Ctrl Pts',(3.03271720490066,-6.04937313736717,-21.6552462882903));
#42301=CARTESIAN_POINT('Ctrl Pts',(3.19303872193976,-5.96899954955905,-21.6468041867086));
#42302=CARTESIAN_POINT('Ctrl Pts',(3.34995335952171,-5.88235308065762,-21.6383620851268));
#42303=CARTESIAN_POINT('Ctrl Pts',(3.50294945914151,-5.78978705020316,-21.6299199835451));
#42304=CARTESIAN_POINT('Ctrl Pts',(3.65594555876131,-5.6972210197487,-21.6214778819633));
#42305=CARTESIAN_POINT('Ctrl Pts',(3.80502278354149,-5.59873575392552,-21.6130357803815));
#42306=CARTESIAN_POINT('Ctrl Pts',(3.94971058606822,-5.49473159365411,-21.6045936787998));
#42307=CARTESIAN_POINT('Ctrl Pts',(4.09254295714659,-5.39206115043665,-21.5962598361071));
#42308=CARTESIAN_POINT('Ctrl Pts',(4.23155224880822,-5.28368659903462,-21.5879259934144));
#42309=CARTESIAN_POINT('Ctrl Pts',(4.3662605840787,-5.1699185208203,-21.5795921507217));
#42310=CARTESIAN_POINT('Ctrl Pts',(4.50081014853403,-5.05628453267902,-21.571268130517));
#42311=CARTESIAN_POINT('Ctrl Pts',(4.6310685914594,-4.93726990388134,-21.5629441103122));
#42312=CARTESIAN_POINT('Ctrl Pts',(4.75658755455274,-4.81322800580587,-21.5546200901075));
#42313=CARTESIAN_POINT('Ctrl Pts',(4.88198159138795,-4.68930956389827,-21.5463043546166));
#42314=CARTESIAN_POINT('Ctrl Pts',(5.00264530054966,-4.56037406439998,-21.5379886191258));
#42315=CARTESIAN_POINT('Ctrl Pts',(5.11816376418442,-4.42681473330313,-21.5296728836349));
#42316=CARTESIAN_POINT('Ctrl Pts',(5.23358842080311,-4.29336385934743,-21.5213639009549));
#42317=CARTESIAN_POINT('Ctrl Pts',(5.34387593080243,-4.15529689752791,-21.5130549182748));
#42318=CARTESIAN_POINT('Ctrl Pts',(5.44864843940284,-4.01304363093563,-21.5047459355948));
#42319=CARTESIAN_POINT('Ctrl Pts',(5.55335505375238,-3.87087983125181,-21.4964421786577));
#42320=CARTESIAN_POINT('Ctrl Pts',(5.65255337342312,-3.72453525312796,-21.4881384217205));
#42321=CARTESIAN_POINT('Ctrl Pts',(5.74590589694503,-3.57447260773562,-21.4798346647833));
#42322=CARTESIAN_POINT('Ctrl Pts',(5.83922052159282,-3.4244708841598,-21.4715342789713));
#42323=CARTESIAN_POINT('Ctrl Pts',(5.9266938955467,-3.27075439587046,-21.4632338931593));
#42324=CARTESIAN_POINT('Ctrl Pts',(6.00803176401268,-3.11381491463681,-21.4549335073473));
#42325=CARTESIAN_POINT('Ctrl Pts',(6.08935248043865,-2.95690852785613,-21.4466348718706));
#42326=CARTESIAN_POINT('Ctrl Pts',(6.16454010903527,-2.79678081075611,-21.438336236394));
#42327=CARTESIAN_POINT('Ctrl Pts',(6.23334618431693,-2.63394843276431,-21.4300376009174));
#42328=CARTESIAN_POINT('Ctrl Pts',(6.30214917120639,-2.47112336357837,-21.4217393379288));
#42329=CARTESIAN_POINT('Ctrl Pts',(6.36457104038087,-2.30559419582851,-21.4134410749402));
#42330=CARTESIAN_POINT('Ctrl Pts',(6.42041126945608,-2.13789806376296,-21.4051428119516));
#42331=CARTESIAN_POINT('Ctrl Pts',(6.47625826054463,-1.97018162441175,-21.3968435440788));
#42332=CARTESIAN_POINT('Ctrl Pts',(6.52552191410141,-1.80029802800402,-21.388544276206));
#42333=CARTESIAN_POINT('Ctrl Pts',(6.56805136520168,-1.62880025296914,-21.3802450083332));
#42334=CARTESIAN_POINT('Ctrl Pts',(6.61061067883143,-1.45718205885458,-21.3719399130367));
#42335=CARTESIAN_POINT('Ctrl Pts',(6.64642625782737,-1.28394775932448,-21.3636348177402));
#42336=CARTESIAN_POINT('Ctrl Pts',(6.67539803959756,-1.10966211656387,-21.3553297224437));
#42337=CARTESIAN_POINT('Ctrl Pts',(6.70438038598591,-0.935312920195172,
-21.3470215986776));
#42338=CARTESIAN_POINT('Ctrl Pts',(6.72651391134347,-0.759911960716135,
-21.3387134749115));
#42339=CARTESIAN_POINT('Ctrl Pts',(6.74175035679169,-0.5840300734544,-21.3304053511454));
#42340=CARTESIAN_POINT('Ctrl Pts',(6.7570029984934,-0.407961224762586,-21.3220883958917));
#42341=CARTESIAN_POINT('Ctrl Pts',(6.76534388934378,-0.231410774170983,
-21.3137714406381));
#42342=CARTESIAN_POINT('Ctrl Pts',(6.7667768782302,-0.0549516173484228,
-21.3054544853844));
#42343=CARTESIAN_POINT('Ctrl Pts',(6.76783296923709,0.075096096469244,-21.2993250159018));
#42344=CARTESIAN_POINT('Ctrl Pts',(6.76513814630155,0.205094195796902,-21.2931955464192));
#42345=CARTESIAN_POINT('Ctrl Pts',(6.75871200404309,0.334814943519255,-21.2870660769367));
#42346=CARTESIAN_POINT('Ctrl Pts',(6.74985194208228,0.513667794296063,-21.2786150534115));
#42347=CARTESIAN_POINT('Ctrl Pts',(6.7338807044077,0.692320057028802,-21.2701640298863));
#42348=CARTESIAN_POINT('Ctrl Pts',(6.71081733390735,0.87018372251419,-21.2617130063611));
#42349=CARTESIAN_POINT('Ctrl Pts',(6.68777427001924,1.04789078432853,-21.2532694237109));
#42350=CARTESIAN_POINT('Ctrl Pts',(6.65765156203011,1.22481030563259,-21.2448258410608));
#42351=CARTESIAN_POINT('Ctrl Pts',(6.62052018187237,1.40035764054068,-21.2363822584106));
#42352=CARTESIAN_POINT('Ctrl Pts',(6.58341644718391,1.57577427498913,-21.2279449622708));
#42353=CARTESIAN_POINT('Ctrl Pts',(6.53931451088454,1.74982043637239,-21.219507666131));
#42354=CARTESIAN_POINT('Ctrl Pts',(6.48833678684317,1.92191954579207,-21.2110703699911));
#42355=CARTESIAN_POINT('Ctrl Pts',(6.437395431521,2.09389587561929,-21.2026390932188));
#42356=CARTESIAN_POINT('Ctrl Pts',(6.37958816691832,2.26392760715644,-21.1942078164464));
#42357=CARTESIAN_POINT('Ctrl Pts',(6.31508787128656,2.43145104370404,-21.1857765396741));
#42358=CARTESIAN_POINT('Ctrl Pts',(6.25061522281635,2.59890267364255,-21.1773488768521));
#42359=CARTESIAN_POINT('Ctrl Pts',(6.17945538143675,2.76384784316277,-21.1689212140302));
#42360=CARTESIAN_POINT('Ctrl Pts',(6.10183041101897,2.92574001496443,-21.1604935512083));
#42361=CARTESIAN_POINT('Ctrl Pts',(6.02422933663726,3.08758234995257,-21.1520684827543));
#42362=CARTESIAN_POINT('Ctrl Pts',(5.94016724537731,3.24637326293725,-21.1436434143003));
#42363=CARTESIAN_POINT('Ctrl Pts',(5.84991363060396,3.40158779314513,-21.1352183458463));
#42364=CARTESIAN_POINT('Ctrl Pts',(5.82521747901043,3.44405923960365,-21.1329129892326));
#42365=CARTESIAN_POINT('Ctrl Pts',(5.80005801344589,3.4862630452555,-21.130607632619));
#42366=CARTESIAN_POINT('Ctrl Pts',(5.77444135510304,3.52818877562919,-21.1283022760053));
#42367=CARTESIAN_POINT('Ctrl Pts',(5.67866889066826,3.68493562634545,-21.1196832874808));
#42368=CARTESIAN_POINT('Ctrl Pts',(5.57654527277411,3.83772354106652,-21.1110642989564));
#42369=CARTESIAN_POINT('Ctrl Pts',(5.46842726088112,3.98604971023345,-21.1024453104319));
#42370=CARTESIAN_POINT('Ctrl Pts',(5.36024447665021,4.13446474001282,-21.0938211583641));
#42371=CARTESIAN_POINT('Ctrl Pts',(5.2460603106858,4.27841244399173,-21.0851970062963));
#42372=CARTESIAN_POINT('Ctrl Pts',(5.12627253381604,4.41742220180993,-21.0765728542285));
#42373=CARTESIAN_POINT('Ctrl Pts',(5.0023819933623,4.56119308123083,-21.0676533226323));
#42374=CARTESIAN_POINT('Ctrl Pts',(4.87249743537002,4.69968150795205,-21.058733791036));
#42375=CARTESIAN_POINT('Ctrl Pts',(4.7371007621332,4.83240782316612,-21.0498142594398));
#42376=CARTESIAN_POINT('Ctrl Pts',(4.60594401454381,4.9609778345766,-21.0411740415805));
#42377=CARTESIAN_POINT('Ctrl Pts',(4.46961540632021,5.08414098228172,-21.0325338237213));
#42378=CARTESIAN_POINT('Ctrl Pts',(4.32858746846222,5.20150166085447,-21.023893605862));
#42379=CARTESIAN_POINT('Ctrl Pts',(4.1807209807577,5.32455324622649,-21.0148344173973));
#42380=CARTESIAN_POINT('Ctrl Pts',(4.02768839344572,5.4412254049512,-21.0057752289326));
#42381=CARTESIAN_POINT('Ctrl Pts',(3.87006994481229,5.551112286944,-20.9967160404678));
#42382=CARTESIAN_POINT('Ctrl Pts',(3.71245149617885,5.6609991689368,-20.9876568520031));
#42383=CARTESIAN_POINT('Ctrl Pts',(3.55024752690922,5.76410059690113,-20.9785976635383));
#42384=CARTESIAN_POINT('Ctrl Pts',(3.38406977779038,5.86006490911541,-20.9695384750736));
#42385=CARTESIAN_POINT('Ctrl Pts',(3.29035203109883,5.91418502538377,-20.9644294473351));
#42386=CARTESIAN_POINT('Ctrl Pts',(3.19532225413756,5.96606438296092,-20.9593204195966));
#42387=CARTESIAN_POINT('Ctrl Pts',(3.09908550384717,6.01564277861014,-20.9542113918581));
#42388=CARTESIAN_POINT('Ctrl Pts',(3.09908550384719,6.01564277861013,-22.9543563216829));
#42389=CARTESIAN_POINT('Ctrl Pts',(2.94506750066652,6.09498840775651,-22.9462261559891));
#42390=CARTESIAN_POINT('Ctrl Pts',(2.78807281632298,6.16837786125163,-22.9380959902953));
#42391=CARTESIAN_POINT('Ctrl Pts',(2.62861170812857,6.23559856692919,-22.9299658246015));
#42392=CARTESIAN_POINT('Ctrl Pts',(2.46907887916276,6.30284950644195,-22.9218320022057));
#42393=CARTESIAN_POINT('Ctrl Pts',(2.3070777574783,6.36392603961682,-22.91369817981));
#42394=CARTESIAN_POINT('Ctrl Pts',(2.14313547521938,6.41866491841226,-22.9055643574142));
#42395=CARTESIAN_POINT('Ctrl Pts',(1.97902262328357,6.47346074891498,-22.8974220723848));
#42396=CARTESIAN_POINT('Ctrl Pts',(1.81296492893481,6.52190565783806,-22.8892797873555));
#42397=CARTESIAN_POINT('Ctrl Pts',(1.64550205599884,6.5638869569565,-22.8811375023261));
#42398=CARTESIAN_POINT('Ctrl Pts',(1.60139656903797,6.57494376977958,-22.8789930303014));
#42399=CARTESIAN_POINT('Ctrl Pts',(1.55719365224243,6.58555250370754,-22.8768485582767));
#42400=CARTESIAN_POINT('Ctrl Pts',(1.51290324157315,6.59571169637041,-22.8747040862519));
#42401=CARTESIAN_POINT('Ctrl Pts',(1.33857467565615,6.63569862494095,-22.8662633712739));
#42402=CARTESIAN_POINT('Ctrl Pts',(1.16253102035022,6.66879946415491,-22.8578226562958));
#42403=CARTESIAN_POINT('Ctrl Pts',(0.985343015162563,6.69487775410951,-22.8493819413177));
#42404=CARTESIAN_POINT('Ctrl Pts',(0.8082889370173,6.7209363328639,-22.8409476062297));
#42405=CARTESIAN_POINT('Ctrl Pts',(0.630092561903329,6.73998289511041,-22.8325132711417));
#42406=CARTESIAN_POINT('Ctrl Pts',(0.451334955646914,6.75193200186519,-22.8240789360536));
#42407=CARTESIAN_POINT('Ctrl Pts',(0.272685012540239,6.76387391184386,-22.815649680845));
#42408=CARTESIAN_POINT('Ctrl Pts',(0.0934748440294833,6.76872686639846,
-22.8072204256364));
#42409=CARTESIAN_POINT('Ctrl Pts',(-0.0857088242301413,6.76645719689773,
-22.7987911704278));
#42410=CARTESIAN_POINT('Ctrl Pts',(-0.264812058153802,6.76418854623628,
-22.7903656990548));
#42411=CARTESIAN_POINT('Ctrl Pts',(-0.443888482710617,6.75480365081094,
-22.7819402276818));
#42412=CARTESIAN_POINT('Ctrl Pts',(-0.622350428176236,6.73832092917433,
-22.7735147563087));
#42413=CARTESIAN_POINT('Ctrl Pts',(-0.800759615113575,6.72184308030841,
-22.7650917757495));
#42414=CARTESIAN_POINT('Ctrl Pts',(-0.978554353579318,6.6982716203976,-22.7566687951903));
#42415=CARTESIAN_POINT('Ctrl Pts',(-1.15515075464894,6.66767693683745,-22.748245814631));
#42416=CARTESIAN_POINT('Ctrl Pts',(-1.33175007978853,6.63708174669282,-22.7398226946047));
#42417=CARTESIAN_POINT('Ctrl Pts',(-1.5071506983219,6.59946315094049,-22.7313995745784));
#42418=CARTESIAN_POINT('Ctrl Pts',(-1.68077692221323,6.55494301559941,-22.722976454552));
#42419=CARTESIAN_POINT('Ctrl Pts',(-1.85440915038874,6.51042134067785,-22.7145530432402));
#42420=CARTESIAN_POINT('Ctrl Pts',(-2.02626653847878,6.45899773296964,-22.7061296319283));
#42421=CARTESIAN_POINT('Ctrl Pts',(-2.19578646472837,6.40084453813055,-22.6977062206165));
#42422=CARTESIAN_POINT('Ctrl Pts',(-2.36533589530772,6.34268122193833,-22.6892813432404));
#42423=CARTESIAN_POINT('Ctrl Pts',(-2.5325467375133,6.2777860916801,-22.6808564658643));
#42424=CARTESIAN_POINT('Ctrl Pts',(-2.69687397725934,6.20638056767238,-22.6724315884881));
#42425=CARTESIAN_POINT('Ctrl Pts',(-2.86125274249415,6.13495265416594,-22.6640040694567));
#42426=CARTESIAN_POINT('Ctrl Pts',(-3.02274579686597,6.0570104098419,-22.6555765504253));
#42427=CARTESIAN_POINT('Ctrl Pts',(-3.18083012460513,5.97282250853016,-22.6471490313939));
#42428=CARTESIAN_POINT('Ctrl Pts',(-3.33905621625991,5.88855911076214,-22.6387139548891));
#42429=CARTESIAN_POINT('Ctrl Pts',(-3.49386717869796,5.79803902158271,-22.6302788783843));
#42430=CARTESIAN_POINT('Ctrl Pts',(-3.644765541231,5.70157637407894,-22.6218438018795));
#42431=CARTESIAN_POINT('Ctrl Pts',(-3.79573683393573,5.6050671055428,-22.6134046486467));
#42432=CARTESIAN_POINT('Ctrl Pts',(-3.94279147898377,5.50260973696425,-22.604965495414));
#42433=CARTESIAN_POINT('Ctrl Pts',(-4.08546238809936,5.39456078614612,-22.5965263421812));
#42434=CARTESIAN_POINT('Ctrl Pts',(-4.22829184459585,5.28639176264978,-22.5880778106831));
#42435=CARTESIAN_POINT('Ctrl Pts',(-4.36672757022377,5.17261894862968,-22.579629279185));
#42436=CARTESIAN_POINT('Ctrl Pts',(-4.50033593007315,5.05363883914281,-22.5711807476869));
#42437=CARTESIAN_POINT('Ctrl Pts',(-4.57415888382355,4.98789846833242,-22.5665126599209));
#42438=CARTESIAN_POINT('Ctrl Pts',(-4.64650872167435,4.92056901762265,-22.5618445721549));
#42439=CARTESIAN_POINT('Ctrl Pts',(-4.71731727448002,4.85172203778127,-22.5571764843889));
#42440=CARTESIAN_POINT('Ctrl Pts',(-4.84231865047318,4.73018351069451,-22.5489357087922));
#42441=CARTESIAN_POINT('Ctrl Pts',(-4.96279257189696,4.60364323105405,-22.5406949331954));
#42442=CARTESIAN_POINT('Ctrl Pts',(-5.07831648673242,4.47247030851874,-22.5324541575986));
#42443=CARTESIAN_POINT('Ctrl Pts',(-5.19371244630784,4.34144267421606,-22.5242225095543));
#42444=CARTESIAN_POINT('Ctrl Pts',(-5.30416908320955,4.2057928787383,-22.5159908615099));
#42445=CARTESIAN_POINT('Ctrl Pts',(-5.40929902691201,4.06592831189248,-22.5077592134655));
#42446=CARTESIAN_POINT('Ctrl Pts',(-5.51433126294195,3.92619373504582,-22.4995352159072));
#42447=CARTESIAN_POINT('Ctrl Pts',(-5.61404645257981,3.78225247080156,-22.4913112183489));
#42448=CARTESIAN_POINT('Ctrl Pts',(-5.70809597807009,3.63454664368749,-22.4830872207906));
#42449=CARTESIAN_POINT('Ctrl Pts',(-5.80206241043929,3.48697131524543,-22.4748704891661));
#42450=CARTESIAN_POINT('Ctrl Pts',(-5.89037296505994,3.3356383519811,-22.4666537575416));
#42451=CARTESIAN_POINT('Ctrl Pts',(-5.97272109854002,3.1810205404956,-22.4584370259171));
#42452=CARTESIAN_POINT('Ctrl Pts',(-6.05502704202283,3.02648194543879,-22.4502245040284));
#42453=CARTESIAN_POINT('Ctrl Pts',(-6.13137648142408,2.86866216718532,-22.4420119821396));
#42454=CARTESIAN_POINT('Ctrl Pts',(-6.20150756057124,2.70806074085826,-22.4337994602509));
#42455=CARTESIAN_POINT('Ctrl Pts',(-6.27161518754793,2.54751302042128,-22.425589684669));
#42456=CARTESIAN_POINT('Ctrl Pts',(-6.33550845455604,2.38418583066897,-22.4173799090872));
#42457=CARTESIAN_POINT('Ctrl Pts',(-6.39297258518575,2.21860102881599,-22.4091701335053));
#42458=CARTESIAN_POINT('Ctrl Pts',(-6.41807142451639,2.14627788928947,-22.4055843168226));
#42459=CARTESIAN_POINT('Ctrl Pts',(-6.44194438404629,2.07352432665489,-22.4019985001399));
#42460=CARTESIAN_POINT('Ctrl Pts',(-6.46457647938253,2.00038494850721,-22.3984126834572));
#42461=CARTESIAN_POINT('Ctrl Pts',(-6.51678662117979,1.83165919654648,-22.3901405374326));
#42462=CARTESIAN_POINT('Ctrl Pts',(-6.56236028910773,1.66097445397087,-22.381868391408));
#42463=CARTESIAN_POINT('Ctrl Pts',(-6.60117389750525,1.48888957780469,-22.3735962453834));
#42464=CARTESIAN_POINT('Ctrl Pts',(-6.64000848849303,1.3167116727603,-22.3653196274466));
#42465=CARTESIAN_POINT('Ctrl Pts',(-6.67207566787301,1.14313246732658,-22.3570430095098));
#42466=CARTESIAN_POINT('Ctrl Pts',(-6.69730339989465,0.968718829051837,
-22.3487663915729));
#42467=CARTESIAN_POINT('Ctrl Pts',(-6.72256647596976,0.794060837263601,
-22.3404781780941));
#42468=CARTESIAN_POINT('Ctrl Pts',(-6.74097091645306,0.618566423146213,
-22.3321899646152));
#42469=CARTESIAN_POINT('Ctrl Pts',(-6.75249666487768,0.442806719479055,
-22.3239017511364));
#42470=CARTESIAN_POINT('Ctrl Pts',(-6.76226879363462,0.293788504675128,
-22.3168745728312));
#42471=CARTESIAN_POINT('Ctrl Pts',(-6.76709705177433,0.14457973026869,-22.3098473945261));
#42472=CARTESIAN_POINT('Ctrl Pts',(-6.7669985214907,-0.00447326979873706,
-22.3028202162209));
#42473=CARTESIAN_POINT('',(-6.767,3.46986979080088E-13,-22.6971797838101));
#42474=CARTESIAN_POINT('Ctrl Pts',(3.09908550384722,6.01564277861012,-23.348603209574));
#42475=CARTESIAN_POINT('Ctrl Pts',(2.93373232018332,6.10082796552478,-23.3398537616747));
#42476=CARTESIAN_POINT('Ctrl Pts',(2.76486502144432,6.17919158180188,-23.3311043137754));
#42477=CARTESIAN_POINT('Ctrl Pts',(2.59305716434359,6.25046746591376,-23.3223548658761));
#42478=CARTESIAN_POINT('Ctrl Pts',(2.42125069459294,6.3217427744722,-23.3136054886287));
#42479=CARTESIAN_POINT('Ctrl Pts',(2.24650397871075,6.3859303555782,-23.3048561113813));
#42480=CARTESIAN_POINT('Ctrl Pts',(2.06941053323792,6.44281220003532,-23.2961067341338));
#42481=CARTESIAN_POINT('Ctrl Pts',(1.89231845896707,6.49969360406678,-23.2873574246312));
#42482=CARTESIAN_POINT('Ctrl Pts',(1.71287996431531,6.54926929700874,-23.2786081151286));
#42483=CARTESIAN_POINT('Ctrl Pts',(1.53170449173533,6.59137090065472,-23.2698588056261));
#42484=CARTESIAN_POINT('Ctrl Pts',(1.35053036178202,6.63347219230077,-23.2611095609615));
#42485=CARTESIAN_POINT('Ctrl Pts',(1.16761955878879,6.66809944062448,-23.2523603162969));
#42486=CARTESIAN_POINT('Ctrl Pts',(0.983593309310867,6.69513503985386,-23.2436110716323));
#42487=CARTESIAN_POINT('Ctrl Pts',(0.799568362460278,6.72217044771211,-23.2348618888991));
#42488=CARTESIAN_POINT('Ctrl Pts',(0.614428268438806,6.74161427235975,-23.2261127061659));
#42489=CARTESIAN_POINT('Ctrl Pts',(0.428801816330394,6.75340047696801,-23.2173635234328));
#42490=CARTESIAN_POINT('Ctrl Pts',(0.243176616522861,6.76518660206242,-23.2086143997246));
#42491=CARTESIAN_POINT('Ctrl Pts',(0.0570653511654892,6.76931519233997,
-23.1998652760165));
#42492=CARTESIAN_POINT('Ctrl Pts',(-0.12889990080005,6.76577222610795,-23.1911161523083));
#42493=CARTESIAN_POINT('Ctrl Pts',(-0.314863959942088,6.76222928260133,
-23.1823670847191));
#42494=CARTESIAN_POINT('Ctrl Pts',(-0.500681721080793,6.75101488651276,
-23.1736180171298));
#42495=CARTESIAN_POINT('Ctrl Pts',(-0.685722110173457,6.73216712415989,
-23.1648689495406));
#42496=CARTESIAN_POINT('Ctrl Pts',(-0.870761373827607,6.71331947644145,
-23.1561199351642));
#42497=CARTESIAN_POINT('Ctrl Pts',(-1.05502298984326,6.68683858439999,-23.1473709207878));
#42498=CARTESIAN_POINT('Ctrl Pts',(-1.23788117676027,6.65281438131432,-23.1386219064115));
#42499=CARTESIAN_POINT('Ctrl Pts',(-1.43009641451764,6.61704912302384,-23.129425195524));
#42500=CARTESIAN_POINT('Ctrl Pts',(-1.62076048992671,6.57294837083171,-23.1202284846364));
#42501=CARTESIAN_POINT('Ctrl Pts',(-1.80915798961111,6.52067760042055,-23.1110317737489));
#42502=CARTESIAN_POINT('Ctrl Pts',(-1.98840443002991,6.47094578577415,-23.1022817760424));
#42503=CARTESIAN_POINT('Ctrl Pts',(-2.16559895952171,6.41381888474482,-23.0935317783359));
#42504=CARTESIAN_POINT('Ctrl Pts',(-2.34013966242301,6.34949095285242,-23.0847817806294));
#42505=CARTESIAN_POINT('Ctrl Pts',(-2.51467682553994,6.28516432556693,-23.0760319603778));
#42506=CARTESIAN_POINT('Ctrl Pts',(-2.68656000078822,6.21363705879669,-23.0672821401262));
#42507=CARTESIAN_POINT('Ctrl Pts',(-2.85520533840869,6.13515211510868,-23.0585323198746));
#42508=CARTESIAN_POINT('Ctrl Pts',(-3.0238474799831,6.0566686588113,-23.0497826654433));
#42509=CARTESIAN_POINT('Ctrl Pts',(-3.18925164684522,5.97122791039852,-23.0410330110121));
#42510=CARTESIAN_POINT('Ctrl Pts',(-3.35085601829144,5.87912008251915,-23.0322833565808));
#42511=CARTESIAN_POINT('Ctrl Pts',(-3.51245754191413,5.78701387778178,-23.0235338563377));
#42512=CARTESIAN_POINT('Ctrl Pts',(-3.67025915510938,5.68824097060981,-23.0147843560946));
#42513=CARTESIAN_POINT('Ctrl Pts',(-3.82372487928844,5.58313684656848,-23.0060348558514));
#42514=CARTESIAN_POINT('Ctrl Pts',(-3.97718810300806,5.47803443501767,-22.9972854981663));
#42515=CARTESIAN_POINT('Ctrl Pts',(-4.12631534263033,5.3666011749637,-22.9885361404812));
#42516=CARTESIAN_POINT('Ctrl Pts',(-4.27060009886231,5.24921554097346,-22.9797867827961));
#42517=CARTESIAN_POINT('Ctrl Pts',(-4.41488269594219,5.13183166360286,-22.9710375560409));
#42518=CARTESIAN_POINT('Ctrl Pts',(-4.55432273235094,5.00849577139466,-22.9622883292857));
#42519=CARTESIAN_POINT('Ctrl Pts',(-4.68844662480212,4.87962675277337,-22.9535391025305));
#42520=CARTESIAN_POINT('Ctrl Pts',(-4.8225686883517,4.7507594913987,-22.944789995079));
#42521=CARTESIAN_POINT('Ctrl Pts',(-4.95137454637881,4.61635945312505,-22.9360408876275));
#42522=CARTESIAN_POINT('Ctrl Pts',(-5.07442674461103,4.47688309134563,-22.927291780176));
#42523=CARTESIAN_POINT('Ctrl Pts',(-5.1974774283858,4.33740844616303,-22.9185427804037));
#42524=CARTESIAN_POINT('Ctrl Pts',(-5.31477440450984,4.19285781735958,-22.9097937806313));
#42525=CARTESIAN_POINT('Ctrl Pts',(-5.42591931531223,4.04372211999312,-22.9010447808589));
#42526=CARTESIAN_POINT('Ctrl Pts',(-5.5370763646305,3.89457013500704,-22.8922948255783));
#42527=CARTESIAN_POINT('Ctrl Pts',(-5.64207983273537,3.74083230916319,-22.8835448702977));
#42528=CARTESIAN_POINT('Ctrl Pts',(-5.74057303468812,3.58303087251723,-22.8747949150171));
#42529=CARTESIAN_POINT('Ctrl Pts',(-5.8390624336383,3.4252355288732,-22.8660452975883));
#42530=CARTESIAN_POINT('Ctrl Pts',(-5.9310419176849,3.26337713156875,-22.8572956801595));
#42531=CARTESIAN_POINT('Ctrl Pts',(-6.0161990669972,3.09800545291032,-22.8485460627307));
#42532=CARTESIAN_POINT('Ctrl Pts',(-6.10135338095453,2.93263928039451,-22.8397967366253));
#42533=CARTESIAN_POINT('Ctrl Pts',(-6.17968568352913,2.76376031540059,-22.8310474105199));
#42534=CARTESIAN_POINT('Ctrl Pts',(-6.25092992694964,2.59194213831355,-22.8222980844145));
#42535=CARTESIAN_POINT('Ctrl Pts',(-6.32217217691168,2.4201287688065,-22.8135490031207));
#42536=CARTESIAN_POINT('Ctrl Pts',(-6.38632665483903,2.24537661647518,-22.8047999218269));
#42537=CARTESIAN_POINT('Ctrl Pts',(-6.44317547869393,2.06827917621322,-22.7960508405332));
#42538=CARTESIAN_POINT('Ctrl Pts',(-6.50002944235973,1.89116572423296,-22.7873009682182));
#42539=CARTESIAN_POINT('Ctrl Pts',(-6.54957634250429,1.71170683289078,-22.7785510959032));
#42540=CARTESIAN_POINT('Ctrl Pts',(-6.59164787708421,1.53051209225252,-22.7698012235883));
#42541=CARTESIAN_POINT('Ctrl Pts',(-6.63371649075027,1.34932993147939,-22.7610519587535));
#42542=CARTESIAN_POINT('Ctrl Pts',(-6.66831071257135,1.16641244173934,-22.7523026939187));
#42543=CARTESIAN_POINT('Ctrl Pts',(-6.6953130484034,0.982380875159536,-22.7435534290839));
#42544=CARTESIAN_POINT('Ctrl Pts',(-6.7223167703305,0.798339861795333,-22.7348037151283));
#42545=CARTESIAN_POINT('Ctrl Pts',(-6.74172778477895,0.61318494072961,-22.7260540011726));
#42546=CARTESIAN_POINT('Ctrl Pts',(-6.75348015835522,0.427545027689976,
-22.717304287217));
#42547=CARTESIAN_POINT('Ctrl Pts',(-6.76249038365222,0.285219953546579,
-22.7105961194147));
#42548=CARTESIAN_POINT('Ctrl Pts',(-6.76699999999999,0.142609995757398,
-22.7038879516124));
#42549=CARTESIAN_POINT('Ctrl Pts',(-6.767,3.46987300839874E-13,-22.6971797838101));
#42550=CARTESIAN_POINT('Ctrl Pts',(-6.76699992255766,-0.00102376982859472,
-22.6971797838101));
#42551=CARTESIAN_POINT('Ctrl Pts',(-6.76699274983805,-0.0484346151663659,
-22.6949554495712));
#42552=CARTESIAN_POINT('Ctrl Pts',(-6.7664872992955,-0.0958431546807729,
-22.6927311153323));
#42553=CARTESIAN_POINT('Ctrl Pts',(-6.7654838603425,-0.143238037703361,
-22.6905067810934));
#42554=CARTESIAN_POINT('Ctrl Pts',(-6.76159567273573,-0.326886675463195,
-22.6818877925689));
#42555=CARTESIAN_POINT('Ctrl Pts',(-6.75022687176097,-0.510310039791529,
-22.6732688040444));
#42556=CARTESIAN_POINT('Ctrl Pts',(-6.73143274283991,-0.692894096253327,
-22.6646498155198));
#42557=CARTESIAN_POINT('Ctrl Pts',(-6.7126273545584,-0.875587536859203,
-22.656025663452));
#42558=CARTESIAN_POINT('Ctrl Pts',(-6.68638779175664,-1.05744036356867,
-22.6474015113841));
#42559=CARTESIAN_POINT('Ctrl Pts',(-6.652820978273,-1.23784572182912,-22.6387773593163));
#42560=CARTESIAN_POINT('Ctrl Pts',(-6.61810449239762,-1.42443001214147,
-22.6298578277201));
#42561=CARTESIAN_POINT('Ctrl Pts',(-6.57555002218844,-1.60946557576452,
-22.6209382961239));
#42562=CARTESIAN_POINT('Ctrl Pts',(-6.52533264709187,-1.79229541225689,
-22.6120187645277));
#42563=CARTESIAN_POINT('Ctrl Pts',(-6.47668782124208,-1.96939996101538,
-22.6033785466684));
#42564=CARTESIAN_POINT('Ctrl Pts',(-6.42085288937884,-2.14443455975871,
-22.5947383288091));
#42565=CARTESIAN_POINT('Ctrl Pts',(-6.35803712842322,-2.31681955999853,
-22.5860981109498));
#42566=CARTESIAN_POINT('Ctrl Pts',(-6.29217538438971,-2.49756363741301,
-22.5770389224852));
#42567=CARTESIAN_POINT('Ctrl Pts',(-6.21863911694482,-2.6753944074447,-22.5679797340205));
#42568=CARTESIAN_POINT('Ctrl Pts',(-6.1377255251347,-2.84966916994061,-22.5589205455559));
#42569=CARTESIAN_POINT('Ctrl Pts',(-6.05681193332454,-3.02394393243659,
-22.5498613570913));
#42570=CARTESIAN_POINT('Ctrl Pts',(-5.96852122234264,-3.19466236274906,
-22.5408021686267));
#42571=CARTESIAN_POINT('Ctrl Pts',(-5.87320508241716,-3.3612127364791,-22.5317429801621));
#42572=CARTESIAN_POINT('Ctrl Pts',(-5.7780540710162,-3.52747457337271,-22.5226994861059));
#42573=CARTESIAN_POINT('Ctrl Pts',(-5.67581502940719,-3.68973637230308,
-22.5136559920496));
#42574=CARTESIAN_POINT('Ctrl Pts',(-5.56683334138906,-3.84742193542626,
-22.5046124979934));
#42575=CARTESIAN_POINT('Ctrl Pts',(-5.45795133852264,-4.00496326414118,
-22.4955772759881));
#42576=CARTESIAN_POINT('Ctrl Pts',(-5.34233913788169,-4.15793651845302,
-22.4865420539828));
#42577=CARTESIAN_POINT('Ctrl Pts',(-5.22038557744195,-4.30579416865647,
-22.4775068319775));
#42578=CARTESIAN_POINT('Ctrl Pts',(-5.09864687262647,-4.45339132586882,
-22.4684875280665));
#42579=CARTESIAN_POINT('Ctrl Pts',(-4.97058926859331,-4.59589069254239,
-22.4594682241554));
#42580=CARTESIAN_POINT('Ctrl Pts',(-4.83664189523819,-4.73277763868394,
-22.4504489202443));
#42581=CARTESIAN_POINT('Ctrl Pts',(-4.70286256821907,-4.86949285059011,
-22.44144093168));
#42582=CARTESIAN_POINT('Ctrl Pts',(-4.5632083840568,-5.00060952406196,-22.4324329431157));
#42583=CARTESIAN_POINT('Ctrl Pts',(-4.41814704867377,-5.12564782796236,
-22.4234249545514));
#42584=CARTESIAN_POINT('Ctrl Pts',(-4.27341333939746,-5.25040372847396,
-22.4144373108447));
#42585=CARTESIAN_POINT('Ctrl Pts',(-4.12329703565662,-5.3691085070198,-22.4054496671381));
#42586=CARTESIAN_POINT('Ctrl Pts',(-3.96830043668197,-5.48132106742797,
-22.3964620234314));
#42587=CARTESIAN_POINT('Ctrl Pts',(-3.83330914181043,-5.57905043007564,
-22.3886344086978));
#42588=CARTESIAN_POINT('Ctrl Pts',(-3.6946166839515,-5.67185578121942,-22.3808067939641));
#42589=CARTESIAN_POINT('Ctrl Pts',(-3.55257685114231,-5.75946930860195,
-22.3729791792304));
#42590=CARTESIAN_POINT('Ctrl Pts',(-3.40517408456408,-5.85039082033881,
-22.3648560207851));
#42591=CARTESIAN_POINT('Ctrl Pts',(-3.25423141251924,-5.93567898960228,
-22.3567328623398));
#42592=CARTESIAN_POINT('Ctrl Pts',(-3.10022620198568,-6.01505498699068,
-22.3486097038945));
#42593=CARTESIAN_POINT('Ctrl Pts',(-2.94623184962556,-6.0944253879558,-22.3404871181744));
#42594=CARTESIAN_POINT('Ctrl Pts',(-2.78917571423031,-6.16788427965845,
-22.3323645324543));
#42595=CARTESIAN_POINT('Ctrl Pts',(-2.6295593600824,-6.23519900017658,-22.3242419467342));
#42596=CARTESIAN_POINT('Ctrl Pts',(-2.46992382638634,-6.30252180925137,
-22.3161183850018));
#42597=CARTESIAN_POINT('Ctrl Pts',(-2.30772779907883,-6.36369883591761,
-22.3079948232694));
#42598=CARTESIAN_POINT('Ctrl Pts',(-2.14349234403927,-6.41854575204112,
-22.299871261537));
#42599=CARTESIAN_POINT('Ctrl Pts',(-1.97913726296015,-6.47343261763447,
-22.2917417827538));
#42600=CARTESIAN_POINT('Ctrl Pts',(-1.81274013478251,-6.52198004777808,
-22.2836123039707));
#42601=CARTESIAN_POINT('Ctrl Pts',(-1.64483730910135,-6.56405356670619,
-22.2754828251876));
#42602=CARTESIAN_POINT('Ctrl Pts',(-1.47686603239342,-6.60614423826743,
-22.2673500321591));
#42603=CARTESIAN_POINT('Ctrl Pts',(-1.30738819255101,-6.64175566249123,
-22.2592172391305));
#42604=CARTESIAN_POINT('Ctrl Pts',(-1.13694957416881,-6.67080464905077,
-22.251084446102));
#42605=CARTESIAN_POINT('Ctrl Pts',(-0.966325629645998,-6.69988522197623,
-22.2429428098949));
#42606=CARTESIAN_POINT('Ctrl Pts',(-0.794739182451133,-6.72238905752447,
-22.2348011736877));
#42607=CARTESIAN_POINT('Ctrl Pts',(-0.622741120960248,-6.73828483341757,
-22.2266595374806));
#42608=CARTESIAN_POINT('Ctrl Pts',(-0.535110444863029,-6.74638351532437,
-22.2225114844201));
#42609=CARTESIAN_POINT('Ctrl Pts',(-0.447372942291769,-6.752767737948,-22.2183634313595));
#42610=CARTESIAN_POINT('Ctrl Pts',(-0.35960133187925,-6.75743855925533,
-22.214215378299));
#42611=CARTESIAN_POINT('Ctrl Pts',(-0.180998229206384,-6.76694303540198,
-22.2057746633209));
#42612=CARTESIAN_POINT('Ctrl Pts',(-0.00188612121038587,-6.76936932874372,
-22.1973339483429));
#42613=CARTESIAN_POINT('Ctrl Pts',(0.177149307238839,-6.76468085891307,
-22.1888932333648));
#42614=CARTESIAN_POINT('Ctrl Pts',(0.356049412276157,-6.75999593284881,
-22.1804588982768));
#42615=CARTESIAN_POINT('Ctrl Pts',(0.534872621195459,-6.74820697237735,
-22.1720245631887));
#42616=CARTESIAN_POINT('Ctrl Pts',(0.713031823750875,-6.72932943303555,
-22.1635902281007));
#42617=CARTESIAN_POINT('Ctrl Pts',(0.89108372356648,-6.71046326336572,-22.1551609728921));
#42618=CARTESIAN_POINT('Ctrl Pts',(1.06847208359119,-6.68451706146053,-22.1467317176835));
#42619=CARTESIAN_POINT('Ctrl Pts',(1.2446130940856,-6.6515582569824,-22.1383024624748));
#42620=CARTESIAN_POINT('Ctrl Pts',(1.42067503607245,-6.61861424748854,-22.1298769911018));
#42621=CARTESIAN_POINT('Ctrl Pts',(1.59549041778119,-6.57866397324414,-22.1214515197288));
#42622=CARTESIAN_POINT('Ctrl Pts',(1.76848343022747,-6.53182634161464,-22.1130260483558));
#42623=CARTESIAN_POINT('Ctrl Pts',(1.9414253009206,-6.48500255654785,-22.1046030677966));
#42624=CARTESIAN_POINT('Ctrl Pts',(2.11254555524785,-6.43129556159063,-22.0961800872373));
#42625=CARTESIAN_POINT('Ctrl Pts',(2.28128101958846,-6.37087481509922,-22.0877571066781));
#42626=CARTESIAN_POINT('Ctrl Pts',(2.45001927783838,-6.31045306816555,-22.0793339866518));
#42627=CARTESIAN_POINT('Ctrl Pts',(2.61637235116062,-6.2433174537385,-22.0709108666255));
#42628=CARTESIAN_POINT('Ctrl Pts',(2.77979397187767,-6.16968674033881,-22.0624877465991));
#42629=CARTESIAN_POINT('Ctrl Pts',(2.94322124398679,-6.09605348066632,-22.0540643352873));
#42630=CARTESIAN_POINT('Ctrl Pts',(3.10371655722626,-6.0159248110216,-22.0456409239754));
#42631=CARTESIAN_POINT('Ctrl Pts',(3.26075517191744,-5.92956699167938,-22.0372175126635));
#42632=CARTESIAN_POINT('Ctrl Pts',(3.41782111861132,-5.84319414207116,-22.0287926352874));
#42633=CARTESIAN_POINT('Ctrl Pts',(3.57142887507701,-5.75059014196348,-22.0203677579113));
#42634=CARTESIAN_POINT('Ctrl Pts',(3.72107946287387,-5.65206658055072,-22.0119428805352));
#42635=CARTESIAN_POINT('Ctrl Pts',(3.87077697423446,-5.55351212666583,-22.0035153615038));
#42636=CARTESIAN_POINT('Ctrl Pts',(4.01651456469795,-5.44903459421697,-21.9950878424723));
#42637=CARTESIAN_POINT('Ctrl Pts',(4.15782303043522,-5.33898835432167,-21.9866603234409));
#42638=CARTESIAN_POINT('Ctrl Pts',(4.29925821614311,-5.22884342921164,-21.9782252469361));
#42639=CARTESIAN_POINT('Ctrl Pts',(4.43625607739851,-5.11312002342242,-21.9697901704313));
#42640=CARTESIAN_POINT('Ctrl Pts',(4.56838037158332,-4.99221291418267,-21.9613550939265));
#42641=CARTESIAN_POINT('Ctrl Pts',(4.70056852230911,-4.87124736974125,-21.9529159406938));
#42642=CARTESIAN_POINT('Ctrl Pts',(4.82787816797478,-4.74509335622317,-21.944476787461));
#42643=CARTESIAN_POINT('Ctrl Pts',(4.94991026570973,-4.61418219855063,-21.9360376342282));
#42644=CARTESIAN_POINT('Ctrl Pts',(5.07207797531951,-4.48312556187823,-21.9275891027301));
#42645=CARTESIAN_POINT('Ctrl Pts',(5.18895619684924,-4.34730146728461,-21.919140571232));
#42646=CARTESIAN_POINT('Ctrl Pts',(5.30018569986966,-4.2071748890315,-21.9106920397339));
#42647=CARTESIAN_POINT('Ctrl Pts',(5.36164360913839,-4.12975040812883,-21.9060239519679));
#42648=CARTESIAN_POINT('Ctrl Pts',(5.4213777547571,-4.0510129594965,-21.9013558642019));
#42649=CARTESIAN_POINT('Ctrl Pts',(5.47933324514631,-3.9710447225679,-21.896687776436));
#42650=CARTESIAN_POINT('Ctrl Pts',(5.58164455865225,-3.82987336323727,-21.8884470008392));
#42651=CARTESIAN_POINT('Ctrl Pts',(5.67863786581217,-3.68455059667655,-21.8802062252424));
#42652=CARTESIAN_POINT('Ctrl Pts',(5.76996015947585,-3.53551251702797,-21.8719654496457));
#42653=CARTESIAN_POINT('Ctrl Pts',(5.86118130379875,-3.3866395132103,-21.8637338016013));
#42654=CARTESIAN_POINT('Ctrl Pts',(5.94674375751435,-3.23405969094357,-21.8555021535569));
#42655=CARTESIAN_POINT('Ctrl Pts',(6.02633573746481,-3.0782408254317,-21.8472705055126));
#42656=CARTESIAN_POINT('Ctrl Pts',(6.1058537447027,-2.92256677782938,-21.8390465079543));
#42657=CARTESIAN_POINT('Ctrl Pts',(6.17941216819836,-2.76365999720127,-21.830822510396));
#42658=CARTESIAN_POINT('Ctrl Pts',(6.24674335927927,-2.60201583455989,-21.8225985128377));
#42659=CARTESIAN_POINT('Ctrl Pts',(6.3140150629913,-2.44051448516415,-21.8143817812132));
#42660=CARTESIAN_POINT('Ctrl Pts',(6.37507036364216,-2.27628090123508,-21.8061650495887));
#42661=CARTESIAN_POINT('Ctrl Pts',(6.42968832115496,-2.10983342773869,-21.7979483179642));
#42662=CARTESIAN_POINT('Ctrl Pts',(6.48427829586609,-1.94347123144506,-21.7897357960755));
#42663=CARTESIAN_POINT('Ctrl Pts',(6.53243738527677,-1.77489774179779,-21.7815232741868));
#42664=CARTESIAN_POINT('Ctrl Pts',(6.57399326105277,-1.60464999412108,-21.7733107522981));
#42665=CARTESIAN_POINT('Ctrl Pts',(6.61553524034389,-1.43445917811064,-21.7651009767162));
#42666=CARTESIAN_POINT('Ctrl Pts',(6.65047832061509,-1.26259556467711,-21.7568912011344));
#42667=CARTESIAN_POINT('Ctrl Pts',(6.67870038343357,-1.08961010839855,-21.7486814255525));
#42668=CARTESIAN_POINT('Ctrl Pts',(6.69102704725852,-1.01405455528866,-21.7450956088698));
#42669=CARTESIAN_POINT('Ctrl Pts',(6.70207218499357,-0.938285141900227,
-21.741509792187));
#42670=CARTESIAN_POINT('Ctrl Pts',(6.71182868254411,-0.862348384458541,
-21.7379239755043));
#42671=CARTESIAN_POINT('Ctrl Pts',(6.73593199385336,-0.674747527188622,
-21.7290652579825));
#42672=CARTESIAN_POINT('Ctrl Pts',(6.75214205920244,-0.486319296408045,
-21.7202065404608));
#42673=CARTESIAN_POINT('Ctrl Pts',(6.76044773986345,-0.297716906767592,
-21.711347822939));
#42674=CARTESIAN_POINT('Ctrl Pts',(6.768768959119,-0.108761672347425,-21.7024725321795));
#42675=CARTESIAN_POINT('Ctrl Pts',(6.76915622979846,0.0803681129719283,
-21.6935972414201));
#42676=CARTESIAN_POINT('Ctrl Pts',(6.7616504580941,0.269020598757414,-21.6847219506606));
#42677=CARTESIAN_POINT('Ctrl Pts',(6.75412336831047,0.458208900020156,-21.6758214520799));
#42678=CARTESIAN_POINT('Ctrl Pts',(6.7386583853227,0.646916928190347,-21.6669209534991));
#42679=CARTESIAN_POINT('Ctrl Pts',(6.71534846787936,0.834496228242138,-21.6580204549183));
#42680=CARTESIAN_POINT('Ctrl Pts',(6.69200699576958,1.02232945464346,-21.6491079077207));
#42681=CARTESIAN_POINT('Ctrl Pts',(6.66079941421044,1.20903064421832,-21.6401953605231));
#42682=CARTESIAN_POINT('Ctrl Pts',(6.62186985046744,1.39396150716953,-21.6312828133254));
#42683=CARTESIAN_POINT('Ctrl Pts',(6.58285432644569,1.57930071552714,-21.6223505863532));
#42684=CARTESIAN_POINT('Ctrl Pts',(6.53608276928002,1.76286152368634,-21.6134183593809));
#42685=CARTESIAN_POINT('Ctrl Pts',(6.48174999680389,1.94401799861337,-21.6044861324086));
#42686=CARTESIAN_POINT('Ctrl Pts',(6.43039925269116,2.11523178661635,-21.5960441464634));
#42687=CARTESIAN_POINT('Ctrl Pts',(6.37229498617801,2.28429788968549,-21.5876021605182));
#42688=CARTESIAN_POINT('Ctrl Pts',(6.30764116018565,2.45070438738168,-21.5791601745729));
#42689=CARTESIAN_POINT('Ctrl Pts',(6.24464550963262,2.61284306081242,-21.5709347000798));
#42690=CARTESIAN_POINT('Ctrl Pts',(6.17531061659187,2.77276620515393,-21.5627092255868));
#42691=CARTESIAN_POINT('Ctrl Pts',(6.09981303746284,2.92994366976541,-21.5544837510937));
#42692=CARTESIAN_POINT('Ctrl Pts',(6.02112223576987,3.09376906444736,-21.545910374442));
#42693=CARTESIAN_POINT('Ctrl Pts',(5.93573613715189,3.25461107827148,-21.5373369977903));
#42694=CARTESIAN_POINT('Ctrl Pts',(5.84391203472763,3.41188820601813,-21.5287636211386));
#42695=CARTESIAN_POINT('Ctrl Pts',(5.75600724214319,3.5624523055066,-21.5205561802116));
#42696=CARTESIAN_POINT('Ctrl Pts',(5.66220280499075,3.70974915038927,-21.5123487392847));
#42697=CARTESIAN_POINT('Ctrl Pts',(5.56277293849444,3.85329031280463,-21.5041412983577));
#42698=CARTESIAN_POINT('Ctrl Pts',(5.4634029665276,3.99674500894293,-21.4959388014263));
#42699=CARTESIAN_POINT('Ctrl Pts',(5.35841451651555,4.1364482339894,-21.4877363044948));
#42700=CARTESIAN_POINT('Ctrl Pts',(5.24812630850918,4.27193858218185,-21.4795338075634));
#42701=CARTESIAN_POINT('Ctrl Pts',(5.13788450026496,4.40737192772602,-21.4713347615349));
#42702=CARTESIAN_POINT('Ctrl Pts',(5.0223476010062,4.53859564917111,-21.4631357155065));
#42703=CARTESIAN_POINT('Ctrl Pts',(4.90187602113822,4.66517957568518,-21.454936669478));
#42704=CARTESIAN_POINT('Ctrl Pts',(4.78143324103618,4.79173324122434,-21.4467395835019));
#42705=CARTESIAN_POINT('Ctrl Pts',(4.65605837803892,4.91364906262556,-21.4385424975259));
#42706=CARTESIAN_POINT('Ctrl Pts',(4.52615031160175,5.03053201528301,-21.4303454115498));
#42707=CARTESIAN_POINT('Ctrl Pts',(4.3962239227512,5.1474314532738,-21.4221471694453));
#42708=CARTESIAN_POINT('Ctrl Pts',(4.26176331661265,5.2592963611186,-21.4139489273409));
#42709=CARTESIAN_POINT('Ctrl Pts',(4.12320250774531,5.36577022244922,-21.4057506852365));
#42710=CARTESIAN_POINT('Ctrl Pts',(3.98462975913752,5.47225325859832,-21.3975517366922));
#42711=CARTESIAN_POINT('Ctrl Pts',(3.8419563917584,5.57334410895098,-21.3893527881479));
#42712=CARTESIAN_POINT('Ctrl Pts',(3.69564733064943,5.66872823545668,-21.3811538396036));
#42713=CARTESIAN_POINT('Ctrl Pts',(3.54926196351698,5.76416210859693,-21.3729506149799));
#42714=CARTESIAN_POINT('Ctrl Pts',(3.39923741989362,5.85388312401151,-21.3647473903562));
#42715=CARTESIAN_POINT('Ctrl Pts',(3.24606567045609,5.93762129670514,-21.3565441657325));
#42716=CARTESIAN_POINT('Ctrl Pts',(3.19738457693707,5.96423498905363,-21.3539370143059));
#42717=CARTESIAN_POINT('Ctrl Pts',(3.14838576474938,5.99024470736143,-21.3513298628792));
#42718=CARTESIAN_POINT('Ctrl Pts',(3.09908550384722,6.01564277861012,-21.3487227114526));
#42719=CARTESIAN_POINT('Origin',(0.,0.,-63.6971797838103));
#42720=CARTESIAN_POINT('',(3.09908550384715,6.01564277861015,-18.9542023328983));
#42721=CARTESIAN_POINT('',(3.09908550384723,6.01564277861011,-19.3485039941327));
#42722=CARTESIAN_POINT('',(3.09908550384721,6.01564277861012,-63.6971797838103));
#42723=CARTESIAN_POINT('',(-6.76699815055718,0.00500303464652949,-20.3028202161448));
#42724=CARTESIAN_POINT('Ctrl Pts',(-6.76699815055718,0.00500303464652949,
-20.3028202161448));
#42725=CARTESIAN_POINT('Ctrl Pts',(-6.76712283725175,-0.163645533901148,
-20.2948669119147));
#42726=CARTESIAN_POINT('Ctrl Pts',(-6.76093875946453,-0.332552986580211,
-20.2869136076846));
#42727=CARTESIAN_POINT('Ctrl Pts',(-6.74841442827687,-0.501190287440406,
-20.2789603034545));
#42728=CARTESIAN_POINT('Ctrl Pts',(-6.73590074886688,-0.669684164511485,
-20.2710137634042));
#42729=CARTESIAN_POINT('Ctrl Pts',(-6.71705756938782,-0.837907967772918,
-20.2630672233539));
#42730=CARTESIAN_POINT('Ctrl Pts',(-6.69190542923894,-1.00533115246792,
-20.2551206833037));
#42731=CARTESIAN_POINT('Ctrl Pts',(-6.66677067925789,-1.17263858091856,
-20.2471796374843));
#42732=CARTESIAN_POINT('Ctrl Pts',(-6.6353357071835,-1.3391461155133,-20.2392385916649));
#42733=CARTESIAN_POINT('Ctrl Pts',(-6.59767297846628,-1.50432718157184,
-20.2312975458455));
#42734=CARTESIAN_POINT('Ctrl Pts',(-6.56002526039464,-1.66944241399267,
-20.2233596649647));
#42735=CARTESIAN_POINT('Ctrl Pts',(-6.51615480937113,-1.83323185725992,
-20.2154217840839));
#42736=CARTESIAN_POINT('Ctrl Pts',(-6.46618536754747,-1.99517813553452,
-20.2074839032032));
#42737=CARTESIAN_POINT('Ctrl Pts',(-6.41622188589341,-2.15710509745798,
-20.1995469691234));
#42738=CARTESIAN_POINT('Ctrl Pts',(-6.36016097106077,-2.31718896535845,
-20.1916100350435));
#42739=CARTESIAN_POINT('Ctrl Pts',(-6.29817646049836,-2.47492672061707,
-20.1836731009637));
#42740=CARTESIAN_POINT('Ctrl Pts',(-6.277471492571,-2.52761658029216,-20.1810218907812));
#42741=CARTESIAN_POINT('Ctrl Pts',(-6.25610598230951,-2.58004480419888,
-20.1783706805986));
#42742=CARTESIAN_POINT('Ctrl Pts',(-6.23408762025765,-2.6321931051787,-20.1757194704161));
#42743=CARTESIAN_POINT('Ctrl Pts',(-6.16051576579193,-2.80644072638164,
-20.1668607528943));
#42744=CARTESIAN_POINT('Ctrl Pts',(-6.07970647936697,-2.97743143841342,
-20.1580020353726));
#42745=CARTESIAN_POINT('Ctrl Pts',(-5.99197883434973,-3.14459514861688,
-20.1491433178508));
#42746=CARTESIAN_POINT('Ctrl Pts',(-5.90408706499864,-3.31207159527391,
-20.1402680270914));
#42747=CARTESIAN_POINT('Ctrl Pts',(-5.80925119159497,-3.47570650227465,
-20.1313927363319));
#42748=CARTESIAN_POINT('Ctrl Pts',(-5.70783457661667,-3.63495714499899,
-20.1225174455725));
#42749=CARTESIAN_POINT('Ctrl Pts',(-5.60612991564855,-3.79466009535581,
-20.1136169469917));
#42750=CARTESIAN_POINT('Ctrl Pts',(-5.49780725073439,-3.94995364274463,
-20.1047164484109));
#42751=CARTESIAN_POINT('Ctrl Pts',(-5.38327321796285,-4.10032418971524,
-20.0958159498302));
#42752=CARTESIAN_POINT('Ctrl Pts',(-5.26858414031805,-4.25089829349628,
-20.0869034026326));
#42753=CARTESIAN_POINT('Ctrl Pts',(-5.14766706099953,-4.39653588227203,
-20.0779908554349));
#42754=CARTESIAN_POINT('Ctrl Pts',(-5.02096771915789,-4.53675789117895,
-20.0690783082373));
#42755=CARTESIAN_POINT('Ctrl Pts',(-4.89398861279517,-4.67728952397654,
-20.060146081265));
#42756=CARTESIAN_POINT('Ctrl Pts',(-4.76120188077836,-4.81238146545405,
-20.0512138542928));
#42757=CARTESIAN_POINT('Ctrl Pts',(-4.62309084950618,-4.94159083668531,
-20.0422816273205));
#42758=CARTESIAN_POINT('Ctrl Pts',(-4.49255997646557,-5.06370861306052,
-20.0338396413752));
#42759=CARTESIAN_POINT('Ctrl Pts',(-4.35727364105156,-5.1805720395231,-20.0253976554299));
#42760=CARTESIAN_POINT('Ctrl Pts',(-4.21766570116265,-5.29184136508609,
-20.0169556694847));
#42761=CARTESIAN_POINT('Ctrl Pts',(-4.08166309068968,-5.40023719668545,
-20.0087316950671));
#42762=CARTESIAN_POINT('Ctrl Pts',(-3.94129875731921,-5.5035303789621,-20.0005077206495));
#42763=CARTESIAN_POINT('Ctrl Pts',(-3.79699181587882,-5.60135181453096,
-19.992283746232));
#42764=CARTESIAN_POINT('Ctrl Pts',(-3.65283727656988,-5.6990699411728,-19.9840684571293));
#42765=CARTESIAN_POINT('Ctrl Pts',(-3.50474871503935,-5.79132762888708,
-19.9758531680267));
#42766=CARTESIAN_POINT('Ctrl Pts',(-3.35317851588266,-5.87779574675941,
-19.967637878924));
#42767=CARTESIAN_POINT('Ctrl Pts',(-3.20173798781057,-5.9641898895714,-19.9594296181518));
#42768=CARTESIAN_POINT('Ctrl Pts',(-3.04682206402243,-6.04480415041973,
-19.9512213573797));
#42769=CARTESIAN_POINT('Ctrl Pts',(-2.88891240264724,-6.11935242732685,
-19.9430130966075));
#42770=CARTESIAN_POINT('Ctrl Pts',(-2.73110617159055,-6.19385187535322,
-19.9348102122196));
#42771=CARTESIAN_POINT('Ctrl Pts',(-2.57031043194759,-6.26229310109508,
-19.9266073278317));
#42772=CARTESIAN_POINT('Ctrl Pts',(-2.40703183625131,-6.32443568544046,
-19.9184044434439));
#42773=CARTESIAN_POINT('Ctrl Pts',(-2.24382745331819,-6.38655002497594,
-19.9102052873997));
#42774=CARTESIAN_POINT('Ctrl Pts',(-2.07814279704653,-6.44237129933789,
-19.9020061313554));
#42775=CARTESIAN_POINT('Ctrl Pts',(-1.91050499431835,-6.49170699174606,
-19.8938069753112));
#42776=CARTESIAN_POINT('Ctrl Pts',(-1.74288177200269,-6.54103839314865,
-19.8856085323942));
#42777=CARTESIAN_POINT('Ctrl Pts',(-1.57330608293532,-6.58388522682869,
-19.8774100894772));
#42778=CARTESIAN_POINT('Ctrl Pts',(-1.40232108498669,-6.62010457429501,
-19.8692116465602));
#42779=CARTESIAN_POINT('Ctrl Pts',(-1.23133778984605,-6.65632356105955,
-19.8610132852899));
#42780=CARTESIAN_POINT('Ctrl Pts',(-1.05894556447187,-6.68591511770607,
-19.8528149240197));
#42781=CARTESIAN_POINT('Ctrl Pts',(-0.88569853639518,-6.70878730491789,
-19.8446165627495));
#42782=CARTESIAN_POINT('Ctrl Pts',(-0.712421762090327,-6.73166341924642,
-19.8364167938342));
#42783=CARTESIAN_POINT('Ctrl Pts',(-0.538290248299013,-6.74781781867277,
-19.8282170249189));
#42784=CARTESIAN_POINT('Ctrl Pts',(-0.363864087781422,-6.75721036564816,
-19.8200172560036));
#42785=CARTESIAN_POINT('Ctrl Pts',(-0.189376292490828,-6.76660623154945,
-19.8118145896393));
#42786=CARTESIAN_POINT('Ctrl Pts',(-0.0145940010320489,-6.76923546609791,
-19.8036119232751));
#42787=CARTESIAN_POINT('Ctrl Pts',(0.159921789960391,-6.76511005240091,
-19.7954092569108));
#42788=CARTESIAN_POINT('Ctrl Pts',(0.334635787271743,-6.76097995326509,
-19.7871972743678));
#42789=CARTESIAN_POINT('Ctrl Pts',(0.50908232046455,-6.7500798880267,-19.7789852918248));
#42790=CARTESIAN_POINT('Ctrl Pts',(0.682703554901262,-6.73247390311505,
-19.7707733092818));
#42791=CARTESIAN_POINT('Ctrl Pts',(0.856427193488416,-6.71485753395557,
-19.7625564832005));
#42792=CARTESIAN_POINT('Ctrl Pts',(1.0293242084062,-6.69052741081406,-19.7543396571192));
#42793=CARTESIAN_POINT('Ctrl Pts',(1.20084618305044,-6.65959889517779,-19.7461228310379));
#42794=CARTESIAN_POINT('Ctrl Pts',(1.37263266935201,-6.62862268330349,-19.737893333424));
#42795=CARTESIAN_POINT('Ctrl Pts',(1.54303952781845,-6.59102782148515,-19.7296638358102));
#42796=CARTESIAN_POINT('Ctrl Pts',(1.71153145798003,-6.54698014876666,-19.7214343381963));
#42797=CARTESIAN_POINT('Ctrl Pts',(1.8617179853064,-6.50771793011884,-19.7140989146714));
#42798=CARTESIAN_POINT('Ctrl Pts',(2.01038312910002,-6.46332959546182,-19.7067634911465));
#42799=CARTESIAN_POINT('Ctrl Pts',(2.1571615090825,-6.41396470396688,-19.6994280676216));
#42800=CARTESIAN_POINT('Ctrl Pts',(2.31865583139229,-6.3596505079741,-19.6913571974352));
#42801=CARTESIAN_POINT('Ctrl Pts',(2.47839234892487,-6.29913379034842,-19.6832863272488));
#42802=CARTESIAN_POINT('Ctrl Pts',(2.63584678961586,-6.2325436782803,-19.6752154570624));
#42803=CARTESIAN_POINT('Ctrl Pts',(2.7931052904937,-6.16603643243088,-19.6671546304466));
#42804=CARTESIAN_POINT('Ctrl Pts',(2.94808702594458,-6.09347097388618,-19.6590938038308));
#42805=CARTESIAN_POINT('Ctrl Pts',(3.10028130905614,-6.01502658387452,-19.651032977215));
#42806=CARTESIAN_POINT('Ctrl Pts',(3.25231957209563,-5.93666261015138,-19.6429804140552));
#42807=CARTESIAN_POINT('Ctrl Pts',(3.40157574060937,-5.85243186780364,-19.6349278508953));
#42808=CARTESIAN_POINT('Ctrl Pts',(3.54755770179896,-5.76256222113106,-19.6268752877355));
#42809=CARTESIAN_POINT('Ctrl Pts',(3.69342197603767,-5.67276502508598,-19.6188292163476));
#42810=CARTESIAN_POINT('Ctrl Pts',(3.83601698061662,-5.57733816728854,-19.6107831449597));
#42811=CARTESIAN_POINT('Ctrl Pts',(3.97487398102934,-5.47655601951956,-19.6027370735718));
#42812=CARTESIAN_POINT('Ctrl Pts',(4.11364941184123,-5.3758330748123,-19.5946957287359));
#42813=CARTESIAN_POINT('Ctrl Pts',(4.24869090868095,-5.26976132127368,-19.5866543839));
#42814=CARTESIAN_POINT('Ctrl Pts',(4.37955768302687,-5.15865907974547,-19.5786130390641));
#42815=CARTESIAN_POINT('Ctrl Pts',(4.51294716610432,-5.04541512886285,-19.5704166818431));
#42816=CARTESIAN_POINT('Ctrl Pts',(4.6419989966731,-4.92694497590987,-19.562220324622));
#42817=CARTESIAN_POINT('Ctrl Pts',(4.76628040783076,-4.80362988519397,-19.5540239674009));
#42818=CARTESIAN_POINT('Ctrl Pts',(4.88817260673625,-4.68268542998077,-19.5459851786924));
#42819=CARTESIAN_POINT('Ctrl Pts',(5.00547587849568,-4.55708091549586,-19.5379463899839));
#42820=CARTESIAN_POINT('Ctrl Pts',(5.11781836831975,-4.42721403919994,-19.5299076012754));
#42821=CARTESIAN_POINT('Ctrl Pts',(5.23017287980833,-4.29733326597132,-19.5218679523437));
#42822=CARTESIAN_POINT('Ctrl Pts',(5.33756530793048,-4.16318950515134,-19.513828303412));
#42823=CARTESIAN_POINT('Ctrl Pts',(5.43966361935346,-4.02521411955718,-19.5057886544802));
#42824=CARTESIAN_POINT('Ctrl Pts',(5.54179307207653,-3.88719664969317,-19.497746553352));
#42825=CARTESIAN_POINT('Ctrl Pts',(5.63862497187286,-3.74534552881586,-19.4897044522238));
#42826=CARTESIAN_POINT('Ctrl Pts',(5.72987029471872,-3.60012158207192,-19.4816623510955));
#42827=CARTESIAN_POINT('Ctrl Pts',(5.82419478871754,-3.44999689769468,-19.4733488606508));
#42828=CARTESIAN_POINT('Ctrl Pts',(5.91254882592503,-3.29626813509692,-19.465035370206));
#42829=CARTESIAN_POINT('Ctrl Pts',(5.99466493256604,-3.1394715074775,-19.4567218797613));
#42830=CARTESIAN_POINT('Ctrl Pts',(6.07424033842432,-2.9875262218276,-19.4486656115905));
#42831=CARTESIAN_POINT('Ctrl Pts',(6.14795798087953,-2.83270044954413,-19.4406093434197));
#42832=CARTESIAN_POINT('Ctrl Pts',(6.21562390031658,-2.67550154733898,-19.432553075249));
#42833=CARTESIAN_POINT('Ctrl Pts',(6.28653049793723,-2.51077402426975,-19.4241109736672));
#42834=CARTESIAN_POINT('Ctrl Pts',(6.35079128159519,-2.34344092609721,-19.4156688720855));
#42835=CARTESIAN_POINT('Ctrl Pts',(6.40824229486414,-2.17410204229573,-19.4072267705038));
#42836=CARTESIAN_POINT('Ctrl Pts',(6.46569330813309,-2.00476315849424,-19.398784668922));
#42837=CARTESIAN_POINT('Ctrl Pts',(6.51633450330733,-1.83341895554725,-19.3903425673403));
#42838=CARTESIAN_POINT('Ctrl Pts',(6.56006365577354,-1.66067872636436,-19.3819004657586));
#42839=CARTESIAN_POINT('Ctrl Pts',(6.60323203916829,-1.49015366423727,-19.3735666230659));
#42840=CARTESIAN_POINT('Ctrl Pts',(6.63980242160831,-1.31772619053291,-19.3652327803732));
#42841=CARTESIAN_POINT('Ctrl Pts',(6.66960917268499,-1.14394164345751,-19.3568989376805));
#42842=CARTESIAN_POINT('Ctrl Pts',(6.69938079273463,-0.970361923456567,
-19.3485749174758));
#42843=CARTESIAN_POINT('Ctrl Pts',(6.72240460365799,-0.79542865631812,-19.340250897271));
#42844=CARTESIAN_POINT('Ctrl Pts',(6.73856511291884,-0.619700910886155,
-19.3319268770663));
#42845=CARTESIAN_POINT('Ctrl Pts',(6.75470953798093,-0.444148063406899,
-19.3236111415754));
#42846=CARTESIAN_POINT('Ctrl Pts',(6.76400423914188,-0.267802657257806,
-19.3152954060846));
#42847=CARTESIAN_POINT('Ctrl Pts',(6.76638497210012,-0.0912327207618753,
-19.3069796705937));
#42848=CARTESIAN_POINT('Ctrl Pts',(6.76876377177906,0.0851938317380542,
-19.2986706879137));
#42849=CARTESIAN_POINT('Ctrl Pts',(6.76423978601747,0.261844204963231,-19.2903617052337));
#42850=CARTESIAN_POINT('Ctrl Pts',(6.75280066705504,0.43814626669764,-19.2820527225537));
#42851=CARTESIAN_POINT('Ctrl Pts',(6.74136874246237,0.614337447320704,-19.2737489656165));
#42852=CARTESIAN_POINT('Ctrl Pts',(6.72303037444839,0.790180406891127,-19.2654452086793));
#42853=CARTESIAN_POINT('Ctrl Pts',(6.69782529232956,0.965103804484467,-19.2571414517421));
#42854=CARTESIAN_POINT('Ctrl Pts',(6.6726304428665,1.13995618739502,-19.2488410659301));
#42855=CARTESIAN_POINT('Ctrl Pts',(6.64057448357458,1.31388940847959,-19.240540680118));
#42856=CARTESIAN_POINT('Ctrl Pts',(6.60174894418908,1.48633774018503,-19.232240294306));
#42857=CARTESIAN_POINT('Ctrl Pts',(6.56293159209956,1.65874970702462,-19.2239416588294));
#42858=CARTESIAN_POINT('Ctrl Pts',(6.51734758024701,1.82967706920284,-19.2156430233527));
#42859=CARTESIAN_POINT('Ctrl Pts',(6.46513950353293,1.99856453482442,-19.2073443878761));
#42860=CARTESIAN_POINT('Ctrl Pts',(6.4129337702025,2.16744441985409,-19.1990461248875));
#42861=CARTESIAN_POINT('Ctrl Pts',(6.35410466737922,2.334284258586,-19.1907478618989));
#42862=CARTESIAN_POINT('Ctrl Pts',(6.28884464858707,2.49854397318473,-19.1824495989104));
#42863=CARTESIAN_POINT('Ctrl Pts',(6.22357672708529,2.66282357893356,-19.1741503310376));
#42864=CARTESIAN_POINT('Ctrl Pts',(6.151876466812,2.82452211500237,-19.1658510631648));
#42865=CARTESIAN_POINT('Ctrl Pts',(6.07398451623223,2.9831193567424,-19.157551795292));
#42866=CARTESIAN_POINT('Ctrl Pts',(5.99603787294857,3.14182795930875,-19.1492466999955));
#42867=CARTESIAN_POINT('Ctrl Pts',(5.91189100566273,3.29743060375431,-19.140941604699));
#42868=CARTESIAN_POINT('Ctrl Pts',(5.82183101912393,3.44943076242537,-19.1326365094025));
#42869=CARTESIAN_POINT('Ctrl Pts',(5.73173819203074,3.60148634825858,-19.1243283856364));
#42870=CARTESIAN_POINT('Ctrl Pts',(5.63572813163984,3.74993653463364,-19.1160202618703));
#42871=CARTESIAN_POINT('Ctrl Pts',(5.53413148795322,3.89431350484841,-19.1077121381042));
#42872=CARTESIAN_POINT('Ctrl Pts',(5.43242684762144,4.03884394694823,-19.0993951828505));
#42873=CARTESIAN_POINT('Ctrl Pts',(5.32512396528859,4.17929224173099,-19.0910782275968));
#42874=CARTESIAN_POINT('Ctrl Pts',(5.21259468491312,4.31522254939598,-19.0827612723431));
#42875=CARTESIAN_POINT('Ctrl Pts',(5.12966231736792,4.41540111801554,-19.0766318028606));
#42876=CARTESIAN_POINT('Ctrl Pts',(5.04389210149061,4.51312643698517,-19.070502333378));
#42877=CARTESIAN_POINT('Ctrl Pts',(4.95544567355009,4.60823688372177,-19.0643728638955));
#42878=CARTESIAN_POINT('Ctrl Pts',(4.83347871531932,4.73939347369998,-19.0559203716268));
#42879=CARTESIAN_POINT('Ctrl Pts',(4.70619836508152,4.8658159181396,-19.0474678793582));
#42880=CARTESIAN_POINT('Ctrl Pts',(4.57399803204446,4.98706637241309,-19.0390153870896));
#42881=CARTESIAN_POINT('Ctrl Pts',(4.4419489224322,5.10817812878369,-19.0305725635926));
#42882=CARTESIAN_POINT('Ctrl Pts',(4.30499129864393,5.22412947218761,-19.0221297400956));
#42883=CARTESIAN_POINT('Ctrl Pts',(4.16355581478407,5.33451890775333,-19.0136869165986));
#42884=CARTESIAN_POINT('Ctrl Pts',(4.0222164140432,5.44483335109656,-19.0052498286694));
#42885=CARTESIAN_POINT('Ctrl Pts',(3.87640547584229,5.54959321322586,-18.9968127407403));
#42886=CARTESIAN_POINT('Ctrl Pts',(3.72658789699992,5.64843621243382,-18.9883756528111));
#42887=CARTESIAN_POINT('Ctrl Pts',(3.57686991233555,5.74721350381675,-18.9799441736019));
#42888=CARTESIAN_POINT('Ctrl Pts',(3.42315087482237,5.84008159441289,-18.9715126943926));
#42889=CARTESIAN_POINT('Ctrl Pts',(3.26592606587821,5.92672050397328,-18.9630812151834));
#42890=CARTESIAN_POINT('Ctrl Pts',(3.21073683449655,5.95713259261561,-18.960121587755));
#42891=CARTESIAN_POINT('Ctrl Pts',(3.15511589980604,5.98677753606144,-18.9571619603267));
#42892=CARTESIAN_POINT('Ctrl Pts',(3.09908550384715,6.01564277861015,-18.9542023328983));
#42893=CARTESIAN_POINT('Ctrl Pts',(3.09908550384717,6.01564277861014,-20.9542113918581));
#42894=CARTESIAN_POINT('Ctrl Pts',(2.92882038742808,6.10335845148578,-20.94517233765));
#42895=CARTESIAN_POINT('Ctrl Pts',(2.75477586505623,6.1838690702449,-20.9361332834419));
#42896=CARTESIAN_POINT('Ctrl Pts',(2.57755385392215,6.25687662737017,-20.9270942292338));
#42897=CARTESIAN_POINT('Ctrl Pts',(2.40051490507444,6.32980877100563,-20.9180645119581));
#42898=CARTESIAN_POINT('Ctrl Pts',(2.22030523965799,6.39525323423264,-20.9090347946824));
#42899=CARTESIAN_POINT('Ctrl Pts',(2.03754785581475,6.45295961054032,-20.9000050774067));
#42900=CARTESIAN_POINT('Ctrl Pts',(1.8551275642729,6.51055954860302,-20.890992015262));
#42901=CARTESIAN_POINT('Ctrl Pts',(1.67016916369237,6.56044982527673,-20.8819789531173));
#42902=CARTESIAN_POINT('Ctrl Pts',(1.48331185316542,6.60242947302423,-20.8729658909726));
#42903=CARTESIAN_POINT('Ctrl Pts',(1.29670371392215,6.64435314157194,-20.8639648476045));
#42904=CARTESIAN_POINT('Ctrl Pts',(1.10820194925722,6.67838717830084,-20.8549638042364));
#42905=CARTESIAN_POINT('Ctrl Pts',(0.918459496959166,6.70438074339797,-20.8459627608683));
#42906=CARTESIAN_POINT('Ctrl Pts',(0.729118848265548,6.7303192638384,-20.8369807783462));
#42907=CARTESIAN_POINT('Ctrl Pts',(0.538542991287307,6.74825126235499,-20.8279987958241));
#42908=CARTESIAN_POINT('Ctrl Pts',(0.347393559309,6.75807714627102,-20.8190168133021));
#42909=CARTESIAN_POINT('Ctrl Pts',(0.288925390215197,6.76108265581584,-20.8162694335821));
#42910=CARTESIAN_POINT('Ctrl Pts',(0.230403634598677,6.76333011234689,-20.8135220538621));
#42911=CARTESIAN_POINT('Ctrl Pts',(0.171847416073251,6.76481762249279,-20.8107746741422));
#42912=CARTESIAN_POINT('Ctrl Pts',(-0.00128534660343033,6.7692157333605,
-20.8026515156969));
#42913=CARTESIAN_POINT('Ctrl Pts',(-0.174642473794895,6.76696439773253,
-20.7945283572516));
#42914=CARTESIAN_POINT('Ctrl Pts',(-0.347671132330947,6.75806287213605,
-20.7864051988064));
#42915=CARTESIAN_POINT('Ctrl Pts',(-0.520687591441088,6.74916197414371,
-20.7782826130863));
#42916=CARTESIAN_POINT('Ctrl Pts',(-0.693375262484683,6.73361183893786,
-20.7701600273662));
#42917=CARTESIAN_POINT('Ctrl Pts',(-0.865183633320813,6.71146379567333,
-20.7620374416461));
#42918=CARTESIAN_POINT('Ctrl Pts',(-1.03701264870072,6.68931309109348,-20.7539138799137));
#42919=CARTESIAN_POINT('Ctrl Pts',(-1.20796179062591,6.6605629477761,-20.7457903181814));
#42920=CARTESIAN_POINT('Ctrl Pts',(-1.37748801595936,6.62531627666849,-20.737666756449));
#42921=CARTESIAN_POINT('Ctrl Pts',(-1.5471377210312,6.5900439325435,-20.7295372776659));
#42922=CARTESIAN_POINT('Ctrl Pts',(-1.71536208077116,6.54826568426473,-20.7214077988828));
#42923=CARTESIAN_POINT('Ctrl Pts',(-1.88162993016014,6.50013521443405,-20.7132783200997));
#42924=CARTESIAN_POINT('Ctrl Pts',(-2.04796556402496,6.45198512265793,-20.7051455270712));
#42925=CARTESIAN_POINT('Ctrl Pts',(-2.21234275044118,6.39747776243313,-20.6970127340427));
#42926=CARTESIAN_POINT('Ctrl Pts',(-2.37424797790894,6.33681588334357,-20.6888799410141));
#42927=CARTESIAN_POINT('Ctrl Pts',(-2.53632925274934,6.27608804366336,-20.680738304807));
#42928=CARTESIAN_POINT('Ctrl Pts',(-2.69593286293405,6.20919246016743,-20.6725966685999));
#42929=CARTESIAN_POINT('Ctrl Pts',(-2.85256698655622,6.13637927341601,-20.6644550323927));
#42930=CARTESIAN_POINT('Ctrl Pts',(-2.93236994499914,6.09928194377897,-20.6603069793321));
#42931=CARTESIAN_POINT('Ctrl Pts',(-3.01140249969909,6.0606492768492,-20.6561589262714));
#42932=CARTESIAN_POINT('Ctrl Pts',(-3.0896023418646,6.02051877907085,-20.6520108732108));
#42933=CARTESIAN_POINT('Ctrl Pts',(-3.24872821836542,5.93885875960588,-20.6435701582327));
#42934=CARTESIAN_POINT('Ctrl Pts',(-3.40473220353192,5.85082586380949,-20.6351294432546));
#42935=CARTESIAN_POINT('Ctrl Pts',(-3.55708975953537,5.75668319804109,-20.6266887282765));
#42936=CARTESIAN_POINT('Ctrl Pts',(-3.70933215651976,5.66261168973496,-20.6182543931885));
#42937=CARTESIAN_POINT('Ctrl Pts',(-3.85793333592621,5.56243979189851,-20.6098200581005));
#42938=CARTESIAN_POINT('Ctrl Pts',(-4.00239371274686,5.45647629594085,-20.6013857230125));
#42939=CARTESIAN_POINT('Ctrl Pts',(-4.1467670831485,5.35057662028141,-20.5929564678039));
#42940=CARTESIAN_POINT('Ctrl Pts',(-4.28700435484837,5.23889249745418,-20.5845272125952));
#42941=CARTESIAN_POINT('Ctrl Pts',(-4.42263494853166,5.12177597245588,-20.5760979573866));
#42942=CARTESIAN_POINT('Ctrl Pts',(-4.55820465855936,5.00471202027304,-20.5676724860136));
#42943=CARTESIAN_POINT('Ctrl Pts',(-4.68917156182421,4.88222074571305,-20.5592470146406));
#42944=CARTESIAN_POINT('Ctrl Pts',(-4.81509789671109,4.75469465319157,-20.5508215432676));
#42945=CARTESIAN_POINT('Ctrl Pts',(-4.94098700412073,4.62720626108207,-20.5423985627084));
#42946=CARTESIAN_POINT('Ctrl Pts',(-5.06183828081076,4.49468625628662,-20.5339755821491));
#42947=CARTESIAN_POINT('Ctrl Pts',(-5.17725032162532,4.35756446965854,-20.5255526015899));
#42948=CARTESIAN_POINT('Ctrl Pts',(-5.29266427342344,4.22044041257863,-20.5171294815635));
#42949=CARTESIAN_POINT('Ctrl Pts',(-5.40263858969954,4.07871467219305,-20.5087063615372));
#42950=CARTESIAN_POINT('Ctrl Pts',(-5.50681128787152,3.93285118454421,-20.5002832415109));
#42951=CARTESIAN_POINT('Ctrl Pts',(-5.61098758850913,3.78698265269271,-20.491859830199));
#42952=CARTESIAN_POINT('Ctrl Pts',(-5.70936167704904,3.63697635957528,-20.4834364188871));
#42953=CARTESIAN_POINT('Ctrl Pts',(-5.80161407269013,3.48332644918099,-20.4750130075753));
#42954=CARTESIAN_POINT('Ctrl Pts',(-5.89388252452679,3.3296497965759,-20.4665881301992));
#42955=CARTESIAN_POINT('Ctrl Pts',(-5.98002698759351,3.17232854828038,-20.4581632528231));
#42956=CARTESIAN_POINT('Ctrl Pts',(-6.05977305275952,3.01188305700098,-20.449738375447));
#42957=CARTESIAN_POINT('Ctrl Pts',(-6.1395441226356,2.85138725737118,-20.4413108564155));
#42958=CARTESIAN_POINT('Ctrl Pts',(-6.21291264632887,2.68776556018021,-20.4328833373841));
#42959=CARTESIAN_POINT('Ctrl Pts',(-6.27965147295604,2.52156030627884,-20.4244558183527));
#42960=CARTESIAN_POINT('Ctrl Pts',(-6.34645014838363,2.35520600592923,-20.4160207418479));
#42961=CARTESIAN_POINT('Ctrl Pts',(-6.40660712288565,2.18626382926887,-20.4075856653431));
#42962=CARTESIAN_POINT('Ctrl Pts',(-6.4599440620716,2.01529444868631,-20.3991505888384));
#42963=CARTESIAN_POINT('Ctrl Pts',(-6.51330677935141,1.84424243747654,-20.3907114356056));
#42964=CARTESIAN_POINT('Ctrl Pts',(-6.55984279598541,1.67116158884748,-20.3822722823728));
#42965=CARTESIAN_POINT('Ctrl Pts',(-6.59942431532174,1.49662543956069,-20.37383312914));
#42966=CARTESIAN_POINT('Ctrl Pts',(-6.63904982082356,1.32189533167719,-20.3653845976419));
#42967=CARTESIAN_POINT('Ctrl Pts',(-6.67170532081396,1.1457070186125,-20.3569360661438));
#42968=CARTESIAN_POINT('Ctrl Pts',(-6.6973143557294,0.968643082121012,-20.3484875346457));
#42969=CARTESIAN_POINT('Ctrl Pts',(-6.71146417840731,0.87080951235629,-20.3438194468797));
#42970=CARTESIAN_POINT('Ctrl Pts',(-6.72346369021172,0.772708718850963,
-20.3391513591137));
#42971=CARTESIAN_POINT('Ctrl Pts',(-6.73330680843928,0.674439340063505,
-20.3344832713477));
#42972=CARTESIAN_POINT('Ctrl Pts',(-6.75556168816653,0.452256373728216,
-20.3239289196285));
#42973=CARTESIAN_POINT('Ctrl Pts',(-6.76683268631128,0.22880640812643,-20.3133745679092));
#42974=CARTESIAN_POINT('Ctrl Pts',(-6.76699815055647,0.00500303560476391,
-20.30282021619));
#42975=CARTESIAN_POINT('',(-6.76699940505972,-0.0028375907681064,-20.6971797837861));
#42976=CARTESIAN_POINT('Ctrl Pts',(3.09908550384722,6.01564277861012,-21.3487227114526));
#42977=CARTESIAN_POINT('Ctrl Pts',(2.94376984384265,6.09565692309225,-21.3405091353549));
#42978=CARTESIAN_POINT('Ctrl Pts',(2.78546096918994,6.16959676464732,-21.3322955592572));
#42979=CARTESIAN_POINT('Ctrl Pts',(2.62468011135187,6.23725446916141,-21.3240819831595));
#42980=CARTESIAN_POINT('Ctrl Pts',(2.46379495760027,6.30495606212213,-21.3158630790492));
#42981=CARTESIAN_POINT('Ctrl Pts',(2.3004349593365,6.36636726981934,-21.307644174939));
#42982=CARTESIAN_POINT('Ctrl Pts',(2.13513727481221,6.42132991036183,-21.2994252708288));
#42983=CARTESIAN_POINT('Ctrl Pts',(1.96960157265642,6.47637169343775,-21.2911945320453));
#42984=CARTESIAN_POINT('Ctrl Pts',(1.80212295443262,6.52494626216037,-21.2829637932618));
#42985=CARTESIAN_POINT('Ctrl Pts',(1.63325058337474,6.56694613438439,-21.2747330544783));
#42986=CARTESIAN_POINT('Ctrl Pts',(1.54365516646979,6.58922921146972,-21.2703662272221));
#42987=CARTESIAN_POINT('Ctrl Pts',(1.45366756059266,6.60966248588322,-21.265999399966));
#42988=CARTESIAN_POINT('Ctrl Pts',(1.36337035817647,6.62823583364728,-21.2616325727098));
#42989=CARTESIAN_POINT('Ctrl Pts',(1.19648099980474,6.66256352053254,-21.2535617025234));
#42990=CARTESIAN_POINT('Ctrl Pts',(1.02798955814346,6.69064665127868,-21.245490832337));
#42991=CARTESIAN_POINT('Ctrl Pts',(0.858414069773042,6.71233299865372,-21.2374199621506));
#42992=CARTESIAN_POINT('Ctrl Pts',(0.689049604917057,6.73399235905511,-21.2293591355348));
#42993=CARTESIAN_POINT('Ctrl Pts',(0.518604142883801,6.74927072839133,-21.221298308919));
#42994=CARTESIAN_POINT('Ctrl Pts',(0.347609218017789,6.75806605705723,-21.2132374823032));
#42995=CARTESIAN_POINT('Ctrl Pts',(0.176789586467174,6.7668523693016,-21.2051849191433));
#42996=CARTESIAN_POINT('Ctrl Pts',(0.00542198239936081,6.76916884768676,
-21.1971323559835));
#42997=CARTESIAN_POINT('Ctrl Pts',(-0.165953663895494,6.76496477311151,
-21.1890797928236));
#42998=CARTESIAN_POINT('Ctrl Pts',(-0.33719115149453,6.76076408775447,-21.1810337214357));
#42999=CARTESIAN_POINT('Ctrl Pts',(-0.508436297411776,6.75005332122249,
-21.1729876500478));
#43000=CARTESIAN_POINT('Ctrl Pts',(-0.679145971473218,6.73283370873154,
-21.1649415786599));
#43001=CARTESIAN_POINT('Ctrl Pts',(-0.849755364526388,6.7156242116609,-21.1569002338241));
#43002=CARTESIAN_POINT('Ctrl Pts',(-1.01982954173331,6.69191351756044,-21.1488588889882));
#43003=CARTESIAN_POINT('Ctrl Pts',(-1.18882740769602,6.66175490353036,-21.1408175441523));
#43004=CARTESIAN_POINT('Ctrl Pts',(-1.36108303250737,6.63101492421995,-21.1326211869312));
#43005=CARTESIAN_POINT('Ctrl Pts',(-1.53222003083641,6.59357590825049,-21.1244248297102));
#43006=CARTESIAN_POINT('Ctrl Pts',(-1.70167256602109,6.54954956298914,-21.1162284724891));
#43007=CARTESIAN_POINT('Ctrl Pts',(-1.86786750966858,6.50636958954265,-21.1081896837806));
#43008=CARTESIAN_POINT('Ctrl Pts',(-2.03244179881798,6.4568533803236,-21.1001508950721));
#43009=CARTESIAN_POINT('Ctrl Pts',(-2.19487396594561,6.40115749482968,-21.0921121063636));
#43010=CARTESIAN_POINT('Ctrl Pts',(-2.35732351478699,6.34545564937133,-21.0840724574319));
#43011=CARTESIAN_POINT('Ctrl Pts',(-2.51763013184477,6.28357293197529,-21.0760328085002));
#43012=CARTESIAN_POINT('Ctrl Pts',(-2.67528982156531,6.21571503293298,-21.0679931595685));
#43013=CARTESIAN_POINT('Ctrl Pts',(-2.83299759952107,6.14783643635781,-21.0599510584403));
#43014=CARTESIAN_POINT('Ctrl Pts',(-2.98805650026762,6.07397917800655,-21.0519089573121));
#43015=CARTESIAN_POINT('Ctrl Pts',(-3.13998487003631,5.99439605097487,-21.043866856184));
#43016=CARTESIAN_POINT('Ctrl Pts',(-3.29704022537577,5.91212730607873,-21.0355533657392));
#43017=CARTESIAN_POINT('Ctrl Pts',(-3.45074967952638,5.82373968225327,-21.0272398752944));
#43018=CARTESIAN_POINT('Ctrl Pts',(-3.60061226632843,5.72956196471993,-21.0189263848497));
#43019=CARTESIAN_POINT('Ctrl Pts',(-3.74583805278521,5.63829813838848,-21.0108701166789));
#43020=CARTESIAN_POINT('Ctrl Pts',(-3.88745121120484,5.5415974458643,-21.0028138485082));
#43021=CARTESIAN_POINT('Ctrl Pts',(-4.02502882471039,5.43980072799091,-20.9947575803374));
#43022=CARTESIAN_POINT('Ctrl Pts',(-4.16919534995163,5.33312872865306,-20.9863154787556));
#43023=CARTESIAN_POINT('Ctrl Pts',(-4.30892990245549,5.22086088420463,-20.9778733771739));
#43024=CARTESIAN_POINT('Ctrl Pts',(-4.44378898078276,5.103433010658,-20.9694312755921));
#43025=CARTESIAN_POINT('Ctrl Pts',(-4.57864805911003,4.98600513711137,-20.9609891740104));
#43026=CARTESIAN_POINT('Ctrl Pts',(-4.70863138729938,4.86341761358131,-20.9525470724286));
#43027=CARTESIAN_POINT('Ctrl Pts',(-4.83334402845879,4.73614553224052,-20.9441049708468));
#43028=CARTESIAN_POINT('Ctrl Pts',(-4.9558363074393,4.61113938090659,-20.9358131709738));
#43029=CARTESIAN_POINT('Ctrl Pts',(-5.07364241516591,4.48120821135264,-20.9275213711007));
#43030=CARTESIAN_POINT('Ctrl Pts',(-5.1863463975287,4.34673441158315,-20.9192295712277));
#43031=CARTESIAN_POINT('Ctrl Pts',(-5.29891343238729,4.21242401199591,-20.9109478467865));
#43032=CARTESIAN_POINT('Ctrl Pts',(-5.40639046637114,4.07358224496628,-20.9026661223453));
#43033=CARTESIAN_POINT('Ctrl Pts',(-5.50839779121519,3.9306288013161,-20.8943843979041));
#43034=CARTESIAN_POINT('Ctrl Pts',(-5.61027524080661,3.78785736532699,-20.8861132177161));
#43035=CARTESIAN_POINT('Ctrl Pts',(-5.70669666066461,3.64098497389965,-20.877842037528));
#43036=CARTESIAN_POINT('Ctrl Pts',(-5.79732225400218,3.4904646801323,-20.86957085734));
#43037=CARTESIAN_POINT('Ctrl Pts',(-5.8878808627161,3.34005564130806,-20.8613057906776));
#43038=CARTESIAN_POINT('Ctrl Pts',(-5.97265199587638,3.18600437059106,-20.8530407240153));
#43039=CARTESIAN_POINT('Ctrl Pts',(-6.05133844476635,3.0287938237676,-20.8447756573529));
#43040=CARTESIAN_POINT('Ctrl Pts',(-6.12998036878378,2.87167223482263,-20.8365152674938));
#43041=CARTESIAN_POINT('Ctrl Pts',(-6.20254430962975,2.7113952450136,-20.8282548776346));
#43042=CARTESIAN_POINT('Ctrl Pts',(-6.26877834314064,2.54847151927796,-20.8199944877755));
#43043=CARTESIAN_POINT('Ctrl Pts',(-6.33498637325979,2.38561175717613,-20.8117373409342));
#43044=CARTESIAN_POINT('Ctrl Pts',(-6.39486931500216,2.22010765550495,-20.803480194093));
#43045=CARTESIAN_POINT('Ctrl Pts',(-6.44822280095868,2.0524891495929,-20.7952230472517));
#43046=CARTESIAN_POINT('Ctrl Pts',(-6.50157393681254,1.88487802690407,-20.7869662641194));
#43047=CARTESIAN_POINT('Ctrl Pts',(-6.54839607469187,1.7151530185966,-20.7787094809872));
#43048=CARTESIAN_POINT('Ctrl Pts',(-6.58853415249703,1.54386097864422,-20.7704526978549));
#43049=CARTESIAN_POINT('Ctrl Pts',(-6.62866964037057,1.37257999140522,-20.7621964474961));
#43050=CARTESIAN_POINT('Ctrl Pts',(-6.66212185064965,1.19973251806868,-20.7539401971373));
#43051=CARTESIAN_POINT('Ctrl Pts',(-6.68878650618458,1.02587722203155,-20.7456839467786));
#43052=CARTESIAN_POINT('Ctrl Pts',(-6.71546374862139,0.851939858571766,
-20.7374237991028));
#43053=CARTESIAN_POINT('Ctrl Pts',(-6.73534698013193,0.676994070549397,
-20.7291636514271));
#43054=CARTESIAN_POINT('Ctrl Pts',(-6.74838353860457,0.501606036537511,
-20.7209035037514));
#43055=CARTESIAN_POINT('Ctrl Pts',(-6.76086417350953,0.333697149863501,
-20.7129955971043));
#43056=CARTESIAN_POINT('Ctrl Pts',(-6.7670699447143,0.165383243452747,-20.7050876904571));
#43057=CARTESIAN_POINT('Ctrl Pts',(-6.76699940505994,-0.002837590259075,
-20.69717978381));
#43058=CARTESIAN_POINT('Ctrl Pts',(-6.76699940505972,-0.00283759076810723,
-20.697179783786));
#43059=CARTESIAN_POINT('Ctrl Pts',(-6.76690610989687,-0.225325032808874,
-20.686720853801));
#43060=CARTESIAN_POINT('Ctrl Pts',(-6.75583636494396,-0.447452435014028,
-20.6762619238159));
#43061=CARTESIAN_POINT('Ctrl Pts',(-6.73391989437842,-0.668290248390996,
-20.6658029938309));
#43062=CARTESIAN_POINT('Ctrl Pts',(-6.71173178705549,-0.891865166146056,
-20.6552144339486));
#43063=CARTESIAN_POINT('Ctrl Pts',(-6.67842640940602,-1.11411854687437,
-20.6446258740662));
#43064=CARTESIAN_POINT('Ctrl Pts',(-6.63418845455005,-1.33410365021419,
-20.6340373141839));
#43065=CARTESIAN_POINT('Ctrl Pts',(-6.62379948372796,-1.3857655958745,-20.6315506657839));
#43066=CARTESIAN_POINT('Ctrl Pts',(-6.61280778413403,-1.43730251158528,
-20.6290640173838));
#43067=CARTESIAN_POINT('Ctrl Pts',(-6.60121614522909,-1.48870225497473,
-20.6265773689837));
#43068=CARTESIAN_POINT('Ctrl Pts',(-6.56182126613055,-1.66338736146639,
-20.6181263454585));
#43069=CARTESIAN_POINT('Ctrl Pts',(-6.51545491227376,-1.83665557159931,
-20.6096753219333));
#43070=CARTESIAN_POINT('Ctrl Pts',(-6.46223666432076,-2.00793084898572,
-20.6012242984081));
#43071=CARTESIAN_POINT('Ctrl Pts',(-6.40906527345337,-2.17905532358093,
-20.5927807157579));
#43072=CARTESIAN_POINT('Ctrl Pts',(-6.34905411108343,-2.34819004782845,
-20.5843371331077));
#43073=CARTESIAN_POINT('Ctrl Pts',(-6.28237334123594,-2.51477120258047,
-20.5758935504575));
#43074=CARTESIAN_POINT('Ctrl Pts',(-6.21574221729914,-2.68122833247269,
-20.5674562543177));
#43075=CARTESIAN_POINT('Ctrl Pts',(-6.1424515076189,-2.84513537610459,-20.5590189581778));
#43076=CARTESIAN_POINT('Ctrl Pts',(-6.06272067319979,-3.00594528206284,
-20.550581662038));
#43077=CARTESIAN_POINT('Ctrl Pts',(-5.9830467206515,-3.1666404624151,-20.5421503852656));
#43078=CARTESIAN_POINT('Ctrl Pts',(-5.89694195483159,-3.32424261618742,
-20.5337191084932));
#43079=CARTESIAN_POINT('Ctrl Pts',(-5.80467334503278,-3.47822603599392,
-20.5252878317209));
#43080=CARTESIAN_POINT('Ctrl Pts',(-5.71244428489993,-3.63214345293304,
-20.5168601688989));
#43081=CARTESIAN_POINT('Ctrl Pts',(-5.61405681789739,-3.78244494431092,
-20.5084325060769));
#43082=CARTESIAN_POINT('Ctrl Pts',(-5.50982342841356,-3.92863014137308,
-20.5000048432549));
#43083=CARTESIAN_POINT('Ctrl Pts',(-5.40562212608989,-4.07477033684934,
-20.4915797748009));
#43084=CARTESIAN_POINT('Ctrl Pts',(-5.29557868237724,-4.21679649545947,
-20.4831547063469));
#43085=CARTESIAN_POINT('Ctrl Pts',(-5.18004860928113,-4.35423763769097,
-20.4747296378929));
#43086=CARTESIAN_POINT('Ctrl Pts',(-5.14843604500035,-4.39184574116723,
-20.4724242812794));
#43087=CARTESIAN_POINT('Ctrl Pts',(-5.11641291745343,-4.42911072769324,
-20.4701189246659));
#43088=CARTESIAN_POINT('Ctrl Pts',(-5.08398704627483,-4.46602336685666,
-20.4678135680524));
#43089=CARTESIAN_POINT('Ctrl Pts',(-4.96275712030799,-4.60402787838927,
-20.4591945795279));
#43090=CARTESIAN_POINT('Ctrl Pts',(-4.83594889133726,-4.73704311541802,
-20.4505755910034));
#43091=CARTESIAN_POINT('Ctrl Pts',(-4.70400004711802,-4.8646348842142,-20.441956602479));
#43092=CARTESIAN_POINT('Ctrl Pts',(-4.57197215376572,-4.99230309186642,
-20.4333324504112));
#43093=CARTESIAN_POINT('Ctrl Pts',(-4.43479771769685,-5.11454113556306,
-20.4247082983434));
#43094=CARTESIAN_POINT('Ctrl Pts',(-4.2929493115592,-5.23095356587911,-20.4160841462757));
#43095=CARTESIAN_POINT('Ctrl Pts',(-4.14624255934967,-5.35135315325208,
-20.4071646146794));
#43096=CARTESIAN_POINT('Ctrl Pts',(-3.99453628083196,-5.46552078351104,
-20.3982450830832));
#43097=CARTESIAN_POINT('Ctrl Pts',(-3.83838748395861,-5.57306652777355,
-20.3893255514869));
#43098=CARTESIAN_POINT('Ctrl Pts',(-3.68712846223965,-5.67724449387327,
-20.3806853336277));
#43099=CARTESIAN_POINT('Ctrl Pts',(-3.5317012273828,-5.77520890086533,-20.3720451157685));
#43100=CARTESIAN_POINT('Ctrl Pts',(-3.37263914307193,-5.86665102171751,
-20.3634048979093));
#43101=CARTESIAN_POINT('Ctrl Pts',(-3.20586401970692,-5.96252723918285,
-20.3543457094445));
#43102=CARTESIAN_POINT('Ctrl Pts',(-3.03509311409394,-6.05123272490519,
-20.3452865209797));
#43103=CARTESIAN_POINT('Ctrl Pts',(-2.86096765872771,-6.13246712634598,
-20.336227332515));
#43104=CARTESIAN_POINT('Ctrl Pts',(-2.68684220336148,-6.21370152778676,
-20.3271681440502));
#43105=CARTESIAN_POINT('Ctrl Pts',(-2.50936256428131,-6.28746472868872,
-20.3181089555854));
#43106=CARTESIAN_POINT('Ctrl Pts',(-2.32919171885676,-6.35351516381358,
-20.3090497671206));
#43107=CARTESIAN_POINT('Ctrl Pts',(-2.14933300678128,-6.41945117119363,
-20.3000062730643));
#43108=CARTESIAN_POINT('Ctrl Pts',(-1.96662700198859,-6.4777626523508,-20.290962779008));
#43109=CARTESIAN_POINT('Ctrl Pts',(-1.78170898057334,-6.52823116230916,
-20.2819192849516));
#43110=CARTESIAN_POINT('Ctrl Pts',(-1.59696010299598,-6.57865350890602,
-20.2728840629462));
#43111=CARTESIAN_POINT('Ctrl Pts',(-1.41000347785843,-6.62124714446272,
-20.2638488409408));
#43112=CARTESIAN_POINT('Ctrl Pts',(-1.2214891677209,-6.65584353881163,-20.2548136189355));
#43113=CARTESIAN_POINT('Ctrl Pts',(-1.03330697875866,-6.69037898184526,
-20.2457943150243));
#43114=CARTESIAN_POINT('Ctrl Pts',(-0.843572818697793,-6.71694527552576,
-20.2367750111131));
#43115=CARTESIAN_POINT('Ctrl Pts',(-0.65294639234871,-6.73542500579725,
-20.2277557072019));
#43116=CARTESIAN_POINT('Ctrl Pts',(-0.46255912016646,-6.75388155195632,
-20.2187477186375));
#43117=CARTESIAN_POINT('Ctrl Pts',(-0.27128205192631,-6.76427175805119,
-20.2097397300731));
#43118=CARTESIAN_POINT('Ctrl Pts',(-0.0797819989741408,-6.76652967425989,
-20.2007317415087));
#43119=CARTESIAN_POINT('Ctrl Pts',(0.111285544400721,-6.76878249088575,
-20.1917440978019));
#43120=CARTESIAN_POINT('Ctrl Pts',(0.302574829586595,-6.76293967716026,
-20.1827564540952));
#43121=CARTESIAN_POINT('Ctrl Pts',(0.493417520390925,-6.74898719442935,
-20.1737688103885));
#43122=CARTESIAN_POINT('Ctrl Pts',(0.659628276733426,-6.73683554902031,
-20.1659411956554));
#43123=CARTESIAN_POINT('Ctrl Pts',(0.825500093690068,-6.71853332503442,
-20.1581135809224));
#43124=CARTESIAN_POINT('Ctrl Pts',(0.990589840914559,-6.69410343265451,
-20.1502859661894));
#43125=CARTESIAN_POINT('Ctrl Pts',(1.16191280712198,-6.66875115186773,-20.1421628077441));
#43126=CARTESIAN_POINT('Ctrl Pts',(1.33231670434845,-6.63680942570651,-20.1340396492988));
#43127=CARTESIAN_POINT('Ctrl Pts',(1.50125675876329,-6.59837231021921,-20.1259164908535));
#43128=CARTESIAN_POINT('Ctrl Pts',(1.67018490202014,-6.55993790474971,-20.1177939051335));
#43129=CARTESIAN_POINT('Ctrl Pts',(1.83764905114325,-6.51500910336602,-20.1096713194134));
#43130=CARTESIAN_POINT('Ctrl Pts',(2.00311564730734,-6.4637308656466,-20.1015487336933));
#43131=CARTESIAN_POINT('Ctrl Pts',(2.16860212598614,-6.4124464663191,-20.0934251719609));
#43132=CARTESIAN_POINT('Ctrl Pts',(2.33209022449831,-6.35481122093328,-20.0853016102286));
#43133=CARTESIAN_POINT('Ctrl Pts',(2.49306258660471,-6.291019626362,-20.0771780484962));
#43134=CARTESIAN_POINT('Ctrl Pts',(2.65415219797476,-6.22718156718405,-20.0690485697131));
#43135=CARTESIAN_POINT('Ctrl Pts',(2.81272207249889,-6.15717833774076,-20.06091909093));
#43136=CARTESIAN_POINT('Ctrl Pts',(2.96827526143845,-6.08125241807413,-20.0527896121469));
#43137=CARTESIAN_POINT('Ctrl Pts',(3.12389186667537,-6.00529554474638,-20.0446568191184));
#43138=CARTESIAN_POINT('Ctrl Pts',(3.27648901257774,-5.92341134117101,-20.0365240260899));
#43139=CARTESIAN_POINT('Ctrl Pts',(3.42559555549937,-5.83588760088326,-20.0283912330614));
#43140=CARTESIAN_POINT('Ctrl Pts',(3.57486422916567,-5.74826869180606,-20.0202495968542));
#43141=CARTESIAN_POINT('Ctrl Pts',(3.72063441109514,-5.65499819520947,-20.0121079606471));
#43142=CARTESIAN_POINT('Ctrl Pts',(3.86246445167112,-5.55640687491268,-20.00396632444));
#43143=CARTESIAN_POINT('Ctrl Pts',(3.93472493088678,-5.50617593637372,-19.9998182713792));
#43144=CARTESIAN_POINT('Ctrl Pts',(4.0059631669425,-5.45456449015567,-19.9956702183184));
#43145=CARTESIAN_POINT('Ctrl Pts',(4.07612420460438,-5.4016201707116,-19.9915221652576));
#43146=CARTESIAN_POINT('Ctrl Pts',(4.21889222439334,-5.2938857942257,-19.9830814502795));
#43147=CARTESIAN_POINT('Ctrl Pts',(4.35749189409003,-5.1804081942767,-19.9746407353014));
#43148=CARTESIAN_POINT('Ctrl Pts',(4.49145155575035,-5.06153651793087,-19.9662000203233));
#43149=CARTESIAN_POINT('Ctrl Pts',(4.62530996438702,-4.94275469039855,-19.9577656852353));
#43150=CARTESIAN_POINT('Ctrl Pts',(4.75453510776097,-4.8185871344218,-19.9493313501472));
#43151=CARTESIAN_POINT('Ctrl Pts',(4.87868774436357,-4.68942372717552,-19.9408970150592));
#43152=CARTESIAN_POINT('Ctrl Pts',(5.00276560560868,-4.56033811320223,-19.9324677598506));
#43153=CARTESIAN_POINT('Ctrl Pts',(5.12177682040649,-4.42626288648985,-19.924038504642));
#43154=CARTESIAN_POINT('Ctrl Pts',(5.23531813964038,-4.28762556396339,-19.9156092494333));
#43155=CARTESIAN_POINT('Ctrl Pts',(5.34880849094456,-4.14905047479266,-19.9071837780603));
#43156=CARTESIAN_POINT('Ctrl Pts',(5.45683363158883,-4.00591763061263,-19.8987583066873));
#43157=CARTESIAN_POINT('Ctrl Pts',(5.55902958131697,-3.8586887817033,-19.8903328353143));
#43158=CARTESIAN_POINT('Ctrl Pts',(5.6611953189577,-3.71150345791277,-19.881909854755));
#43159=CARTESIAN_POINT('Ctrl Pts',(5.7575351123742,-3.56022481780452,-19.8734868741958));
#43160=CARTESIAN_POINT('Ctrl Pts',(5.84772719934591,-3.40534515167407,-19.8650638936365));
#43161=CARTESIAN_POINT('Ctrl Pts',(5.93792077971138,-3.25046292105781,-19.8566407736102));
#43162=CARTESIAN_POINT('Ctrl Pts',(6.02196627679717,-3.09197983001042,-19.8482176535838));
#43163=CARTESIAN_POINT('Ctrl Pts',(6.09958661481354,-2.9304150095827,-19.8397945335575));
#43164=CARTESIAN_POINT('Ctrl Pts',(6.17720963707058,-2.76884460197417,-19.8313711222456));
#43165=CARTESIAN_POINT('Ctrl Pts',(6.24840691266008,-2.60419255303586,-19.8229477109338));
#43166=CARTESIAN_POINT('Ctrl Pts',(6.31294841761153,-2.43700046708574,-19.8145242996219));
#43167=CARTESIAN_POINT('Ctrl Pts',(6.37750115577832,-2.26977928195817,-19.8060994222458));
#43168=CARTESIAN_POINT('Ctrl Pts',(6.43539569367677,-2.10001748954333,-19.7976745448697));
#43169=CARTESIAN_POINT('Ctrl Pts',(6.48645090528201,-1.92827478678902,-19.7892496674935));
#43170=CARTESIAN_POINT('Ctrl Pts',(6.53752212546106,-1.7564782333964,-19.7808221484621));
#43171=CARTESIAN_POINT('Ctrl Pts',(6.58174964880295,-1.58269985085183,-19.7723946294307));
#43172=CARTESIAN_POINT('Ctrl Pts',(6.61900267776738,-1.40751289575201,-19.7639671103992));
#43173=CARTESIAN_POINT('Ctrl Pts',(6.65628911380841,-1.23216883976163,-19.7555320338944));
#43174=CARTESIAN_POINT('Ctrl Pts',(6.68658848873907,-1.0554140137599,-19.7470969573896));
#43175=CARTESIAN_POINT('Ctrl Pts',(6.70982124171321,-0.87783136436004,-19.7386618808848));
#43176=CARTESIAN_POINT('Ctrl Pts',(6.73306522322976,-0.700162888097009,
-19.7302227276521));
#43177=CARTESIAN_POINT('Ctrl Pts',(6.74923573608721,-0.521666121963206,
-19.7217835744193));
#43178=CARTESIAN_POINT('Ctrl Pts',(6.75830521449227,-0.342928021261989,
-19.7133444211865));
#43179=CARTESIAN_POINT('Ctrl Pts',(6.76738477163065,-0.163991292417934,
-19.7048958896884));
#43180=CARTESIAN_POINT('Ctrl Pts',(6.76934751775323,0.0151869734734661,
-19.6964473581903));
#43181=CARTESIAN_POINT('Ctrl Pts',(6.76421801476277,0.194019712294481,-19.6879988266921));
#43182=CARTESIAN_POINT('Ctrl Pts',(6.76138379793354,0.292830602730925,-19.6833307389264));
#43183=CARTESIAN_POINT('Ctrl Pts',(6.75638529577431,0.391536068360939,-19.6786626511606));
#43184=CARTESIAN_POINT('Ctrl Pts',(6.74923342816245,0.490037888509266,-19.6739945633948));
#43185=CARTESIAN_POINT('Ctrl Pts',(6.73660792944772,0.663927377405493,-19.6657537877981));
#43186=CARTESIAN_POINT('Ctrl Pts',(6.71724048820842,0.837568704094568,-19.6575130122014));
#43187=CARTESIAN_POINT('Ctrl Pts',(6.69114183123352,1.01040090771779,-19.6492722366046));
#43188=CARTESIAN_POINT('Ctrl Pts',(6.66507208135067,1.18304168093814,-19.6410405885603));
#43189=CARTESIAN_POINT('Ctrl Pts',(6.63228601375324,1.3548747668677,-19.6328089405159));
#43190=CARTESIAN_POINT('Ctrl Pts',(6.59284629547915,1.52534151067453,-19.6245772924716));
#43191=CARTESIAN_POINT('Ctrl Pts',(6.55344323244275,1.69564982284732,-19.6163532949133));
#43192=CARTESIAN_POINT('Ctrl Pts',(6.50739891388341,1.86459397730371,-19.6081292973551));
#43193=CARTESIAN_POINT('Ctrl Pts',(6.4548275304281,2.03162264026257,-19.5999052997968));
#43194=CARTESIAN_POINT('Ctrl Pts',(6.40230259399432,2.19850373274878,-19.5916885681723));
#43195=CARTESIAN_POINT('Ctrl Pts',(6.34326219268906,2.36347236868078,-19.5834718365478));
#43196=CARTESIAN_POINT('Ctrl Pts',(6.27787105981086,2.52598969839335,-19.5752551049234));
#43197=CARTESIAN_POINT('Ctrl Pts',(6.21251342923086,2.68842376446137,-19.5670425830347));
#43198=CARTESIAN_POINT('Ctrl Pts',(6.14081167967596,2.84840869629969,-19.558830061146));
#43199=CARTESIAN_POINT('Ctrl Pts',(6.06297977202706,3.00542264648264,-19.5506175392573));
#43200=CARTESIAN_POINT('Ctrl Pts',(5.98517389174274,3.16238409044484,-19.5424077636755));
#43201=CARTESIAN_POINT('Ctrl Pts',(5.90124209495802,3.31637621352116,-19.5341979880937));
#43202=CARTESIAN_POINT('Ctrl Pts',(5.81144572066407,3.46689884994866,-19.5259882125118));
#43203=CARTESIAN_POINT('Ctrl Pts',(5.77222499729605,3.532643226939,-19.5224023958289));
#43204=CARTESIAN_POINT('Ctrl Pts',(5.73188607893753,3.59772602604172,-19.518816579146));
#43205=CARTESIAN_POINT('Ctrl Pts',(5.69045347539414,3.66210707713124,-19.5152307624631));
#43206=CARTESIAN_POINT('Ctrl Pts',(5.58809472048836,3.82115969911162,-19.5063720449413));
#43207=CARTESIAN_POINT('Ctrl Pts',(5.47916413964674,3.97576271632485,-19.4975133274195));
#43208=CARTESIAN_POINT('Ctrl Pts',(5.36407382894608,4.12540918668872,-19.4886546098977));
#43209=CARTESIAN_POINT('Ctrl Pts',(5.24876820275861,4.27533562156413,-19.4797793191383));
#43210=CARTESIAN_POINT('Ctrl Pts',(5.12727997516108,4.42028677274613,-19.4709040283788));
#43211=CARTESIAN_POINT('Ctrl Pts',(5.00006018296063,4.55979025469064,-19.4620287376193));
#43212=CARTESIAN_POINT('Ctrl Pts',(4.87247905794568,4.69968995789044,-19.4531282390385));
#43213=CARTESIAN_POINT('Ctrl Pts',(4.73913396803678,4.83411083644751,-19.4442277404577));
#43214=CARTESIAN_POINT('Ctrl Pts',(4.60051358868938,4.96261662032081,-19.4353272418769));
#43215=CARTESIAN_POINT('Ctrl Pts',(4.46170555874889,5.09129636264577,-19.4264146946792));
#43216=CARTESIAN_POINT('Ctrl Pts',(4.31760816908561,5.21404484380893,-19.4175021474816));
#43217=CARTESIAN_POINT('Ctrl Pts',(4.16874269820536,5.33046651956088,-19.4085896002839));
#43218=CARTESIAN_POINT('Ctrl Pts',(4.01954851782667,5.44714526574305,-19.3996573733117));
#43219=CARTESIAN_POINT('Ctrl Pts',(3.86556540283638,5.55746910337499,-19.3907251463394));
#43220=CARTESIAN_POINT('Ctrl Pts',(3.70734545794155,5.66108458296466,-19.3817929193671));
#43221=CARTESIAN_POINT('Ctrl Pts',(3.55780933943677,5.75901317626022,-19.373350933422));
#43222=CARTESIAN_POINT('Ctrl Pts',(3.40448908974002,5.85094986113632,-19.3649089474768));
#43223=CARTESIAN_POINT('Ctrl Pts',(3.24787039536178,5.93663430699016,-19.3564669615317));
#43224=CARTESIAN_POINT('Ctrl Pts',(3.19862647078751,5.96357514189857,-19.3538126390654));
#43225=CARTESIAN_POINT('Ctrl Pts',(3.14902628467463,5.98991472998606,-19.351158316599));
#43226=CARTESIAN_POINT('Ctrl Pts',(3.09908550384723,6.01564277861011,-19.3485039941327));
#43227=CARTESIAN_POINT('Origin',(0.,0.,-63.6971797838103));
#43228=CARTESIAN_POINT('',(3.09908550384726,6.0156427786101,-16.9542436419539));
#43229=CARTESIAN_POINT('',(3.09908550384714,6.01564277861016,-17.3484577403131));
#43230=CARTESIAN_POINT('',(3.09908550384721,6.01564277861012,-63.6971797838103));
#43231=CARTESIAN_POINT('',(-6.767,5.61700751015859E-13,-18.30282021619));
#43232=CARTESIAN_POINT('Ctrl Pts',(-6.767,5.61700785041895E-13,-18.30282021619));
#43233=CARTESIAN_POINT('Ctrl Pts',(-6.76700000000002,-0.186007249559512,
-18.2940707043773));
#43234=CARTESIAN_POINT('Ctrl Pts',(-6.75932637294249,-0.372014355815761,
-18.2853211925645));
#43235=CARTESIAN_POINT('Ctrl Pts',(-6.74400518263364,-0.557389537586201,
-18.2765716807518));
#43236=CARTESIAN_POINT('Ctrl Pts',(-6.7286840570373,-0.742763936382802,
-18.2678222058946));
#43237=CARTESIAN_POINT('Ctrl Pts',(-6.70571545643561,-0.927506130405237,
-18.2590727310374));
#43238=CARTESIAN_POINT('Ctrl Pts',(-6.67517739401568,-1.11098864009588,
-18.2503232561801));
#43239=CARTESIAN_POINT('Ctrl Pts',(-6.64463945804381,-1.29447039004583,
-18.2415738175516));
#43240=CARTESIAN_POINT('Ctrl Pts',(-6.60653217002715,-1.47669218339318,
-18.2328243789231));
#43241=CARTESIAN_POINT('Ctrl Pts',(-6.5609849608547,-1.65703510627821,-18.2240749402946));
#43242=CARTESIAN_POINT('Ctrl Pts',(-6.5154379364954,-1.83737729740069,-18.215325537168));
#43243=CARTESIAN_POINT('Ctrl Pts',(-6.46245112156871,-2.01584035545033,
-18.2065761340413));
#43244=CARTESIAN_POINT('Ctrl Pts',(-6.40220448361682,-2.1918181379751,-18.1978267309147));
#43245=CARTESIAN_POINT('Ctrl Pts',(-6.3419580851193,-2.36779522106419,-18.1890773625632));
#43246=CARTESIAN_POINT('Ctrl Pts',(-6.27445201416302,-2.54128677725873,
-18.1803279942116));
#43247=CARTESIAN_POINT('Ctrl Pts',(-6.19991555052662,-2.71170355428801,
-18.1715786258601));
#43248=CARTESIAN_POINT('Ctrl Pts',(-6.12537937695044,-2.8821196681368,-18.1628292915569));
#43249=CARTESIAN_POINT('Ctrl Pts',(-6.04381298028259,-3.04946076420052,
-18.1540799572537));
#43250=CARTESIAN_POINT('Ctrl Pts',(-5.95549339308771,-3.21315848424704,
-18.1453306229505));
#43251=CARTESIAN_POINT('Ctrl Pts',(-5.86717414225596,-3.37685558085452,
-18.136581321969));
#43252=CARTESIAN_POINT('Ctrl Pts',(-5.77210188843853,-3.53690907700348,
-18.1278320209874));
#43253=CARTESIAN_POINT('Ctrl Pts',(-5.67059953311159,-3.69277537024318,
-18.1190827200059));
#43254=CARTESIAN_POINT('Ctrl Pts',(-5.56909755592481,-3.84864108281355,
-18.1103334516192));
#43255=CARTESIAN_POINT('Ctrl Pts',(-5.46116568154725,-4.00031938355158,
-18.1015841832326));
#43256=CARTESIAN_POINT('Ctrl Pts',(-5.34717048488122,-4.14729511918493,
-18.092834914846));
#43257=CARTESIAN_POINT('Ctrl Pts',(-5.23317570343027,-4.29427031947518,
-18.0840856783276));
#43258=CARTESIAN_POINT('Ctrl Pts',(-5.11311781951246,-4.43654276249904,
-18.0753364418093));
#43259=CARTESIAN_POINT('Ctrl Pts',(-4.98740458928918,-4.57362924412738,
-18.0665872052909));
#43260=CARTESIAN_POINT('Ctrl Pts',(-4.86169180652402,-4.71071523781617,
-18.0578379999142));
#43261=CARTESIAN_POINT('Ctrl Pts',(-4.73032391141222,-4.84261509584832,
-18.0490887945375));
#43262=CARTESIAN_POINT('Ctrl Pts',(-4.59374706946965,-4.96888084599933,
-18.0403395891608));
#43263=CARTESIAN_POINT('Ctrl Pts',(-4.45717070231158,-5.09514615721047,
-18.0315904141991));
#43264=CARTESIAN_POINT('Ctrl Pts',(-4.31538563497028,-5.21577720520859,
-18.0228412392374));
#43265=CARTESIAN_POINT('Ctrl Pts',(-4.16887340951722,-5.33036429293724,
-18.0140920642757));
#43266=CARTESIAN_POINT('Ctrl Pts',(-4.02236168122208,-5.44495099183909,
-18.0053429190024));
#43267=CARTESIAN_POINT('Ctrl Pts',(-3.87112305262913,-5.55349359498114,
-17.9965937737292));
#43268=CARTESIAN_POINT('Ctrl Pts',(-3.71567116928738,-5.65562346357381,
-17.9878446284559));
#43269=CARTESIAN_POINT('Ctrl Pts',(-3.56021980053049,-5.75775299409089,
-17.9790955121446));
#43270=CARTESIAN_POINT('Ctrl Pts',(-3.40055544441818,-5.85346967520033,
-17.9703463958332));
#43271=CARTESIAN_POINT('Ctrl Pts',(-3.23722035886573,-5.9424484304153,-17.9615972795218));
#43272=CARTESIAN_POINT('Ctrl Pts',(-3.07388580043242,-6.03142689847576,
-17.9528481914458));
#43273=CARTESIAN_POINT('Ctrl Pts',(-2.90688078788998,-6.11366734708007,
-17.9440991033698));
#43274=CARTESIAN_POINT('Ctrl Pts',(-2.73677250610193,-6.18889047001517,
-17.9353500152938));
#43275=CARTESIAN_POINT('Ctrl Pts',(-2.56666475916757,-6.26411335643406,
-17.9266009547267));
#43276=CARTESIAN_POINT('Ctrl Pts',(-2.39345402456937,-6.33231884545314,
-17.9178518941595));
#43277=CARTESIAN_POINT('Ctrl Pts',(-2.21772855943933,-6.39327529804928,
-17.9091028335924));
#43278=CARTESIAN_POINT('Ctrl Pts',(-2.04200363223431,-6.45423156404754,
-17.9003537998076));
#43279=CARTESIAN_POINT('Ctrl Pts',(-1.86376426060846,-6.50793874412508,
-17.8916047660227));
#43280=CARTESIAN_POINT('Ctrl Pts',(-1.68361577621471,-6.55421443943368,
-17.8828557322379));
#43281=CARTESIAN_POINT('Ctrl Pts',(-1.50346782832989,-6.6004899969264,-17.874106724509));
#43282=CARTESIAN_POINT('Ctrl Pts',(-1.32141105657151,-6.63933404265209,
-17.8653577167801));
#43283=CARTESIAN_POINT('Ctrl Pts',(-1.1380637534629,-6.67061465631571,-17.8566087090512));
#43284=CARTESIAN_POINT('Ctrl Pts',(-0.954716981167104,-6.70189517941813,
-17.8478597266518));
#43285=CARTESIAN_POINT('Ctrl Pts',(-0.770079967438926,-6.72561226609044,
-17.8391107442523));
#43286=CARTESIAN_POINT('Ctrl Pts',(-0.58477976406926,-6.74168536996018,
-17.8303617618529));
#43287=CARTESIAN_POINT('Ctrl Pts',(-0.391489587589147,-6.75845153117895,
-17.8212355314372));
#43288=CARTESIAN_POINT('Ctrl Pts',(-0.19747809180143,-6.76689985146405,
-17.8121093010216));
#43289=CARTESIAN_POINT('Ctrl Pts',(-0.0034621475272351,-6.76699911434415,
-17.802983070606));
#43290=CARTESIAN_POINT('Ctrl Pts',(0.184490798488409,-6.76709527525925,
-17.7941420348909));
#43291=CARTESIAN_POINT('Ctrl Pts',(0.372447602158518,-6.75935633790742,
-17.7853009991758));
#43292=CARTESIAN_POINT('Ctrl Pts',(0.559756448197919,-6.74380914014482,
-17.7764599634606));
#43293=CARTESIAN_POINT('Ctrl Pts',(0.745136131047101,-6.72842206873113,
-17.7677099848473));
#43294=CARTESIAN_POINT('Ctrl Pts',(0.929880851948822,-6.70538686355671,
-17.758960006234));
#43295=CARTESIAN_POINT('Ctrl Pts',(1.11336305057844,-6.67478177303249,-17.7502100276207));
#43296=CARTESIAN_POINT('Ctrl Pts',(1.2968433709051,-6.64417699581185,-17.7414601385807));
#43297=CARTESIAN_POINT('Ctrl Pts',(1.47906091205583,-6.60600253547972,-17.7327102495407));
#43298=CARTESIAN_POINT('Ctrl Pts',(1.65939671095619,-6.56038806441111,-17.7239603605008));
#43299=CARTESIAN_POINT('Ctrl Pts',(1.83973072369562,-6.51477404513736,-17.7152105581253));
#43300=CARTESIAN_POINT('Ctrl Pts',(2.01818275357441,-6.46172023288534,-17.7064607557498));
#43301=CARTESIAN_POINT('Ctrl Pts',(2.19414664033734,-6.40140683917968,-17.6977109533743));
#43302=CARTESIAN_POINT('Ctrl Pts',(2.37010884271667,-6.34109402281345,-17.6889612347547));
#43303=CARTESIAN_POINT('Ctrl Pts',(2.54358267848213,-6.27352185699627,-17.6802115161352));
#43304=CARTESIAN_POINT('Ctrl Pts',(2.71397890842147,-6.19891986435084,-17.6714617975156));
#43305=CARTESIAN_POINT('Ctrl Pts',(2.88437356389346,-6.12431856103053,-17.6627121597438));
#43306=CARTESIAN_POINT('Ctrl Pts',(3.05169040787575,-6.04268767582354,-17.653962521972));
#43307=CARTESIAN_POINT('Ctrl Pts',(3.21536112512454,-5.95430447953729,-17.6452128842002));
#43308=CARTESIAN_POINT('Ctrl Pts',(3.37903038443229,-5.8659220705482,-17.6364633243681));
#43309=CARTESIAN_POINT('Ctrl Pts',(3.53905332980346,-5.77078760703148,-17.6277137645361));
#43310=CARTESIAN_POINT('Ctrl Pts',(3.69488643042251,-5.66922422085065,-17.618964204704));
#43311=CARTESIAN_POINT('Ctrl Pts',(3.85071819469098,-5.56766170562912,-17.610214719904));
#43312=CARTESIAN_POINT('Ctrl Pts',(4.00235994599577,-5.45967053455993,-17.601465235104));
#43313=CARTESIAN_POINT('Ctrl Pts',(4.14929662974649,-5.34561750206414,-17.592715750304));
#43314=CARTESIAN_POINT('Ctrl Pts',(4.29623210225383,-5.23156540974187,-17.5839663376287));
#43315=CARTESIAN_POINT('Ctrl Pts',(4.43846235842447,-5.111451731719,-17.5752169249533));
#43316=CARTESIAN_POINT('Ctrl Pts',(4.57550431797748,-4.98568443006268,-17.5664675122779));
#43317=CARTESIAN_POINT('Ctrl Pts',(4.71254519337812,-4.85991812336382,-17.55771816882));
#43318=CARTESIAN_POINT('Ctrl Pts',(4.84439764315299,-4.72849847630778,-17.5489688253621));
#43319=CARTESIAN_POINT('Ctrl Pts',(4.97061384196998,-4.59187184425006,-17.5402194819042));
#43320=CARTESIAN_POINT('Ctrl Pts',(5.09682908420515,-4.45524624767395,-17.5314702047569));
#43321=CARTESIAN_POINT('Ctrl Pts',(5.21740796650475,-4.31341395556525,-17.5227209276095));
#43322=CARTESIAN_POINT('Ctrl Pts',(5.3319409594255,-4.16685668162473,-17.5139716504621));
#43323=CARTESIAN_POINT('Ctrl Pts',(5.44647312235422,-4.02030046974822,-17.5052224367186));
#43324=CARTESIAN_POINT('Ctrl Pts',(5.55495930712568,-3.86901957035145,-17.4964732229751));
#43325=CARTESIAN_POINT('Ctrl Pts',(5.65703106080064,-3.71352778057964,-17.4877240092315));
#43326=CARTESIAN_POINT('Ctrl Pts',(5.75910210868999,-3.55803706597177,-17.4789748559853));
#43327=CARTESIAN_POINT('Ctrl Pts',(5.85475865698805,-3.39833575880459,-17.4702257027391));
#43328=CARTESIAN_POINT('Ctrl Pts',(5.9436758306931,-3.23496624706266,-17.4614765494929));
#43329=CARTESIAN_POINT('Ctrl Pts',(6.03259241910311,-3.0715978106964,-17.4527274538378));
#43330=CARTESIAN_POINT('Ctrl Pts',(6.11476958471188,-2.9045614697537,-17.4439783581827));
#43331=CARTESIAN_POINT('Ctrl Pts',(6.18992823574592,-2.7344245164779,-17.4352292625276));
#43332=CARTESIAN_POINT('Ctrl Pts',(6.26508641701131,-2.56428862661937,-17.4264802215574));
#43333=CARTESIAN_POINT('Ctrl Pts',(6.33322605570482,-2.39105242530786,-17.4177311805873));
#43334=CARTESIAN_POINT('Ctrl Pts',(6.39411573747941,-2.21530425353227,-17.4089821396172));
#43335=CARTESIAN_POINT('Ctrl Pts',(6.45500505889285,-2.03955712188055,-17.4002331504262));
#43336=CARTESIAN_POINT('Ctrl Pts',(6.50864441545075,-1.86129832025062,-17.3914841612352));
#43337=CARTESIAN_POINT('Ctrl Pts',(6.55485164050038,-1.68113324011795,-17.3827351720442));
#43338=CARTESIAN_POINT('Ctrl Pts',(6.60199852639227,-1.49730435912381,-17.3738082651673));
#43339=CARTESIAN_POINT('Ctrl Pts',(6.64140767441113,-1.31149113173131,-17.3648813582904));
#43340=CARTESIAN_POINT('Ctrl Pts',(6.6729397526969,-1.12435050445909,-17.3559544514136));
#43341=CARTESIAN_POINT('Ctrl Pts',(6.7038466483158,-0.940920291558521,-17.3472045372296));
#43342=CARTESIAN_POINT('Ctrl Pts',(6.72718585889724,-0.756215114272718,
-17.3384546230456));
#43343=CARTESIAN_POINT('Ctrl Pts',(6.74287810451908,-0.570862389369925,
-17.3297047088616));
#43344=CARTESIAN_POINT('Ctrl Pts',(6.75857004154153,-0.385513309562867,
-17.320954966751));
#43345=CARTESIAN_POINT('Ctrl Pts',(6.76661529035571,-0.199516993253964,
-17.3122052246404));
#43346=CARTESIAN_POINT('Ctrl Pts',(6.76698652348897,-0.0135052181998018,
-17.3034554825298));
#43347=CARTESIAN_POINT('Ctrl Pts',(6.7673577498151,0.172503146043099,-17.2947059008592));
#43348=CARTESIAN_POINT('Ctrl Pts',(6.76005524147457,0.358526681837624,-17.2859563191885));
#43349=CARTESIAN_POINT('Ctrl Pts',(6.74510380214848,0.543933542118961,-17.2772067375179));
#43350=CARTESIAN_POINT('Ctrl Pts',(6.73015261710935,0.7293372490888,-17.268457304656));
#43351=CARTESIAN_POINT('Ctrl Pts',(6.7075527844455,0.914124015858719,-17.2597078717941));
#43352=CARTESIAN_POINT('Ctrl Pts',(6.67738106408223,1.09766621749789,-17.2509584389321));
#43353=CARTESIAN_POINT('Ctrl Pts',(6.64720981677177,1.28120554143722,-17.2422091432498));
#43354=CARTESIAN_POINT('Ctrl Pts',(6.60946696581435,1.46350005651017,-17.2334598475674));
#43355=CARTESIAN_POINT('Ctrl Pts',(6.56428070010896,1.64393062206928,-17.2247105518851));
#43356=CARTESIAN_POINT('Ctrl Pts',(6.51909508282631,1.82435859845046,-17.2159613817551));
#43357=CARTESIAN_POINT('Ctrl Pts',(6.4664663341554,2.00292240086956,-17.2072122116251));
#43358=CARTESIAN_POINT('Ctrl Pts',(6.40657319597059,2.17901557696845,-17.1984630414951));
#43359=CARTESIAN_POINT('Ctrl Pts',(6.34668083768153,2.35510646007816,-17.189713985292));
#43360=CARTESIAN_POINT('Ctrl Pts',(6.27952437143735,2.52872650996903,-17.180964929089));
#43361=CARTESIAN_POINT('Ctrl Pts',(6.20533187334978,2.69928607998288,-17.1722158728859));
#43362=CARTESIAN_POINT('Ctrl Pts',(6.1283144978409,2.87633970115742,-17.1631336965971));
#43363=CARTESIAN_POINT('Ctrl Pts',(6.04371489462988,3.05009490562676,-17.1540515203082));
#43364=CARTESIAN_POINT('Ctrl Pts',(5.95184265120324,3.2199158459994,-17.1449693440194));
#43365=CARTESIAN_POINT('Ctrl Pts',(5.86333281335316,3.38352155905606,-17.136219563665));
#43366=CARTESIAN_POINT('Ctrl Pts',(5.76807337235499,3.54347560904126,-17.1274697833105));
#43367=CARTESIAN_POINT('Ctrl Pts',(5.66638790086161,3.69923467178945,-17.1187200029561));
#43368=CARTESIAN_POINT('Ctrl Pts',(5.56470608502536,3.85498813490062,-17.1099705371619));
#43369=CARTESIAN_POINT('Ctrl Pts',(5.45659885766734,4.00654667256559,-17.1012210713676));
#43370=CARTESIAN_POINT('Ctrl Pts',(5.34243340580277,4.15339551506507,-17.0924716055733));
#43371=CARTESIAN_POINT('Ctrl Pts',(5.22827145140352,4.30023985884164,-17.0837224078194));
#43372=CARTESIAN_POINT('Ctrl Pts',(5.10805181977837,4.44237456993333,-17.0749732100656));
#43373=CARTESIAN_POINT('Ctrl Pts',(4.98218281282288,4.57931691626735,-17.0662240123117));
#43374=CARTESIAN_POINT('Ctrl Pts',(4.85631699295956,4.71625579512443,-17.0574750360937));
#43375=CARTESIAN_POINT('Ctrl Pts',(4.72480227791555,4.84800236136045,-17.0487260598757));
#43376=CARTESIAN_POINT('Ctrl Pts',(4.58808530847821,4.97410918679179,-17.0399770836577));
#43377=CARTESIAN_POINT('Ctrl Pts',(4.45135945056669,5.10022421089272,-17.0312275386365));
#43378=CARTESIAN_POINT('Ctrl Pts',(4.3094308720773,5.22069856612243,-17.0224779936153));
#43379=CARTESIAN_POINT('Ctrl Pts',(4.16278164322149,5.33512305301932,-17.0137284485941));
#43380=CARTESIAN_POINT('Ctrl Pts',(4.0161410353407,5.44954081331663,-17.0049794179268));
#43381=CARTESIAN_POINT('Ctrl Pts',(3.86478055833092,5.55790924068561,-16.9962303872596));
#43382=CARTESIAN_POINT('Ctrl Pts',(3.7092142581163,5.65986029751501,-16.9874813565923));
#43383=CARTESIAN_POINT('Ctrl Pts',(3.55364584529801,5.7618127388485,-16.9787322071125));
#43384=CARTESIAN_POINT('Ctrl Pts',(3.39387173464027,5.85734747818247,-16.9699830576326));
#43385=CARTESIAN_POINT('Ctrl Pts',(3.23043456092091,5.94614005448978,-16.9612339081528));
#43386=CARTESIAN_POINT('Ctrl Pts',(3.18690768806183,5.96978744811392,-16.9589038194198));
#43387=CARTESIAN_POINT('Ctrl Pts',(3.14312114982779,5.99295688499353,-16.9565737306868));
#43388=CARTESIAN_POINT('Ctrl Pts',(3.09908550384726,6.0156427786101,-16.9542436419538));
#43389=CARTESIAN_POINT('Ctrl Pts',(3.09908550384715,6.01564277861015,-18.9542023328983));
#43390=CARTESIAN_POINT('Ctrl Pts',(2.93955287157862,6.09782938546984,-18.9457755290877));
#43391=CARTESIAN_POINT('Ctrl Pts',(2.77669907250746,6.17369168653797,-18.937348725277));
#43392=CARTESIAN_POINT('Ctrl Pts',(2.61105431770974,6.24297079521996,-18.9289219214663));
#43393=CARTESIAN_POINT('Ctrl Pts',(2.45830155335587,6.30685796977052,-18.9211509686323));
#43394=CARTESIAN_POINT('Ctrl Pts',(2.30317581700008,6.36514720210411,-18.9133800157982));
#43395=CARTESIAN_POINT('Ctrl Pts',(2.14610905555137,6.41767130053265,-18.9056090629641));
#43396=CARTESIAN_POINT('Ctrl Pts',(1.97190176805378,6.47592729709804,-18.8969900744397));
#43397=CARTESIAN_POINT('Ctrl Pts',(1.79538450031526,6.52706470421298,-18.8883710859152));
#43398=CARTESIAN_POINT('Ctrl Pts',(1.61715397565048,6.5709285507482,-18.8797520973908));
#43399=CARTESIAN_POINT('Ctrl Pts',(1.43881667499724,6.61481867564163,-18.8711279453231));
#43400=CARTESIAN_POINT('Ctrl Pts',(1.25876436438882,6.65142647100605,-18.8625037932554));
#43401=CARTESIAN_POINT('Ctrl Pts',(1.07760441734818,6.68064800148247,-18.8538796411878));
#43402=CARTESIAN_POINT('Ctrl Pts',(0.89023969338103,6.71087037723964,-18.8449601095915));
#43403=CARTESIAN_POINT('Ctrl Pts',(0.701690470581387,6.73319151794819,-18.8360405779952));
#43404=CARTESIAN_POINT('Ctrl Pts',(0.512634310865934,6.74755474696745,-18.8271210463989));
#43405=CARTESIAN_POINT('Ctrl Pts',(0.329498415226465,6.76146819371617,-18.8184808285397));
#43406=CARTESIAN_POINT('Ctrl Pts',(0.145887157616835,6.76791462308545,-18.8098406106805));
#43407=CARTESIAN_POINT('Ctrl Pts',(-0.0375831936387921,6.76689563267795,
-18.8012003928213));
#43408=CARTESIAN_POINT('Ctrl Pts',(-0.229950159010604,6.7658272306659,-18.7921412043565));
#43409=CARTESIAN_POINT('Ctrl Pts',(-0.422161825523465,6.75655142030718,
-18.7830820158916));
#43410=CARTESIAN_POINT('Ctrl Pts',(-0.613512922072761,6.73913131601171,
-18.7740228274268));
#43411=CARTESIAN_POINT('Ctrl Pts',(-0.804864018621992,6.72171121171625,
-18.764963638962));
#43412=CARTESIAN_POINT('Ctrl Pts',(-0.995354170387055,6.69614689720996,
-18.7559044504972));
#43413=CARTESIAN_POINT('Ctrl Pts',(-1.18428889692815,6.66256323111554,-18.7468452620324));
#43414=CARTESIAN_POINT('Ctrl Pts',(-1.37289630730937,6.62903774636671,-18.7378017679761));
#43415=CARTESIAN_POINT('Ctrl Pts',(-1.56012757976248,6.58749062086662,-18.7287582739198));
#43416=CARTESIAN_POINT('Ctrl Pts',(-1.74532380658997,6.53805275369894,-18.7197147798635));
#43417=CARTESIAN_POINT('Ctrl Pts',(-1.93035063510609,6.48866010716755,-18.7106795578582));
#43418=CARTESIAN_POINT('Ctrl Pts',(-2.11334590455118,6.4313911903526,-18.7016443358528));
#43419=CARTESIAN_POINT('Ctrl Pts',(-2.29366304647345,6.36642747773366,-18.6926091138475));
#43420=CARTESIAN_POINT('Ctrl Pts',(-2.47366250884614,6.30157821703395,-18.6835898099363));
#43421=CARTESIAN_POINT('Ctrl Pts',(-2.65099304180712,6.22906131187865,-18.6745705060252));
#43422=CARTESIAN_POINT('Ctrl Pts',(-2.82502546611859,6.14910726169104,-18.6655512021141));
#43423=CARTESIAN_POINT('Ctrl Pts',(-2.99883955459871,6.06925351944366,-18.6565432135496));
#43424=CARTESIAN_POINT('Ctrl Pts',(-3.16936357616707,5.98198135157004,-18.6475352249852));
#43425=CARTESIAN_POINT('Ctrl Pts',(-3.33598810726092,5.88756930729599,-18.6385272364208));
#43426=CARTESIAN_POINT('Ctrl Pts',(-3.50223631101512,5.79337049593079,-18.6295395927141));
#43427=CARTESIAN_POINT('Ctrl Pts',(-3.66460239738049,5.69206411361652,-18.6205519490073));
#43428=CARTESIAN_POINT('Ctrl Pts',(-3.82250174688802,5.58397433688928,-18.6115643053006));
#43429=CARTESIAN_POINT('Ctrl Pts',(-3.96002113627314,5.4898356330842,-18.6037366905674));
#43430=CARTESIAN_POINT('Ctrl Pts',(-4.09415263965759,5.39055234715943,-18.5959090758343));
#43431=CARTESIAN_POINT('Ctrl Pts',(-4.22452484614403,5.28636726158065,-18.5880814611011));
#43432=CARTESIAN_POINT('Ctrl Pts',(-4.35981945711452,5.17824850680777,-18.5799583026558));
#43433=CARTESIAN_POINT('Ctrl Pts',(-4.49100401349823,5.064897837526,-18.5718351442105));
#43434=CARTESIAN_POINT('Ctrl Pts',(-4.61765506804729,4.94667066546149,-18.5637119857652));
#43435=CARTESIAN_POINT('Ctrl Pts',(-4.74429719303384,4.82845182903166,-18.5555894000452));
#43436=CARTESIAN_POINT('Ctrl Pts',(-4.86640618530508,4.70535742444016,-18.5474668143251));
#43437=CARTESIAN_POINT('Ctrl Pts',(-4.983593904042,4.57778120923177,-18.539344228605));
#43438=CARTESIAN_POINT('Ctrl Pts',(-5.10079570409027,4.45018966442718,-18.5312206668726));
#43439=CARTESIAN_POINT('Ctrl Pts',(-5.21307480638164,4.31811550702032,-18.5230971051402));
#43440=CARTESIAN_POINT('Ctrl Pts',(-5.320081999144,4.18198714995443,-18.5149735434078));
#43441=CARTESIAN_POINT('Ctrl Pts',(-5.42716713394764,4.04575963953491,-18.5068440646247));
#43442=CARTESIAN_POINT('Ctrl Pts',(-5.52897246337977,3.90547231958631,-18.4987145858416));
#43443=CARTESIAN_POINT('Ctrl Pts',(-5.62519055643087,3.76158479950153,-18.4905851070585));
#43444=CARTESIAN_POINT('Ctrl Pts',(-5.72144787590491,3.61763861900748,-18.48245231403));
#43445=CARTESIAN_POINT('Ctrl Pts',(-5.81211322713935,3.47008962437107,-18.4743195210015));
#43446=CARTESIAN_POINT('Ctrl Pts',(-5.8969242809301,3.31942359830394,-18.466186727973));
#43447=CARTESIAN_POINT('Ctrl Pts',(-5.98182755387526,3.16859374579081,-18.4580450917659));
#43448=CARTESIAN_POINT('Ctrl Pts',(-6.06086364816737,3.01464041755744,-18.4499034555588));
#43449=CARTESIAN_POINT('Ctrl Pts',(-6.13381734516322,2.8580716884247,-18.4417618193516));
#43450=CARTESIAN_POINT('Ctrl Pts',(-6.17098626286205,2.77830204758421,-18.4376137662909));
#43451=CARTESIAN_POINT('Ctrl Pts',(-6.20657711544618,2.6978538103809,-18.4334657132302));
#43452=CARTESIAN_POINT('Ctrl Pts',(-6.240566382091,2.61679579461518,-18.4293176601694));
#43453=CARTESIAN_POINT('Ctrl Pts',(-6.31738329510644,2.43360188780494,-18.4199429174167));
#43454=CARTESIAN_POINT('Ctrl Pts',(-6.38614096433329,2.24699678707267,-18.4105681746639));
#43455=CARTESIAN_POINT('Ctrl Pts',(-6.44657563827959,2.05765680810483,-18.4011934319112));
#43456=CARTESIAN_POINT('Ctrl Pts',(-6.50687594802183,1.8687377880652,-18.3918395319919));
#43457=CARTESIAN_POINT('Ctrl Pts',(-6.55889016789018,1.67709619195425,-18.3824856320727));
#43458=CARTESIAN_POINT('Ctrl Pts',(-6.60240453971986,1.48342283044539,-18.3731317321535));
#43459=CARTESIAN_POINT('Ctrl Pts',(-6.64583505185042,1.29012271090559,-18.3637958588126));
#43460=CARTESIAN_POINT('Ctrl Pts',(-6.68079837636695,1.0947988041738,-18.3544599854717));
#43461=CARTESIAN_POINT('Ctrl Pts',(-6.70713108362105,0.898154567501827,
-18.3451241121308));
#43462=CARTESIAN_POINT('Ctrl Pts',(-6.73336361908543,0.702258381720841,
-18.3358237532219));
#43463=CARTESIAN_POINT('Ctrl Pts',(-6.75103101770111,0.505052053478654,
-18.326523394313));
#43464=CARTESIAN_POINT('Ctrl Pts',(-6.7600214043759,0.307245199115813,-18.3172230354042));
#43465=CARTESIAN_POINT('Ctrl Pts',(-6.76466233329813,0.205135291651743,
-18.3124220956661));
#43466=CARTESIAN_POINT('Ctrl Pts',(-6.76699188960486,0.102865576435023,
-18.307621155928));
#43467=CARTESIAN_POINT('Ctrl Pts',(-6.76699997885676,0.000534932305956201,
-18.30282021619));
#43468=CARTESIAN_POINT('',(-6.76699999116254,0.000345841369350949,-18.697179783767));
#43469=CARTESIAN_POINT('Ctrl Pts',(3.09908550384723,6.01564277861011,-19.3485039941327));
#43470=CARTESIAN_POINT('Ctrl Pts',(2.94440847816585,6.09532791712462,-19.3402830032412));
#43471=CARTESIAN_POINT('Ctrl Pts',(2.78646210386894,6.16914348376745,-19.3320620123498));
#43472=CARTESIAN_POINT('Ctrl Pts',(2.62573141136858,6.23681197049842,-19.3238410214583));
#43473=CARTESIAN_POINT('Ctrl Pts',(2.46516006366625,6.30441337221169,-19.3156281806726));
#43474=CARTESIAN_POINT('Ctrl Pts',(2.30181022276318,6.3658796917601,-19.3074153398868));
#43475=CARTESIAN_POINT('Ctrl Pts',(2.1361914294365,6.42097930044959,-19.2992024991011));
#43476=CARTESIAN_POINT('Ctrl Pts',(1.97070361066912,6.47603533529808,-19.2909961531894));
#43477=CARTESIAN_POINT('Ctrl Pts',(1.80295075182054,6.5247345746493,-19.2827898072777));
#43478=CARTESIAN_POINT('Ctrl Pts',(1.63346236967899,6.56689345785682,-19.2745834613659));
#43479=CARTESIAN_POINT('Ctrl Pts',(1.4640740386589,6.60902745414589,-19.2663819597633));
#43480=CARTESIAN_POINT('Ctrl Pts',(1.29295257209241,6.64462869882177,-19.2581804581607));
#43481=CARTESIAN_POINT('Ctrl Pts',(1.12064273434524,6.67356343057884,-19.2499789565581));
#43482=CARTESIAN_POINT('Ctrl Pts',(0.94840007031874,6.70248688234392,-19.2417806522505));
#43483=CARTESIAN_POINT('Ctrl Pts',(0.774970311197606,6.72474893997004,-19.2335823479428));
#43484=CARTESIAN_POINT('Ctrl Pts',(0.600908592751125,6.74026689851061,-19.2253840436352));
#43485=CARTESIAN_POINT('Ctrl Pts',(0.426847945465729,6.75578476155499,-19.2171857897792));
#43486=CARTESIAN_POINT('Ctrl Pts',(0.252155702755887,6.76455856672819,-19.2089875359233));
#43487=CARTESIAN_POINT('Ctrl Pts',(0.0773927041020941,6.76655742378292,
-19.2007892820673));
#43488=CARTESIAN_POINT('Ctrl Pts',(-0.0973787949803039,6.76855637806157,
-19.1925906294503));
#43489=CARTESIAN_POINT('Ctrl Pts',(-0.2722206981662,6.763779722904,-19.1843919768333));
#43490=CARTESIAN_POINT('Ctrl Pts',(-0.446571735709607,6.75224871319661,
-19.1761933242164));
#43491=CARTESIAN_POINT('Ctrl Pts',(-0.620962925836858,6.74071504792813,
-19.1679927834713));
#43492=CARTESIAN_POINT('Ctrl Pts',(-0.794862667244472,6.72242395300531,
-19.1597922427263));
#43493=CARTESIAN_POINT('Ctrl Pts',(-0.967714327126197,6.69744861727768,
-19.1515917019812));
#43494=CARTESIAN_POINT('Ctrl Pts',(-1.14063719453846,6.67246299277421,-19.1433877829622));
#43495=CARTESIAN_POINT('Ctrl Pts',(-1.31251076567566,6.64078769346307,-19.1351838639433));
#43496=CARTESIAN_POINT('Ctrl Pts',(-1.48278806505245,6.60254712623379,-19.1269799449243));
#43497=CARTESIAN_POINT('Ctrl Pts',(-1.65326209435543,6.56426237775429,-19.1187665475052));
#43498=CARTESIAN_POINT('Ctrl Pts',(-1.82213581810475,6.5193972894121,-19.110553150086));
#43499=CARTESIAN_POINT('Ctrl Pts',(-1.98887594887905,6.46812658039177,-19.1023397526669));
#43500=CARTESIAN_POINT('Ctrl Pts',(-2.15572319202591,6.41682293552533,-19.0941210790345));
#43501=CARTESIAN_POINT('Ctrl Pts',(-2.32043377276798,6.3591055865086,-19.0859024054021));
#43502=CARTESIAN_POINT('Ctrl Pts',(-2.48249400881984,6.29519757403798,-19.0776837317698));
#43503=CARTESIAN_POINT('Ctrl Pts',(-2.64478933304299,6.23119685518762,-19.0694531359472));
#43504=CARTESIAN_POINT('Ctrl Pts',(-2.8044263051849,6.16098767801956,-19.0612225401246));
#43505=CARTESIAN_POINT('Ctrl Pts',(-2.96091450546015,6.08483970958609,-19.0529919443021));
#43506=CARTESIAN_POINT('Ctrl Pts',(-3.0499750354599,6.041502394599,-19.0483077494243));
#43507=CARTESIAN_POINT('Ctrl Pts',(-3.13801617845152,5.99624234036059,-19.0436235545464));
#43508=CARTESIAN_POINT('Ctrl Pts',(-3.22495178421901,5.94911547958708,-19.0389393596686));
#43509=CARTESIAN_POINT('Ctrl Pts',(-3.37474187771986,5.86791587420853,-19.0308684894822));
#43510=CARTESIAN_POINT('Ctrl Pts',(-3.52173671608847,5.78090699168158,-19.0227976192958));
#43511=CARTESIAN_POINT('Ctrl Pts',(-3.66544193120517,5.68830593841109,-19.0147267491094));
#43512=CARTESIAN_POINT('Ctrl Pts',(-3.80896831635165,5.59582011995366,-19.0066659224936));
#43513=CARTESIAN_POINT('Ctrl Pts',(-3.94921291406009,5.49775617698324,-18.9986050958778));
#43514=CARTESIAN_POINT('Ctrl Pts',(-4.08570333956989,5.39437829791604,-18.990544269262));
#43515=CARTESIAN_POINT('Ctrl Pts',(-4.22205384362153,5.2911063953928,-18.9824917061021));
#43516=CARTESIAN_POINT('Ctrl Pts',(-4.35465753938026,5.18253162084947,-18.9744391429422));
#43517=CARTESIAN_POINT('Ctrl Pts',(-4.48306867116872,5.06896284160631,-18.9663865797824));
#43518=CARTESIAN_POINT('Ctrl Pts',(-4.61137628116239,4.95548561863009,-18.9583405083945));
#43519=CARTESIAN_POINT('Ctrl Pts',(-4.73549777645621,4.83702265004525,-18.9502944370066));
#43520=CARTESIAN_POINT('Ctrl Pts',(-4.85501840760994,4.7139246135008,-18.9422483656187));
#43521=CARTESIAN_POINT('Ctrl Pts',(-4.97446882804233,4.5908988891744,-18.9342070207828));
#43522=CARTESIAN_POINT('Ctrl Pts',(-5.08932350550706,4.46324378417688,-18.9261656759469));
#43523=CARTESIAN_POINT('Ctrl Pts',(-5.19920275818625,4.3313484827786,-18.9181243311111));
#43524=CARTESIAN_POINT('Ctrl Pts',(-5.31120014475798,4.19691064581199,-18.90992797389));
#43525=CARTESIAN_POINT('Ctrl Pts',(-5.41802803229019,4.05806773256378,-18.9017316166689));
#43526=CARTESIAN_POINT('Ctrl Pts',(-5.51932543404989,3.91526956326764,-18.8935352594479));
#43527=CARTESIAN_POINT('Ctrl Pts',(-5.6186754730372,3.77521657631599,-18.8854964707394));
#43528=CARTESIAN_POINT('Ctrl Pts',(-5.71270553000589,3.63135935539557,-18.8774576820309));
#43529=CARTESIAN_POINT('Ctrl Pts',(-5.80111744591931,3.48415346657559,-18.8694188933224));
#43530=CARTESIAN_POINT('Ctrl Pts',(-5.88953882270863,3.336931825392,-18.8613792443907));
#43531=CARTESIAN_POINT('Ctrl Pts',(-5.97234066898833,3.18636112293837,-18.8533395954589));
#43532=CARTESIAN_POINT('Ctrl Pts',(-6.04926982971491,3.03292326432782,-18.8452999465272));
#43533=CARTESIAN_POINT('Ctrl Pts',(-6.12622245482632,2.8794386051942,-18.837257845399));
#43534=CARTESIAN_POINT('Ctrl Pts',(-6.19729866162558,2.72308538284473,-18.8292157442708));
#43535=CARTESIAN_POINT('Ctrl Pts',(-6.26229271905741,2.56436715406366,-18.8211736431427));
#43536=CARTESIAN_POINT('Ctrl Pts',(-6.32948007057329,2.40029280864714,-18.8128601526979));
#43537=CARTESIAN_POINT('Ctrl Pts',(-6.39016742727578,2.23369144887705,-18.8045466622531));
#43538=CARTESIAN_POINT('Ctrl Pts',(-6.44418321522352,2.06513720818533,-18.7962331718084));
#43539=CARTESIAN_POINT('Ctrl Pts',(-6.49652773598207,1.90179809408472,-18.7881769036376));
#43540=CARTESIAN_POINT('Ctrl Pts',(-6.54260735312553,1.73662551931482,-18.7801206354669));
#43541=CARTESIAN_POINT('Ctrl Pts',(-6.58231797049406,1.5701525834488,-18.7720643672961));
#43542=CARTESIAN_POINT('Ctrl Pts',(-6.62393042164316,1.3957068716866,-18.7636222657143));
#43543=CARTESIAN_POINT('Ctrl Pts',(-6.65854872492751,1.21983365843838,-18.7551801641326));
#43544=CARTESIAN_POINT('Ctrl Pts',(-6.68611419154111,1.04315196288582,-18.7467380625508));
#43545=CARTESIAN_POINT('Ctrl Pts',(-6.71367965815473,0.86647026733319,-18.738295960969));
#43546=CARTESIAN_POINT('Ctrl Pts',(-6.73419232108136,0.688980557231193,
-18.7298538593873));
#43547=CARTESIAN_POINT('Ctrl Pts',(-6.74765593860622,0.511300629954842,
-18.7214117578055));
#43548=CARTESIAN_POINT('Ctrl Pts',(-6.76053780325359,0.341298119893798,
-18.7133344331403));
#43549=CARTESIAN_POINT('Ctrl Pts',(-6.76699127607909,0.17087146288988,-18.7052571084752));
#43550=CARTESIAN_POINT('Ctrl Pts',(-6.76699999116249,0.00034584227915461,
-18.6971797838101));
#43551=CARTESIAN_POINT('Ctrl Pts',(-6.76699999116254,0.000345841369450119,
-18.697179783767));
#43552=CARTESIAN_POINT('Ctrl Pts',(-6.76700886075812,-0.173203532875599,
-18.6889592322969));
#43553=CARTESIAN_POINT('Ctrl Pts',(-6.76033706239097,-0.347008637377228,
-18.6807386808267));
#43554=CARTESIAN_POINT('Ctrl Pts',(-6.74695149338562,-0.520513732673331,
-18.6725181293566));
#43555=CARTESIAN_POINT('Ctrl Pts',(-6.73358181676881,-0.693812829226717,
-18.6643073379645));
#43556=CARTESIAN_POINT('Ctrl Pts',(-6.71351426905476,-0.866812270721374,
-18.6560965465724));
#43557=CARTESIAN_POINT('Ctrl Pts',(-6.68676770786251,-1.03895458085862,
-18.6478857551803));
#43558=CARTESIAN_POINT('Ctrl Pts',(-6.6600474945024,-1.21092731492747,-18.6396830521757));
#43559=CARTESIAN_POINT('Ctrl Pts',(-6.62666142542678,-1.38204424617926,
-18.6314803491712));
#43560=CARTESIAN_POINT('Ctrl Pts',(-6.58668028507848,-1.55175121142484,
-18.6232776461667));
#43561=CARTESIAN_POINT('Ctrl Pts',(-6.54673044924656,-1.72132529915803,
-18.6150813657316));
#43562=CARTESIAN_POINT('Ctrl Pts',(-6.50019590959801,-1.88949127127693,
-18.6068850852965));
#43563=CARTESIAN_POINT('Ctrl Pts',(-6.44719884464295,-2.05570330000092,
-18.5986888048614));
#43564=CARTESIAN_POINT('Ctrl Pts',(-6.39423269145756,-2.22181838169672,
-18.5904973050973));
#43565=CARTESIAN_POINT('Ctrl Pts',(-6.33481163146196,-2.38598144875708,
-18.5823058053333));
#43566=CARTESIAN_POINT('Ctrl Pts',(-6.26910820932196,-2.54765995764978,
-18.5741143055692));
#43567=CARTESIAN_POINT('Ctrl Pts',(-6.20342535141963,-2.70928786346617,
-18.5659253696282));
#43568=CARTESIAN_POINT('Ctrl Pts',(-6.13146418170005,-2.86843242670336,
-18.5577364336872));
#43569=CARTESIAN_POINT('Ctrl Pts',(-6.05344614695941,-3.02457910226569,
-18.5495474977462));
#43570=CARTESIAN_POINT('Ctrl Pts',(-5.97543825004887,-3.18070548779542,
-18.541359625893));
#43571=CARTESIAN_POINT('Ctrl Pts',(-5.89137521634352,-3.33383443989974,
-18.5331717540398));
#43572=CARTESIAN_POINT('Ctrl Pts',(-5.80152542174885,-3.4834740964735,-18.5249838821867));
#43573=CARTESIAN_POINT('Ctrl Pts',(-5.71167085621008,-3.63312169877981,
-18.5167955755648));
#43574=CARTESIAN_POINT('Ctrl Pts',(-5.61602910355558,-3.77927932862279,
-18.5086072689429));
#43575=CARTESIAN_POINT('Ctrl Pts',(-5.51491303654802,-3.92148227068703,
-18.500418962321));
#43576=CARTESIAN_POINT('Ctrl Pts',(-5.41372845284464,-4.06378157009599,
-18.4922251072662));
#43577=CARTESIAN_POINT('Ctrl Pts',(-5.30706235095607,-4.2021205333795,-18.4840312522114));
#43578=CARTESIAN_POINT('Ctrl Pts',(-5.19526971211486,-4.33606522303136,
-18.4758373971566));
#43579=CARTESIAN_POINT('Ctrl Pts',(-5.08343967464097,-4.4700547219685,-18.4676408009645));
#43580=CARTESIAN_POINT('Ctrl Pts',(-4.96647992018391,-4.59964674775006,
-18.4594442047724));
#43581=CARTESIAN_POINT('Ctrl Pts',(-4.84478375289696,-4.72444275948664,
-18.4512476085802));
#43582=CARTESIAN_POINT('Ctrl Pts',(-4.72294827922223,-4.84938162602292,
-18.4430416296916));
#43583=CARTESIAN_POINT('Ctrl Pts',(-4.59636581679491,-4.96951325720256,
-18.4348356508029));
#43584=CARTESIAN_POINT('Ctrl Pts',(-4.4654651359907,-5.08447736933222,-18.4266296719143));
#43585=CARTESIAN_POINT('Ctrl Pts',(-4.34452065691637,-5.19069740247753,
-18.419047833257));
#43586=CARTESIAN_POINT('Ctrl Pts',(-4.21989040011406,-5.29250639405488,
-18.4114659945997));
#43587=CARTESIAN_POINT('Ctrl Pts',(-4.09193520383977,-5.38965261288488,
-18.4038841559424));
#43588=CARTESIAN_POINT('Ctrl Pts',(-3.94931117518839,-5.49793571119752,
-18.3954331324173));
#43589=CARTESIAN_POINT('Ctrl Pts',(-3.80226569196563,-5.60064567797856,
-18.3869821088921));
#43590=CARTESIAN_POINT('Ctrl Pts',(-3.65126116601532,-5.69741879253653,
-18.3785310853669));
#43591=CARTESIAN_POINT('Ctrl Pts',(-3.50038959506147,-5.79410670124375,
-18.3700875027167));
#43592=CARTESIAN_POINT('Ctrl Pts',(-3.34556620707401,-5.88486799854257,
-18.3616439200665));
#43593=CARTESIAN_POINT('Ctrl Pts',(-3.18728424791836,-5.96938088271904,
-18.3532003374163));
#43594=CARTESIAN_POINT('Ctrl Pts',(-3.02912013461292,-6.05383084442005,
-18.3447630412765));
#43595=CARTESIAN_POINT('Ctrl Pts',(-2.86750287476671,-6.13204151119479,
-18.3363257451367));
#43596=CARTESIAN_POINT('Ctrl Pts',(-2.70295263390817,-6.20373565352755,
-18.3278884489969));
#43597=CARTESIAN_POINT('Ctrl Pts',(-2.53851978709984,-6.27537864755629,
-18.3194571722245));
#43598=CARTESIAN_POINT('Ctrl Pts',(-2.37115843619585,-6.3405142583537,-18.3110258954521));
#43599=CARTESIAN_POINT('Ctrl Pts',(-2.20141135110492,-6.39891217811484,
-18.3025946186798));
#43600=CARTESIAN_POINT('Ctrl Pts',(-2.03173702575806,-6.45728506641407,
-18.2941669558578));
#43601=CARTESIAN_POINT('Ctrl Pts',(-1.85967931772671,-6.50892591343173,
-18.2857392930358));
#43602=CARTESIAN_POINT('Ctrl Pts',(-1.68579950411636,-6.55365310585791,
-18.2773116302138));
#43603=CARTESIAN_POINT('Ctrl Pts',(-1.51197321759026,-6.59836652948513,
-18.2688865617598));
#43604=CARTESIAN_POINT('Ctrl Pts',(-1.3363262647527,-6.63617046040107,-18.2604614933057));
#43605=CARTESIAN_POINT('Ctrl Pts',(-1.15943391848391,-6.66693347714443,
-18.2520364248517));
#43606=CARTESIAN_POINT('Ctrl Pts',(-1.11103075801335,-6.67535118015643,
-18.2497310682382));
#43607=CARTESIAN_POINT('Ctrl Pts',(-1.06253441866942,-6.68324199690499,
-18.2474257116246));
#43608=CARTESIAN_POINT('Ctrl Pts',(-1.01395682684652,-6.69060390049294,
-18.2451203550111));
#43609=CARTESIAN_POINT('Ctrl Pts',(-0.832340800932257,-6.71812769536696,
-18.2365013664866));
#43610=CARTESIAN_POINT('Ctrl Pts',(-0.649669552838091,-6.73824225069642,
-18.2278823779622));
#43611=CARTESIAN_POINT('Ctrl Pts',(-0.466557540377591,-6.75089720418826,
-18.2192633894377));
#43612=CARTESIAN_POINT('Ctrl Pts',(-0.283335827480763,-6.76355973912656,
-18.21063923737));
#43613=CARTESIAN_POINT('Ctrl Pts',(-0.0996731266688622,-6.76875373256227,
-18.2020150853023));
#43614=CARTESIAN_POINT('Ctrl Pts',(0.0838143623222932,-6.76648092827199,
-18.1933909332346));
#43615=CARTESIAN_POINT('Ctrl Pts',(0.273586347176263,-6.76413027982329,
-18.1844714016383));
#43616=CARTESIAN_POINT('Ctrl Pts',(0.463170547829503,-6.75379231080564,
-18.175551870042));
#43617=CARTESIAN_POINT('Ctrl Pts',(0.651889718517968,-6.73552735833584,
-18.1666323384458));
#43618=CARTESIAN_POINT('Ctrl Pts',(0.834699177889882,-6.7178343699962,-18.1579921205865));
#43619=CARTESIAN_POINT('Ctrl Pts',(1.01669666844332,-6.69270343676662,-18.1493519027273));
#43620=CARTESIAN_POINT('Ctrl Pts',(1.19727532199404,-6.66024179766351,-18.1407116848681));
#43621=CARTESIAN_POINT('Ctrl Pts',(1.38661036908222,-6.62620606947917,-18.1316524964033));
#43622=CARTESIAN_POINT('Ctrl Pts',(1.57438517879334,-6.58411110256957,-18.1225933079385));
#43623=CARTESIAN_POINT('Ctrl Pts',(1.75991574583252,-6.53414000214036,-18.1135341194737));
#43624=CARTESIAN_POINT('Ctrl Pts',(1.9454463128717,-6.48416890171115,-18.1044749310089));
#43625=CARTESIAN_POINT('Ctrl Pts',(2.1287322823246,-6.42632181451492,-18.0954157425442));
#43626=CARTESIAN_POINT('Ctrl Pts',(2.30911086639724,-6.36084082544802,-18.0863565540794));
#43627=CARTESIAN_POINT('Ctrl Pts',(2.48917695722757,-6.2954732776008,-18.0773130600231));
#43628=CARTESIAN_POINT('Ctrl Pts',(2.66651190243871,-6.22243883210547,-18.0682695659668));
#43629=CARTESIAN_POINT('Ctrl Pts',(2.84048899588266,-6.14197942558175,-18.0592260719105));
#43630=CARTESIAN_POINT('Ctrl Pts',(3.01430695311574,-6.06159361498282,-18.0501908499051));
#43631=CARTESIAN_POINT('Ctrl Pts',(3.18477297476097,-5.9737965026322,-18.0411556278997));
#43632=CARTESIAN_POINT('Ctrl Pts',(3.35128118281941,-5.87887773590169,-18.0321204058943));
#43633=CARTESIAN_POINT('Ctrl Pts',(3.51749603966346,-5.7841261953747,-18.0231011019832));
#43634=CARTESIAN_POINT('Ctrl Pts',(3.67976680017574,-5.68227817263267,-18.014081798072));
#43635=CARTESIAN_POINT('Ctrl Pts',(3.83751312385074,-5.57366863244249,-18.0050624941609));
#43636=CARTESIAN_POINT('Ctrl Pts',(3.99506154374408,-5.46519535050687,-17.9960545055965));
#43637=CARTESIAN_POINT('Ctrl Pts',(4.14809665906958,-5.34997761448417,-17.9870465170321));
#43638=CARTESIAN_POINT('Ctrl Pts',(4.29606583103446,-5.2283943400836,-17.9780385284677));
#43639=CARTESIAN_POINT('Ctrl Pts',(4.4437008094418,-5.10708566576675,-17.969050884761));
#43640=CARTESIAN_POINT('Ctrl Pts',(4.58629249937627,-4.97944030133634,-17.9600632410543));
#43641=CARTESIAN_POINT('Ctrl Pts',(4.72332052205592,-4.84587786122653,-17.9510755973476));
#43642=CARTESIAN_POINT('Ctrl Pts',(4.84266243237038,-4.72955423313019,-17.9432479826144));
#43643=CARTESIAN_POINT('Ctrl Pts',(4.95778453973587,-4.60874309349494,-17.9354203678813));
#43644=CARTESIAN_POINT('Ctrl Pts',(5.06836256078318,-4.48374731139606,-17.9275927531481));
#43645=CARTESIAN_POINT('Ctrl Pts',(5.18311562620026,-4.35403212003886,-17.9194695947028));
#43646=CARTESIAN_POINT('Ctrl Pts',(5.29292244058772,-4.21986720072514,-17.9113464362575));
#43647=CARTESIAN_POINT('Ctrl Pts',(5.39742676618268,-4.08167530601036,-17.9032232778122));
#43648=CARTESIAN_POINT('Ctrl Pts',(5.50192372367604,-3.94349315454703,-17.895100692092));
#43649=CARTESIAN_POINT('Ctrl Pts',(5.60111871627963,-3.80128488517399,-17.8869781063719));
#43650=CARTESIAN_POINT('Ctrl Pts',(5.69469686456815,-3.65550497478497,-17.8788555206518));
#43651=CARTESIAN_POINT('Ctrl Pts',(5.7882862572339,-3.50970754743998,-17.8707319589194));
#43652=CARTESIAN_POINT('Ctrl Pts',(5.87625726494517,-3.36033793316674,-17.862608397187));
#43653=CARTESIAN_POINT('Ctrl Pts',(5.95833930282776,-3.20787807629561,-17.8544848354546));
#43654=CARTESIAN_POINT('Ctrl Pts',(6.04048112773466,-3.05530717051045,-17.8463553566715));
#43655=CARTESIAN_POINT('Ctrl Pts',(6.11672524203291,-2.89964184915036,-17.8382258778884));
#43656=CARTESIAN_POINT('Ctrl Pts',(6.18684757181488,-2.74138762730269,-17.8300963991053));
#43657=CARTESIAN_POINT('Ctrl Pts',(6.25699848923641,-2.58306888799438,-17.8219636060768));
#43658=CARTESIAN_POINT('Ctrl Pts',(6.32102251216015,-2.42215948422491,-17.8138308130482));
#43659=CARTESIAN_POINT('Ctrl Pts',(6.37874448824341,-2.25918298367006,-17.8056980200197));
#43660=CARTESIAN_POINT('Ctrl Pts',(6.43652922821884,-2.0960292708955,-17.7975563838126));
#43661=CARTESIAN_POINT('Ctrl Pts',(6.48799812596531,-1.93080432108446,-17.7894147476055));
#43662=CARTESIAN_POINT('Ctrl Pts',(6.53302626424293,-1.76404558634748,-17.7812731113983));
#43663=CARTESIAN_POINT('Ctrl Pts',(6.55596748908339,-1.6790842760636,-17.7771250583377));
#43664=CARTESIAN_POINT('Ctrl Pts',(6.57723766630649,-1.59372499292872,-17.7729770052771));
#43665=CARTESIAN_POINT('Ctrl Pts',(6.59682542287081,-1.50803956850123,-17.7688289522164));
#43666=CARTESIAN_POINT('Ctrl Pts',(6.63668380168188,-1.33368156613357,-17.7603882372383));
#43667=CARTESIAN_POINT('Ctrl Pts',(6.6696548284095,-1.15761355221121,-17.7519475222603));
#43668=CARTESIAN_POINT('Ctrl Pts',(6.69560246401532,-0.980406366703095,
-17.7435068072822));
#43669=CARTESIAN_POINT('Ctrl Pts',(6.72153048717569,-0.803333122734483,
-17.7350724721942));
#43670=CARTESIAN_POINT('Ctrl Pts',(6.74044565347653,-0.625122752326402,
-17.7266381371062));
#43671=CARTESIAN_POINT('Ctrl Pts',(6.75226295239851,-0.446356384144486,
-17.7182038020182));
#43672=CARTESIAN_POINT('Ctrl Pts',(6.76407313393036,-0.267697684389556,
-17.7097745468095));
#43673=CARTESIAN_POINT('Ctrl Pts',(6.76879394889027,-0.0884839863314638,
-17.7013452916009));
#43674=CARTESIAN_POINT('Ctrl Pts',(6.76639216127063,0.0906979597089435,
-17.6929160363923));
#43675=CARTESIAN_POINT('Ctrl Pts',(6.7639914517972,0.269799472186608,-17.6844905650193));
#43676=CARTESIAN_POINT('Ctrl Pts',(6.75447451926184,0.448868928234639,-17.6760650936463));
#43677=CARTESIAN_POINT('Ctrl Pts',(6.73786021552276,0.627318671869125,-17.6676396222733));
#43678=CARTESIAN_POINT('Ctrl Pts',(6.72125082345384,0.805715660582545,-17.659216641714));
#43679=CARTESIAN_POINT('Ctrl Pts',(6.69754827532386,0.983492970610003,-17.6507936611548));
#43680=CARTESIAN_POINT('Ctrl Pts',(6.6668233890321,1.16006676508492,-17.6423706805955));
#43681=CARTESIAN_POINT('Ctrl Pts',(6.63609799400002,1.3366434832552,-17.6339475605692));
#43682=CARTESIAN_POINT('Ctrl Pts',(6.5983500791201,1.51201631652878,-17.6255244405429));
#43683=CARTESIAN_POINT('Ctrl Pts',(6.55370193485421,1.68560966688265,-17.6171013205165));
#43684=CARTESIAN_POINT('Ctrl Pts',(6.50905224658108,1.85920902038388,-17.6086779092047));
#43685=CARTESIAN_POINT('Ctrl Pts',(6.45750193605262,2.03102844523218,-17.6002544978929));
#43686=CARTESIAN_POINT('Ctrl Pts',(6.39922376371957,2.20050544690231,-17.591831086581));
#43687=CARTESIAN_POINT('Ctrl Pts',(6.3409354482813,2.37001194543193,-17.5834062092049));
#43688=CARTESIAN_POINT('Ctrl Pts',(6.27591704493449,2.53717489260836,-17.5749813318287));
#43689=CARTESIAN_POINT('Ctrl Pts',(6.20439037579449,2.70144943775536,-17.5665564544526));
#43690=CARTESIAN_POINT('Ctrl Pts',(6.13284127917035,2.86577549186816,-17.5581289354212));
#43691=CARTESIAN_POINT('Ctrl Pts',(6.05477998124062,3.02721103264571,-17.5497014163898));
#43692=CARTESIAN_POINT('Ctrl Pts',(5.97047554140099,3.18523324256365,-17.5412738973584));
#43693=CARTESIAN_POINT('Ctrl Pts',(5.88609550059781,3.34339716069241,-17.5328388208536));
#43694=CARTESIAN_POINT('Ctrl Pts',(5.79546128818487,3.49814133724314,-17.5244037443488));
#43695=CARTESIAN_POINT('Ctrl Pts',(5.69888740396738,3.64896853328471,-17.515968667844));
#43696=CARTESIAN_POINT('Ctrl Pts',(5.6022668449561,3.79986862510271,-17.5075295146112));
#43697=CARTESIAN_POINT('Ctrl Pts',(5.49970107540827,3.94684768457486,-17.4990903613784));
#43698=CARTESIAN_POINT('Ctrl Pts',(5.39154695743122,4.08943888642612,-17.4906512081456));
#43699=CARTESIAN_POINT('Ctrl Pts',(5.28327264990592,4.23218854708096,-17.4822026766475));
#43700=CARTESIAN_POINT('Ctrl Pts',(5.16939779304018,4.3705403461799,-17.4737541451494));
#43701=CARTESIAN_POINT('Ctrl Pts',(5.05031920151829,4.50406094128129,-17.4653056136513));
#43702=CARTESIAN_POINT('Ctrl Pts',(4.98452441618804,4.57783540216116,-17.4606375258853));
#43703=CARTESIAN_POINT('Ctrl Pts',(4.91714163757313,4.65013557585458,-17.4559694381194));
#43704=CARTESIAN_POINT('Ctrl Pts',(4.84824246668551,4.72089334599155,-17.4513013503534));
#43705=CARTESIAN_POINT('Ctrl Pts',(4.72174813934906,4.85079993879947,-17.4427310495167));
#43706=CARTESIAN_POINT('Ctrl Pts',(4.58984736139188,4.97580553276005,-17.43416074868));
#43707=CARTESIAN_POINT('Ctrl Pts',(4.45295658557858,5.09543586427622,-17.4255904478433));
#43708=CARTESIAN_POINT('Ctrl Pts',(4.32148988795948,5.21032603511549,-17.4173597314791));
#43709=CARTESIAN_POINT('Ctrl Pts',(4.18542130781511,5.32025841659972,-17.4091290151148));
#43710=CARTESIAN_POINT('Ctrl Pts',(4.04515988920989,5.42484750667956,-17.4008982987506));
#43711=CARTESIAN_POINT('Ctrl Pts',(3.90501616407355,5.52934883597,-17.392674488787));
#43712=CARTESIAN_POINT('Ctrl Pts',(3.76068688788923,5.62851558813638,-17.3844506788235));
#43713=CARTESIAN_POINT('Ctrl Pts',(3.61261576397932,5.7220010784557,-17.3762268688599));
#43714=CARTESIAN_POINT('Ctrl Pts',(3.4646649870818,5.81541058704971,-17.3680097429205));
#43715=CARTESIAN_POINT('Ctrl Pts',(3.31297872228734,5.90314784555181,-17.359792616981));
#43716=CARTESIAN_POINT('Ctrl Pts',(3.15803123466129,5.98490833020053,-17.3515754910416));
#43717=CARTESIAN_POINT('Ctrl Pts',(3.13843445406855,5.99524888043058,-17.3505362407988));
#43718=CARTESIAN_POINT('Ctrl Pts',(3.11878554649122,6.00549388532804,-17.3494969905559));
#43719=CARTESIAN_POINT('Ctrl Pts',(3.09908550384714,6.01564277861016,-17.3484577403131));
#43720=CARTESIAN_POINT('Origin',(0.,0.,-63.6971797838103));
#43721=CARTESIAN_POINT('',(3.09908550384715,6.01564277861015,-14.9545069759344));
#43722=CARTESIAN_POINT('',(3.09908550384718,6.01564277861013,-15.3486931990458));
#43723=CARTESIAN_POINT('',(3.09908550384721,6.01564277861012,-63.6971797838103));
#43724=CARTESIAN_POINT('',(-6.76699974845141,-0.0016519250911805,-16.30282021619));
#43725=CARTESIAN_POINT('Ctrl Pts',(-6.76699968617377,-0.00206090370965092,
-16.30282021619));
#43726=CARTESIAN_POINT('Ctrl Pts',(-6.76694375844654,-0.185700202734719,
-16.2942112662645));
#43727=CARTESIAN_POINT('Ctrl Pts',(-6.75940830309195,-0.369187997043884,
-16.2856023163391));
#43728=CARTESIAN_POINT('Ctrl Pts',(-6.74445571692456,-0.551911299434681,
-16.2769933664136));
#43729=CARTESIAN_POINT('Ctrl Pts',(-6.72948741384525,-0.734826665326396,
-16.2683753674777));
#43730=CARTESIAN_POINT('Ctrl Pts',(-6.70708645163332,-0.916975633748548,
-16.2597573685419));
#43731=CARTESIAN_POINT('Ctrl Pts',(-6.67736667878218,-1.0977537233321,-16.2511393696061));
#43732=CARTESIAN_POINT('Ctrl Pts',(-6.64758963169228,-1.27888019806367,
-16.2425047625578));
#43733=CARTESIAN_POINT('Ctrl Pts',(-6.6104656300992,-1.45863021283409,-16.2338701555095));
#43734=CARTESIAN_POINT('Ctrl Pts',(-6.56615938183854,-1.63641069792815,
-16.2252355484613));
#43735=CARTESIAN_POINT('Ctrl Pts',(-6.53432670080435,-1.76414052607361,
-16.2190318480169));
#43736=CARTESIAN_POINT('Ctrl Pts',(-6.49878761153712,-1.8908539874124,-16.2128281475725));
#43737=CARTESIAN_POINT('Ctrl Pts',(-6.45961868919721,-2.01633712215346,
-16.2066244471282));
#43738=CARTESIAN_POINT('Ctrl Pts',(-6.40632570504453,-2.18706866930073,
-16.1981837321501));
#43739=CARTESIAN_POINT('Ctrl Pts',(-6.34622040540474,-2.35581222350463,
-16.189743017172));
#43740=CARTESIAN_POINT('Ctrl Pts',(-6.27947247758363,-2.52200602760376,
-16.1813023021939));
#43741=CARTESIAN_POINT('Ctrl Pts',(-6.21277500099128,-2.68807421459533,
-16.1728679671059));
#43742=CARTESIAN_POINT('Ctrl Pts',(-6.13944502871916,-2.85159618499573,
-16.1644336320179));
#43743=CARTESIAN_POINT('Ctrl Pts',(-6.05970152261526,-3.01202696814194,
-16.1559992969299));
#43744=CARTESIAN_POINT('Ctrl Pts',(-5.98000604488462,-3.17236112612187,
-16.1475700417213));
#43745=CARTESIAN_POINT('Ctrl Pts',(-5.89390488238898,-3.32960751076188,
-16.1391407865127));
#43746=CARTESIAN_POINT('Ctrl Pts',(-5.80166456771601,-3.48324234639345,
-16.1307115313041));
#43747=CARTESIAN_POINT('Ctrl Pts',(-5.70946565909596,-3.63680821638723,
-16.1222860599311));
#43748=CARTESIAN_POINT('Ctrl Pts',(-5.61113326445851,-3.78676548449717,
-16.1138605885581));
#43749=CARTESIAN_POINT('Ctrl Pts',(-5.50697938482385,-3.93261580314238,
-16.1054351171851));
#43750=CARTESIAN_POINT('Ctrl Pts',(-5.40285629609775,-4.07842300420195,
-16.0970121366259));
#43751=CARTESIAN_POINT('Ctrl Pts',(-5.2929153479968,-4.22012540601256,-16.0885891560667));
#43752=CARTESIAN_POINT('Ctrl Pts',(-5.17751152717624,-4.35725411078551,
-16.0801661755074));
#43753=CARTESIAN_POINT('Ctrl Pts',(-5.06210579550756,-4.49438508612563,
-16.0717430554811));
#43754=CARTESIAN_POINT('Ctrl Pts',(-4.94123721996666,-4.62694195382757,
-16.0633199354548));
#43755=CARTESIAN_POINT('Ctrl Pts',(-4.81530112237883,-4.7544888369642,-16.0548968154284));
#43756=CARTESIAN_POINT('Ctrl Pts',(-4.6893606697109,-4.88204013088458,-16.0464734041166));
#43757=CARTESIAN_POINT('Ctrl Pts',(-4.55835257978465,-5.00458085735821,
-16.0380499928047));
#43758=CARTESIAN_POINT('Ctrl Pts',(-4.42270919529753,-5.12171185970381,
-16.0296265814929));
#43759=CARTESIAN_POINT('Ctrl Pts',(-4.28704220257016,-5.23886324827654,
-16.0212017041168));
#43760=CARTESIAN_POINT('Ctrl Pts',(-4.14673855925296,-5.35060281760719,
-16.0127768267407));
#43761=CARTESIAN_POINT('Ctrl Pts',(-4.00226412717075,-5.45657134621753,
-16.0043519493646));
#43762=CARTESIAN_POINT('Ctrl Pts',(-3.85774439452989,-5.56257310170044,
-15.9959244303331));
#43763=CARTESIAN_POINT('Ctrl Pts',(-3.70905153459146,-5.66280001157985,
-15.9874969113017));
#43764=CARTESIAN_POINT('Ctrl Pts',(-3.55668114302472,-5.7569356646442,-15.9790693922703));
#43765=CARTESIAN_POINT('Ctrl Pts',(-3.40417411157982,-5.85115573492395,
-15.9706343157655));
#43766=CARTESIAN_POINT('Ctrl Pts',(-3.24798324287393,-5.93927345827658,
-15.9621992392607));
#43767=CARTESIAN_POINT('Ctrl Pts',(-3.0886305295471,-6.02101739342693,-15.9537641627559));
#43768=CARTESIAN_POINT('Ctrl Pts',(-2.92920080000524,-6.10280083595908,
-15.9453250095232));
#43769=CARTESIAN_POINT('Ctrl Pts',(-2.76660647833734,-6.17820420171611,
-15.9368858562904));
#43770=CARTESIAN_POINT('Ctrl Pts',(-2.60139086113565,-6.24700364875833,
-15.9284467030577));
#43771=CARTESIAN_POINT('Ctrl Pts',(-2.43599164306149,-6.31587955127563,
-15.9199981715596));
#43772=CARTESIAN_POINT('Ctrl Pts',(-2.26796561981151,-6.37813675046467,
-15.9115496400614));
#43773=CARTESIAN_POINT('Ctrl Pts',(-2.09787376510411,-6.43360044342885,
-15.9031011085633));
#43774=CARTESIAN_POINT('Ctrl Pts',(-2.00389249673217,-6.46424593331626,
-15.8984330207972));
#43775=CARTESIAN_POINT('Ctrl Pts',(-1.90928079902951,-6.49281830858076,
-15.8937649330312));
#43776=CARTESIAN_POINT('Ctrl Pts',(-1.81413482365927,-6.51929473498374,
-15.8890968452651));
#43777=CARTESIAN_POINT('Ctrl Pts',(-1.64616955152901,-6.56603470636466,
-15.8808560696683));
#43778=CARTESIAN_POINT('Ctrl Pts',(-1.47616488830859,-6.60634379464391,
-15.8726152940716));
#43779=CARTESIAN_POINT('Ctrl Pts',(-1.30465256828463,-6.64004297245645,
-15.8643745184748));
#43780=CARTESIAN_POINT('Ctrl Pts',(-1.13333021674917,-6.67370482477615,
-15.8561428704304));
#43781=CARTESIAN_POINT('Ctrl Pts',(-0.96050387951586,-6.70077127646936,
-15.8479112223861));
#43782=CARTESIAN_POINT('Ctrl Pts',(-0.78672063134305,-6.72111297689744,
-15.8396795743417));
#43783=CARTESIAN_POINT('Ctrl Pts',(-0.613098897160356,-6.74143577176796,
-15.8314555767834));
#43784=CARTESIAN_POINT('Ctrl Pts',(-0.438522374509828,-6.75504622128248,
-15.8232315792251));
#43785=CARTESIAN_POINT('Ctrl Pts',(-0.263548616740972,-6.76186595006245,
-15.8150075816668));
#43786=CARTESIAN_POINT('Ctrl Pts',(-0.0887294489668274,-6.76867965358555,
-15.8067908500423));
#43787=CARTESIAN_POINT('Ctrl Pts',(0.0864859002690414,-6.76871458046289,
-15.7985741184178));
#43788=CARTESIAN_POINT('Ctrl Pts',(0.261534590517598,-6.76194414779972,
-15.7903573867933));
#43789=CARTESIAN_POINT('Ctrl Pts',(0.436493596841361,-6.75517718387986,
-15.7821448649046));
#43790=CARTESIAN_POINT('Ctrl Pts',(0.611285759586278,-6.74161181814315,
-15.773932343016));
#43791=CARTESIAN_POINT('Ctrl Pts',(0.785347648178865,-6.72127354535582,
-15.7657198211273));
#43792=CARTESIAN_POINT('Ctrl Pts',(0.959351329638174,-6.70094207378478,
-15.7575100455454));
#43793=CARTESIAN_POINT('Ctrl Pts',(1.13262487044065,-6.67384224834337,-15.7493002699636));
#43794=CARTESIAN_POINT('Ctrl Pts',(1.30460927888467,-6.64005147792154,-15.7410904943818));
#43795=CARTESIAN_POINT('Ctrl Pts',(1.37972760030674,-6.62529254729166,-15.7375046776991));
#43796=CARTESIAN_POINT('Ctrl Pts',(1.45460007362233,-6.60925784080126,-15.7339188610164));
#43797=CARTESIAN_POINT('Ctrl Pts',(1.52918061718094,-6.59195689003183,-15.7303330443337));
#43798=CARTESIAN_POINT('Ctrl Pts',(1.71343096416494,-6.54921509665893,-15.721474326812));
#43799=CARTESIAN_POINT('Ctrl Pts',(1.8957078910182,-6.49878607415575,-15.7126156092902));
#43800=CARTESIAN_POINT('Ctrl Pts',(2.07539519919948,-6.44088687737487,-15.7037568917684));
#43801=CARTESIAN_POINT('Ctrl Pts',(2.2554186734751,-6.3828793604959,-15.694881601009));
#43802=CARTESIAN_POINT('Ctrl Pts',(2.43284260030617,-6.31737381980341,-15.6860063102495));
#43803=CARTESIAN_POINT('Ctrl Pts',(2.60707018573707,-6.24463562160683,-15.6771310194901));
#43804=CARTESIAN_POINT('Ctrl Pts',(2.78179261668468,-6.1716908305726,-15.6682305209093));
#43805=CARTESIAN_POINT('Ctrl Pts',(2.95330029856249,-6.09147237476867,-15.6593300223285));
#43806=CARTESIAN_POINT('Ctrl Pts',(3.121017748684,-6.00429323171341,-15.6504295237478));
#43807=CARTESIAN_POINT('Ctrl Pts',(3.28896223814215,-5.91699607413555,-15.6415169765502));
#43808=CARTESIAN_POINT('Ctrl Pts',(3.45310601962957,-5.82271953233222,-15.6326044293525));
#43809=CARTESIAN_POINT('Ctrl Pts',(3.61290095983023,-5.72182100860013,-15.6236918821549));
#43810=CARTESIAN_POINT('Ctrl Pts',(3.77304874286516,-5.62069969107343,-15.6147596551827));
#43811=CARTESIAN_POINT('Ctrl Pts',(3.92882825750772,-5.51292728426395,-15.6058274282104));
#43812=CARTESIAN_POINT('Ctrl Pts',(4.0797206076869,-5.39890440397076,-15.5968952012381));
#43813=CARTESIAN_POINT('Ctrl Pts',(4.22233130302963,-5.29113961520391,-15.5884532152928));
#43814=CARTESIAN_POINT('Ctrl Pts',(4.36057671102482,-5.17779209576435,-15.5800112293474));
#43815=CARTESIAN_POINT('Ctrl Pts',(4.49404799525455,-5.05923132662943,-15.5715692434021));
#43816=CARTESIAN_POINT('Ctrl Pts',(4.62407242719406,-4.9437323506059,-15.5633452689845));
#43817=CARTESIAN_POINT('Ctrl Pts',(4.74981382066025,-4.82306450254085,-15.5551212945669));
#43818=CARTESIAN_POINT('Ctrl Pts',(4.87083694085045,-4.69757772640823,-15.5468973201494));
#43819=CARTESIAN_POINT('Ctrl Pts',(4.99173224888356,-4.57222347648644,-15.5386820310467));
#43820=CARTESIAN_POINT('Ctrl Pts',(5.10791895950427,-4.44206068889404,-15.5304667419441));
#43821=CARTESIAN_POINT('Ctrl Pts',(5.21899553731649,-4.30747891248125,-15.5222514528414));
#43822=CARTESIAN_POINT('Ctrl Pts',(5.32997708707946,-4.17301227324614,-15.5140431920692));
#43823=CARTESIAN_POINT('Ctrl Pts',(5.43585698396787,-4.03413444949387,-15.505834931297));
#43824=CARTESIAN_POINT('Ctrl Pts',(5.5362710917825,-3.89127118025632,-15.4976266705248));
#43825=CARTESIAN_POINT('Ctrl Pts',(5.63661942868097,-3.74850148599851,-15.4894237861369));
#43826=CARTESIAN_POINT('Ctrl Pts',(5.73150890217019,-3.60175183833447,-15.4812209017491));
#43827=CARTESIAN_POINT('Ctrl Pts',(5.82061612079869,-3.45148040329051,-15.4730180173612));
#43828=CARTESIAN_POINT('Ctrl Pts',(5.90968283875454,-3.30127726904522,-15.4648188613169));
#43829=CARTESIAN_POINT('Ctrl Pts',(5.99297235524397,-3.14755584425924,-15.4566197052727));
#43830=CARTESIAN_POINT('Ctrl Pts',(6.07020498216446,-2.99080264720122,-15.4484205492285));
#43831=CARTESIAN_POINT('Ctrl Pts',(6.14743089172441,-2.83406308385969,-15.4402221063115));
#43832=CARTESIAN_POINT('Ctrl Pts',(6.21860079500695,-2.67429259113385,-15.4320236633945));
#43833=CARTESIAN_POINT('Ctrl Pts',(6.28348113694317,-2.51200195097046,-15.4238252204774));
#43834=CARTESIAN_POINT('Ctrl Pts',(6.34836083274802,-2.34971292702967,-15.4156268592072));
#43835=CARTESIAN_POINT('Ctrl Pts',(6.40695095783095,-2.18490413831689,-15.407428497937));
#43836=CARTESIAN_POINT('Ctrl Pts',(6.45906631490303,-2.0181058792058,-15.3992301366667));
#43837=CARTESIAN_POINT('Ctrl Pts',(6.51119062009564,-1.85127898110976,-15.3910303677514));
#43838=CARTESIAN_POINT('Ctrl Pts',(6.55683783545461,-1.68246227445443,-15.3828305988362));
#43839=CARTESIAN_POINT('Ctrl Pts',(6.59587278640836,-1.51220077553138,-15.3746308299209));
#43840=CARTESIAN_POINT('Ctrl Pts',(6.63492153065081,-1.34187911344802,-15.3664281635566));
#43841=CARTESIAN_POINT('Ctrl Pts',(6.66735327604792,-1.17011199152787,-15.3582254971923));
#43842=CARTESIAN_POINT('Ctrl Pts',(6.69308404909215,-0.997454215384487,
-15.350022830828));
#43843=CARTESIAN_POINT('Ctrl Pts',(6.7188440458631,-0.824600343163547,-15.3418108482849));
#43844=CARTESIAN_POINT('Ctrl Pts',(6.73788781280401,-0.650854150958018,
-15.3335988657419));
#43845=CARTESIAN_POINT('Ctrl Pts',(6.75018321515767,-0.476776217741226,
-15.3253868831989));
#43846=CARTESIAN_POINT('Ctrl Pts',(6.76248586950582,-0.302595611006688,
-15.3171700571176));
#43847=CARTESIAN_POINT('Ctrl Pts',(6.76803221378007,-0.128083231145394,
-15.3089532310363));
#43848=CARTESIAN_POINT('Ctrl Pts',(6.76684228280827,0.0462008614439957,
-15.300736404955));
#43849=CARTESIAN_POINT('Ctrl Pts',(6.76565051679105,0.220753725275382,-15.2925069073411));
#43850=CARTESIAN_POINT('Ctrl Pts',(6.75770173226373,0.395077240247219,-15.2842774097272));
#43851=CARTESIAN_POINT('Ctrl Pts',(6.74306793982273,0.568615651327713,-15.2760479121134));
#43852=CARTESIAN_POINT('Ctrl Pts',(6.73002400076775,0.723300396718125,-15.2687124885886));
#43853=CARTESIAN_POINT('Ctrl Pts',(6.71166946035732,0.877361294022358,-15.2613770650638));
#43854=CARTESIAN_POINT('Ctrl Pts',(6.68808929934123,1.03041279302879,-15.2540416415391));
#43855=CARTESIAN_POINT('Ctrl Pts',(6.66214389424629,1.19881635649048,-15.2459704271499));
#43856=CARTESIAN_POINT('Ctrl Pts',(6.6297863745111,1.36654684253158,-15.2378992127606));
#43857=CARTESIAN_POINT('Ctrl Pts',(6.59105446675761,1.53306556162305,-15.2298279983714));
#43858=CARTESIAN_POINT('Ctrl Pts',(6.55237110533006,1.69937556721494,-15.2217669003908));
#43859=CARTESIAN_POINT('Ctrl Pts',(6.50732933721513,1.86447646922579,-15.2137058024102));
#43860=CARTESIAN_POINT('Ctrl Pts',(6.45601863229179,2.0278344161941,-15.2056447044296));
#43861=CARTESIAN_POINT('Ctrl Pts',(6.40476098686464,2.19102343758676,-15.1975919422884));
#43862=CARTESIAN_POINT('Ctrl Pts',(6.34724741661247,2.35247273791885,-15.1895391801472));
#43863=CARTESIAN_POINT('Ctrl Pts',(6.28361843518846,2.51165848812289,-15.181486418006));
#43864=CARTESIAN_POINT('Ctrl Pts',(6.22004131774242,2.6707144860339,-15.1734402196706));
#43865=CARTESIAN_POINT('Ctrl Pts',(6.15035884863705,2.82751026159654,-15.1653940213353));
#43866=CARTESIAN_POINT('Ctrl Pts',(6.07476135706578,2.98153709597923,-15.1573478229999));
#43867=CARTESIAN_POINT('Ctrl Pts',(5.99535398464795,3.14332640863964,-15.1488961210389));
#43868=CARTESIAN_POINT('Ctrl Pts',(5.90942006254912,3.30206005554164,-15.1404444190778));
#43869=CARTESIAN_POINT('Ctrl Pts',(5.81723777276029,3.45717134304491,-15.1319927171167));
#43870=CARTESIAN_POINT('Ctrl Pts',(5.72955553002772,3.60471058938582,-15.1239536004431));
#43871=CARTESIAN_POINT('Ctrl Pts',(5.63622066750068,3.74897236409537,-15.1159144837695));
#43872=CARTESIAN_POINT('Ctrl Pts',(5.53751977969006,3.88949401459127,-15.1078753670959));
#43873=CARTESIAN_POINT('Ctrl Pts',(5.43882850951006,4.03000197234987,-15.0998370337714));
#43874=CARTESIAN_POINT('Ctrl Pts',(5.33477246883049,4.1667702254605,-15.0917987004469));
#43875=CARTESIAN_POINT('Ctrl Pts',(5.22568128450892,4.29936554769808,-15.0837603671225));
#43876=CARTESIAN_POINT('Ctrl Pts',(5.11657913495448,4.4319741976724,-15.0757212258299));
#43877=CARTESIAN_POINT('Ctrl Pts',(5.00244107187347,4.56040879379873,-15.0676820845373));
#43878=CARTESIAN_POINT('Ctrl Pts',(4.88363656133641,4.68426973356342,-15.0596429432447));
#43879=CARTESIAN_POINT('Ctrl Pts',(4.76479658663491,4.80816764688001,-15.0516014021996));
#43880=CARTESIAN_POINT('Ctrl Pts',(4.6412876507134,4.92748891767104,-15.0435598611544));
#43881=CARTESIAN_POINT('Ctrl Pts',(4.51351544708178,5.04187140940288,-15.0355183201093));
#43882=CARTESIAN_POINT('Ctrl Pts',(4.38561739910311,5.15636655779694,-15.0274688588557));
#43883=CARTESIAN_POINT('Ctrl Pts',(4.25344797869773,5.26591296694721,-15.0194193976022));
#43884=CARTESIAN_POINT('Ctrl Pts',(4.117445765198,5.37018895111271,-15.0113699363486));
#43885=CARTESIAN_POINT('Ctrl Pts',(3.98136553561481,5.47452475198027,-15.0033158576155));
#43886=CARTESIAN_POINT('Ctrl Pts',(3.84144843792085,5.57358389181528,-14.9952617788824));
#43887=CARTESIAN_POINT('Ctrl Pts',(3.69816084534254,5.66708879072628,-14.9872077001493));
#43888=CARTESIAN_POINT('Ctrl Pts',(3.55469045356767,5.76071297854489,-14.9791433464224));
#43889=CARTESIAN_POINT('Ctrl Pts',(3.40784130244595,5.84876859034578,-14.9710789926955));
#43890=CARTESIAN_POINT('Ctrl Pts',(3.2581036634238,5.93102432286232,-14.9630146389686));
#43891=CARTESIAN_POINT('Ctrl Pts',(3.20544735148314,5.9599501396348,-14.9601787512905));
#43892=CARTESIAN_POINT('Ctrl Pts',(3.15243401629433,5.98815916502779,-14.9573428636125));
#43893=CARTESIAN_POINT('Ctrl Pts',(3.09908550384716,6.01564277861015,-14.9545069759344));
#43894=CARTESIAN_POINT('Ctrl Pts',(3.09908550384726,6.0156427786101,-16.9542436419538));
#43895=CARTESIAN_POINT('Ctrl Pts',(2.9337323201833,6.1008279655248,-16.9454941940546));
#43896=CARTESIAN_POINT('Ctrl Pts',(2.76486502144424,6.17919158180191,-16.9367447461553));
#43897=CARTESIAN_POINT('Ctrl Pts',(2.59305716434346,6.25046746591382,-16.927995298256));
#43898=CARTESIAN_POINT('Ctrl Pts',(2.42125069459278,6.32174277447227,-16.9192459210085));
#43899=CARTESIAN_POINT('Ctrl Pts',(2.24650397871055,6.38593035557827,-16.9104965437611));
#43900=CARTESIAN_POINT('Ctrl Pts',(2.06941053323769,6.44281220003539,-16.9017471665137));
#43901=CARTESIAN_POINT('Ctrl Pts',(1.89231845896684,6.49969360406685,-16.8929978570111));
#43902=CARTESIAN_POINT('Ctrl Pts',(1.71287996431508,6.5492692970088,-16.8842485475085));
#43903=CARTESIAN_POINT('Ctrl Pts',(1.5317044917351,6.59137090065478,-16.8754992380059));
#43904=CARTESIAN_POINT('Ctrl Pts',(1.35053036178179,6.63347219230081,-16.8667499933413));
#43905=CARTESIAN_POINT('Ctrl Pts',(1.16761955878856,6.66809944062452,-16.8580007486768));
#43906=CARTESIAN_POINT('Ctrl Pts',(0.98359330931063,6.69513503985389,-16.8492515040122));
#43907=CARTESIAN_POINT('Ctrl Pts',(0.799568362460039,6.72217044771214,-16.840502321279));
#43908=CARTESIAN_POINT('Ctrl Pts',(0.614428268438568,6.74161427235978,-16.8317531385458));
#43909=CARTESIAN_POINT('Ctrl Pts',(0.428801816330156,6.75340047696803,-16.8230039558126));
#43910=CARTESIAN_POINT('Ctrl Pts',(0.243176616522558,6.76518660206243,-16.8142548321045));
#43911=CARTESIAN_POINT('Ctrl Pts',(0.0570653511651231,6.76931519233997,
-16.8055057083963));
#43912=CARTESIAN_POINT('Ctrl Pts',(-0.12889990080048,6.76577222610794,-16.7967565846882));
#43913=CARTESIAN_POINT('Ctrl Pts',(-0.314863959942389,6.76222928260131,
-16.788007517099));
#43914=CARTESIAN_POINT('Ctrl Pts',(-0.500681721080966,6.75101488651274,
-16.7792584495097));
#43915=CARTESIAN_POINT('Ctrl Pts',(-0.685722110173501,6.73216712415989,
-16.7705093819204));
#43916=CARTESIAN_POINT('Ctrl Pts',(-0.870761373827683,6.71331947644144,
-16.7617603675441));
#43917=CARTESIAN_POINT('Ctrl Pts',(-1.05502298984337,6.68683858439997,-16.7530113531677));
#43918=CARTESIAN_POINT('Ctrl Pts',(-1.23788117676041,6.65281438131429,-16.7442623387914));
#43919=CARTESIAN_POINT('Ctrl Pts',(-1.43009641451775,6.61704912302381,-16.7350656279038));
#43920=CARTESIAN_POINT('Ctrl Pts',(-1.62076048992678,6.57294837083169,-16.7258689170163));
#43921=CARTESIAN_POINT('Ctrl Pts',(-1.80915798961115,6.52067760042054,-16.7166722061288));
#43922=CARTESIAN_POINT('Ctrl Pts',(-1.98840443003001,6.47094578577412,-16.7079222084223));
#43923=CARTESIAN_POINT('Ctrl Pts',(-2.16559895952187,6.41381888474477,-16.6991722107158));
#43924=CARTESIAN_POINT('Ctrl Pts',(-2.34013966242323,6.34949095285234,-16.6904222130093));
#43925=CARTESIAN_POINT('Ctrl Pts',(-2.51467682554013,6.28516432556686,-16.6816723927577));
#43926=CARTESIAN_POINT('Ctrl Pts',(-2.68656000078838,6.21363705879663,-16.6729225725061));
#43927=CARTESIAN_POINT('Ctrl Pts',(-2.85520533840881,6.13515211510862,-16.6641727522545));
#43928=CARTESIAN_POINT('Ctrl Pts',(-3.02384747998319,6.05666865881125,-16.6554230978232));
#43929=CARTESIAN_POINT('Ctrl Pts',(-3.18925164684528,5.97122791039849,-16.646673443392));
#43930=CARTESIAN_POINT('Ctrl Pts',(-3.35085601829148,5.87912008251913,-16.6379237889607));
#43931=CARTESIAN_POINT('Ctrl Pts',(-3.51245754191405,5.78701387778182,-16.6291742887176));
#43932=CARTESIAN_POINT('Ctrl Pts',(-3.6702591551092,5.68824097060993,-16.6204247884745));
#43933=CARTESIAN_POINT('Ctrl Pts',(-3.82372487928815,5.58313684656868,-16.6116752882313));
#43934=CARTESIAN_POINT('Ctrl Pts',(-3.97718810300776,5.47803443501789,-16.6029259305462));
#43935=CARTESIAN_POINT('Ctrl Pts',(-4.12631534263,5.36660117496396,-16.5941765728611));
#43936=CARTESIAN_POINT('Ctrl Pts',(-4.27060009886196,5.24921554097374,-16.585427215176));
#43937=CARTESIAN_POINT('Ctrl Pts',(-4.41488269594188,5.13183166360313,-16.5766779884208));
#43938=CARTESIAN_POINT('Ctrl Pts',(-4.55432273235066,5.00849577139491,-16.5679287616656));
#43939=CARTESIAN_POINT('Ctrl Pts',(-4.68844662480187,4.87962675277361,-16.5591795349104));
#43940=CARTESIAN_POINT('Ctrl Pts',(-4.82256868835127,4.75075949139912,-16.5504304274589));
#43941=CARTESIAN_POINT('Ctrl Pts',(-4.95137454637822,4.61635945312568,-16.5416813200075));
#43942=CARTESIAN_POINT('Ctrl Pts',(-5.07442674461028,4.47688309134647,-16.532932212556));
#43943=CARTESIAN_POINT('Ctrl Pts',(-5.19747742838496,4.33740844616403,-16.5241832127836));
#43944=CARTESIAN_POINT('Ctrl Pts',(-5.3147744045089,4.19285781736076,-16.5154342130112));
#43945=CARTESIAN_POINT('Ctrl Pts',(-5.42591931531122,4.04372211999448,-16.5066852132388));
#43946=CARTESIAN_POINT('Ctrl Pts',(-5.53707636462956,3.89457013500837,-16.4979352579583));
#43947=CARTESIAN_POINT('Ctrl Pts',(-5.64207983273451,3.74083230916451,-16.4891853026777));
#43948=CARTESIAN_POINT('Ctrl Pts',(-5.74057303468732,3.58303087251851,-16.4804353473971));
#43949=CARTESIAN_POINT('Ctrl Pts',(-5.83906243363747,3.42523552887461,-16.4716857299683));
#43950=CARTESIAN_POINT('Ctrl Pts',(-5.93104191768405,3.2633771315703,-16.4629361125395));
#43951=CARTESIAN_POINT('Ctrl Pts',(-6.01619906699633,3.098005452912,-16.4541864951107));
#43952=CARTESIAN_POINT('Ctrl Pts',(-6.10135338095362,2.93263928039639,-16.4454371690053));
#43953=CARTESIAN_POINT('Ctrl Pts',(-6.1796856835282,2.76376031540267,-16.4366878428999));
#43954=CARTESIAN_POINT('Ctrl Pts',(-6.25092992694869,2.59194213831584,-16.4279385167945));
#43955=CARTESIAN_POINT('Ctrl Pts',(-6.32217217691087,2.42012876880863,-16.4191894355007));
#43956=CARTESIAN_POINT('Ctrl Pts',(-6.38632665483835,2.24537661647715,-16.4104403542069));
#43957=CARTESIAN_POINT('Ctrl Pts',(-6.44317547869335,2.06827917621502,-16.4016912729131));
#43958=CARTESIAN_POINT('Ctrl Pts',(-6.50002944235924,1.89116572423465,-16.3929414005982));
#43959=CARTESIAN_POINT('Ctrl Pts',(-6.54957634250388,1.71170683289237,-16.3841915282832));
#43960=CARTESIAN_POINT('Ctrl Pts',(-6.59164787708387,1.53051209225399,-16.3754416559682));
#43961=CARTESIAN_POINT('Ctrl Pts',(-6.63371649074998,1.34932993148081,-16.3666923911335));
#43962=CARTESIAN_POINT('Ctrl Pts',(-6.66831071257112,1.16641244174071,-16.3579431262987));
#43963=CARTESIAN_POINT('Ctrl Pts',(-6.69531304840321,0.982380875160844,
-16.3491938614639));
#43964=CARTESIAN_POINT('Ctrl Pts',(-6.72231677033033,0.79833986179671,-16.3404441475082));
#43965=CARTESIAN_POINT('Ctrl Pts',(-6.74172778477882,0.613184940731055,
-16.3316944335526));
#43966=CARTESIAN_POINT('Ctrl Pts',(-6.75348015835512,0.427545027691487,
-16.3229447195969));
#43967=CARTESIAN_POINT('Ctrl Pts',(-6.76249038365218,0.285219953547709,
-16.3162365517946));
#43968=CARTESIAN_POINT('Ctrl Pts',(-6.76699999999999,0.142609995758143,
-16.3095283839923));
#43969=CARTESIAN_POINT('Ctrl Pts',(-6.767,7.07605502806519E-13,-16.30282021619));
#43970=CARTESIAN_POINT('',(-6.76699777839932,0.00548335104101128,-16.6971797838448));
#43971=CARTESIAN_POINT('Ctrl Pts',(3.09908550384714,6.01564277861016,-17.3484577403131));
#43972=CARTESIAN_POINT('Ctrl Pts',(2.94341968881325,6.09583731285535,-17.3402457917913));
#43973=CARTESIAN_POINT('Ctrl Pts',(2.78455904321523,6.1700270282288,-17.3320338432694));
#43974=CARTESIAN_POINT('Ctrl Pts',(2.62300731811465,6.23795812819523,-17.3238218947476));
#43975=CARTESIAN_POINT('Ctrl Pts',(2.46150629672237,6.30586790769187,-17.3156125235813));
#43976=CARTESIAN_POINT('Ctrl Pts',(2.29731620634852,6.36752284783082,-17.307403152415));
#43977=CARTESIAN_POINT('Ctrl Pts',(2.13096231121924,6.42271660811554,-17.2991937812488));
#43978=CARTESIAN_POINT('Ctrl Pts',(2.08600190077923,6.43763380686342,-17.2969750373065));
#43979=CARTESIAN_POINT('Ctrl Pts',(2.04088354244671,6.45207931767505,-17.2947562933643));
#43980=CARTESIAN_POINT('Ctrl Pts',(1.99561783376721,6.46604967979293,-17.292537549422));
#43981=CARTESIAN_POINT('Ctrl Pts',(1.81488669171063,6.52182875791112,-17.2836788319002));
#43982=CARTESIAN_POINT('Ctrl Pts',(1.63199268618497,6.56997174407535,-17.2748201143784));
#43983=CARTESIAN_POINT('Ctrl Pts',(1.44757753915087,6.61035613776943,-17.2659613968566));
#43984=CARTESIAN_POINT('Ctrl Pts',(1.26281738099823,6.65081608417739,-17.2570861060972));
#43985=CARTESIAN_POINT('Ctrl Pts',(1.07653064752107,6.68348837523857,-17.2482108153378));
#43986=CARTESIAN_POINT('Ctrl Pts',(0.889366602281064,6.70830202411512,-17.2393355245785));
#43987=CARTESIAN_POINT('Ctrl Pts',(0.701670969067837,6.73318614933396,-17.2304350259977));
#43988=CARTESIAN_POINT('Ctrl Pts',(0.513093296472913,6.75016693239313,-17.221534527417));
#43989=CARTESIAN_POINT('Ctrl Pts',(0.324288389596506,6.75922525444839,-17.2126340288362));
#43990=CARTESIAN_POINT('Ctrl Pts',(0.135227897265158,6.76829583876634,-17.2037214816386));
#43991=CARTESIAN_POINT('Ctrl Pts',(-0.0540601844917341,6.76942253308639,
-17.194808934441));
#43992=CARTESIAN_POINT('Ctrl Pts',(-0.242922330392475,6.76263837133088,
-17.1858963872434));
#43993=CARTESIAN_POINT('Ctrl Pts',(-0.432201502356002,6.75583922948365,
-17.1769641602712));
#43994=CARTESIAN_POINT('Ctrl Pts',(-0.621052597054832,6.74109430213405,
-17.1680319332989));
#43995=CARTESIAN_POINT('Ctrl Pts',(-0.808825609984669,6.71848867920702,
-17.1590997063267));
#43996=CARTESIAN_POINT('Ctrl Pts',(-0.986292790456334,6.6971237551369,-17.1506577203812));
#43997=CARTESIAN_POINT('Ctrl Pts',(-1.16279686929245,6.66873778765191,-17.1422157344357));
#43998=CARTESIAN_POINT('Ctrl Pts',(-1.33779861920414,6.6334443432093,-17.1337737484903));
#43999=CARTESIAN_POINT('Ctrl Pts',(-1.50828100612134,6.59906234043424,-17.1255497740727));
#44000=CARTESIAN_POINT('Ctrl Pts',(-1.67766311369186,6.55805832572131,-17.1173257996551));
#44001=CARTESIAN_POINT('Ctrl Pts',(-1.84539273303507,6.51051569853429,-17.1091018252375));
#44002=CARTESIAN_POINT('Ctrl Pts',(-2.01294521362656,6.46302328097431,-17.1008865361348));
#44003=CARTESIAN_POINT('Ctrl Pts',(-2.17884833909721,6.40900609891225,-17.0926712470321));
#44004=CARTESIAN_POINT('Ctrl Pts',(-2.34255909327287,6.34859873472285,-17.0844559579294));
#44005=CARTESIAN_POINT('Ctrl Pts',(-2.50612978989543,6.28824305014156,-17.0762476971573));
#44006=CARTESIAN_POINT('Ctrl Pts',(-2.66751151617282,6.22150819478933,-17.0680394363851));
#44007=CARTESIAN_POINT('Ctrl Pts',(-2.82617536416221,6.14857884482281,-17.0598311756129));
#44008=CARTESIAN_POINT('Ctrl Pts',(-2.9847352878433,6.07569726334513,-17.0516282912251));
#44009=CARTESIAN_POINT('Ctrl Pts',(-3.14058055455183,5.99662941834599,-17.0434254068372));
#44010=CARTESIAN_POINT('Ctrl Pts',(-3.29320114934089,5.91160851122432,-17.0352225224494));
#44011=CARTESIAN_POINT('Ctrl Pts',(-3.44575237560108,5.82662624748011,-17.0270233664052));
#44012=CARTESIAN_POINT('Ctrl Pts',(-3.59508153730921,5.73569648635172,-17.0188242103609));
#44013=CARTESIAN_POINT('Ctrl Pts',(-3.74070211966927,5.63909892198229,-17.0106250543167));
#44014=CARTESIAN_POINT('Ctrl Pts',(-3.88631003657973,5.54250975925199,-17.0024266113997));
#44015=CARTESIAN_POINT('Ctrl Pts',(-4.02820971331193,5.44025396615212,-16.9942281684826));
#44016=CARTESIAN_POINT('Ctrl Pts',(-4.16594229225302,5.33265541898383,-16.9860297255656));
#44017=CARTESIAN_POINT('Ctrl Pts',(-4.30367349954042,5.2250579433699,-16.9778313642954));
#44018=CARTESIAN_POINT('Ctrl Pts',(-4.43723740837643,5.11211803965734,-16.9696330030252));
#44019=CARTESIAN_POINT('Ctrl Pts',(-4.56620713172781,4.99420077992045,-16.9614346417549));
#44020=CARTESIAN_POINT('Ctrl Pts',(-4.69519899896738,4.87626327398511,-16.9532348728397));
#44021=CARTESIAN_POINT('Ctrl Pts',(-4.81959484443921,4.75334695145079,-16.9450351039244));
#44022=CARTESIAN_POINT('Ctrl Pts',(-4.93900360107153,4.62585477815749,-16.9368353350091));
#44023=CARTESIAN_POINT('Ctrl Pts',(-5.05845455167121,4.49831755456176,-16.9286326686448));
#44024=CARTESIAN_POINT('Ctrl Pts',(-5.17291465799895,4.36620152093371,-16.9204300022805));
#44025=CARTESIAN_POINT('Ctrl Pts',(-5.28203217332817,4.22994386723112,-16.9122273359162));
#44026=CARTESIAN_POINT('Ctrl Pts',(-5.39127361888083,4.09353145889158,-16.9040153533732));
#44027=CARTESIAN_POINT('Ctrl Pts',(-5.49516012661644,3.95296831338133,-16.8958033708302));
#44028=CARTESIAN_POINT('Ctrl Pts',(-5.59338184206356,3.8087226951924,-16.8875913882871));
#44029=CARTESIAN_POINT('Ctrl Pts',(-5.69166149000614,3.66439199898806,-16.8793745622058));
#44030=CARTESIAN_POINT('Ctrl Pts',(-5.78426949558031,3.51637480416475,-16.8711577361245));
#44031=CARTESIAN_POINT('Ctrl Pts',(-5.87094134858256,3.36516517893307,-16.8629409100432));
#44032=CARTESIAN_POINT('Ctrl Pts',(-5.95774686209968,3.2137223666209,-16.8547114124293));
#44033=CARTESIAN_POINT('Ctrl Pts',(-6.03859776317304,3.05907760323322,-16.8464819148154));
#44034=CARTESIAN_POINT('Ctrl Pts',(-6.11327662389944,2.90174739074315,-16.8382524172016));
#44035=CARTESIAN_POINT('Ctrl Pts',(-6.17984217838067,2.76150994296765,-16.8309169936769));
#44036=CARTESIAN_POINT('Ctrl Pts',(-6.24150455586689,2.61913929840205,-16.8235815701522));
#44037=CARTESIAN_POINT('Ctrl Pts',(-6.29814318430964,2.47501139996041,-16.8162461466275));
#44038=CARTESIAN_POINT('Ctrl Pts',(-6.36901475643026,2.29466503512352,-16.8070673756781));
#44039=CARTESIAN_POINT('Ctrl Pts',(-6.43221623805483,2.11106898827689,-16.7978886047287));
#44040=CARTESIAN_POINT('Ctrl Pts',(-6.48746710585673,1.92485312437777,-16.7887098337793));
#44041=CARTESIAN_POINT('Ctrl Pts',(-6.5424239752946,1.73962814372671,-16.7795799044817));
#44042=CARTESIAN_POINT('Ctrl Pts',(-6.58951450754699,1.55181133498299,-16.770449975184));
#44043=CARTESIAN_POINT('Ctrl Pts',(-6.6285078353735,1.36204731062915,-16.7613200458863));
#44044=CARTESIAN_POINT('Ctrl Pts',(-6.66736715134499,1.17293546525917,-16.7522214942327));
#44045=CARTESIAN_POINT('Ctrl Pts',(-6.69818470336403,0.981889947406345,
-16.7431229425791));
#44046=CARTESIAN_POINT('Ctrl Pts',(-6.72077875918299,0.789570687218579,
-16.7340243909255));
#44047=CARTESIAN_POINT('Ctrl Pts',(-6.74325216393855,0.598278401711175,
-16.7249744250566));
#44048=CARTESIAN_POINT('Ctrl Pts',(-6.75758956453549,0.405726136249686,
-16.7159244591878));
#44049=CARTESIAN_POINT('Ctrl Pts',(-6.76366008874744,0.212582228525706,
-16.7068744933189));
#44050=CARTESIAN_POINT('Ctrl Pts',(-6.7658277569075,0.143614230958435,-16.7036429234942));
#44051=CARTESIAN_POINT('Ctrl Pts',(-6.76694179617376,0.0745709569908315,
-16.7004113536695));
#44052=CARTESIAN_POINT('Ctrl Pts',(-6.76699777839932,0.00548335104101361,
-16.6971797838448));
#44053=CARTESIAN_POINT('Ctrl Pts',(-6.76699777839992,0.00548335030004697,
-16.6971797838101));
#44054=CARTESIAN_POINT('Ctrl Pts',(-6.76714103050534,-0.171303946887046,
-16.6889105655165));
#44055=CARTESIAN_POINT('Ctrl Pts',(-6.76035171325591,-0.348144388963959,
-16.680641347223));
#44056=CARTESIAN_POINT('Ctrl Pts',(-6.74664681532118,-0.524448042532959,
-16.6723721289294));
#44057=CARTESIAN_POINT('Ctrl Pts',(-6.7332601547828,-0.696657800915976,
-16.664294927717));
#44058=CARTESIAN_POINT('Ctrl Pts',(-6.71327559157909,-0.868355045356068,
-16.6562177265046));
#44059=CARTESIAN_POINT('Ctrl Pts',(-6.68676157954093,-1.03899402230006,
-16.6481405252923));
#44060=CARTESIAN_POINT('Ctrl Pts',(-6.66024189380405,-1.20966951405535,
-16.6400615956502));
#44061=CARTESIAN_POINT('Ctrl Pts',(-6.62719003316591,-1.37928592273975,
-16.6319826660081));
#44062=CARTESIAN_POINT('Ctrl Pts',(-6.58772579263647,-1.54730665384476,
-16.623903736366));
#44063=CARTESIAN_POINT('Ctrl Pts',(-6.54824546994387,-1.71539585546319,
-16.6158215144608));
#44064=CARTESIAN_POINT('Ctrl Pts',(-6.50234764835162,-1.88188772587341,
-16.6077392925556));
#44065=CARTESIAN_POINT('Ctrl Pts',(-6.45020227626436,-2.04625990413586,
-16.5996570706504));
#44066=CARTESIAN_POINT('Ctrl Pts',(-6.3959321649428,-2.21732966652132,-16.5912455268265));
#44067=CARTESIAN_POINT('Ctrl Pts',(-6.3348948134272,-2.3861029402516,-16.5828339830027));
#44068=CARTESIAN_POINT('Ctrl Pts',(-6.26733703151375,-2.55201401512931,
-16.5744224391789));
#44069=CARTESIAN_POINT('Ctrl Pts',(-6.20229412505351,-2.71174895932588,
-16.5663240196834));
#44070=CARTESIAN_POINT('Ctrl Pts',(-6.13120770860825,-2.86883066175132,
-16.5582256001879));
#44071=CARTESIAN_POINT('Ctrl Pts',(-6.05434470713789,-3.02278003949203,
-16.5501271806924));
#44072=CARTESIAN_POINT('Ctrl Pts',(-5.97741756226229,-3.17685789045306,
-16.5420220029362));
#44073=CARTESIAN_POINT('Ctrl Pts',(-5.89470440723982,-3.32779788958514,
-16.53391682518));
#44074=CARTESIAN_POINT('Ctrl Pts',(-5.80651557822335,-3.47514975790247,
-16.5258116474238));
#44075=CARTESIAN_POINT('Ctrl Pts',(-5.71819348913538,-3.62272428617259,
-16.5176942221236));
#44076=CARTESIAN_POINT('Ctrl Pts',(-5.62437941383026,-3.76669955783019,
-16.5095767968234));
#44077=CARTESIAN_POINT('Ctrl Pts',(-5.52542443370626,-3.90665762863882,
-16.5014593715231));
#44078=CARTESIAN_POINT('Ctrl Pts',(-5.51428713965884,-3.92240978367893,
-16.5005457626036));
#44079=CARTESIAN_POINT('Ctrl Pts',(-5.50308476279341,-3.93811108989045,
-16.499632153684));
#44080=CARTESIAN_POINT('Ctrl Pts',(-5.49181783252863,-3.95376098092949,
-16.4987185447644));
#44081=CARTESIAN_POINT('Ctrl Pts',(-5.38904210163831,-4.09651761047212,
-16.4903847020717));
#44082=CARTESIAN_POINT('Ctrl Pts',(-5.28056508301162,-4.23544695578761,
-16.482050859379));
#44083=CARTESIAN_POINT('Ctrl Pts',(-5.16669771029274,-4.37007136903458,
-16.4737170166864));
#44084=CARTESIAN_POINT('Ctrl Pts',(-5.05296454467821,-4.50453711037893,
-16.4653929964816));
#44085=CARTESIAN_POINT('Ctrl Pts',(-4.93385390387229,-4.63470776401472,
-16.4570689762769));
#44086=CARTESIAN_POINT('Ctrl Pts',(-4.80971948974867,-4.76013523231555,
-16.4487449560721));
#44087=CARTESIAN_POINT('Ctrl Pts',(-4.68570862387184,-4.88543786542126,
-16.4404292205813));
#44088=CARTESIAN_POINT('Ctrl Pts',(-4.55668418961337,-5.00600647287748,
-16.4321134850904));
#44089=CARTESIAN_POINT('Ctrl Pts',(-4.42303971879279,-5.12142642688357,
-16.4237977495995));
#44090=CARTESIAN_POINT('Ctrl Pts',(-4.28950377425102,-5.23675265386877,
-16.4154887669194));
#44091=CARTESIAN_POINT('Ctrl Pts',(-4.15135553090812,-5.34693833201893,
-16.4071797842394));
#44092=CARTESIAN_POINT('Ctrl Pts',(-4.00902505034459,-5.45160592355221,
-16.3988708015593));
#44093=CARTESIAN_POINT('Ctrl Pts',(-3.8667840852522,-5.55620768681925,-16.3905670446222));
#44094=CARTESIAN_POINT('Ctrl Pts',(-3.72036640432536,-5.6552980742625,-16.382263287685));
#44095=CARTESIAN_POINT('Ctrl Pts',(-3.57023496746212,-5.74853992567772,
-16.3739595307479));
#44096=CARTESIAN_POINT('Ctrl Pts',(-3.42016448034264,-5.84174392314928,
-16.3656591449359));
#44097=CARTESIAN_POINT('Ctrl Pts',(-3.26638353648927,-5.92910393248157,
-16.3573587591238));
#44098=CARTESIAN_POINT('Ctrl Pts',(-3.10938412450249,-6.01032606156204,
-16.3490583733118));
#44099=CARTESIAN_POINT('Ctrl Pts',(-2.95241781960651,-6.09153106300892,
-16.3407597378351));
#44100=CARTESIAN_POINT('Ctrl Pts',(-2.79223470741902,-6.1666006030878,-16.3324611023585));
#44101=CARTESIAN_POINT('Ctrl Pts',(-2.62935164042987,-6.23528659734007,
-16.3241624668819));
#44102=CARTESIAN_POINT('Ctrl Pts',(-2.46647588452209,-6.30396950858991,
-16.3158642038933));
#44103=CARTESIAN_POINT('Ctrl Pts',(-2.30090073581917,-6.36626931002763,
-16.3075659409047));
#44104=CARTESIAN_POINT('Ctrl Pts',(-2.13316347627594,-6.42198587537238,
-16.2992676779161));
#44105=CARTESIAN_POINT('Ctrl Pts',(-1.96540590446547,-6.47770918775573,
-16.2909684100433));
#44106=CARTESIAN_POINT('Ctrl Pts',(-1.79548603032544,-6.52684756647184,
-16.2826691421704));
#44107=CARTESIAN_POINT('Ctrl Pts',(-1.6239569433732,-6.56925055436843,-16.2743698742976));
#44108=CARTESIAN_POINT('Ctrl Pts',(-1.4523074153562,-6.61168331599671,-16.2660647790011));
#44109=CARTESIAN_POINT('Ctrl Pts',(-1.27904675476757,-6.64737115321012,
-16.2577596837045));
#44110=CARTESIAN_POINT('Ctrl Pts',(-1.10473979741864,-6.67621441986396,
-16.249454588408));
#44111=CARTESIAN_POINT('Ctrl Pts',(-0.930369278689102,-6.70506820427266,
-16.2411464646419));
#44112=CARTESIAN_POINT('Ctrl Pts',(-0.754952047023796,-6.72707239400851,
-16.2328383408758));
#44113=CARTESIAN_POINT('Ctrl Pts',(-0.579058973178254,-6.74217915110402,
-16.2245302171097));
#44114=CARTESIAN_POINT('Ctrl Pts',(-0.402978926011551,-6.75730196659504,
-16.216213261856));
#44115=CARTESIAN_POINT('Ctrl Pts',(-0.226422373365127,-6.7655126780107,
-16.2078963066023));
#44116=CARTESIAN_POINT('Ctrl Pts',(-0.0499622079141649,-6.76681555665443,
-16.1995793513486));
#44117=CARTESIAN_POINT('Ctrl Pts',(0.0800862492438838,-6.76777575839202,
-16.1934498818662));
#44118=CARTESIAN_POINT('Ctrl Pts',(0.210082326238034,-6.76498508378958,
-16.1873204123838));
#44119=CARTESIAN_POINT('Ctrl Pts',(0.33979830046276,-6.75846329538029,-16.1811909429014));
#44120=CARTESIAN_POINT('Ctrl Pts',(0.518644569769884,-6.74947136101613,
-16.1727399193762));
#44121=CARTESIAN_POINT('Ctrl Pts',(0.697285007755008,-6.73336840077228,
-16.1642888958511));
#44122=CARTESIAN_POINT('Ctrl Pts',(0.875131619415711,-6.71017389109246,
-16.1558378723259));
#44123=CARTESIAN_POINT('Ctrl Pts',(1.052821642421,-6.68699980348899,-16.1473942896758));
#44124=CARTESIAN_POINT('Ctrl Pts',(1.22971890504705,-6.65674665439173,-16.1389507070256));
#44125=CARTESIAN_POINT('Ctrl Pts',(1.40523881389734,-6.61948584679478,-16.1305071243755));
#44126=CARTESIAN_POINT('Ctrl Pts',(1.58062804270633,-6.58225278103012,-16.1220698282358));
#44127=CARTESIAN_POINT('Ctrl Pts',(1.75464163879023,-6.53802252605743,-16.113632532096));
#44128=CARTESIAN_POINT('Ctrl Pts',(1.92670311366764,-6.48691792084526,-16.1051952359562));
#44129=CARTESIAN_POINT('Ctrl Pts',(2.09864183580343,-6.43584977487188,-16.0967639591839));
#44130=CARTESIAN_POINT('Ctrl Pts',(2.26863089768929,-6.37791715530852,-16.0883326824115));
#44131=CARTESIAN_POINT('Ctrl Pts',(2.43610673024851,-6.313293355994,-16.0799014056392));
#44132=CARTESIAN_POINT('Ctrl Pts',(2.60351077660312,-6.24869725677929,-16.0714737428173));
#44133=CARTESIAN_POINT('Ctrl Pts',(2.76840343250652,-6.17741581457886,-16.0630460799954));
#44134=CARTESIAN_POINT('Ctrl Pts',(2.93023832454289,-6.09967149618568,-16.0546184171735));
#44135=CARTESIAN_POINT('Ctrl Pts',(3.09202339739928,-6.02195111056832,-16.0461933487195));
#44136=CARTESIAN_POINT('Ctrl Pts',(3.25075228513535,-5.93777195975516,-16.0377682802655));
#44137=CARTESIAN_POINT('Ctrl Pts',(3.40590022582786,-5.84740392411075,-16.0293432118115));
#44138=CARTESIAN_POINT('Ctrl Pts',(3.44835345136134,-5.82267646346186,-16.0270378551976));
#44139=CARTESIAN_POINT('Ctrl Pts',(3.49053869454235,-5.79748588630927,-16.0247324985836));
#44140=CARTESIAN_POINT('Ctrl Pts',(3.5324455254156,-5.77183832153772,-16.0224271419697));
#44141=CARTESIAN_POINT('Ctrl Pts',(3.68912171694834,-5.67595030789503,-16.0138081534452));
#44142=CARTESIAN_POINT('Ctrl Pts',(3.84183429062203,-5.57371406158912,-16.0051891649207));
#44143=CARTESIAN_POINT('Ctrl Pts',(3.99008070006634,-5.46548671272359,-15.9965701763962));
#44144=CARTESIAN_POINT('Ctrl Pts',(4.13841592234035,-5.35719452601719,-15.9879460243284));
#44145=CARTESIAN_POINT('Ctrl Pts',(4.28227939498782,-5.24290425313291,-15.9793218722606));
#44146=CARTESIAN_POINT('Ctrl Pts',(4.42120079106756,-5.12301401179653,-15.9706977201927));
#44147=CARTESIAN_POINT('Ctrl Pts',(4.56488028233511,-4.99901749744198,-15.9617781885965));
#44148=CARTESIAN_POINT('Ctrl Pts',(4.70327290272848,-4.8690308621258,-15.9528586570003));
#44149=CARTESIAN_POINT('Ctrl Pts',(4.83589934889496,-4.73353636168112,-15.9439391254041));
#44150=CARTESIAN_POINT('Ctrl Pts',(4.96437261864278,-4.60228485032625,-15.9352989075449));
#44151=CARTESIAN_POINT('Ctrl Pts',(5.08743521275111,-4.46586546642328,-15.9266586896856));
#44152=CARTESIAN_POINT('Ctrl Pts',(5.20469187431502,-4.32475103253809,-15.9180184718263));
#44153=CARTESIAN_POINT('Ctrl Pts',(5.32763439881402,-4.17679385455178,-15.9089592833616));
#44154=CARTESIAN_POINT('Ctrl Pts',(5.44419368924396,-4.0236752821493,-15.899900094897));
#44155=CARTESIAN_POINT('Ctrl Pts',(5.55396432346168,-3.86597585270716,-15.8908409064323));
#44156=CARTESIAN_POINT('Ctrl Pts',(5.66373495767941,-3.70827642326501,-15.8817817179677));
#44157=CARTESIAN_POINT('Ctrl Pts',(5.76671675863962,-3.5459964775991,-15.872722529503));
#44158=CARTESIAN_POINT('Ctrl Pts',(5.86255851577539,-3.37974801562327,-15.8636633410384));
#44159=CARTESIAN_POINT('Ctrl Pts',(5.95823423379154,-3.21378756744321,-15.8546198469821));
#44160=CARTESIAN_POINT('Ctrl Pts',(6.04688350104808,-3.04371987375538,-15.8455763529259));
#44161=CARTESIAN_POINT('Ctrl Pts',(6.12818261729637,-2.87013358732074,-15.8365328588696));
#44162=CARTESIAN_POINT('Ctrl Pts',(6.20940736954039,-2.69670607962739,-15.8274976368643));
#44163=CARTESIAN_POINT('Ctrl Pts',(6.28329529268741,-2.51976662024883,-15.818462414859));
#44164=CARTESIAN_POINT('Ctrl Pts',(6.34956934387557,-2.33992695341448,-15.8094271928536));
#44165=CARTESIAN_POINT('Ctrl Pts',(6.41572663461302,-2.16040412492303,-15.8004078889426));
#44166=CARTESIAN_POINT('Ctrl Pts',(6.47429675723077,-1.97799151519004,-15.7913885850315));
#44167=CARTESIAN_POINT('Ctrl Pts',(6.52505138820639,-1.79331909633114,-15.7823692811204));
#44168=CARTESIAN_POINT('Ctrl Pts',(6.57574234395251,-1.60887836192006,-15.7733612925561));
#44169=CARTESIAN_POINT('Ctrl Pts',(6.61863731271837,-1.42218370513725,-15.7643533039917));
#44170=CARTESIAN_POINT('Ctrl Pts',(6.65355746626208,-1.23388088693688,-15.7553453154273));
#44171=CARTESIAN_POINT('Ctrl Pts',(6.68839875141585,-1.04600335724721,-15.7463576717207));
#44172=CARTESIAN_POINT('Ctrl Pts',(6.71530113041781,-0.856525149786348,
-15.737370028014));
#44173=CARTESIAN_POINT('Ctrl Pts',(6.73413666365722,-0.666102390918678,
-15.7283823843074));
#44174=CARTESIAN_POINT('Ctrl Pts',(6.75054110761511,-0.500257366175054,
-15.7205547695738));
#44175=CARTESIAN_POINT('Ctrl Pts',(6.76082741180869,-0.333696197191793,
-15.7127271548403));
#44176=CARTESIAN_POINT('Ctrl Pts',(6.76494249303895,-0.166859419500229,
-15.7048995401067));
#44177=CARTESIAN_POINT('Ctrl Pts',(6.76921294553139,0.00627653900395247,
-15.6967763816614));
#44178=CARTESIAN_POINT('Ctrl Pts',(6.76683378790335,0.179631959079449,-15.688653223216));
#44179=CARTESIAN_POINT('Ctrl Pts',(6.75780468430653,0.35265400715816,-15.6805300647707));
#44180=CARTESIAN_POINT('Ctrl Pts',(6.74877621730882,0.52566385627594,-15.6724074790506));
#44181=CARTESIAN_POINT('Ctrl Pts',(6.73309875733268,0.698340014688396,-15.6642848933305));
#44182=CARTESIAN_POINT('Ctrl Pts',(6.71082403943189,0.870132008251117,-15.6561623076104));
#44183=CARTESIAN_POINT('Ctrl Pts',(6.68854664499442,1.04194464439049,-15.648038745878));
#44184=CARTESIAN_POINT('Ctrl Pts',(6.65967046237651,1.21287254130438,-15.6399151841456));
#44185=CARTESIAN_POINT('Ctrl Pts',(6.62429880290322,1.38237273188348,-15.6317916224132));
#44186=CARTESIAN_POINT('Ctrl Pts',(6.5889013793734,1.55199638323761,-15.6236621436301));
#44187=CARTESIAN_POINT('Ctrl Pts',(6.546999104418,1.72018989260391,-15.615532664847));
#44188=CARTESIAN_POINT('Ctrl Pts',(6.49874605224474,1.8864222084235,-15.6074031860638));
#44189=CARTESIAN_POINT('Ctrl Pts',(6.45047332815091,2.05272229423413,-15.5992703930352));
#44190=CARTESIAN_POINT('Ctrl Pts',(6.39584478137198,2.21705924567967,-15.5911376000066));
#44191=CARTESIAN_POINT('Ctrl Pts',(6.33506354006774,2.37891970089458,-15.583004806978));
#44192=CARTESIAN_POINT('Ctrl Pts',(6.27421620838508,2.54095615479771,-15.5748631707708));
#44193=CARTESIAN_POINT('Ctrl Pts',(6.2072029614369,2.70051039701334,-15.5667215345636));
#44194=CARTESIAN_POINT('Ctrl Pts',(6.13427430235387,2.85709079020618,-15.5585798983564));
#44195=CARTESIAN_POINT('Ctrl Pts',(6.09711814113509,2.93686637371924,-15.5544318452961));
#44196=CARTESIAN_POINT('Ctrl Pts',(6.05842721108827,3.01587042163798,-15.5502837922357));
#44197=CARTESIAN_POINT('Ctrl Pts',(6.01823906458994,3.09404065284275,-15.5461357391753));
#44198=CARTESIAN_POINT('Ctrl Pts',(5.93646814879128,3.25309380534565,-15.5376956858989));
#44199=CARTESIAN_POINT('Ctrl Pts',(5.84832765968676,3.40902085888638,-15.5292556326224));
#44200=CARTESIAN_POINT('Ctrl Pts',(5.75408102651073,3.56129759221962,-15.5208155793459));
#44201=CARTESIAN_POINT('Ctrl Pts',(5.65990187834529,3.71346528826827,-15.5123815695435));
#44202=CARTESIAN_POINT('Ctrl Pts',(5.55962547525091,3.86198759124696,-15.5039475597412));
#44203=CARTESIAN_POINT('Ctrl Pts',(5.45356093673978,4.00636519918816,-15.4955135499388));
#44204=CARTESIAN_POINT('Ctrl Pts',(5.3475575192247,4.15065960775537,-15.4870844003384));
#44205=CARTESIAN_POINT('Ctrl Pts',(5.23577281199732,4.29081381430065,-15.4786552507379));
#44206=CARTESIAN_POINT('Ctrl Pts',(5.11855918845502,4.42635751315714,-15.4702261011375));
#44207=CARTESIAN_POINT('Ctrl Pts',(5.0013967416352,4.5618420321841,-15.4618006317941));
#44208=CARTESIAN_POINT('Ctrl Pts',(4.87881032196602,4.69271980509314,-15.4533751624506));
#44209=CARTESIAN_POINT('Ctrl Pts',(4.75119275114153,4.81855335567639,-15.4449496931071));
#44210=CARTESIAN_POINT('Ctrl Pts',(4.62360288746935,4.94435958643739,-15.436526053024));
#44211=CARTESIAN_POINT('Ctrl Pts',(4.49098428562376,5.06512354239626,-15.4281024129408));
#44212=CARTESIAN_POINT('Ctrl Pts',(4.35376717008197,5.1804440377941,-15.4196787728577));
#44213=CARTESIAN_POINT('Ctrl Pts',(4.21657229000281,5.29574584598549,-15.4112564977904));
#44214=CARTESIAN_POINT('Ctrl Pts',(4.074780638481,5.40560573954111,-15.4028342227231));
#44215=CARTESIAN_POINT('Ctrl Pts',(3.92885627539957,5.50966218267993,-15.3944119476558));
#44216=CARTESIAN_POINT('Ctrl Pts',(3.78290470038821,5.61373803023197,-15.3859881020053));
#44217=CARTESIAN_POINT('Ctrl Pts',(3.63281914390815,5.71200806910145,-15.3775642563547));
#44218=CARTESIAN_POINT('Ctrl Pts',(3.4790940583063,5.80415312801599,-15.3691404107042));
#44219=CARTESIAN_POINT('Ctrl Pts',(3.3547150239598,5.8787077356958,-15.3623246734847));
#44220=CARTESIAN_POINT('Ctrl Pts',(3.22795402870168,5.94925343469849,-15.3555089362653));
#44221=CARTESIAN_POINT('Ctrl Pts',(3.09908550384719,6.01564277861013,-15.3486931990458));
#44222=CARTESIAN_POINT('Origin',(0.,0.,-63.6971797838103));
#44223=CARTESIAN_POINT('',(3.09908550384713,6.01564277861016,-12.9539582652632));
#44224=CARTESIAN_POINT('',(3.09908550384717,6.01564277861014,-13.3487674371071));
#44225=CARTESIAN_POINT('',(3.09908550384721,6.01564277861012,-63.6971797838103));
#44226=CARTESIAN_POINT('',(-6.76699997822088,-0.000542916823992785,-14.302820216237));
#44227=CARTESIAN_POINT('Ctrl Pts',(-6.7669999782208,-0.000542917819759636,
-14.30282021619));
#44228=CARTESIAN_POINT('Ctrl Pts',(-6.76699920699295,-0.010155604417516,
-14.3023664227766));
#44229=CARTESIAN_POINT('Ctrl Pts',(-6.7669779531837,-0.0197681796252492,
-14.3019126293633));
#44230=CARTESIAN_POINT('Ctrl Pts',(-6.76693621826583,-0.0293805704865878,
-14.3014588359501));
#44231=CARTESIAN_POINT('Ctrl Pts',(-6.7661044973316,-0.220942627319672,
-14.2924153418939));
#44232=CARTESIAN_POINT('Ctrl Pts',(-6.75713396258636,-0.412518310869544,
-14.2833718478376));
#44233=CARTESIAN_POINT('Ctrl Pts',(-6.7400410938386,-0.603436039168142,
-14.2743283537814));
#44234=CARTESIAN_POINT('Ctrl Pts',(-6.72296385987539,-0.794179135718705,
-14.2652931317761));
#44235=CARTESIAN_POINT('Ctrl Pts',(-6.69777914608514,-0.984265241636963,
-14.2562579097708));
#44236=CARTESIAN_POINT('Ctrl Pts',(-6.66455537180709,-1.17302629813539,
-14.2472226877655));
#44237=CARTESIAN_POINT('Ctrl Pts',(-6.63139013058659,-1.3614547987451,-14.2382033838545));
#44238=CARTESIAN_POINT('Ctrl Pts',(-6.59021415199377,-1.54856267736042,
-14.2291840799434));
#44239=CARTESIAN_POINT('Ctrl Pts',(-6.54114712940774,-1.73369063890906,
-14.2201647760324));
#44240=CARTESIAN_POINT('Ctrl Pts',(-6.49214166482879,-1.91858634449908,
-14.211156787468));
#44241=CARTESIAN_POINT('Ctrl Pts',(-6.43526497380221,-2.10150686066446,
-14.2021487989037));
#44242=CARTESIAN_POINT('Ctrl Pts',(-6.37068746695663,-2.28180415425202,
-14.1931408103394));
#44243=CARTESIAN_POINT('Ctrl Pts',(-6.30625581067216,-2.46169424008687,
-14.1841531666328));
#44244=CARTESIAN_POINT('Ctrl Pts',(-6.23415813584952,-2.63897270573763,
-14.1751655229261));
#44245=CARTESIAN_POINT('Ctrl Pts',(-6.15461404537522,-2.81300816786409,
-14.1661778792195));
#44246=CARTESIAN_POINT('Ctrl Pts',(-6.08533665578346,-2.9645809929555,-14.1583502644858));
#44247=CARTESIAN_POINT('Ctrl Pts',(-6.01041179618313,-3.11369402552463,
-14.1505226497521));
#44248=CARTESIAN_POINT('Ctrl Pts',(-5.93001527222477,-3.25993985698832,
-14.1426950350184));
#44249=CARTESIAN_POINT('Ctrl Pts',(-5.84658325304866,-3.41170742621089,
-14.1345718765731));
#44250=CARTESIAN_POINT('Ctrl Pts',(-5.75729441569808,-3.56031854822074,
-14.1264487181278));
#44251=CARTESIAN_POINT('Ctrl Pts',(-5.66242665705949,-3.7052953125793,-14.1183255596825));
#44252=CARTESIAN_POINT('Ctrl Pts',(-5.56756558709448,-3.85026185531706,
-14.1102029739623));
#44253=CARTESIAN_POINT('Ctrl Pts',(-5.46712657976063,-3.99159424453248,
-14.1020803882422));
#44254=CARTESIAN_POINT('Ctrl Pts',(-5.36143134271823,-4.12884281092398,
-14.0939578025221));
#44255=CARTESIAN_POINT('Ctrl Pts',(-5.25572340530491,-4.26610786914378,
-14.0858342407897));
#44256=CARTESIAN_POINT('Ctrl Pts',(-5.14475820481112,-4.39928783815394,
-14.0777106790573));
#44257=CARTESIAN_POINT('Ctrl Pts',(-5.02889824193671,-4.52796548929493,
-14.0695871173249));
#44258=CARTESIAN_POINT('Ctrl Pts',(-4.91295388882835,-4.65673686683472,
-14.0614576385417));
#44259=CARTESIAN_POINT('Ctrl Pts',(-4.7921078977559,-4.78099910438522,-14.0533281597586));
#44260=CARTESIAN_POINT('Ctrl Pts',(-4.66676064117878,-4.90037081433075,
-14.0451986809755));
#44261=CARTESIAN_POINT('Ctrl Pts',(-4.54136228273138,-5.01979119002137,
-14.0370658879469));
#44262=CARTESIAN_POINT('Ctrl Pts',(-4.41145927526905,-5.13431682202207,
-14.0289330949184));
#44263=CARTESIAN_POINT('Ctrl Pts',(-4.27748548064466,-5.24360629365651,
-14.0208003018899));
#44264=CARTESIAN_POINT('Ctrl Pts',(-4.14336600984325,-5.35301460101147,
-14.0126586656827));
#44265=CARTESIAN_POINT('Ctrl Pts',(-4.00516720296143,-5.45717515617468,
-14.0045170294756));
#44266=CARTESIAN_POINT('Ctrl Pts',(-3.86335292998348,-5.55578915532151,
-13.9963753932684));
#44267=CARTESIAN_POINT('Ctrl Pts',(-3.79110048415139,-5.60603164842198,
-13.9922273402079));
#44268=CARTESIAN_POINT('Ctrl Pts',(-3.71790997768687,-5.65483510546349,
-13.9880792871475));
#44269=CARTESIAN_POINT('Ctrl Pts',(-3.64384520217837,-5.70216460149667,
-13.983931234087));
#44270=CARTESIAN_POINT('Ctrl Pts',(-3.49313361511055,-5.79847358796571,
-13.9754905191089));
#44271=CARTESIAN_POINT('Ctrl Pts',(-3.33849008577207,-5.88887498709142,
-13.9670498041309));
#44272=CARTESIAN_POINT('Ctrl Pts',(-3.18040616753894,-5.97304826780098,
-13.9586090891528));
#44273=CARTESIAN_POINT('Ctrl Pts',(-3.02244173657929,-6.05715792637918,
-13.9501747540648));
#44274=CARTESIAN_POINT('Ctrl Pts',(-2.86104239372446,-6.13504869453032,
-13.9417404189767));
#44275=CARTESIAN_POINT('Ctrl Pts',(-2.69672658276436,-6.20644461328804,
-13.9333060838887));
#44276=CARTESIAN_POINT('Ctrl Pts',(-2.53250973686716,-6.27779753130499,
-13.9248768286801));
#44277=CARTESIAN_POINT('Ctrl Pts',(-2.36538022983778,-6.34266326606286,
-13.9164475734715));
#44278=CARTESIAN_POINT('Ctrl Pts',(-2.19587925359299,-6.40081270649594,
-13.9080183182628));
#44279=CARTESIAN_POINT('Ctrl Pts',(-2.02645436518907,-6.45893604403883,
-13.8995928468898));
#44280=CARTESIAN_POINT('Ctrl Pts',(-1.85466044499256,-6.51034899063576,
-13.8911673755168));
#44281=CARTESIAN_POINT('Ctrl Pts',(-1.68105709881265,-6.55487116811091,
-13.8827419041438));
#44282=CARTESIAN_POINT('Ctrl Pts',(-1.50750507481849,-6.5993801835387,-13.8743189235846));
#44283=CARTESIAN_POINT('Ctrl Pts',(-1.33214501420962,-6.63700240957085,
-13.8658959430253));
#44284=CARTESIAN_POINT('Ctrl Pts',(-1.15555044746035,-6.66760767917356,
-13.8574729624661));
#44285=CARTESIAN_POINT('Ctrl Pts',(-0.978952956671259,-6.69821345553606,
-13.8490498424398));
#44286=CARTESIAN_POINT('Ctrl Pts',(-0.801121246206729,-6.72180197989719,
-13.8406267224134));
#44287=CARTESIAN_POINT('Ctrl Pts',(-0.622638443870925,-6.73829432187508,
-13.8322036023871));
#44288=CARTESIAN_POINT('Ctrl Pts',(-0.444149469302229,-6.75478723418566,
-13.8237801910752));
#44289=CARTESIAN_POINT('Ctrl Pts',(-0.26500969004412,-6.76418344396783,
-13.8153567797634));
#44290=CARTESIAN_POINT('Ctrl Pts',(-0.0858069133771682,-6.76645595371881,
-13.8069333684515));
#44291=CARTESIAN_POINT('Ctrl Pts',(0.0934270528844234,-6.76872885899189,
-13.7985084910754));
#44292=CARTESIAN_POINT('Ctrl Pts',(0.272723704955782,-6.76387558810306,
-13.7900836136993));
#44293=CARTESIAN_POINT('Ctrl Pts',(0.451495305415063,-6.75192128132343,
-13.7816587363232));
#44294=CARTESIAN_POINT('Ctrl Pts',(0.630322960452874,-6.7399632262212,-13.7732312172917));
#44295=CARTESIAN_POINT('Ctrl Pts',(0.808624903030451,-6.72089971831177,
-13.7648036982603));
#44296=CARTESIAN_POINT('Ctrl Pts',(0.985818212988376,-6.6948077979088,-13.7563761792288));
#44297=CARTESIAN_POINT('Ctrl Pts',(1.1631704230581,-6.66869247928007,-13.7479411027241));
#44298=CARTESIAN_POINT('Ctrl Pts',(1.33941168375111,-6.63553620287084,-13.7395060262193));
#44299=CARTESIAN_POINT('Ctrl Pts',(1.51396783584278,-6.59546741270348,-13.7310709497145));
#44300=CARTESIAN_POINT('Ctrl Pts',(1.68860835207155,-6.55537925702613,-13.7226317964817));
#44301=CARTESIAN_POINT('Ctrl Pts',(1.86156181245422,-6.50837200707619,-13.714192643249));
#44302=CARTESIAN_POINT('Ctrl Pts',(2.03226840845491,-6.45462424281973,-13.7057534900162));
#44303=CARTESIAN_POINT('Ctrl Pts',(2.20316470734511,-6.40081674972782,-13.6973049585181));
#44304=CARTESIAN_POINT('Ctrl Pts',(2.37180883712501,-6.34025388296169,-13.68885642702));
#44305=CARTESIAN_POINT('Ctrl Pts',(2.53765904186203,-6.27316312455335,-13.6804078955219));
#44306=CARTESIAN_POINT('Ctrl Pts',(2.62929666100186,-6.23609330376793,-13.6757398077559));
#44307=CARTESIAN_POINT('Ctrl Pts',(2.72008169611202,-6.19703141223764,-13.6710717199899));
#44308=CARTESIAN_POINT('Ctrl Pts',(2.80992587884462,-6.15602189367447,-13.666403632224));
#44309=CARTESIAN_POINT('Ctrl Pts',(2.96853166898681,-6.08362603122422,-13.6581628566272));
#44310=CARTESIAN_POINT('Ctrl Pts',(3.12455680518312,-6.00499674285417,-13.6499220810305));
#44311=CARTESIAN_POINT('Ctrl Pts',(3.27747918214943,-5.92033945062081,-13.6416813054337));
#44312=CARTESIAN_POINT('Ctrl Pts',(3.43023218100444,-5.83577592551657,-13.6334496573893));
#44313=CARTESIAN_POINT('Ctrl Pts',(3.57988895507602,-5.74519786181873,-13.625218009345));
#44314=CARTESIAN_POINT('Ctrl Pts',(3.72594765005738,-5.64885856691703,-13.6169863613006));
#44315=CARTESIAN_POINT('Ctrl Pts',(3.87187059822284,-5.55260880966682,-13.6087623637423));
#44316=CARTESIAN_POINT('Ctrl Pts',(4.01420183182877,-5.4506086795835,-13.600538366184));
#44317=CARTESIAN_POINT('Ctrl Pts',(4.15246430348639,-5.34315723222434,-13.5923143686257));
#44318=CARTESIAN_POINT('Ctrl Pts',(4.29060461971304,-5.23580071863646,-13.5840976370012));
#44319=CARTESIAN_POINT('Ctrl Pts',(4.42468305888894,-5.12300270457643,-13.5758809053767));
#44320=CARTESIAN_POINT('Ctrl Pts',(4.55425187874156,-5.00510527611348,-13.5676641737522));
#44321=CARTESIAN_POINT('Ctrl Pts',(4.68375431569098,-4.88726825086783,-13.5594516518635));
#44322=CARTESIAN_POINT('Ctrl Pts',(4.80875147230765,-4.76433725338367,-13.5512391299748));
#44323=CARTESIAN_POINT('Ctrl Pts',(4.92882868868712,-4.63669459395104,-13.5430266080861));
#44324=CARTESIAN_POINT('Ctrl Pts',(5.04886575066748,-4.50909461883809,-13.5348168325042));
#44325=CARTESIAN_POINT('Ctrl Pts',(5.16398590643266,-4.37678637942024,-13.5266070569224));
#44326=CARTESIAN_POINT('Ctrl Pts',(5.27381132078866,-4.24018904681399,-13.5183972813405));
#44327=CARTESIAN_POINT('Ctrl Pts',(5.32178020849591,-4.18052688075415,-13.5148114646578));
#44328=CARTESIAN_POINT('Ctrl Pts',(5.36873950156936,-4.12004693476471,-13.511225647975));
#44329=CARTESIAN_POINT('Ctrl Pts',(5.41466008086364,-4.0587861743016,-13.5076398312923));
#44330=CARTESIAN_POINT('Ctrl Pts',(5.52810632655735,-3.90744219324369,-13.4987811137705));
#44331=CARTESIAN_POINT('Ctrl Pts',(5.63509275972133,-3.75148749632004,-13.4899223962488));
#44332=CARTESIAN_POINT('Ctrl Pts',(5.73528769752079,-3.59148493337598,-13.481063678727));
#44333=CARTESIAN_POINT('Ctrl Pts',(5.83567008395668,-3.4311830313345,-13.4721883879676));
#44334=CARTESIAN_POINT('Ctrl Pts',(5.92923544571463,-3.26681834914082,-13.4633130972081));
#44335=CARTESIAN_POINT('Ctrl Pts',(6.01569805499498,-3.09897820436505,-13.4544378064486));
#44336=CARTESIAN_POINT('Ctrl Pts',(6.10240623752637,-2.93066135584009,-13.4455373078679));
#44337=CARTESIAN_POINT('Ctrl Pts',(6.18197117859569,-2.75884952345563,-13.4366368092871));
#44338=CARTESIAN_POINT('Ctrl Pts',(6.25415411332366,-2.58415272899973,-13.4277363107063));
#44339=CARTESIAN_POINT('Ctrl Pts',(6.32643476218699,-2.40921944725936,-13.4188237635087));
#44340=CARTESIAN_POINT('Ctrl Pts',(6.39131335007299,-2.231393644381,-13.4099112163111));
#44341=CARTESIAN_POINT('Ctrl Pts',(6.44860064292124,-2.05130172039996,-13.4009986691135));
#44342=CARTESIAN_POINT('Ctrl Pts',(6.50601443170702,-1.87081213586222,-13.3920664421412));
#44343=CARTESIAN_POINT('Ctrl Pts',(6.55580331910349,-1.68804666991308,-13.3831342151689));
#44344=CARTESIAN_POINT('Ctrl Pts',(6.59782826630241,-1.50364595845598,-13.3742019881967));
#44345=CARTESIAN_POINT('Ctrl Pts',(6.63754669427166,-1.32936599230108,-13.3657600022514));
#44346=CARTESIAN_POINT('Ctrl Pts',(6.67033043952174,-1.15362561833584,-13.3573180163062));
#44347=CARTESIAN_POINT('Ctrl Pts',(6.69610462071256,-0.97697078179025,-13.3488760303609));
#44348=CARTESIAN_POINT('Ctrl Pts',(6.72121319209869,-0.804877998657023,
-13.3406520559434));
#44349=CARTESIAN_POINT('Ctrl Pts',(6.73971650077403,-0.631588486119616,
-13.3324280815258));
#44350=CARTESIAN_POINT('Ctrl Pts',(6.75150688791752,-0.457650240251565,
-13.3242041071083));
#44351=CARTESIAN_POINT('Ctrl Pts',(6.76328482326822,-0.283895690047411,
-13.3159888180056));
#44352=CARTESIAN_POINT('Ctrl Pts',(6.76836393060619,-0.109494125641494,
-13.3077735289029));
#44353=CARTESIAN_POINT('Ctrl Pts',(6.76668783666093,0.0649978552340806,
-13.2995582398003));
#44354=CARTESIAN_POINT('Ctrl Pts',(6.76501317664478,0.239340555020245,-13.2913499790281));
#44355=CARTESIAN_POINT('Ctrl Pts',(6.75659482862921,0.413773160664588,-13.2831417182559));
#44356=CARTESIAN_POINT('Ctrl Pts',(6.74142833678462,0.587735467704081,-13.2749334574838));
#44357=CARTESIAN_POINT('Ctrl Pts',(6.7262717789432,0.761583829994425,-13.2667305730959));
#44358=CARTESIAN_POINT('Ctrl Pts',(6.70437591250843,0.934962151308051,-13.258527688708));
#44359=CARTESIAN_POINT('Ctrl Pts',(6.67578833555443,1.1073116539057,-13.2503248043201));
#44360=CARTESIAN_POINT('Ctrl Pts',(6.64721375211669,1.27958282086594,-13.2421256482759));
#44361=CARTESIAN_POINT('Ctrl Pts',(6.61195357615987,1.45082574768838,-13.2339264922317));
#44362=CARTESIAN_POINT('Ctrl Pts',(6.57010709944948,1.62048810602347,-13.2257273361875));
#44363=CARTESIAN_POINT('Ctrl Pts',(6.52826426236501,1.79013570785894,-13.2175288932705));
#44364=CARTESIAN_POINT('Ctrl Pts',(6.47983634307929,1.9582026650894,-13.2093304503535));
#44365=CARTESIAN_POINT('Ctrl Pts',(6.42497355327282,2.12414779140833,-13.2011320074365));
#44366=CARTESIAN_POINT('Ctrl Pts',(6.37011130983481,2.29009126511018,-13.1929336461663));
#44367=CARTESIAN_POINT('Ctrl Pts',(6.30881443510904,2.4539126090888,-13.184735284896));
#44368=CARTESIAN_POINT('Ctrl Pts',(6.24128270340019,2.61508684678685,-13.1765369236258));
#44369=CARTESIAN_POINT('Ctrl Pts',(6.17373937660476,2.77628875783481,-13.1683371547105));
#44370=CARTESIAN_POINT('Ctrl Pts',(6.09995919866833,2.93484232625759,-13.1601373857953));
#44371=CARTESIAN_POINT('Ctrl Pts',(6.02018969564446,3.09024352251669,-13.15193761688));
#44372=CARTESIAN_POINT('Ctrl Pts',(5.94039200547652,3.2456996309382,-13.1437349505157));
#44373=CARTESIAN_POINT('Ctrl Pts',(5.8546009380752,3.39800082934557,-13.1355322841514));
#44374=CARTESIAN_POINT('Ctrl Pts',(5.76310949658806,3.54666856787275,-13.1273296177871));
#44375=CARTESIAN_POINT('Ctrl Pts',(5.67151414369185,3.69550515579111,-13.1191176352441));
#44376=CARTESIAN_POINT('Ctrl Pts',(5.57420567071083,3.8406997336901,-13.1109056527011));
#44377=CARTESIAN_POINT('Ctrl Pts',(5.47152045981557,3.98180271457786,-13.1026936701581));
#44378=CARTESIAN_POINT('Ctrl Pts',(5.36877468379513,4.12298891991076,-13.0944768440768));
#44379=CARTESIAN_POINT('Ctrl Pts',(5.26064607014841,4.26007843654286,-13.0862600179955));
#44380=CARTESIAN_POINT('Ctrl Pts',(5.14751058168329,4.39265566729952,-13.0780431919142));
#44381=CARTESIAN_POINT('Ctrl Pts',(5.03420062195521,4.52543735129366,-13.0698136943003));
#44382=CARTESIAN_POINT('Ctrl Pts',(4.91586860047096,4.6536925801889,-13.0615841966865));
#44383=CARTESIAN_POINT('Ctrl Pts',(4.79292747399547,4.77704251907176,-13.0533546990726));
#44384=CARTESIAN_POINT('Ctrl Pts',(4.68334299221497,4.88699139881323,-13.0460192755477));
#44385=CARTESIAN_POINT('Ctrl Pts',(4.57009711768723,4.99304337255841,-13.0386838520228));
#44386=CARTESIAN_POINT('Ctrl Pts',(4.45350313218971,5.0949581795709,-13.0313484284979));
#44387=CARTESIAN_POINT('Ctrl Pts',(4.32521708721857,5.2070930161994,-13.0232774077829));
#44388=CARTESIAN_POINT('Ctrl Pts',(4.19245880451748,5.31458421796954,-13.0152063870678));
#44389=CARTESIAN_POINT('Ctrl Pts',(4.05560399409322,5.41704395801761,-13.0071353663528));
#44390=CARTESIAN_POINT('Ctrl Pts',(3.91889938514553,5.51939124601379,-12.9990732037789));
#44391=CARTESIAN_POINT('Ctrl Pts',(3.77810748377986,5.6167178323874,-12.991011041205));
#44392=CARTESIAN_POINT('Ctrl Pts',(3.63364066539739,5.7086727454611,-12.9829488786311));
#44393=CARTESIAN_POINT('Ctrl Pts',(3.48933819013631,5.80052305210954,-12.9748958874433));
#44394=CARTESIAN_POINT('Ctrl Pts',(3.34136943327677,5.88701365279755,-12.9668428962555));
#44395=CARTESIAN_POINT('Ctrl Pts',(3.19017924681859,5.96783422802343,-12.9587899050677));
#44396=CARTESIAN_POINT('Ctrl Pts',(3.15994217896421,5.98399782484398,-12.9571793584662));
#44397=CARTESIAN_POINT('Ctrl Pts',(3.12957636278804,5.99993476827424,-12.9555688118647));
#44398=CARTESIAN_POINT('Ctrl Pts',(3.09908550384713,6.01564277861016,-12.9539582652632));
#44399=CARTESIAN_POINT('Ctrl Pts',(3.09908550384716,6.01564277861015,-14.9545069759344));
#44400=CARTESIAN_POINT('Ctrl Pts',(2.98625823505507,6.07376813046706,-14.948509330515));
#44401=CARTESIAN_POINT('Ctrl Pts',(2.87193152134139,6.12864783471719,-14.9425116850955));
#44402=CARTESIAN_POINT('Ctrl Pts',(2.75631524042156,6.18021158985838,-14.936514039676));
#44403=CARTESIAN_POINT('Ctrl Pts',(2.59566421314202,6.25186041100985,-14.9281801969833));
#44404=CARTESIAN_POINT('Ctrl Pts',(2.43201220990593,6.31733291208247,-14.9198463542906));
#44405=CARTESIAN_POINT('Ctrl Pts',(2.26586828330762,6.37637278730632,-14.9115125115979));
#44406=CARTESIAN_POINT('Ctrl Pts',(2.09992017834578,6.43534307656805,-14.9031884913932));
#44407=CARTESIAN_POINT('Ctrl Pts',(1.93148632585958,6.48789572786059,-14.8948644711884));
#44408=CARTESIAN_POINT('Ctrl Pts',(1.76109786767077,6.53382149285435,-14.8865404509837));
#44409=CARTESIAN_POINT('Ctrl Pts',(1.59087899336004,6.57970154894615,-14.8782247154928));
#44410=CARTESIAN_POINT('Ctrl Pts',(1.41870972295788,6.61896776939942,-14.8699089800019));
#44411=CARTESIAN_POINT('Ctrl Pts',(1.24513877598369,6.65145987197862,-14.8615932445111));
#44412=CARTESIAN_POINT('Ctrl Pts',(1.07170877766893,6.6839255892763,-14.8532842618311));
#44413=CARTESIAN_POINT('Ctrl Pts',(0.89687971125176,6.70962808611324,-14.844975279151));
#44414=CARTESIAN_POINT('Ctrl Pts',(0.721213200343631,6.72845751414469,-14.836666296471));
#44415=CARTESIAN_POINT('Ctrl Pts',(0.545657170832591,6.74727509984202,-14.8283625395338));
#44416=CARTESIAN_POINT('Ctrl Pts',(0.369265091352969,6.75922819436496,-14.8200587825967));
#44417=CARTESIAN_POINT('Ctrl Pts',(0.192606697121493,6.76425839691418,-14.8117550256595));
#44418=CARTESIAN_POINT('Ctrl Pts',(0.0160200219395562,6.76928655732242,
-14.8034546398475));
#44419=CARTESIAN_POINT('Ctrl Pts',(-0.160832405434871,6.76739741606613,
-14.7951542540354));
#44420=CARTESIAN_POINT('Ctrl Pts',(-0.33737753669317,6.75858457058391,-14.7868538682234));
#44421=CARTESIAN_POINT('Ctrl Pts',(-0.513885439177,6.74977358350149,-14.7785552327468));
#44422=CARTESIAN_POINT('Ctrl Pts',(-0.690085827485077,6.73404181825613,
-14.7702565972701));
#44423=CARTESIAN_POINT('Ctrl Pts',(-0.865407217231237,6.71143496939098,
-14.7619579617935));
#44424=CARTESIAN_POINT('Ctrl Pts',(-1.04072073759645,6.6888291352446,-14.7536596988049));
#44425=CARTESIAN_POINT('Ctrl Pts',(-1.21515499313482,6.65934887707142,-14.7453614358164));
#44426=CARTESIAN_POINT('Ctrl Pts',(-1.38814497762178,6.62309161352185,-14.7370631728278));
#44427=CARTESIAN_POINT('Ctrl Pts',(-1.56115591045733,6.58682995937245,-14.728763904955));
#44428=CARTESIAN_POINT('Ctrl Pts',(-1.73272188349723,6.54378973649846,-14.7204646370822));
#44429=CARTESIAN_POINT('Ctrl Pts',(-1.90228922373603,6.49411924045577,-14.7121653692094));
#44430=CARTESIAN_POINT('Ctrl Pts',(-2.07197562757813,6.44441386771908,-14.7038602739129));
#44431=CARTESIAN_POINT('Ctrl Pts',(-2.23966026028805,6.38806901715204,-14.6955551786164));
#44432=CARTESIAN_POINT('Ctrl Pts',(-2.40480486629651,6.32528280435244,-14.6872500833199));
#44433=CARTESIAN_POINT('Ctrl Pts',(-2.57000969261578,6.26247369643479,-14.6789419595538));
#44434=CARTESIAN_POINT('Ctrl Pts',(-2.73267232373408,6.19321867518292,-14.6706338357877));
#44435=CARTESIAN_POINT('Ctrl Pts',(-2.89227535886588,6.11776366399498,-14.6623257120216));
#44436=CARTESIAN_POINT('Ctrl Pts',(-3.05204805110204,6.04222844456603,-14.6540087567679));
#44437=CARTESIAN_POINT('Ctrl Pts',(-3.20875433785463,5.96048022283296,-14.6456918015142));
#44438=CARTESIAN_POINT('Ctrl Pts',(-3.36190129256284,5.87281097082686,-14.6373748462605));
#44439=CARTESIAN_POINT('Ctrl Pts',(-3.47476826810658,5.80820006595472,-14.6312453767781));
#44440=CARTESIAN_POINT('Ctrl Pts',(-3.58570252880072,5.74037412915269,-14.6251159072956));
#44441=CARTESIAN_POINT('Ctrl Pts',(-3.69451722846025,5.66946482911839,-14.6189864378132));
#44442=CARTESIAN_POINT('Ctrl Pts',(-3.84454580586621,5.57169842952086,-14.610535414288));
#44443=CARTESIAN_POINT('Ctrl Pts',(-3.99081822580794,5.46789047907122,-14.6020843907628));
#44444=CARTESIAN_POINT('Ctrl Pts',(-4.13283616202823,5.35835368913175,-14.5936333672377));
#44445=CARTESIAN_POINT('Ctrl Pts',(-4.27472905567653,5.24891334308032,-14.5851897845876));
#44446=CARTESIAN_POINT('Ctrl Pts',(-4.41237467072089,5.13375441284117,-14.5767462019374));
#44447=CARTESIAN_POINT('Ctrl Pts',(-4.54530375002421,5.01323277137776,-14.5683026192873));
#44448=CARTESIAN_POINT('Ctrl Pts',(-4.67813385948723,4.89280086203067,-14.5598653231475));
#44449=CARTESIAN_POINT('Ctrl Pts',(-4.80625418865864,4.76701442265624,-14.5514280270077));
#44450=CARTESIAN_POINT('Ctrl Pts',(-4.92922836711494,4.63626969716274,-14.5429907308679));
#44451=CARTESIAN_POINT('Ctrl Pts',(-5.05211481287109,4.50561824806221,-14.5345594540955));
#44452=CARTESIAN_POINT('Ctrl Pts',(-5.16986220454636,4.37001580957461,-14.5261281773232));
#44453=CARTESIAN_POINT('Ctrl Pts',(-5.28207072526785,4.22989572605145,-14.5176969005509));
#44454=CARTESIAN_POINT('Ctrl Pts',(-5.39423114935557,4.08983570306824,-14.509269237729));
#44455=CARTESIAN_POINT('Ctrl Pts',(-5.50085722866169,3.94526215367283,-14.5008415749071));
#44456=CARTESIAN_POINT('Ctrl Pts',(-5.60158875020747,3.79664226304627,-14.4924139120852));
#44457=CARTESIAN_POINT('Ctrl Pts',(-5.70228926260703,3.6480681234999,-14.4839888436312));
#44458=CARTESIAN_POINT('Ctrl Pts',(-5.79709865021273,3.49545040088813,-14.4755637751773));
#44459=CARTESIAN_POINT('Ctrl Pts',(-5.88569923463785,3.33928637876171,-14.4671387067233));
#44460=CARTESIAN_POINT('Ctrl Pts',(-5.90994306653303,3.29655512224604,-14.4648333501094));
#44461=CARTESIAN_POINT('Ctrl Pts',(-5.9337222751961,3.25355850429868,-14.4625279934954));
#44462=CARTESIAN_POINT('Ctrl Pts',(-5.95703093145548,3.21030706968705,-14.4602226368815));
#44463=CARTESIAN_POINT('Ctrl Pts',(-6.04408268935635,3.04877423086624,-14.4516127306046));
#44464=CARTESIAN_POINT('Ctrl Pts',(-6.12452935516968,2.8837560899616,-14.4430028243278));
#44465=CARTESIAN_POINT('Ctrl Pts',(-6.19811660568511,2.71581286953473,-14.434392918051));
#44466=CARTESIAN_POINT('Ctrl Pts',(-6.27174700067294,2.54777118338742,-14.4257779637549));
#44467=CARTESIAN_POINT('Ctrl Pts',(-6.33850983194855,2.37680127508355,-14.4171630094587));
#44468=CARTESIAN_POINT('Ctrl Pts',(-6.39819923629958,2.20348259185669,-14.4085480551625));
#44469=CARTESIAN_POINT('Ctrl Pts',(-6.45924455656327,2.0262267683098,-14.3997374019187));
#44470=CARTESIAN_POINT('Ctrl Pts',(-6.51289115985987,1.84651451363404,-14.390926748675));
#44471=CARTESIAN_POINT('Ctrl Pts',(-6.55897313549348,1.66498060285243,-14.3821160954312));
#44472=CARTESIAN_POINT('Ctrl Pts',(-6.60411423036851,1.48715316865601,-14.3734853340864));
#44473=CARTESIAN_POINT('Ctrl Pts',(-6.64199658241001,1.30757805290614,-14.3648545727416));
#44474=CARTESIAN_POINT('Ctrl Pts',(-6.67251620037296,1.12686137379909,-14.3562238113968));
#44475=CARTESIAN_POINT('Ctrl Pts',(-6.70399000391936,0.940494648544629,
-14.3473232122035));
#44476=CARTESIAN_POINT('Ctrl Pts',(-6.72763318165452,0.752914176868978,
-14.3384226130102));
#44477=CARTESIAN_POINT('Ctrl Pts',(-6.74338945277686,0.564789950492972,
-14.3295220138169));
#44478=CARTESIAN_POINT('Ctrl Pts',(-6.75914572389919,0.376665724116966,
-14.3206214146236));
#44479=CARTESIAN_POINT('Ctrl Pts',(-6.76701510487806,0.1879980978005,-14.3117208154303));
#44480=CARTESIAN_POINT('Ctrl Pts',(-6.76699997822088,-0.000542916824000972,
-14.302820216237));
#44481=CARTESIAN_POINT('',(-6.76699761007657,-0.00568728563850417,-14.6971797837756));
#44482=CARTESIAN_POINT('Ctrl Pts',(3.09908550384719,6.01564277861013,-15.3486931990458));
#44483=CARTESIAN_POINT('Ctrl Pts',(2.93975348353047,6.09772603598339,-15.3402662756962));
#44484=CARTESIAN_POINT('Ctrl Pts',(2.77719934489261,6.17345415443444,-15.3318393523467));
#44485=CARTESIAN_POINT('Ctrl Pts',(2.61196173671878,6.24259119964755,-15.3234124289971));
#44486=CARTESIAN_POINT('Ctrl Pts',(2.44657711471286,6.31178975689819,-15.3149780081153));
#44487=CARTESIAN_POINT('Ctrl Pts',(2.27850456010173,6.37438539343999,-15.3065435872335));
#44488=CARTESIAN_POINT('Ctrl Pts',(2.10830190077073,6.4301906733165,-15.2981091663517));
#44489=CARTESIAN_POINT('Ctrl Pts',(1.93802114287125,6.48602155979922,-15.2896708752824));
#44490=CARTESIAN_POINT('Ctrl Pts',(1.76560865014932,6.5350557792074,-15.2812325842131));
#44491=CARTESIAN_POINT('Ctrl Pts',(1.59163596375048,6.57715622126281,-15.2727942931438));
#44492=CARTESIAN_POINT('Ctrl Pts',(1.41746237657205,6.61930528021209,-15.2643462576757));
#44493=CARTESIAN_POINT('Ctrl Pts',(1.24172532122487,6.65450448902835,-15.2558982222075));
#44494=CARTESIAN_POINT('Ctrl Pts',(1.06500636527423,6.68266791348526,-15.2474501867393));
#44495=CARTESIAN_POINT('Ctrl Pts',(0.933624842107104,6.70360598197285,-15.2411695035969));
#44496=CARTESIAN_POINT('Ctrl Pts',(0.801700799415876,6.72065632612268,-15.2348888204545));
#44497=CARTESIAN_POINT('Ctrl Pts',(0.669474440955553,6.73380226713758,-15.2286081373122));
#44498=CARTESIAN_POINT('Ctrl Pts',(0.495982525609927,6.75105082871225,-15.2203673617154));
#44499=CARTESIAN_POINT('Ctrl Pts',(0.321584056323243,6.76161406804796,-15.2121265861186));
#44500=CARTESIAN_POINT('Ctrl Pts',(0.146833588963459,6.76540677987304,-15.2038858105218));
#44501=CARTESIAN_POINT('Ctrl Pts',(-0.0277233233071831,6.76919529085856,
-15.1956541624775));
#44502=CARTESIAN_POINT('Ctrl Pts',(-0.202631104760295,6.76622819874597,
-15.1874225144332));
#44503=CARTESIAN_POINT('Ctrl Pts',(-0.377328603778492,6.75647186960551,
-15.1791908663888));
#44504=CARTESIAN_POINT('Ctrl Pts',(-0.551863739105498,6.74672460798817,
-15.1709668688304));
#44505=CARTESIAN_POINT('Ctrl Pts',(-0.726188628068499,6.73020069545278,
-15.1627428712721));
#44506=CARTESIAN_POINT('Ctrl Pts',(-0.899740535828375,6.70691851509971,
-15.1545188737137));
#44507=CARTESIAN_POINT('Ctrl Pts',(-1.07313910980138,6.68365690464371,-15.1463021420892));
#44508=CARTESIAN_POINT('Ctrl Pts',(-1.24576571244587,6.6536489742404,-15.1380854104647));
#44509=CARTESIAN_POINT('Ctrl Pts',(-1.41706128043353,6.61696503901117,-15.1298686788402));
#44510=CARTESIAN_POINT('Ctrl Pts',(-1.588269087361,6.58029989831986,-15.1216561569515));
#44511=CARTESIAN_POINT('Ctrl Pts',(-1.75814687074162,6.53696563914039,-15.1134436350627));
#44512=CARTESIAN_POINT('Ctrl Pts',(-1.92614391507259,6.48708398422811,-15.105231113174));
#44513=CARTESIAN_POINT('Ctrl Pts',(-2.09408478038252,6.43721900998156,-15.0970213375922));
#44514=CARTESIAN_POINT('Ctrl Pts',(-2.26014581884749,6.38081110286614,-15.0888115620103));
#44515=CARTESIAN_POINT('Ctrl Pts',(-2.42378958927283,6.31803236988642,-15.0806017864285));
#44516=CARTESIAN_POINT('Ctrl Pts',(-2.49526493669721,6.29061225032474,-15.0770159697459));
#44517=CARTESIAN_POINT('Ctrl Pts',(-2.56627933281965,6.26197740065527,-15.0734301530634));
#44518=CARTESIAN_POINT('Ctrl Pts',(-2.63678901268566,6.23214511244565,-15.0698443363808));
#44519=CARTESIAN_POINT('Ctrl Pts',(-2.81098233927863,6.15844479877255,-15.060985618859));
#44520=CARTESIAN_POINT('Ctrl Pts',(-2.98191342115986,6.07750945654687,-15.0521269013372));
#44521=CARTESIAN_POINT('Ctrl Pts',(-3.14901240109173,5.98965857939921,-15.0432681838153));
#44522=CARTESIAN_POINT('Ctrl Pts',(-3.316423996375,5.90164334737133,-15.0343928930559));
#44523=CARTESIAN_POINT('Ctrl Pts',(-3.47998893290189,5.80668684568764,-15.0255176022965));
#44524=CARTESIAN_POINT('Ctrl Pts',(-3.63916475412043,5.7051528368982,-15.0166423115371));
#44525=CARTESIAN_POINT('Ctrl Pts',(-3.7987926704622,5.6033304486937,-15.0077418129564));
#44526=CARTESIAN_POINT('Ctrl Pts',(-3.95400630533589,5.49489330955781,-14.9988413143756));
#44527=CARTESIAN_POINT('Ctrl Pts',(-4.1042923612587,5.38024843416301,-14.9899408157948));
#44528=CARTESIAN_POINT('Ctrl Pts',(-4.25478185961625,5.26544836384718,-14.9810282685972));
#44529=CARTESIAN_POINT('Ctrl Pts',(-4.40033025217478,5.14442393342543,-14.9721157213996));
#44530=CARTESIAN_POINT('Ctrl Pts',(-4.54045880286092,5.01762123515943,-14.963203174202));
#44531=CARTESIAN_POINT('Ctrl Pts',(-4.68089677107267,4.89053854415143,-14.9542709472297));
#44532=CARTESIAN_POINT('Ctrl Pts',(-4.81589076726617,4.75765223995337,-14.9453387202575));
#44533=CARTESIAN_POINT('Ctrl Pts',(-4.94499826901006,4.61944597538357,-14.9364064932852));
#44534=CARTESIAN_POINT('Ctrl Pts',(-5.06701976695758,4.48882509587813,-14.9279645073399));
#44535=CARTESIAN_POINT('Ctrl Pts',(-5.18378341004267,4.35345262951812,-14.9195225213945));
#44536=CARTESIAN_POINT('Ctrl Pts',(-5.29494976727013,4.21376268459509,-14.9110805354492));
#44537=CARTESIAN_POINT('Ctrl Pts',(-5.40168110092664,4.07964572248637,-14.9029753457035));
#44538=CARTESIAN_POINT('Ctrl Pts',(-5.50347933923222,3.94126249702449,-14.8948701559579));
#44539=CARTESIAN_POINT('Ctrl Pts',(-5.59997854021005,3.79901689245874,-14.8867649662123));
#44540=CARTESIAN_POINT('Ctrl Pts',(-5.69634300185476,3.65696990174373,-14.878671093533));
#44541=CARTESIAN_POINT('Ctrl Pts',(-5.78742296033443,3.51107157932362,-14.8705772208538));
#44542=CARTESIAN_POINT('Ctrl Pts',(-5.87289225286514,3.36175929927123,-14.8624833481745));
#44543=CARTESIAN_POINT('Ctrl Pts',(-5.95829265641316,3.21256736619695,-14.8543959992261));
#44544=CARTESIAN_POINT('Ctrl Pts',(-6.03809121013814,3.05996727008916,-14.8463086502776));
#44545=CARTESIAN_POINT('Ctrl Pts',(-6.11200434243221,2.90442626315246,-14.8382213013291));
#44546=CARTESIAN_POINT('Ctrl Pts',(-6.18587232017185,2.7489802783674,-14.830138893054));
#44547=CARTESIAN_POINT('Ctrl Pts',(-6.25386187434581,2.59059729164678,-14.8220564847788));
#44548=CARTESIAN_POINT('Ctrl Pts',(-6.31573484108605,2.42977003378752,-14.8139740765036));
#44549=CARTESIAN_POINT('Ctrl Pts',(-6.37758207633992,2.2690096601365,-14.8058950295086));
#44550=CARTESIAN_POINT('Ctrl Pts',(-6.43331765589511,2.10580738396821,-14.7978159825136));
#44551=CARTESIAN_POINT('Ctrl Pts',(-6.48275117260066,1.94067674643275,-14.7897369355187));
#44552=CARTESIAN_POINT('Ctrl Pts',(-6.53218320338001,1.77555107257288,-14.7816581313724));
#44553=CARTESIAN_POINT('Ctrl Pts',(-6.57531343199198,1.60849750413756,-14.7735793272262));
#44554=CARTESIAN_POINT('Ctrl Pts',(-6.61200098781636,1.44004581076973,-14.76550052308));
#44555=CARTESIAN_POINT('Ctrl Pts',(-6.64868681141072,1.27160207097293,-14.7574221003805));
#44556=CARTESIAN_POINT('Ctrl Pts',(-6.67893049380477,1.10176070052763,-14.749343677681));
#44557=CARTESIAN_POINT('Ctrl Pts',(-6.70264216311613,0.931062314358147,
-14.7412652549814));
#44558=CARTESIAN_POINT('Ctrl Pts',(-6.72636607119617,0.760275822284553,
-14.7331826626072));
#44559=CARTESIAN_POINT('Ctrl Pts',(-6.74355118206697,0.588631798153986,
-14.725100070233));
#44560=CARTESIAN_POINT('Ctrl Pts',(-6.75415939711594,0.416677139222255,
-14.7170174778589));
#44561=CARTESIAN_POINT('Ctrl Pts',(-6.76283823491131,0.275996865855036,
-14.7104049131759));
#44562=CARTESIAN_POINT('Ctrl Pts',(-6.76711594140666,0.135108866044254,
-14.703792348493));
#44563=CARTESIAN_POINT('Ctrl Pts',(-6.76699761007719,-0.00568728490314065,
-14.6971797838101));
#44564=CARTESIAN_POINT('Ctrl Pts',(-6.76699761007657,-0.00568728563859448,
-14.6971797837755));
#44565=CARTESIAN_POINT('Ctrl Pts',(-6.76681707131456,-0.220500721906246,
-14.6870909586725));
#44566=CARTESIAN_POINT('Ctrl Pts',(-6.75640429646117,-0.434842481389935,
-14.6770021335695));
#44567=CARTESIAN_POINT('Ctrl Pts',(-6.73591575628249,-0.647864124848208,
-14.6669133084664));
#44568=CARTESIAN_POINT('Ctrl Pts',(-6.71520918628652,-0.863152648698912,
-14.6567171226303));
#44569=CARTESIAN_POINT('Ctrl Pts',(-6.68421135166224,-1.07709290079024,
-14.6465209367942));
#44570=CARTESIAN_POINT('Ctrl Pts',(-6.64313163371893,-1.28883323090414,
-14.636324750958));
#44571=CARTESIAN_POINT('Ctrl Pts',(-6.60159558463147,-1.50292566351396,
-14.626015301512));
#44572=CARTESIAN_POINT('Ctrl Pts',(-6.54975243440539,-1.71476912737992,
-14.6157058520659));
#44573=CARTESIAN_POINT('Ctrl Pts',(-6.48786653253983,-1.9235063961291,-14.6053964026199));
#44574=CARTESIAN_POINT('Ctrl Pts',(-6.46416841085701,-2.00343867545994,
-14.6014485796086));
#44575=CARTESIAN_POINT('Ctrl Pts',(-6.43899814227914,-2.08291570187134,
-14.5975007565974));
#44576=CARTESIAN_POINT('Ctrl Pts',(-6.41237240559593,-2.16189017573786,
-14.5935529335862));
#44577=CARTESIAN_POINT('Ctrl Pts',(-6.35793914863978,-2.32334440628553,
-14.5854820633998));
#44578=CARTESIAN_POINT('Ctrl Pts',(-6.29730466783117,-2.48303625918558,
-14.5774111932134));
#44579=CARTESIAN_POINT('Ctrl Pts',(-6.23059847689061,-2.64044155772637,
-14.569340323027));
#44580=CARTESIAN_POINT('Ctrl Pts',(-6.16397529661965,-2.79765097760813,
-14.5612794964112));
#44581=CARTESIAN_POINT('Ctrl Pts',(-6.09129558404343,-2.95257916573787,
-14.5532186697954));
#44582=CARTESIAN_POINT('Ctrl Pts',(-6.01273899688986,-3.10471556753271,
-14.5451578431796));
#44583=CARTESIAN_POINT('Ctrl Pts',(-5.93426294104238,-3.25669600859168,
-14.5371052800197));
#44584=CARTESIAN_POINT('Ctrl Pts',(-5.84992216950608,-3.40589003009599,
-14.5290527168598));
#44585=CARTESIAN_POINT('Ctrl Pts',(-5.75994490937173,-3.55180568739376,
-14.5210001536999));
#44586=CARTESIAN_POINT('Ctrl Pts',(-5.67004018662044,-3.69760371119268,
-14.5129540823121));
#44587=CARTESIAN_POINT('Ctrl Pts',(-5.57450821420038,-3.84012831526304,
-14.5049080109242));
#44588=CARTESIAN_POINT('Ctrl Pts',(-5.47362370943306,-3.97891096753022,
-14.4968619395363));
#44589=CARTESIAN_POINT('Ctrl Pts',(-5.37279846785594,-4.11761209387093,
-14.4888205947005));
#44590=CARTESIAN_POINT('Ctrl Pts',(-5.26662717206891,-4.25257534338023,
-14.4807792498646));
#44591=CARTESIAN_POINT('Ctrl Pts',(-5.15542846783685,-4.38336016236602,
-14.4727379050287));
#44592=CARTESIAN_POINT('Ctrl Pts',(-5.04208619474571,-4.51666611023683,
-14.4645415478077));
#44593=CARTESIAN_POINT('Ctrl Pts',(-4.92352091931624,-4.6456305533063,-14.4563451905866));
#44594=CARTESIAN_POINT('Ctrl Pts',(-4.80011422484727,-4.76982100590986,
-14.4481488333655));
#44595=CARTESIAN_POINT('Ctrl Pts',(-4.679079926891,-4.89162399486782,-14.440110044657));
#44596=CARTESIAN_POINT('Ctrl Pts',(-4.55338895451524,-5.00883462189334,
-14.4320712559485));
#44597=CARTESIAN_POINT('Ctrl Pts',(-4.42343927925482,-5.12108132553522,
-14.42403246724));
#44598=CARTESIAN_POINT('Ctrl Pts',(-4.29347569820182,-5.23334004059134,
-14.4159928183083));
#44599=CARTESIAN_POINT('Ctrl Pts',(-4.1592527894436,-5.34063353037173,-14.4079531693766));
#44600=CARTESIAN_POINT('Ctrl Pts',(-4.02120216050053,-5.44263007969363,
-14.3999135204449));
#44601=CARTESIAN_POINT('Ctrl Pts',(-3.88310942433789,-5.54465773927653,
-14.3918714193167));
#44602=CARTESIAN_POINT('Ctrl Pts',(-3.74118694428551,-5.64138502068034,
-14.3838293181885));
#44603=CARTESIAN_POINT('Ctrl Pts',(-3.59589575847288,-5.73252323974328,
-14.3757872170603));
#44604=CARTESIAN_POINT('Ctrl Pts',(-3.44570156597138,-5.82673701562805,
-14.3674737266155));
#44605=CARTESIAN_POINT('Ctrl Pts',(-3.29190769846732,-5.91497767892445,
-14.3591602361708));
#44606=CARTESIAN_POINT('Ctrl Pts',(-3.13505056623211,-5.99697815129985,
-14.350846745726));
#44607=CARTESIAN_POINT('Ctrl Pts',(-2.98304664800076,-6.07644150065646,
-14.3427904775552));
#44608=CARTESIAN_POINT('Ctrl Pts',(-2.82816656306412,-6.15004496431317,
-14.3347342093845));
#44609=CARTESIAN_POINT('Ctrl Pts',(-2.67091781100977,-6.21759495680048,
-14.3266779412137));
#44610=CARTESIAN_POINT('Ctrl Pts',(-2.50613805066523,-6.28838007546068,
-14.3182358396319));
#44611=CARTESIAN_POINT('Ctrl Pts',(-2.33875761612971,-6.35251746077792,
-14.3097937380502));
#44612=CARTESIAN_POINT('Ctrl Pts',(-2.16937641760564,-6.40984359861741,
-14.3013516364684));
#44613=CARTESIAN_POINT('Ctrl Pts',(-1.99999521908157,-6.46716973645689,
-14.2929095348866));
#44614=CARTESIAN_POINT('Ctrl Pts',(-1.82861372308746,-6.51768457945689,
-14.2844674333049));
#44615=CARTESIAN_POINT('Ctrl Pts',(-1.65584129774126,-6.561286352286,-14.2760253317231));
#44616=CARTESIAN_POINT('Ctrl Pts',(-1.48528445232515,-6.6043289895204,-14.2676914890304));
#44617=CARTESIAN_POINT('Ctrl Pts',(-1.31283006079866,-6.64077222487531,
-14.2593576463377));
#44618=CARTESIAN_POINT('Ctrl Pts',(-1.13902358334522,-6.67045083008513,
-14.251023803645));
#44619=CARTESIAN_POINT('Ctrl Pts',(-0.965421958813958,-6.70009445530403,
-14.2426997834403));
#44620=CARTESIAN_POINT('Ctrl Pts',(-0.790471762921994,-6.72298927521063,
-14.2343757632355));
#44621=CARTESIAN_POINT('Ctrl Pts',(-0.614732149518258,-6.7390202095222,
-14.2260517430308));
#44622=CARTESIAN_POINT('Ctrl Pts',(-0.439167445879287,-6.7550351885981,
-14.2177360075399));
#44623=CARTESIAN_POINT('Ctrl Pts',(-0.262815234340318,-6.76419986125205,
-14.2094202720491));
#44624=CARTESIAN_POINT('Ctrl Pts',(-0.0862435904396328,-6.76645040202824,
-14.2011045365582));
#44625=CARTESIAN_POINT('Ctrl Pts',(0.0901846680792544,-6.76869911524797,
-14.1927955538782));
#44626=CARTESIAN_POINT('Ctrl Pts',(0.266831657583918,-6.76404487987223,
-14.1844865711981));
#44627=CARTESIAN_POINT('Ctrl Pts',(0.443125236909414,-6.75247576999829,
-14.1761775885181));
#44628=CARTESIAN_POINT('Ctrl Pts',(0.619307940457356,-6.74091393624897,
-14.1678738315809));
#44629=CARTESIAN_POINT('Ctrl Pts',(0.795137330671534,-6.72244591771199,
-14.1595700746438));
#44630=CARTESIAN_POINT('Ctrl Pts',(0.970042096076698,-6.69711186496382,
-14.1512663177066));
#44631=CARTESIAN_POINT('Ctrl Pts',(1.14487585436354,-6.67178809723033,-14.1429659318946));
#44632=CARTESIAN_POINT('Ctrl Pts',(1.3187853921246,-6.63960389926502,-14.1346655460825));
#44633=CARTESIAN_POINT('Ctrl Pts',(1.49120504944879,-6.60065121791013,-14.1263651602705));
#44634=CARTESIAN_POINT('Ctrl Pts',(1.66358834795367,-6.56170675066217,-14.1180665247939));
#44635=CARTESIAN_POINT('Ctrl Pts',(1.83448205289264,-6.51599672014443,-14.1097678893172));
#44636=CARTESIAN_POINT('Ctrl Pts',(2.00333097766183,-6.46366413065689,-14.1014692538406));
#44637=CARTESIAN_POINT('Ctrl Pts',(2.17217232356975,-6.41133389014158,-14.093170990852));
#44638=CARTESIAN_POINT('Ctrl Pts',(2.33896874007954,-6.35238178613532,-14.0848727278634));
#44639=CARTESIAN_POINT('Ctrl Pts',(2.50318029140565,-6.28700067032908,-14.0765744648748));
#44640=CARTESIAN_POINT('Ctrl Pts',(2.66741172804957,-6.22161163714885,-14.068275197002));
#44641=CARTESIAN_POINT('Ctrl Pts',(2.82905735291413,-6.14979217006359,-14.0599759291292));
#44642=CARTESIAN_POINT('Ctrl Pts',(2.98759711893101,-6.07178330105375,-14.0516766612564));
#44643=CARTESIAN_POINT('Ctrl Pts',(3.14624820541665,-5.9937196572446,-14.0433715659599));
#44644=CARTESIAN_POINT('Ctrl Pts',(3.30178876297166,-5.90945808125631,-14.0350664706634));
#44645=CARTESIAN_POINT('Ctrl Pts',(3.45372247577024,-5.81928604386823,-14.0267613753669));
#44646=CARTESIAN_POINT('Ctrl Pts',(3.60571159150095,-5.72908112506642,-14.0184532516007));
#44647=CARTESIAN_POINT('Ctrl Pts',(3.75409094575897,-5.63296163296958,-14.0101451278346));
#44648=CARTESIAN_POINT('Ctrl Pts',(3.89839296576975,-5.53125856242835,-14.0018370040685));
#44649=CARTESIAN_POINT('Ctrl Pts',(4.04284837799412,-5.42944738211072,-13.9935200488149));
#44650=CARTESIAN_POINT('Ctrl Pts',(4.18321751622051,-5.32204097123177,-13.9852030935612));
#44651=CARTESIAN_POINT('Ctrl Pts',(4.31906481494099,-5.20941149500965,-13.9768861383075));
#44652=CARTESIAN_POINT('Ctrl Pts',(4.4191822072307,-5.12640528465051,-13.970756668825));
#44653=CARTESIAN_POINT('Ctrl Pts',(4.51684425808701,-5.04056303560228,-13.9646271993425));
#44654=CARTESIAN_POINT('Ctrl Pts',(4.61188946415114,-4.95204650326021,-13.95849772986));
#44655=CARTESIAN_POINT('Ctrl Pts',(4.742933313002,-4.83000408191801,-13.9500467063348));
#44656=CARTESIAN_POINT('Ctrl Pts',(4.86924074728128,-4.70265360701531,-13.9415956828097));
#44657=CARTESIAN_POINT('Ctrl Pts',(4.9903744377037,-4.57038860180549,-13.9331446592845));
#44658=CARTESIAN_POINT('Ctrl Pts',(5.11140147351199,-4.43824005200161,-13.9247010766344));
#44659=CARTESIAN_POINT('Ctrl Pts',(5.22726362225071,-4.30118583993763,-13.9162574939842));
#44660=CARTESIAN_POINT('Ctrl Pts',(5.33755959374235,-4.15965702711762,-13.9078139113341));
#44661=CARTESIAN_POINT('Ctrl Pts',(5.44777344644726,-4.01823358690768,-13.8993766151943));
#44662=CARTESIAN_POINT('Ctrl Pts',(5.55242918005835,-3.87234244769853,-13.8909393190545));
#44663=CARTESIAN_POINT('Ctrl Pts',(5.65116482608073,-3.7224488053522,-13.8825020229147));
#44664=CARTESIAN_POINT('Ctrl Pts',(5.74983003174796,-3.57266210069074,-13.8740707461424));
#44665=CARTESIAN_POINT('Ctrl Pts',(5.842583392462,-3.41887886478249,-13.8656394693701));
#44666=CARTESIAN_POINT('Ctrl Pts',(5.92910531318734,-3.26159457706406,-13.8572081925977));
#44667=CARTESIAN_POINT('Ctrl Pts',(6.01559014748542,-3.10437770708494,-13.8487805297758));
#44668=CARTESIAN_POINT('Ctrl Pts',(6.09584870711687,-2.94366306687168,-13.8403528669539));
#44669=CARTESIAN_POINT('Ctrl Pts',(6.16960621678527,-2.77997268508245,-13.831925204132));
#44670=CARTESIAN_POINT('Ctrl Pts',(6.24334102097504,-2.6163326936668,-13.8235001356781));
#44671=CARTESIAN_POINT('Ctrl Pts',(6.31057863024381,-2.44971908938091,-13.8150750672241));
#44672=CARTESIAN_POINT('Ctrl Pts',(6.37109133465156,-2.28067626057005,-13.8066499987701));
#44673=CARTESIAN_POINT('Ctrl Pts',(6.38764946282475,-2.23442096833673,-13.8043446421563));
#44674=CARTESIAN_POINT('Ctrl Pts',(6.40370434955022,-2.18798390844266,-13.8020392855424));
#44675=CARTESIAN_POINT('Ctrl Pts',(6.41925196146129,-2.14137648611247,-13.7997339289286));
#44676=CARTESIAN_POINT('Ctrl Pts',(6.47737949272454,-1.96712629167147,-13.7911149404041));
#44677=CARTESIAN_POINT('Ctrl Pts',(6.52838673323858,-1.79057136641632,-13.7824959518796));
#44678=CARTESIAN_POINT('Ctrl Pts',(6.57211915190241,-1.61230854776547,-13.7738769633551));
#44679=CARTESIAN_POINT('Ctrl Pts',(6.61587777018779,-1.43393893377768,-13.7652528112873));
#44680=CARTESIAN_POINT('Ctrl Pts',(6.65235279638334,-1.25385967983139,-13.7566286592195));
#44681=CARTESIAN_POINT('Ctrl Pts',(6.68144074299728,-1.0726782359198,-13.7480045071517));
#44682=CARTESIAN_POINT('Ctrl Pts',(6.71152495960808,-0.885291278812168,
-13.7390849755555));
#44683=CARTESIAN_POINT('Ctrl Pts',(6.73370706994347,-0.696725649066451,
-13.7301654439593));
#44684=CARTESIAN_POINT('Ctrl Pts',(6.74793089696959,-0.507658950204924,
-13.7212459123631));
#44685=CARTESIAN_POINT('Ctrl Pts',(6.76170930707696,-0.324512845448838,
-13.7126056945038));
#44686=CARTESIAN_POINT('Ctrl Pts',(6.76802035133266,-0.140896884559492,
-13.7039654766445));
#44687=CARTESIAN_POINT('Ctrl Pts',(6.76686608173633,0.0425726654844531,
-13.6953252587853));
#44688=CARTESIAN_POINT('Ctrl Pts',(6.76565584074674,0.234938790789733,-13.6862660703206));
#44689=CARTESIAN_POINT('Ctrl Pts',(6.75623830814933,0.427143565653001,-13.6772068818559));
#44690=CARTESIAN_POINT('Ctrl Pts',(6.73867711835929,0.618481765697974,-13.6681476933912));
#44691=CARTESIAN_POINT('Ctrl Pts',(6.72111592856926,0.809819965742948,-13.6590885049265));
#44692=CARTESIAN_POINT('Ctrl Pts',(6.69541116558886,1.00029121621086,-13.6500293164618));
#44693=CARTESIAN_POINT('Ctrl Pts',(6.66168820007291,1.18920112891359,-13.6409701279971));
#44694=CARTESIAN_POINT('Ctrl Pts',(6.62802365722869,1.37778376844662,-13.6319266339408));
#44695=CARTESIAN_POINT('Ctrl Pts',(6.58633849049111,1.56498435577368,-13.6228831398846));
#44696=CARTESIAN_POINT('Ctrl Pts',(6.53676408474523,1.75014407989311,-13.6138396458283));
#44697=CARTESIAN_POINT('Ctrl Pts',(6.48723502452701,1.93513443908993,-13.604804423823));
#44698=CARTESIAN_POINT('Ctrl Pts',(6.42983119410984,2.11808743230304,-13.5957692018176));
#44699=CARTESIAN_POINT('Ctrl Pts',(6.36473454466274,2.29835662506426,-13.5867339798123));
#44700=CARTESIAN_POINT('Ctrl Pts',(6.29975258134059,2.47830822275199,-13.5777146759012));
#44701=CARTESIAN_POINT('Ctrl Pts',(6.22710494354743,2.6555852381161,-13.5686953719901));
#44702=CARTESIAN_POINT('Ctrl Pts',(6.14702259456094,2.82955866204559,-13.559676068079));
#44703=CARTESIAN_POINT('Ctrl Pts',(6.06704071447482,3.00331382416315,-13.5506680795146));
#44704=CARTESIAN_POINT('Ctrl Pts',(5.97964283666695,3.17377345038416,-13.5416600909503));
#44705=CARTESIAN_POINT('Ctrl Pts',(5.88510795963793,3.34032832269619,-13.5326521023859));
#44706=CARTESIAN_POINT('Ctrl Pts',(5.79078659293997,3.50650702499514,-13.5236644586792));
#44707=CARTESIAN_POINT('Ctrl Pts',(5.68936051965363,3.66879837028608,-13.5146768149726));
#44708=CARTESIAN_POINT('Ctrl Pts',(5.58115434728841,3.82661797828627,-13.5056891712659));
#44709=CARTESIAN_POINT('Ctrl Pts',(5.48691427094528,3.96406791835236,-13.4978615565324));
#44710=CARTESIAN_POINT('Ctrl Pts',(5.38753211189394,4.09812618004806,-13.4900339417989));
#44711=CARTESIAN_POINT('Ctrl Pts',(5.28325092638908,4.22842153158942,-13.4822063270654));
#44712=CARTESIAN_POINT('Ctrl Pts',(5.17503689028484,4.36363082948576,-13.4740835024228));
#44713=CARTESIAN_POINT('Ctrl Pts',(5.06159440159116,4.49472655455563,-13.4659606777802));
#44714=CARTESIAN_POINT('Ctrl Pts',(4.94327913949059,4.62128557320116,-13.4578378531375));
#44715=CARTESIAN_POINT('Ctrl Pts',(4.82497424657797,4.74783350017325,-13.4497157403819));
#44716=CARTESIAN_POINT('Ctrl Pts',(4.70179768157302,4.8698452461068,-13.4415936276263));
#44717=CARTESIAN_POINT('Ctrl Pts',(4.57414341672341,4.98693302574297,-13.4334715148706));
#44718=CARTESIAN_POINT('Ctrl Pts',(4.44643674257854,5.10406887653462,-13.4253460675284));
#44719=CARTESIAN_POINT('Ctrl Pts',(4.31424896499503,5.21627647373275,-13.4172206201861));
#44720=CARTESIAN_POINT('Ctrl Pts',(4.17800905335186,5.32320667925921,-13.4090951728438));
#44721=CARTESIAN_POINT('Ctrl Pts',(4.04173783311935,5.43016145786307,-13.4009678582345));
#44722=CARTESIAN_POINT('Ctrl Pts',(3.90141291699111,5.53183620972697,-13.3928405436252));
#44723=CARTESIAN_POINT('Ctrl Pts',(3.75749377382145,5.62792408794691,-13.3847132290159));
#44724=CARTESIAN_POINT('Ctrl Pts',(3.61345871113064,5.7240893600464,-13.3765793682697));
#44725=CARTESIAN_POINT('Ctrl Pts',(3.46582394965658,5.81465857691305,-13.3684455075235));
#44726=CARTESIAN_POINT('Ctrl Pts',(3.31507565523197,5.89936966125096,-13.3603116467773));
#44727=CARTESIAN_POINT('Ctrl Pts',(3.24375774226913,5.93944585423782,-13.3564635768872));
#44728=CARTESIAN_POINT('Ctrl Pts',(3.17174330901091,5.9782115748284,-13.3526155069972));
#44729=CARTESIAN_POINT('Ctrl Pts',(3.09908550384717,6.01564277861014,-13.3487674371071));
#44730=CARTESIAN_POINT('Origin',(0.,0.,-63.6971797838103));
#44731=CARTESIAN_POINT('',(3.0990855038472,6.01564277861013,-10.9542570414832));
#44732=CARTESIAN_POINT('',(3.09908550384727,6.01564277861009,-11.3484335646661));
#44733=CARTESIAN_POINT('',(3.09908550384721,6.01564277861012,-63.6971797838103));
#44734=CARTESIAN_POINT('',(-6.76699969835648,0.00202050572450262,-12.3028202161486));
#44735=CARTESIAN_POINT('Ctrl Pts',(-6.76699969835648,0.00202050572450262,
-12.3028202161486));
#44736=CARTESIAN_POINT('Ctrl Pts',(-6.76705055160899,-0.168295242583025,
-12.294822198901));
#44737=CARTESIAN_POINT('Ctrl Pts',(-6.7606671827498,-0.338707913742557,
-12.2868241816533));
#44738=CARTESIAN_POINT('Ctrl Pts',(-6.74785397761637,-0.508680348319968,
-12.2788261644057));
#44739=CARTESIAN_POINT('Ctrl Pts',(-6.73504188905724,-0.678637971080195,
-12.270828844125));
#44740=CARTESIAN_POINT('Ctrl Pts',(-6.715801100073,-0.84815505553999,-12.2628315238443));
#44741=CARTESIAN_POINT('Ctrl Pts',(-6.69018805542417,-1.01669699668079,
-12.2548342035636));
#44742=CARTESIAN_POINT('Ctrl Pts',(-6.67171402995344,-1.13826193190081,
-12.2490659436558));
#44743=CARTESIAN_POINT('Ctrl Pts',(-6.6499260169178,-1.25931959581929,-12.243297683748));
#44744=CARTESIAN_POINT('Ctrl Pts',(-6.62486185616072,-1.37967184025286,
-12.2375294238403));
#44745=CARTESIAN_POINT('Ctrl Pts',(-6.58741075003943,-1.55950330247109,
-12.2289104353158));
#44746=CARTESIAN_POINT('Ctrl Pts',(-6.54264676604676,-1.73774349421691,
-12.2202914467914));
#44747=CARTESIAN_POINT('Ctrl Pts',(-6.4907366932037,-1.91379888689986,-12.2116724582669));
#44748=CARTESIAN_POINT('Ctrl Pts',(-6.43879552159444,-2.08995975247458,
-12.2030483061991));
#44749=CARTESIAN_POINT('Ctrl Pts',(-6.37969980329426,-2.26393291510661,
-12.1944241541314));
#44750=CARTESIAN_POINT('Ctrl Pts',(-6.313665777883,-2.43514136041198,-12.1858000020636));
#44751=CARTESIAN_POINT('Ctrl Pts',(-6.24537006933625,-2.61221374102931,
-12.1768804704674));
#44752=CARTESIAN_POINT('Ctrl Pts',(-6.16965249749903,-2.78632833563775,
-12.1679609388711));
#44753=CARTESIAN_POINT('Ctrl Pts',(-6.08680548758214,-2.95687131210337,
-12.1590414072748));
#44754=CARTESIAN_POINT('Ctrl Pts',(-6.00655281882438,-3.12207376193214,
-12.1504011894156));
#44755=CARTESIAN_POINT('Ctrl Pts',(-5.9196106539085,-3.28392465112468,-12.1417609715564));
#44756=CARTESIAN_POINT('Ctrl Pts',(-5.82629087306156,-3.44189245364808,
-12.1331207536971));
#44757=CARTESIAN_POINT('Ctrl Pts',(-5.72844594646879,-3.60752023268534,
-12.1240615652324));
#44758=CARTESIAN_POINT('Ctrl Pts',(-5.62358972766744,-3.76887864981842,
-12.1150023767676));
#44759=CARTESIAN_POINT('Ctrl Pts',(-5.51213207804354,-3.92539029323243,
-12.1059431883029));
#44760=CARTESIAN_POINT('Ctrl Pts',(-5.40067442841965,-4.08190193664644,
-12.0968839998381));
#44761=CARTESIAN_POINT('Ctrl Pts',(-5.2826156091448,-4.23356652475674,-12.0878248113733));
#44762=CARTESIAN_POINT('Ctrl Pts',(-5.15841337933328,-4.37984707585955,
-12.0787656229086));
#44763=CARTESIAN_POINT('Ctrl Pts',(-5.0344263211717,-4.52587420616965,-12.0697221288523));
#44764=CARTESIAN_POINT('Ctrl Pts',(-4.90420354310854,-4.66667101399946,
-12.060678634796));
#44765=CARTESIAN_POINT('Ctrl Pts',(-4.76819009904572,-4.80173428870886,
-12.0516351407398));
#44766=CARTESIAN_POINT('Ctrl Pts',(-4.63230106598284,-4.93667402153476,
-12.0425999187344));
#44767=CARTESIAN_POINT('Ctrl Pts',(-4.49063211060068,-5.06589052416948,
-12.0335646967291));
#44768=CARTESIAN_POINT('Ctrl Pts',(-4.34366575669864,-5.18891672645492,
-12.0245294747238));
#44769=CARTESIAN_POINT('Ctrl Pts',(-4.196958325518,-5.3117261833544,-12.0155101708127));
#44770=CARTESIAN_POINT('Ctrl Pts',(-4.0449723147111,-5.42836696512622,-12.0064908669016));
#44771=CARTESIAN_POINT('Ctrl Pts',(-3.88822383432558,-5.53841172306488,
-11.9974715629905));
#44772=CARTESIAN_POINT('Ctrl Pts',(-3.7316720058581,-5.64831842216772,-11.9884635744262));
#44773=CARTESIAN_POINT('Ctrl Pts',(-3.57036982584233,-5.75164547544265,
-11.9794555858618));
#44774=CARTESIAN_POINT('Ctrl Pts',(-3.40486495593366,-5.84800680846516,
-11.9704475972975));
#44775=CARTESIAN_POINT('Ctrl Pts',(-3.23973388457008,-5.94415050604221,
-11.9614599535908));
#44776=CARTESIAN_POINT('Ctrl Pts',(-3.07041927543412,-6.03335976694991,
-11.9524723098842));
#44777=CARTESIAN_POINT('Ctrl Pts',(-2.89749570565441,-6.11529293130871,
-11.9434846661775));
#44778=CARTESIAN_POINT('Ctrl Pts',(-2.74689126173724,-6.18665103866418,
-11.9356570514441));
#44779=CARTESIAN_POINT('Ctrl Pts',(-2.59354989145506,-6.2524906561159,-11.9278294367106));
#44780=CARTESIAN_POINT('Ctrl Pts',(-2.43786844108653,-6.31261328325713,
-11.9200018219772));
#44781=CARTESIAN_POINT('Ctrl Pts',(-2.27630899655625,-6.37500593325907,
-11.9118786635319));
#44782=CARTESIAN_POINT('Ctrl Pts',(-2.11230104511112,-6.43121228452732,
-11.9037555050867));
#44783=CARTESIAN_POINT('Ctrl Pts',(-1.94636493985081,-6.48104563484316,
-11.8956323466414));
#44784=CARTESIAN_POINT('Ctrl Pts',(-1.78044053395428,-6.53087547164702,
-11.8875097609213));
#44785=CARTESIAN_POINT('Ctrl Pts',(-1.61258859558895,-6.57433309724159,
-11.8793871752012));
#44786=CARTESIAN_POINT('Ctrl Pts',(-1.4433448121048,-6.61128162714085,-11.8712645894811));
#44787=CARTESIAN_POINT('Ctrl Pts',(-1.27408069223837,-6.64823459678622,
-11.8631410277488));
#44788=CARTESIAN_POINT('Ctrl Pts',(-1.10342475207964,-6.67867683642486,
-11.8550174660164));
#44789=CARTESIAN_POINT('Ctrl Pts',(-0.931923000236129,-6.7025225491326,
-11.8468939042841));
#44790=CARTESIAN_POINT('Ctrl Pts',(-0.760296329717402,-6.72638563061243,
-11.838764425501));
#44791=CARTESIAN_POINT('Ctrl Pts',(-0.587822979958832,-6.74364253827996,
-11.8306349467179));
#44792=CARTESIAN_POINT('Ctrl Pts',(-0.415054856188062,-6.75425928332298,
-11.8225054679348));
#44793=CARTESIAN_POINT('Ctrl Pts',(-0.242216297894182,-6.7648803566261,
-11.8143726749062));
#44794=CARTESIAN_POINT('Ctrl Pts',(-0.0690830917128784,-6.7688558628985,
-11.8062398818777));
#44795=CARTESIAN_POINT('Ctrl Pts',(0.103792972747499,-6.76620395929714,
-11.7981070888492));
#44796=CARTESIAN_POINT('Ctrl Pts',(0.276857013701378,-6.76354917215292,
-11.7899654526421));
#44797=CARTESIAN_POINT('Ctrl Pts',(0.44966298943481,-6.7542526014934,-11.781823816435));
#44798=CARTESIAN_POINT('Ctrl Pts',(0.621663590627383,-6.73838433009637,
-11.7736821802279));
#44799=CARTESIAN_POINT('Ctrl Pts',(0.709295560672166,-6.73029966135635,
-11.7695341271672));
#44800=CARTESIAN_POINT('Ctrl Pts',(0.796718609205389,-6.72050996055453,
-11.7653860741065));
#44801=CARTESIAN_POINT('Ctrl Pts',(0.883861440874248,-6.70902958357881,
-11.7612380210458));
#44802=CARTESIAN_POINT('Ctrl Pts',(1.06118506565371,-6.68566860230035,-11.7527973060677));
#44803=CARTESIAN_POINT('Ctrl Pts',(1.23771297400534,-6.65525591246259,-11.7443565910896));
#44804=CARTESIAN_POINT('Ctrl Pts',(1.41286268563528,-6.6178627993892,-11.7359158761115));
#44805=CARTESIAN_POINT('Ctrl Pts',(1.5878800108616,-6.58049794979232,-11.7274815410235));
#44806=CARTESIAN_POINT('Ctrl Pts',(1.76152089104537,-6.53616326397663,-11.7190472059354));
#44807=CARTESIAN_POINT('Ctrl Pts',(1.93321097312708,-6.48498144433591,-11.7106128708474));
#44808=CARTESIAN_POINT('Ctrl Pts',(2.10479764872785,-6.43383045077316,-11.7021836156387));
#44809=CARTESIAN_POINT('Ctrl Pts',(2.27443554992023,-6.37584064007484,-11.6937543604301));
#44810=CARTESIAN_POINT('Ctrl Pts',(2.44156308554208,-6.31118520559477,-11.6853251052214));
#44811=CARTESIAN_POINT('Ctrl Pts',(2.60861559874496,-6.24655879450139,-11.6768996338483));
#44812=CARTESIAN_POINT('Ctrl Pts',(2.77315968282938,-6.17527284576334,-11.6684741624753));
#44813=CARTESIAN_POINT('Ctrl Pts',(2.93465103840383,-6.09754969498366,-11.6600486911022));
#44814=CARTESIAN_POINT('Ctrl Pts',(3.09609465244811,-6.01984952142239,-11.6516257105429));
#44815=CARTESIAN_POINT('Ctrl Pts',(3.25448703761365,-5.93571608532095,-11.6432027299837));
#44816=CARTESIAN_POINT('Ctrl Pts',(3.40930557283041,-5.84541910482623,-11.6347797494244));
#44817=CARTESIAN_POINT('Ctrl Pts',(3.56412667152051,-5.75512062920109,-11.6263566293981));
#44818=CARTESIAN_POINT('Ctrl Pts',(3.71537351076483,-5.65865856750349,-11.6179335093717));
#44819=CARTESIAN_POINT('Ctrl Pts',(3.86254911897326,-5.55634801857469,-11.6095103893454));
#44820=CARTESIAN_POINT('Ctrl Pts',(4.00972981675929,-5.45403393157675,-11.6010869780335));
#44821=CARTESIAN_POINT('Ctrl Pts',(4.15283872885666,-5.34587114431071,-11.5926635667217));
#44822=CARTESIAN_POINT('Ctrl Pts',(4.2914087440828,-5.23221750228426,-11.5842401554098));
#44823=CARTESIAN_POINT('Ctrl Pts',(4.43000287691887,-5.11854407925251,-11.5758152780337));
#44824=CARTESIAN_POINT('Ctrl Pts',(4.5640562800505,-4.9993781076363,-11.5673904006576));
#44825=CARTESIAN_POINT('Ctrl Pts',(4.6931354683193,-4.87511727817941,-11.5589655232815));
#44826=CARTESIAN_POINT('Ctrl Pts',(4.82225512990375,-4.7508174862233,-11.55053800425));
#44827=CARTESIAN_POINT('Ctrl Pts',(4.94639722687289,-4.62141988261056,-11.5421104852186));
#44828=CARTESIAN_POINT('Ctrl Pts',(5.06516537921543,-4.48735876448467,-11.5336829661872));
#44829=CARTESIAN_POINT('Ctrl Pts',(5.18404003824691,-4.35317742552917,-11.5252478896824));
#44830=CARTESIAN_POINT('Ctrl Pts',(5.29753090195221,-4.21432446556266,-11.5168128131776));
#44831=CARTESIAN_POINT('Ctrl Pts',(5.40528139314174,-4.07126786897591,-11.5083777366728));
#44832=CARTESIAN_POINT('Ctrl Pts',(5.51308396085323,-3.92814213219398,-11.49993858344));
#44833=CARTESIAN_POINT('Ctrl Pts',(5.61514042889908,-3.78080897796015,-11.4914994302072));
#44834=CARTESIAN_POINT('Ctrl Pts',(5.71113748325057,-3.62976550859836,-11.4830602769744));
#44835=CARTESIAN_POINT('Ctrl Pts',(5.80724121724375,-3.47855418759468,-11.4746117454763));
#44836=CARTESIAN_POINT('Ctrl Pts',(5.89727191068491,-3.3236245984951,-11.4661632139782));
#44837=CARTESIAN_POINT('Ctrl Pts',(5.98096155049406,-3.16549963378796,-11.4577146824801));
#44838=CARTESIAN_POINT('Ctrl Pts',(6.02720279180377,-3.07813046041372,-11.4530465947143));
#44839=CARTESIAN_POINT('Ctrl Pts',(6.07150899249474,-2.98978616490185,-11.4483785069486));
#44840=CARTESIAN_POINT('Ctrl Pts',(6.11384123732871,-2.90055758859207,-11.4437104191828));
#44841=CARTESIAN_POINT('Ctrl Pts',(6.18857216521329,-2.74303855487194,-11.435469643586));
#44842=CARTESIAN_POINT('Ctrl Pts',(6.25731482406535,-2.58241210945067,-11.4272288679892));
#44843=CARTESIAN_POINT('Ctrl Pts',(6.31980203050053,-2.41917161344155,-11.4189880923925));
#44844=CARTESIAN_POINT('Ctrl Pts',(6.38222002558022,-2.25611192397901,-11.4107564443481));
#44845=CARTESIAN_POINT('Ctrl Pts',(6.4383962382608,-2.09044427844205,-11.4025247963037));
#44846=CARTESIAN_POINT('Ctrl Pts',(6.48810981337129,-1.92268563463587,-11.3942931482593));
#44847=CARTESIAN_POINT('Ctrl Pts',(6.53777718473113,-1.75508290555784,-11.386069150701));
#44848=CARTESIAN_POINT('Ctrl Pts',(6.58099377990189,-1.58539338761749,-11.3778451531427));
#44849=CARTESIAN_POINT('Ctrl Pts',(6.61758718147738,-1.41415306651943,-11.3696211555843));
#44850=CARTESIAN_POINT('Ctrl Pts',(6.65414825264026,-1.24306403691103,-11.3614044239598));
#44851=CARTESIAN_POINT('Ctrl Pts',(6.68409771903145,-1.07042728158184,-11.3531876923353));
#44852=CARTESIAN_POINT('Ctrl Pts',(6.70731329259347,-0.896792838396328,
-11.3449709607108));
#44853=CARTESIAN_POINT('Ctrl Pts',(6.73051697195755,-0.723247354565245,
-11.3367584388222));
#44854=CARTESIAN_POINT('Ctrl Pts',(6.74699358254226,-0.548705552672509,
-11.3285459169335));
#44855=CARTESIAN_POINT('Ctrl Pts',(6.75667204855774,-0.373726943420741,
-11.3203333950449));
#44856=CARTESIAN_POINT('Ctrl Pts',(6.76634727804768,-0.19880684785651,-11.312123619463));
#44857=CARTESIAN_POINT('Ctrl Pts',(6.76922887208773,-0.023450590776209,
-11.3039138438811));
#44858=CARTESIAN_POINT('Ctrl Pts',(6.7652976646355,0.151777827357827,-11.2957040682993));
#44859=CARTESIAN_POINT('Ctrl Pts',(6.76358061535384,0.228313047933185,-11.2921182516165));
#44860=CARTESIAN_POINT('Ctrl Pts',(6.76056454762015,0.304823847224531,-11.2885324349338));
#44861=CARTESIAN_POINT('Ctrl Pts',(6.75625098540567,0.381263192827391,-11.2849466182511));
#44862=CARTESIAN_POINT('Ctrl Pts',(6.745594381192,0.570105688180169,-11.2760879007293));
#44863=CARTESIAN_POINT('Ctrl Pts',(6.72702648891292,0.758316202631355,-11.2672291832076));
#44864=CARTESIAN_POINT('Ctrl Pts',(6.70065597101318,0.945250526646458,-11.2583704656858));
#44865=CARTESIAN_POINT('Ctrl Pts',(6.67423611810987,1.13253457475795,-11.2494951749264));
#44866=CARTESIAN_POINT('Ctrl Pts',(6.63998450378622,1.31853740427817,-11.240619884167));
#44867=CARTESIAN_POINT('Ctrl Pts',(6.59806070560644,1.50262567698419,-11.2317445934075));
#44868=CARTESIAN_POINT('Ctrl Pts',(6.55601783441344,1.6872368017762,-11.2228440948268));
#44869=CARTESIAN_POINT('Ctrl Pts',(6.50625923139748,1.86992223365413,-11.213943596246));
#44870=CARTESIAN_POINT('Ctrl Pts',(6.44899502480975,2.05006150395033,-11.2050430976653));
#44871=CARTESIAN_POINT('Ctrl Pts',(6.39165329958869,2.23044462901855,-11.1961305504676));
#44872=CARTESIAN_POINT('Ctrl Pts',(6.3267857597072,2.40827446230105,-11.18721800327));
#44873=CARTESIAN_POINT('Ctrl Pts',(6.25465097536171,2.58294989816039,-11.1783054560723));
#44874=CARTESIAN_POINT('Ctrl Pts',(6.18235691036745,2.75801103444154,-11.1693732291001));
#44875=CARTESIAN_POINT('Ctrl Pts',(6.10276360407996,2.92990360102342,-11.1604410021278));
#44876=CARTESIAN_POINT('Ctrl Pts',(6.01617719747231,3.09804792225915,-11.1515087751555));
#44877=CARTESIAN_POINT('Ctrl Pts',(5.93434304458952,3.25696372243466,-11.1430667892102));
#44878=CARTESIAN_POINT('Ctrl Pts',(5.84626283162006,3.41253148605386,-11.134624803265));
#44879=CARTESIAN_POINT('Ctrl Pts',(5.75223081267895,3.56428529689571,-11.1261828173197));
#44880=CARTESIAN_POINT('Ctrl Pts',(5.66063148459453,3.71211310346517,-11.1179592329599));
#44881=CARTESIAN_POINT('Ctrl Pts',(5.56320847393852,3.8566035721493,-11.1097356486001));
#44882=CARTESIAN_POINT('Ctrl Pts',(5.46023223800644,3.9972681805247,-11.1015120642403));
#44883=CARTESIAN_POINT('Ctrl Pts',(5.35736011285873,4.13779057450879,-11.0932967940688));
#44884=CARTESIAN_POINT('Ctrl Pts',(5.24894615066667,4.27449452244008,-11.0850815238973));
#44885=CARTESIAN_POINT('Ctrl Pts',(5.13530562095612,4.40691787753941,-11.0768662537259));
#44886=CARTESIAN_POINT('Ctrl Pts',(5.02175933092625,4.53923141675941,-11.0686577963037));
#44887=CARTESIAN_POINT('Ctrl Pts',(4.90299533665791,4.66727116144228,-11.0604493388815));
#44888=CARTESIAN_POINT('Ctrl Pts',(4.77937098021986,4.79060560194974,-11.0522408814593));
#44889=CARTESIAN_POINT('Ctrl Pts',(4.65583332537734,4.91385354418871,-11.0440381808829));
#44890=CARTESIAN_POINT('Ctrl Pts',(4.52744235295573,5.03240250484075,-11.0358354803064));
#44891=CARTESIAN_POINT('Ctrl Pts',(4.39459426022936,5.14585564196657,-11.02763277973));
#44892=CARTESIAN_POINT('Ctrl Pts',(4.26180254935955,5.25926062861938,-11.0194335604493));
#44893=CARTESIAN_POINT('Ctrl Pts',(4.12455775784663,5.36757386679171,-11.0112343411685));
#44894=CARTESIAN_POINT('Ctrl Pts',(3.98329151703703,5.47043670014569,-11.0030351218877));
#44895=CARTESIAN_POINT('Ctrl Pts',(3.84203836885357,5.57329000012062,-10.9948366625147));
#44896=CARTESIAN_POINT('Ctrl Pts',(3.69676479861999,5.67069368391839,-10.9866382031417));
#44897=CARTESIAN_POINT('Ctrl Pts',(3.54793421467625,5.76233041471327,-10.9784397437687));
#44898=CARTESIAN_POINT('Ctrl Pts',(3.40160079849206,5.85242961011947,-10.9703788430069));
#44899=CARTESIAN_POINT('Ctrl Pts',(3.25182909134223,5.93695369163598,-10.962317942245));
#44900=CARTESIAN_POINT('Ctrl Pts',(3.0990855038472,6.01564277861013,-10.9542570414832));
#44901=CARTESIAN_POINT('Ctrl Pts',(3.09908550384713,6.01564277861016,-12.9539582652632));
#44902=CARTESIAN_POINT('Ctrl Pts',(2.94677792813768,6.09410724489889,-12.9459132820467));
#44903=CARTESIAN_POINT('Ctrl Pts',(2.7913481699967,6.16685580942879,-12.9378682988301));
#44904=CARTESIAN_POINT('Ctrl Pts',(2.6332745528485,6.23363089453655,-12.9298233156135));
#44905=CARTESIAN_POINT('Ctrl Pts',(2.47528686967876,6.30036967852823,-12.9217827059125));
#44906=CARTESIAN_POINT('Ctrl Pts',(2.31465853174747,6.36114130317295,-12.9137420962114));
#44907=CARTESIAN_POINT('Ctrl Pts',(2.15189080981932,6.41573494952957,-12.9057014865103));
#44908=CARTESIAN_POINT('Ctrl Pts',(1.98915021135736,6.47031949845026,-12.8976622166892));
#44909=CARTESIAN_POINT('Ctrl Pts',(1.82427128925733,6.51872799142564,-12.8896229468681));
#44910=CARTESIAN_POINT('Ctrl Pts',(1.65777370470937,6.56079837702502,-12.8815836770469));
#44911=CARTESIAN_POINT('Ctrl Pts',(1.49128530389774,6.60286644209027,-12.8735448506589));
#44912=CARTESIAN_POINT('Ctrl Pts',(1.32317878006311,6.63859700283098,-12.8655060242708));
#44913=CARTESIAN_POINT('Ctrl Pts',(1.15398703298249,6.66787844278135,-12.8574671978827));
#44914=CARTESIAN_POINT('Ctrl Pts',(0.984771124091398,6.69716406433405,-12.8494272234919));
#44915=CARTESIAN_POINT('Ctrl Pts',(0.814470051410564,6.71999866778069,-12.841387249101));
#44916=CARTESIAN_POINT('Ctrl Pts',(0.643624789566233,6.73632215160883,-12.8333472747101));
#44917=CARTESIAN_POINT('Ctrl Pts',(0.472721299876386,6.75265119884145,-12.8253045601181));
#44918=CARTESIAN_POINT('Ctrl Pts',(0.301273623332456,6.76246467383177,-12.8172618455261));
#44919=CARTESIAN_POINT('Ctrl Pts',(0.129825561801393,6.76575452728688,-12.809219130934));
#44920=CARTESIAN_POINT('Ctrl Pts',(-0.0418248302162636,6.76904826318689,
-12.8011669249174));
#44921=CARTESIAN_POINT('Ctrl Pts',(-0.213475234481144,6.76580299376193,
-12.7931147189007));
#44922=CARTESIAN_POINT('Ctrl Pts',(-0.384583255898232,6.75606281196991,
-12.785062512884));
#44923=CARTESIAN_POINT('Ctrl Pts',(-0.555794869911432,6.74631673325552,
-12.777005431883));
#44924=CARTESIAN_POINT('Ctrl Pts',(-0.726463076460481,6.73006794642621,
-12.7689483508819));
#44925=CARTESIAN_POINT('Ctrl Pts',(-0.896053401502798,6.70741211658083,
-12.7608912698809));
#44926=CARTESIAN_POINT('Ctrl Pts',(-1.06592357492262,6.68471890136442,-12.7528208935398));
#44927=CARTESIAN_POINT('Ctrl Pts',(-1.23471194646283,6.65559758535737,-12.7447505171987));
#44928=CARTESIAN_POINT('Ctrl Pts',(-1.40189580009872,6.62019464711315,-12.7366801408576));
#44929=CARTESIAN_POINT('Ctrl Pts',(-1.55974503709853,6.58676841205595,-12.72906036945));
#44930=CARTESIAN_POINT('Ctrl Pts',(-1.71616380877214,6.54774295278436,-12.7214405980424));
#44931=CARTESIAN_POINT('Ctrl Pts',(-1.87072815952014,6.50328110673208,-12.7138208266348));
#44932=CARTESIAN_POINT('Ctrl Pts',(-2.03977719211289,6.45465260975944,-12.7054869839421));
#44933=CARTESIAN_POINT('Ctrl Pts',(-2.20714519044762,6.39936626702175,-12.6971531412494));
#44934=CARTESIAN_POINT('Ctrl Pts',(-2.37227764169204,6.33755377024354,-12.6888192985568));
#44935=CARTESIAN_POINT('Ctrl Pts',(-2.53721546345172,6.27581412731269,-12.680495278352));
#44936=CARTESIAN_POINT('Ctrl Pts',(-2.69992266403518,6.20756377420348,-12.6721712581472));
#44937=CARTESIAN_POINT('Ctrl Pts',(-2.85985813155339,6.13298462963898,-12.6638472379425));
#44938=CARTESIAN_POINT('Ctrl Pts',(-3.01963441882481,6.05847971205377,-12.6555315024516));
#44939=CARTESIAN_POINT('Ctrl Pts',(-3.17664415587532,5.97765869862999,-12.6472157669608));
#44940=CARTESIAN_POINT('Ctrl Pts',(-3.33036431251776,5.89075229031981,-12.6389000314699));
#44941=CARTESIAN_POINT('Ctrl Pts',(-3.48395964037755,5.80391645454476,-12.6305910487899));
#44942=CARTESIAN_POINT('Ctrl Pts',(-3.63427040917541,5.71100524105929,-12.6222820661099));
#44943=CARTESIAN_POINT('Ctrl Pts',(-3.78079619131092,5.612296246615,-12.6139730834298));
#44944=CARTESIAN_POINT('Ctrl Pts',(-3.92722981943772,5.51364933291447,-12.6056693264927));
#44945=CARTESIAN_POINT('Ctrl Pts',(-4.06988291727517,5.40921209889775,-12.5973655695555));
#44946=CARTESIAN_POINT('Ctrl Pts',(-4.2082819792181,5.2993067266755,-12.5890618126184));
#44947=CARTESIAN_POINT('Ctrl Pts',(-4.34662485447842,5.18944597338477,-12.5807614268064));
#44948=CARTESIAN_POINT('Ctrl Pts',(-4.48071686314835,5.07412172123556,-12.5724610409943));
#44949=CARTESIAN_POINT('Ctrl Pts',(-4.61011544752674,4.95369806916765,-12.5641606551823));
#44950=CARTESIAN_POINT('Ctrl Pts',(-4.73948674511074,4.83329981131445,-12.5558620197057));
#44951=CARTESIAN_POINT('Ctrl Pts',(-4.86416633571904,4.70780453266443,-12.547563384229));
#44952=CARTESIAN_POINT('Ctrl Pts',(-4.9837464045838,4.57761518421962,-12.5392647487524));
#44953=CARTESIAN_POINT('Ctrl Pts',(-5.1033211060424,4.44743167938335,-12.5309664857638));
#44954=CARTESIAN_POINT('Ctrl Pts',(-5.21779650676553,4.31255478085536,-12.5226682227752));
#44955=CARTESIAN_POINT('Ctrl Pts',(-5.32680305458562,4.17342284194369,-12.5143699597866));
#44956=CARTESIAN_POINT('Ctrl Pts',(-5.43582280263355,4.03427405474785,-12.5060706919138));
#44957=CARTESIAN_POINT('Ctrl Pts',(-5.53937216415358,3.8908694745588,-12.497771424041));
#44958=CARTESIAN_POINT('Ctrl Pts',(-5.63712301861594,3.74367908253236,-12.4894721561681));
#44959=CARTESIAN_POINT('Ctrl Pts',(-5.7349425099331,3.59638533912734,-12.4811670608716));
#44960=CARTESIAN_POINT('Ctrl Pts',(-5.82695516600972,3.44530076230277,-12.4728619655751));
#44961=CARTESIAN_POINT('Ctrl Pts',(-5.9128767422217,3.29092352255317,-12.4645568702786));
#44962=CARTESIAN_POINT('Ctrl Pts',(-5.99882964990834,3.13648998883422,-12.4562487465125));
#44963=CARTESIAN_POINT('Ctrl Pts',(-6.07868688808047,2.97876170651755,-12.4479406227464));
#44964=CARTESIAN_POINT('Ctrl Pts',(-6.15221095237008,2.81825999466651,-12.4396324989803));
#44965=CARTESIAN_POINT('Ctrl Pts',(-6.22581317231511,2.65758767042335,-12.4313155437266));
#44966=CARTESIAN_POINT('Ctrl Pts',(-6.2930686295534,2.49413634575469,-12.4229985884729));
#44967=CARTESIAN_POINT('Ctrl Pts',(-6.35378819641643,2.32844681173507,-12.4146816332192));
#44968=CARTESIAN_POINT('Ctrl Pts',(-6.39853759336842,2.20633614606845,-12.4085521637367));
#44969=CARTESIAN_POINT('Ctrl Pts',(-6.43973806006985,2.0830101980983,-12.4024226942542));
#44970=CARTESIAN_POINT('Ctrl Pts',(-6.47733142606586,1.95869002062594,-12.3962932247717));
#44971=CARTESIAN_POINT('Ctrl Pts',(-6.53293815762291,1.77480016259717,-12.3872267377714));
#44972=CARTESIAN_POINT('Ctrl Pts',(-6.58073898742956,1.5884447635909,-12.378160250771));
#44973=CARTESIAN_POINT('Ctrl Pts',(-6.62053851835857,1.40027094768494,-12.3690937637707));
#44974=CARTESIAN_POINT('Ctrl Pts',(-6.66028028210385,1.21237025739489,-12.3600404363581));
#44975=CARTESIAN_POINT('Ctrl Pts',(-6.69204387419446,1.0226566416069,-12.3509871089456));
#44976=CARTESIAN_POINT('Ctrl Pts',(-6.71568417086439,0.831790308432012,
-12.341933781533));
#44977=CARTESIAN_POINT('Ctrl Pts',(-6.73926725371455,0.641385906515465,
-12.3329023648202));
#44978=CARTESIAN_POINT('Ctrl Pts',(-6.75476624873634,0.449834583210811,
-12.3238709481074));
#44979=CARTESIAN_POINT('Ctrl Pts',(-6.7620873952382,0.257804303999635,-12.3148395313947));
#44980=CARTESIAN_POINT('Ctrl Pts',(-6.76533513846844,0.172617504479535,
-12.3108330929931));
#44981=CARTESIAN_POINT('Ctrl Pts',(-6.7669742244786,0.0873365959912321,
-12.3068266545915));
#44982=CARTESIAN_POINT('Ctrl Pts',(-6.76699969835621,0.00202050660550186,
-12.30282021619));
#44983=CARTESIAN_POINT('',(-6.76699999341342,0.000298567942575067,-12.6971797837809));
#44984=CARTESIAN_POINT('Ctrl Pts',(3.09908550384717,6.01564277861014,-13.3487674371071));
#44985=CARTESIAN_POINT('Ctrl Pts',(2.93969369619203,6.09775683669425,-13.3403258001161));
#44986=CARTESIAN_POINT('Ctrl Pts',(2.77720452294419,6.17344477825237,-13.3318841631251));
#44987=CARTESIAN_POINT('Ctrl Pts',(2.6121936832283,6.24249414587648,-13.323442526134));
#44988=CARTESIAN_POINT('Ctrl Pts',(2.44720086633562,6.31153597178669,-13.315001811156));
#44989=CARTESIAN_POINT('Ctrl Pts',(2.27934724675824,6.37408352589492,-13.3065610961779));
#44990=CARTESIAN_POINT('Ctrl Pts',(2.10917205664407,6.42990530532696,-13.2981203811998));
#44991=CARTESIAN_POINT('Ctrl Pts',(1.93912549295624,6.48568489202812,-13.2896860461118));
#44992=CARTESIAN_POINT('Ctrl Pts',(1.76676117239651,6.53474873447013,-13.2812517110237));
#44993=CARTESIAN_POINT('Ctrl Pts',(1.59263717699892,6.57691385244181,-13.2728173759357));
#44994=CARTESIAN_POINT('Ctrl Pts',(1.41861805399358,6.61905357496594,-13.2643881207271));
#44995=CARTESIAN_POINT('Ctrl Pts',(1.24284169231492,6.65430277836938,-13.2559588655185));
#44996=CARTESIAN_POINT('Ctrl Pts',(1.06588055273195,6.68252853696173,-13.2475296103098));
#44997=CARTESIAN_POINT('Ctrl Pts',(0.888998849806665,6.71074162520211,-13.2391041389368));
#44998=CARTESIAN_POINT('Ctrl Pts',(0.710933758113983,6.73193750250743,-13.2306786675638));
#44999=CARTESIAN_POINT('Ctrl Pts',(0.532267523909018,6.74603441163709,-13.2222531961908));
#45000=CARTESIAN_POINT('Ctrl Pts',(0.353654108626332,6.76012715331144,-13.2138302156315));
#45001=CARTESIAN_POINT('Ctrl Pts',(0.174440237263183,6.76712508582163,-13.2054072350723));
#45002=CARTESIAN_POINT('Ctrl Pts',(-0.00478673464667945,6.76699830701704,
-13.1969842545131));
#45003=CARTESIAN_POINT('Ctrl Pts',(-0.184016674183397,6.76687152611325,
-13.1885611344867));
#45004=CARTESIAN_POINT('Ctrl Pts',(-0.363259381365447,6.75961979181696,
-13.1801380144604));
#45005=CARTESIAN_POINT('Ctrl Pts',(-0.541926830466349,6.74526532542796,
-13.1717148944341));
#45006=CARTESIAN_POINT('Ctrl Pts',(-0.720600458185537,6.73091036263757,
-13.1632914831222));
#45007=CARTESIAN_POINT('Ctrl Pts',(-0.898698455710701,6.70945220455209,
-13.1548680718104));
#45008=CARTESIAN_POINT('Ctrl Pts',(-1.07563709152317,6.68096503862575,-13.1464446604985));
#45009=CARTESIAN_POINT('Ctrl Pts',(-1.25260652286495,6.65247291461126,-13.1380197831224));
#45010=CARTESIAN_POINT('Ctrl Pts',(-1.42841586095319,6.61694939672042,-13.1295949057463));
#45011=CARTESIAN_POINT('Ctrl Pts',(-1.60249038261121,6.5745200261037,-13.1211700283702));
#45012=CARTESIAN_POINT('Ctrl Pts',(-1.77661948605881,6.53207735158152,-13.1127425093387));
#45013=CARTESIAN_POINT('Ctrl Pts',(-1.94901236469206,6.48272458613518,-13.1043149903073));
#45014=CARTESIAN_POINT('Ctrl Pts',(-2.11910794001518,6.42663757641308,-13.0958874712759));
#45015=CARTESIAN_POINT('Ctrl Pts',(-2.28935605047631,6.37050027002835,-13.0874523947711));
#45016=CARTESIAN_POINT('Ctrl Pts',(-2.45730242416982,6.30761675709199,-13.0790173182663));
#45017=CARTESIAN_POINT('Ctrl Pts',(-2.62240342745077,6.23821202458641,-13.0705822417615));
#45018=CARTESIAN_POINT('Ctrl Pts',(-2.78758422513324,6.16877374831681,-13.0621430885287));
#45019=CARTESIAN_POINT('Ctrl Pts',(-2.94991660570296,6.09280810328691,-13.053703935296));
#45020=CARTESIAN_POINT('Ctrl Pts',(-3.10887966997177,6.01058700940567,-13.0452647820632));
#45021=CARTESIAN_POINT('Ctrl Pts',(-3.26801938677344,5.92827454483681,-13.0368162505651));
#45022=CARTESIAN_POINT('Ctrl Pts',(-3.42378201332264,5.83969290164503,-13.028367719067));
#45023=CARTESIAN_POINT('Ctrl Pts',(-3.57567282042132,5.74515908233186,-13.0199191875689));
#45024=CARTESIAN_POINT('Ctrl Pts',(-3.65959741945254,5.69292608000412,-13.0152510998029));
#45025=CARTESIAN_POINT('Ctrl Pts',(-3.74234050073199,5.63887669082813,-13.0105830120369));
#45026=CARTESIAN_POINT('Ctrl Pts',(-3.82382272336077,5.58306983480503,-13.005914924271));
#45027=CARTESIAN_POINT('Ctrl Pts',(-3.96766678659879,5.48455159772313,-12.9976741486742));
#45028=CARTESIAN_POINT('Ctrl Pts',(-4.10789963213892,5.38033472218766,-12.9894333730775));
#45029=CARTESIAN_POINT('Ctrl Pts',(-4.24404210803553,5.27071110811637,-12.9811925974807));
#45030=CARTESIAN_POINT('Ctrl Pts',(-4.38003379138044,5.16120891408231,-12.9729609494363));
#45031=CARTESIAN_POINT('Ctrl Pts',(-4.51194385150957,5.0463121269841,-12.964729301392));
#45032=CARTESIAN_POINT('Ctrl Pts',(-4.63932129795759,4.92635635072385,-12.9564976533476));
#45033=CARTESIAN_POINT('Ctrl Pts',(-4.7665803599245,4.80651206125127,-12.9482736557893));
#45034=CARTESIAN_POINT('Ctrl Pts',(-4.88931494026081,4.68161838892821,-12.940049658231));
#45035=CARTESIAN_POINT('Ctrl Pts',(-5.00710633201655,4.55205175496498,-12.9318256606727));
#45036=CARTESIAN_POINT('Ctrl Pts',(-5.12479365462031,4.42259959362595,-12.9236089290482));
#45037=CARTESIAN_POINT('Ctrl Pts',(-5.23754625476821,4.28848296159373,-12.9153921974237));
#45038=CARTESIAN_POINT('Ctrl Pts',(-5.34498167464297,4.15011564871762,-12.9071754657992));
#45039=CARTESIAN_POINT('Ctrl Pts',(-5.45236205137442,4.01181922653882,-12.8989629439105));
#45040=CARTESIAN_POINT('Ctrl Pts',(-5.55443045567882,3.8692767411272,-12.8907504220219));
#45041=CARTESIAN_POINT('Ctrl Pts',(-5.65084391902132,3.72293593859199,-12.8825379001332));
#45042=CARTESIAN_POINT('Ctrl Pts',(-5.74722514123779,3.57664407312525,-12.8743281245513));
#45043=CARTESIAN_POINT('Ctrl Pts',(-5.83795499414237,3.42655671765138,-12.8661183489695));
#45044=CARTESIAN_POINT('Ctrl Pts',(-5.92273310871932,3.27315161929294,-12.8579085733877));
#45045=CARTESIAN_POINT('Ctrl Pts',(-5.95976198661663,3.20614825782064,-12.8543227567049));
#45046=CARTESIAN_POINT('Ctrl Pts',(-5.99565600464417,3.13851233139998,-12.8507369400221));
#45047=CARTESIAN_POINT('Ctrl Pts',(-6.03039281295659,3.07028525082631,-12.8471511233393));
#45048=CARTESIAN_POINT('Ctrl Pts',(-6.11507093287449,2.90396769918182,-12.8384099571292));
#45049=CARTESIAN_POINT('Ctrl Pts',(-6.19279029492635,2.73429120459534,-12.8296687909191));
#45050=CARTESIAN_POINT('Ctrl Pts',(-6.26332310264359,2.56184947096645,-12.820927624709));
#45051=CARTESIAN_POINT('Ctrl Pts',(-6.33396409351821,2.38914324636079,-12.812173051306));
#45052=CARTESIAN_POINT('Ctrl Pts',(-6.39739640571944,2.21366356988124,-12.8034184779029));
#45053=CARTESIAN_POINT('Ctrl Pts',(-6.45344171234111,2.03602039906673,-12.7946639044999));
#45054=CARTESIAN_POINT('Ctrl Pts',(-6.50962377189001,1.85794377137464,-12.7858879695661));
#45055=CARTESIAN_POINT('Ctrl Pts',(-6.55838268520997,1.67769335789036,-12.7771120346324));
#45056=CARTESIAN_POINT('Ctrl Pts',(-6.59959037899519,1.49589298730698,-12.7683360996986));
#45057=CARTESIAN_POINT('Ctrl Pts',(-6.6408491657772,1.31386720430911,-12.7595492835732));
#45058=CARTESIAN_POINT('Ctrl Pts',(-6.6745379815588,1.13028790139143,-12.7507624674477));
#45059=CARTESIAN_POINT('Ctrl Pts',(-6.70058035367453,0.94578640503599,-12.7419756513222));
#45060=CARTESIAN_POINT('Ctrl Pts',(-6.72667643939347,0.760904365766798,
-12.73317071198));
#45061=CARTESIAN_POINT('Ctrl Pts',(-6.74509450769083,0.575096608282414,
-12.7243657726378));
#45062=CARTESIAN_POINT('Ctrl Pts',(-6.75580998387632,0.388999308170436,
-12.7155608332956));
#45063=CARTESIAN_POINT('Ctrl Pts',(-6.76326646901383,0.259501399874452,
-12.7094338168004));
#45064=CARTESIAN_POINT('Ctrl Pts',(-6.76699427685383,0.129863310485216,
-12.7033068003053));
#45065=CARTESIAN_POINT('Ctrl Pts',(-6.76699999341339,0.000298568560796373,
-12.6971797838101));
#45066=CARTESIAN_POINT('Ctrl Pts',(-6.76699999341342,0.000298567942480405,
-12.6971797837809));
#45067=CARTESIAN_POINT('Ctrl Pts',(-6.76700272788868,-0.061677925269276,
-12.6942489633232));
#45068=CARTESIAN_POINT('Ctrl Pts',(-6.76615404016013,-0.123652304761972,
-12.6913181428656));
#45069=CARTESIAN_POINT('Ctrl Pts',(-6.76445405791803,-0.185607915553967,
-12.6883873224079));
#45070=CARTESIAN_POINT('Ctrl Pts',(-6.75968385425956,-0.359457308767372,
-12.6801633479904));
#45071=CARTESIAN_POINT('Ctrl Pts',(-6.74820101348188,-0.533353174028972,
-12.6719393735728));
#45072=CARTESIAN_POINT('Ctrl Pts',(-6.72999343021052,-0.706737171318463,
-12.6637153991552));
#45073=CARTESIAN_POINT('Ctrl Pts',(-6.71180507591366,-0.879938058284459,
-12.6555001100526));
#45074=CARTESIAN_POINT('Ctrl Pts',(-6.68690615869465,-1.05262780007581,
-12.6472848209499));
#45075=CARTESIAN_POINT('Ctrl Pts',(-6.65533657408663,-1.22424837579018,
-12.6390695318473));
#45076=CARTESIAN_POINT('Ctrl Pts',(-6.62379399783722,-1.39572212695454,
-12.6308612710751));
#45077=CARTESIAN_POINT('Ctrl Pts',(-6.58559218453351,-1.56612818305414,
-12.622653010303));
#45078=CARTESIAN_POINT('Ctrl Pts',(-6.54082279672109,-1.73491387160682,
-12.6144447495308));
#45079=CARTESIAN_POINT('Ctrl Pts',(-6.49608273271306,-1.90358900607873,
-12.6062418651429));
#45080=CARTESIAN_POINT('Ctrl Pts',(-6.44478375441965,-2.07064554170197,
-12.598038980755));
#45081=CARTESIAN_POINT('Ctrl Pts',(-6.38706856280714,-2.23554113672747,
-12.5898360963672));
#45082=CARTESIAN_POINT('Ctrl Pts',(-6.32937960368294,-2.40036178403733,
-12.581636940323));
#45083=CARTESIAN_POINT('Ctrl Pts',(-6.26528035943658,-2.56302310974894,
-12.5734377842788));
#45084=CARTESIAN_POINT('Ctrl Pts',(-6.19496335339311,-2.72299798937062,
-12.5652386282345));
#45085=CARTESIAN_POINT('Ctrl Pts',(-6.12465246321934,-2.88295895506771,
-12.5570401853175));
#45086=CARTESIAN_POINT('Ctrl Pts',(-6.04812502480654,-3.04023360861682,
-12.5488417424005));
#45087=CARTESIAN_POINT('Ctrl Pts',(-5.96562181692079,-3.19431453327293,
-12.5406432994835));
#45088=CARTESIAN_POINT('Ctrl Pts',(-5.8831194306693,-3.34839392346549,-12.5324449382133));
#45089=CARTESIAN_POINT('Ctrl Pts',(-5.79464156186918,-3.49927933139718,
-12.5242465769431));
#45090=CARTESIAN_POINT('Ctrl Pts',(-5.70047503863014,-3.64648780800851,
-12.5160482156728));
#45091=CARTESIAN_POINT('Ctrl Pts',(-5.60629234715482,-3.79372156007178,
-12.5078484467576));
#45092=CARTESIAN_POINT('Ctrl Pts',(-5.50641924859686,-3.93727682086154,
-12.4996486778423));
#45093=CARTESIAN_POINT('Ctrl Pts',(-5.40118602410122,-4.07669946562825,
-12.491448908927));
#45094=CARTESIAN_POINT('Ctrl Pts',(-5.29591561466701,-4.21617137641819,
-12.4832462425627));
#45095=CARTESIAN_POINT('Ctrl Pts',(-5.18528152229535,-4.35150747613821,
-12.4750435761983));
#45096=CARTESIAN_POINT('Ctrl Pts',(-5.06965446303003,-4.48228653986776,
-12.466840909834));
#45097=CARTESIAN_POINT('Ctrl Pts',(-4.95389608032675,-4.61321413592504,
-12.458628927291));
#45098=CARTESIAN_POINT('Ctrl Pts',(-4.83313363948699,-4.73957408704741,
-12.450416944748));
#45099=CARTESIAN_POINT('Ctrl Pts',(-4.70777562722417,-4.86098114002863,
-12.442204962205));
#45100=CARTESIAN_POINT('Ctrl Pts',(-4.5823436771115,-4.98245980053052,-12.4339881361237));
#45101=CARTESIAN_POINT('Ctrl Pts',(-4.45231101921201,-5.09897950075,-12.4257713100424));
#45102=CARTESIAN_POINT('Ctrl Pts',(-4.3181193068555,-5.21019526042564,-12.417554483961));
#45103=CARTESIAN_POINT('Ctrl Pts',(-4.18372065149776,-5.32158253086515,
-12.4093249863472));
#45104=CARTESIAN_POINT('Ctrl Pts',(-4.04515040909436,-5.42764929742197,
-12.4010954887333));
#45105=CARTESIAN_POINT('Ctrl Pts',(-3.90288037585503,-5.5280931406558,-12.3928659911195));
#45106=CARTESIAN_POINT('Ctrl Pts',(-3.77606693016552,-5.61762450273365,
-12.3855305675946));
#45107=CARTESIAN_POINT('Ctrl Pts',(-3.64631447432866,-5.702688886801,-12.3781951440698));
#45108=CARTESIAN_POINT('Ctrl Pts',(-3.51397284577488,-5.78310330524683,
-12.3708597205449));
#45109=CARTESIAN_POINT('Ctrl Pts',(-3.3683626978814,-5.87158004148336,-12.3627888503585));
#45110=CARTESIAN_POINT('Ctrl Pts',(-3.21914287105219,-5.95471530131142,
-12.3547179801721));
#45111=CARTESIAN_POINT('Ctrl Pts',(-3.06674998333667,-6.03219143758755,
-12.3466471099857));
#45112=CARTESIAN_POINT('Ctrl Pts',(-2.91454673672493,-6.10957116083403,
-12.3385862833699));
#45113=CARTESIAN_POINT('Ctrl Pts',(-2.75917861433286,-6.18130560612759,
-12.3305254567541));
#45114=CARTESIAN_POINT('Ctrl Pts',(-2.60111182744723,-6.24711983726214,
-12.3224646301383));
#45115=CARTESIAN_POINT('Ctrl Pts',(-2.44320708075705,-6.31286659975836,
-12.3144120669784));
#45116=CARTESIAN_POINT('Ctrl Pts',(-2.28260951646843,-6.37270508353508,
-12.3063595038185));
#45117=CARTESIAN_POINT('Ctrl Pts',(-2.11981052260914,-6.426405865508,-12.2983069406586));
#45118=CARTESIAN_POINT('Ctrl Pts',(-1.95714277316589,-6.48006335527373,
-12.2902608692707));
#45119=CARTESIAN_POINT('Ctrl Pts',(-1.79227747893726,-6.5275928753536,-12.2822147978828));
#45120=CARTESIAN_POINT('Ctrl Pts',(-1.62572652144183,-6.56881285145807,
-12.2741687264949));
#45121=CARTESIAN_POINT('Ctrl Pts',(-1.45927340197547,-6.61000861346446,
-12.266127381659));
#45122=CARTESIAN_POINT('Ctrl Pts',(-1.29113695165918,-6.64490212063055,
-12.2580860368232));
#45123=CARTESIAN_POINT('Ctrl Pts',(-1.12184464548294,-6.67336149113783,
-12.2500446919873));
#45124=CARTESIAN_POINT('Ctrl Pts',(-0.949288904556731,-6.70236947073888,
-12.2418483347662));
#45125=CARTESIAN_POINT('Ctrl Pts',(-0.775532667203259,-6.72469259987832,
-12.2336519775452));
#45126=CARTESIAN_POINT('Ctrl Pts',(-0.601146366280044,-6.74024569628647,
-12.2254556203241));
#45127=CARTESIAN_POINT('Ctrl Pts',(-0.430112504654712,-6.75549979666497,
-12.2174168316156));
#45128=CARTESIAN_POINT('Ctrl Pts',(-0.258472971865798,-6.7642417877685,
-12.2093780429071));
#45129=CARTESIAN_POINT('Ctrl Pts',(-0.0867715089438693,-6.76644365270528,
-12.2013392541986));
#45130=CARTESIAN_POINT('Ctrl Pts',(0.0849483275902528,-6.76864575326156,
-12.1932996052669));
#45131=CARTESIAN_POINT('Ctrl Pts',(0.25672973398804,-6.76430632924852,-12.1852599563352));
#45132=CARTESIAN_POINT('Ctrl Pts',(0.428028892403548,-6.75344950875238,
-12.1772203074034));
#45133=CARTESIAN_POINT('Ctrl Pts',(0.599380299268728,-6.74258937678616,
-12.1691782062752));
#45134=CARTESIAN_POINT('Ctrl Pts',(0.770248792854648,-6.72520791505771,
-12.1611361051471));
#45135=CARTESIAN_POINT('Ctrl Pts',(0.940095746729051,-6.70138112533394,
-12.1530940040189));
#45136=CARTESIAN_POINT('Ctrl Pts',(1.11567436798678,-6.67675027506981,-12.1447805135741));
#45137=CARTESIAN_POINT('Ctrl Pts',(1.29016086458142,-6.64523153704258,-12.1364670231294));
#45138=CARTESIAN_POINT('Ctrl Pts',(1.46297285585442,-6.60696597713604,-12.1281535326846));
#45139=CARTESIAN_POINT('Ctrl Pts',(1.63043798425864,-6.56988436690748,-12.1200972645139));
#45140=CARTESIAN_POINT('Ctrl Pts',(1.79633034633245,-6.52646737970495,-12.1120409963431));
#45141=CARTESIAN_POINT('Ctrl Pts',(1.96013700431782,-6.47689369407156,-12.1039847281724));
#45142=CARTESIAN_POINT('Ctrl Pts',(2.13178874395328,-6.4249458093899,-12.0955426265906));
#45143=CARTESIAN_POINT('Ctrl Pts',(2.30114962883959,-6.36623716666166,-12.0871005250089));
#45144=CARTESIAN_POINT('Ctrl Pts',(2.46765538209628,-6.30102895686183,-12.0786584234271));
#45145=CARTESIAN_POINT('Ctrl Pts',(2.63416113535291,-6.23582074706202,-12.0702163218454));
#45146=CARTESIAN_POINT('Ctrl Pts',(2.79781136955294,-6.16411323435529,-12.0617742202636));
#45147=CARTESIAN_POINT('Ctrl Pts',(2.95807432651015,-6.08622093575657,-12.0533321186819));
#45148=CARTESIAN_POINT('Ctrl Pts',(3.11628212107551,-6.00932750380635,-12.0449982759892));
#45149=CARTESIAN_POINT('Ctrl Pts',(3.27169222448777,-5.92616305035882,-12.0366644332965));
#45150=CARTESIAN_POINT('Ctrl Pts',(3.42378091540367,-5.8369523934428,-12.0283305906038));
#45151=CARTESIAN_POINT('Ctrl Pts',(3.5756903505566,-5.74784688257198,-12.0200065703991));
#45152=CARTESIAN_POINT('Ctrl Pts',(3.72428587417744,-5.65270953879435,-12.0116825501943));
#45153=CARTESIAN_POINT('Ctrl Pts',(3.86906557931096,-5.5518123656146,-12.0033585299896));
#45154=CARTESIAN_POINT('Ctrl Pts',(4.01370118839411,-5.45101561316809,-11.9950427944987));
#45155=CARTESIAN_POINT('Ctrl Pts',(4.15452826186678,-5.34447065028088,-11.9867270590079));
#45156=CARTESIAN_POINT('Ctrl Pts',(4.29107107088441,-5.23249443999886,-11.978411323517));
#45157=CARTESIAN_POINT('Ctrl Pts',(4.42750300002168,-5.12060916023809,-11.970102340837));
#45158=CARTESIAN_POINT('Ctrl Pts',(4.55965732922994,-5.00330164095815,-11.9617933581569));
#45159=CARTESIAN_POINT('Ctrl Pts',(4.68708863826475,-4.88093117110347,-11.9534843754769));
#45160=CARTESIAN_POINT('Ctrl Pts',(4.81443980231853,-4.75863766333182,-11.9451806185397));
#45161=CARTESIAN_POINT('Ctrl Pts',(4.9370736157764,-4.63128779105709,-11.9368768616026));
#45162=CARTESIAN_POINT('Ctrl Pts',(5.05457882629018,-4.49928015229314,-11.9285731046654));
#45163=CARTESIAN_POINT('Ctrl Pts',(5.17203633252132,-4.36732610544808,-11.9202727188534));
#45164=CARTESIAN_POINT('Ctrl Pts',(5.28436915363902,-4.23071831935014,-11.9119723330414));
#45165=CARTESIAN_POINT('Ctrl Pts',(5.39120371393617,-4.08989138179009,-11.9036719472294));
#45166=CARTESIAN_POINT('Ctrl Pts',(5.49801574560448,-3.94909414096674,-11.8953733117527));
#45167=CARTESIAN_POINT('Ctrl Pts',(5.59933161625974,-3.80407979812098,-11.8870746762761));
#45168=CARTESIAN_POINT('Ctrl Pts',(5.69481864018185,-3.65531526074528,-11.8787760407995));
#45169=CARTESIAN_POINT('Ctrl Pts',(5.79030137812491,-3.50655740073435,-11.8704777778109));
#45170=CARTESIAN_POINT('Ctrl Pts',(5.87995560299437,-3.35404997439035,-11.8621795148224));
#45171=CARTESIAN_POINT('Ctrl Pts',(5.96349239510832,-3.19828820675769,-11.8538812518338));
#45172=CARTESIAN_POINT('Ctrl Pts',(6.04703930317096,-3.0425075770403,-11.8455819839611));
#45173=CARTESIAN_POINT('Ctrl Pts',(6.12446713852243,-2.88347212752461,-11.8372827160883));
#45174=CARTESIAN_POINT('Ctrl Pts',(6.19553322246003,-2.72170113888245,-11.8289834482155));
#45175=CARTESIAN_POINT('Ctrl Pts',(6.26664920624323,-2.55981656093146,-11.820678352919));
#45176=CARTESIAN_POINT('Ctrl Pts',(6.33139437276218,-2.39519292458183,-11.8123732576225));
#45177=CARTESIAN_POINT('Ctrl Pts',(6.38957410279937,-2.228369759451,-11.804068162326));
#45178=CARTESIAN_POINT('Ctrl Pts',(6.44777504819142,-2.06148576191948,-11.7957600385599));
#45179=CARTESIAN_POINT('Ctrl Pts',(6.49940567781079,-1.89240096775964,-11.7874519147938));
#45180=CARTESIAN_POINT('Ctrl Pts',(6.54432138956985,-1.72166969829247,-11.7791437910277));
#45181=CARTESIAN_POINT('Ctrl Pts',(6.58928484647106,-1.55075694247213,-11.770826835774));
#45182=CARTESIAN_POINT('Ctrl Pts',(6.62751904274004,-1.37819455288503,-11.7625098805203));
#45183=CARTESIAN_POINT('Ctrl Pts',(6.65893037524787,-1.20454773985977,-11.7541929252666));
#45184=CARTESIAN_POINT('Ctrl Pts',(6.68208004939455,-1.07657268063102,-11.748063455784));
#45185=CARTESIAN_POINT('Ctrl Pts',(6.7015249770888,-0.948008833898331,-11.7419339863014));
#45186=CARTESIAN_POINT('Ctrl Pts',(6.71724575092009,-0.819083952807052,
-11.7358045168188));
#45187=CARTESIAN_POINT('Ctrl Pts',(6.73892081266221,-0.641328405418721,
-11.7273534932936));
#45188=CARTESIAN_POINT('Ctrl Pts',(6.7535541152242,-0.462561580005216,-11.7189024697684));
#45189=CARTESIAN_POINT('Ctrl Pts',(6.76106445889872,-0.283366163499842,
-11.7104514462432));
#45190=CARTESIAN_POINT('Ctrl Pts',(6.76856818993887,-0.104328523232263,
-11.7020078635931));
#45191=CARTESIAN_POINT('Ctrl Pts',(6.76896144866933,0.0751366263168869,
-11.6935642809429));
#45192=CARTESIAN_POINT('Ctrl Pts',(6.76221478027886,0.254441084296753,-11.6851206982927));
#45193=CARTESIAN_POINT('Ctrl Pts',(6.75547313499325,0.433612044520193,-11.676683402153));
#45194=CARTESIAN_POINT('Ctrl Pts',(6.74160217200139,0.612622221501215,-11.6682461060132));
#45195=CARTESIAN_POINT('Ctrl Pts',(6.72062450102552,0.790882618481051,-11.6598088098734));
#45196=CARTESIAN_POINT('Ctrl Pts',(6.69966179601826,0.969015840260736,-11.6513775331011));
#45197=CARTESIAN_POINT('Ctrl Pts',(6.67160253482747,1.1464000205918,-11.6429462563287));
#45198=CARTESIAN_POINT('Ctrl Pts',(6.63652124700247,1.3224502781144,-11.6345149795564));
#45199=CARTESIAN_POINT('Ctrl Pts',(6.60145499628745,1.49842507412315,-11.6260873167345));
#45200=CARTESIAN_POINT('Ctrl Pts',(6.55937278396115,1.67306676267044,-11.6176596539126));
#45201=CARTESIAN_POINT('Ctrl Pts',(6.51040052640408,1.84579901013016,-11.6092319910907));
#45202=CARTESIAN_POINT('Ctrl Pts',(6.46144334444441,2.01847808377374,-11.6008069226367));
#45203=CARTESIAN_POINT('Ctrl Pts',(6.40560043743466,2.18924857001311,-11.5923818541827));
#45204=CARTESIAN_POINT('Ctrl Pts',(6.34304812896488,2.35754733433609,-11.5839567857287));
#45205=CARTESIAN_POINT('Ctrl Pts',(6.32593190269042,2.40359902774811,-11.5816514291149));
#45206=CARTESIAN_POINT('Ctrl Pts',(6.30831360625685,2.4494657428033,-11.5793460725012));
#45207=CARTESIAN_POINT('Ctrl Pts',(6.29019749782231,2.49513615628286,-11.5770407158874));
#45208=CARTESIAN_POINT('Ctrl Pts',(6.22246718235915,2.66588317535046,-11.5684217273629));
#45209=CARTESIAN_POINT('Ctrl Pts',(6.14780512269873,2.83380862626157,-11.5598027388385));
#45210=CARTESIAN_POINT('Ctrl Pts',(6.06647740403953,2.99835636745832,-11.551183750314));
#45211=CARTESIAN_POINT('Ctrl Pts',(5.98510096281952,3.16300268743556,-11.5425595982463));
#45212=CARTESIAN_POINT('Ctrl Pts',(5.89705102790888,3.32426698664446,-11.5339354461786));
#45213=CARTESIAN_POINT('Ctrl Pts',(5.80263957124182,3.48161787194668,-11.5253112941109));
#45214=CARTESIAN_POINT('Ctrl Pts',(5.70499449678336,3.64435806740434,-11.5163917625147));
#45215=CARTESIAN_POINT('Ctrl Pts',(5.60054460875648,3.80291172908376,-11.5074722309184));
#45216=CARTESIAN_POINT('Ctrl Pts',(5.48968324925971,3.95672425407651,-11.4985526993221));
#45217=CARTESIAN_POINT('Ctrl Pts',(5.38229349589826,4.10572016390346,-11.4899124814629));
#45218=CARTESIAN_POINT('Ctrl Pts',(5.26888796700644,4.25026716798676,-11.4812722636037));
#45219=CARTESIAN_POINT('Ctrl Pts',(5.14986505942818,4.38989508640934,-11.4726320457444));
#45220=CARTESIAN_POINT('Ctrl Pts',(5.0250706423261,4.53629366669326,-11.4635728572796));
#45221=CARTESIAN_POINT('Ctrl Pts',(4.89410078483449,4.67728395653573,-11.4545136688149));
#45222=CARTESIAN_POINT('Ctrl Pts',(4.75745828152374,4.81236736955536,-11.4454544803501));
#45223=CARTESIAN_POINT('Ctrl Pts',(4.62081577821295,4.94745078257504,-11.4363952918853));
#45224=CARTESIAN_POINT('Ctrl Pts',(4.47850093466733,5.07662708613753,-11.4273361034205));
#45225=CARTESIAN_POINT('Ctrl Pts',(4.33105680174849,5.1994457377713,-11.4182769149557));
#45226=CARTESIAN_POINT('Ctrl Pts',(4.18385813299746,5.32205992160078,-11.4092328081772));
#45227=CARTESIAN_POINT('Ctrl Pts',(4.03141216534033,5.43845122077355,-11.4001887013987));
#45228=CARTESIAN_POINT('Ctrl Pts',(3.87424375000041,5.54820010143675,-11.3911445946202));
#45229=CARTESIAN_POINT('Ctrl Pts',(3.71725952241186,5.65782036593047,-11.3821110867505));
#45230=CARTESIAN_POINT('Ctrl Pts',(3.55556409441686,5.7608136214315,-11.3730775788807));
#45231=CARTESIAN_POINT('Ctrl Pts',(3.38971261093798,5.85680266145685,-11.3640440710109));
#45232=CARTESIAN_POINT('Ctrl Pts',(3.29417845549221,5.91209449049882,-11.358840568896));
#45233=CARTESIAN_POINT('Ctrl Pts',(3.19726589331876,5.96506307616248,-11.353637066781));
#45234=CARTESIAN_POINT('Ctrl Pts',(3.09908550384727,6.01564277861009,-11.3484335646661));
#45235=CARTESIAN_POINT('Origin',(0.,0.,-63.6971797838103));
#45236=CARTESIAN_POINT('',(3.09908550384723,6.01564277861011,-8.95438620791578));
#45237=CARTESIAN_POINT('',(3.09908550384716,6.01564277861014,-9.34860320957392));
#45238=CARTESIAN_POINT('',(3.09908550384721,6.01564277861012,-63.6971797838103));
#45239=CARTESIAN_POINT('',(-6.76699998098446,0.000507303006826857,-10.3028202161471));
#45240=CARTESIAN_POINT('Ctrl Pts',(-6.76699998098446,0.000507303006836547,
-10.302820216147));
#45241=CARTESIAN_POINT('Ctrl Pts',(-6.76701416573043,-0.188705404997191,
-10.2939567430814));
#45242=CARTESIAN_POINT('Ctrl Pts',(-6.75908815674408,-0.377745891299328,
-10.2850932700157));
#45243=CARTESIAN_POINT('Ctrl Pts',(-6.74329100385126,-0.565964166161285,
-10.27622979695));
#45244=CARTESIAN_POINT('Ctrl Pts',(-6.72744985035007,-0.754706694897294,
-10.2673416360048));
#45245=CARTESIAN_POINT('Ctrl Pts',(-6.70369370392128,-0.942622170167142,
-10.2584534750596));
#45246=CARTESIAN_POINT('Ctrl Pts',(-6.6721434554764,-1.12906629988833,-10.2495653141144));
#45247=CARTESIAN_POINT('Ctrl Pts',(-6.64055091653122,-1.31576034255509,
-10.2406652393241));
#45248=CARTESIAN_POINT('Ctrl Pts',(-6.60114345573103,-1.50097884609136,
-10.2317651645338));
#45249=CARTESIAN_POINT('Ctrl Pts',(-6.55409264275158,-1.68408985218415,
-10.2228650897435));
#45250=CARTESIAN_POINT('Ctrl Pts',(-6.5069417445632,-1.86759036702593,-10.2139460829563));
#45251=CARTESIAN_POINT('Ctrl Pts',(-6.45211504091601,-2.04897416683534,
-10.2050270761691));
#45252=CARTESIAN_POINT('Ctrl Pts',(-6.38983416972207,-2.22762390978644,
-10.1961080693819));
#45253=CARTESIAN_POINT('Ctrl Pts',(-6.33744337954934,-2.37790442157022,
-10.1886053834981));
#45254=CARTESIAN_POINT('Ctrl Pts',(-6.27977875266993,-2.52625051222462,
-10.1811026976143));
#45255=CARTESIAN_POINT('Ctrl Pts',(-6.21699811996086,-2.67230675192859,
-10.1736000117305));
#45256=CARTESIAN_POINT('Ctrl Pts',(-6.1462820307936,-2.83682446423335,-10.1651489882053));
#45257=CARTESIAN_POINT('Ctrl Pts',(-6.06897179667702,-2.99867266197861,
-10.1566979646801));
#45258=CARTESIAN_POINT('Ctrl Pts',(-5.98529045676721,-3.15730694550456,
-10.1482469411549));
#45259=CARTESIAN_POINT('Ctrl Pts',(-5.90168279578987,-3.31580155625909,
-10.1398033585047));
#45260=CARTESIAN_POINT('Ctrl Pts',(-5.81171536389781,-3.47108760120228,
-10.1313597758545));
#45261=CARTESIAN_POINT('Ctrl Pts',(-5.71565869118012,-3.62264195386974,
-10.1229161932043));
#45262=CARTESIAN_POINT('Ctrl Pts',(-5.61967353564768,-3.77408346960033,
-10.1144788970645));
#45263=CARTESIAN_POINT('Ctrl Pts',(-5.5176083537432,-3.92179855251581,-10.1060416009246));
#45264=CARTESIAN_POINT('Ctrl Pts',(-5.40977906859614,-4.06528958734542,
-10.0976043047847));
#45265=CARTESIAN_POINT('Ctrl Pts',(-5.30202671142249,-4.20867825226229,
-10.0891730280123));
#45266=CARTESIAN_POINT('Ctrl Pts',(-5.18851865223275,-4.34784861573657,
-10.0807417512399));
#45267=CARTESIAN_POINT('Ctrl Pts',(-5.06961361076516,-4.482332745072,-10.0723104744675));
#45268=CARTESIAN_POINT('Ctrl Pts',(-4.95075953630283,-4.61675922964112,
-10.0638828116456));
#45269=CARTESIAN_POINT('Ctrl Pts',(-4.82651331048086,-4.7465032366021,-10.0554551488237));
#45270=CARTESIAN_POINT('Ctrl Pts',(-4.69727375868692,-4.87113007791327,
-10.0470274860017));
#45271=CARTESIAN_POINT('Ctrl Pts',(-4.56807399193894,-4.9957185541532,-10.0386024175477));
#45272=CARTESIAN_POINT('Ctrl Pts',(-4.43388420300839,-5.11519277639464,
-10.0301773490938));
#45273=CARTESIAN_POINT('Ctrl Pts',(-4.29514013578894,-5.22915482787945,
-10.0217522806398));
#45274=CARTESIAN_POINT('Ctrl Pts',(-4.2571755121538,-5.2603383334521,-10.0194469240262));
#45275=CARTESIAN_POINT('Ctrl Pts',(-4.21887009675871,-5.2911093436752,-10.0171415674127));
#45276=CARTESIAN_POINT('Ctrl Pts',(-4.18023326724005,-5.32146021609291,
-10.0148362107991));
#45277=CARTESIAN_POINT('Ctrl Pts',(-4.03578256131235,-5.43493238761628,
-10.0062172222747));
#45278=CARTESIAN_POINT('Ctrl Pts',(-3.88676147890056,-5.54247817885556,
-9.9975982337502));
#45279=CARTESIAN_POINT('Ctrl Pts',(-3.73367981419581,-5.64375088439123,
-9.98897924522574));
#45280=CARTESIAN_POINT('Ctrl Pts',(-3.58050643991341,-5.74508426131475,
-9.98035509315803));
#45281=CARTESIAN_POINT('Ctrl Pts',(-3.42326788217518,-5.84013688462208,
-9.97173094109032));
#45282=CARTESIAN_POINT('Ctrl Pts',(-3.26250113558949,-5.92860652601244,
-9.9631067890226));
#45283=CARTESIAN_POINT('Ctrl Pts',(-3.09622808468068,-6.02010627642222,
-9.95418725742634));
#45284=CARTESIAN_POINT('Ctrl Pts',(-2.92618120058117,-6.1045639578302,-9.94526772583007));
#45285=CARTESIAN_POINT('Ctrl Pts',(-2.7529794746539,-6.18169823043267,-9.9363481942338));
#45286=CARTESIAN_POINT('Ctrl Pts',(-2.58520153368723,-6.25641705535153,
-9.92770797637456));
#45287=CARTESIAN_POINT('Ctrl Pts',(-2.41446364764021,-6.32426412338664,
-9.91906775851531));
#45288=CARTESIAN_POINT('Ctrl Pts',(-2.24134669418592,-6.38503359399634,
-9.91042754065607));
#45289=CARTESIAN_POINT('Ctrl Pts',(-2.05983517059483,-6.44874982154134,
-9.90136835219129));
#45290=CARTESIAN_POINT('Ctrl Pts',(-1.8757084891318,-6.50468487829986,-9.89230916372652));
#45291=CARTESIAN_POINT('Ctrl Pts',(-1.6896520389102,-6.55266090892903,-9.88324997526175));
#45292=CARTESIAN_POINT('Ctrl Pts',(-1.50359558868855,-6.60063693955821,
-9.87419078679697));
#45293=CARTESIAN_POINT('Ctrl Pts',(-1.31560975084686,-6.64065389679344,
-9.86513159833219));
#45294=CARTESIAN_POINT('Ctrl Pts',(-1.12639052691803,-6.67259570039047,
-9.85607240986742));
#45295=CARTESIAN_POINT('Ctrl Pts',(-0.937499112019785,-6.70448216705367,
-9.8470289158111));
#45296=CARTESIAN_POINT('Ctrl Pts',(-0.747204705913315,-6.72835164602761,
-9.83798542175478));
#45297=CARTESIAN_POINT('Ctrl Pts',(-0.556171843592307,-6.74410571391012,
-9.82894192769847));
#45298=CARTESIAN_POINT('Ctrl Pts',(-0.365313718332193,-6.75984537160433,
-9.81990670569311));
#45299=CARTESIAN_POINT('Ctrl Pts',(-0.173718722500571,-6.76748441897586,
-9.81087148368774));
#45300=CARTESIAN_POINT('Ctrl Pts',(0.0179432125647909,-6.76697621106524,
-9.80183626168238));
#45301=CARTESIAN_POINT('Ctrl Pts',(0.209267481025032,-6.76646889850632,
-9.79281695777124));
#45302=CARTESIAN_POINT('Ctrl Pts',(0.400658215445884,-6.75784299382939,
-9.78379765386011));
#45303=CARTESIAN_POINT('Ctrl Pts',(0.591445365356354,-6.74110386953046,
-9.77477834994897));
#45304=CARTESIAN_POINT('Ctrl Pts',(0.781993159461948,-6.72438574563208,
-9.76577036138454));
#45305=CARTESIAN_POINT('Ctrl Pts',(0.971938643774609,-6.69957473584734,
-9.75676237282008));
#45306=CARTESIAN_POINT('Ctrl Pts',(1.16061420527621,-6.66672810803854,-9.74775438425564));
#45307=CARTESIAN_POINT('Ctrl Pts',(1.34886363641287,-6.63395566548926,-9.73876674054892));
#45308=CARTESIAN_POINT('Ctrl Pts',(1.53584863573185,-6.59318387219167,-9.72977909684219));
#45309=CARTESIAN_POINT('Ctrl Pts',(1.72090959681955,-6.54452130866532,-9.72079145313548));
#45310=CARTESIAN_POINT('Ctrl Pts',(1.88208486731399,-6.50213958864607,-9.71296383840234));
#45311=CARTESIAN_POINT('Ctrl Pts',(2.04180067145334,-6.45377335070993,-9.70513622366922));
#45312=CARTESIAN_POINT('Ctrl Pts',(2.19962556666777,-6.39952626109633,-9.69730860893608));
#45313=CARTESIAN_POINT('Ctrl Pts',(2.36340938512926,-6.3432309886346,-9.68918545049079));
#45314=CARTESIAN_POINT('Ctrl Pts',(2.52508305395478,-6.28062598189569,-9.68106229204549));
#45315=CARTESIAN_POINT('Ctrl Pts',(2.68412823352618,-6.21190346238475,-9.6729391336002));
#45316=CARTESIAN_POINT('Ctrl Pts',(2.84316219958018,-6.14318578817104,-9.66481654788009));
#45317=CARTESIAN_POINT('Ctrl Pts',(2.99956770952428,-6.06835160550946,-9.65669396216));
#45318=CARTESIAN_POINT('Ctrl Pts',(3.15284677027445,-5.98764112511513,-9.64857137643989));
#45319=CARTESIAN_POINT('Ctrl Pts',(3.3061442490806,-5.90692094652629,-9.64044781470754));
#45320=CARTESIAN_POINT('Ctrl Pts',(3.45631420733181,-5.82032323579165,-9.63232425297518));
#45321=CARTESIAN_POINT('Ctrl Pts',(3.60288365155014,-5.72813393640483,-9.62420069124283));
#45322=CARTESIAN_POINT('Ctrl Pts',(3.74955985421652,-5.63587748805268,-9.61607121245971));
#45323=CARTESIAN_POINT('Ctrl Pts',(3.89262999478622,-5.53802151165535,-9.6079417336766));
#45324=CARTESIAN_POINT('Ctrl Pts',(4.0316499286213,-5.43489538565812,-9.59981225489348));
#45325=CARTESIAN_POINT('Ctrl Pts',(4.17072653843616,-5.33172721695471,-9.59167946186497));
#45326=CARTESIAN_POINT('Ctrl Pts',(4.30574936501194,-5.22328484499509,-9.58354666883644));
#45327=CARTESIAN_POINT('Ctrl Pts',(4.43630793002299,-5.10993747026469,-9.57541387580793));
#45328=CARTESIAN_POINT('Ctrl Pts',(4.56700845766692,-4.99646684745981,-9.56727223960079));
#45329=CARTESIAN_POINT('Ctrl Pts',(4.69323476170268,-4.87808081937901,-9.55913060339365));
#45330=CARTESIAN_POINT('Ctrl Pts',(4.81461322760548,-4.75518542946186,-9.55098896718652));
#45331=CARTESIAN_POINT('Ctrl Pts',(4.87645390731439,-4.69257189757183,-9.54684091412581));
#45332=CARTESIAN_POINT('Ctrl Pts',(4.93703683782887,-4.62878838726588,-9.54269286106512));
#45333=CARTESIAN_POINT('Ctrl Pts',(4.9963167156584,-4.56389179065767,-9.53854480800441));
#45334=CARTESIAN_POINT('Ctrl Pts',(5.11694307828481,-4.43183618119447,-9.53010409302633));
#45335=CARTESIAN_POINT('Ctrl Pts',(5.23241990530334,-4.29489774045607,-9.52166337804825));
#45336=CARTESIAN_POINT('Ctrl Pts',(5.34234744748511,-4.15350607924791,-9.51322266307017));
#45337=CARTESIAN_POINT('Ctrl Pts',(5.45219190125168,-4.01222128851841,-9.50478832798213));
#45338=CARTESIAN_POINT('Ctrl Pts',(5.55649522757408,-3.86649024942434,-9.49635399289409));
#45339=CARTESIAN_POINT('Ctrl Pts',(5.65489700380936,-3.71677667829371,-9.48791965780605));
#45340=CARTESIAN_POINT('Ctrl Pts',(5.75323951406211,-3.56715327750583,-9.4794904025974));
#45341=CARTESIAN_POINT('Ctrl Pts',(5.84568737782654,-3.41355240462048,-9.47106114738875));
#45342=CARTESIAN_POINT('Ctrl Pts',(5.93192244865042,-3.25646818857443,-9.4626318921801));
#45343=CARTESIAN_POINT('Ctrl Pts',(6.01811880913471,-3.09945448656969,-9.45420642080706));
#45344=CARTESIAN_POINT('Ctrl Pts',(6.09810777723121,-2.9389608509411,-9.44578094943403));
#45345=CARTESIAN_POINT('Ctrl Pts',(6.17161607998804,-2.77550787446785,-9.43735547806099));
#45346=CARTESIAN_POINT('Ctrl Pts',(6.24510265155741,-2.61210321943776,-9.42893249750179));
#45347=CARTESIAN_POINT('Ctrl Pts',(6.31211224186913,-2.44574127200291,-9.4205095169426));
#45348=CARTESIAN_POINT('Ctrl Pts',(6.37241867447862,-2.27696491785802,-9.4120865363834));
#45349=CARTESIAN_POINT('Ctrl Pts',(6.43272610563781,-2.10818576912604,-9.40366341635707));
#45350=CARTESIAN_POINT('Ctrl Pts',(6.48633003895352,-1.936992445479,-9.39524029633074));
#45351=CARTESIAN_POINT('Ctrl Pts',(6.53305314376033,-1.76394603681726,-9.38681717630442));
#45352=CARTESIAN_POINT('Ctrl Pts',(6.57977786433003,-1.59089364392205,-9.37839376499256));
#45353=CARTESIAN_POINT('Ctrl Pts',(6.61962119485132,-1.41598836017141,-9.36997035368069));
#45354=CARTESIAN_POINT('Ctrl Pts',(6.65245617608273,-1.23980475289408,-9.36154694236883));
#45355=CARTESIAN_POINT('Ctrl Pts',(6.68529687212382,-1.06359048149737,-9.3531220649927));
#45356=CARTESIAN_POINT('Ctrl Pts',(6.71112672590027,-0.886097770840552,
-9.34469718761657));
#45357=CARTESIAN_POINT('Ctrl Pts',(6.72987016234946,-0.707910021060919,
-9.33627231024044));
#45358=CARTESIAN_POINT('Ctrl Pts',(6.74861947588111,-0.529666399771182,
-9.32784479120897));
#45359=CARTESIAN_POINT('Ctrl Pts',(6.76027790719262,-0.350727636390128,
-9.31941727217751));
#45360=CARTESIAN_POINT('Ctrl Pts',(6.76482184169824,-0.171681245575883,
-9.31098975314604));
#45361=CARTESIAN_POINT('Ctrl Pts',(6.76936985102868,0.00752570712074452,
-9.30255467664126));
#45362=CARTESIAN_POINT('Ctrl Pts',(6.76679060691772,0.186840146404907,-9.29411960013649));
#45363=CARTESIAN_POINT('Ctrl Pts',(6.75711263952535,0.365674413606876,-9.28568452363171));
#45364=CARTESIAN_POINT('Ctrl Pts',(6.7474299947076,0.544595112587973,-9.2772453703989));
#45365=CARTESIAN_POINT('Ctrl Pts',(6.73064181025444,0.723034844344235,-9.26880621716608));
#45366=CARTESIAN_POINT('Ctrl Pts',(6.70682846627655,0.900411530325205,-9.26036706393327));
#45367=CARTESIAN_POINT('Ctrl Pts',(6.68298865899698,1.07798533153518,-9.25191853243515));
#45368=CARTESIAN_POINT('Ctrl Pts',(6.65210814530788,1.25449339711444,-9.24347000093703));
#45369=CARTESIAN_POINT('Ctrl Pts',(6.61431857154867,1.42936308685597,-9.23502146943891));
#45370=CARTESIAN_POINT('Ctrl Pts',(6.59343860596157,1.5259842640964,-9.23035338167305));
#45371=CARTESIAN_POINT('Ctrl Pts',(6.57045025428671,1.62210548785427,-9.2256852939072));
#45372=CARTESIAN_POINT('Ctrl Pts',(6.54538223735837,1.71763219778671,-9.22101720614135));
#45373=CARTESIAN_POINT('Ctrl Pts',(6.50112859164225,1.88626959698187,-9.2127764305446));
#45374=CARTESIAN_POINT('Ctrl Pts',(6.45029244045929,2.05342848501208,-9.20453565494785));
#45375=CARTESIAN_POINT('Ctrl Pts',(6.39298704908826,2.21855935016168,-9.19629487935111));
#45376=CARTESIAN_POINT('Ctrl Pts',(6.33574512965081,2.38350731497582,-9.18806323130674));
#45377=CARTESIAN_POINT('Ctrl Pts',(6.27204835323481,2.54643139644607,-9.17983158326238));
#45378=CARTESIAN_POINT('Ctrl Pts',(6.20206062487855,2.70679386088619,-9.171599935218));
#45379=CARTESIAN_POINT('Ctrl Pts',(6.13213794305246,2.86700728459976,-9.16337593765974));
#45380=CARTESIAN_POINT('Ctrl Pts',(6.05593609486273,3.02466350848271,-9.15515194010147));
#45381=CARTESIAN_POINT('Ctrl Pts',(5.97366829717051,3.17924143081019,-9.1469279425432));
#45382=CARTESIAN_POINT('Ctrl Pts',(5.8914731833971,3.33368278294286,-9.13871121091872));
#45383=CARTESIAN_POINT('Ctrl Pts',(5.8032229682675,3.48505094127598,-9.13049447929424));
#45384=CARTESIAN_POINT('Ctrl Pts',(5.70917827070372,3.6328463321925,-9.12227774766976));
#45385=CARTESIAN_POINT('Ctrl Pts',(5.61518175571999,3.78056600205895,-9.11406522578107));
#45386=CARTESIAN_POINT('Ctrl Pts',(5.51539686137002,3.92471625063394,-9.10585270389237));
#45387=CARTESIAN_POINT('Ctrl Pts',(5.4101294884512,4.06482323332649,-9.09764018200368));
#45388=CARTESIAN_POINT('Ctrl Pts',(5.30489731744878,4.20488336356935,-9.08943040642185));
#45389=CARTESIAN_POINT('Ctrl Pts',(5.19418653364245,4.34090263731415,-9.08122063084003));
#45390=CARTESIAN_POINT('Ctrl Pts',(5.07834564463575,4.47243720063335,-9.07301085525821));
#45391=CARTESIAN_POINT('Ctrl Pts',(5.02774935388386,4.52988808060059,-9.06942503857545));
#45392=CARTESIAN_POINT('Ctrl Pts',(4.97617491922371,4.58648381155589,-9.06583922189268));
#45393=CARTESIAN_POINT('Ctrl Pts',(4.92365379175857,4.64218939067564,-9.06225340520992));
#45394=CARTESIAN_POINT('Ctrl Pts',(4.79199371448726,4.78183225832386,-9.05326447210208));
#45395=CARTESIAN_POINT('Ctrl Pts',(4.65452043799943,4.9157320726033,-9.04427553899425));
#45396=CARTESIAN_POINT('Ctrl Pts',(4.51175443477957,5.04344732501955,-9.0352866058864));
#45397=CARTESIAN_POINT('Ctrl Pts',(4.37074449949692,5.16959163859321,-9.02640823955821));
#45398=CARTESIAN_POINT('Ctrl Pts',(4.22457154299096,5.28970256620136,-9.01752987323002));
#45399=CARTESIAN_POINT('Ctrl Pts',(4.0737664341739,5.40339856384832,-9.00865150690183));
#45400=CARTESIAN_POINT('Ctrl Pts',(3.92014424708681,5.51921843201182,-8.99960729040415));
#45401=CARTESIAN_POINT('Ctrl Pts',(3.76171540559239,5.62838120861716,-8.99056307390648));
#45402=CARTESIAN_POINT('Ctrl Pts',(3.59906836988956,5.73053190104204,-8.98151885740881));
#45403=CARTESIAN_POINT('Ctrl Pts',(3.43642133418668,5.83268259346696,-8.97247464091113));
#45404=CARTESIAN_POINT('Ctrl Pts',(3.2695563726811,5.9278211080299,-8.96343042441345));
#45405=CARTESIAN_POINT('Ctrl Pts',(3.09908550384723,6.01564277861011,-8.95438620791577));
#45406=CARTESIAN_POINT('Ctrl Pts',(3.0990855038472,6.01564277861013,-10.9542570414832));
#45407=CARTESIAN_POINT('Ctrl Pts',(2.94371122680837,6.0956871208962,-10.9460573085275));
#45408=CARTESIAN_POINT('Ctrl Pts',(2.78526207069075,6.16969346450379,-10.9378575755718));
#45409=CARTESIAN_POINT('Ctrl Pts',(2.62425162136487,6.23743476340746,-10.9296578426161));
#45410=CARTESIAN_POINT('Ctrl Pts',(2.46318476932544,6.305199792405,-10.9214552372556));
#45411=CARTESIAN_POINT('Ctrl Pts',(2.29955516720259,6.36669526584841,-10.9132526318951));
#45412=CARTESIAN_POINT('Ctrl Pts',(2.13389486804937,6.42174288586148,-10.9050500265346));
#45413=CARTESIAN_POINT('Ctrl Pts',(1.96804659819913,6.47685296706506,-10.896838113878));
#45414=CARTESIAN_POINT('Ctrl Pts',(1.80016336871473,6.52550046506747,-10.8886262012215));
#45415=CARTESIAN_POINT('Ctrl Pts',(1.63079185720553,6.56755714999665,-10.880414288565));
#45416=CARTESIAN_POINT('Ctrl Pts',(1.4613209119989,6.60963852533361,-10.8721975549038));
#45417=CARTESIAN_POINT('Ctrl Pts',(1.29036029374117,6.64512130188961,-10.8639808212426));
#45418=CARTESIAN_POINT('Ctrl Pts',(1.11846516112074,6.67392872926878,-10.8557640875815));
#45419=CARTESIAN_POINT('Ctrl Pts',(0.946304103210026,6.70278072232803,-10.8475346424651));
#45420=CARTESIAN_POINT('Ctrl Pts',(0.77320599739447,6.72493668341888,-10.8393051973487));
#45421=CARTESIAN_POINT('Ctrl Pts',(0.599730732672557,6.74037180341619,-10.8310757522323));
#45422=CARTESIAN_POINT('Ctrl Pts',(0.442190400473157,6.75438909824962,-10.8236022399737));
#45423=CARTESIAN_POINT('Ctrl Pts',(0.284339235273718,6.76286421240504,-10.8161287277152));
#45424=CARTESIAN_POINT('Ctrl Pts',(0.126594363644664,6.76581575769644,-10.8086552154566));
#45425=CARTESIAN_POINT('Ctrl Pts',(-0.0437590575373766,6.76900322003972,
-10.8005843452702));
#45426=CARTESIAN_POINT('Ctrl Pts',(-0.214544006950354,6.76575834722171,
-10.7925134750838));
#45427=CARTESIAN_POINT('Ctrl Pts',(-0.3852233321942,6.75602634574002,-10.7844426048974));
#45428=CARTESIAN_POINT('Ctrl Pts',(-0.555690260284677,6.7463064549777,-10.7763817782816));
#45429=CARTESIAN_POINT('Ctrl Pts',(-0.726051458031113,6.73011551924833,
-10.7683209516657));
#45430=CARTESIAN_POINT('Ctrl Pts',(-0.89576569172678,6.70745054588741,-10.7602601250499));
#45431=CARTESIAN_POINT('Ctrl Pts',(-1.06530594499202,6.6848088072413,-10.75220756189));
#45432=CARTESIAN_POINT('Ctrl Pts',(-1.23420018744348,6.65570628736731,-10.7441549987301));
#45433=CARTESIAN_POINT('Ctrl Pts',(-1.40190833073111,6.62019199360764,-10.7361024355702));
#45434=CARTESIAN_POINT('Ctrl Pts',(-1.56948127196993,6.58470633057028,-10.7280563641823));
#45435=CARTESIAN_POINT('Ctrl Pts',(-1.73586965415927,6.5428192586714,-10.7200102927945));
#45436=CARTESIAN_POINT('Ctrl Pts',(-1.90053975673978,6.49463144705314,-10.7119642214066));
#45437=CARTESIAN_POINT('Ctrl Pts',(-2.06511312617447,6.44647194269001,-10.7039228765707));
#45438=CARTESIAN_POINT('Ctrl Pts',(-2.22796986830822,6.39201917132693,-10.6958815317348));
#45439=CARTESIAN_POINT('Ctrl Pts',(-2.38858779255754,6.33142459145216,-10.6878401868989));
#45440=CARTESIAN_POINT('Ctrl Pts',(-2.55230193616371,6.26966193452742,-10.6796438296778));
#45441=CARTESIAN_POINT('Ctrl Pts',(-2.71368967910526,6.20151834684661,-10.6714474724568));
#45442=CARTESIAN_POINT('Ctrl Pts',(-2.87221520727613,6.12720725968134,-10.6632511152357));
#45443=CARTESIAN_POINT('Ctrl Pts',(-3.02769320701448,6.05432474464323,-10.6552123265272));
#45444=CARTESIAN_POINT('Ctrl Pts',(-3.18041770050255,5.9755098938006,-10.6471735378187));
#45445=CARTESIAN_POINT('Ctrl Pts',(-3.32990470562327,5.8910121075642,-10.6391347491102));
#45446=CARTESIAN_POINT('Ctrl Pts',(-3.47940770720776,5.8065052792992,-10.6310951001785));
#45447=CARTESIAN_POINT('Ctrl Pts',(-3.62567220541206,5.71631448847311,-10.6230554512467));
#45448=CARTESIAN_POINT('Ctrl Pts',(-3.76824039120981,5.62073423620571,-10.615015802315));
#45449=CARTESIAN_POINT('Ctrl Pts',(-3.91085206214143,5.52512483072967,-10.6069737011867));
#45450=CARTESIAN_POINT('Ctrl Pts',(-4.04976486650263,5.42412289957467,-10.5989316000585));
#45451=CARTESIAN_POINT('Ctrl Pts',(-4.18455158447879,5.31806515913787,-10.5908894989302));
#45452=CARTESIAN_POINT('Ctrl Pts',(-4.32388682462316,5.20842838665154,-10.5825760084855));
#45453=CARTESIAN_POINT('Ctrl Pts',(-4.45881228399271,5.09338887711495,-10.5742625180408));
#45454=CARTESIAN_POINT('Ctrl Pts',(-4.5888956721546,4.97336159052213,-10.5659490275961));
#45455=CARTESIAN_POINT('Ctrl Pts',(-4.71495423522875,4.8570479897513,-10.5578927594253));
#45456=CARTESIAN_POINT('Ctrl Pts',(-4.83646568675954,4.73605097442007,-10.5498364912546));
#45457=CARTESIAN_POINT('Ctrl Pts',(-4.95307667346797,4.61078306437719,-10.5417802230838));
#45458=CARTESIAN_POINT('Ctrl Pts',(-5.07527243141323,4.47951578291441,-10.5333381215021));
#45459=CARTESIAN_POINT('Ctrl Pts',(-5.19208647558606,4.3435588296383,-10.5248960199204));
#45460=CARTESIAN_POINT('Ctrl Pts',(-5.30316260749174,4.20342186301844,-10.5164539183387));
#45461=CARTESIAN_POINT('Ctrl Pts',(-5.41423873939742,4.06328489639858,-10.508011816757));
#45462=CARTESIAN_POINT('Ctrl Pts',(-5.51957675716195,3.91896833967192,-10.4995697151753));
#45463=CARTESIAN_POINT('Ctrl Pts',(-5.61887539771207,3.77101157051872,-10.4911276135935));
#45464=CARTESIAN_POINT('Ctrl Pts',(-5.7203506356957,3.61981163184953,-10.4825004635909));
#45465=CARTESIAN_POINT('Ctrl Pts',(-5.81582121332627,3.46436145607391,-10.4738733135882));
#45466=CARTESIAN_POINT('Ctrl Pts',(-5.90493347073066,3.30515502000206,-10.4652461635856));
#45467=CARTESIAN_POINT('Ctrl Pts',(-5.9939235529799,3.1461668599743,-10.4566308416234));
#45468=CARTESIAN_POINT('Ctrl Pts',(-6.07657254515671,2.98343297541944,-10.4480155196613));
#45469=CARTESIAN_POINT('Ctrl Pts',(-6.1525698941479,2.8174762993901,-10.4394001976991));
#45470=CARTESIAN_POINT('Ctrl Pts',(-6.22846946782509,2.65173313694149,-10.4307959598843));
#45471=CARTESIAN_POINT('Ctrl Pts',(-6.29773433308201,2.48277572998217,-10.4221917220694));
#45472=CARTESIAN_POINT('Ctrl Pts',(-6.36009942576228,2.31115215734887,-10.4135874842545));
#45473=CARTESIAN_POINT('Ctrl Pts',(-6.4223895239155,2.13973496344615,-10.4049935931051));
#45474=CARTESIAN_POINT('Ctrl Pts',(-6.47779628827751,1.96565828633327,-10.3963997019556));
#45475=CARTESIAN_POINT('Ctrl Pts',(-6.52610218492109,1.78949134447982,-10.3878058108061));
#45476=CARTESIAN_POINT('Ctrl Pts',(-6.57433558199768,1.61358880154843,-10.3792248177381));
#45477=CARTESIAN_POINT('Ctrl Pts',(-6.61548929352954,1.43560255063745,-10.37064382467));
#45478=CARTESIAN_POINT('Ctrl Pts',(-6.64939518380052,1.2561181033846,-10.3620628316019));
#45479=CARTESIAN_POINT('Ctrl Pts',(-6.68326992107623,1.07679856783558,-10.3534897228169));
#45480=CARTESIAN_POINT('Ctrl Pts',(-6.70991005583626,0.895983883167295,
-10.3449166140319));
#45481=CARTESIAN_POINT('Ctrl Pts',(-6.72919786552631,0.714272417636402,
-10.3363435052469));
#45482=CARTESIAN_POINT('Ctrl Pts',(-6.74846454119377,0.532760056839584,
-10.3277797901814));
#45483=CARTESIAN_POINT('Ctrl Pts',(-6.76039493087367,0.350353182417493,
-10.319216075116));
#45484=CARTESIAN_POINT('Ctrl Pts',(-6.76492274477394,0.167658155901406,
-10.3106523600505));
#45485=CARTESIAN_POINT('Ctrl Pts',(-6.76630308378061,0.111962167289865,
-10.3080416454303));
#45486=CARTESIAN_POINT('Ctrl Pts',(-6.76699580289412,0.0562394508427558,
-10.3054309308102));
#45487=CARTESIAN_POINT('Ctrl Pts',(-6.76699998098439,0.000507303923607805,
-10.30282021619));
#45488=CARTESIAN_POINT('',(-6.76699933288377,0.00183566786179907,-10.6971797838101));
#45489=CARTESIAN_POINT('Ctrl Pts',(3.09908550384727,6.01564277861009,-11.3484335646661));
#45490=CARTESIAN_POINT('Ctrl Pts',(2.92902828004936,6.10325135120861,-11.3394206331789));
#45491=CARTESIAN_POINT('Ctrl Pts',(2.7551659932718,6.1836904247374,-11.3304077016917));
#45492=CARTESIAN_POINT('Ctrl Pts',(2.57809464427906,6.25665381854707,-11.3213947702044));
#45493=CARTESIAN_POINT('Ctrl Pts',(2.40125969901093,6.32951980067408,-11.3123938716666));
#45494=CARTESIAN_POINT('Ctrl Pts',(2.2212244602406,6.39492992811433,-11.3033929731287));
#45495=CARTESIAN_POINT('Ctrl Pts',(2.03860694960393,6.45262510185014,-11.2943920745908));
#45496=CARTESIAN_POINT('Ctrl Pts',(1.85637556106118,6.51019828629142,-11.2854102073374));
#45497=CARTESIAN_POINT('Ctrl Pts',(1.67157302439807,6.56008900143514,-11.2764283400839));
#45498=CARTESIAN_POINT('Ctrl Pts',(1.48483461019973,6.60208718363769,-11.2674464728305));
#45499=CARTESIAN_POINT('Ctrl Pts',(1.4298548455648,6.61445234258211,-11.2648020198951));
#45500=CARTESIAN_POINT('Ctrl Pts',(1.37470739957853,6.62613366495919,-11.2621575669598));
#45501=CARTESIAN_POINT('Ctrl Pts',(1.31940879332319,6.63712659485273,-11.2595131140244));
#45502=CARTESIAN_POINT('Ctrl Pts',(1.14954404193941,6.67089437725803,-11.2513899555791));
#45503=CARTESIAN_POINT('Ctrl Pts',(0.97832774299963,6.69814765297914,-11.2432667971338));
#45504=CARTESIAN_POINT('Ctrl Pts',(0.806304555653694,6.71879170413342,-11.2351436386886));
#45505=CARTESIAN_POINT('Ctrl Pts',(0.634293496844222,6.73943429977388,-11.2270210529685));
#45506=CARTESIAN_POINT('Ctrl Pts',(0.461476026364602,6.75346855543135,-11.2188984672485));
#45507=CARTESIAN_POINT('Ctrl Pts',(0.288403368807972,6.76085146241657,-11.2107758815285));
#45508=CARTESIAN_POINT('Ctrl Pts',(0.115309914790117,6.76823525653405,-11.2026523197962));
#45509=CARTESIAN_POINT('Ctrl Pts',(-0.0580384216276527,6.76896609612683,
-11.1945287580639));
#45510=CARTESIAN_POINT('Ctrl Pts',(-0.231089006889341,6.76305307319815,
-11.1864051963316));
#45511=CARTESIAN_POINT('Ctrl Pts',(-0.404265638968567,6.75713574333389,
-11.1782757175485));
#45512=CARTESIAN_POINT('Ctrl Pts',(-0.577143720549638,6.74456489817517,
-11.1701462387654));
#45513=CARTESIAN_POINT('Ctrl Pts',(-0.749173691772695,6.72540168165112,
-11.1620167599823));
#45514=CARTESIAN_POINT('Ctrl Pts',(-0.921273796586807,6.70623065262101,
-11.1538839669538));
#45515=CARTESIAN_POINT('Ctrl Pts',(-1.09252474014897,6.68046194947762,-11.1457511739253));
#45516=CARTESIAN_POINT('Ctrl Pts',(-1.26238601742938,6.64820807007413,-11.1376183808968));
#45517=CARTESIAN_POINT('Ctrl Pts',(-1.43243199307947,6.61591911946997,-11.1294767446897));
#45518=CARTESIAN_POINT('Ctrl Pts',(-1.60108492812652,6.57713099016385,-11.1213351084826));
#45519=CARTESIAN_POINT('Ctrl Pts',(-1.76781763462296,6.53200656848385,-11.1131934722755));
#45520=CARTESIAN_POINT('Ctrl Pts',(-1.85276568387851,6.50901628855588,-11.1090454192145));
#45521=CARTESIAN_POINT('Ctrl Pts',(-1.93721556152399,6.48438204768635,-11.1048973661536));
#45522=CARTESIAN_POINT('Ctrl Pts',(-2.02109948946135,6.45813021343632,-11.1007493130927));
#45523=CARTESIAN_POINT('Ctrl Pts',(-2.19179169531306,6.40471135709549,-11.0923085981146));
#45524=CARTESIAN_POINT('Ctrl Pts',(-2.36049088578999,6.34448165293996,-11.0838678831365));
#45525=CARTESIAN_POINT('Ctrl Pts',(-2.52663542900019,6.2776112024337,-11.0754271681584));
#45526=CARTESIAN_POINT('Ctrl Pts',(-2.69265439233694,6.21079129576444,-11.0669928330703));
#45527=CARTESIAN_POINT('Ctrl Pts',(-2.85612224939063,6.13734077263783,-11.0585584979823));
#45528=CARTESIAN_POINT('Ctrl Pts',(-3.01649419109503,6.05747899666932,-11.0501241628943));
#45529=CARTESIAN_POINT('Ctrl Pts',(-3.17676954307263,5.97766532030627,-11.0416949076856));
#45530=CARTESIAN_POINT('Ctrl Pts',(-3.3339523994017,5.89144823764874,-11.033265652477));
#45531=CARTESIAN_POINT('Ctrl Pts',(-3.48751918108041,5.79909466741114,-11.0248363972683));
#45532=CARTESIAN_POINT('Ctrl Pts',(-3.64101702767104,5.70678255406563,-11.0164109258952));
#45533=CARTESIAN_POINT('Ctrl Pts',(-3.79090175091294,5.60833961712535,-11.0079854545222));
#45534=CARTESIAN_POINT('Ctrl Pts',(-3.93667523341055,5.50407822497573,-10.9995599831491));
#45535=CARTESIAN_POINT('Ctrl Pts',(-4.08240562103731,5.39984765551864,-10.9911370025898));
#45536=CARTESIAN_POINT('Ctrl Pts',(-4.22402692080827,5.28980225488819,-10.9827140220305));
#45537=CARTESIAN_POINT('Ctrl Pts',(-4.36107049680697,5.17429735537878,-10.9742910414712));
#45538=CARTESIAN_POINT('Ctrl Pts',(-4.49811634196246,5.05879054334829,-10.9658679214449));
#45539=CARTESIAN_POINT('Ctrl Pts',(-4.63058405276663,4.93782426158901,-10.9574448014186));
#45540=CARTESIAN_POINT('Ctrl Pts',(-4.75803804389615,4.81179415320699,-10.9490216813922));
#45541=CARTESIAN_POINT('Ctrl Pts',(-4.88549644259733,4.68575968649355,-10.9405982700803));
#45542=CARTESIAN_POINT('Ctrl Pts',(-5.00794053865764,4.55466127837574,-10.9321748587685));
#45543=CARTESIAN_POINT('Ctrl Pts',(-5.12497149428656,4.41893156574643,-10.9237514474566));
#45544=CARTESIAN_POINT('Ctrl Pts',(-5.24202281872921,4.2831782298525,-10.9153265700805));
#45545=CARTESIAN_POINT('Ctrl Pts',(-5.35365890662719,4.14279223496335,-10.9069016927044));
#45546=CARTESIAN_POINT('Ctrl Pts',(-5.45952088009703,3.99823970764443,-10.8984768153283));
#45547=CARTESIAN_POINT('Ctrl Pts',(-5.56541604702837,3.85364185528013,-10.8900492962969));
#45548=CARTESIAN_POINT('Ctrl Pts',(-5.66553329292517,3.70487513475965,-10.8816217772655));
#45549=CARTESIAN_POINT('Ctrl Pts',(-5.75955657208287,3.55243537491916,-10.8731942582341));
#45550=CARTESIAN_POINT('Ctrl Pts',(-5.85366416768367,3.39985891299328,-10.8647591817293));
#45551=CARTESIAN_POINT('Ctrl Pts',(-5.94166670178693,3.24360311429356,-10.8563241052246));
#45552=CARTESIAN_POINT('Ctrl Pts',(-6.0232931180757,3.08419017146186,-10.8478890287198));
#45553=CARTESIAN_POINT('Ctrl Pts',(-6.10495898494882,2.92470018330546,-10.8394498754871));
#45554=CARTESIAN_POINT('Ctrl Pts',(-6.18024244341045,2.7620503081495,-10.8310107222543));
#45555=CARTESIAN_POINT('Ctrl Pts',(-6.24892005217444,2.59678400748547,-10.8225715690215));
#45556=CARTESIAN_POINT('Ctrl Pts',(-6.31767398101696,2.43133404962553,-10.8141230375234));
#45557=CARTESIAN_POINT('Ctrl Pts',(-6.37980727148993,2.26326216751822,-10.8056745060253));
#45558=CARTESIAN_POINT('Ctrl Pts',(-6.43514553437091,2.09312946361809,-10.7972259745272));
#45559=CARTESIAN_POINT('Ctrl Pts',(-6.46572172006557,1.99912562474853,-10.7925578867614));
#45560=CARTESIAN_POINT('Ctrl Pts',(-6.49422432686232,1.90449288530371,-10.7878897989957));
#45561=CARTESIAN_POINT('Ctrl Pts',(-6.52063059142497,1.80932741375709,-10.7832217112299));
#45562=CARTESIAN_POINT('Ctrl Pts',(-6.57219902465109,1.6234800647978,-10.774105466421));
#45563=CARTESIAN_POINT('Ctrl Pts',(-6.61586758024389,1.43524805792121,-10.764989221612));
#45564=CARTESIAN_POINT('Ctrl Pts',(-6.65143297376662,1.24528245610789,-10.7558729768031));
#45565=CARTESIAN_POINT('Ctrl Pts',(-6.68690764314078,1.05580143961126,-10.746779986722));
#45566=CARTESIAN_POINT('Ctrl Pts',(-6.71432033728555,0.864595860334953,
-10.737686996641));
#45567=CARTESIAN_POINT('Ctrl Pts',(-6.73351772814808,0.672330279487316,
-10.72859400656));
#45568=CARTESIAN_POINT('Ctrl Pts',(-6.75264138544654,0.480803154538571,
-10.7195359409419));
#45569=CARTESIAN_POINT('Ctrl Pts',(-6.763612642134,0.288224363417974,-10.7104778753239));
#45570=CARTESIAN_POINT('Ctrl Pts',(-6.76632938619459,0.0952661404672239,
-10.7014198097059));
#45571=CARTESIAN_POINT('Ctrl Pts',(-6.76675328336554,0.0651586135911492,
-10.7000064677406));
#45572=CARTESIAN_POINT('Ctrl Pts',(-6.76697631772227,0.0350418758827705,
-10.6985931257754));
#45573=CARTESIAN_POINT('Ctrl Pts',(-6.76699821252111,0.00491850953762435,
-10.6971797838101));
#45574=CARTESIAN_POINT('Ctrl Pts',(-6.767,1.02749929591548E-12,-10.6971797838101));
#45575=CARTESIAN_POINT('Ctrl Pts',(-6.76700000000003,-0.186007249559046,
-10.6884302719974));
#45576=CARTESIAN_POINT('Ctrl Pts',(-6.75932637294252,-0.372014355815296,
-10.6796807601846));
#45577=CARTESIAN_POINT('Ctrl Pts',(-6.74400518263368,-0.557389537585737,
-10.6709312483719));
#45578=CARTESIAN_POINT('Ctrl Pts',(-6.72868405703735,-0.742763936382339,
-10.6621817735147));
#45579=CARTESIAN_POINT('Ctrl Pts',(-6.70571545643567,-0.927506130404779,
-10.6534322986574));
#45580=CARTESIAN_POINT('Ctrl Pts',(-6.67517739401575,-1.11098864009542,
-10.6446828238002));
#45581=CARTESIAN_POINT('Ctrl Pts',(-6.64463945804388,-1.2944703900455,-10.6359333851717));
#45582=CARTESIAN_POINT('Ctrl Pts',(-6.6065321700272,-1.47669218339297,-10.6271839465432));
#45583=CARTESIAN_POINT('Ctrl Pts',(-6.56098496085472,-1.65703510627813,
-10.6184345079147));
#45584=CARTESIAN_POINT('Ctrl Pts',(-6.51543793649544,-1.83737729740055,
-10.609685104788));
#45585=CARTESIAN_POINT('Ctrl Pts',(-6.46245112156878,-2.01584035545013,
-10.6009357016614));
#45586=CARTESIAN_POINT('Ctrl Pts',(-6.40220448361691,-2.19181813797484,
-10.5921862985348));
#45587=CARTESIAN_POINT('Ctrl Pts',(-6.34195808511944,-2.36779522106381,
-10.5834369301833));
#45588=CARTESIAN_POINT('Ctrl Pts',(-6.27445201416322,-2.54128677725824,
-10.5746875618317));
#45589=CARTESIAN_POINT('Ctrl Pts',(-6.19991555052688,-2.7117035542874,-10.5659381934802));
#45590=CARTESIAN_POINT('Ctrl Pts',(-6.12537937695072,-2.8821196681362,-10.557188859177));
#45591=CARTESIAN_POINT('Ctrl Pts',(-6.04381298028289,-3.04946076419993,
-10.5484395248738));
#45592=CARTESIAN_POINT('Ctrl Pts',(-5.95549339308802,-3.21315848424646,
-10.5396901905706));
#45593=CARTESIAN_POINT('Ctrl Pts',(-5.86717414225629,-3.37685558085395,
-10.5309408895891));
#45594=CARTESIAN_POINT('Ctrl Pts',(-5.77210188843887,-3.53690907700292,
-10.5221915886075));
#45595=CARTESIAN_POINT('Ctrl Pts',(-5.67059953311195,-3.69277537024263,
-10.513442287626));
#45596=CARTESIAN_POINT('Ctrl Pts',(-5.56909755592501,-3.84864108281328,
-10.5046930192393));
#45597=CARTESIAN_POINT('Ctrl Pts',(-5.46116568154727,-4.00031938355157,
-10.4959437508527));
#45598=CARTESIAN_POINT('Ctrl Pts',(-5.34717048488103,-4.14729511918517,
-10.4871944824661));
#45599=CARTESIAN_POINT('Ctrl Pts',(-5.2331757034302,-4.29427031947526,-10.4784452459477));
#45600=CARTESIAN_POINT('Ctrl Pts',(-5.11311781951251,-4.43654276249897,
-10.4696960094294));
#45601=CARTESIAN_POINT('Ctrl Pts',(-4.98740458928937,-4.57362924412718,
-10.460946772911));
#45602=CARTESIAN_POINT('Ctrl Pts',(-4.86169180652416,-4.71071523781602,
-10.4521975675343));
#45603=CARTESIAN_POINT('Ctrl Pts',(-4.73032391141232,-4.84261509584822,
-10.4434483621576));
#45604=CARTESIAN_POINT('Ctrl Pts',(-4.59374706946971,-4.96888084599928,
-10.4346991567809));
#45605=CARTESIAN_POINT('Ctrl Pts',(-4.45717070231174,-5.09514615721033,
-10.4259499818192));
#45606=CARTESIAN_POINT('Ctrl Pts',(-4.31538563497053,-5.21577720520837,
-10.4172008068575));
#45607=CARTESIAN_POINT('Ctrl Pts',(-4.16887340951759,-5.33036429293695,
-10.4084516318958));
#45608=CARTESIAN_POINT('Ctrl Pts',(-4.02236168122231,-5.44495099183894,
-10.3997024866225));
#45609=CARTESIAN_POINT('Ctrl Pts',(-3.8711230526292,-5.5534935949811,-10.3909533413493));
#45610=CARTESIAN_POINT('Ctrl Pts',(-3.71567116928729,-5.65562346357387,
-10.382204196076));
#45611=CARTESIAN_POINT('Ctrl Pts',(-3.56021980053062,-5.75775299409081,
-10.3734550797647));
#45612=CARTESIAN_POINT('Ctrl Pts',(-3.40055544441853,-5.85346967520012,
-10.3647059634533));
#45613=CARTESIAN_POINT('Ctrl Pts',(-3.23722035886631,-5.94244843041498,
-10.3559568471419));
#45614=CARTESIAN_POINT('Ctrl Pts',(-3.07388580043301,-6.03142689847546,
-10.3472077590659));
#45615=CARTESIAN_POINT('Ctrl Pts',(-2.90688078789058,-6.11366734707979,
-10.33845867099));
#45616=CARTESIAN_POINT('Ctrl Pts',(-2.73677250610253,-6.1888904700149,-10.329709582914));
#45617=CARTESIAN_POINT('Ctrl Pts',(-2.56666475916788,-6.26411335643394,
-10.3209605223468));
#45618=CARTESIAN_POINT('Ctrl Pts',(-2.39345402456939,-6.33231884545314,
-10.3122114617796));
#45619=CARTESIAN_POINT('Ctrl Pts',(-2.21772855943905,-6.39327529804938,
-10.3034624012124));
#45620=CARTESIAN_POINT('Ctrl Pts',(-2.04200363223433,-6.45423156404753,
-10.2947133674276));
#45621=CARTESIAN_POINT('Ctrl Pts',(-1.86376426060878,-6.50793874412498,
-10.2859643336428));
#45622=CARTESIAN_POINT('Ctrl Pts',(-1.68361577621535,-6.55421443943352,
-10.277215299858));
#45623=CARTESIAN_POINT('Ctrl Pts',(-1.50346782833053,-6.60048999692625,
-10.2684662921291));
#45624=CARTESIAN_POINT('Ctrl Pts',(-1.32141105657216,-6.63933404265196,
-10.2597172844002));
#45625=CARTESIAN_POINT('Ctrl Pts',(-1.13806375346355,-6.6706146563156,-10.2509682766713));
#45626=CARTESIAN_POINT('Ctrl Pts',(-0.954716981168329,-6.70189517941794,
-10.2422192942719));
#45627=CARTESIAN_POINT('Ctrl Pts',(-0.770079967440725,-6.72561226609021,
-10.2334703118725));
#45628=CARTESIAN_POINT('Ctrl Pts',(-0.58477976407164,-6.74168536995997,
-10.224721329473));
#45629=CARTESIAN_POINT('Ctrl Pts',(-0.391489587591469,-6.75845153117881,
-10.2155950990574));
#45630=CARTESIAN_POINT('Ctrl Pts',(-0.197478091803694,-6.76689985146399,
-10.2064688686418));
#45631=CARTESIAN_POINT('Ctrl Pts',(-0.00346214752943487,-6.76699911434415,
-10.1973426382262));
#45632=CARTESIAN_POINT('Ctrl Pts',(0.18449079848621,-6.76709527525931,-10.1885016025111));
#45633=CARTESIAN_POINT('Ctrl Pts',(0.372447602156321,-6.75935633790754,
-10.1796605667959));
#45634=CARTESIAN_POINT('Ctrl Pts',(0.559756448195727,-6.74380914014501,
-10.1708195310808));
#45635=CARTESIAN_POINT('Ctrl Pts',(0.74513613104485,-6.72842206873138,-10.1620695524675));
#45636=CARTESIAN_POINT('Ctrl Pts',(0.929880851946518,-6.70538686355703,
-10.1533195738542));
#45637=CARTESIAN_POINT('Ctrl Pts',(1.11336305057608,-6.67478177303288,-10.1445695952409));
#45638=CARTESIAN_POINT('Ctrl Pts',(1.29684337090276,-6.64417699581231,-10.1358197062009));
#45639=CARTESIAN_POINT('Ctrl Pts',(1.47906091205349,-6.60600253548024,-10.1270698171609));
#45640=CARTESIAN_POINT('Ctrl Pts',(1.65939671095387,-6.5603880644117,-10.1183199281209));
#45641=CARTESIAN_POINT('Ctrl Pts',(1.83973072369326,-6.51477404513803,-10.1095701257455));
#45642=CARTESIAN_POINT('Ctrl Pts',(2.01818275357201,-6.46172023288609,-10.10082032337));
#45643=CARTESIAN_POINT('Ctrl Pts',(2.1941466403349,-6.40140683918052,-10.0920705209945));
#45644=CARTESIAN_POINT('Ctrl Pts',(2.37010884271419,-6.34109402281438,-10.0833208023749));
#45645=CARTESIAN_POINT('Ctrl Pts',(2.54358267847961,-6.27352185699729,-10.0745710837554));
#45646=CARTESIAN_POINT('Ctrl Pts',(2.71397890841893,-6.19891986435195,-10.0658213651359));
#45647=CARTESIAN_POINT('Ctrl Pts',(2.88437356389095,-6.12431856103171,-10.057071727364));
#45648=CARTESIAN_POINT('Ctrl Pts',(3.05169040787327,-6.04268767582479,-10.0483220895922));
#45649=CARTESIAN_POINT('Ctrl Pts',(3.2153611251221,-5.95430447953861,-10.0395724518204));
#45650=CARTESIAN_POINT('Ctrl Pts',(3.37903038442994,-5.86592207054955,-10.0308228919883));
#45651=CARTESIAN_POINT('Ctrl Pts',(3.5390533298012,-5.77078760703287,-10.0220733321563));
#45652=CARTESIAN_POINT('Ctrl Pts',(3.69488643042035,-5.66922422085206,-10.0133237723242));
#45653=CARTESIAN_POINT('Ctrl Pts',(3.85071819468886,-5.56766170563059,-10.0045742875242));
#45654=CARTESIAN_POINT('Ctrl Pts',(4.00235994599368,-5.45967053456146,-9.9958248027242));
#45655=CARTESIAN_POINT('Ctrl Pts',(4.14929662974445,-5.34561750206572,-9.9870753179242));
#45656=CARTESIAN_POINT('Ctrl Pts',(4.29623210225178,-5.23156540974356,-9.97832590524885));
#45657=CARTESIAN_POINT('Ctrl Pts',(4.43846235842242,-5.11145173172078,-9.96957649257349));
#45658=CARTESIAN_POINT('Ctrl Pts',(4.57550431797543,-4.98568443006456,-9.96082707989814));
#45659=CARTESIAN_POINT('Ctrl Pts',(4.71254519337612,-4.85991812336575,-9.95207773644024));
#45660=CARTESIAN_POINT('Ctrl Pts',(4.84439764315105,-4.72849847630977,-9.94332839298234));
#45661=CARTESIAN_POINT('Ctrl Pts',(4.9706138419681,-4.5918718442521,-9.93457904952444));
#45662=CARTESIAN_POINT('Ctrl Pts',(5.09682908420336,-4.45524624767599,-9.92582977237707));
#45663=CARTESIAN_POINT('Ctrl Pts',(5.21740796650306,-4.31341395556729,-9.91708049522971));
#45664=CARTESIAN_POINT('Ctrl Pts',(5.33194095942391,-4.16685668162677,-9.90833121808234));
#45665=CARTESIAN_POINT('Ctrl Pts',(5.44647312235277,-4.0203004697502,-9.89958200433879));
#45666=CARTESIAN_POINT('Ctrl Pts',(5.55495930712435,-3.86901957035337,-9.89083279059525));
#45667=CARTESIAN_POINT('Ctrl Pts',(5.65703106079944,-3.71352778058148,-9.88208357685171));
#45668=CARTESIAN_POINT('Ctrl Pts',(5.75910210868873,-3.55803706597381,-9.87333442360551));
#45669=CARTESIAN_POINT('Ctrl Pts',(5.85475865698675,-3.39833575880683,-9.86458527035931));
#45670=CARTESIAN_POINT('Ctrl Pts',(5.94367583069178,-3.2349662470651,-9.85583611711312));
#45671=CARTESIAN_POINT('Ctrl Pts',(6.03259241910188,-3.07159781069882,-9.847087021458));
#45672=CARTESIAN_POINT('Ctrl Pts',(6.11476958471074,-2.90456146975609,-9.83833792580288));
#45673=CARTESIAN_POINT('Ctrl Pts',(6.18992823574488,-2.73442451648026,-9.82958883014776));
#45674=CARTESIAN_POINT('Ctrl Pts',(6.26508641701031,-2.56428862662182,-9.82083978917764));
#45675=CARTESIAN_POINT('Ctrl Pts',(6.33322605570386,-2.3910524253104,-9.81209074820753));
#45676=CARTESIAN_POINT('Ctrl Pts',(6.3941157374785,-2.21530425353489,-9.80334170723741));
#45677=CARTESIAN_POINT('Ctrl Pts',(6.45500505889206,-2.03955712188307,-9.79459271804641));
#45678=CARTESIAN_POINT('Ctrl Pts',(6.50864441545006,-1.86129832025304,-9.7858437288554));
#45679=CARTESIAN_POINT('Ctrl Pts',(6.55485164049979,-1.68113324012027,-9.7770947396644));
#45680=CARTESIAN_POINT('Ctrl Pts',(6.60199852639174,-1.49730435912615,-9.76816783278752));
#45681=CARTESIAN_POINT('Ctrl Pts',(6.64140767441066,-1.31149113173366,-9.75924092591062));
#45682=CARTESIAN_POINT('Ctrl Pts',(6.6729397526965,-1.12435050446145,-9.75031401903374));
#45683=CARTESIAN_POINT('Ctrl Pts',(6.70384664831547,-0.940920291560891,
-9.74156410484975));
#45684=CARTESIAN_POINT('Ctrl Pts',(6.72718585889698,-0.756215114275096,
-9.73281419066575));
#45685=CARTESIAN_POINT('Ctrl Pts',(6.74287810451888,-0.570862389372309,
-9.72406427648176));
#45686=CARTESIAN_POINT('Ctrl Pts',(6.75857004154139,-0.385513309565321,
-9.71531453437118));
#45687=CARTESIAN_POINT('Ctrl Pts',(6.76661529035564,-0.199516993256485,
-9.7065647922606));
#45688=CARTESIAN_POINT('Ctrl Pts',(6.76698652348897,-0.0135052182023869,
-9.69781505015002));
#45689=CARTESIAN_POINT('Ctrl Pts',(6.76735774981517,0.172503146040514,-9.68906546847938));
#45690=CARTESIAN_POINT('Ctrl Pts',(6.76005524147471,0.358526681835042,-9.68031588680874));
#45691=CARTESIAN_POINT('Ctrl Pts',(6.74510380214869,0.543933542116385,-9.6715663051381));
#45692=CARTESIAN_POINT('Ctrl Pts',(6.73015261710963,0.729337249086165,-9.66281687227618));
#45693=CARTESIAN_POINT('Ctrl Pts',(6.70755278444587,0.914124015856029,-9.65406743941425));
#45694=CARTESIAN_POINT('Ctrl Pts',(6.67738106408268,1.09766621749515,-9.64531800655233));
#45695=CARTESIAN_POINT('Ctrl Pts',(6.6472098167723,1.28120554143443,-9.63656871086998));
#45696=CARTESIAN_POINT('Ctrl Pts',(6.60946696581497,1.46350005650733,-9.62781941518764));
#45697=CARTESIAN_POINT('Ctrl Pts',(6.56428070010968,1.6439306220664,-9.6190701195053));
#45698=CARTESIAN_POINT('Ctrl Pts',(6.51909508282712,1.82435859844753,-9.61032094937531));
#45699=CARTESIAN_POINT('Ctrl Pts',(6.46646633415632,2.00292240086659,-9.60157177924532));
#45700=CARTESIAN_POINT('Ctrl Pts',(6.40657319597161,2.17901557696546,-9.59282260911533));
#45701=CARTESIAN_POINT('Ctrl Pts',(6.34668083768265,2.35510646007513,-9.58407355291226));
#45702=CARTESIAN_POINT('Ctrl Pts',(6.27952437143858,2.52872650996598,-9.57532449670918));
#45703=CARTESIAN_POINT('Ctrl Pts',(6.20533187335112,2.6992860799798,-9.56657544050611));
#45704=CARTESIAN_POINT('Ctrl Pts',(6.12831449784227,2.8763397011545,-9.55749326421726));
#45705=CARTESIAN_POINT('Ctrl Pts',(6.04371489463128,3.05009490562399,-9.54841108792844));
#45706=CARTESIAN_POINT('Ctrl Pts',(5.95184265120465,3.21991584599679,-9.53932891163959));
#45707=CARTESIAN_POINT('Ctrl Pts',(5.86333281335461,3.38352155905355,-9.53057913128517));
#45708=CARTESIAN_POINT('Ctrl Pts',(5.76807337235648,3.54347560903884,-9.52182935093074));
#45709=CARTESIAN_POINT('Ctrl Pts',(5.66638790086312,3.69923467178713,-9.51307957057632));
#45710=CARTESIAN_POINT('Ctrl Pts',(5.56470608502698,3.85498813489829,-9.50433010478206));
#45711=CARTESIAN_POINT('Ctrl Pts',(5.45659885766906,4.00654667256325,-9.49558063898779));
#45712=CARTESIAN_POINT('Ctrl Pts',(5.34243340580459,4.15339551506273,-9.48683117319353));
#45713=CARTESIAN_POINT('Ctrl Pts',(5.22827145140537,4.3002398588394,-9.47808197543966));
#45714=CARTESIAN_POINT('Ctrl Pts',(5.10805181978023,4.44237456993119,-9.46933277768577));
#45715=CARTESIAN_POINT('Ctrl Pts',(4.98218281282476,4.57931691626531,-9.4605835799319));
#45716=CARTESIAN_POINT('Ctrl Pts',(4.85631699296158,4.71625579512234,-9.4518346037139));
#45717=CARTESIAN_POINT('Ctrl Pts',(4.72480227791772,4.84800236135833,-9.44308562749591));
#45718=CARTESIAN_POINT('Ctrl Pts',(4.58808530848053,4.97410918678964,-9.43433665127791));
#45719=CARTESIAN_POINT('Ctrl Pts',(4.45135945056902,5.10022421089068,-9.42558710625671));
#45720=CARTESIAN_POINT('Ctrl Pts',(4.30943087207964,5.22069856612049,-9.41683756123551));
#45721=CARTESIAN_POINT('Ctrl Pts',(4.16278164322383,5.3351230530175,-9.40808801621431));
#45722=CARTESIAN_POINT('Ctrl Pts',(4.01614103534304,5.4495408133149,-9.39933898554705));
#45723=CARTESIAN_POINT('Ctrl Pts',(3.86478055833326,5.55790924068398,-9.39058995487979));
#45724=CARTESIAN_POINT('Ctrl Pts',(3.70921425811863,5.65986029751349,-9.38184092421253));
#45725=CARTESIAN_POINT('Ctrl Pts',(3.55364584530037,5.76181273884705,-9.37309177473269));
#45726=CARTESIAN_POINT('Ctrl Pts',(3.39387173464268,5.85734747818107,-9.36434262525284));
#45727=CARTESIAN_POINT('Ctrl Pts',(3.23043456092335,5.94614005448846,-9.355593475773));
#45728=CARTESIAN_POINT('Ctrl Pts',(3.18690768806344,5.96978744811307,-9.35326338703997));
#45729=CARTESIAN_POINT('Ctrl Pts',(3.14312114982855,5.99295688499314,-9.35093329830694));
#45730=CARTESIAN_POINT('Ctrl Pts',(3.09908550384716,6.01564277861015,-9.34860320957391));
#45731=CARTESIAN_POINT('Origin',(0.,0.,-63.6971797838103));
#45732=CARTESIAN_POINT('',(3.09908550384728,6.01564277861009,-6.95401477785999));
#45733=CARTESIAN_POINT('',(3.09908550384714,6.01564277861016,-7.34868366182765));
#45734=CARTESIAN_POINT('',(3.09908550384721,6.01564277861012,-63.6971797838103));
#45735=CARTESIAN_POINT('',(-6.76699555771448,-0.00775382954289589,-8.30282021621437));
#45736=CARTESIAN_POINT('Ctrl Pts',(-6.76699555771388,-0.0077538300588502,
-8.30282021618999));
#45737=CARTESIAN_POINT('Ctrl Pts',(-6.76671757908296,-0.250353957523485,
-8.2913582776441));
#45738=CARTESIAN_POINT('Ctrl Pts',(-6.75339413019389,-0.492429368534453,
-8.27989633909821));
#45739=CARTESIAN_POINT('Ctrl Pts',(-6.72719065642958,-0.732935789852377,
-8.26843440055233));
#45740=CARTESIAN_POINT('Ctrl Pts',(-6.70813841430844,-0.907805221739758,
-8.26010055785963));
#45741=CARTESIAN_POINT('Ctrl Pts',(-6.68223907331561,-1.08215501582084,
-8.25176671516695));
#45742=CARTESIAN_POINT('Ctrl Pts',(-6.64952771791692,-1.25541631686646,
-8.24343287247425));
#45743=CARTESIAN_POINT('Ctrl Pts',(-6.61685491698888,-1.42847340754959,
-8.23510885226948));
#45744=CARTESIAN_POINT('Ctrl Pts',(-6.57738615977623,-1.60044422200792,
-8.2267848320647));
#45745=CARTESIAN_POINT('Ctrl Pts',(-6.53120830826043,-1.77076453378476,
-8.21846081185993));
#45746=CARTESIAN_POINT('Ctrl Pts',(-6.48507641654277,-1.94091532950809,
-8.21014507636905));
#45747=CARTESIAN_POINT('Ctrl Pts',(-6.43224882461589,-2.10941856173476,
-8.20182934087818));
#45748=CARTESIAN_POINT('Ctrl Pts',(-6.37286354758082,-2.275719491483,-8.1935136053873));
#45749=CARTESIAN_POINT('Ctrl Pts',(-6.3135264944873,-2.44188537620464,-8.18520462270727));
#45750=CARTESIAN_POINT('Ctrl Pts',(-6.24764248369236,-2.60585219580411,
-8.17689564002723));
#45751=CARTESIAN_POINT('Ctrl Pts',(-6.17539959654923,-2.76707947535658,
-8.1685866573472));
#45752=CARTESIAN_POINT('Ctrl Pts',(-6.10320214490235,-2.92820535473328,
-8.16028290041002));
#45753=CARTESIAN_POINT('Ctrl Pts',(-6.02465392885783,-3.08659481122614,
-8.15197914347284));
#45754=CARTESIAN_POINT('Ctrl Pts',(-5.93999155697001,-3.24172628442394,
-8.14367538653566));
#45755=CARTESIAN_POINT('Ctrl Pts',(-5.85536355596431,-3.39679477798321,
-8.13537500072362));
#45756=CARTESIAN_POINT('Ctrl Pts',(-5.76462651144932,-3.54860761892777,
-8.12707461491158));
#45757=CARTESIAN_POINT('Ctrl Pts',(-5.66806361718742,-3.69666658376384,
-8.11877422909955));
#45758=CARTESIAN_POINT('Ctrl Pts',(-5.57152108552739,-3.84469432681668,
-8.11047559362291));
#45759=CARTESIAN_POINT('Ctrl Pts',(-5.46915534151305,-3.98896947966734,
-8.10217695814627));
#45760=CARTESIAN_POINT('Ctrl Pts',(-5.36129379228389,-4.12902141830462,
-8.09387832266963));
#45761=CARTESIAN_POINT('Ctrl Pts',(-5.25343708446977,-4.26906707064649,
-8.08558005968105));
#45762=CARTESIAN_POINT('Ctrl Pts',(-5.14008527535029,-4.40488961110492,
-8.07728179669246));
#45763=CARTESIAN_POINT('Ctrl Pts',(-5.02160718726101,-4.53605007212757,
-8.06898353370387));
#45764=CARTESIAN_POINT('Ctrl Pts',(-4.90311475198104,-4.66722641612214,
-8.06068426583106));
#45765=CARTESIAN_POINT('Ctrl Pts',(-4.77949503433162,-4.79373929806913,
-8.05238499795825));
#45766=CARTESIAN_POINT('Ctrl Pts',(-4.65115509386475,-4.91518517380739,
-8.04408573008544));
#45767=CARTESIAN_POINT('Ctrl Pts',(-4.52272503807419,-5.03671632412474,
-8.03578063478893));
#45768=CARTESIAN_POINT('Ctrl Pts',(-4.38956838971817,-5.15317311968058,
-8.02747553949242));
#45769=CARTESIAN_POINT('Ctrl Pts',(-4.2521274748599,-5.2641904351516,-8.01917044419591));
#45770=CARTESIAN_POINT('Ctrl Pts',(-4.1146364418973,-5.37524823330862,-8.0108623204298));
#45771=CARTESIAN_POINT('Ctrl Pts',(-3.97285830377808,-5.48086238521259,
-8.00255419666371));
#45772=CARTESIAN_POINT('Ctrl Pts',(-3.82726617535817,-5.58070986729818,
-7.9942460728976));
#45773=CARTESIAN_POINT('Ctrl Pts',(-3.68151928334678,-5.68066348668044,
-7.98592911764392));
#45774=CARTESIAN_POINT('Ctrl Pts',(-3.53195059187763,-5.7748379980757,-7.97761216239025));
#45775=CARTESIAN_POINT('Ctrl Pts',(-3.37906066141835,-5.86295471980255,
-7.96929520713657));
#45776=CARTESIAN_POINT('Ctrl Pts',(-3.26638310883645,-5.92789540305026,
-7.96316573765416));
#45777=CARTESIAN_POINT('Ctrl Pts',(-3.15190219783778,-5.98954675271497,
-7.95703626817173));
#45778=CARTESIAN_POINT('Ctrl Pts',(-3.03582580395668,-6.04781371141926,
-7.95090679868932));
#45779=CARTESIAN_POINT('Ctrl Pts',(-2.87578514493605,-6.12814944686357,
-7.94245577516412));
#45780=CARTESIAN_POINT('Ctrl Pts',(-2.71241830995243,-6.20219665234776,
-7.9340047516389));
#45781=CARTESIAN_POINT('Ctrl Pts',(-2.54624649463297,-6.26968243123759,
-7.92555372811368));
#45782=CARTESIAN_POINT('Ctrl Pts',(-2.38022098865794,-6.33710879090492,
-7.9171101454635));
#45783=CARTESIAN_POINT('Ctrl Pts',(-2.21139573062863,-6.39798511476414,
-7.90866656281331));
#45784=CARTESIAN_POINT('Ctrl Pts',(-2.04031455288437,-6.45208536252337,
-7.90022298016313));
#45785=CARTESIAN_POINT('Ctrl Pts',(-1.86936075040631,-6.50614533096285,
-7.89178568402326));
#45786=CARTESIAN_POINT('Ctrl Pts',(-1.69615469144868,-6.55343918065076,
-7.88334838788341));
#45787=CARTESIAN_POINT('Ctrl Pts',(-1.52125851104757,-6.59378961922242,
-7.87491109174353));
#45788=CARTESIAN_POINT('Ctrl Pts',(-1.34648710573618,-6.63411127083269,
-7.86647981497115));
#45789=CARTESIAN_POINT('Ctrl Pts',(-1.17002830631589,-6.66749931776143,
-7.85804853819875));
#45790=CARTESIAN_POINT('Ctrl Pts',(-0.992457877972095,-6.69382673516809,
-7.84961726142637));
#45791=CARTESIAN_POINT('Ctrl Pts',(-0.814963562742269,-6.72014286769056,
-7.84118959860444));
#45792=CARTESIAN_POINT('Ctrl Pts',(-0.636358895781466,-6.73940435551116,
-7.8327619357825));
#45793=CARTESIAN_POINT('Ctrl Pts',(-0.457228919895582,-6.75153543387066,
-7.82433427296057));
#45794=CARTESIAN_POINT('Ctrl Pts',(-0.278154087300592,-6.76366277780448,
-7.81590920450656));
#45795=CARTESIAN_POINT('Ctrl Pts',(-0.0985545986133285,-6.76866406733705,
-7.80748413605254));
#45796=CARTESIAN_POINT('Ctrl Pts',(0.0809799350677422,-6.76651544372112,
-7.79905906759853));
#45797=CARTESIAN_POINT('Ctrl Pts',(0.130106078891218,-6.76592751453216,
-7.79675371098491));
#45798=CARTESIAN_POINT('Ctrl Pts',(0.179227345766093,-6.76480454548256,
-7.7944483543713));
#45799=CARTESIAN_POINT('Ctrl Pts',(0.228331639799978,-6.76314672783803,
-7.79214299775768));
#45800=CARTESIAN_POINT('Ctrl Pts',(0.411916836239953,-6.75694867970556,
-7.78352400923331));
#45801=CARTESIAN_POINT('Ctrl Pts',(0.595182676320826,-6.74327344386702,
-7.77490502070893));
#45802=CARTESIAN_POINT('Ctrl Pts',(0.777515869642375,-6.72218402548266,
-7.76628603218456));
#45803=CARTESIAN_POINT('Ctrl Pts',(0.959958296818278,-6.70108197265465,
-7.7576618801169));
#45804=CARTESIAN_POINT('Ctrl Pts',(1.14146666002476,-6.67255690783578,-7.74903772804925));
#45805=CARTESIAN_POINT('Ctrl Pts',(1.32143549775019,-6.63672338019943,-7.74041357598159));
#45806=CARTESIAN_POINT('Ctrl Pts',(1.50756831658762,-6.59966254460066,-7.73149404438532));
#45807=CARTESIAN_POINT('Ctrl Pts',(1.69205393505231,-6.5547838266985,-7.72257451278904));
#45808=CARTESIAN_POINT('Ctrl Pts',(1.87423760706012,-6.50227055668107,-7.71365498119277));
#45809=CARTESIAN_POINT('Ctrl Pts',(2.05071622586826,-6.4514017315024,-7.70501476333362));
#45810=CARTESIAN_POINT('Ctrl Pts',(2.22503461206296,-6.39336940769518,-7.69637454547447));
#45811=CARTESIAN_POINT('Ctrl Pts',(2.39661579557263,-6.32839013718432,-7.68773432761533));
#45812=CARTESIAN_POINT('Ctrl Pts',(2.57651707859292,-6.26025997340115,-7.67867513915049));
#45813=CARTESIAN_POINT('Ctrl Pts',(2.75340874473678,-6.18449254074994,-7.66961595068564));
#45814=CARTESIAN_POINT('Ctrl Pts',(2.92665188325398,-6.10139309946884,-7.66055676222079));
#45815=CARTESIAN_POINT('Ctrl Pts',(3.09989502177124,-6.01829365818771,-7.65149757375595));
#45816=CARTESIAN_POINT('Ctrl Pts',(3.26948931062098,-5.92786241753779,-7.64243838529112));
#45817=CARTESIAN_POINT('Ctrl Pts',(3.43482749781613,-5.83045873497499,-7.63337919682628));
#45818=CARTESIAN_POINT('Ctrl Pts',(3.59987924820414,-5.73322379745719,-7.62433570276974));
#45819=CARTESIAN_POINT('Ctrl Pts',(3.76084211478365,-5.62895170816136,-7.61529220871318));
#45820=CARTESIAN_POINT('Ctrl Pts',(3.91714428998133,-5.5179950717146,-7.60624871465665));
#45821=CARTESIAN_POINT('Ctrl Pts',(4.07330349615089,-5.40713992689748,-7.59721349265107));
#45822=CARTESIAN_POINT('Ctrl Pts',(4.22481032829184,-5.2896125799144,-7.5881782706455));
#45823=CARTESIAN_POINT('Ctrl Pts',(4.37112219132356,-5.16580872550647,-7.57914304863991));
#45824=CARTESIAN_POINT('Ctrl Pts',(4.51717628470422,-5.04222298653832,-7.57012374472856));
#45825=CARTESIAN_POINT('Ctrl Pts',(4.65805350367384,-4.91238297486737,-7.5611044408172));
#45826=CARTESIAN_POINT('Ctrl Pts',(4.79324465710423,-4.77672426011192,-7.55208513690585));
#45827=CARTESIAN_POINT('Ctrl Pts',(4.92826620378978,-4.64123573868965,-7.54307714834124));
#45828=CARTESIAN_POINT('Ctrl Pts',(5.05761575351991,-4.49994325055495,-7.53406915977664));
#45829=CARTESIAN_POINT('Ctrl Pts',(5.18081939652793,-4.35332050055587,-7.52506117121203));
#45830=CARTESIAN_POINT('Ctrl Pts',(5.30374477979261,-4.2070289031736,-7.51607352750513));
#45831=CARTESIAN_POINT('Ctrl Pts',(5.42055181069141,-4.0554312559849,-7.5070858837982));
#45832=CARTESIAN_POINT('Ctrl Pts',(5.53080574651703,-3.89903536715098,-7.49809824009129));
#45833=CARTESIAN_POINT('Ctrl Pts',(5.62682928288425,-3.76282538782762,-7.49027062535915));
#45834=CARTESIAN_POINT('Ctrl Pts',(5.71788263937237,-3.62297647889661,-7.48244301062701));
#45835=CARTESIAN_POINT('Ctrl Pts',(5.80370247531395,-3.47984576928845,-7.47461539589487));
#45836=CARTESIAN_POINT('Ctrl Pts',(5.89276257202811,-3.33131093814352,-7.46649223744977));
#45837=CARTESIAN_POINT('Ctrl Pts',(5.97614524251994,-3.17930734502623,-7.45836907900467));
#45838=CARTESIAN_POINT('Ctrl Pts',(6.05357768438367,-3.02431582661798,-7.45024592055957));
#45839=CARTESIAN_POINT('Ctrl Pts',(6.13100466685498,-2.869335235923,-7.44212333483966));
#45840=CARTESIAN_POINT('Ctrl Pts',(6.20248209276141,-2.71136746699568,-7.43400074911974));
#45841=CARTESIAN_POINT('Ctrl Pts',(6.26778362790867,-2.5509169711537,-7.42587816339983));
#45842=CARTESIAN_POINT('Ctrl Pts',(6.33309300970753,-2.39044719553316,-7.41775460166764));
#45843=CARTESIAN_POINT('Ctrl Pts',(6.39222488619314,-2.22749443842895,-7.40963103993543));
#45844=CARTESIAN_POINT('Ctrl Pts',(6.44500149845093,-2.06258204320829,-7.40150747820324));
#45845=CARTESIAN_POINT('Ctrl Pts',(6.49781655220792,-1.89754952887733,-7.39337799942033));
#45846=CARTESIAN_POINT('Ctrl Pts',(6.54426698461811,-1.73055487457134,-7.38524852063744));
#45847=CARTESIAN_POINT('Ctrl Pts',(6.58422507744907,-1.56213607905675,-7.37711904185452));
#45848=CARTESIAN_POINT('Ctrl Pts',(6.62419946049119,-1.39364862216351,-7.36898624882619));
#45849=CARTESIAN_POINT('Ctrl Pts',(6.65767615736533,-1.2237362256238,-7.36085345579785));
#45850=CARTESIAN_POINT('Ctrl Pts',(6.68457884990569,-1.05294567732319,-7.35272066276952));
#45851=CARTESIAN_POINT('Ctrl Pts',(6.71151079504283,-0.881969420211572,
-7.34457902656258));
#45852=CARTESIAN_POINT('Ctrl Pts',(6.73185441557633,-0.710113467223356,
-7.33643739035563));
#45853=CARTESIAN_POINT('Ctrl Pts',(6.74558532148725,-0.537929057158783,
-7.32829575414868));
#45854=CARTESIAN_POINT('Ctrl Pts',(6.75258103154576,-0.450203438964313,
-7.32414770108685));
#45855=CARTESIAN_POINT('Ctrl Pts',(6.75786107417153,-0.362392569416437,
-7.31999964802502));
#45856=CARTESIAN_POINT('Ctrl Pts',(6.76142742199599,-0.274569148085876,
-7.31585159496318));
#45857=CARTESIAN_POINT('Ctrl Pts',(6.76868444717152,-0.095860617407945,
-7.30741087998507));
#45858=CARTESIAN_POINT('Ctrl Pts',(6.76885744666228,0.0832678398555202,
-7.29897016500697));
#45859=CARTESIAN_POINT('Ctrl Pts',(6.7619172104908,0.262230125020561,-7.29052945002885));
#45860=CARTESIAN_POINT('Ctrl Pts',(6.75498222007681,0.441057142058771,-7.28209511494079));
#45861=CARTESIAN_POINT('Ctrl Pts',(6.74094472464119,0.619717905404618,-7.2736607798527));
#45862=CARTESIAN_POINT('Ctrl Pts',(6.71982756392381,0.797625545685325,-7.26522644476464));
#45863=CARTESIAN_POINT('Ctrl Pts',(6.69872312177031,0.975426034738707,-7.25679718955598));
#45864=CARTESIAN_POINT('Ctrl Pts',(6.67054755442464,1.15247397477357,-7.24836793434734));
#45865=CARTESIAN_POINT('Ctrl Pts',(6.63537563012189,1.32818645045964,-7.23993867913868));
#45866=CARTESIAN_POINT('Ctrl Pts',(6.60021949425791,1.50382005000461,-7.23151320776563));
#45867=CARTESIAN_POINT('Ctrl Pts',(6.55807332882956,1.6781190541158,-7.22308773639258));
#45868=CARTESIAN_POINT('Ctrl Pts',(6.50906327505818,1.85050919513761,-7.21466226501953));
#45869=CARTESIAN_POINT('Ctrl Pts',(6.46006771008052,2.02284837263255,-7.20623928446025));
#45870=CARTESIAN_POINT('Ctrl Pts',(6.40421239445543,2.19327949204761,-7.19781630390098));
#45871=CARTESIAN_POINT('Ctrl Pts',(6.3416738574515,2.36124155598623,-7.1893933233417));
#45872=CARTESIAN_POINT('Ctrl Pts',(6.27913428493913,2.52920640102819,-7.18097020331533));
#45873=CARTESIAN_POINT('Ctrl Pts',(6.20991138006599,2.69470179422524,-7.17254708328897));
#45874=CARTESIAN_POINT('Ctrl Pts',(6.13423076569902,2.85718426307293,-7.1641239632626));
#45875=CARTESIAN_POINT('Ctrl Pts',(6.05854753417025,3.01967235083525,-7.15570055195071));
#45876=CARTESIAN_POINT('Ctrl Pts',(5.97640628854111,3.17914700411167,-7.1472771406388));
#45877=CARTESIAN_POINT('Ctrl Pts',(5.88807986886808,3.33508687410546,-7.1388537293269));
#45878=CARTESIAN_POINT('Ctrl Pts',(5.79973807630137,3.49105388486925,-7.13042885195075));
#45879=CARTESIAN_POINT('Ctrl Pts',(5.70520912781137,3.64348459561988,-7.1220039745746));
#45880=CARTESIAN_POINT('Ctrl Pts',(5.60481086472979,3.7918839869657,-7.11357909719845));
#45881=CARTESIAN_POINT('Ctrl Pts',(5.50438112135551,3.9403299095575,-7.10515157816698));
#45882=CARTESIAN_POINT('Ctrl Pts',(5.3980785810301,4.08474171648936,-7.09672405913553));
#45883=CARTESIAN_POINT('Ctrl Pts',(5.28626348908012,4.22465469879119,-7.08829654010406));
#45884=CARTESIAN_POINT('Ctrl Pts',(5.17434812567725,4.36469314964802,-7.07986146359924));
#45885=CARTESIAN_POINT('Ctrl Pts',(5.05691054133703,4.50022445385707,-7.07142638709441));
#45886=CARTESIAN_POINT('Ctrl Pts',(4.93435096967174,4.6308173693312,-7.0629913105896));
#45887=CARTESIAN_POINT('Ctrl Pts',(4.81173216415882,4.7614734012209,-7.05455215735678));
#45888=CARTESIAN_POINT('Ctrl Pts',(4.68398666818812,4.88718604682869,-7.04611300412398));
#45889=CARTESIAN_POINT('Ctrl Pts',(4.55155079222759,5.00756172061538,-7.03767385089117));
#45890=CARTESIAN_POINT('Ctrl Pts',(4.4189677428777,5.12807116552548,-7.02922531939302));
#45891=CARTESIAN_POINT('Ctrl Pts',(4.28168415078579,5.2432315696701,-7.02077678789487));
#45892=CARTESIAN_POINT('Ctrl Pts',(4.14016947228494,5.35268958008587,-7.01232825639672));
#45893=CARTESIAN_POINT('Ctrl Pts',(4.06197802096618,5.41316868220828,-7.00766016863119));
#45894=CARTESIAN_POINT('Ctrl Pts',(3.98249538951366,5.47190764087666,-7.00299208086567));
#45895=CARTESIAN_POINT('Ctrl Pts',(3.90180444135521,5.52885260261302,-6.99832399310014));
#45896=CARTESIAN_POINT('Ctrl Pts',(3.75936801179357,5.6293723909705,-6.99008384015391));
#45897=CARTESIAN_POINT('Ctrl Pts',(3.61284801776542,5.72452318394757,-6.98184368720769));
#45898=CARTESIAN_POINT('Ctrl Pts',(3.46268485834673,5.81395756535738,-6.97360353426146));
#45899=CARTESIAN_POINT('Ctrl Pts',(3.34369396220178,5.88482632725157,-6.9670739487943));
#45900=CARTESIAN_POINT('Ctrl Pts',(3.22241623088389,5.95210634827264,-6.96054436332713));
#45901=CARTESIAN_POINT('Ctrl Pts',(3.09908550384728,6.01564277861009,-6.95401477785997));
#45902=CARTESIAN_POINT('Ctrl Pts',(3.09908550384723,6.01564277861011,-8.95438620791577));
#45903=CARTESIAN_POINT('Ctrl Pts',(2.93072002576928,6.10237981264993,-8.94545369149881));
#45904=CARTESIAN_POINT('Ctrl Pts',(2.75883745800324,6.18197965111236,-8.93652117508186));
#45905=CARTESIAN_POINT('Ctrl Pts',(2.58404611684415,6.2541981633158,-8.92758865866489));
#45906=CARTESIAN_POINT('Ctrl Pts',(2.42685614408101,6.31914432077974,-8.91955564053608));
#45907=CARTESIAN_POINT('Ctrl Pts',(2.26731409375055,6.37812149969473,-8.9115226224073));
#45908=CARTESIAN_POINT('Ctrl Pts',(2.10587265006943,6.43098665693606,-8.9034896042785));
#45909=CARTESIAN_POINT('Ctrl Pts',(1.94059351320184,6.48510849430313,-8.89526562986093));
#45910=CARTESIAN_POINT('Ctrl Pts',(1.77300748142415,6.53292637318214,-8.88704165544333));
#45911=CARTESIAN_POINT('Ctrl Pts',(1.60363612383975,6.57424065442666,-8.87881768102576));
#45912=CARTESIAN_POINT('Ctrl Pts',(1.43444363884181,6.61551130378176,-8.87060239192308));
#45913=CARTESIAN_POINT('Ctrl Pts',(1.26346992815423,6.65029194857872,-8.86238710282042));
#45914=CARTESIAN_POINT('Ctrl Pts',(1.09125379238239,6.67843201362498,-8.85417181371775));
#45915=CARTESIAN_POINT('Ctrl Pts',(0.919184990673696,6.70654800432942,-8.8459635529456));
#45916=CARTESIAN_POINT('Ctrl Pts',(0.745876232693255,6.72803467234293,-8.83775529217344));
#45917=CARTESIAN_POINT('Ctrl Pts',(0.571878736844368,6.74279198183848,-8.82954703140128));
#45918=CARTESIAN_POINT('Ctrl Pts',(0.397995208792228,6.75753962534407,-8.82134414701337));
#45919=CARTESIAN_POINT('Ctrl Pts',(0.223424197492965,6.76556665982803,-8.81314126262547));
#45920=CARTESIAN_POINT('Ctrl Pts',(0.048724402896398,6.76682458266523,-8.80493837823756));
#45921=CARTESIAN_POINT('Ctrl Pts',(-0.125895987817598,6.76808193375615,
-8.79673922219329));
#45922=CARTESIAN_POINT('Ctrl Pts',(-0.300644687367139,6.7625763001542,-8.78854006614903));
#45923=CARTESIAN_POINT('Ctrl Pts',(-0.474960524675801,6.75031121504777,
-8.78034091010476));
#45924=CARTESIAN_POINT('Ctrl Pts',(-0.649261200744174,6.73804719670559,
-8.77214246718775));
#45925=CARTESIAN_POINT('Ctrl Pts',(-0.823128731524467,6.71902491452393,
-8.76394402427075));
#45926=CARTESIAN_POINT('Ctrl Pts',(-0.996004230675472,6.6932999762805,-8.75574558135374));
#45927=CARTESIAN_POINT('Ctrl Pts',(-1.16887800819147,6.66757529422696,-8.74754722008351));
#45928=CARTESIAN_POINT('Ctrl Pts',(-1.34075941880886,6.63514814081499,-8.73934885881327));
#45929=CARTESIAN_POINT('Ctrl Pts',(-1.51109708595469,6.59612572627442,-8.73115049754303));
#45930=CARTESIAN_POINT('Ctrl Pts',(-1.68146399979623,6.55709661164982,-8.72295072862773));
#45931=CARTESIAN_POINT('Ctrl Pts',(-1.8502862924431,6.51147005993338,-8.71475095971243));
#45932=CARTESIAN_POINT('Ctrl Pts',(-2.01702507398081,6.45940390832875,-8.70655119079712));
#45933=CARTESIAN_POINT('Ctrl Pts',(-2.18382277389909,6.40731935876471,-8.69834852443288));
#45934=CARTESIAN_POINT('Ctrl Pts',(-2.34853515395549,6.34879078336805,-8.69014585806862));
#45935=CARTESIAN_POINT('Ctrl Pts',(-2.5106406653547,6.28402517893327,-8.68194319170438));
#45936=CARTESIAN_POINT('Ctrl Pts',(-2.6729302880974,6.21918601695969,-8.67373120916136));
#45937=CARTESIAN_POINT('Ctrl Pts',(-2.83260679374606,6.14809580730292,-8.66551922661835));
#45938=CARTESIAN_POINT('Ctrl Pts',(-2.98916976489375,6.07100923378025,-8.65730724407533));
#45939=CARTESIAN_POINT('Ctrl Pts',(-3.14582507899738,5.99387719355488,-8.64909041799404));
#45940=CARTESIAN_POINT('Ctrl Pts',(-3.29936288309264,5.910741909992,-8.64087359191275));
#45941=CARTESIAN_POINT('Ctrl Pts',(-3.44930949280502,5.82190286958183,-8.63265676583146));
#45942=CARTESIAN_POINT('Ctrl Pts',(-3.59948734184626,5.73292682654039,-8.62442726821761));
#45943=CARTESIAN_POINT('Ctrl Pts',(-3.74606262823561,5.63822964354398,-8.61619777060375));
#45944=CARTESIAN_POINT('Ctrl Pts',(-3.88859157399989,5.5381535344027,-8.6079682729899));
#45945=CARTESIAN_POINT('Ctrl Pts',(-4.01563580328179,5.44894995482657,-8.60063284946506));
#45946=CARTESIAN_POINT('Ctrl Pts',(-4.13946546436669,5.3554734108814,-8.59329742594022));
#45947=CARTESIAN_POINT('Ctrl Pts',(-4.25979033663362,5.25799156407871,-8.58596200241539));
#45948=CARTESIAN_POINT('Ctrl Pts',(-4.39058181114603,5.15203014279224,-8.57798849834336));
#45949=CARTESIAN_POINT('Ctrl Pts',(-4.51767880598209,5.04097313569127,-8.57001499427135));
#45950=CARTESIAN_POINT('Ctrl Pts',(-4.64064040705468,4.92511376644351,-8.56204149019932));
#45951=CARTESIAN_POINT('Ctrl Pts',(-4.76344931244249,4.80939827321535,-8.5540778877523));
#45952=CARTESIAN_POINT('Ctrl Pts',(-4.88213276429453,4.6888925373059,-8.54611428530528));
#45953=CARTESIAN_POINT('Ctrl Pts',(-4.99627964831274,4.56393236977236,-8.53815068285827));
#45954=CARTESIAN_POINT('Ctrl Pts',(-5.11031082616481,4.43909886940131,-8.53019515279899));
#45955=CARTESIAN_POINT('Ctrl Pts',(-5.21981432897755,4.30982019869699,-8.52223962273972));
#45956=CARTESIAN_POINT('Ctrl Pts',(-5.32441308937246,4.17647150759097,-8.51428409268045));
#45957=CARTESIAN_POINT('Ctrl Pts',(-5.42892960616438,4.04322766549818,-8.50633481787175));
#45958=CARTESIAN_POINT('Ctrl Pts',(-5.5285488193977,3.90592046881269,-8.49838554306304));
#45959=CARTESIAN_POINT('Ctrl Pts',(-5.62293159514742,3.7649607270585,-8.49043626825434));
#45960=CARTESIAN_POINT('Ctrl Pts',(-5.71726578799842,3.62407354338288,-8.48249108528136));
#45961=CARTESIAN_POINT('Ctrl Pts',(-5.80636869352626,3.47953787092645,-8.47454590230839));
#45962=CARTESIAN_POINT('Ctrl Pts',(-5.88994255353325,3.33179616964757,-8.46660071933541));
#45963=CARTESIAN_POINT('Ctrl Pts',(-5.97349419453688,3.18409374707804,-8.45865764867419));
#45964=CARTESIAN_POINT('Ctrl Pts',(-6.05151952528861,3.0331873225431,-8.45071457801297));
#45965=CARTESIAN_POINT('Ctrl Pts',(-6.12376519705261,2.87954663295581,-8.44277150735175));
#45966=CARTESIAN_POINT('Ctrl Pts',(-6.19600647268141,2.72591529237488,-8.43482892002485));
#45967=CARTESIAN_POINT('Ctrl Pts',(-6.26246862651552,2.56955036320333,-8.42688633269795));
#45968=CARTESIAN_POINT('Ctrl Pts',(-6.32294531131199,2.41094412837747,-8.41894374537105));
#45969=CARTESIAN_POINT('Ctrl Pts',(-6.38343071629526,2.25231502397794,-8.41100001279543));
#45970=CARTESIAN_POINT('Ctrl Pts',(-6.43792880016635,2.09144432801209,-8.4030562802198));
#45971=CARTESIAN_POINT('Ctrl Pts',(-6.48628229156297,1.92884188936176,-8.39511254764418));
#45972=CARTESIAN_POINT('Ctrl Pts',(-6.53467837228234,1.76609623193776,-8.38716181829996));
#45973=CARTESIAN_POINT('Ctrl Pts',(-6.57691894305228,1.60161615197891,-8.37921108895577));
#45974=CARTESIAN_POINT('Ctrl Pts',(-6.61289718464963,1.4359247282685,-8.37126035961155));
#45975=CARTESIAN_POINT('Ctrl Pts',(-6.64889153959868,1.27015909736887,-8.36330606942354));
#45976=CARTESIAN_POINT('Ctrl Pts',(-6.67861791486571,1.10318141787854,-8.35535177923551));
#45977=CARTESIAN_POINT('Ctrl Pts',(-6.70202119829351,0.935521703449177,
-8.3473974890475));
#45978=CARTESIAN_POINT('Ctrl Pts',(-6.72545661367217,0.767631797657053,
-8.33943227787645));
#45979=CARTESIAN_POINT('Ctrl Pts',(-6.742551560049,0.599058365788259,-8.33146706670544));
#45980=CARTESIAN_POINT('Ctrl Pts',(-6.75330301016183,0.430334117795963,
-8.32350185553439));
#45981=CARTESIAN_POINT('Ctrl Pts',(-6.76260837606804,0.284303503474789,
-8.31660797576105));
#45982=CARTESIAN_POINT('Ctrl Pts',(-6.76716275029939,0.138160066701469,
-8.30971409598767));
#45983=CARTESIAN_POINT('Ctrl Pts',(-6.76699555771448,-0.0077538295429859,
-8.30282021621433));
#45984=CARTESIAN_POINT('',(-6.76715677348915,-0.000698709272743195,-8.69690852530228));
#45985=CARTESIAN_POINT('Ctrl Pts',(3.09908550384716,6.01564277861015,-9.34860320957391));
#45986=CARTESIAN_POINT('Ctrl Pts',(2.93373232018315,6.10082796552487,-9.33985376167461));
#45987=CARTESIAN_POINT('Ctrl Pts',(2.76486502144403,6.17919158180201,-9.33110431377533));
#45988=CARTESIAN_POINT('Ctrl Pts',(2.59305716434318,6.25046746591393,-9.32235486587604));
#45989=CARTESIAN_POINT('Ctrl Pts',(2.4212506945925,6.32174277447237,-9.31360548862862));
#45990=CARTESIAN_POINT('Ctrl Pts',(2.24650397871026,6.38593035557837,-9.30485611138119));
#45991=CARTESIAN_POINT('Ctrl Pts',(2.0694105332374,6.44281220003549,-9.29610673413378));
#45992=CARTESIAN_POINT('Ctrl Pts',(1.89231845896649,6.49969360406696,-9.28735742463118));
#45993=CARTESIAN_POINT('Ctrl Pts',(1.71287996431467,6.54926929700891,-9.27860811512858));
#45994=CARTESIAN_POINT('Ctrl Pts',(1.53170449173462,6.59137090065489,-9.26985880562599));
#45995=CARTESIAN_POINT('Ctrl Pts',(1.35053036178131,6.63347219230091,-9.2611095609614));
#45996=CARTESIAN_POINT('Ctrl Pts',(1.16761955878807,6.66809944062461,-9.2523603162968));
#45997=CARTESIAN_POINT('Ctrl Pts',(0.983593309310145,6.69513503985396,-9.24361107163221));
#45998=CARTESIAN_POINT('Ctrl Pts',(0.79956836245968,6.72217044771218,-9.23486188889904));
#45999=CARTESIAN_POINT('Ctrl Pts',(0.614428268438334,6.74161427235979,-9.22611270616587));
#46000=CARTESIAN_POINT('Ctrl Pts',(0.428801816330049,6.75340047696803,-9.2173635234327));
#46001=CARTESIAN_POINT('Ctrl Pts',(0.24317661652258,6.76518660206243,-9.20861439972456));
#46002=CARTESIAN_POINT('Ctrl Pts',(0.0570653511652714,6.76931519233997,
-9.19986527601643));
#46003=CARTESIAN_POINT('Ctrl Pts',(-0.128899900800203,6.76577222610795,
-9.1911161523083));
#46004=CARTESIAN_POINT('Ctrl Pts',(-0.314863959942112,6.76222928260132,
-9.18236708471904));
#46005=CARTESIAN_POINT('Ctrl Pts',(-0.50068172108069,6.75101488651276,-9.17361801712978));
#46006=CARTESIAN_POINT('Ctrl Pts',(-0.685722110173226,6.73216712415992,
-9.16486894954052));
#46007=CARTESIAN_POINT('Ctrl Pts',(-0.8707613738276,6.71331947644145,-9.15611993516416));
#46008=CARTESIAN_POINT('Ctrl Pts',(-1.05502298984348,6.68683858439996,-9.14737092078779));
#46009=CARTESIAN_POINT('Ctrl Pts',(-1.2378811767607,6.65281438131424,-9.13862190641143));
#46010=CARTESIAN_POINT('Ctrl Pts',(-1.43009641451804,6.61704912302375,-9.1294251955239));
#46011=CARTESIAN_POINT('Ctrl Pts',(-1.62076048992708,6.57294837083162,-9.12022848463638));
#46012=CARTESIAN_POINT('Ctrl Pts',(-1.80915798961144,6.52067760042046,-9.11103177374885));
#46013=CARTESIAN_POINT('Ctrl Pts',(-1.98840443003024,6.47094578577405,-9.10228177604234));
#46014=CARTESIAN_POINT('Ctrl Pts',(-2.16559895952203,6.41381888474472,-9.09353177833584));
#46015=CARTESIAN_POINT('Ctrl Pts',(-2.34013966242333,6.3494909528523,-9.08478178062933));
#46016=CARTESIAN_POINT('Ctrl Pts',(-2.51467682554023,6.28516432556682,-9.07603196037774));
#46017=CARTESIAN_POINT('Ctrl Pts',(-2.68656000078848,6.21363705879658,-9.06728214012614));
#46018=CARTESIAN_POINT('Ctrl Pts',(-2.85520533840891,6.13515211510858,-9.05853231987454));
#46019=CARTESIAN_POINT('Ctrl Pts',(-3.02384747998335,6.05666865881118,-9.0497826654433));
#46020=CARTESIAN_POINT('Ctrl Pts',(-3.18925164684549,5.97122791039838,-9.04103301101204));
#46021=CARTESIAN_POINT('Ctrl Pts',(-3.35085601829174,5.87912008251899,-9.03228335658079));
#46022=CARTESIAN_POINT('Ctrl Pts',(-3.51245754191436,5.78701387778163,-9.02353385633765));
#46023=CARTESIAN_POINT('Ctrl Pts',(-3.67025915510956,5.6882409706097,-9.01478435609451));
#46024=CARTESIAN_POINT('Ctrl Pts',(-3.82372487928856,5.5831368465684,-9.00603485585137));
#46025=CARTESIAN_POINT('Ctrl Pts',(-3.97718810300831,5.47803443501749,-8.99728549816624));
#46026=CARTESIAN_POINT('Ctrl Pts',(-4.1263153426307,5.36660117496342,-8.98853614048113));
#46027=CARTESIAN_POINT('Ctrl Pts',(-4.2706000988628,5.24921554097306,-8.979786782796));
#46028=CARTESIAN_POINT('Ctrl Pts',(-4.41488269594284,5.13183166360231,-8.97103755604081));
#46029=CARTESIAN_POINT('Ctrl Pts',(-4.55432273235174,5.00849577139394,-8.96228832928563));
#46030=CARTESIAN_POINT('Ctrl Pts',(-4.68844662480306,4.87962675277247,-8.95353910253043));
#46031=CARTESIAN_POINT('Ctrl Pts',(-4.82256868835247,4.75075949139791,-8.94478999507895));
#46032=CARTESIAN_POINT('Ctrl Pts',(-4.95137454637943,4.61635945312439,-8.93604088762745));
#46033=CARTESIAN_POINT('Ctrl Pts',(-5.0744267446115,4.47688309134509,-8.92729178017596));
#46034=CARTESIAN_POINT('Ctrl Pts',(-5.19747742838613,4.33740844616262,-8.91854278040359));
#46035=CARTESIAN_POINT('Ctrl Pts',(-5.31477440451004,4.19285781735932,-8.90979378063122));
#46036=CARTESIAN_POINT('Ctrl Pts',(-5.42591931531231,4.04372211999301,-8.90104478085884));
#46037=CARTESIAN_POINT('Ctrl Pts',(-5.53707636463062,3.89457013500687,-8.89229482557826));
#46038=CARTESIAN_POINT('Ctrl Pts',(-5.64207983273552,3.74083230916297,-8.88354487029768));
#46039=CARTESIAN_POINT('Ctrl Pts',(-5.7405730346883,3.58303087251695,-8.8747949150171));
#46040=CARTESIAN_POINT('Ctrl Pts',(-5.83906243363843,3.42523552887297,-8.86604529758829));
#46041=CARTESIAN_POINT('Ctrl Pts',(-5.931041917685,3.26337713156858,-8.85729568015948));
#46042=CARTESIAN_POINT('Ctrl Pts',(-6.01619906699726,3.0980054529102,-8.84854606273067));
#46043=CARTESIAN_POINT('Ctrl Pts',(-6.1013533809545,2.93263928039456,-8.83979673662528));
#46044=CARTESIAN_POINT('Ctrl Pts',(-6.17968568352903,2.76376031540081,-8.83104741051989));
#46045=CARTESIAN_POINT('Ctrl Pts',(-6.25092992694947,2.59194213831396,-8.8222980844145));
#46046=CARTESIAN_POINT('Ctrl Pts',(-6.32217217691157,2.42012876880679,-8.81354900312071));
#46047=CARTESIAN_POINT('Ctrl Pts',(-6.38632665483898,2.24537661647535,-8.80479992182692));
#46048=CARTESIAN_POINT('Ctrl Pts',(-6.44317547869392,2.06827917621327,-8.79605084053313));
#46049=CARTESIAN_POINT('Ctrl Pts',(-6.50002944235971,1.89116572423301,-8.78730096821817));
#46050=CARTESIAN_POINT('Ctrl Pts',(-6.54957634250428,1.71170683289083,-8.77855109590321));
#46051=CARTESIAN_POINT('Ctrl Pts',(-6.5916478770842,1.53051209225258,-8.76980122358825));
#46052=CARTESIAN_POINT('Ctrl Pts',(-6.63371649075031,1.3493299314792,-8.76105195875345));
#46053=CARTESIAN_POINT('Ctrl Pts',(-6.66831071257144,1.1664124417389,-8.75230269391866));
#46054=CARTESIAN_POINT('Ctrl Pts',(-6.6953130484035,0.982380875158835,-8.74355342908387));
#46055=CARTESIAN_POINT('Ctrl Pts',(-6.72231677033057,0.798339861794692,
-8.73480371512821));
#46056=CARTESIAN_POINT('Ctrl Pts',(-6.741727784779,0.613184940729031,-8.72605400117256));
#46057=CARTESIAN_POINT('Ctrl Pts',(-6.75348015835525,0.42754502768946,-8.7173042872169));
#46058=CARTESIAN_POINT('Ctrl Pts',(-6.76249038365221,0.285219953546511,
-8.71059611941464));
#46059=CARTESIAN_POINT('Ctrl Pts',(-6.76699999999998,0.142609995757779,
-8.70388795161236));
#46060=CARTESIAN_POINT('Ctrl Pts',(-6.767,1.17640916536316E-12,-8.69717978381009));
#46061=CARTESIAN_POINT('Ctrl Pts',(-6.76699937553265,-0.00290715337751525,
-8.69717978381009));
#46062=CARTESIAN_POINT('Ctrl Pts',(-6.76691524467507,-0.198739084742533,
-8.68799239733351));
#46063=CARTESIAN_POINT('Ctrl Pts',(-6.75832612228008,-0.394331070678668,
-8.67880501085691));
#46064=CARTESIAN_POINT('Ctrl Pts',(-6.74131915260648,-0.588986487706674,
-8.66961762438032));
#46065=CARTESIAN_POINT('Ctrl Pts',(-6.72423368363483,-0.784540378354171,
-8.66038783156073));
#46066=CARTESIAN_POINT('Ctrl Pts',(-6.69865254006024,-0.979148843300637,
-8.65115803874112));
#46067=CARTESIAN_POINT('Ctrl Pts',(-6.66471496962178,-1.17211918067205,
-8.64192824592153));
#46068=CARTESIAN_POINT('Ctrl Pts',(-6.63070812902098,-1.36548339086417,
-8.63267961412088));
#46069=CARTESIAN_POINT('Ctrl Pts',(-6.58831079808566,-1.55720259933329,
-8.62343098232023));
#46070=CARTESIAN_POINT('Ctrl Pts',(-6.53771293764988,-1.74659627415308,
-8.61418235051957));
#46071=CARTESIAN_POINT('Ctrl Pts',(-6.48698320754632,-1.93648355247235,
-8.60490961465616));
#46072=CARTESIAN_POINT('Ctrl Pts',(-6.42801022788074,-2.12403298150376,
-8.59563687879274));
#46073=CARTESIAN_POINT('Ctrl Pts',(-6.361034284994,-2.30857787937312,-8.58636414292933));
#46074=CARTESIAN_POINT('Ctrl Pts',(-6.29883161931191,-2.47997053307438,
-8.57775226134902));
#46075=CARTESIAN_POINT('Ctrl Pts',(-6.22972660763097,-2.64877173829918,
-8.5691403797687));
#46076=CARTESIAN_POINT('Ctrl Pts',(-6.15394835814301,-2.81446417730071,
-8.56052849818839));
#46077=CARTESIAN_POINT('Ctrl Pts',(-6.0814355694657,-2.97301654418608,-8.55228772259161));
#46078=CARTESIAN_POINT('Ctrl Pts',(-6.00269125937446,-3.12898366169191,
-8.54404694699483));
#46079=CARTESIAN_POINT('Ctrl Pts',(-5.91792123483746,-3.28184357614129,
-8.53580617139805));
#46080=CARTESIAN_POINT('Ctrl Pts',(-5.83324510229286,-3.43453418166333,
-8.52757452335366));
#46081=CARTESIAN_POINT('Ctrl Pts',(-5.74255671575046,-3.58412412850215,
-8.51934287530926));
#46082=CARTESIAN_POINT('Ctrl Pts',(-5.64610975256684,-3.73011174926028,
-8.51111122726487));
#46083=CARTESIAN_POINT('Ctrl Pts',(-5.5497524271015,-3.87596368925887,-8.50288722970655));
#46084=CARTESIAN_POINT('Ctrl Pts',(-5.44764737866993,-4.01821967571203,
-8.49466323214823));
#46085=CARTESIAN_POINT('Ctrl Pts',(-5.34009401449279,-4.15640288186531,
-8.48643923458991));
#46086=CARTESIAN_POINT('Ctrl Pts',(-5.23263567413076,-4.2944640026191,-8.47822250296538));
#46087=CARTESIAN_POINT('Ctrl Pts',(-5.11973882974768,-4.42845923520702,
-8.47000577134084));
#46088=CARTESIAN_POINT('Ctrl Pts',(-5.00174589745669,-4.55794108971092,
-8.46178903971632));
#46089=CARTESIAN_POINT('Ctrl Pts',(-4.88381341731307,-4.68735660586728,
-8.45357651782759));
#46090=CARTESIAN_POINT('Ctrl Pts',(-4.76079028822517,-4.8122630869417,-8.44536399593886));
#46091=CARTESIAN_POINT('Ctrl Pts',(-4.63305912612318,-4.93224615503391,
-8.43715147405013));
#46092=CARTESIAN_POINT('Ctrl Pts',(-4.50537067793673,-5.05218910021051,
-8.42894169846826));
#46093=CARTESIAN_POINT('Ctrl Pts',(-4.37297759214175,-5.16721166893132,
-8.42073192288636));
#46094=CARTESIAN_POINT('Ctrl Pts',(-4.23629931833264,-5.27693633517541,
-8.41252214730448));
#46095=CARTESIAN_POINT('Ctrl Pts',(-4.17660179926291,-5.32486121872108,
-8.408936330622));
#46096=CARTESIAN_POINT('Ctrl Pts',(-4.11608724489742,-5.3717759049282,-8.40535051393954));
#46097=CARTESIAN_POINT('Ctrl Pts',(-4.05479264215265,-5.41765130191532,
-8.40176469725706));
#46098=CARTESIAN_POINT('Ctrl Pts',(-3.90336505412913,-5.53098592526393,
-8.39290597973533));
#46099=CARTESIAN_POINT('Ctrl Pts',(-3.74733151455158,-5.63785733818777,
-8.38404726221361));
#46100=CARTESIAN_POINT('Ctrl Pts',(-3.5872551176743,-5.7379342729522,-8.37518854469188));
#46101=CARTESIAN_POINT('Ctrl Pts',(-3.42687924356829,-5.83819843558826,
-8.36631325393246));
#46102=CARTESIAN_POINT('Ctrl Pts',(-3.26244561685854,-5.93164257976171,
-8.35743796317304));
#46103=CARTESIAN_POINT('Ctrl Pts',(-3.09454176563316,-6.01798141080147,
-8.34856267241363));
#46104=CARTESIAN_POINT('Ctrl Pts',(-2.92616102971802,-6.1045654635342,-8.33966217383289));
#46105=CARTESIAN_POINT('Ctrl Pts',(-2.75429057786916,-6.18400369976604,
-8.33076167525215));
#46106=CARTESIAN_POINT('Ctrl Pts',(-2.57954060775898,-6.25605780447419,
-8.32186117667141));
#46107=CARTESIAN_POINT('Ctrl Pts',(-2.40455407838045,-6.3282094489203,-8.31294862947384));
#46108=CARTESIAN_POINT('Ctrl Pts',(-2.22668048646314,-6.39295690163863,
-8.30403608227627));
#46109=CARTESIAN_POINT('Ctrl Pts',(-2.04654637140133,-6.45011139048808,
-8.29512353507869));
#46110=CARTESIAN_POINT('Ctrl Pts',(-1.86601450262073,-6.50739208203088,
-8.28619130810647));
#46111=CARTESIAN_POINT('Ctrl Pts',(-1.68321237516878,-6.55704619616572,
-8.27725908113423));
#46112=CARTESIAN_POINT('Ctrl Pts',(-1.49878072729321,-6.59893516648667,
-8.268326854162));
#46113=CARTESIAN_POINT('Ctrl Pts',(-1.32447152264319,-6.63852508060585,
-8.25988486821644));
#46114=CARTESIAN_POINT('Ctrl Pts',(-1.14870702377738,-6.6711792370778,-8.25144288227087));
#46115=CARTESIAN_POINT('Ctrl Pts',(-0.972033230990177,-6.69682315712837,
-8.24300089632531));
#46116=CARTESIAN_POINT('Ctrl Pts',(-0.799921981160285,-6.72180483132471,
-8.23477692190774));
#46117=CARTESIAN_POINT('Ctrl Pts',(-0.626618872555658,-6.740180362213,-8.22655294749019));
#46118=CARTESIAN_POINT('Ctrl Pts',(-0.452671980481697,-6.75184249505917,
-8.21832897307262));
#46119=CARTESIAN_POINT('Ctrl Pts',(-0.278908793202929,-6.76349231156153,
-8.21011368396996));
#46120=CARTESIAN_POINT('Ctrl Pts',(-0.104503531191567,-6.76844282480463,
-8.20189839486732));
#46121=CARTESIAN_POINT('Ctrl Pts',(0.0699871664054911,-6.7666380719334,
-8.19368310576466));
#46122=CARTESIAN_POINT('Ctrl Pts',(0.244328584011008,-6.76483486306134,
-8.18547484499248));
#46123=CARTESIAN_POINT('Ctrl Pts',(0.41875493508005,-6.7562879017321,-8.1772665842203));
#46124=CARTESIAN_POINT('Ctrl Pts',(0.592706012016421,-6.74099314517673,
-8.16905832344812));
#46125=CARTESIAN_POINT('Ctrl Pts',(0.766543151559387,-6.72570840663748,
-8.16085543906023));
#46126=CARTESIAN_POINT('Ctrl Pts',(0.939905281112293,-6.70368470791542,
-8.15265255467232));
#46127=CARTESIAN_POINT('Ctrl Pts',(1.11223365818358,-6.67497005907918,-8.14444967028443));
#46128=CARTESIAN_POINT('Ctrl Pts',(1.28448370921923,-6.64626846151545,-8.13625051424022));
#46129=CARTESIAN_POINT('Ctrl Pts',(1.45570059086233,-6.61088203140942,-8.12805135819602));
#46130=CARTESIAN_POINT('Ctrl Pts',(1.62533204812493,-6.56891046775171,-8.11985220215181));
#46131=CARTESIAN_POINT('Ctrl Pts',(1.79494875157561,-6.52694255459943,-8.1116537592348));
#46132=CARTESIAN_POINT('Ctrl Pts',(1.96297995542665,-6.47839072650358,-8.10345531631777));
#46133=CARTESIAN_POINT('Ctrl Pts',(2.12888458427527,-6.42340559414047,-8.09525687340076));
#46134=CARTESIAN_POINT('Ctrl Pts',(2.29478756091017,-6.3684210093642,-8.08705851213053));
#46135=CARTESIAN_POINT('Ctrl Pts',(2.45856366390742,-6.3070033597739,-8.0788601508603));
#46136=CARTESIAN_POINT('Ctrl Pts',(2.61968806415335,-6.23935280670459,-8.07066178959007));
#46137=CARTESIAN_POINT('Ctrl Pts',(2.78084012919206,-6.17169063814732,-8.06246202067478));
#46138=CARTESIAN_POINT('Ctrl Pts',(2.93933925366482,-6.09779357286524,-8.05426225175951));
#46139=CARTESIAN_POINT('Ctrl Pts',(3.09468159068023,-6.01790950848423,-8.04606248284423));
#46140=CARTESIAN_POINT('Ctrl Pts',(3.25007881905982,-5.937997216478,-8.03785981647993));
#46141=CARTESIAN_POINT('Ctrl Pts',(3.40231671914451,-5.85209387509924,-8.02965715011561));
#46142=CARTESIAN_POINT('Ctrl Pts',(3.55091695724035,-5.76049284026835,-8.02145448375131));
#46143=CARTESIAN_POINT('Ctrl Pts',(3.69968596806375,-5.66878776955776,-8.01324250120829));
#46144=CARTESIAN_POINT('Ctrl Pts',(3.84480875736337,-5.57137226570385,-8.00503051866528));
#46145=CARTESIAN_POINT('Ctrl Pts',(3.98583598629654,-5.46858304228284,-7.99681853612226));
#46146=CARTESIAN_POINT('Ctrl Pts',(4.12694639499528,-5.3657331923887,-7.98860171004095));
#46147=CARTESIAN_POINT('Ctrl Pts',(4.26395614714185,-5.25750352697139,-7.98038488395965));
#46148=CARTESIAN_POINT('Ctrl Pts',(4.39644992288586,-5.14427031517172,-7.97216805787834));
#46149=CARTESIAN_POINT('Ctrl Pts',(4.52914802316771,-5.03086248140555,-7.96393856026449));
#46150=CARTESIAN_POINT('Ctrl Pts',(4.65731596662949,-4.91243592477088,-7.95570906265064));
#46151=CARTESIAN_POINT('Ctrl Pts',(4.78057522294897,-4.78940388124936,-7.94747956503679));
#46152=CARTESIAN_POINT('Ctrl Pts',(4.89044327211488,-4.6797383598903,-7.94014414151203));
#46153=CARTESIAN_POINT('Ctrl Pts',(4.99641171666389,-4.56641432011216,-7.93280871798728));
#46154=CARTESIAN_POINT('Ctrl Pts',(5.09824052691913,-4.44974522076032,-7.92547329446253));
#46155=CARTESIAN_POINT('Ctrl Pts',(5.21027865342028,-4.32137892364666,-7.91740242427613));
#46156=CARTESIAN_POINT('Ctrl Pts',(5.31767002221868,-4.18854398075456,-7.90933155408973));
#46157=CARTESIAN_POINT('Ctrl Pts',(5.42002710494732,-4.05161636654266,-7.90126068390332));
#46158=CARTESIAN_POINT('Ctrl Pts',(5.52225681224249,-3.91485914810358,-7.89319985728754));
#46159=CARTESIAN_POINT('Ctrl Pts',(5.61946447830822,-3.77401968717285,-7.88513903067177));
#46160=CARTESIAN_POINT('Ctrl Pts',(5.71129960605998,-3.62951040910742,-7.87707820405598));
#46161=CARTESIAN_POINT('Ctrl Pts',(5.80304059017546,-3.48514927292676,-7.86902564089611));
#46162=CARTESIAN_POINT('Ctrl Pts',(5.88941979791398,-3.33712611843255,-7.86097307773622));
#46163=CARTESIAN_POINT('Ctrl Pts',(5.97012727855626,-3.18588594865517,-7.85292051457634));
#46164=CARTESIAN_POINT('Ctrl Pts',(6.05076969487639,-3.03476770486344,-7.84487444318847));
#46165=CARTESIAN_POINT('Ctrl Pts',(6.12574931006339,-2.88043793512903,-7.8368283718006));
#46166=CARTESIAN_POINT('Ctrl Pts',(6.19479982072789,-2.72337000444481,-7.82878230041273));
#46167=CARTESIAN_POINT('Ctrl Pts',(6.26380976863658,-2.56639434111758,-7.82074095557686));
#46168=CARTESIAN_POINT('Ctrl Pts',(6.32689739591313,-2.40668405950758,-7.81269961074098));
#46169=CARTESIAN_POINT('Ctrl Pts',(6.3838426996995,-2.24473637327269,-7.8046582659051));
#46170=CARTESIAN_POINT('Ctrl Pts',(6.44188573372201,-2.07966683396069,-7.79646190868403));
#46171=CARTESIAN_POINT('Ctrl Pts',(6.49354703322238,-1.91227309976545,-7.78826555146296));
#46172=CARTESIAN_POINT('Ctrl Pts',(6.53864527488889,-1.74310268463255,-7.78006919424189));
#46173=CARTESIAN_POINT('Ctrl Pts',(6.58287653837624,-1.57718443750134,-7.7720304055334));
#46174=CARTESIAN_POINT('Ctrl Pts',(6.62079471588866,-1.40955757975313,-7.76399161682492));
#46175=CARTESIAN_POINT('Ctrl Pts',(6.65227936732864,-1.24075308543387,-7.75595282811643));
#46176=CARTESIAN_POINT('Ctrl Pts',(6.6837673879116,-1.07193052750424,-7.74791317918471));
#46177=CARTESIAN_POINT('Ctrl Pts',(6.70882044304195,-0.901930449229639,
-7.73987353025298));
#46178=CARTESIAN_POINT('Ctrl Pts',(6.72736945885729,-0.731292803215058,
-7.73183388132126));
#46179=CARTESIAN_POINT('Ctrl Pts',(6.74592413236132,-0.560603110521183,
-7.7237917801931));
#46180=CARTESIAN_POINT('Ctrl Pts',(6.75797077743414,-0.3892758340752,-7.71574967906493));
#46181=CARTESIAN_POINT('Ctrl Pts',(6.76349231859536,-0.217854667844397,
-7.70770757793677));
#46182=CARTESIAN_POINT('Ctrl Pts',(6.76920019007729,-0.0406487107467705,
-7.69939408749199));
#46183=CARTESIAN_POINT('Ctrl Pts',(6.76793484465814,0.13665714714267,-7.69108059704721));
#46184=CARTESIAN_POINT('Ctrl Pts',(6.75973584536604,0.313464991463971,-7.68276710660243));
#46185=CARTESIAN_POINT('Ctrl Pts',(6.75179052595205,0.484802339838399,-7.67471083843168));
#46186=CARTESIAN_POINT('Ctrl Pts',(6.73733432666607,0.655671672588204,-7.66665457026091));
#46187=CARTESIAN_POINT('Ctrl Pts',(6.71645572713968,0.825537076921797,-7.65859830209016));
#46188=CARTESIAN_POINT('Ctrl Pts',(6.69457720294565,1.00353773035373,-7.65015620050837));
#46189=CARTESIAN_POINT('Ctrl Pts',(6.66564606210925,1.18043544981528,-7.64171409892659));
#46190=CARTESIAN_POINT('Ctrl Pts',(6.62982331990504,1.35562964958847,-7.6332719973448));
#46191=CARTESIAN_POINT('Ctrl Pts',(6.59400057770082,1.53082384936166,-7.62482989576301));
#46192=CARTESIAN_POINT('Ctrl Pts',(6.55128642826821,1.70431410260632,-7.61638779418121));
#46193=CARTESIAN_POINT('Ctrl Pts',(6.50189998196866,1.87552276031936,-7.60794569259942));
#46194=CARTESIAN_POINT('Ctrl Pts',(6.45314010446022,2.04455928357593,-7.59961069646413));
#46195=CARTESIAN_POINT('Ctrl Pts',(6.39772177856541,2.21190939702059,-7.59127570032886));
#46196=CARTESIAN_POINT('Ctrl Pts',(6.33577716324021,2.37701845549501,-7.58294070419358));
#46197=CARTESIAN_POINT('Ctrl Pts',(6.27390699817602,2.54192907198325,-7.57461572575935));
#46198=CARTESIAN_POINT('Ctrl Pts',(6.20552629156955,2.70460367639919,-7.5662907473251));
#46199=CARTESIAN_POINT('Ctrl Pts',(6.13081743388125,2.86450110707218,-7.55796576889087));
#46200=CARTESIAN_POINT('Ctrl Pts',(6.05256284100748,3.0319873828105,-7.54924568109657));
#46201=CARTESIAN_POINT('Ctrl Pts',(5.96736484040027,3.19642607303085,-7.54052559330226));
#46202=CARTESIAN_POINT('Ctrl Pts',(5.87549126295921,3.35721483061332,-7.53180550550796));
#46203=CARTESIAN_POINT('Ctrl Pts',(5.78796009492851,3.51040389921607,-7.52349757311625));
#46204=CARTESIAN_POINT('Ctrl Pts',(5.69437002363127,3.66027974671692,-7.51518964072453));
#46205=CARTESIAN_POINT('Ctrl Pts',(5.59500117228749,3.80634350553147,-7.50688170833281));
#46206=CARTESIAN_POINT('Ctrl Pts',(5.495688731653,3.95232434540187,-7.49857849227175));
#46207=CARTESIAN_POINT('Ctrl Pts',(5.39060424171314,4.09449712128488,-7.49027527621069));
#46208=CARTESIAN_POINT('Ctrl Pts',(5.2800723035603,4.23239004218367,-7.48197206014962));
#46209=CARTESIAN_POINT('Ctrl Pts',(5.1695847597814,4.37022757936263,-7.47367217901676));
#46210=CARTESIAN_POINT('Ctrl Pts',(5.05365434478513,4.50378841599753,-7.4653722978839));
#46211=CARTESIAN_POINT('Ctrl Pts',(4.93264739987986,4.63263193319505,-7.45707241675104));
#46212=CARTESIAN_POINT('Ctrl Pts',(4.81166896840162,4.7614450903977,-7.44877449135762));
#46213=CARTESIAN_POINT('Ctrl Pts',(4.68561662948535,4.88554289072229,-7.44047656596422));
#46214=CARTESIAN_POINT('Ctrl Pts',(4.55489534294085,5.00451969871793,-7.4321786405708));
#46215=CARTESIAN_POINT('Ctrl Pts',(4.42415951349688,5.12350974302575,-7.42387979202327));
#46216=CARTESIAN_POINT('Ctrl Pts',(4.28875395277039,5.23737741924336,-7.41558094347571));
#46217=CARTESIAN_POINT('Ctrl Pts',(4.14911900494689,5.34575537064582,-7.40728209492817));
#46218=CARTESIAN_POINT('Ctrl Pts',(4.00947544449892,5.45414000675443,-7.39898273451117));
#46219=CARTESIAN_POINT('Ctrl Pts',(3.86560225478318,5.5570340338487,-7.39068337409417));
#46220=CARTESIAN_POINT('Ctrl Pts',(3.71797109773611,5.65411177077346,-7.38238401367717));
#46221=CARTESIAN_POINT('Ctrl Pts',(3.5702711685822,5.75123473013384,-7.37408078710811));
#46222=CARTESIAN_POINT('Ctrl Pts',(3.41881006875823,5.84253580051775,-7.36577756053905));
#46223=CARTESIAN_POINT('Ctrl Pts',(3.26408704510001,5.92773352656901,-7.35747433396999));
#46224=CARTESIAN_POINT('Ctrl Pts',(3.20948500324953,5.9577999620188,-7.35454410992254));
#46225=CARTESIAN_POINT('Ctrl Pts',(3.15447694539446,5.98710670692936,-7.35161388587509));
#46226=CARTESIAN_POINT('Ctrl Pts',(3.09908550384714,6.01564277861016,-7.34868366182764));
#46227=CARTESIAN_POINT('Origin',(0.,0.,-63.6971797838103));
#46228=CARTESIAN_POINT('',(3.09908550384723,6.01564277861011,-4.95428495819038));
#46229=CARTESIAN_POINT('',(3.09908550384725,6.0156427786101,-5.34860320957391));
#46230=CARTESIAN_POINT('',(3.09908550384721,6.01564277861012,-63.6971797838103));
#46231=CARTESIAN_POINT('',(-6.76699461023805,0.00854078504219338,-6.30282021615864));
#46232=CARTESIAN_POINT('Ctrl Pts',(-6.76699461023805,0.00854078504218888,
-6.30282021615862));
#46233=CARTESIAN_POINT('Ctrl Pts',(-6.76720711237283,-0.159827906309611,
-6.29489054746016));
#46234=CARTESIAN_POINT('Ctrl Pts',(-6.76113188488697,-0.328457192148686,
-6.28696087876169));
#46235=CARTESIAN_POINT('Ctrl Pts',(-6.74873761255546,-0.496819521435291,
-6.27903121006323));
#46236=CARTESIAN_POINT('Ctrl Pts',(-6.73635391184144,-0.665038247120448,
-6.27110830492636));
#46237=CARTESIAN_POINT('Ctrl Pts',(-6.71766191538891,-0.832990088934394,
-6.2631853997895));
#46238=CARTESIAN_POINT('Ctrl Pts',(-6.69268233672883,-1.00014605915232,
-6.25526249465262));
#46239=CARTESIAN_POINT('Ctrl Pts',(-6.66771834284764,-1.16719774062817,
-6.24734453262253));
#46240=CARTESIAN_POINT('Ctrl Pts',(-6.63647462801936,-1.33345416009714,
-6.23942657059243));
#46241=CARTESIAN_POINT('Ctrl Pts',(-6.59902383464015,-1.49839027955045,
-6.23150860856234));
#46242=CARTESIAN_POINT('Ctrl Pts',(-6.5615829075879,-1.66328294695544,-6.22359273250146));
#46243=CARTESIAN_POINT('Ctrl Pts',(-6.51793823272174,-1.82685563078568,
-6.21567685644061));
#46244=CARTESIAN_POINT('Ctrl Pts',(-6.4682137653419,-1.98859238805783,-6.20776098037973));
#46245=CARTESIAN_POINT('Ctrl Pts',(-6.41849483366338,-2.15031113957894,
-6.19984598557366));
#46246=CARTESIAN_POINT('Ctrl Pts',(-6.3626975674472,-2.31019400355646,-6.19193099076755));
#46247=CARTESIAN_POINT('Ctrl Pts',(-6.30099600942057,-2.46773951001033,
-6.18401599596148));
#46248=CARTESIAN_POINT('Ctrl Pts',(-6.23928856251318,-2.62530005282199,
-6.17610024573752));
#46249=CARTESIAN_POINT('Ctrl Pts',(-6.17167584289126,-2.78052243652897,
-6.16818449551357));
#46250=CARTESIAN_POINT('Ctrl Pts',(-6.09838020600375,-2.93292479668704,
-6.16026874528961));
#46251=CARTESIAN_POINT('Ctrl Pts',(-6.02506240823449,-3.08537323558628,
-6.1523506017444));
#46252=CARTESIAN_POINT('Ctrl Pts',(-5.94605844226286,-3.23499960916278,
-6.1444324581992));
#46253=CARTESIAN_POINT('Ctrl Pts',(-5.86163666280367,-3.38134657100922,
-6.13651431465399));
#46254=CARTESIAN_POINT('Ctrl Pts',(-5.77712022036392,-3.52785763315885,
-6.12858729241572));
#46255=CARTESIAN_POINT('Ctrl Pts',(-5.68717402701725,-3.67108160870135,
-6.12066027017744));
#46256=CARTESIAN_POINT('Ctrl Pts',(-5.5921101966152,-3.81058952773876,-6.11273324793917));
#46257=CARTESIAN_POINT('Ctrl Pts',(-5.49699055219573,-3.95017935487298,
-6.10480157157581));
#46258=CARTESIAN_POINT('Ctrl Pts',(-5.3967475187954,-4.08604847600277,-6.09686989521247));
#46259=CARTESIAN_POINT('Ctrl Pts',(-5.29173303922776,-4.21780161239778,
-6.08893821884911));
#46260=CARTESIAN_POINT('Ctrl Pts',(-5.18655314231556,-4.34976228449692,
-6.08099404861969));
#46261=CARTESIAN_POINT('Ctrl Pts',(-5.07658704153737,-4.47759373644785,
-6.07304987839026));
#46262=CARTESIAN_POINT('Ctrl Pts',(-4.9622236475352,-4.60093745576295,-6.06510570816084));
#46263=CARTESIAN_POINT('Ctrl Pts',(-4.86930048330324,-4.70115736255132,
-6.05865086794422));
#46264=CARTESIAN_POINT('Ctrl Pts',(-4.77347497316505,-4.79841515873253,
-6.0521960277276));
#46265=CARTESIAN_POINT('Ctrl Pts',(-4.67497079558671,-4.89253891761847,
-6.04574118751098));
#46266=CARTESIAN_POINT('Ctrl Pts',(-4.54779207501027,-5.01406208064819,
-6.03740734482067));
#46267=CARTESIAN_POINT('Ctrl Pts',(-4.41570929584349,-5.13077868610561,
-6.02907350213037));
#46268=CARTESIAN_POINT('Ctrl Pts',(-4.27911559842972,-5.24227609872615,
-6.02073965944007));
#46269=CARTESIAN_POINT('Ctrl Pts',(-4.14268289396909,-5.35364209754015,
-6.01241563923771));
#46270=CARTESIAN_POINT('Ctrl Pts',(-4.00175012975998,-5.45980093973423,
-6.00409161903534));
#46271=CARTESIAN_POINT('Ctrl Pts',(-3.85674708017347,-5.56037687208101,
-5.99576759883298));
#46272=CARTESIAN_POINT('Ctrl Pts',(-3.71188834892672,-5.66085270341876,
-5.98745186334448));
#46273=CARTESIAN_POINT('Ctrl Pts',(-3.56296768742227,-5.75575649838763,
-5.97913612785599));
#46274=CARTESIAN_POINT('Ctrl Pts',(-3.4104478977206,-5.84475270109294,-5.9708203923675));
#46275=CARTESIAN_POINT('Ctrl Pts',(-3.25805196204173,-5.93367663424069,
-5.96251140968987));
#46276=CARTESIAN_POINT('Ctrl Pts',(-3.10206302102442,-6.01670235959786,
-5.95420242701225));
#46277=CARTESIAN_POINT('Ctrl Pts',(-2.94297299712593,-6.09353747327344,
-5.94589344433462));
#46278=CARTESIAN_POINT('Ctrl Pts',(-2.78398302922535,-6.17032426327803,
-5.93758968739983));
#46279=CARTESIAN_POINT('Ctrl Pts',(-2.62189617763117,-6.24092804996952,
-5.92928593046504));
#46280=CARTESIAN_POINT('Ctrl Pts',(-2.45722931315714,-6.30510214846368,
-5.92098217353026));
#46281=CARTESIAN_POINT('Ctrl Pts',(-2.29262929946001,-6.36925019382108,
-5.91268178772058));
#46282=CARTESIAN_POINT('Ctrl Pts',(-2.12545168351879,-6.42697362610326,
-5.90438140191092));
#46283=CARTESIAN_POINT('Ctrl Pts',(-1.95623395102337,-6.47807361249187,
-5.89608101610124));
#46284=CARTESIAN_POINT('Ctrl Pts',(-1.78705190214475,-6.52916282322296,
-5.88778238062696));
#46285=CARTESIAN_POINT('Ctrl Pts',(-1.61583092653991,-6.5736312701686,-5.87948374515266));
#46286=CARTESIAN_POINT('Ctrl Pts',(-1.44312456535219,-6.6113297065626,-5.87118510967838));
#46287=CARTESIAN_POINT('Ctrl Pts',(-1.27042595616791,-6.64902645084516,
-5.86288684669212));
#46288=CARTESIAN_POINT('Ctrl Pts',(-1.09624243406426,-6.67995371612954,
-5.85458858370586));
#46289=CARTESIAN_POINT('Ctrl Pts',(-0.921138842400919,-6.70401314385796,
-5.8462903207196));
#46290=CARTESIAN_POINT('Ctrl Pts',(-0.746014046440189,-6.72807548508036,
-5.83799105284912));
#46291=CARTESIAN_POINT('Ctrl Pts',(-0.56996930351817,-6.7452682848114,-5.82969178497865));
#46292=CARTESIAN_POINT('Ctrl Pts',(-0.393575902158023,-6.75554490838752,
-5.82139251710817));
#46293=CARTESIAN_POINT('Ctrl Pts',(-0.217058644198134,-6.76582874780982,
-5.81308742181393));
#46294=CARTESIAN_POINT('Ctrl Pts',(-0.0401925862366737,-6.76918668714386,
-5.80478232651967));
#46295=CARTESIAN_POINT('Ctrl Pts',(0.136448739733167,-6.76562419451637,
-5.79647723122542));
#46296=CARTESIAN_POINT('Ctrl Pts',(0.313154478316598,-6.76206040281879,
-5.78816910746153));
#46297=CARTESIAN_POINT('Ctrl Pts',(0.489634974060889,-6.75157116378814,
-5.77986098369766));
#46298=CARTESIAN_POINT('Ctrl Pts',(0.665320248879113,-6.73421398282171,
-5.77155285993377));
#46299=CARTESIAN_POINT('Ctrl Pts',(0.841192276130339,-6.71683835127211,
-5.76323590468228));
#46300=CARTESIAN_POINT('Ctrl Pts',(1.01626704799254,-6.69258023296174,-5.7549189494308));
#46301=CARTESIAN_POINT('Ctrl Pts',(1.18998214059048,-6.66154873171965,-5.7466019941793));
#46302=CARTESIAN_POINT('Ctrl Pts',(1.31800752143857,-6.63867898732732,-5.74047252466894));
#46303=CARTESIAN_POINT('Ctrl Pts',(1.44529456930429,-6.61213137919877,-5.73434305515856));
#46304=CARTESIAN_POINT('Ctrl Pts',(1.57162303078922,-6.58196703494426,-5.72821358564819));
#46305=CARTESIAN_POINT('Ctrl Pts',(1.74579875685357,-6.54037785939326,-5.71976256210363));
#46306=CARTESIAN_POINT('Ctrl Pts',(1.91847000250474,-6.49183558419278,-5.71131153855909));
#46307=CARTESIAN_POINT('Ctrl Pts',(2.08906228116901,-6.43646702666897,-5.70286051501453));
#46308=CARTESIAN_POINT('Ctrl Pts',(2.25950435839969,-6.38114721951524,-5.69441693234514));
#46309=CARTESIAN_POINT('Ctrl Pts',(2.4278708032841,-6.31901321164062,-5.68597334967575));
#46310=CARTESIAN_POINT('Ctrl Pts',(2.59359998182422,-6.25024224604786,-5.67752976700637));
#46311=CARTESIAN_POINT('Ctrl Pts',(2.75920576982523,-6.18152248258253,-5.66909247084747));
#46312=CARTESIAN_POINT('Ctrl Pts',(2.92217790050786,-6.10617573852384,-5.66065517468856));
#46313=CARTESIAN_POINT('Ctrl Pts',(3.08197212640254,-6.02442833902752,-5.65221787852966));
#46314=CARTESIAN_POINT('Ctrl Pts',(3.2416523512941,-5.9427392600712,-5.64378660173861));
#46315=CARTESIAN_POINT('Ctrl Pts',(3.39815889929805,-5.85465878469378,-5.63535532494755));
#46316=CARTESIAN_POINT('Ctrl Pts',(3.5509694629037,-5.76046047408759,-5.6269240481565));
#46317=CARTESIAN_POINT('Ctrl Pts',(3.70371452636554,-5.66630254029009,-5.61849638531613));
#46318=CARTESIAN_POINT('Ctrl Pts',(3.85276648200666,-5.56603217261552,-5.61006872247578));
#46319=CARTESIAN_POINT('Ctrl Pts',(3.99762893149013,-5.45996812500889,-5.60164105963542));
#46320=CARTESIAN_POINT('Ctrl Pts',(4.14244678657624,-5.35393672811541,-5.59321599116335));
#46321=CARTESIAN_POINT('Ctrl Pts',(4.28307744033944,-5.24211540368635,-5.58479092269128));
#46322=CARTESIAN_POINT('Ctrl Pts',(4.419054422616,-5.1248655601838,-5.57636585421921));
#46323=CARTESIAN_POINT('Ctrl Pts',(4.45626188521486,-5.09278241571475,-5.57406049771829));
#46324=CARTESIAN_POINT('Ctrl Pts',(4.49312109345409,-5.06029305666917,-5.57175514121737));
#46325=CARTESIAN_POINT('Ctrl Pts',(4.5296229160184,-5.02740541817358,-5.56944978471645));
#46326=CARTESIAN_POINT('Ctrl Pts',(4.66609152203814,-4.9044490870789,-5.56083079623976));
#46327=CARTESIAN_POINT('Ctrl Pts',(4.79750107732584,-4.77597765589931,-5.55221180776308));
#46328=CARTESIAN_POINT('Ctrl Pts',(4.92342292830874,-4.64243423959928,-5.5435928192864));
#46329=CARTESIAN_POINT('Ctrl Pts',(5.04942021771019,-4.50881081888339,-5.53496866726698));
#46330=CARTESIAN_POINT('Ctrl Pts',(5.16992303305106,-4.37010957027606,-5.52634451524756));
#46331=CARTESIAN_POINT('Ctrl Pts',(5.28454190082363,-4.22680800349855,-5.51772036322813));
#46332=CARTESIAN_POINT('Ctrl Pts',(5.40308649663685,-4.07859831827684,-5.50880083160788));
#46333=CARTESIAN_POINT('Ctrl Pts',(5.5153367379354,-3.9254678958385,-5.49988129998763));
#46334=CARTESIAN_POINT('Ctrl Pts',(5.62090973344387,-3.76797860509796,-5.49096176836738));
#46335=CARTESIAN_POINT('Ctrl Pts',(5.72317672625415,-3.61542106814178,-5.48232155055708));
#46336=CARTESIAN_POINT('Ctrl Pts',(5.81917821852534,-3.45877381000802,-5.47368133274678));
#46337=CARTESIAN_POINT('Ctrl Pts',(5.90861221698887,-3.29857403573876,-5.46504111493648));
#46338=CARTESIAN_POINT('Ctrl Pts',(6.00238293787045,-3.13060605290927,-5.45598192641126));
#46339=CARTESIAN_POINT('Ctrl Pts',(6.0889332302011,-2.95873280659627,-5.44692273788604));
#46340=CARTESIAN_POINT('Ctrl Pts',(6.16797083144579,-2.78359925679577,-5.43786354936081));
#46341=CARTESIAN_POINT('Ctrl Pts',(6.2470084326905,-2.60846570699522,-5.42880436083559));
#46342=CARTESIAN_POINT('Ctrl Pts',(6.31853323120567,-2.43007222117997,-5.41974517231035));
#46343=CARTESIAN_POINT('Ctrl Pts',(6.38231202064313,-2.24908476299898,-5.41068598378512));
#46344=CARTESIAN_POINT('Ctrl Pts',(6.44598031801662,-2.06841085228392,-5.40164248963802));
#46345=CARTESIAN_POINT('Ctrl Pts',(6.50198887538156,-1.88498578516538,-5.39259899549091));
#46346=CARTESIAN_POINT('Ctrl Pts',(6.55012725636153,-1.69944753536844,-5.38355550134381));
#46347=CARTESIAN_POINT('Ctrl Pts',(6.59822160533842,-1.51407899673791,-5.37452027924812));
#46348=CARTESIAN_POINT('Ctrl Pts',(6.63846009066339,-1.32660136477124,-5.36548505715244));
#46349=CARTESIAN_POINT('Ctrl Pts',(6.6706823728222,-1.13766677059639,-5.35644983505675));
#46350=CARTESIAN_POINT('Ctrl Pts',(6.70284788632655,-0.949065038092803,
-5.34743053105769));
#46351=CARTESIAN_POINT('Ctrl Pts',(6.72702535817801,-0.759011703455649,
-5.33841122705862));
#46352=CARTESIAN_POINT('Ctrl Pts',(6.74310568222232,-0.56816789629568,-5.32939192305955));
#46353=CARTESIAN_POINT('Ctrl Pts',(6.75916583237354,-0.377563516062186,
-5.32038393440925));
#46354=CARTESIAN_POINT('Ctrl Pts',(6.7671490875398,-0.186170878945884,-5.31137594575893));
#46355=CARTESIAN_POINT('Ctrl Pts',(6.7669978911239,0.00534242685262255,
-5.30236795710862));
#46356=CARTESIAN_POINT('Ctrl Pts',(6.76684703619048,0.196423193049244,-5.29338031332056));
#46357=CARTESIAN_POINT('Ctrl Pts',(6.75859840195246,0.38762384627601,-5.2843926695325));
#46358=CARTESIAN_POINT('Ctrl Pts',(6.74224635805464,0.578275926612022,-5.27540502574443));
#46359=CARTESIAN_POINT('Ctrl Pts',(6.72800486210553,0.744320663695759,-5.26757741144743));
#46360=CARTESIAN_POINT('Ctrl Pts',(6.70761753852657,0.909949118378983,-5.25974979715043));
#46361=CARTESIAN_POINT('Ctrl Pts',(6.68111286994208,1.07471848364786,-5.25192218285343));
#46362=CARTESIAN_POINT('Ctrl Pts',(6.65360747519168,1.24570897990876,-5.24379902445563));
#46363=CARTESIAN_POINT('Ctrl Pts',(6.61952471774068,1.41569758942989,-5.23567586605784));
#46364=CARTESIAN_POINT('Ctrl Pts',(6.57896549905707,1.5841407646471,-5.22755270766005));
#46365=CARTESIAN_POINT('Ctrl Pts',(6.53840914001137,1.7525720637359,-5.21943012198757));
#46366=CARTESIAN_POINT('Ctrl Pts',(6.49137731497009,1.91945778970711,-5.21130753631509));
#46367=CARTESIAN_POINT('Ctrl Pts',(6.43802168382705,2.08426624944434,-5.20318495064262));
#46368=CARTESIAN_POINT('Ctrl Pts',(6.38465964145645,2.24909451261215,-5.19506138895799));
#46369=CARTESIAN_POINT('Ctrl Pts',(6.3249723937789,2.41184466467059,-5.18693782727336));
#46370=CARTESIAN_POINT('Ctrl Pts',(6.25916093024621,2.57200183695103,-5.17881426558873));
#46371=CARTESIAN_POINT('Ctrl Pts',(6.19330153087195,2.73227566472615,-5.1706847868534));
#46372=CARTESIAN_POINT('Ctrl Pts',(6.12130914558339,2.88995240163682,-5.16255530811808));
#46373=CARTESIAN_POINT('Ctrl Pts',(6.04343248649321,3.04453818849402,-5.15442582938275));
#46374=CARTESIAN_POINT('Ctrl Pts',(5.96552407846039,3.19918699725454,-5.14629303640209));
#46375=CARTESIAN_POINT('Ctrl Pts',(5.88172679186075,3.35074202406299,-5.1381602434214));
#46376=CARTESIAN_POINT('Ctrl Pts',(5.79233432410532,3.49873578279233,-5.13002745044074));
#46377=CARTESIAN_POINT('Ctrl Pts',(5.70284465560015,3.64689046228675,-5.12188581428129));
#46378=CARTESIAN_POINT('Ctrl Pts',(5.60774785532039,3.79147583397952,-5.11374417812184));
#46379=CARTESIAN_POINT('Ctrl Pts',(5.50738021654732,3.93205444397495,-5.10560254196239));
#46380=CARTESIAN_POINT('Ctrl Pts',(5.45624426404744,4.00367734166491,-5.10145448861561));
#46381=CARTESIAN_POINT('Ctrl Pts',(5.40374077199387,4.07426071113786,-5.09730643526883));
#46382=CARTESIAN_POINT('Ctrl Pts',(5.34991806237872,4.14375020070394,-5.09315838192204));
#46383=CARTESIAN_POINT('Ctrl Pts',(5.24039083725283,4.28515874408661,-5.0847172466467));
#46384=CARTESIAN_POINT('Ctrl Pts',(5.12517271087284,4.42232659902459,-5.07627611137136));
#46385=CARTESIAN_POINT('Ctrl Pts',(5.00461878989457,4.55478646786369,-5.06783497609601));
#46386=CARTESIAN_POINT('Ctrl Pts',(4.88415430102167,4.68714807225107,-5.05940010281939));
#46387=CARTESIAN_POINT('Ctrl Pts',(4.75836213143086,4.81480840661897,-5.05096522954278));
#46388=CARTESIAN_POINT('Ctrl Pts',(4.62763773171091,4.93733308822136,-5.04253035626616));
#46389=CARTESIAN_POINT('Ctrl Pts',(4.49700434453506,5.05977246606248,-5.03410135549136));
#46390=CARTESIAN_POINT('Ctrl Pts',(4.36144581882315,5.17708309505497,-5.02567235471656));
#46391=CARTESIAN_POINT('Ctrl Pts',(4.22139467466584,5.28886717555876,-5.01724335394176));
#46392=CARTESIAN_POINT('Ctrl Pts',(4.08140243801101,5.40060423808895,-5.00881789852453));
#46393=CARTESIAN_POINT('Ctrl Pts',(3.93692161000627,5.50681917839115,-5.00039244310729));
#46394=CARTESIAN_POINT('Ctrl Pts',(3.78841848304066,5.60715385889811,-4.99196698769006));
#46395=CARTESIAN_POINT('Ctrl Pts',(3.6399552691467,5.70746157252985,-4.98354379677603));
#46396=CARTESIAN_POINT('Ctrl Pts',(3.48747218749065,5.80189199062351,-4.97512060586202));
#46397=CARTESIAN_POINT('Ctrl Pts',(3.33146557681007,5.89012954955403,-4.96669741494799));
#46398=CARTESIAN_POINT('Ctrl Pts',(3.25483486647963,5.93347198734671,-4.96255992936213));
#46399=CARTESIAN_POINT('Ctrl Pts',(3.17735444124636,5.97532088147924,-4.95842244377625));
#46400=CARTESIAN_POINT('Ctrl Pts',(3.09908550384723,6.01564277861011,-4.95428495819038));
#46401=CARTESIAN_POINT('Ctrl Pts',(3.09908550384728,6.01564277861009,-6.95401477785997));
#46402=CARTESIAN_POINT('Ctrl Pts',(2.94372312579465,6.09568099088196,-6.94578931815296));
#46403=CARTESIAN_POINT('Ctrl Pts',(2.78510216617008,6.16977702221691,-6.93756385844597));
#46404=CARTESIAN_POINT('Ctrl Pts',(2.62371606615217,6.23766005840451,-6.92933839873896));
#46405=CARTESIAN_POINT('Ctrl Pts',(2.46248089378075,6.30547961064345,-6.92112063144954));
#46406=CARTESIAN_POINT('Ctrl Pts',(2.29848606155289,6.36709761084517,-6.91290286416012));
#46407=CARTESIAN_POINT('Ctrl Pts',(2.13224832484289,6.42228978489796,-6.90468509687069));
#46408=CARTESIAN_POINT('Ctrl Pts',(1.9661012565253,6.47745185636518,-6.89647181166677));
#46409=CARTESIAN_POINT('Ctrl Pts',(1.79771405661862,6.52619496945636,-6.88825852646284));
#46410=CARTESIAN_POINT('Ctrl Pts',(1.62762253474435,6.56834331352986,-6.88004524125892));
#46411=CARTESIAN_POINT('Ctrl Pts',(1.45759198929683,6.61047654776492,-6.87183490045092));
#46412=CARTESIAN_POINT('Ctrl Pts',(1.28585868366744,6.64601963619481,-6.86362455964293));
#46413=CARTESIAN_POINT('Ctrl Pts',(1.11297273894915,6.67484686583565,-6.85541421883494));
#46414=CARTESIAN_POINT('Ctrl Pts',(1.00169281192937,6.69340182711861,-6.85012954327956));
#46415=CARTESIAN_POINT('Ctrl Pts',(0.889935635221197,6.70917542902428,-6.84484486772417));
#46416=CARTESIAN_POINT('Ctrl Pts',(0.777850161710652,6.722145351443,-6.83956019216879));
#46417=CARTESIAN_POINT('Ctrl Pts',(0.589960945506097,6.74388687138455,-6.83070147464816));
#46418=CARTESIAN_POINT('Ctrl Pts',(0.401343712628413,6.75772536213437,-6.82184275712753));
#46419=CARTESIAN_POINT('Ctrl Pts',(0.212651766161567,6.7636579028177,-6.8129840396069));
#46420=CARTESIAN_POINT('Ctrl Pts',(0.0236068073694866,6.76960154233181,
-6.80410874884863));
#46421=CARTESIAN_POINT('Ctrl Pts',(-0.165512885127531,6.76760966529908,
-6.79523345809037));
#46422=CARTESIAN_POINT('Ctrl Pts',(-0.354056027043083,6.75773137448615,
-6.7863581673321));
#46423=CARTESIAN_POINT('Ctrl Pts',(-0.543134673873633,6.74782502710628,
-6.77745766875256));
#46424=CARTESIAN_POINT('Ctrl Pts',(-0.731633232608158,6.72998745607991,
-6.76855717017301));
#46425=CARTESIAN_POINT('Ctrl Pts',(-0.918904468882634,6.70431976989967,
-6.75965667159348));
#46426=CARTESIAN_POINT('Ctrl Pts',(-1.10642921447976,6.67861733733836,-6.75074412439712));
#46427=CARTESIAN_POINT('Ctrl Pts',(-1.29272306280434,6.64506365792602,-6.74183157720076));
#46428=CARTESIAN_POINT('Ctrl Pts',(-1.47714958757996,6.60381087675233,-6.7329190300044));
#46429=CARTESIAN_POINT('Ctrl Pts',(-1.6619833441341,6.5624670054089,-6.7239868030334));
#46430=CARTESIAN_POINT('Ctrl Pts',(-1.84494127586665,6.51339008559803,-6.71505457606242));
#46431=CARTESIAN_POINT('Ctrl Pts',(-2.02539994993796,6.45678279352739,-6.70612234909142));
#46432=CARTESIAN_POINT('Ctrl Pts',(-2.19595423570235,6.40328236569897,-6.69768036313999));
#46433=CARTESIAN_POINT('Ctrl Pts',(-2.36427605199081,6.34305596615075,-6.68923837718855));
#46434=CARTESIAN_POINT('Ctrl Pts',(-2.52985608457464,6.27631398125848,-6.68079639123712));
#46435=CARTESIAN_POINT('Ctrl Pts',(-2.69116006683436,6.21129558635274,-6.67257241681886));
#46436=CARTESIAN_POINT('Ctrl Pts',(-2.85016978965994,6.1399686234312,-6.66434844240058));
#46437=CARTESIAN_POINT('Ctrl Pts',(-3.00635765272632,6.06251619906239,-6.6561244679823));
#46438=CARTESIAN_POINT('Ctrl Pts',(-3.16238056625533,5.98514557196846,-6.64790917887894));
#46439=CARTESIAN_POINT('Ctrl Pts',(-3.31558723591539,5.90166252353698,-6.63969388977555));
#46440=CARTESIAN_POINT('Ctrl Pts',(-3.46546847096888,5.81229879451501,-6.63147860067218));
#46441=CARTESIAN_POINT('Ctrl Pts',(-3.61522147987744,5.72301151780187,-6.62327033989929));
#46442=CARTESIAN_POINT('Ctrl Pts',(-3.76165441395981,5.62785376290883,-6.61506207912641));
#46443=CARTESIAN_POINT('Ctrl Pts',(-3.9042811250425,5.5271039339456,-6.60685381835351));
#46444=CARTESIAN_POINT('Ctrl Pts',(-4.04681441609006,5.42642009579495,-6.59865093396491));
#46445=CARTESIAN_POINT('Ctrl Pts',(-4.18554615821571,5.32015168562442,-6.59044804957631));
#46446=CARTESIAN_POINT('Ctrl Pts',(-4.32001766245039,5.20862135273017,-6.58224516518771));
#46447=CARTESIAN_POINT('Ctrl Pts',(-4.454428047211,5.09714171217649,-6.57404600914276));
#46448=CARTESIAN_POINT('Ctrl Pts',(-4.58458177634407,4.98040514210116,-6.56584685309781));
#46449=CARTESIAN_POINT('Ctrl Pts',(-4.71005177716155,4.85877569521966,-6.55764769705286));
#46450=CARTESIAN_POINT('Ctrl Pts',(-4.83551086513983,4.73715682714256,-6.54944925413513));
#46451=CARTESIAN_POINT('Ctrl Pts',(-4.95628677300689,4.61064617319267,-6.54125081121741));
#46452=CARTESIAN_POINT('Ctrl Pts',(-5.07198770799842,4.47964615677544,-6.53305236829967));
#46453=CARTESIAN_POINT('Ctrl Pts',(-5.1876874907456,4.3486474449633,-6.52485400702872));
#46454=CARTESIAN_POINT('Ctrl Pts',(-5.29831216303947,4.21315972788572,-6.51665564575777));
#46455=CARTESIAN_POINT('Ctrl Pts',(-5.40350890565426,4.07362007390418,-6.50845728448682));
#46456=CARTESIAN_POINT('Ctrl Pts',(-5.50872371037568,3.93405646119497,-6.5002575155708));
#46457=CARTESIAN_POINT('Ctrl Pts',(-5.60850851273157,3.79043981195242,-6.49205774665481));
#46458=CARTESIAN_POINT('Ctrl Pts',(-5.70255264668566,3.64323788844188,-6.48385797773879));
#46459=CARTESIAN_POINT('Ctrl Pts',(-5.79663001183018,3.49598395004272,-6.47565531137377));
#46460=CARTESIAN_POINT('Ctrl Pts',(-5.8849624747538,3.34514251581136,-6.46745264500874));
#46461=CARTESIAN_POINT('Ctrl Pts',(-5.96728429184347,3.19120779334693,-6.45924997864372));
#46462=CARTESIAN_POINT('Ctrl Pts',(-6.04969960594082,3.03709823951412,-6.45103799609998));
#46463=CARTESIAN_POINT('Ctrl Pts',(-6.12609046668072,2.87988869538403,-6.44282601355628));
#46464=CARTESIAN_POINT('Ctrl Pts',(-6.1962380045632,2.72009624660722,-6.43461403101254));
#46465=CARTESIAN_POINT('Ctrl Pts',(-6.26642691641151,2.56020955008465,-6.42639720493053));
#46466=CARTESIAN_POINT('Ctrl Pts',(-6.33036503393945,2.39773724539352,-6.41818037884849));
#46467=CARTESIAN_POINT('Ctrl Pts',(-6.38788279024429,2.2332134824286,-6.40996355276648));
#46468=CARTESIAN_POINT('Ctrl Pts',(-6.44548924723638,2.06843600005976,-6.40173405515192));
#46469=CARTESIAN_POINT('Ctrl Pts',(-6.49665545189059,1.90160107999209,-6.39350455753737));
#46470=CARTESIAN_POINT('Ctrl Pts',(-6.54126223146,1.73325630513059,-6.38527505992281));
#46471=CARTESIAN_POINT('Ctrl Pts',(-6.58102281408157,1.58320094595872,-6.37793963640657));
#46472=CARTESIAN_POINT('Ctrl Pts',(-6.61557250581569,1.43194629982475,-6.37060421289033));
#46473=CARTESIAN_POINT('Ctrl Pts',(-6.64486161374839,1.27988403151738,-6.36326878937409));
#46474=CARTESIAN_POINT('Ctrl Pts',(-6.6917400058292,1.0365022716225,-6.35152814980036));
#46475=CARTESIAN_POINT('Ctrl Pts',(-6.7252771074405,0.790369188616169,-6.33978751022664));
#46476=CARTESIAN_POINT('Ctrl Pts',(-6.74520470436182,0.542680841982831,
-6.32804687065291));
#46477=CARTESIAN_POINT('Ctrl Pts',(-6.75947725452555,0.365281411120508,
-6.31963798583193));
#46478=CARTESIAN_POINT('Ctrl Pts',(-6.7667692658776,0.187084554290086,-6.31122910101097));
#46479=CARTESIAN_POINT('Ctrl Pts',(-6.76699461023721,0.0085407857079797,
-6.30282021618999));
#46480=CARTESIAN_POINT('',(-6.767,1.31899902783804E-12,-6.69717978381011));
#46481=CARTESIAN_POINT('Ctrl Pts',(3.09908550384714,6.01564277861016,-7.34868366182764));
#46482=CARTESIAN_POINT('Ctrl Pts',(2.94200344356414,6.09656692152444,-7.34037397322581));
#46483=CARTESIAN_POINT('Ctrl Pts',(2.7818368468515,6.17128969279476,-7.33206428462395));
#46484=CARTESIAN_POINT('Ctrl Pts',(2.61911520635259,6.23959329891401,-7.32375459602213));
#46485=CARTESIAN_POINT('Ctrl Pts',(2.4562330644433,6.30796427668145,-7.31543671111197));
#46486=CARTESIAN_POINT('Ctrl Pts',(2.29079116923637,6.36990331782327,-7.30711882620181));
#46487=CARTESIAN_POINT('Ctrl Pts',(2.12333635217102,6.42524176475478,-7.29880094129163));
#46488=CARTESIAN_POINT('Ctrl Pts',(2.06708211921916,6.44383198472835,-7.29600665777322));
#46489=CARTESIAN_POINT('Ctrl Pts',(2.01060083010719,6.46167772582537,-7.29321237425482));
#46490=CARTESIAN_POINT('Ctrl Pts',(1.95391351252487,6.47877387979954,-7.29041809073641));
#46491=CARTESIAN_POINT('Ctrl Pts',(1.78246854235173,6.53047944169917,-7.28196706721121));
#46492=CARTESIAN_POINT('Ctrl Pts',(1.60882488134752,6.57541929489793,-7.273516043686));
#46493=CARTESIAN_POINT('Ctrl Pts',(1.43354279756602,6.61341394799589,-7.2650650201608));
#46494=CARTESIAN_POINT('Ctrl Pts',(1.25841504444962,6.65137514793107,-7.25662143751063));
#46495=CARTESIAN_POINT('Ctrl Pts',(1.08165206635396,6.68240326630607,-7.24817785486046));
#46496=CARTESIAN_POINT('Ctrl Pts',(0.903828398855612,6.7063688554554,-7.23973427221029));
#46497=CARTESIAN_POINT('Ctrl Pts',(0.726137126617511,6.73031660147699,-7.23129697607045));
#46498=CARTESIAN_POINT('Ctrl Pts',(0.547387066681654,6.74721225626119,-7.22285967993061));
#46499=CARTESIAN_POINT('Ctrl Pts',(0.368162427983455,6.75697753634133,-7.21442238379078));
#46500=CARTESIAN_POINT('Ctrl Pts',(0.189065652399561,6.76673584963871,-7.20599110701841));
#46501=CARTESIAN_POINT('Ctrl Pts',(0.00949530359264483,6.76937391707232,
-7.19755983024603));
#46502=CARTESIAN_POINT('Ctrl Pts',(-0.169959600044876,6.76486531531505,
-7.18912855347367));
#46503=CARTESIAN_POINT('Ctrl Pts',(-0.34933758281461,6.7603586461077,-7.18070089065173));
#46504=CARTESIAN_POINT('Ctrl Pts',(-0.528599888290563,6.74871142288825,
-7.17227322782982));
#46505=CARTESIAN_POINT('Ctrl Pts',(-0.707157146879609,6.72994931404517,
-7.16384556500788));
#46506=CARTESIAN_POINT('Ctrl Pts',(-0.885659438482283,6.71119298092127,
-7.15542049655389));
#46507=CARTESIAN_POINT('Ctrl Pts',(-1.06345678674942,6.68532616467469,-7.14699542809988));
#46508=CARTESIAN_POINT('Ctrl Pts',(-1.23996422122642,6.65242645431563,-7.13857035964589));
#46509=CARTESIAN_POINT('Ctrl Pts',(-1.28826205805277,6.64342408652718,-7.13626500303217));
#46510=CARTESIAN_POINT('Ctrl Pts',(-1.3364633524736,6.63389543839418,-7.13395964641846));
#46511=CARTESIAN_POINT('Ctrl Pts',(-1.38455622051691,6.62384277230581,-7.13165428980474));
#46512=CARTESIAN_POINT('Ctrl Pts',(-1.56436001976624,6.58625907998689,-7.12303530128034));
#46513=CARTESIAN_POINT('Ctrl Pts',(-1.74256715692082,6.54136368508706,-7.11441631275595));
#46514=CARTESIAN_POINT('Ctrl Pts',(-1.91858422653124,6.48932381421251,-7.10579732423155));
#46515=CARTESIAN_POINT('Ctrl Pts',(-2.09470674607431,6.4372527668112,-7.09717317216385));
#46516=CARTESIAN_POINT('Ctrl Pts',(-2.26863628795792,6.3780287877381,-7.08854902009614));
#46517=CARTESIAN_POINT('Ctrl Pts',(-2.43979599739637,6.31186854196827,-7.07992486802844));
#46518=CARTESIAN_POINT('Ctrl Pts',(-2.61681797293183,6.2434422899811,-7.07100533643219));
#46519=CARTESIAN_POINT('Ctrl Pts',(-2.79087669084853,6.16759635760581,-7.06208580483594));
#46520=CARTESIAN_POINT('Ctrl Pts',(-2.96135853479528,6.08462362257479,-7.05316627323968));
#46521=CARTESIAN_POINT('Ctrl Pts',(-3.12650176645941,6.00424916576569,-7.04452605538049));
#46522=CARTESIAN_POINT('Ctrl Pts',(-3.28828850598584,5.91718768584641,-7.03588583752132));
#46523=CARTESIAN_POINT('Ctrl Pts',(-3.44618745744697,5.82375145487298,-7.02724561966213));
#46524=CARTESIAN_POINT('Ctrl Pts',(-3.61174304678404,5.72578443139944,-7.01818643119735));
#46525=CARTESIAN_POINT('Ctrl Pts',(-3.77302410569276,5.62080926558137,-7.00912724273256));
#46526=CARTESIAN_POINT('Ctrl Pts',(-3.92945352472115,5.50923624444047,-7.00006805426778));
#46527=CARTESIAN_POINT('Ctrl Pts',(-4.08588294374954,5.39766322329956,-6.991008865803));
#46528=CARTESIAN_POINT('Ctrl Pts',(-4.2374604415056,5.27949260821497,-6.9819496773382));
#46529=CARTESIAN_POINT('Ctrl Pts',(-4.38364937395421,5.15518255411299,-6.97289048887341));
#46530=CARTESIAN_POINT('Ctrl Pts',(-4.52958504433626,5.03108785845619,-6.9638469948169));
#46531=CARTESIAN_POINT('Ctrl Pts',(-4.67028579583294,4.90076130110252,-6.95480350076039));
#46532=CARTESIAN_POINT('Ctrl Pts',(-4.80524874609557,4.76464830686872,-6.94576000670389));
#46533=CARTESIAN_POINT('Ctrl Pts',(-4.9400882462411,4.62865981469304,-6.93672478469832));
#46534=CARTESIAN_POINT('Ctrl Pts',(-5.06920025600074,4.48689562171797,-6.92768956269277));
#46535=CARTESIAN_POINT('Ctrl Pts',(-5.19211806112594,4.33983859599984,-6.91865434068721));
#46536=CARTESIAN_POINT('Ctrl Pts',(-5.31481931183733,4.19304065274716,-6.90963503677588));
#46537=CARTESIAN_POINT('Ctrl Pts',(-5.4313479970059,4.04096867969486,-6.90061573286456));
#46538=CARTESIAN_POINT('Ctrl Pts',(-5.54127714858927,3.88413910185029,-6.89159642895323));
#46539=CARTESIAN_POINT('Ctrl Pts',(-5.65106838637363,3.72750627766539,-6.88258844038864));
#46540=CARTESIAN_POINT('Ctrl Pts',(-5.75427647750861,3.56612795463913,-6.87358045182403));
#46541=CARTESIAN_POINT('Ctrl Pts',(-5.85051575148578,3.40055207894495,-6.86457246325944));
#46542=CARTESIAN_POINT('Ctrl Pts',(-5.94653766569161,3.23535016216579,-6.85558481955256));
#46543=CARTESIAN_POINT('Ctrl Pts',(-6.03562206043584,3.06596982176754,-6.84659717584569));
#46544=CARTESIAN_POINT('Ctrl Pts',(-6.11742769958871,2.89298588664113,-6.83760953213881));
#46545=CARTESIAN_POINT('Ctrl Pts',(-6.18867474131694,2.7423288687156,-6.82978191740645));
#46546=CARTESIAN_POINT('Ctrl Pts',(-6.25440127660616,2.58893899415625,-6.82195430267408));
#46547=CARTESIAN_POINT('Ctrl Pts',(-6.31440909771308,2.43321325549535,-6.81412668794172));
#46548=CARTESIAN_POINT('Ctrl Pts',(-6.37465596804438,2.27686716241471,-6.80626789085354));
#46549=CARTESIAN_POINT('Ctrl Pts',(-6.42912601522734,2.11819375689573,-6.79840909376536));
#46550=CARTESIAN_POINT('Ctrl Pts',(-6.47763603090721,1.95768241834388,-6.79055029667717));
#46551=CARTESIAN_POINT('Ctrl Pts',(-6.52615098102859,1.79715475256967,-6.7826907001917));
#46552=CARTESIAN_POINT('Ctrl Pts',(-6.56870456311595,1.63478914977025,-6.77483110370624));
#46553=CARTESIAN_POINT('Ctrl Pts',(-6.60516308027976,1.47109132378285,-6.76697150722077));
#46554=CARTESIAN_POINT('Ctrl Pts',(-6.64162179949535,1.30739259058809,-6.7591118671777));
#46555=CARTESIAN_POINT('Ctrl Pts',(-6.67198530883263,1.14236200194392,-6.75125222713463));
#46556=CARTESIAN_POINT('Ctrl Pts',(-6.69617098524394,0.976515814709235,
-6.74339258709157));
#46557=CARTESIAN_POINT('Ctrl Pts',(-6.720373904881,0.810551387107869,-6.73552734350262));
#46558=CARTESIAN_POINT('Ctrl Pts',(-6.73839014284395,0.643770586544007,
-6.72766209991364));
#46559=CARTESIAN_POINT('Ctrl Pts',(-6.75018891372674,0.4766955307118,-6.71979685632468));
#46560=CARTESIAN_POINT('Ctrl Pts',(-6.76140225160766,0.31791042748965,-6.71232187145086));
#46561=CARTESIAN_POINT('Ctrl Pts',(-6.76700020687108,0.158859864586206,
-6.70484688657703));
#46562=CARTESIAN_POINT('Ctrl Pts',(-6.76699999999426,-8.81190322315926E-6,
-6.6973719017032));
#46563=CARTESIAN_POINT('Ctrl Pts',(-6.767,1.31899900917185E-12,-6.6971797838101));
#46564=CARTESIAN_POINT('Ctrl Pts',(-6.76700000000004,-0.186007249558627,
-6.68843027199736));
#46565=CARTESIAN_POINT('Ctrl Pts',(-6.75932637294254,-0.372014355814748,
-6.67968076018463));
#46566=CARTESIAN_POINT('Ctrl Pts',(-6.74400518263374,-0.557389537585063,
-6.67093124837189));
#46567=CARTESIAN_POINT('Ctrl Pts',(-6.72868405703741,-0.742763936381794,
-6.66218177351468));
#46568=CARTESIAN_POINT('Ctrl Pts',(-6.70571545643574,-0.927506130404363,
-6.65343229865747));
#46569=CARTESIAN_POINT('Ctrl Pts',(-6.6751773940158,-1.11098864009513,-6.64468282380025));
#46570=CARTESIAN_POINT('Ctrl Pts',(-6.64463945804395,-1.29447039004509,
-6.63593338517174));
#46571=CARTESIAN_POINT('Ctrl Pts',(-6.60653217002731,-1.47669218339244,
-6.62718394654323));
#46572=CARTESIAN_POINT('Ctrl Pts',(-6.56098496085489,-1.65703510627748,
-6.61843450791471));
#46573=CARTESIAN_POINT('Ctrl Pts',(-6.51543793649563,-1.83737729739984,
-6.60968510478808));
#46574=CARTESIAN_POINT('Ctrl Pts',(-6.46245112156901,-2.01584035544936,
-6.60093570166145));
#46575=CARTESIAN_POINT('Ctrl Pts',(-6.40220448361719,-2.19181813797402,
-6.59218629853481));
#46576=CARTESIAN_POINT('Ctrl Pts',(-6.34195808511981,-2.36779522106281,
-6.58343693018329));
#46577=CARTESIAN_POINT('Ctrl Pts',(-6.27445201416368,-2.54128677725708,
-6.57468756183176));
#46578=CARTESIAN_POINT('Ctrl Pts',(-6.19991555052746,-2.71170355428608,
-6.56593819348024));
#46579=CARTESIAN_POINT('Ctrl Pts',(-6.12537937695139,-2.88211966813477,
-6.55718885917705));
#46580=CARTESIAN_POINT('Ctrl Pts',(-6.04381298028365,-3.04946076419841,
-6.54843952487388));
#46581=CARTESIAN_POINT('Ctrl Pts',(-5.95549339308889,-3.21315848424485,
-6.5396901905707));
#46582=CARTESIAN_POINT('Ctrl Pts',(-5.86717414225711,-3.37685558085253,
-6.53094088958914));
#46583=CARTESIAN_POINT('Ctrl Pts',(-5.77210188843963,-3.53690907700169,
-6.52219158860758));
#46584=CARTESIAN_POINT('Ctrl Pts',(-5.67059953311263,-3.69277537024158,
-6.51344228762603));
#46585=CARTESIAN_POINT('Ctrl Pts',(-5.56909755592579,-3.84864108281213,
-6.5046930192394));
#46586=CARTESIAN_POINT('Ctrl Pts',(-5.46116568154816,-4.00031938355035,
-6.49594375085278));
#46587=CARTESIAN_POINT('Ctrl Pts',(-5.34717048488204,-4.14729511918388,
-6.48719448246615));
#46588=CARTESIAN_POINT('Ctrl Pts',(-5.2331757034312,-4.29427031947405,-6.4784452459478));
#46589=CARTESIAN_POINT('Ctrl Pts',(-5.1131178195135,-4.43654276249783,-6.46969600942943));
#46590=CARTESIAN_POINT('Ctrl Pts',(-4.98740458929035,-4.57362924412612,
-6.46094677291107));
#46591=CARTESIAN_POINT('Ctrl Pts',(-4.86169180652517,-4.71071523781498,
-6.45219756753435));
#46592=CARTESIAN_POINT('Ctrl Pts',(-4.73032391141336,-4.84261509584721,
-6.44344836215764));
#46593=CARTESIAN_POINT('Ctrl Pts',(-4.59374706947077,-4.9688808459983,-6.43469915678092));
#46594=CARTESIAN_POINT('Ctrl Pts',(-4.45717070231283,-5.09514615720938,
-6.42594998181922));
#46595=CARTESIAN_POINT('Ctrl Pts',(-4.31538563497165,-5.21577720520745,
-6.41720080685753));
#46596=CARTESIAN_POINT('Ctrl Pts',(-4.16887340951873,-5.33036429293606,
-6.40845163189584));
#46597=CARTESIAN_POINT('Ctrl Pts',(-4.02236168122362,-5.44495099183796,
-6.39970248662259));
#46598=CARTESIAN_POINT('Ctrl Pts',(-3.8711230526307,-5.55349359498005,-6.39095334134935));
#46599=CARTESIAN_POINT('Ctrl Pts',(-3.71567116928898,-5.65562346357276,
-6.3822041960761));
#46600=CARTESIAN_POINT('Ctrl Pts',(-3.56021980053228,-5.75775299408978,
-6.37345507976474));
#46601=CARTESIAN_POINT('Ctrl Pts',(-3.40055544442016,-5.85346967519918,
-6.36470596345339));
#46602=CARTESIAN_POINT('Ctrl Pts',(-3.23722035886792,-5.94244843041411,
-6.35595684714203));
#46603=CARTESIAN_POINT('Ctrl Pts',(-3.0738858004343,-6.03142689847482,-6.34720775906601));
#46604=CARTESIAN_POINT('Ctrl Pts',(-2.90688078789154,-6.11366734707935,
-6.33845867098999));
#46605=CARTESIAN_POINT('Ctrl Pts',(-2.73677250610315,-6.18889047001463,
-6.32970958291397));
#46606=CARTESIAN_POINT('Ctrl Pts',(-2.56666475916863,-6.26411335643363,
-6.32096052234681));
#46607=CARTESIAN_POINT('Ctrl Pts',(-2.39345402457027,-6.33231884545281,
-6.31221146177964));
#46608=CARTESIAN_POINT('Ctrl Pts',(-2.21772855944005,-6.39327529804903,
-6.30346240121247));
#46609=CARTESIAN_POINT('Ctrl Pts',(-2.0420036322354,-6.45423156404718,-6.29471336742767));
#46610=CARTESIAN_POINT('Ctrl Pts',(-1.86376426060992,-6.50793874412465,
-6.28596433364288));
#46611=CARTESIAN_POINT('Ctrl Pts',(-1.68361577621656,-6.5542144394332,-6.27721529985808));
#46612=CARTESIAN_POINT('Ctrl Pts',(-1.50346782833206,-6.60048999692589,
-6.26846629212919));
#46613=CARTESIAN_POINT('Ctrl Pts',(-1.32141105657402,-6.63933404265158,
-6.25971728440031));
#46614=CARTESIAN_POINT('Ctrl Pts',(-1.13806375346573,-6.67061465631523,
-6.25096827667143));
#46615=CARTESIAN_POINT('Ctrl Pts',(-0.954716981170584,-6.70189517941762,
-6.24221929427201));
#46616=CARTESIAN_POINT('Ctrl Pts',(-0.770079967443055,-6.72561226608995,
-6.23347031187258));
#46617=CARTESIAN_POINT('Ctrl Pts',(-0.58477976407404,-6.74168536995976,
-6.22472132947316));
#46618=CARTESIAN_POINT('Ctrl Pts',(-0.391489587593874,-6.75845153117867,
-6.21559509905754));
#46619=CARTESIAN_POINT('Ctrl Pts',(-0.1974780918061,-6.76689985146392,-6.20646886864193));
#46620=CARTESIAN_POINT('Ctrl Pts',(-0.0034621475318405,-6.76699911434415,
-6.19734263822631));
#46621=CARTESIAN_POINT('Ctrl Pts',(0.184490798483868,-6.76709527525937,
-6.18850160251118));
#46622=CARTESIAN_POINT('Ctrl Pts',(0.372447602154045,-6.75935633790767,
-6.17966056679605));
#46623=CARTESIAN_POINT('Ctrl Pts',(0.55975644819352,-6.74380914014519,-6.17081953108092));
#46624=CARTESIAN_POINT('Ctrl Pts',(0.745136131042648,-6.72842206873162,
-6.16206955246761));
#46625=CARTESIAN_POINT('Ctrl Pts',(0.929880851944321,-6.70538686355733,
-6.15331957385431));
#46626=CARTESIAN_POINT('Ctrl Pts',(1.11336305057389,-6.67478177303324,-6.144569595241));
#46627=CARTESIAN_POINT('Ctrl Pts',(1.29684337090052,-6.64417699581275,-6.13581970620102));
#46628=CARTESIAN_POINT('Ctrl Pts',(1.47906091205121,-6.60600253548075,-6.12706981716103));
#46629=CARTESIAN_POINT('Ctrl Pts',(1.65939671095154,-6.56038806441229,-6.11831992812105));
#46630=CARTESIAN_POINT('Ctrl Pts',(1.83973072369088,-6.5147740451387,-6.10957012574556));
#46631=CARTESIAN_POINT('Ctrl Pts',(2.01818275356959,-6.46172023288685,-6.10082032337007));
#46632=CARTESIAN_POINT('Ctrl Pts',(2.19414664033244,-6.40140683918136,-6.09207052099458));
#46633=CARTESIAN_POINT('Ctrl Pts',(2.37010884271175,-6.34109402281529,-6.08332080237505));
#46634=CARTESIAN_POINT('Ctrl Pts',(2.54358267847721,-6.27352185699826,-6.07457108375552));
#46635=CARTESIAN_POINT('Ctrl Pts',(2.71397890841655,-6.19891986435299,-6.06582136513599));
#46636=CARTESIAN_POINT('Ctrl Pts',(2.88437356388866,-6.12431856103279,-6.05707172736416));
#46637=CARTESIAN_POINT('Ctrl Pts',(3.05169040787107,-6.0426876758259,-6.04832208959234));
#46638=CARTESIAN_POINT('Ctrl Pts',(3.21536112511998,-5.95430447953975,-6.03957245182052));
#46639=CARTESIAN_POINT('Ctrl Pts',(3.37903038442792,-5.86592207055072,-6.03082289198845));
#46640=CARTESIAN_POINT('Ctrl Pts',(3.53905332979926,-5.77078760703406,-6.02207333215635));
#46641=CARTESIAN_POINT('Ctrl Pts',(3.69488643041849,-5.66922422085327,-6.01332377232428));
#46642=CARTESIAN_POINT('Ctrl Pts',(3.85071819468698,-5.56766170563189,-6.00457428752429));
#46643=CARTESIAN_POINT('Ctrl Pts',(4.00235994599179,-5.45967053456284,-5.9958248027243));
#46644=CARTESIAN_POINT('Ctrl Pts',(4.14929662974255,-5.3456175020672,-5.9870753179243));
#46645=CARTESIAN_POINT('Ctrl Pts',(4.29623210225003,-5.231565409745,-5.97832590524894));
#46646=CARTESIAN_POINT('Ctrl Pts',(4.43846235842079,-5.11145173172219,-5.96957649257358));
#46647=CARTESIAN_POINT('Ctrl Pts',(4.57550431797394,-4.98568443006593,-5.96082707989822));
#46648=CARTESIAN_POINT('Ctrl Pts',(4.71254519337467,-4.85991812336716,-5.95207773644033));
#46649=CARTESIAN_POINT('Ctrl Pts',(4.84439764314964,-4.72849847631122,-5.94332839298243));
#46650=CARTESIAN_POINT('Ctrl Pts',(4.97061384196672,-4.59187184425359,-5.93457904952453));
#46651=CARTESIAN_POINT('Ctrl Pts',(5.09682908420199,-4.45524624767756,-5.92582977237716));
#46652=CARTESIAN_POINT('Ctrl Pts',(5.21740796650169,-4.31341395556895,-5.9170804952298));
#46653=CARTESIAN_POINT('Ctrl Pts',(5.33194095942255,-4.16685668162851,-5.90833121808243));
#46654=CARTESIAN_POINT('Ctrl Pts',(5.44647312235137,-4.02030046975208,-5.89958200433889));
#46655=CARTESIAN_POINT('Ctrl Pts',(5.55495930712293,-3.86901957035539,-5.89083279059536));
#46656=CARTESIAN_POINT('Ctrl Pts',(5.65703106079801,-3.71352778058365,-5.88208357685183));
#46657=CARTESIAN_POINT('Ctrl Pts',(5.7591021086874,-3.55803706597597,-5.87333442360563));
#46658=CARTESIAN_POINT('Ctrl Pts',(5.85475865698551,-3.39833575880897,-5.86458527035943));
#46659=CARTESIAN_POINT('Ctrl Pts',(5.94367583069063,-3.23496624706721,-5.85583611711323));
#46660=CARTESIAN_POINT('Ctrl Pts',(6.03259241910076,-3.07159781070102,-5.84708702145811));
#46661=CARTESIAN_POINT('Ctrl Pts',(6.11476958470965,-2.90456146975838,-5.83833792580299));
#46662=CARTESIAN_POINT('Ctrl Pts',(6.18992823574383,-2.73442451648264,-5.82958883014787));
#46663=CARTESIAN_POINT('Ctrl Pts',(6.26508641700938,-2.5642886266241,-5.82083978917775));
#46664=CARTESIAN_POINT('Ctrl Pts',(6.33322605570304,-2.39105242531259,-5.81209074820762));
#46665=CARTESIAN_POINT('Ctrl Pts',(6.39411573747778,-2.21530425353698,-5.8033417072375));
#46666=CARTESIAN_POINT('Ctrl Pts',(6.45500505889137,-2.03955712188525,-5.7945927180465));
#46667=CARTESIAN_POINT('Ctrl Pts',(6.50864441544941,-1.8612983202553,-5.7858437288555));
#46668=CARTESIAN_POINT('Ctrl Pts',(6.55485164049919,-1.6811332401226,-5.7770947396645));
#46669=CARTESIAN_POINT('Ctrl Pts',(6.60199852639122,-1.49730435912843,-5.76816783278761));
#46670=CARTESIAN_POINT('Ctrl Pts',(6.64140767441022,-1.3114911317359,-5.75924092591072));
#46671=CARTESIAN_POINT('Ctrl Pts',(6.67293975269614,-1.12435050446364,-5.75031401903384));
#46672=CARTESIAN_POINT('Ctrl Pts',(6.70384664831516,-0.940920291563085,
-5.74156410484984));
#46673=CARTESIAN_POINT('Ctrl Pts',(6.72718585889673,-0.756215114277297,
-5.73281419066585));
#46674=CARTESIAN_POINT('Ctrl Pts',(6.7428781045187,-0.570862389374515,-5.72406427648186));
#46675=CARTESIAN_POINT('Ctrl Pts',(6.75857004154126,-0.385513309567596,
-5.71531453437128));
#46676=CARTESIAN_POINT('Ctrl Pts',(6.76661529035557,-0.199516993258827,
-5.7065647922607));
#46677=CARTESIAN_POINT('Ctrl Pts',(6.76698652348896,-0.0135052182047926,
-5.69781505015012));
#46678=CARTESIAN_POINT('Ctrl Pts',(6.76735774981523,0.172503146038172,-5.68906546847948));
#46679=CARTESIAN_POINT('Ctrl Pts',(6.76005524147483,0.358526681832767,-5.68031588680884));
#46680=CARTESIAN_POINT('Ctrl Pts',(6.74510380214887,0.543933542114178,-5.67156630513819));
#46681=CARTESIAN_POINT('Ctrl Pts',(6.73015261710987,0.729337249084028,-5.66281687227627));
#46682=CARTESIAN_POINT('Ctrl Pts',(6.70755278444615,0.914124015853962,-5.65406743941434));
#46683=CARTESIAN_POINT('Ctrl Pts',(6.67738106408301,1.09766621749315,-5.64531800655242));
#46684=CARTESIAN_POINT('Ctrl Pts',(6.64720981677268,1.28120554143251,-5.63656871087007));
#46685=CARTESIAN_POINT('Ctrl Pts',(6.60946696581539,1.46350005650549,-5.62781941518771));
#46686=CARTESIAN_POINT('Ctrl Pts',(6.56428070011012,1.64393062206462,-5.61907011950536));
#46687=CARTESIAN_POINT('Ctrl Pts',(6.51909508282762,1.82435859844577,-5.61032094937537));
#46688=CARTESIAN_POINT('Ctrl Pts',(6.46646633415686,2.00292240086485,-5.60157177924539));
#46689=CARTESIAN_POINT('Ctrl Pts',(6.4065731959722,2.17901557696373,-5.5928226091154));
#46690=CARTESIAN_POINT('Ctrl Pts',(6.34668083768323,2.3551064600736,-5.58407355291232));
#46691=CARTESIAN_POINT('Ctrl Pts',(6.27952437143912,2.52872650996464,-5.57532449670924));
#46692=CARTESIAN_POINT('Ctrl Pts',(6.20533187335162,2.69928607997866,-5.56657544050616));
#46693=CARTESIAN_POINT('Ctrl Pts',(6.12831449784278,2.87633970115342,-5.55749326421731));
#46694=CARTESIAN_POINT('Ctrl Pts',(6.04371489463178,3.05009490562299,-5.54841108792846));
#46695=CARTESIAN_POINT('Ctrl Pts',(5.95184265120515,3.21991584599586,-5.53932891163961));
#46696=CARTESIAN_POINT('Ctrl Pts',(5.86333281335517,3.38352155905257,-5.5305791312852));
#46697=CARTESIAN_POINT('Ctrl Pts',(5.7680733723571,3.54347560903783,-5.52182935093079));
#46698=CARTESIAN_POINT('Ctrl Pts',(5.66638790086381,3.69923467178608,-5.51307957057637));
#46699=CARTESIAN_POINT('Ctrl Pts',(5.56470608502773,3.8549881348972,-5.50433010478211));
#46700=CARTESIAN_POINT('Ctrl Pts',(5.45659885766987,4.00654667256213,-5.49558063898784));
#46701=CARTESIAN_POINT('Ctrl Pts',(5.34243340580548,4.15339551506159,-5.48683117319358));
#46702=CARTESIAN_POINT('Ctrl Pts',(5.22827145140633,4.30023985883823,-5.47808197543971));
#46703=CARTESIAN_POINT('Ctrl Pts',(5.10805181978127,4.44237456993,-5.46933277768583));
#46704=CARTESIAN_POINT('Ctrl Pts',(4.98218281282587,4.5793169162641,-5.46058357993196));
#46705=CARTESIAN_POINT('Ctrl Pts',(4.85631699296259,4.71625579512131,-5.45183460371396));
#46706=CARTESIAN_POINT('Ctrl Pts',(4.72480227791862,4.84800236135746,-5.44308562749596));
#46707=CARTESIAN_POINT('Ctrl Pts',(4.58808530848131,4.97410918678892,-5.43433665127795));
#46708=CARTESIAN_POINT('Ctrl Pts',(4.45135945056987,5.10022421088994,-5.42558710625675));
#46709=CARTESIAN_POINT('Ctrl Pts',(4.30943087208055,5.22069856611974,-5.41683756123554));
#46710=CARTESIAN_POINT('Ctrl Pts',(4.16278164322482,5.33512305301673,-5.40808801621434));
#46711=CARTESIAN_POINT('Ctrl Pts',(4.01614103534405,5.44954081331416,-5.39933898554708));
#46712=CARTESIAN_POINT('Ctrl Pts',(3.86478055833429,5.55790924068327,-5.39058995487984));
#46713=CARTESIAN_POINT('Ctrl Pts',(3.70921425811968,5.6598602975128,-5.38184092421258));
#46714=CARTESIAN_POINT('Ctrl Pts',(3.55364584530144,5.76181273884639,-5.37309177473274));
#46715=CARTESIAN_POINT('Ctrl Pts',(3.39387173464376,5.85734747818045,-5.36434262525288));
#46716=CARTESIAN_POINT('Ctrl Pts',(3.23043456092445,5.94614005448786,-5.35559347577304));
#46717=CARTESIAN_POINT('Ctrl Pts',(3.1869076880642,5.96978744811267,-5.35326338703999));
#46718=CARTESIAN_POINT('Ctrl Pts',(3.14312114982898,5.99295688499292,-5.35093329830695));
#46719=CARTESIAN_POINT('Ctrl Pts',(3.09908550384725,6.0156427786101,-5.3486032095739));
#46720=CARTESIAN_POINT('Origin',(0.,0.,-63.6971797838103));
#46721=CARTESIAN_POINT('',(3.09908550384716,6.01564277861015,-2.95434584629073));
#46722=CARTESIAN_POINT('',(3.09908550384726,6.0156427786101,-3.34860320957391));
#46723=CARTESIAN_POINT('',(3.09908550384721,6.01564277861012,-63.6971797838103));
#46724=CARTESIAN_POINT('',(-6.76699993702048,-0.000923236083376258,-4.30282021616649));
#46725=CARTESIAN_POINT('Ctrl Pts',(-6.76699993702048,-0.000923236083286258,
-4.30282021616649));
#46726=CARTESIAN_POINT('Ctrl Pts',(-6.7669744401561,-0.187806399292575,
-4.29407494551509));
#46727=CARTESIAN_POINT('Ctrl Pts',(-6.75920300097723,-0.374494000220519,
-4.2853296748637));
#46728=CARTESIAN_POINT('Ctrl Pts',(-6.74375962059959,-0.560352727815666,
-4.27658440421229));
#46729=CARTESIAN_POINT('Ctrl Pts',(-6.72828782458872,-0.746553433223164,
-4.26782304236859));
#46730=CARTESIAN_POINT('Ctrl Pts',(-6.70511590738353,-0.931921941745487,
-4.2590616805249));
#46731=CARTESIAN_POINT('Ctrl Pts',(-6.6743692209328,-1.11583354612812,-4.2503003186812));
#46732=CARTESIAN_POINT('Ctrl Pts',(-6.64228067589974,-1.30777149068659,
-4.24115659015217));
#46733=CARTESIAN_POINT('Ctrl Pts',(-6.60194150520994,-1.49812216265994,
-4.23201286162312));
#46734=CARTESIAN_POINT('Ctrl Pts',(-6.55355158142941,-1.68619413756071,
-4.22286913309409));
#46735=CARTESIAN_POINT('Ctrl Pts',(-6.50697258852339,-1.86722775985893,
-4.21406759688544));
#46736=CARTESIAN_POINT('Ctrl Pts',(-6.45293460916008,-2.04614991837855,
-4.20526606067679));
#46737=CARTESIAN_POINT('Ctrl Pts',(-6.39166523521518,-2.2223646237604,-4.19646452446813));
#46738=CARTESIAN_POINT('Ctrl Pts',(-6.33030499424766,-2.39884066861074,
-4.18764993492894));
#46739=CARTESIAN_POINT('Ctrl Pts',(-6.26169203660224,-2.57260098166927,
-4.17883534538975));
#46740=CARTESIAN_POINT('Ctrl Pts',(-6.18610139645694,-2.74307100031215,
-4.17002075585056));
#46741=CARTESIAN_POINT('Ctrl Pts',(-6.11035348030401,-2.9138957036607,-4.16118782642896));
#46742=CARTESIAN_POINT('Ctrl Pts',(-6.02759897279409,-3.08141617416001,
-4.15235489700738));
#46743=CARTESIAN_POINT('Ctrl Pts',(-5.93815896279803,-3.24508199165159,
-4.14352196758578));
#46744=CARTESIAN_POINT('Ctrl Pts',(-5.92821415851176,-3.26327993822358,
-4.14253983716812));
#46745=CARTESIAN_POINT('Ctrl Pts',(-5.91818674397737,-3.28143025942478,
-4.14155770675046));
#46746=CARTESIAN_POINT('Ctrl Pts',(-5.90807719298252,-3.29953222165807,
-4.14057557633281));
#46747=CARTESIAN_POINT('Ctrl Pts',(-5.82499975830413,-3.44828903447326,
-4.13250470595885));
#46748=CARTESIAN_POINT('Ctrl Pts',(-5.73614866817978,-3.59417773654744,
-4.12443383558491));
#46749=CARTESIAN_POINT('Ctrl Pts',(-5.64174723066037,-3.73670672990752,
-4.11636296521097));
#46750=CARTESIAN_POINT('Ctrl Pts',(-5.54746326837892,-3.87905835703406,
-4.10830213840673));
#46751=CARTESIAN_POINT('Ctrl Pts',(-5.44764290525162,-4.01805828733157,
-4.10024131160252));
#46752=CARTESIAN_POINT('Ctrl Pts',(-5.3425562510797,-4.15323749670655,-4.09218048479828));
#46753=CARTESIAN_POINT('Ctrl Pts',(-5.23757732516842,-4.28827812881672,
-4.08412792144917));
#46754=CARTESIAN_POINT('Ctrl Pts',(-5.12734307878022,-4.41950554250522,
-4.07607535810006));
#46755=CARTESIAN_POINT('Ctrl Pts',(-5.01216796210952,-4.54647790268499,
-4.06802279475095));
#46756=CARTESIAN_POINT('Ctrl Pts',(-4.89708569668207,-4.67334790098451,
-4.05997672317315));
#46757=CARTESIAN_POINT('Ctrl Pts',(-4.77707073828189,-4.79596939842845,
-4.05193065159535));
#46758=CARTESIAN_POINT('Ctrl Pts',(-4.65247895408675,-4.91393208965894,
-4.04388458001755));
#46759=CARTESIAN_POINT('Ctrl Pts',(-4.52796035958034,-5.03182548536798,
-4.03584323499117));
#46760=CARTESIAN_POINT('Ctrl Pts',(-4.39887056169622,-5.14506526717237,
-4.02780188996477));
#46761=CARTESIAN_POINT('Ctrl Pts',(-4.26560349006025,-5.25327667894866,
-4.01976054493839));
#46762=CARTESIAN_POINT('Ctrl Pts',(-4.12976744452351,-5.36357406957334,
-4.01156418783554));
#46763=CARTESIAN_POINT('Ctrl Pts',(-3.989591700041,-5.46864695758852,-4.00336783073271));
#46764=CARTESIAN_POINT('Ctrl Pts',(-3.84553058218129,-5.56814004327373,
-3.99517147362985));
#46765=CARTESIAN_POINT('Ctrl Pts',(-3.70423892045861,-5.6657204564708,-3.98713268473011));
#46766=CARTESIAN_POINT('Ctrl Pts',(-3.55921024720981,-5.75793345376984,
-3.97909389583036));
#46767=CARTESIAN_POINT('Ctrl Pts',(-3.41090384310648,-5.84448663041344,
-3.97105510693062));
#46768=CARTESIAN_POINT('Ctrl Pts',(-3.26258156887137,-5.9310490690328,-3.96301545780748));
#46769=CARTESIAN_POINT('Ctrl Pts',(-3.11098118792053,-6.01195029270372,
-3.95497580868433));
#46770=CARTESIAN_POINT('Ctrl Pts',(-2.95658775176706,-6.08694322842763,
-3.94693615956119));
#46771=CARTESIAN_POINT('Ctrl Pts',(-2.8021472236272,-6.16195903796274,-3.93889405824153));
#46772=CARTESIAN_POINT('Ctrl Pts',(-2.64491228029246,-6.23106280938724,
-3.93085195692187));
#46773=CARTESIAN_POINT('Ctrl Pts',(-2.48538902667397,-6.29405516230106,
-3.92280985560221));
#46774=CARTESIAN_POINT('Ctrl Pts',(-2.32048250087141,-6.3591732553409,-3.91449636550785));
#46775=CARTESIAN_POINT('Ctrl Pts',(-2.15313092619656,-6.41776008038371,
-3.90618287541348));
#46776=CARTESIAN_POINT('Ctrl Pts',(-1.98391054883965,-6.46965129927439,
-3.89786938531912));
#46777=CARTESIAN_POINT('Ctrl Pts',(-1.81992589778733,-6.51993698918583,
-3.88981311695804));
#46778=CARTESIAN_POINT('Ctrl Pts',(-1.65418673905913,-6.56393520726695,
-3.88175684859694));
#46779=CARTESIAN_POINT('Ctrl Pts',(-1.48722743952302,-6.60154857159514,
-3.87370058023586));
#46780=CARTESIAN_POINT('Ctrl Pts',(-1.31227208800184,-6.64096332355095,
-3.86525847927485));
#46781=CARTESIAN_POINT('Ctrl Pts',(-1.13597732951258,-6.67336652512646,
-3.85681637831386));
#46782=CARTESIAN_POINT('Ctrl Pts',(-0.958962872365025,-6.69870727897745,
-3.84837427735285));
#46783=CARTESIAN_POINT('Ctrl Pts',(-0.781948415217469,-6.72404803282843,
-3.83993217639185));
#46784=CARTESIAN_POINT('Ctrl Pts',(-0.604214726714419,-6.74232637782005,
-3.83149007543084));
#46785=CARTESIAN_POINT('Ctrl Pts',(-0.426379507918857,-6.75355384336476,
-3.82304797446984));
#46786=CARTESIAN_POINT('Ctrl Pts',(-0.250824807746037,-6.76463733043077,
-3.81471413310211));
#46787=CARTESIAN_POINT('Ctrl Pts',(-0.0746130893532963,-6.76888553519746,
-3.8063802917344));
#46788=CARTESIAN_POINT('Ctrl Pts',(0.101689154437278,-6.76623590453879,
-3.79804645036667));
#46789=CARTESIAN_POINT('Ctrl Pts',(0.277783603723323,-6.76358939680515,
-3.7897224314856));
#46790=CARTESIAN_POINT('Ctrl Pts',(0.453968021015937,-6.75406125446949,
-3.78139841260451));
#46791=CARTESIAN_POINT('Ctrl Pts',(0.629671634160306,-6.73764073197242,
-3.77307439372344));
#46792=CARTESIAN_POINT('Ctrl Pts',(0.805200373409075,-6.72123655245594,
-3.7647586595531));
#46793=CARTESIAN_POINT('Ctrl Pts',(0.980248917723264,-6.69795369201965,
-3.75644292538275));
#46794=CARTESIAN_POINT('Ctrl Pts',(1.1542471095858,-6.66783342698457,-3.7481271912124));
#46795=CARTESIAN_POINT('Ctrl Pts',(1.32810400592666,-6.63773762116092,-3.73981820984785));
#46796=CARTESIAN_POINT('Ctrl Pts',(1.50091190811382,-6.6008155333522,-3.73150922848331));
#46797=CARTESIAN_POINT('Ctrl Pts',(1.67210616528295,-6.55716020637156,-3.72320024711875));
#46798=CARTESIAN_POINT('Ctrl Pts',(1.8431927539021,-6.51353233536891,-3.7148964914901));
#46799=CARTESIAN_POINT('Ctrl Pts',(2.01266738391637,-6.46317975023025,-3.70659273586143));
#46800=CARTESIAN_POINT('Ctrl Pts',(2.17997575605842,-6.40624653779399,-3.69828898023278));
#46801=CARTESIAN_POINT('Ctrl Pts',(2.34721620534498,-6.3493364387639,-3.68998859571334));
#46802=CARTESIAN_POINT('Ctrl Pts',(2.51229182036566,-6.28585114760582,-3.68168821119389));
#46803=CARTESIAN_POINT('Ctrl Pts',(2.674663342484,-6.21598463675485,-3.67338782667445));
#46804=CARTESIAN_POINT('Ctrl Pts',(2.83700062487769,-6.14613285884512,-3.66508919247967));
#46805=CARTESIAN_POINT('Ctrl Pts',(2.9966346310973,-6.06990267944113,-3.65679055828492));
#46806=CARTESIAN_POINT('Ctrl Pts',(3.15304574806969,-5.98753634732848,-3.64849192409014));
#46807=CARTESIAN_POINT('Ctrl Pts',(3.30944984469072,-5.90517371214353,-3.64019366237099));
#46808=CARTESIAN_POINT('Ctrl Pts',(3.46263103270155,-5.81667563527687,-3.63189540065179));
#46809=CARTESIAN_POINT('Ctrl Pts',(3.61209381974494,-5.72233057742738,-3.62359713893263));
#46810=CARTESIAN_POINT('Ctrl Pts',(3.76157470635164,-5.62797409463139,-3.61529787231509));
#46811=CARTESIAN_POINT('Ctrl Pts',(3.90733600098045,-5.5277694061083,-3.60699860569756));
#46812=CARTESIAN_POINT('Ctrl Pts',(4.04891058620135,-5.42204869629061,-3.59869933908002));
#46813=CARTESIAN_POINT('Ctrl Pts',(4.19058458010979,-5.31625375311391,-3.59039424500976));
#46814=CARTESIAN_POINT('Ctrl Pts',(4.32806571145238,-5.20493525774109,-3.58208915093949));
#46815=CARTESIAN_POINT('Ctrl Pts',(4.46091869638858,-5.0884667026729,-3.57378405686923));
#46816=CARTESIAN_POINT('Ctrl Pts',(4.59382012668081,-4.97195567689455,-3.56547593431421));
#46817=CARTESIAN_POINT('Ctrl Pts',(4.72208979020483,-4.8502910831247,-3.5571678117592));
#46818=CARTESIAN_POINT('Ctrl Pts',(4.84532863005262,-4.72388393875129,-3.54885968920418));
#46819=CARTESIAN_POINT('Ctrl Pts',(4.96869847261396,-4.59734242376107,-3.54054273512656));
#46820=CARTESIAN_POINT('Ctrl Pts',(5.08702656919703,-4.46604854002439,-3.53222578104894));
#46821=CARTESIAN_POINT('Ctrl Pts',(5.19995286785108,-4.33044791818668,-3.52390882697133));
#46822=CARTESIAN_POINT('Ctrl Pts',(5.28317805141306,-4.23051205932944,-3.51777934218314));
#46823=CARTESIAN_POINT('Ctrl Pts',(5.36347007604982,-4.1282377104919,-3.51164985739497));
#46824=CARTESIAN_POINT('Ctrl Pts',(5.44069978791588,-4.02381346706979,-3.50552037260679));
#46825=CARTESIAN_POINT('Ctrl Pts',(5.54718029662547,-3.8798384826689,-3.49706934200465));
#46826=CARTESIAN_POINT('Ctrl Pts',(5.64803248650558,-3.7315124930526,-3.48861831140253));
#46827=CARTESIAN_POINT('Ctrl Pts',(5.74289848198448,-3.57930244958712,-3.4801672808004));
#46828=CARTESIAN_POINT('Ctrl Pts',(5.83768095012316,-3.42722642358515,-3.47172369113752));
#46829=CARTESIAN_POINT('Ctrl Pts',(5.92648755485924,-3.27127344009668,-3.46328010147462));
#46830=CARTESIAN_POINT('Ctrl Pts',(6.00900272415619,-3.11194075475154,-3.45483651181173));
#46831=CARTESIAN_POINT('Ctrl Pts',(6.09145645761784,-2.95272669894683,-3.44639920873819));
#46832=CARTESIAN_POINT('Ctrl Pts',(6.16762794147849,-2.79013825084872,-3.43796190566463));
#46833=CARTESIAN_POINT('Ctrl Pts',(6.23724651100191,-2.62469902293472,-3.42952460259108));
#46834=CARTESIAN_POINT('Ctrl Pts',(6.30681541179301,-2.45937782612629,-3.42109331903432));
#46835=CARTESIAN_POINT('Ctrl Pts',(6.3698405952902,-2.29121021117695,-3.41266203547756));
#46836=CARTESIAN_POINT('Ctrl Pts',(6.4260985991014,-2.12074180291404,-3.4042307519208));
#46837=CARTESIAN_POINT('Ctrl Pts',(6.4823324880812,-1.95034646544364,-3.39580308240947));
#46838=CARTESIAN_POINT('Ctrl Pts',(6.53180487642007,-1.77765261495826,-3.38737541289814));
#46839=CARTESIAN_POINT('Ctrl Pts',(6.57434122516572,-1.60322376949896,-3.3789477433868));
#46840=CARTESIAN_POINT('Ctrl Pts',(6.61686447872655,-1.42884862347647,-3.37052266840681));
#46841=CARTESIAN_POINT('Ctrl Pts',(6.65245587262219,-1.25273986934714,-3.36209759342683));
#46842=CARTESIAN_POINT('Ctrl Pts',(6.68099123182748,-1.0754743884651,-3.35367251844684));
#46843=CARTESIAN_POINT('Ctrl Pts',(6.68879923455886,-1.02697002764914,-3.35136720285636));
#46844=CARTESIAN_POINT('Ctrl Pts',(6.69607923934458,-0.978379126285159,
-3.34906188726589));
#46845=CARTESIAN_POINT('Ctrl Pts',(6.70282936956514,-0.92971363467198,-3.34675657167541));
#46846=CARTESIAN_POINT('Ctrl Pts',(6.72806635269987,-0.747766005373889,
-3.3381375956296));
#46847=CARTESIAN_POINT('Ctrl Pts',(6.74588142968121,-0.564856441547501,
-3.32951861958377));
#46848=CARTESIAN_POINT('Ctrl Pts',(6.75623197145129,-0.381599984197407,
-3.32089964353796));
#46849=CARTESIAN_POINT('Ctrl Pts',(6.766588713977,-0.198233742399754,-3.31227550407507));
#46850=CARTESIAN_POINT('Ctrl Pts',(6.76947197975218,-0.0145204960127364,
-3.3036513646122));
#46851=CARTESIAN_POINT('Ctrl Pts',(6.76489126357795,0.168923627615384,-3.2950272251493));
#46852=CARTESIAN_POINT('Ctrl Pts',(6.76015364638722,0.358651172519226,-3.28610768728216));
#46853=CARTESIAN_POINT('Ctrl Pts',(6.74743169061268,0.548090474372401,-3.27718814941503));
#46854=CARTESIAN_POINT('Ctrl Pts',(6.72679424816834,0.73656509746889,-3.26826861154789));
#46855=CARTESIAN_POINT('Ctrl Pts',(6.70680310738943,0.919137271018851,-3.25962840636424));
#46856=CARTESIAN_POINT('Ctrl Pts',(6.67938484532721,1.10080397853448,-3.25098820118059));
#46857=CARTESIAN_POINT('Ctrl Pts',(6.64465432640456,1.28095975057503,-3.24234799599694));
#46858=CARTESIAN_POINT('Ctrl Pts',(6.60823958201906,1.46985201570466,-3.23328879178807));
#46859=CARTESIAN_POINT('Ctrl Pts',(6.5637858348098,1.6570827815149,-3.22422958757919));
#46860=CARTESIAN_POINT('Ctrl Pts',(6.51148478162744,1.84197039569973,-3.21517038337031));
#46861=CARTESIAN_POINT('Ctrl Pts',(6.45918372844511,2.02685800988449,-3.20611117916144));
#46862=CARTESIAN_POINT('Ctrl Pts',(6.39903552049933,2.20940211939612,-3.19705197495256));
#46863=CARTESIAN_POINT('Ctrl Pts',(6.33129056347372,2.38894303005924,-3.18799277074368));
#46864=CARTESIAN_POINT('Ctrl Pts',(6.26366301495595,2.56817277910472,-3.17894926700456));
#46865=CARTESIAN_POINT('Ctrl Pts',(6.18840351584211,2.74457514840907,-3.16990576326542));
#46866=CARTESIAN_POINT('Ctrl Pts',(6.10576186767639,2.91752652348337,-3.16086225952629));
#46867=CARTESIAN_POINT('Ctrl Pts',(6.0231958127705,3.09031969795877,-3.15182702798336));
#46868=CARTESIAN_POINT('Ctrl Pts',(5.93326119283621,3.25966796585851,-3.14279179644043));
#46869=CARTESIAN_POINT('Ctrl Pts',(5.836255254385,3.42496913937389,-3.1337565648975));
#46870=CARTESIAN_POINT('Ctrl Pts',(5.73942022348833,3.589979081035,-3.12473725185763));
#46871=CARTESIAN_POINT('Ctrl Pts',(5.63553887235576,3.7509559615117,-3.11571793881776));
#46872=CARTESIAN_POINT('Ctrl Pts',(5.52495344003932,3.90732369856885,-3.10669862577788));
#46873=CARTESIAN_POINT('Ctrl Pts',(5.41450674835925,4.06349525644675,-3.09769062838062));
#46874=CARTESIAN_POINT('Ctrl Pts',(5.29737289792351,4.21506901725398,-3.08868263098338));
#46875=CARTESIAN_POINT('Ctrl Pts',(5.17393772677935,4.3614971511408,-3.07967463358612));
#46876=CARTESIAN_POINT('Ctrl Pts',(5.05078134635042,4.50759456239973,-3.07068698165454));
#46877=CARTESIAN_POINT('Ctrl Pts',(4.92135220708575,4.64856936344266,-3.06169932972296));
#46878=CARTESIAN_POINT('Ctrl Pts',(4.78607643669927,4.78390649386796,-3.05271167779137));
#46879=CARTESIAN_POINT('Ctrl Pts',(4.66826140793107,4.90177496261819,-3.044884108465));
#46880=CARTESIAN_POINT('Ctrl Pts',(4.54601235635552,5.01536756173044,-3.03705653913864));
#46881=CARTESIAN_POINT('Ctrl Pts',(4.4196362004456,5.12436384888025,-3.02922896981227));
#46882=CARTESIAN_POINT('Ctrl Pts',(4.28848975550654,5.23747439151649,-3.02110593519172));
#46883=CARTESIAN_POINT('Ctrl Pts',(4.15295629101846,5.34558325009788,-3.01298290057119));
#46884=CARTESIAN_POINT('Ctrl Pts',(4.01346298745678,5.44833954965313,-3.00485986595064));
#46885=CARTESIAN_POINT('Ctrl Pts',(3.86888714423837,5.55483984948749,-2.99644086267399));
#46886=CARTESIAN_POINT('Ctrl Pts',(3.72005776986405,5.65558990884324,-2.98802185939734));
#46887=CARTESIAN_POINT('Ctrl Pts',(3.56748588484631,5.75024638267112,-2.97960285612069));
#46888=CARTESIAN_POINT('Ctrl Pts',(3.41491399982863,5.84490285649897,-2.97118385284403));
#46889=CARTESIAN_POINT('Ctrl Pts',(3.2585999821917,5.93346552412804,-2.96276484956737));
#46890=CARTESIAN_POINT('Ctrl Pts',(3.09908550384716,6.01564277861015,-2.95434584629072));
#46891=CARTESIAN_POINT('Ctrl Pts',(3.09908550384723,6.01564277861011,-4.95428495819038));
#46892=CARTESIAN_POINT('Ctrl Pts',(2.93974516298852,6.09773032248641,-4.94586184187556));
#46893=CARTESIAN_POINT('Ctrl Pts',(2.77713547189578,6.17348621254161,-4.93743872556074));
#46894=CARTESIAN_POINT('Ctrl Pts',(2.61179029507344,6.24266292975684,-4.92901560924592));
#46895=CARTESIAN_POINT('Ctrl Pts',(2.44642807142854,6.31184677898067,-4.92059162452131));
#46896=CARTESIAN_POINT('Ctrl Pts',(2.27833010742088,6.3744499742426,-4.9121676397967));
#46897=CARTESIAN_POINT('Ctrl Pts',(2.10805000452703,6.43027325845594,-4.9037436550721));
#46898=CARTESIAN_POINT('Ctrl Pts',(1.93772859501676,6.48611008430421,-4.89531762685386));
#46899=CARTESIAN_POINT('Ctrl Pts',(1.76522430811125,6.53516361624418,-4.88689159863562));
#46900=CARTESIAN_POINT('Ctrl Pts',(1.59110600155887,6.57728444662411,-4.87846557041738));
#46901=CARTESIAN_POINT('Ctrl Pts',(1.41402158440019,6.62012280662058,-4.86989600455419));
#46902=CARTESIAN_POINT('Ctrl Pts',(1.23526800822187,6.65579004345812,-4.86132643869098));
#46903=CARTESIAN_POINT('Ctrl Pts',(1.05545426470397,6.68418321824875,-4.85275687282779));
#46904=CARTESIAN_POINT('Ctrl Pts',(0.878421895293671,6.71213720502377,-4.84431986173009));
#46905=CARTESIAN_POINT('Ctrl Pts',(0.700362257308595,6.73304053449834,-4.8358828506324));
#46906=CARTESIAN_POINT('Ctrl Pts',(0.521861552053374,6.74684737640392,-4.8274458395347));
#46907=CARTESIAN_POINT('Ctrl Pts',(0.339154181869231,6.76097959941957,-4.81880999628876));
#46908=CARTESIAN_POINT('Ctrl Pts',(0.155985072554053,6.76767670853061,-4.81017415304279));
#46909=CARTESIAN_POINT('Ctrl Pts',(-0.0270172230871244,6.76694606670222,
-4.80153830979685));
#46910=CARTESIAN_POINT('Ctrl Pts',(-0.210019518728302,6.76621542487383,
-4.7929024665509));
#46911=CARTESIAN_POINT('Ctrl Pts',(-0.392854630975622,6.75805708424938,
-4.78426662330496));
#46912=CARTESIAN_POINT('Ctrl Pts',(-0.574899632783152,6.74253508794918,
-4.77563078005902));
#46913=CARTESIAN_POINT('Ctrl Pts',(-0.748616549970566,6.72772318254615,
-4.7673900041459));
#46914=CARTESIAN_POINT('Ctrl Pts',(-0.922000515700265,6.70617298925634,
-4.75914922823277));
#46915=CARTESIAN_POINT('Ctrl Pts',(-1.09449074839643,6.67790229051568,-4.75090845231965));
#46916=CARTESIAN_POINT('Ctrl Pts',(-1.26678992941556,6.64966290464603,-4.74267680396137));
#46917=CARTESIAN_POINT('Ctrl Pts',(-1.43819700046978,6.61471789211129,-4.7344451556031));
#46918=CARTESIAN_POINT('Ctrl Pts',(-1.60815413919947,6.5731369424785,-4.72621350724482));
#46919=CARTESIAN_POINT('Ctrl Pts',(-1.77795331987167,6.53159463815406,-4.71798950937533));
#46920=CARTESIAN_POINT('Ctrl Pts',(-1.94630490837617,6.48342876343106,-4.70976551150581));
#46921=CARTESIAN_POINT('Ctrl Pts',(-2.11265905095506,6.42876043529526,-4.70154151363632));
#46922=CARTESIAN_POINT('Ctrl Pts',(-2.27886621890777,6.37414040687095,-4.69332478170559));
#46923=CARTESIAN_POINT('Ctrl Pts',(-2.4430791215607,6.31302948597131,-4.68510804977489));
#46924=CARTESIAN_POINT('Ctrl Pts',(-2.60476102407502,6.24559917121325,-4.67689131784416));
#46925=CARTESIAN_POINT('Ctrl Pts',(-2.76636009090852,6.17820340352536,-4.66867879565226));
#46926=CARTESIAN_POINT('Ctrl Pts',(-2.92543041260506,6.10449482673665,-4.66046627346035));
#46927=CARTESIAN_POINT('Ctrl Pts',(-3.08145287446718,6.02469394927559,-4.65225375126845));
#46928=CARTESIAN_POINT('Ctrl Pts',(-3.23742316157219,5.9449197576606,-4.6440439753885));
#46929=CARTESIAN_POINT('Ctrl Pts',(-3.39034730284099,5.85905748574763,-4.63583419950854));
#46930=CARTESIAN_POINT('Ctrl Pts',(-3.53972845950541,5.7673747435872,-4.62762442362858));
#46931=CARTESIAN_POINT('Ctrl Pts',(-3.60497423177531,5.72733012584791,-4.62403860879483));
#46932=CARTESIAN_POINT('Ctrl Pts',(-3.66954441310266,5.68617572491462,-4.62045279396108));
#46933=CARTESIAN_POINT('Ctrl Pts',(-3.73339914491863,5.64393655392412,-4.61686697912732));
#46934=CARTESIAN_POINT('Ctrl Pts',(-3.89115157019759,5.53958513820244,-4.60800826230965));
#46935=CARTESIAN_POINT('Ctrl Pts',(-4.04437207474734,5.4287183903029,-4.599149545492));
#46936=CARTESIAN_POINT('Ctrl Pts',(-4.19255894052685,5.31175475057051,-4.59029082867433));
#46937=CARTESIAN_POINT('Ctrl Pts',(-4.3410230397332,5.19457229096844,-4.58141553864413));
#46938=CARTESIAN_POINT('Ctrl Pts',(-4.4844344771304,5.07127030552435,-4.57254024861391));
#46939=CARTESIAN_POINT('Ctrl Pts',(-4.62232657832742,4.94230573753668,-4.56366495858371));
#46940=CARTESIAN_POINT('Ctrl Pts',(-4.76061032371742,4.81297488153313,-4.55476446075864));
#46941=CARTESIAN_POINT('Ctrl Pts',(-4.89334317243053,4.67794943720698,-4.54586396293358));
#46942=CARTESIAN_POINT('Ctrl Pts',(-5.02009503618959,4.53772352921866,-4.53696346510851));
#46943=CARTESIAN_POINT('Ctrl Pts',(-5.14701848396949,4.3973077973934,-4.52805091867792));
#46944=CARTESIAN_POINT('Ctrl Pts',(-5.26794460461904,4.25167773611181,-4.51913837224735));
#46945=CARTESIAN_POINT('Ctrl Pts',(-5.38248444255352,4.10135955820376,-4.51022582581677));
#46946=CARTESIAN_POINT('Ctrl Pts',(-5.49727719558463,3.9507094631464,-4.50129359961728));
#46947=CARTESIAN_POINT('Ctrl Pts',(-5.60565530267525,3.79535075324253,-4.49236137341778));
#46948=CARTESIAN_POINT('Ctrl Pts',(-5.7072722874395,3.63583993556167,-4.48342914721828));
#46949=CARTESIAN_POINT('Ctrl Pts',(-5.80331212307908,3.48508371357432,-4.47498715754416));
#46950=CARTESIAN_POINT('Ctrl Pts',(-5.89331291743969,3.33061903030178,-4.46654516787004));
#46951=CARTESIAN_POINT('Ctrl Pts',(-5.97702046976212,3.17293480929638,-4.45810317819592));
#46952=CARTESIAN_POINT('Ctrl Pts',(-6.06103424403036,3.01467374226404,-4.44963030573483));
#46953=CARTESIAN_POINT('Ctrl Pts',(-6.13886019197762,2.85288229057625,-4.44115743327376));
#46954=CARTESIAN_POINT('Ctrl Pts',(-6.2101993575957,2.68806862615483,-4.43268456081268));
#46955=CARTESIAN_POINT('Ctrl Pts',(-6.28144175108267,2.52347853274668,-4.42422318186877));
#46956=CARTESIAN_POINT('Ctrl Pts',(-6.34621476874222,2.355874695178,-4.41576180292485));
#46957=CARTESIAN_POINT('Ctrl Pts',(-6.40426491590136,2.18579044900352,-4.40730042398094));
#46958=CARTESIAN_POINT('Ctrl Pts',(-6.46399800312121,2.0107752662924,-4.39859373999837));
#46959=CARTESIAN_POINT('Ctrl Pts',(-6.51661233897661,1.83313396935372,-4.38988705601582));
#46960=CARTESIAN_POINT('Ctrl Pts',(-6.56188355911143,1.65347305894686,-4.38118037203324));
#46961=CARTESIAN_POINT('Ctrl Pts',(-6.60576150047129,1.47934143916692,-4.37274164720787));
#46962=CARTESIAN_POINT('Ctrl Pts',(-6.64274148190805,1.30331301880828,-4.3643029223825));
#46963=CARTESIAN_POINT('Ctrl Pts',(-6.67266859811752,1.1259586047881,-4.35586419755713));
#46964=CARTESIAN_POINT('Ctrl Pts',(-6.70402115093086,0.940156752269966,
-4.34702353399594));
#46965=CARTESIAN_POINT('Ctrl Pts',(-6.72763241147778,0.752899831740139,
-4.33818287043475));
#46966=CARTESIAN_POINT('Ctrl Pts',(-6.74338357278951,0.564860151039709,
-4.32934220687356));
#46967=CARTESIAN_POINT('Ctrl Pts',(-6.75913473410124,0.376820470339342,
-4.32050154331238));
#46968=CARTESIAN_POINT('Ctrl Pts',(-6.76702571198923,0.187998438435085,
-4.31166087975119));
#46969=CARTESIAN_POINT('Ctrl Pts',(-6.76699993702055,-0.000923235581007906,
-4.30282021619));
#46970=CARTESIAN_POINT('',(-6.767,-8.1208758347662E-10,-4.69717978377183));
#46971=CARTESIAN_POINT('Ctrl Pts',(3.09908550384725,6.0156427786101,-5.3486032095739));
#46972=CARTESIAN_POINT('Ctrl Pts',(2.93373232018335,6.10082796552477,-5.33985376167461));
#46973=CARTESIAN_POINT('Ctrl Pts',(2.76486502144435,6.17919158180187,-5.33110431377533));
#46974=CARTESIAN_POINT('Ctrl Pts',(2.59305716434362,6.25046746591375,-5.32235486587604));
#46975=CARTESIAN_POINT('Ctrl Pts',(2.42125069459295,6.3217427744722,-5.31360548862862));
#46976=CARTESIAN_POINT('Ctrl Pts',(2.24650397871072,6.38593035557821,-5.30485611138121));
#46977=CARTESIAN_POINT('Ctrl Pts',(2.06941053323786,6.44281220003534,-5.29610673413379));
#46978=CARTESIAN_POINT('Ctrl Pts',(1.89231845896701,6.4996936040668,-5.2873574246312));
#46979=CARTESIAN_POINT('Ctrl Pts',(1.71287996431525,6.54926929700875,-5.2786081151286));
#46980=CARTESIAN_POINT('Ctrl Pts',(1.53170449173527,6.59137090065473,-5.269858805626));
#46981=CARTESIAN_POINT('Ctrl Pts',(1.35053036178197,6.63347219230078,-5.26110956096141));
#46982=CARTESIAN_POINT('Ctrl Pts',(1.16761955878874,6.66809944062449,-5.25236031629683));
#46983=CARTESIAN_POINT('Ctrl Pts',(0.983593309310811,6.69513503985387,-5.24361107163224));
#46984=CARTESIAN_POINT('Ctrl Pts',(0.799568362460158,6.72217044771213,-5.23486188889906));
#46985=CARTESIAN_POINT('Ctrl Pts',(0.614428268438623,6.74161427235977,-5.22611270616587));
#46986=CARTESIAN_POINT('Ctrl Pts',(0.428801816330147,6.75340047696803,-5.21736352343269));
#46987=CARTESIAN_POINT('Ctrl Pts',(0.243176616522549,6.76518660206243,-5.20861439972455));
#46988=CARTESIAN_POINT('Ctrl Pts',(0.0570653511651141,6.76931519233997,
-5.19986527601641));
#46989=CARTESIAN_POINT('Ctrl Pts',(-0.128899900800489,6.76577222610794,
-5.19111615230827));
#46990=CARTESIAN_POINT('Ctrl Pts',(-0.314863959942398,6.76222928260131,
-5.18236708471901));
#46991=CARTESIAN_POINT('Ctrl Pts',(-0.500681721080975,6.75101488651274,
-5.17361801712975));
#46992=CARTESIAN_POINT('Ctrl Pts',(-0.68572211017351,6.73216712415989,-5.1648689495405));
#46993=CARTESIAN_POINT('Ctrl Pts',(-0.870761373827884,6.71331947644142,
-5.15611993516413));
#46994=CARTESIAN_POINT('Ctrl Pts',(-1.05502298984376,6.68683858439991,-5.14737092078777));
#46995=CARTESIAN_POINT('Ctrl Pts',(-1.23788117676098,6.65281438131419,-5.13862190641141));
#46996=CARTESIAN_POINT('Ctrl Pts',(-1.43009641451832,6.61704912302369,-5.12942519552388));
#46997=CARTESIAN_POINT('Ctrl Pts',(-1.62076048992735,6.57294837083155,-5.12022848463636));
#46998=CARTESIAN_POINT('Ctrl Pts',(-1.80915798961171,6.52067760042038,-5.11103177374883));
#46999=CARTESIAN_POINT('Ctrl Pts',(-1.98840443003051,6.47094578577397,-5.10228177604233));
#47000=CARTESIAN_POINT('Ctrl Pts',(-2.1655989595223,6.41381888474463,-5.09353177833581));
#47001=CARTESIAN_POINT('Ctrl Pts',(-2.3401396624236,6.3494909528522,-5.08478178062931));
#47002=CARTESIAN_POINT('Ctrl Pts',(-2.51467682554049,6.28516432556671,-5.07603196037771));
#47003=CARTESIAN_POINT('Ctrl Pts',(-2.68656000078874,6.21363705879647,-5.06728214012612));
#47004=CARTESIAN_POINT('Ctrl Pts',(-2.85520533840917,6.13515211510846,-5.05853231987452));
#47005=CARTESIAN_POINT('Ctrl Pts',(-3.02384747998354,6.05666865881108,-5.04978266544328));
#47006=CARTESIAN_POINT('Ctrl Pts',(-3.18925164684563,5.9712279103983,-5.04103301101203));
#47007=CARTESIAN_POINT('Ctrl Pts',(-3.35085601829182,5.87912008251894,-5.03228335658078));
#47008=CARTESIAN_POINT('Ctrl Pts',(-3.51245754191444,5.78701387778158,-5.02353385633764));
#47009=CARTESIAN_POINT('Ctrl Pts',(-3.67025915510964,5.68824097060965,-5.0147843560945));
#47010=CARTESIAN_POINT('Ctrl Pts',(-3.82372487928863,5.58313684656835,-5.00603485585136));
#47011=CARTESIAN_POINT('Ctrl Pts',(-3.97718810300823,5.47803443501755,-4.99728549816624));
#47012=CARTESIAN_POINT('Ctrl Pts',(-4.12631534263046,5.3666011749636,-4.98853614048114));
#47013=CARTESIAN_POINT('Ctrl Pts',(-4.27060009886242,5.24921554097337,-4.97978678279602));
#47014=CARTESIAN_POINT('Ctrl Pts',(-4.41488269594247,5.13183166360263,-4.97103755604083));
#47015=CARTESIAN_POINT('Ctrl Pts',(-4.55432273235138,5.00849577139426,-4.96228832928563));
#47016=CARTESIAN_POINT('Ctrl Pts',(-4.68844662480271,4.87962675277281,-4.95353910253044));
#47017=CARTESIAN_POINT('Ctrl Pts',(-4.82256868835227,4.75075949139812,-4.94478999507895));
#47018=CARTESIAN_POINT('Ctrl Pts',(-4.95137454637936,4.61635945312446,-4.93604088762745));
#47019=CARTESIAN_POINT('Ctrl Pts',(-5.07442674461156,4.47688309134502,-4.92729178017596));
#47020=CARTESIAN_POINT('Ctrl Pts',(-5.19747742838615,4.3374084461626,-4.91854278040358));
#47021=CARTESIAN_POINT('Ctrl Pts',(-5.31477440451002,4.19285781735935,-4.9097937806312));
#47022=CARTESIAN_POINT('Ctrl Pts',(-5.42591931531225,4.04372211999309,-4.90104478085883));
#47023=CARTESIAN_POINT('Ctrl Pts',(-5.53707636463048,3.89457013500706,-4.89229482557825));
#47024=CARTESIAN_POINT('Ctrl Pts',(-5.64207983273532,3.74083230916327,-4.88354487029767));
#47025=CARTESIAN_POINT('Ctrl Pts',(-5.74057303468804,3.58303087251736,-4.8747949150171));
#47026=CARTESIAN_POINT('Ctrl Pts',(-5.83906243363822,3.42523552887333,-4.86604529758829));
#47027=CARTESIAN_POINT('Ctrl Pts',(-5.93104191768483,3.26337713156889,-4.85729568015948));
#47028=CARTESIAN_POINT('Ctrl Pts',(-6.01619906699712,3.09800545291046,-4.84854606273067));
#47029=CARTESIAN_POINT('Ctrl Pts',(-6.10135338095431,2.93263928039494,-4.83979673662528));
#47030=CARTESIAN_POINT('Ctrl Pts',(-6.1796856835288,2.76376031540131,-4.83104741051991));
#47031=CARTESIAN_POINT('Ctrl Pts',(-6.25092992694921,2.59194213831458,-4.82229808441453));
#47032=CARTESIAN_POINT('Ctrl Pts',(-6.32217217691145,2.42012876880713,-4.81354900312072));
#47033=CARTESIAN_POINT('Ctrl Pts',(-6.38632665483897,2.24537661647539,-4.80479992182691));
#47034=CARTESIAN_POINT('Ctrl Pts',(-6.443175478694,2.068279176213,-4.79605084053311));
#47035=CARTESIAN_POINT('Ctrl Pts',(-6.50002944235977,1.8911657242328,-4.78730096821815));
#47036=CARTESIAN_POINT('Ctrl Pts',(-6.54957634250432,1.71170683289068,-4.77855109590318));
#47037=CARTESIAN_POINT('Ctrl Pts',(-6.59164787708422,1.53051209225249,-4.76980122358822));
#47038=CARTESIAN_POINT('Ctrl Pts',(-6.63371649075029,1.34932993147929,-4.76105195875344));
#47039=CARTESIAN_POINT('Ctrl Pts',(-6.66831071257138,1.16641244173919,-4.75230269391867));
#47040=CARTESIAN_POINT('Ctrl Pts',(-6.69531304840343,0.982380875159316,
-4.74355342908389));
#47041=CARTESIAN_POINT('Ctrl Pts',(-6.72231677033051,0.798339861795239,
-4.73480371512824));
#47042=CARTESIAN_POINT('Ctrl Pts',(-6.74172778477894,0.61318494072964,-4.72605400117257));
#47043=CARTESIAN_POINT('Ctrl Pts',(-6.75348015835521,0.427545027690135,
-4.71730428721692));
#47044=CARTESIAN_POINT('Ctrl Pts',(-6.76249038365219,0.285219953547058,
-4.71059611941464));
#47045=CARTESIAN_POINT('Ctrl Pts',(-6.76699999999997,0.142609995758198,
-4.70388795161237));
#47046=CARTESIAN_POINT('Ctrl Pts',(-6.767,1.46790887861953E-12,-4.6971797838101));
#47047=CARTESIAN_POINT('Ctrl Pts',(-6.767,-8.12088412195109E-10,-4.69717978377182));
#47048=CARTESIAN_POINT('Ctrl Pts',(-6.76699999997768,-0.186007250372196,
-4.68843027195908));
#47049=CARTESIAN_POINT('Ctrl Pts',(-6.75932637289781,-0.372014356627555,
-4.67968076014633));
#47050=CARTESIAN_POINT('Ctrl Pts',(-6.7440051825667,-0.557389538396189,
-4.67093124833359));
#47051=CARTESIAN_POINT('Ctrl Pts',(-6.72868405694809,-0.742763937190855,
-4.66218177347638));
#47052=CARTESIAN_POINT('Ctrl Pts',(-6.70571545632424,-0.927506131210442,
-4.6534322986192));
#47053=CARTESIAN_POINT('Ctrl Pts',(-6.67517739388229,-1.11098864089732,
-4.644682823762));
#47054=CARTESIAN_POINT('Ctrl Pts',(-6.64463945788839,-1.29447039084364,
-4.63593338513348));
#47055=CARTESIAN_POINT('Ctrl Pts',(-6.60653216984984,-1.47669218418644,
-4.62718394650495));
#47056=CARTESIAN_POINT('Ctrl Pts',(-6.56098496065573,-1.65703510706604,
-4.61843450787644));
#47057=CARTESIAN_POINT('Ctrl Pts',(-6.51543793627481,-1.83737729818289,
-4.60968510474981));
#47058=CARTESIAN_POINT('Ctrl Pts',(-6.46245112132675,-2.01584035622603,
-4.60093570162319));
#47059=CARTESIAN_POINT('Ctrl Pts',(-6.40220448335379,-2.19181813874342,
-4.59218629849656));
#47060=CARTESIAN_POINT('Ctrl Pts',(-6.34195808483518,-2.36779522182518,
-4.58343693014502));
#47061=CARTESIAN_POINT('Ctrl Pts',(-6.27445201385812,-2.54128677801154,
-4.57468756179349));
#47062=CARTESIAN_POINT('Ctrl Pts',(-6.19991555020131,-2.71170355503178,
-4.56593819344195));
#47063=CARTESIAN_POINT('Ctrl Pts',(-6.1253793766047,-2.8821196688716,-4.55718885913876));
#47064=CARTESIAN_POINT('Ctrl Pts',(-6.04381297991678,-3.04946076492552,
-4.54843952483557));
#47065=CARTESIAN_POINT('Ctrl Pts',(-5.95549339270228,-3.21315848496141,
-4.53969019053238));
#47066=CARTESIAN_POINT('Ctrl Pts',(-5.86717414185079,-3.3768555815585,-4.53094088955082));
#47067=CARTESIAN_POINT('Ctrl Pts',(-5.77210188801403,-3.53690907769625,
-4.52219158856927));
#47068=CARTESIAN_POINT('Ctrl Pts',(-5.67059953266826,-3.69277537092395,
-4.51344228758771));
#47069=CARTESIAN_POINT('Ctrl Pts',(-5.56909755546278,-3.84864108348211,
-4.5046930192011));
#47070=CARTESIAN_POINT('Ctrl Pts',(-5.46116568106704,-4.00031938420715,
-4.49594375081448));
#47071=CARTESIAN_POINT('Ctrl Pts',(-5.34717048438338,-4.1472951198268,-4.48719448242787));
#47072=CARTESIAN_POINT('Ctrl Pts',(-5.23317570291497,-4.29427032010314,
-4.47844524590952));
#47073=CARTESIAN_POINT('Ctrl Pts',(-5.11311781898027,-4.43654276311237,
-4.46969600939117));
#47074=CARTESIAN_POINT('Ctrl Pts',(-4.98740458874075,-4.57362924472543,
-4.46094677287282));
#47075=CARTESIAN_POINT('Ctrl Pts',(-4.8616918059593,-4.71071523839898,-4.45219756749611));
#47076=CARTESIAN_POINT('Ctrl Pts',(-4.73032391083184,-4.84261509641523,
-4.4434483621194));
#47077=CARTESIAN_POINT('Ctrl Pts',(-4.5937470688743,-4.96888084654973,-4.4346991567427));
#47078=CARTESIAN_POINT('Ctrl Pts',(-4.45717070170109,-5.09514615774453,
-4.425949981781));
#47079=CARTESIAN_POINT('Ctrl Pts',(-4.3153856343453,-5.21577720572568,-4.4172008068193));
#47080=CARTESIAN_POINT('Ctrl Pts',(-4.16887340887849,-5.33036429343679,
-4.4084516318576));
#47081=CARTESIAN_POINT('Ctrl Pts',(-4.02236168056949,-5.44495099232119,
-4.39970248658434));
#47082=CARTESIAN_POINT('Ctrl Pts',(-3.8711230519634,-5.5534935954452,-4.3909533413111));
#47083=CARTESIAN_POINT('Ctrl Pts',(-3.71567116860927,-5.65562346401932,
-4.38220419603785));
#47084=CARTESIAN_POINT('Ctrl Pts',(-3.56021979984027,-5.75775299451768,
-4.37345507972648));
#47085=CARTESIAN_POINT('Ctrl Pts',(-3.40055544371662,-5.8534696756079,-4.36470596341512));
#47086=CARTESIAN_POINT('Ctrl Pts',(-3.23722035815365,-5.94244843080321,
-4.35595684710376));
#47087=CARTESIAN_POINT('Ctrl Pts',(-3.07388579970981,-6.03142689884403,
-4.34720775902776));
#47088=CARTESIAN_POINT('Ctrl Pts',(-2.90688078715767,-6.11366734742827,
-4.33845867095178));
#47089=CARTESIAN_POINT('Ctrl Pts',(-2.73677250536075,-6.18889047034292,
-4.32970958287579));
#47090=CARTESIAN_POINT('Ctrl Pts',(-2.56666475841723,-6.26411335674151,
-4.32096052230863));
#47091=CARTESIAN_POINT('Ctrl Pts',(-2.39345402381071,-6.3323188457399,-4.31221146174146));
#47092=CARTESIAN_POINT('Ctrl Pts',(-2.21772855867322,-6.39327529831504,
-4.30346240117429));
#47093=CARTESIAN_POINT('Ctrl Pts',(-2.04200363146135,-6.45423156429208,
-4.2947133673895));
#47094=CARTESIAN_POINT('Ctrl Pts',(-1.86376425982952,-6.50793874434814,
-4.28596433360469));
#47095=CARTESIAN_POINT('Ctrl Pts',(-1.6836157754307,-6.55421443963507,-4.27721529981989));
#47096=CARTESIAN_POINT('Ctrl Pts',(-1.50346782754062,-6.60048999710617,
-4.26846629209101));
#47097=CARTESIAN_POINT('Ctrl Pts',(-1.32141105577788,-6.63933404281004,
-4.25971728436212));
#47098=CARTESIAN_POINT('Ctrl Pts',(-1.13806375266581,-6.6706146564517,-4.25096827663324));
#47099=CARTESIAN_POINT('Ctrl Pts',(-0.954716980367006,-6.70189517953209,
-4.24221929423382));
#47100=CARTESIAN_POINT('Ctrl Pts',(-0.770079966636729,-6.72561226618227,
-4.2334703118344));
#47101=CARTESIAN_POINT('Ctrl Pts',(-0.58477976326588,-6.74168537002986,
-4.22472132943498));
#47102=CARTESIAN_POINT('Ctrl Pts',(-0.391489586792104,-6.75845153122487,
-4.21559509901976));
#47103=CARTESIAN_POINT('Ctrl Pts',(-0.197478091011775,-6.76689985148686,
-4.20646886860455));
#47104=CARTESIAN_POINT('Ctrl Pts',(-0.00346214674593483,-6.76699911434455,
-4.19734263818933));
#47105=CARTESIAN_POINT('Ctrl Pts',(0.184490799261612,-6.76709527523794,
-4.18850160247459));
#47106=CARTESIAN_POINT('Ctrl Pts',(0.372447602922716,-6.75935633786509,
-4.17966056675984));
#47107=CARTESIAN_POINT('Ctrl Pts',(0.559756448952297,-6.74380914008221,
-4.17081953104509));
#47108=CARTESIAN_POINT('Ctrl Pts',(0.745136131799664,-6.72842206864779,
-4.16206955243179));
#47109=CARTESIAN_POINT('Ctrl Pts',(0.929880852698716,-6.70538686345272,
-4.15331957381849));
#47110=CARTESIAN_POINT('Ctrl Pts',(1.11336305132482,-6.67478177290799,-4.14456959520518));
#47111=CARTESIAN_POINT('Ctrl Pts',(1.29684337164803,-6.64417699566684,-4.1358197061652));
#47112=CARTESIAN_POINT('Ctrl Pts',(1.47906091279446,-6.60600253531434,-4.12706981712522));
#47113=CARTESIAN_POINT('Ctrl Pts',(1.65939671168969,-6.56038806422558,-4.11831992808523));
#47114=CARTESIAN_POINT('Ctrl Pts',(1.83973072442393,-6.51477404493169,-4.10957012570974));
#47115=CARTESIAN_POINT('Ctrl Pts',(2.0181827542967,-6.46172023265975,-4.10082032333425));
#47116=CARTESIAN_POINT('Ctrl Pts',(2.1941466410528,-6.40140683893445,-4.09207052095876));
#47117=CARTESIAN_POINT('Ctrl Pts',(2.37010884342536,-6.34109402254856,-4.08332080233923));
#47118=CARTESIAN_POINT('Ctrl Pts',(2.54358267918324,-6.27352185671201,-4.07457108371969));
#47119=CARTESIAN_POINT('Ctrl Pts',(2.71397890911422,-6.19891986404754,-4.06582136510015));
#47120=CARTESIAN_POINT('Ctrl Pts',(2.88437356457784,-6.12431856070821,-4.05707172732833));
#47121=CARTESIAN_POINT('Ctrl Pts',(3.05169040855098,-6.04268767548253,-4.0483220895565));
#47122=CARTESIAN_POINT('Ctrl Pts',(3.21536112578986,-5.95430447917801,-4.03957245178468));
#47123=CARTESIAN_POINT('Ctrl Pts',(3.37903038508777,-5.86592207017061,-4.03082289195261));
#47124=CARTESIAN_POINT('Ctrl Pts',(3.53905333044834,-5.770787606636,-4.02207333212056));
#47125=CARTESIAN_POINT('Ctrl Pts',(3.69488643105606,-5.66922422043773,-4.01332377228849));
#47126=CARTESIAN_POINT('Ctrl Pts',(3.85071819531322,-5.56766170519877,-4.00457428748849));
#47127=CARTESIAN_POINT('Ctrl Pts',(4.00235994660596,-5.45967053411261,-3.99582480268849));
#47128=CARTESIAN_POINT('Ctrl Pts',(4.14929663034396,-5.34561750160038,-3.98707531788849));
#47129=CARTESIAN_POINT('Ctrl Pts',(4.29623210283858,-5.23156540926167,-3.97832590521313));
#47130=CARTESIAN_POINT('Ctrl Pts',(4.43846235899581,-5.11145173122288,-3.96957649253777));
#47131=CARTESIAN_POINT('Ctrl Pts',(4.57550431853479,-4.98568442955122,-3.96082707986241));
#47132=CARTESIAN_POINT('Ctrl Pts',(4.7125451939213,-4.8599181228371,-3.95207773640452));
#47133=CARTESIAN_POINT('Ctrl Pts',(4.84439764368142,-4.72849847576639,-3.94332839294662));
#47134=CARTESIAN_POINT('Ctrl Pts',(4.97061384248308,-4.59187184369464,-3.93457904948873));
#47135=CARTESIAN_POINT('Ctrl Pts',(5.09682908470292,-4.45524624710449,-3.92582977234136));
#47136=CARTESIAN_POINT('Ctrl Pts',(5.21740796698661,-4.31341395498239,-3.91708049519402));
#47137=CARTESIAN_POINT('Ctrl Pts',(5.33194095989094,-4.16685668102916,-3.90833121804665));
#47138=CARTESIAN_POINT('Ctrl Pts',(5.44647312280323,-4.02030046913993,-3.89958200430312));
#47139=CARTESIAN_POINT('Ctrl Pts',(5.55495930755774,-3.86901956973112,-3.89083279055957));
#47140=CARTESIAN_POINT('Ctrl Pts',(5.65703106121529,-3.71352777994799,-3.88208357681604));
#47141=CARTESIAN_POINT('Ctrl Pts',(5.75910210908722,-3.55803706532881,-3.87333442356984));
#47142=CARTESIAN_POINT('Ctrl Pts',(5.8547586573674,-3.39833575815103,-3.86458527032366));
#47143=CARTESIAN_POINT('Ctrl Pts',(5.94367583105418,-3.23496624639925,-3.85583611707746));
#47144=CARTESIAN_POINT('Ctrl Pts',(6.03259241944603,-3.07159781002292,-3.84708702142233));
#47145=CARTESIAN_POINT('Ctrl Pts',(6.11476958503622,-2.9045614690709,-3.8383379257672));
#47146=CARTESIAN_POINT('Ctrl Pts',(6.18992823605133,-2.73442451578656,-3.82958883011207));
#47147=CARTESIAN_POINT('Ctrl Pts',(6.26508641729767,-2.56428862591972,-3.82083978914196));
#47148=CARTESIAN_POINT('Ctrl Pts',(6.33322605597181,-2.39105242460069,-3.81209074817183));
#47149=CARTESIAN_POINT('Ctrl Pts',(6.39411573772674,-2.21530425281839,-3.80334170720171));
#47150=CARTESIAN_POINT('Ctrl Pts',(6.4550050591206,-2.03955712115978,-3.79459271801071));
#47151=CARTESIAN_POINT('Ctrl Pts',(6.50864441565861,-1.86129831952377,-3.78584372881972));
#47152=CARTESIAN_POINT('Ctrl Pts',(6.55485164068815,-1.68113323938585,-3.77709473962872));
#47153=CARTESIAN_POINT('Ctrl Pts',(6.60199852655558,-1.49730435840175,-3.76816783275258));
#47154=CARTESIAN_POINT('Ctrl Pts',(6.64140767455104,-1.31149113102048,-3.75924092587644));
#47155=CARTESIAN_POINT('Ctrl Pts',(6.6729397528146,-1.12435050376054,-3.7503140190003));
#47156=CARTESIAN_POINT('Ctrl Pts',(6.70384664841429,-0.940920290856767,
-3.74156410481631));
#47157=CARTESIAN_POINT('Ctrl Pts',(6.7271858589764,-0.756215113568551,-3.73281419063232));
#47158=CARTESIAN_POINT('Ctrl Pts',(6.74287810457884,-0.570862388664146,
-3.72406427644832));
#47159=CARTESIAN_POINT('Ctrl Pts',(6.75857004158188,-0.38551330885554,-3.71531453433774));
#47160=CARTESIAN_POINT('Ctrl Pts',(6.76661529037659,-0.199516992545889,
-3.70656479222716));
#47161=CARTESIAN_POINT('Ctrl Pts',(6.76698652349039,-0.0135052174917819,
-3.69781505011657));
#47162=CARTESIAN_POINT('Ctrl Pts',(6.76735774979706,0.172503146751192,-3.68906546844593));
#47163=CARTESIAN_POINT('Ctrl Pts',(6.76005524143706,0.358526682544987,-3.68031588677528));
#47164=CARTESIAN_POINT('Ctrl Pts',(6.74510380209157,0.543933542824793,-3.67156630510464));
#47165=CARTESIAN_POINT('Ctrl Pts',(6.73015261703303,0.729337249793037,-3.66281687224272));
#47166=CARTESIAN_POINT('Ctrl Pts',(6.70755278434985,0.914124016560562,-3.6540674393808));
#47167=CARTESIAN_POINT('Ctrl Pts',(6.67738106396738,1.09766621819654,-3.64531800651888));
#47168=CARTESIAN_POINT('Ctrl Pts',(6.64720981663772,1.28120554213269,-3.63656871083653));
#47169=CARTESIAN_POINT('Ctrl Pts',(6.60946696566123,1.46350005720166,-3.62781941515418));
#47170=CARTESIAN_POINT('Ctrl Pts',(6.56428069993697,1.64393062275601,-3.61907011947183));
#47171=CARTESIAN_POINT('Ctrl Pts',(6.51909508263546,1.82435859913243,-3.61032094934184));
#47172=CARTESIAN_POINT('Ctrl Pts',(6.46646633394588,2.002922401546,-3.60157177921185));
#47173=CARTESIAN_POINT('Ctrl Pts',(6.40657319574266,2.1790155776386,-3.59282260908186));
#47174=CARTESIAN_POINT('Ctrl Pts',(6.34668083743517,2.35510646074208,-3.58407355287879));
#47175=CARTESIAN_POINT('Ctrl Pts',(6.27952437117281,2.52872651062595,-3.57532449667571));
#47176=CARTESIAN_POINT('Ctrl Pts',(6.20533187306738,2.69928608063207,-3.56657544047263));
#47177=CARTESIAN_POINT('Ctrl Pts',(6.12831449755176,2.87633970177148,-3.55749326418519));
#47178=CARTESIAN_POINT('Ctrl Pts',(6.04371489433665,3.0500949062059,-3.54841108789775));
#47179=CARTESIAN_POINT('Ctrl Pts',(5.95184265090852,3.21991584654418,-3.5393289116103));
#47180=CARTESIAN_POINT('Ctrl Pts',(5.86333281304345,3.38352155959277,-3.53057913125588));
#47181=CARTESIAN_POINT('Ctrl Pts',(5.76807337203062,3.54347560956928,-3.52182935090146));
#47182=CARTESIAN_POINT('Ctrl Pts',(5.66638790052296,3.69923467230818,-3.51307957054704));
#47183=CARTESIAN_POINT('Ctrl Pts',(5.56470608467248,3.85498813541002,-3.50433010475277));
#47184=CARTESIAN_POINT('Ctrl Pts',(5.45659885730059,4.00654667306507,-3.4955806389585));
#47185=CARTESIAN_POINT('Ctrl Pts',(5.3424334054226,4.15339551555407,-3.48683117316423));
#47186=CARTESIAN_POINT('Ctrl Pts',(5.22827145100989,4.30023985932022,-3.47808197541036));
#47187=CARTESIAN_POINT('Ctrl Pts',(5.10805181937171,4.44237457040093,-3.46933277765649));
#47188=CARTESIAN_POINT('Ctrl Pts',(4.98218281240366,4.57931691672346,-3.46058357990262));
#47189=CARTESIAN_POINT('Ctrl Pts',(4.85631699252778,4.71625579556903,-3.45183460368461));
#47190=CARTESIAN_POINT('Ctrl Pts',(4.72480227747168,4.84800236179304,-3.4430856274666));
#47191=CARTESIAN_POINT('Ctrl Pts',(4.58808530802277,4.97410918721188,-3.43433665124859));
#47192=CARTESIAN_POINT('Ctrl Pts',(4.45135945009968,5.10022421130032,-3.42558710622739));
#47193=CARTESIAN_POINT('Ctrl Pts',(4.30943087159923,5.22069856651705,-3.4168375612062));
#47194=CARTESIAN_POINT('Ctrl Pts',(4.16278164273292,5.33512305340054,-3.408088016185));
#47195=CARTESIAN_POINT('Ctrl Pts',(4.01614103484162,5.44954081368443,-3.39933898551774));
#47196=CARTESIAN_POINT('Ctrl Pts',(3.86478055782189,5.55790924103957,-3.39058995485048));
#47197=CARTESIAN_POINT('Ctrl Pts',(3.70921425759791,5.65986029785475,-3.38184092418322));
#47198=CARTESIAN_POINT('Ctrl Pts',(3.55364584477024,5.76181273917401,-3.37309177470338));
#47199=CARTESIAN_POINT('Ctrl Pts',(3.39387173410373,5.85734747849335,-3.36434262522353));
#47200=CARTESIAN_POINT('Ctrl Pts',(3.2304345603762,5.94614005478571,-3.35559347574369));
#47201=CARTESIAN_POINT('Ctrl Pts',(3.18690768769653,5.96978744830722,-3.35326338702042));
#47202=CARTESIAN_POINT('Ctrl Pts',(3.1431211496441,5.99295688508816,-3.35093329829716));
#47203=CARTESIAN_POINT('Ctrl Pts',(3.09908550384726,6.0156427786101,-3.34860320957389));
#47204=CARTESIAN_POINT('Origin',(0.,0.,-63.6971797838103));
#47205=CARTESIAN_POINT('',(3.0990855038472,6.01564277861013,-0.95422544671683));
#47206=CARTESIAN_POINT('',(3.09908550384728,6.01564277861008,-1.34871979865156));
#47207=CARTESIAN_POINT('',(3.09908550384721,6.01564277861012,-63.6971797838103));
#47208=CARTESIAN_POINT('',(-6.76699839382599,-0.00466239815280736,-2.30282021621694));
#47209=CARTESIAN_POINT('Ctrl Pts',(-6.76699839382559,-0.0046623987238019,
-2.30282021619001));
#47210=CARTESIAN_POINT('Ctrl Pts',(-6.76683414407748,-0.243054232521557,
-2.29158517435079));
#47211=CARTESIAN_POINT('Ctrl Pts',(-6.75406843836986,-0.481031945011058,
-2.28035013251158));
#47212=CARTESIAN_POINT('Ctrl Pts',(-6.72885664862788,-0.7174797573565,-2.26911509067237));
#47213=CARTESIAN_POINT('Ctrl Pts',(-6.70364485888591,-0.953927569701941,
-2.25788004883316));
#47214=CARTESIAN_POINT('Ctrl Pts',(-6.66598706078046,-1.18884602160625,
-2.24664500699395));
#47215=CARTESIAN_POINT('Ctrl Pts',(-6.61609060837904,-1.42113829788612,
-2.23540996515474));
#47216=CARTESIAN_POINT('Ctrl Pts',(-6.57956666468819,-1.59117503617786,
-2.22718597295188));
#47217=CARTESIAN_POINT('Ctrl Pts',(-6.53643504805841,-1.760028269909,-2.21896198074902));
#47218=CARTESIAN_POINT('Ctrl Pts',(-6.4867860993046,-1.92714688123885,-2.21073798854616));
#47219=CARTESIAN_POINT('Ctrl Pts',(-6.43718958452491,-2.09408899954798,
-2.20252268165498));
#47220=CARTESIAN_POINT('Ctrl Pts',(-6.38108954510199,-2.25929980253373,
-2.19430737476378));
#47221=CARTESIAN_POINT('Ctrl Pts',(-6.31862738505078,-2.42223800830686,
-2.18609206787259));
#47222=CARTESIAN_POINT('Ctrl Pts',(-6.25621866251127,-2.58503681748739,
-2.17788378932557));
#47223=CARTESIAN_POINT('Ctrl Pts',(-6.18745878708354,-2.74556656867843,
-2.16967551077858));
#47224=CARTESIAN_POINT('Ctrl Pts',(-6.1125390750994,-2.9033007173531,-2.16146723223156));
#47225=CARTESIAN_POINT('Ctrl Pts',(-6.03766843545712,-3.06093155030669,
-2.15326433009937));
#47226=CARTESIAN_POINT('Ctrl Pts',(-5.95664614923389,-3.2157701053826,-2.14506142796716));
#47227=CARTESIAN_POINT('Ctrl Pts',(-5.86971181647224,-3.36730934004676,
-2.13685852583498));
#47228=CARTESIAN_POINT('Ctrl Pts',(-5.78281699718807,-3.5187796969506,-2.12865935209385));
#47229=CARTESIAN_POINT('Ctrl Pts',(-5.69001566293867,-3.66695341065426,
-2.12046017835272));
#47230=CARTESIAN_POINT('Ctrl Pts',(-5.59159360718813,-3.81134752181599,
-2.11226100461159));
#47231=CARTESIAN_POINT('Ctrl Pts',(-5.49318011331474,-3.95572907192489,
-2.10406254412846));
#47232=CARTESIAN_POINT('Ctrl Pts',(-5.38914706663194,-4.09633137351286,
-2.09586408364533));
#47233=CARTESIAN_POINT('Ctrl Pts',(-5.27982409132891,-4.23269967805688,
-2.0876656231622));
#47234=CARTESIAN_POINT('Ctrl Pts',(-5.17050220583707,-4.36906662318216,
-2.0794672444073));
#47235=CARTESIAN_POINT('Ctrl Pts',(-5.05589072029722,-4.50119937480523,
-2.07126886565242));
#47236=CARTESIAN_POINT('Ctrl Pts',(-4.93636004923348,-4.62867567067856,
-2.06307048689752));
#47237=CARTESIAN_POINT('Ctrl Pts',(-4.81680885640397,-4.75617385247173,
-2.0548707005942));
#47238=CARTESIAN_POINT('Ctrl Pts',(-4.69233704080369,-4.87901372411103,
-2.04667091429086));
#47239=CARTESIAN_POINT('Ctrl Pts',(-4.56335245713835,-4.99680931714723,
-2.03847112798753));
#47240=CARTESIAN_POINT('Ctrl Pts',(-4.43432229767364,-5.11464653243132,
-2.03026844434714));
#47241=CARTESIAN_POINT('Ctrl Pts',(-4.30077645846428,-5.227435676881,-2.02206576070675));
#47242=CARTESIAN_POINT('Ctrl Pts',(-4.16315652102638,-5.33483052977651,
-2.01386307706635));
#47243=CARTESIAN_POINT('Ctrl Pts',(-4.02538028656725,-5.44234735261269,
-2.00565107751547));
#47244=CARTESIAN_POINT('Ctrl Pts',(-3.88352099307658,-5.54445742369008,
-1.9974390779646));
#47245=CARTESIAN_POINT('Ctrl Pts',(-3.73805076719158,-5.64085680210892,
-1.98922707841372));
#47246=CARTESIAN_POINT('Ctrl Pts',(-3.5924947433204,-5.73731303664719,-1.98101023544543));
#47247=CARTESIAN_POINT('Ctrl Pts',(-3.44332384770358,-5.82805167849745,
-1.97279339247713));
#47248=CARTESIAN_POINT('Ctrl Pts',(-3.29103543832631,-5.91281445199157,
-1.96457654950884));
#47249=CARTESIAN_POINT('Ctrl Pts',(-3.13851218547216,-5.99770793789197,
-1.95634703537287));
#47250=CARTESIAN_POINT('Ctrl Pts',(-2.98286213142457,-6.07660697774788,
-1.94811752123689));
#47251=CARTESIAN_POINT('Ctrl Pts',(-2.82460447394779,-6.14930065664008,
-1.93988800710091));
#47252=CARTESIAN_POINT('Ctrl Pts',(-2.6835446421044,-6.21409472906666,-1.93255279249783));
#47253=CARTESIAN_POINT('Ctrl Pts',(-2.54041358176544,-6.27395945691981,
-1.92521757789475));
#47254=CARTESIAN_POINT('Ctrl Pts',(-2.39558868938805,-6.32877901583521,
-1.91788236329167));
#47255=CARTESIAN_POINT('Ctrl Pts',(-2.23623556789188,-6.38909784424109,
-1.90981131055579));
#47256=CARTESIAN_POINT('Ctrl Pts',(-2.07431185801297,-6.44350422937888,
-1.9017402578199));
#47257=CARTESIAN_POINT('Ctrl Pts',(-1.91030498556335,-6.49176585083996,
-1.89366920508402));
#47258=CARTESIAN_POINT('Ctrl Pts',(-1.74650219917809,-6.53996741674216,
-1.88560819576501));
#47259=CARTESIAN_POINT('Ctrl Pts',(-1.58062176144763,-6.58203932943863,
-1.87754718644599));
#47260=CARTESIAN_POINT('Ctrl Pts',(-1.41317236866547,-6.61779667687369,
-1.86948617712698));
#47261=CARTESIAN_POINT('Ctrl Pts',(-1.24589462961894,-6.65351736916082,
-1.86143343121424));
#47262=CARTESIAN_POINT('Ctrl Pts',(-1.07705149789421,-6.68293630070154,
-1.85338068530152));
#47263=CARTESIAN_POINT('Ctrl Pts',(-0.907168085471193,-6.70591791365675,
-1.84532793938877));
#47264=CARTESIAN_POINT('Ctrl Pts',(-0.737421626671457,-6.7288809996992,
-1.83728168529718));
#47265=CARTESIAN_POINT('Ctrl Pts',(-0.566636924103956,-6.74541704638878,
-1.82923543120557));
#47266=CARTESIAN_POINT('Ctrl Pts',(-0.395350473852723,-6.7554412885336,
-1.82118917711398));
#47267=CARTESIAN_POINT('Ctrl Pts',(-0.224164644211534,-6.76545964203189,
-1.81314764971848));
#47268=CARTESIAN_POINT('Ctrl Pts',(-0.0524780250569159,-6.76897378436333,
-1.80510612232298));
#47269=CARTESIAN_POINT('Ctrl Pts',(0.119166657993148,-6.76595065808366,
-1.79706459492748));
#47270=CARTESIAN_POINT('Ctrl Pts',(0.294113713877558,-6.76286936810255,
-1.78886835186502));
#47271=CARTESIAN_POINT('Ctrl Pts',(0.469016810825393,-6.75299664798575,
-1.78067210880258));
#47272=CARTESIAN_POINT('Ctrl Pts',(0.64329960582345,-6.73635321350858,-1.77247586574013));
#47273=CARTESIAN_POINT('Ctrl Pts',(0.814238192715004,-6.72002913992128,
-1.76443689547384));
#47274=CARTESIAN_POINT('Ctrl Pts',(0.984579684449283,-6.69719189655806,
-1.75639792520754));
#47275=CARTESIAN_POINT('Ctrl Pts',(1.1537843844718,-6.6679135112979,-1.74835895494125));
#47276=CARTESIAN_POINT('Ctrl Pts',(1.32300718046266,-6.63863199479651,-1.74031912492963));
#47277=CARTESIAN_POINT('Ctrl Pts',(1.49109257463482,-6.60290802834851,-1.73227929491801));
#47278=CARTESIAN_POINT('Ctrl Pts',(1.65751034340853,-6.56086491718079,-1.72423946490639));
#47279=CARTESIAN_POINT('Ctrl Pts',(1.82397885896552,-6.51880898555126,-1.71619718326046));
#47280=CARTESIAN_POINT('Ctrl Pts',(1.98877837504448,-6.47043016506247,-1.7081549016145));
#47281=CARTESIAN_POINT('Ctrl Pts',(2.151393270295,-6.41590180695819,-1.70011261996857));
#47282=CARTESIAN_POINT('Ctrl Pts',(2.31948522096978,-6.35953687146615,-1.69179946509024));
#47283=CARTESIAN_POINT('Ctrl Pts',(2.4852424055632,-6.29660105568209,-1.68348631021192));
#47284=CARTESIAN_POINT('Ctrl Pts',(2.64811820204749,-6.22733963968441,-1.67517315533359));
#47285=CARTESIAN_POINT('Ctrl Pts',(2.80596442074268,-6.16021700481359,-1.66711670930971));
#47286=CARTESIAN_POINT('Ctrl Pts',(2.96110425850402,-6.08715385393473,-1.65906026328583));
#47287=CARTESIAN_POINT('Ctrl Pts',(3.1130661472397,-6.0084197725284,-1.65100381726195));
#47288=CARTESIAN_POINT('Ctrl Pts',(3.27229115713246,-5.9259225424984,-1.64256230795639));
#47289=CARTESIAN_POINT('Ctrl Pts',(3.42802655569584,-5.83719922644851,-1.63412079865084));
#47290=CARTESIAN_POINT('Ctrl Pts',(3.57976554674399,-5.74260982745169,-1.62567928934529));
#47291=CARTESIAN_POINT('Ctrl Pts',(3.73150453779209,-5.6480204284549,-1.61723778003973));
#47292=CARTESIAN_POINT('Ctrl Pts',(3.87924678897198,-5.54756527697109,-1.60879627073416));
#47293=CARTESIAN_POINT('Ctrl Pts',(4.02252722040997,-5.44165083049812,-1.6003547614286));
#47294=CARTESIAN_POINT('Ctrl Pts',(4.16397288302205,-5.33709266500959,-1.5920213493556));
#47295=CARTESIAN_POINT('Ctrl Pts',(4.30152031993196,-5.22688229002238,-1.58368793728259));
#47296=CARTESIAN_POINT('Ctrl Pts',(4.43469586182674,-5.1113365779507,-1.57535452520958));
#47297=CARTESIAN_POINT('Ctrl Pts',(4.56771445692495,-4.99592703599787,-1.56703093402644));
#47298=CARTESIAN_POINT('Ctrl Pts',(4.69637116022414,-4.87519490859631,-1.5587073428433));
#47299=CARTESIAN_POINT('Ctrl Pts',(4.82022238645935,-4.74949946258299,-1.55038375166016));
#47300=CARTESIAN_POINT('Ctrl Pts',(4.94395037254816,-4.6239290918365,-1.54206844299975));
#47301=CARTESIAN_POINT('Ctrl Pts',(5.06288216577888,-4.49340548852718,-1.53375313433935));
#47302=CARTESIAN_POINT('Ctrl Pts',(5.1766081478372,-4.35832732636565,-1.52543782567894));
#47303=CARTESIAN_POINT('Ctrl Pts',(5.2902418118422,-4.223358815075,-1.51712926704252));
#47304=CARTESIAN_POINT('Ctrl Pts',(5.39867786200226,-4.08384337692888,-1.50882070840609));
#47305=CARTESIAN_POINT('Ctrl Pts',(5.50154422585003,-3.9402157467601,-1.50051214976968));
#47306=CARTESIAN_POINT('Ctrl Pts',(5.60434593288425,-3.79667839396242,-1.49220881349076));
#47307=CARTESIAN_POINT('Ctrl Pts',(5.70158472839756,-3.64903428224829,-1.48390547721187));
#47308=CARTESIAN_POINT('Ctrl Pts',(5.7929293278183,-3.49775053468693,-1.47560214093295));
#47309=CARTESIAN_POINT('Ctrl Pts',(5.88423691686185,-3.34652808323496,-1.46730216894277));
#47310=CARTESIAN_POINT('Ctrl Pts',(5.96965488888101,-3.19166923166052,-1.45900219695258));
#47311=CARTESIAN_POINT('Ctrl Pts',(6.04889558886728,-3.03366958566387,-1.45070222496241));
#47312=CARTESIAN_POINT('Ctrl Pts',(6.12811962113046,-2.87570317377984,-1.44240399881288));
#47313=CARTESIAN_POINT('Ctrl Pts',(6.20116881411983,-2.71459759438054,-1.43410577266335));
#47314=CARTESIAN_POINT('Ctrl Pts',(6.26780162997457,-2.55087273835607,-1.42580754651382));
#47315=CARTESIAN_POINT('Ctrl Pts',(6.3344314952917,-2.38715513215795,-1.4175096878143));
#47316=CARTESIAN_POINT('Ctrl Pts',(6.39464541870508,-2.22081880267863,-1.40921182911477));
#47317=CARTESIAN_POINT('Ctrl Pts',(6.44825007422594,-2.0524034642938,-1.40091397041524));
#47318=CARTESIAN_POINT('Ctrl Pts',(6.50186125743187,-1.88396761719982,-1.39261510124735));
#47319=CARTESIAN_POINT('Ctrl Pts',(6.54886146408816,-1.71345258833752,-1.38431623207946));
#47320=CARTESIAN_POINT('Ctrl Pts',(6.58910723279088,-1.5414132718979,-1.37601736291158));
#47321=CARTESIAN_POINT('Ctrl Pts',(6.62938131468486,-1.36925292454671,-1.36771265542881));
#47322=CARTESIAN_POINT('Ctrl Pts',(6.66289138438381,-1.19556648598138,-1.35940794794606));
#47323=CARTESIAN_POINT('Ctrl Pts',(6.68954493557173,-1.02091995522011,-1.3511032404633));
#47324=CARTESIAN_POINT('Ctrl Pts',(6.7162082249102,-0.846209615542786,-1.34279549876978));
#47325=CARTESIAN_POINT('Ctrl Pts',(6.73600995759143,-0.670538829432128,
-1.33448775707625));
#47326=CARTESIAN_POINT('Ctrl Pts',(6.74890950767273,-0.494478975533438,
-1.32618001538273));
#47327=CARTESIAN_POINT('Ctrl Pts',(6.76182279011761,-0.318231695103592,
-1.31786342958776));
#47328=CARTESIAN_POINT('Ctrl Pts',(6.76781919118983,-0.141594866962051,
-1.3095468437928));
#47329=CARTESIAN_POINT('Ctrl Pts',(6.7669102156302,0.034858766468189,-1.30123025799784));
#47330=CARTESIAN_POINT('Ctrl Pts',(6.76623974952352,0.165012079571077,-1.29509589185374));
#47331=CARTESIAN_POINT('Ctrl Pts',(6.76181341237456,0.295065708862492,-1.28896152570965));
#47332=CARTESIAN_POINT('Ctrl Pts',(6.75365390418925,0.424791645903411,-1.28282715956554));
#47333=CARTESIAN_POINT('Ctrl Pts',(6.74241150413655,0.603531693502222,-1.2743750572212));
#47334=CARTESIAN_POINT('Ctrl Pts',(6.72405955500997,0.781976433371651,-1.26592295487685));
#47335=CARTESIAN_POINT('Ctrl Pts',(6.69862491618937,0.959538030620478,-1.25747085253251));
#47336=CARTESIAN_POINT('Ctrl Pts',(6.67321272079666,1.13694294819584,-1.24902620829091));
#47337=CARTESIAN_POINT('Ctrl Pts',(6.64073033942457,1.31346594993434,-1.2405815640493));
#47338=CARTESIAN_POINT('Ctrl Pts',(6.6012565110271,1.48852325330251,-1.2321369198077));
#47339=CARTESIAN_POINT('Ctrl Pts',(6.56181215926768,1.66344983459537,-1.22369858150935));
#47340=CARTESIAN_POINT('Ctrl Pts',(6.51538684054236,1.83691257716809,-1.215260243211));
#47341=CARTESIAN_POINT('Ctrl Pts',(6.46211062418777,2.00833644610648,-1.20682190491265));
#47342=CARTESIAN_POINT('Ctrl Pts',(6.40887262314128,2.17963735180879,-1.19838961947841));
#47343=CARTESIAN_POINT('Ctrl Pts',(6.34879362477254,2.34890198542799,-1.18995733404419));
#47344=CARTESIAN_POINT('Ctrl Pts',(6.28205398723239,2.51556886240423,-1.18152504860995));
#47345=CARTESIAN_POINT('Ctrl Pts',(6.21534311734696,2.68216389878695,-1.17309639785347));
#47346=CARTESIAN_POINT('Ctrl Pts',(6.14197745474585,2.84616310375001,-1.16466774709697));
#47347=CARTESIAN_POINT('Ctrl Pts',(6.06218631264873,3.00702279850593,-1.15623909634049));
#47348=CARTESIAN_POINT('Ctrl Pts',(5.98242004989309,3.16783233627485,-1.14781307368625));
#47349=CARTESIAN_POINT('Ctrl Pts',(5.89623245022907,3.32550401957339,-1.13938705103205));
#47350=CARTESIAN_POINT('Ctrl Pts',(5.80389996755179,3.47951636964857,-1.13096102837782));
#47351=CARTESIAN_POINT('Ctrl Pts',(5.77870504470176,3.52154198366415,-1.12866180512994));
#47352=CARTESIAN_POINT('Ctrl Pts',(5.75305284538321,3.56329526650867,-1.12636258188204));
#47353=CARTESIAN_POINT('Ctrl Pts',(5.7269495768861,3.60476594854702,-1.12406335863416));
#47354=CARTESIAN_POINT('Ctrl Pts',(5.62909068991299,3.76023593448914,-1.11544377032609));
#47355=CARTESIAN_POINT('Ctrl Pts',(5.52493312005685,3.91166182871268,-1.10682418201804));
#47356=CARTESIAN_POINT('Ctrl Pts',(5.41484041301644,4.05854558944013,-1.09820459370997));
#47357=CARTESIAN_POINT('Ctrl Pts',(5.30468141757354,4.20551779099271,-1.0895798154238));
#47358=CARTESIAN_POINT('Ctrl Pts',(5.18858033539406,4.34794215774012,-1.0809550371376));
#47359=CARTESIAN_POINT('Ctrl Pts',(5.06694128655958,4.48535338614004,-1.07233025885143));
#47360=CARTESIAN_POINT('Ctrl Pts',(4.94114952461637,4.62745578415146,-1.06341103375568));
#47361=CARTESIAN_POINT('Ctrl Pts',(4.80943523720456,4.76419644679313,-1.05449180865994));
#47362=CARTESIAN_POINT('Ctrl Pts',(4.67228663297741,4.89510230938033,-1.04557258356419));
#47363=CARTESIAN_POINT('Ctrl Pts',(4.53941781836711,5.02192319017247,-1.03693168727223));
#47364=CARTESIAN_POINT('Ctrl Pts',(4.40144899293313,5.1432677689271,-1.02829079098026));
#47365=CARTESIAN_POINT('Ctrl Pts',(4.25885802004751,5.2587467485207,-1.01964989468829));
#47366=CARTESIAN_POINT('Ctrl Pts',(4.10937762731945,5.37980520595427,-1.01059150519065));
#47367=CARTESIAN_POINT('Ctrl Pts',(3.95481768651747,5.49441698771944,-1.00153311569303));
#47368=CARTESIAN_POINT('Ctrl Pts',(3.79576360793486,5.60218418410867,-0.99247472619539));
#47369=CARTESIAN_POINT('Ctrl Pts',(3.63670952935225,5.7099513804979,-0.983416336697754));
#47370=CARTESIAN_POINT('Ctrl Pts',(3.47316165563625,5.81087381904181,-0.974357947200104));
#47371=CARTESIAN_POINT('Ctrl Pts',(3.30573614850423,5.90460815943552,-0.965299557702465));
#47372=CARTESIAN_POINT('Ctrl Pts',(3.23750883840348,5.94280569587234,-0.961608187373922));
#47373=CARTESIAN_POINT('Ctrl Pts',(3.16861202014468,5.97982472446026,-0.957916817045377));
#47374=CARTESIAN_POINT('Ctrl Pts',(3.0990855038472,6.01564277861013,-0.954225446716826));
#47375=CARTESIAN_POINT('Ctrl Pts',(3.09908550384716,6.01564277861015,-2.95434584629072));
#47376=CARTESIAN_POINT('Ctrl Pts',(2.94505279430701,6.0949959840484,-2.94621616489886));
#47377=CARTESIAN_POINT('Ctrl Pts',(2.78803629944485,6.16839524135199,-2.938086483507));
#47378=CARTESIAN_POINT('Ctrl Pts',(2.6285457489766,6.23562637154737,-2.92995680211514));
#47379=CARTESIAN_POINT('Ctrl Pts',(2.46898819084288,6.30288574793708,-2.92182370515433));
#47380=CARTESIAN_POINT('Ctrl Pts',(2.30695484747266,6.36397170294264,-2.91369060819352));
#47381=CARTESIAN_POINT('Ctrl Pts',(2.14297252482312,6.4187193238101,-2.90555751123271));
#47382=CARTESIAN_POINT('Ctrl Pts',(1.9788142104859,6.47352570178039,-2.89741568554166));
#47383=CARTESIAN_POINT('Ctrl Pts',(1.81270309031937,6.52198005798384,-2.88927385985062));
#47384=CARTESIAN_POINT('Ctrl Pts',(1.64517880988649,6.56396798312579,-2.88113203415956));
#47385=CARTESIAN_POINT('Ctrl Pts',(1.57201917722354,6.58230455601975,-2.87757641239999));
#47386=CARTESIAN_POINT('Ctrl Pts',(1.49859014298685,6.5994085385298,-2.87402079064042));
#47387=CARTESIAN_POINT('Ctrl Pts',(1.42493704901875,6.61527349444706,-2.87046516888085));
#47388=CARTESIAN_POINT('Ctrl Pts',(1.25009215240008,6.65293527384785,-2.86202448722753));
#47389=CARTESIAN_POINT('Ctrl Pts',(1.07362401827726,6.68368879323515,-2.85358380557422));
#47390=CARTESIAN_POINT('Ctrl Pts',(0.896105147946706,6.70740520349139,-2.8451431239209));
#47391=CARTESIAN_POINT('Ctrl Pts',(0.718720460886934,6.73110368694643,-2.83670882242462));
#47392=CARTESIAN_POINT('Ctrl Pts',(0.540286950172614,6.7477756208244,-2.82827452092834));
#47393=CARTESIAN_POINT('Ctrl Pts',(0.361386763349121,6.75734330985751,-2.81984021943207));
#47394=CARTESIAN_POINT('Ctrl Pts',(0.182594330036346,6.7669052361684,-2.81141099800649));
#47395=CARTESIAN_POINT('Ctrl Pts',(0.00333611310928791,6.76937143062896,
-2.80298177658091));
#47396=CARTESIAN_POINT('Ctrl Pts',(-0.175800769736442,6.76471603907807,
-2.79455255515533));
#47397=CARTESIAN_POINT('Ctrl Pts',(-0.354857236466523,6.76006273737323,
-2.78612711768108));
#47398=CARTESIAN_POINT('Ctrl Pts',(-0.533792144965517,6.74829423267054,
-2.77770168020682));
#47399=CARTESIAN_POINT('Ctrl Pts',(-0.712018126993741,6.72943676594352,
-2.76927624273257));
#47400=CARTESIAN_POINT('Ctrl Pts',(-0.890191419189449,6.71058487414307,
-2.76085329611226));
#47401=CARTESIAN_POINT('Ctrl Pts',(-1.06765587165717,6.6846482347562,-2.75243034949195));
#47402=CARTESIAN_POINT('Ctrl Pts',(-1.24382858853427,6.65170500265495,-2.74400740287164));
#47403=CARTESIAN_POINT('Ctrl Pts',(-1.42000422530965,6.61876122455039,-2.73558431664885));
#47404=CARTESIAN_POINT('Ctrl Pts',(-1.59488775484884,6.57881067648143,-2.72716123042605));
#47405=CARTESIAN_POINT('Ctrl Pts',(-1.76790516686299,6.53198287819091,-2.71873814420326));
#47406=CARTESIAN_POINT('Ctrl Pts',(-1.94092856479743,6.48515345978906,-2.71031476656517));
#47407=CARTESIAN_POINT('Ctrl Pts',(-2.11208539450655,6.43144640372495,-2.7018913889271));
#47408=CARTESIAN_POINT('Ctrl Pts',(-2.28081538299629,6.37104153091843,-2.69346801128901));
#47409=CARTESIAN_POINT('Ctrl Pts',(-2.44957474239012,6.31062614340886,-2.68504316738982));
#47410=CARTESIAN_POINT('Ctrl Pts',(-2.61590610436534,6.24351072711649,-2.67661832349062));
#47411=CARTESIAN_POINT('Ctrl Pts',(-2.77926745554553,6.16992393879742,-2.66819347959143));
#47412=CARTESIAN_POINT('Ctrl Pts',(-2.94268003467798,6.09631407463788,-2.65976599377298));
#47413=CARTESIAN_POINT('Ctrl Pts',(-3.10312044219389,6.01622892941827,-2.65133850795452));
#47414=CARTESIAN_POINT('Ctrl Pts',(-3.26006929038381,5.92994411625408,-2.64291102213607));
#47415=CARTESIAN_POINT('Ctrl Pts',(-3.4171588965251,5.84358191944755,-2.63447597821411));
#47416=CARTESIAN_POINT('Ctrl Pts',(-3.57075039389726,5.7510091056195,-2.62604093429216));
#47417=CARTESIAN_POINT('Ctrl Pts',(-3.72035054300453,5.65254640292018,-2.61760589037021));
#47418=CARTESIAN_POINT('Ctrl Pts',(-3.87002300130549,5.55403610829878,-2.60916676937194));
#47419=CARTESIAN_POINT('Ctrl Pts',(-4.01569998984316,5.44963043701574,-2.60072764837366));
#47420=CARTESIAN_POINT('Ctrl Pts',(-4.15691921338945,5.33969209349693,-2.59228852737539));
#47421=CARTESIAN_POINT('Ctrl Pts',(-4.29829538564324,5.22963156632291,-2.58384002727774));
#47422=CARTESIAN_POINT('Ctrl Pts',(-4.43520363545698,5.11402629175641,-2.57539152718009));
#47423=CARTESIAN_POINT('Ctrl Pts',(-4.56721565045773,4.99327850236836,-2.56694302708243));
#47424=CARTESIAN_POINT('Ctrl Pts',(-4.64016307634304,4.92655548161036,-2.56227454039421));
#47425=CARTESIAN_POINT('Ctrl Pts',(-4.71161610343265,4.85826286943379,-2.55760605370602));
#47426=CARTESIAN_POINT('Ctrl Pts',(-4.78150750434896,4.7884731372176,-2.5529375670178));
#47427=CARTESIAN_POINT('Ctrl Pts',(-4.90488130088784,4.66527880844385,-2.54469665441244));
#47428=CARTESIAN_POINT('Ctrl Pts',(-5.02366127589653,4.53714331615842,-2.5364557418071));
#47429=CARTESIAN_POINT('Ctrl Pts',(-5.13742982010061,4.40444137701264,-2.52821482920175));
#47430=CARTESIAN_POINT('Ctrl Pts',(-5.25107233795084,4.27188643756399,-2.51998304541295));
#47431=CARTESIAN_POINT('Ctrl Pts',(-5.35971424928701,4.13477539128512,-2.51175126162414));
#47432=CARTESIAN_POINT('Ctrl Pts',(-5.46297363312294,3.99352076291129,-2.50351947783533));
#47433=CARTESIAN_POINT('Ctrl Pts',(-5.56613703177179,3.85239743836116,-2.49529534593518));
#47434=CARTESIAN_POINT('Ctrl Pts',(-5.66392765853334,3.70713848799727,-2.48707121403503));
#47435=CARTESIAN_POINT('Ctrl Pts',(-5.75600280431726,3.55819065210001,-2.47884708213488));
#47436=CARTESIAN_POINT('Ctrl Pts',(-5.84799657513271,3.40937445460903,-2.47063021862912));
#47437=CARTESIAN_POINT('Ctrl Pts',(-5.9342847463501,3.25687617096491,-2.46241335512337));
#47438=CARTESIAN_POINT('Ctrl Pts',(-6.01456708783003,3.10117264046873,-2.45419649161762));
#47439=CARTESIAN_POINT('Ctrl Pts',(-6.09480828430846,2.94554890861666,-2.44598383928527));
#47440=CARTESIAN_POINT('Ctrl Pts',(-6.16904961859227,2.78672351696052,-2.4377711869529));
#47441=CARTESIAN_POINT('Ctrl Pts',(-6.23703589978149,2.62519945620078,-2.42955853462055));
#47442=CARTESIAN_POINT('Ctrl Pts',(-6.30499942553193,2.4637294585669,-2.42134863111493));
#47443=CARTESIAN_POINT('Ctrl Pts',(-6.36671193103798,2.29956291878483,-2.41313872760933));
#47444=CARTESIAN_POINT('Ctrl Pts',(-6.42196559806087,2.13322452107665,-2.40492882410371));
#47445=CARTESIAN_POINT('Ctrl Pts',(-6.44609322205822,2.06058951723948,-2.40134380476453));
#47446=CARTESIAN_POINT('Ctrl Pts',(-6.46898988947276,1.98754063857672,-2.39775878542533));
#47447=CARTESIAN_POINT('Ctrl Pts',(-6.49064122044032,1.91412265738666,-2.39417376608615));
#47448=CARTESIAN_POINT('Ctrl Pts',(-6.54045949825669,1.7451927477602,-2.38592487415039));
#47449=CARTESIAN_POINT('Ctrl Pts',(-6.58365384022403,1.57440063720012,-2.37767598221462));
#47450=CARTESIAN_POINT('Ctrl Pts',(-6.62010824159231,1.40230377222685,-2.36942709027886));
#47451=CARTESIAN_POINT('Ctrl Pts',(-6.65658155097781,1.2301176447677,-2.36117391984216));
#47452=CARTESIAN_POINT('Ctrl Pts',(-6.68630788869608,1.05662575944793,-2.35292074940546));
#47453=CARTESIAN_POINT('Ctrl Pts',(-6.70922288550451,0.882392924168423,
-2.34466757896875));
#47454=CARTESIAN_POINT('Ctrl Pts',(-6.73216758693566,0.707934231531007,
-2.33640370997878));
#47455=CARTESIAN_POINT('Ctrl Pts',(-6.74828327122341,0.532733019499745,
-2.32813984098882));
#47456=CARTESIAN_POINT('Ctrl Pts',(-6.75755759151857,0.357357520292742,
-2.31987597199884));
#47457=CARTESIAN_POINT('Ctrl Pts',(-6.76393799849216,0.236705329886858,
-2.31419072007154));
#47458=CARTESIAN_POINT('Ctrl Pts',(-6.76708150887763,0.115970675755758,
-2.30850546814425));
#47459=CARTESIAN_POINT('Ctrl Pts',(-6.76699839382599,-0.00466239815271638,
-2.30282021621695));
#47460=CARTESIAN_POINT('',(-6.767,1.61215658878167E-12,-2.69717978381011));
#47461=CARTESIAN_POINT('Ctrl Pts',(3.09908550384726,6.0156427786101,-3.34860320957389));
#47462=CARTESIAN_POINT('Ctrl Pts',(2.93373232018333,6.10082796552478,-3.3398537616746));
#47463=CARTESIAN_POINT('Ctrl Pts',(2.76486502144429,6.17919158180189,-3.33110431377531));
#47464=CARTESIAN_POINT('Ctrl Pts',(2.59305716434354,6.25046746591378,-3.32235486587602));
#47465=CARTESIAN_POINT('Ctrl Pts',(2.42125069459283,6.32174277447225,-3.31360548862861));
#47466=CARTESIAN_POINT('Ctrl Pts',(2.24650397871057,6.38593035557826,-3.30485611138118));
#47467=CARTESIAN_POINT('Ctrl Pts',(2.06941053323768,6.4428122000354,-3.29610673413377));
#47468=CARTESIAN_POINT('Ctrl Pts',(1.89231845896679,6.49969360406686,-3.28735742463117));
#47469=CARTESIAN_POINT('Ctrl Pts',(1.712879964315,6.54926929700882,-3.27860811512858));
#47470=CARTESIAN_POINT('Ctrl Pts',(1.53170449173499,6.5913709006548,-3.26985880562598));
#47471=CARTESIAN_POINT('Ctrl Pts',(1.35053036178164,6.63347219230084,-3.26110956096139));
#47472=CARTESIAN_POINT('Ctrl Pts',(1.16761955878838,6.66809944062455,-3.2523603162968));
#47473=CARTESIAN_POINT('Ctrl Pts',(0.983593309310419,6.69513503985392,-3.24361107163221));
#47474=CARTESIAN_POINT('Ctrl Pts',(0.799568362459921,6.72217044771215,-3.23486188889903));
#47475=CARTESIAN_POINT('Ctrl Pts',(0.614428268438543,6.74161427235978,-3.22611270616587));
#47476=CARTESIAN_POINT('Ctrl Pts',(0.428801816330225,6.75340047696802,-3.2173635234327));
#47477=CARTESIAN_POINT('Ctrl Pts',(0.243176616522786,6.76518660206242,-3.20861439972456));
#47478=CARTESIAN_POINT('Ctrl Pts',(0.0570653511655087,6.76931519233997,
-3.19986527601642));
#47479=CARTESIAN_POINT('Ctrl Pts',(-0.128899900799936,6.76577222610795,
-3.19111615230829));
#47480=CARTESIAN_POINT('Ctrl Pts',(-0.314863959942007,6.76222928260133,
-3.18236708471902));
#47481=CARTESIAN_POINT('Ctrl Pts',(-0.500681721080748,6.75101488651276,
-3.17361801712977));
#47482=CARTESIAN_POINT('Ctrl Pts',(-0.685722110173445,6.73216712415989,
-3.16486894954051));
#47483=CARTESIAN_POINT('Ctrl Pts',(-0.870761373827916,6.71331947644142,
-3.15611993516414));
#47484=CARTESIAN_POINT('Ctrl Pts',(-1.05502298984389,6.6868385843999,-3.14737092078778));
#47485=CARTESIAN_POINT('Ctrl Pts',(-1.23788117676121,6.65281438131415,-3.13862190641141));
#47486=CARTESIAN_POINT('Ctrl Pts',(-1.43009641451851,6.61704912302365,-3.12942519552388));
#47487=CARTESIAN_POINT('Ctrl Pts',(-1.62076048992751,6.57294837083151,-3.12022848463634));
#47488=CARTESIAN_POINT('Ctrl Pts',(-1.80915798961184,6.52067760042035,-3.11103177374881));
#47489=CARTESIAN_POINT('Ctrl Pts',(-1.98840443003061,6.47094578577394,-3.10228177604231));
#47490=CARTESIAN_POINT('Ctrl Pts',(-2.16559895952237,6.4138188847446,-3.09353177833581));
#47491=CARTESIAN_POINT('Ctrl Pts',(-2.34013966242364,6.34949095285219,-3.0847817806293));
#47492=CARTESIAN_POINT('Ctrl Pts',(-2.51467682554056,6.28516432556668,-3.0760319603777));
#47493=CARTESIAN_POINT('Ctrl Pts',(-2.68656000078884,6.21363705879643,-3.0672821401261));
#47494=CARTESIAN_POINT('Ctrl Pts',(-2.8552053384093,6.1351521151084,-3.05853231987451));
#47495=CARTESIAN_POINT('Ctrl Pts',(-3.02384747998358,6.05666865881105,-3.04978266544327));
#47496=CARTESIAN_POINT('Ctrl Pts',(-3.18925164684558,5.97122791039832,-3.04103301101202));
#47497=CARTESIAN_POINT('Ctrl Pts',(-3.3508560182917,5.87912008251901,-3.03228335658078));
#47498=CARTESIAN_POINT('Ctrl Pts',(-3.5124575419143,5.78701387778167,-3.02353385633764));
#47499=CARTESIAN_POINT('Ctrl Pts',(-3.67025915510947,5.68824097060975,-3.01478435609451));
#47500=CARTESIAN_POINT('Ctrl Pts',(-3.82372487928845,5.58313684656848,-3.00603485585137));
#47501=CARTESIAN_POINT('Ctrl Pts',(-3.97718810300807,5.47803443501766,-2.99728549816625));
#47502=CARTESIAN_POINT('Ctrl Pts',(-4.12631534263033,5.3666011749637,-2.98853614048113));
#47503=CARTESIAN_POINT('Ctrl Pts',(-4.27060009886232,5.24921554097345,-2.97978678279601));
#47504=CARTESIAN_POINT('Ctrl Pts',(-4.41488269594215,5.13183166360289,-2.97103755604083));
#47505=CARTESIAN_POINT('Ctrl Pts',(-4.55432273235086,5.00849577139473,-2.96228832928566));
#47506=CARTESIAN_POINT('Ctrl Pts',(-4.688446624802,4.87962675277349,-2.95353910253048));
#47507=CARTESIAN_POINT('Ctrl Pts',(-4.82256868835142,4.75075949139897,-2.944789995079));
#47508=CARTESIAN_POINT('Ctrl Pts',(-4.95137454637838,4.61635945312551,-2.93604088762752));
#47509=CARTESIAN_POINT('Ctrl Pts',(-5.07442674461046,4.47688309134626,-2.92729178017603));
#47510=CARTESIAN_POINT('Ctrl Pts',(-5.19747742838464,4.33740844616438,-2.91854278040369));
#47511=CARTESIAN_POINT('Ctrl Pts',(-5.31477440450814,4.19285781736169,-2.90979378063135));
#47512=CARTESIAN_POINT('Ctrl Pts',(-5.42591931531006,4.04372211999603,-2.901044780859));
#47513=CARTESIAN_POINT('Ctrl Pts',(-5.53707636462847,3.89457013500993,-2.89229482557842));
#47514=CARTESIAN_POINT('Ctrl Pts',(-5.64207983273348,3.74083230916606,-2.88354487029784));
#47515=CARTESIAN_POINT('Ctrl Pts',(-5.74057303468636,3.58303087252006,-2.87479491501725));
#47516=CARTESIAN_POINT('Ctrl Pts',(-5.83906243363663,3.42523552887605,-2.86604529758844));
#47517=CARTESIAN_POINT('Ctrl Pts',(-5.93104191768333,3.26337713157162,-2.85729568015964));
#47518=CARTESIAN_POINT('Ctrl Pts',(-6.01619906699572,3.0980054529132,-2.84854606273083));
#47519=CARTESIAN_POINT('Ctrl Pts',(-6.10135338095293,2.9326392803978,-2.83979673662545));
#47520=CARTESIAN_POINT('Ctrl Pts',(-6.17968568352746,2.7637603154043,-2.83104741052006));
#47521=CARTESIAN_POINT('Ctrl Pts',(-6.25092992694792,2.59194213831769,-2.82229808441468));
#47522=CARTESIAN_POINT('Ctrl Pts',(-6.32217217691024,2.4201287688103,-2.81354900312087));
#47523=CARTESIAN_POINT('Ctrl Pts',(-6.38632665483784,2.24537661647862,-2.80479992182707));
#47524=CARTESIAN_POINT('Ctrl Pts',(-6.44317547869295,2.06827917621629,-2.79605084053326));
#47525=CARTESIAN_POINT('Ctrl Pts',(-6.50002944235886,1.89116572423596,-2.7873009682183));
#47526=CARTESIAN_POINT('Ctrl Pts',(-6.54957634250353,1.71170683289371,-2.77855109590334));
#47527=CARTESIAN_POINT('Ctrl Pts',(-6.59164787708355,1.53051209225538,-2.76980122358837));
#47528=CARTESIAN_POINT('Ctrl Pts',(-6.6337164907497,1.34932993148217,-2.76105195875359));
#47529=CARTESIAN_POINT('Ctrl Pts',(-6.66831071257088,1.16641244174204,-2.7523026939188));
#47530=CARTESIAN_POINT('Ctrl Pts',(-6.69531304840301,0.982380875162153,
-2.74355342908402));
#47531=CARTESIAN_POINT('Ctrl Pts',(-6.72231677033017,0.798339861798054,
-2.73480371512836));
#47532=CARTESIAN_POINT('Ctrl Pts',(-6.74172778477869,0.613184940732429,
-2.72605400117271));
#47533=CARTESIAN_POINT('Ctrl Pts',(-6.75348015835503,0.427545027692894,
-2.71730428721705));
#47534=CARTESIAN_POINT('Ctrl Pts',(-6.76249038365213,0.285219953548949,
-2.71059611941474));
#47535=CARTESIAN_POINT('Ctrl Pts',(-6.76699999999997,0.142609995759217,
-2.70388795161242));
#47536=CARTESIAN_POINT('Ctrl Pts',(-6.767,1.61215615940619E-12,-2.69717978381011));
#47537=CARTESIAN_POINT('Ctrl Pts',(-6.76699995433269,-0.000786168808179289,
-2.69717978381012));
#47538=CARTESIAN_POINT('Ctrl Pts',(-6.76699094693078,-0.0783179758107126,
-2.6935424771142));
#47539=CARTESIAN_POINT('Ctrl Pts',(-6.76564930093462,-0.155845262926331,
-2.6899051704183));
#47540=CARTESIAN_POINT('Ctrl Pts',(-6.76297653321342,-0.23331826161836,
-2.68626786372241));
#47541=CARTESIAN_POINT('Ctrl Pts',(-6.7566431324609,-0.41689857962518,-2.67764888767665));
#47542=CARTESIAN_POINT('Ctrl Pts',(-6.7428328025016,-0.60015403054839,-2.6690299116309));
#47543=CARTESIAN_POINT('Ctrl Pts',(-6.72160900020107,-0.782471372266058,
-2.66041093558513));
#47544=CARTESIAN_POINT('Ctrl Pts',(-6.70037248324128,-0.964897935830279,
-2.65178679612227));
#47545=CARTESIAN_POINT('Ctrl Pts',(-6.67171366577148,-1.14638496649781,
-2.64316265665942));
#47546=CARTESIAN_POINT('Ctrl Pts',(-6.63574754288657,-1.32632708902249,
-2.63453851719656));
#47547=CARTESIAN_POINT('Ctrl Pts',(-6.59854949009672,-1.51243268050393,
-2.62561897932941));
#47548=CARTESIAN_POINT('Ctrl Pts',(-6.55353475948872,-1.69688530660009,
-2.61669944146222));
#47549=CARTESIAN_POINT('Ctrl Pts',(-6.50088716470291,-1.87903035414573,
-2.60777990359508));
#47550=CARTESIAN_POINT('Ctrl Pts',(-6.4498883317872,-2.05547117511759,-2.59913969841149));
#47551=CARTESIAN_POINT('Ctrl Pts',(-6.39172761537296,-2.22974648828572,
-2.5904994932279));
#47552=CARTESIAN_POINT('Ctrl Pts',(-6.32662199237576,-2.40127948510527,
-2.58185928804431));
#47553=CARTESIAN_POINT('Ctrl Pts',(-6.25835913040098,-2.58113082124127,
-2.57280008383537));
#47554=CARTESIAN_POINT('Ctrl Pts',(-6.18246119374536,-2.7579668993438,-2.56374087962646));
#47555=CARTESIAN_POINT('Ctrl Pts',(-6.09923391623129,-2.93114902983351,
-2.55468167541753));
#47556=CARTESIAN_POINT('Ctrl Pts',(-6.01600663871724,-3.10433116032317,
-2.54562247120861));
#47557=CARTESIAN_POINT('Ctrl Pts',(-5.92545022984855,-3.27385902130687,
-2.53656326699969));
#47558=CARTESIAN_POINT('Ctrl Pts',(-5.82792449794053,-3.43912562235005,
-2.52750406279076));
#47559=CARTESIAN_POINT('Ctrl Pts',(-5.73056778747931,-3.60410580052341,
-2.51846055905157));
#47560=CARTESIAN_POINT('Ctrl Pts',(-5.62617692789581,-3.76499189855237,
-2.50941705531238));
#47561=CARTESIAN_POINT('Ctrl Pts',(-5.51510494610675,-3.92121236780525,
-2.50037355157318));
#47562=CARTESIAN_POINT('Ctrl Pts',(-5.40413456312874,-4.07728994040966,
-2.49133832003021));
#47563=CARTESIAN_POINT('Ctrl Pts',(-5.2864953970188,-4.22871021085151,-2.48230308848723));
#47564=CARTESIAN_POINT('Ctrl Pts',(-5.16258354324788,-4.37493087476661,
-2.47326785694426));
#47565=CARTESIAN_POINT('Ctrl Pts',(-5.03889000056429,-4.52089392335956,
-2.46424854390434));
#47566=CARTESIAN_POINT('Ctrl Pts',(-4.90894599217956,-4.66167547700369,
-2.45522923086442));
#47567=CARTESIAN_POINT('Ctrl Pts',(-4.77318746376898,-4.79676666471475,
-2.4462099178245));
#47568=CARTESIAN_POINT('Ctrl Pts',(-4.63759925819609,-4.93168836683468,
-2.4372019204272));
#47569=CARTESIAN_POINT('Ctrl Pts',(-4.49621125898455,-5.06093378285568,
-2.4281939230299));
#47570=CARTESIAN_POINT('Ctrl Pts',(-4.34949752101403,-5.18402935125688,
-2.4191859256326));
#47571=CARTESIAN_POINT('Ctrl Pts',(-4.20311515073677,-5.30684689596981,
-2.41019827370098));
#47572=CARTESIAN_POINT('Ctrl Pts',(-4.05143123417201,-5.42354216612182,
-2.40121062176937));
#47573=CARTESIAN_POINT('Ctrl Pts',(-3.89495390058917,-5.53368079240981,
-2.39222296983774));
#47574=CARTESIAN_POINT('Ctrl Pts',(-3.75867390377791,-5.62960325795577,
-2.38439540051164));
#47575=CARTESIAN_POINT('Ctrl Pts',(-3.61875868543511,-5.72055291907881,
-2.37656783118552));
#47576=CARTESIAN_POINT('Ctrl Pts',(-3.47556556181662,-5.80626670292662,
-2.36874026185942));
#47577=CARTESIAN_POINT('Ctrl Pts',(-3.3269649527174,-5.89521734640807,-2.36061709546545));
#47578=CARTESIAN_POINT('Ctrl Pts',(-3.17489976460162,-5.97848799426903,
-2.35249392907148));
#47579=CARTESIAN_POINT('Ctrl Pts',(-3.01985103637224,-6.05580619885755,
-2.34437076267751));
#47580=CARTESIAN_POINT('Ctrl Pts',(-2.86481323790383,-6.13311895309827,
-2.33624816890524));
#47581=CARTESIAN_POINT('Ctrl Pts',(-2.70679264580833,-6.20447993653089,
-2.32812557513295));
#47582=CARTESIAN_POINT('Ctrl Pts',(-2.5462938792863,-6.26966318715042,-2.32000298136068));
#47583=CARTESIAN_POINT('Ctrl Pts',(-2.38577582527473,-6.33485427098444,
-2.31187941147847));
#47584=CARTESIAN_POINT('Ctrl Pts',(-2.22277934339818,-6.39386600711472,
-2.30375584159626));
#47585=CARTESIAN_POINT('Ctrl Pts',(-2.0578279090229,-6.44652102275688,-2.29563227171405));
#47586=CARTESIAN_POINT('Ctrl Pts',(-1.89275632476716,-6.49921439207484,
-2.28750278466019));
#47587=CARTESIAN_POINT('Ctrl Pts',(-1.72572729299683,-6.54554168174518,
-2.27937329760633));
#47588=CARTESIAN_POINT('Ctrl Pts',(-1.55727890752929,-6.58537557047162,
-2.27124381055247));
#47589=CARTESIAN_POINT('Ctrl Pts',(-1.388761847141,-6.62522569912309,-2.26311100917845));
#47590=CARTESIAN_POINT('Ctrl Pts',(-1.21882463853448,-6.65857707953059,
-2.25497820780443));
#47591=CARTESIAN_POINT('Ctrl Pts',(-1.0480141266985,-6.68535379693853,-2.24684540643041));
#47592=CARTESIAN_POINT('Ctrl Pts',(-0.877017882973423,-6.7121596301793,
-2.23870376180344));
#47593=CARTESIAN_POINT('Ctrl Pts',(-0.705146802449887,-6.73237647888262,
-2.23056211717648));
#47594=CARTESIAN_POINT('Ctrl Pts',(-0.532952142707695,-6.74598035970928,
-2.22242047254951));
#47595=CARTESIAN_POINT('Ctrl Pts',(-0.445222433489368,-6.75291126285662,
-2.21827246867557));
#47596=CARTESIAN_POINT('Ctrl Pts',(-0.357408740641188,-6.7581264770849,
-2.21412446480163));
#47597=CARTESIAN_POINT('Ctrl Pts',(-0.269583759570994,-6.76162802855759,
-2.20997646092768));
#47598=CARTESIAN_POINT('Ctrl Pts',(-0.0908706414179498,-6.76875325846862,
-2.20153577927436));
#47599=CARTESIAN_POINT('Ctrl Pts',(0.0882571890225949,-6.76879421211967,
-2.19309509762102));
#47600=CARTESIAN_POINT('Ctrl Pts',(0.267213616123141,-6.76172210929719,
-2.18465441596769));
#47601=CARTESIAN_POINT('Ctrl Pts',(0.44603477332994,-6.75465535214802,-2.17622011447142));
#47602=CARTESIAN_POINT('Ctrl Pts',(0.624684453502308,-6.74048626963007,
-2.16778581297514));
#47603=CARTESIAN_POINT('Ctrl Pts',(0.802575808428136,-6.71923813179187,
-2.15935151147887));
#47604=CARTESIAN_POINT('Ctrl Pts',(0.980360017473445,-6.69800279193613,
-2.15092229005329));
#47605=CARTESIAN_POINT('Ctrl Pts',(1.15738648162811,-6.66969693671389,-2.14249306862772));
#47606=CARTESIAN_POINT('Ctrl Pts',(1.33307234478328,-6.63439576175359,-2.13406384720214));
#47607=CARTESIAN_POINT('Ctrl Pts',(1.50867934101614,-6.59911043379984,-2.12563840972788));
#47608=CARTESIAN_POINT('Ctrl Pts',(1.68294660984761,-6.5568361130292,-2.11721297225361));
#47609=CARTESIAN_POINT('Ctrl Pts',(1.85529998054192,-6.50769936169467,-2.10878753477935));
#47610=CARTESIAN_POINT('Ctrl Pts',(2.02760239755298,-6.45857713690205,-2.10036458815902));
#47611=CARTESIAN_POINT('Ctrl Pts',(2.19799172449061,-6.40259661869964,-2.09194164153869));
#47612=CARTESIAN_POINT('Ctrl Pts',(2.36590709789767,-6.339934747623,-2.08351869491836));
#47613=CARTESIAN_POINT('Ctrl Pts',(2.53382525434494,-6.27727183798446,-2.07509560869557));
#47614=CARTESIAN_POINT('Ctrl Pts',(2.69926906072849,-6.20792746456873,-2.06667252247277));
#47615=CARTESIAN_POINT('Ctrl Pts',(2.86169521457616,-6.13212764861201,-2.05824943624999));
#47616=CARTESIAN_POINT('Ctrl Pts',(3.02412698791627,-6.05632521019282,-2.04982605861188));
#47617=CARTESIAN_POINT('Ctrl Pts',(3.18354059826417,-5.97406702480634,-2.0414026809738));
#47618=CARTESIAN_POINT('Ctrl Pts',(3.33941490162489,-5.88562631457398,-2.03297930333569));
#47619=CARTESIAN_POINT('Ctrl Pts',(3.49531633809476,-5.79717020942794,-2.0245544594365));
#47620=CARTESIAN_POINT('Ctrl Pts',(3.64767694922484,-5.70252959839476,-2.01612961553731));
#47621=CARTESIAN_POINT('Ctrl Pts',(3.79600195360329,-5.60202268544497,-2.00770477163812));
#47622=CARTESIAN_POINT('Ctrl Pts',(3.94437347073541,-5.50148425486061,-1.99927728581965));
#47623=CARTESIAN_POINT('Ctrl Pts',(4.08870658205265,-5.39507604170789,-1.99084980000117));
#47624=CARTESIAN_POINT('Ctrl Pts',(4.22853684786533,-5.28315863156172,-1.9824223141827));
#47625=CARTESIAN_POINT('Ctrl Pts',(4.36849251900562,-5.17114084944386,-1.97398727026074));
#47626=CARTESIAN_POINT('Ctrl Pts',(4.50393701486435,-5.05360420636309,-1.96555222633878));
#47627=CARTESIAN_POINT('Ctrl Pts',(4.6344393921433,-4.93094925146776,-1.95711718241682));
#47628=CARTESIAN_POINT('Ctrl Pts',(4.76500484771274,-4.80823501133154,-1.94867806141855));
#47629=CARTESIAN_POINT('Ctrl Pts',(4.89062318330465,-4.68039775952832,-1.94023894042027));
#47630=CARTESIAN_POINT('Ctrl Pts',(5.01090113887212,-4.54787409417302,-1.931799819422));
#47631=CARTESIAN_POINT('Ctrl Pts',(5.13131276936844,-4.41520314420971,-1.92335131932434));
#47632=CARTESIAN_POINT('Ctrl Pts',(5.24637194241103,-4.27783562594789,-1.9149028192267));
#47633=CARTESIAN_POINT('Ctrl Pts',(5.35572565503845,-4.13624125359765,-1.90645431912905));
#47634=CARTESIAN_POINT('Ctrl Pts',(5.41615251729663,-4.05799879224021,-1.901785832441));
#47635=CARTESIAN_POINT('Ctrl Pts',(5.47483798966932,-3.97846621218753,-1.89711734575295));
#47636=CARTESIAN_POINT('Ctrl Pts',(5.53172826624605,-3.8977264383759,-1.89244885906491));
#47637=CARTESIAN_POINT('Ctrl Pts',(5.63215219988649,-3.75520286184755,-1.88420794645958));
#47638=CARTESIAN_POINT('Ctrl Pts',(5.72720313160569,-3.60859894912544,-1.87596703385426));
#47639=CARTESIAN_POINT('Ctrl Pts',(5.81653388517389,-3.45835547083061,-1.86772612124894));
#47640=CARTESIAN_POINT('Ctrl Pts',(5.90576568318962,-3.30827842375688,-1.85949433746014));
#47641=CARTESIAN_POINT('Ctrl Pts',(5.9892897399464,-3.15457014208908,-1.85126255367135));
#47642=CARTESIAN_POINT('Ctrl Pts',(6.06680052155676,-2.99770252554163,-1.84303076988255));
#47643=CARTESIAN_POINT('Ctrl Pts',(6.14423925269989,-2.84098072593513,-1.83480663798238));
#47644=CARTESIAN_POINT('Ctrl Pts',(6.21567568402042,-2.68110575721418,-1.82658250608222));
#47645=CARTESIAN_POINT('Ctrl Pts',(6.28084877942527,-2.51857650469311,-1.81835837418205));
#47646=CARTESIAN_POINT('Ctrl Pts',(6.34596427558815,-2.3561908936806,-1.8101415106763));
#47647=CARTESIAN_POINT('Ctrl Pts',(6.40482733670172,-2.19115600330071,-1.80192464717055));
#47648=CARTESIAN_POINT('Ctrl Pts',(6.4572239373238,-2.02399308873637,-1.7937077836648));
#47649=CARTESIAN_POINT('Ctrl Pts',(6.50959368449124,-1.85691584579362,-1.78549513133246));
#47650=CARTESIAN_POINT('Ctrl Pts',(6.55550346537122,-1.68771308940238,-1.77728247900012));
#47651=CARTESIAN_POINT('Ctrl Pts',(6.59478811068874,-1.51692411646675,-1.76906982666778));
#47652=CARTESIAN_POINT('Ctrl Pts',(6.63405960718674,-1.34619230768174,-1.76085992316218));
#47653=CARTESIAN_POINT('Ctrl Pts',(6.66671030593745,-1.17387568633946,-1.75265001965659));
#47654=CARTESIAN_POINT('Ctrl Pts',(6.69262542835401,-1.00052679911601,-1.74444011615099));
#47655=CARTESIAN_POINT('Ctrl Pts',(6.70394178730754,-0.924830524157983,
-1.74085509681171));
#47656=CARTESIAN_POINT('Ctrl Pts',(6.71397445593086,-0.848937562605707,
-1.73727007747243));
#47657=CARTESIAN_POINT('Ctrl Pts',(6.72271694394573,-0.77289448929655,-1.73368505813315));
#47658=CARTESIAN_POINT('Ctrl Pts',(6.74431934565474,-0.584994544336063,
-1.72482659269746));
#47659=CARTESIAN_POINT('Ctrl Pts',(6.75801862979966,-0.396372405831646,
-1.71596812726178));
#47660=CARTESIAN_POINT('Ctrl Pts',(6.7638123466204,-0.207681341736289,-1.70710966182609));
#47661=CARTESIAN_POINT('Ctrl Pts',(6.76961689746334,-0.0186374327851885,
-1.69823463140904));
#47662=CARTESIAN_POINT('Ctrl Pts',(6.76748633003523,0.170475400059,-1.68935960099199));
#47663=CARTESIAN_POINT('Ctrl Pts',(6.75747021679043,0.359005945898372,-1.68048457057494));
#47664=CARTESIAN_POINT('Ctrl Pts',(6.74742566410994,0.548071799416485,-1.67158434067677));
#47665=CARTESIAN_POINT('Ctrl Pts',(6.72945077441733,0.736551796775352,-1.66268411077861));
#47666=CARTESIAN_POINT('Ctrl Pts',(6.70364712284126,0.9237988159887,-1.65378388088044));
#47667=CARTESIAN_POINT('Ctrl Pts',(6.67780854976143,1.11129924691262,-1.64487160581064));
#47668=CARTESIAN_POINT('Ctrl Pts',(6.64412009238467,1.29756311042424,-1.63595933074085));
#47669=CARTESIAN_POINT('Ctrl Pts',(6.60273435444023,1.48195413042873,-1.62704705567105));
#47670=CARTESIAN_POINT('Ctrl Pts',(6.56125723488288,1.66675229428643,-1.61811510188798));
#47671=CARTESIAN_POINT('Ctrl Pts',(6.51204889709496,1.84966908917597,-1.60918314810491));
#47672=CARTESIAN_POINT('Ctrl Pts',(6.4553124662422,2.03008127009192,-1.60025119432184));
#47673=CARTESIAN_POINT('Ctrl Pts',(6.4016799217538,2.20062362134301,-1.59180788194849));
#47674=CARTESIAN_POINT('Ctrl Pts',(6.34132091572155,2.36892787838849,-1.58336456957514));
#47675=CARTESIAN_POINT('Ctrl Pts',(6.27444632298704,2.53448463004896,-1.57492125720179));
#47676=CARTESIAN_POINT('Ctrl Pts',(6.20929631430771,2.69577194959081,-1.56669568375285));
#47677=CARTESIAN_POINT('Ctrl Pts',(6.13783698063295,2.85475945785251,-1.55847011030391));
#47678=CARTESIAN_POINT('Ctrl Pts',(6.06025193000832,3.01091938530916,-1.55024453685496));
#47679=CARTESIAN_POINT('Ctrl Pts',(5.9810512360148,3.17033121180112,-1.54184767276315));
#47680=CARTESIAN_POINT('Ctrl Pts',(5.89546697102152,3.32679603403316,-1.53345080867134));
#47681=CARTESIAN_POINT('Ctrl Pts',(5.80374756332198,3.4797705702006,-1.52505394457953));
#47682=CARTESIAN_POINT('Ctrl Pts',(5.71409531493739,3.6292973874466,-1.51684632784833));
#47683=CARTESIAN_POINT('Ctrl Pts',(5.61858168015793,3.77548921626075,-1.50863871111713));
#47684=CARTESIAN_POINT('Ctrl Pts',(5.51748638254428,3.91786077068067,-1.50043109438593));
#47685=CARTESIAN_POINT('Ctrl Pts',(5.41645265011226,4.06014562343577,-1.49222847594275));
#47686=CARTESIAN_POINT('Ctrl Pts',(5.30984423053164,4.19861454334708,-1.48402585749956));
#47687=CARTESIAN_POINT('Ctrl Pts',(5.19798504347307,4.33280976824858,-1.47582323905637));
#47688=CARTESIAN_POINT('Ctrl Pts',(5.08617365571423,4.46694764928814,-1.46762412572912));
#47689=CARTESIAN_POINT('Ctrl Pts',(4.96911619876696,4.59681519798083,-1.45942501240185));
#47690=CARTESIAN_POINT('Ctrl Pts',(4.84717792625352,4.72198635652843,-1.45122589907459));
#47691=CARTESIAN_POINT('Ctrl Pts',(4.72013759570419,4.85239484132451,-1.44268372403934));
#47692=CARTESIAN_POINT('Ctrl Pts',(4.58779944702644,4.97770512743408,-1.4341415490041));
#47693=CARTESIAN_POINT('Ctrl Pts',(4.4506207720848,5.09747621309676,-1.42559937396885));
#47694=CARTESIAN_POINT('Ctrl Pts',(4.31896857378499,5.21242211651037,-1.41740133500885));
#47695=CARTESIAN_POINT('Ctrl Pts',(4.18285854295231,5.32226616906058,-1.40920329604884));
#47696=CARTESIAN_POINT('Ctrl Pts',(4.04273003568223,5.42665853528603,-1.40100525708883));
#47697=CARTESIAN_POINT('Ctrl Pts',(3.90258913388723,5.53106013513433,-1.39280649300302));
#47698=CARTESIAN_POINT('Ctrl Pts',(3.75842933855136,5.63000887862587,-1.3846077289172));
#47699=CARTESIAN_POINT('Ctrl Pts',(3.61072026394537,5.72319737345606,-1.37640896483138));
#47700=CARTESIAN_POINT('Ctrl Pts',(3.4629419197733,5.81642956991133,-1.36820635585768));
#47701=CARTESIAN_POINT('Ctrl Pts',(3.31161128004421,5.90389593936438,-1.36000374688397));
#47702=CARTESIAN_POINT('Ctrl Pts',(3.15722423136878,5.98533408865853,-1.35180113791027));
#47703=CARTESIAN_POINT('Ctrl Pts',(3.13789221657325,5.99553159888094,-1.35077402482403));
#47704=CARTESIAN_POINT('Ctrl Pts',(3.11851230807468,6.00563464987257,-1.34974691173779));
#47705=CARTESIAN_POINT('Ctrl Pts',(3.09908550384728,6.01564277861008,-1.34871979865154));
#47706=CARTESIAN_POINT('Origin',(0.,0.,-63.6971797838103));
#47707=CARTESIAN_POINT('',(3.09908550384726,6.0156427786101,1.04588102939736));
#47708=CARTESIAN_POINT('',(3.09908550384723,6.01564277861011,0.651473025530853));
#47709=CARTESIAN_POINT('',(3.09908550384721,6.01564277861012,-63.6971797838103));
#47710=CARTESIAN_POINT('',(-6.76699833344662,0.00474922421608585,-0.30282021614616));
#47711=CARTESIAN_POINT('Ctrl Pts',(-6.76699833344662,0.00474922421608134,
-0.302820216146117));
#47712=CARTESIAN_POINT('Ctrl Pts',(-6.76711739371051,-0.164895452611073,
-0.294814773799422));
#47713=CARTESIAN_POINT('Ctrl Pts',(-6.76085299225617,-0.334804302025666,
-0.286809331452755));
#47714=CARTESIAN_POINT('Ctrl Pts',(-6.74817206586946,-0.50444302891323,
-0.278803889106058));
#47715=CARTESIAN_POINT('Ctrl Pts',(-6.73550285360902,-0.673925050414571,
-0.270805841862813));
#47716=CARTESIAN_POINT('Ctrl Pts',(-6.71642893600105,-0.843137071533396,
-0.26280779461959));
#47717=CARTESIAN_POINT('Ctrl Pts',(-6.6909692592208,-1.0115430649074,-0.254809747376342));
#47718=CARTESIAN_POINT('Ctrl Pts',(-6.66553007862698,-1.17981348387234,
-0.246818138921328));
#47719=CARTESIAN_POINT('Ctrl Pts',(-6.63371543035107,-1.34727879468629,
-0.238826530466301));
#47720=CARTESIAN_POINT('Ctrl Pts',(-6.59559619156139,-1.51340671263905,
-0.23083492201129));
#47721=CARTESIAN_POINT('Ctrl Pts',(-6.55749478096564,-1.67945693332309,
-0.222847051195066));
#47722=CARTESIAN_POINT('Ctrl Pts',(-6.51309473124773,-1.84417063787405,
-0.214859180378844));
#47723=CARTESIAN_POINT('Ctrl Pts',(-6.46251825217731,-2.00702437460911,
-0.206871309562622));
#47724=CARTESIAN_POINT('Ctrl Pts',(-6.4119521146099,-2.16984481222097,-0.19888507204693));
#47725=CARTESIAN_POINT('Ctrl Pts',(-6.35521217029182,-2.33080567695449,
-0.190898834531245));
#47726=CARTESIAN_POINT('Ctrl Pts',(-6.29247083559223,-2.48939747393245,
-0.182912597015552));
#47727=CARTESIAN_POINT('Ctrl Pts',(-6.26253342991367,-2.56507050489605,
-0.179101915692029));
#47728=CARTESIAN_POINT('Ctrl Pts',(-6.23123036841646,-2.64020438570276,
-0.175291234368502));
#47729=CARTESIAN_POINT('Ctrl Pts',(-6.1985843025168,-2.71474522646092,-0.171480553044979));
#47730=CARTESIAN_POINT('Ctrl Pts',(-6.12300021659017,-2.88732655158057,
-0.16265784021088));
#47731=CARTESIAN_POINT('Ctrl Pts',(-6.04027740399832,-3.05658346159284,
-0.153835127376766));
#47732=CARTESIAN_POINT('Ctrl Pts',(-5.950739396998,-3.22195431826957,-0.145012414542663));
#47733=CARTESIAN_POINT('Ctrl Pts',(-5.86104116092577,-3.38762110758734,
-0.136173913384289));
#47734=CARTESIAN_POINT('Ctrl Pts',(-5.7645034872635,-3.54938771430167,-0.127335412225904));
#47735=CARTESIAN_POINT('Ctrl Pts',(-5.66149380543021,-3.70672050350109,
-0.118496911067531));
#47736=CARTESIAN_POINT('Ctrl Pts',(-5.55819742015028,-3.86449119185844,
-0.109633810000682));
#47737=CARTESIAN_POINT('Ctrl Pts',(-5.44839312850079,-4.01780314579878,
-0.100770708933852));
#47738=CARTESIAN_POINT('Ctrl Pts',(-5.33249117548759,-4.166152525214,-0.0919076078670003));
#47739=CARTESIAN_POINT('Ctrl Pts',(-5.21643407329633,-4.3147004887228,-0.0830326424371255));
#47740=CARTESIAN_POINT('Ctrl Pts',(-5.09426317499926,-4.45827240387543,
-0.0741576770072431));
#47741=CARTESIAN_POINT('Ctrl Pts',(-4.96642729574578,-4.59639956009824,
-0.0652827115773675));
#47742=CARTESIAN_POINT('Ctrl Pts',(-4.83830328111168,-4.73483804770128,
-0.0563877424399488));
#47743=CARTESIAN_POINT('Ctrl Pts',(-4.7044889277927,-4.86780703436492,-0.0474927733025496));
#47744=CARTESIAN_POINT('Ctrl Pts',(-4.56547008504128,-4.99487456324913,
-0.0385978041651356));
#47745=CARTESIAN_POINT('Ctrl Pts',(-4.43063904179203,-5.11811431365618,
-0.0299707868146038));
#47746=CARTESIAN_POINT('Ctrl Pts',(-4.29091269533491,-5.23580287374704,
-0.021343769464066));
#47747=CARTESIAN_POINT('Ctrl Pts',(-4.14676186211144,-5.34758403944605,
-0.0127167521135334));
#47748=CARTESIAN_POINT('Ctrl Pts',(-4.00982403171967,-5.45377191201807,
-0.00452141246605009));
#47749=CARTESIAN_POINT('Ctrl Pts',(-3.86861282731891,-5.55484528617162,
0.00367392718142589));
#47750=CARTESIAN_POINT('Ctrl Pts',(-3.72354778978322,-5.65044076663056,
0.01186926682891));
#47751=CARTESIAN_POINT('Ctrl Pts',(-3.57863977833541,-5.74593276947304,
0.020055735406248));
#47752=CARTESIAN_POINT('Ctrl Pts',(-3.42988653875487,-5.83595848762258,
0.0282422039835867));
#47753=CARTESIAN_POINT('Ctrl Pts',(-3.27774058002029,-5.92019473413572,
0.0364286725609233));
#47754=CARTESIAN_POINT('Ctrl Pts',(-3.12572818164929,-6.00435703439484,
0.0446079546988116));
#47755=CARTESIAN_POINT('Ctrl Pts',(-2.97032930915141,-6.0827398094413,0.0527872368366991));
#47756=CARTESIAN_POINT('Ctrl Pts',(-2.81202539050201,-6.15506313559593,
0.0609665189745883));
#47757=CARTESIAN_POINT('Ctrl Pts',(-2.65382805791667,-6.22733776643879,
0.0691402939999721));
#47758=CARTESIAN_POINT('Ctrl Pts',(-2.49272990224806,-6.29356092426462,
0.0773140690253551));
#47759=CARTESIAN_POINT('Ctrl Pts',(-2.32923693719625,-6.35349858663718,
0.0854878440507392));
#47760=CARTESIAN_POINT('Ctrl Pts',(-2.16582061799092,-6.41340815010734,
0.0936577871931698));
#47761=CARTESIAN_POINT('Ctrl Pts',(-2.00001206442768,-6.46703796370879,
0.101827730335612));
#47762=CARTESIAN_POINT('Ctrl Pts',(-1.83233730168922,-6.5142021010127,0.109997673478041));
#47763=CARTESIAN_POINT('Ctrl Pts',(-1.66467846498493,-6.56136175858663,
0.118166840625374));
#47764=CARTESIAN_POINT('Ctrl Pts',(-1.49515411740455,-6.60205685664008,
0.126336007772689));
#47765=CARTESIAN_POINT('Ctrl Pts',(-1.32430580213373,-6.63615122962361,
0.134505174920022));
#47766=CARTESIAN_POINT('Ctrl Pts',(-1.15345997221496,-6.67024510663199,
0.142674223229448));
#47767=CARTESIAN_POINT('Ctrl Pts',(-0.981290567314751,-6.69773837790576,
0.150843271538878));
#47768=CARTESIAN_POINT('Ctrl Pts',(-0.808349536187398,-6.71854597568147,
0.159012319848301));
#47769=CARTESIAN_POINT('Ctrl Pts',(-0.635378980098935,-6.73935712578661,
0.167182762799772));
#47770=CARTESIAN_POINT('Ctrl Pts',(-0.461636894350587,-6.75348028543297,
0.175353205751246));
#47771=CARTESIAN_POINT('Ctrl Pts',(-0.287680581486563,-6.76088225626179,
0.183523648702717));
#47772=CARTESIAN_POINT('Ctrl Pts',(-0.113662340719825,-6.76828686216906,
0.191697000306298));
#47773=CARTESIAN_POINT('Ctrl Pts',(0.0605699180535765,-6.76896549814052,
0.199870351909894));
#47774=CARTESIAN_POINT('Ctrl Pts',(0.234458642070341,-6.76293709457352,
0.208043703513475));
#47775=CARTESIAN_POINT('Ctrl Pts',(0.408549242425096,-6.75690169232364,
0.216226543980122));
#47776=CARTESIAN_POINT('Ctrl Pts',(0.582295149546237,-6.74414370742732,
0.224409384446751));
#47777=CARTESIAN_POINT('Ctrl Pts',(0.755142638418673,-6.7247340910732,0.232592224913397));
#47778=CARTESIAN_POINT('Ctrl Pts',(0.928093459013221,-6.70531287125816,
0.240779957247449));
#47779=CARTESIAN_POINT('Ctrl Pts',(1.10014443411077,-6.67923214884072,0.24896768958151));
#47780=CARTESIAN_POINT('Ctrl Pts',(1.27075197801329,-6.64661405607211,0.257155421915563));
#47781=CARTESIAN_POINT('Ctrl Pts',(1.44163107605683,-6.61394404544593,0.26535618657263));
#47782=CARTESIAN_POINT('Ctrl Pts',(1.61106179982824,-6.57471595244428,0.273556951229701));
#47783=CARTESIAN_POINT('Ctrl Pts',(1.77851437334723,-6.52910220656694,0.281757715886769));
#47784=CARTESIAN_POINT('Ctrl Pts',(1.93542277373969,-6.48636067234556,0.289442093841041));
#47785=CARTESIAN_POINT('Ctrl Pts',(2.09059423390549,-6.43801290758808,0.2971264717953));
#47786=CARTESIAN_POINT('Ctrl Pts',(2.24360986589362,-6.38423869930196,0.304810849749572));
#47787=CARTESIAN_POINT('Ctrl Pts',(2.40603247148264,-6.32715860291028,0.312967641793932));
#47788=CARTESIAN_POINT('Ctrl Pts',(2.56654333132276,-6.26378195897024,0.321124433838292));
#47789=CARTESIAN_POINT('Ctrl Pts',(2.72461256508535,-6.19425341507587,0.329281225882653));
#47790=CARTESIAN_POINT('Ctrl Pts',(2.88248672069836,-6.12481067851644,0.337427951376676));
#47791=CARTESIAN_POINT('Ctrl Pts',(3.03792491751405,-6.04923130013865,0.345574676870704));
#47792=CARTESIAN_POINT('Ctrl Pts',(3.19041215785423,-5.96770971671846,0.353721402364727));
#47793=CARTESIAN_POINT('Ctrl Pts',(3.34274326961125,-5.88627160158904,0.361859786592254));
#47794=CARTESIAN_POINT('Ctrl Pts',(3.49212912016178,-5.79890356470488,0.369998170819779));
#47795=CARTESIAN_POINT('Ctrl Pts',(3.63807444548162,-5.70584816912732,0.378136555047305));
#47796=CARTESIAN_POINT('Ctrl Pts',(3.78390100651039,-5.6128684981957,0.386268316593145));
#47797=CARTESIAN_POINT('Ctrl Pts',(3.92629231027381,-5.51421087925476,0.394400078138987));
#47798=CARTESIAN_POINT('Ctrl Pts',(4.06477748702086,-5.41016385897954,0.402531839684826));
#47799=CARTESIAN_POINT('Ctrl Pts',(4.2031790566202,-5.30617965463017,0.4106586918721));
#47800=CARTESIAN_POINT('Ctrl Pts',(4.33767890412596,-5.1968127475801,0.41878554405939));
#47801=CARTESIAN_POINT('Ctrl Pts',(4.46783497657259,-5.08239506749668,0.426912396246664));
#47802=CARTESIAN_POINT('Ctrl Pts',(4.59824569830731,-4.96775353016073,0.435055148553578));
#47803=CARTESIAN_POINT('Ctrl Pts',(4.72429532883956,-4.84804164851499,0.443197900860493));
#47804=CARTESIAN_POINT('Ctrl Pts',(4.84557192025978,-4.72363438102379,0.451340653167406));
#47805=CARTESIAN_POINT('Ctrl Pts',(4.96656198496555,-4.5995210367472,0.459464167499062));
#47806=CARTESIAN_POINT('Ctrl Pts',(5.08280128871719,-4.47073473738736,0.467587681830721));
#47807=CARTESIAN_POINT('Ctrl Pts',(5.19391741158416,-4.33768497261419,0.475711196162379));
#47808=CARTESIAN_POINT('Ctrl Pts',(5.30504043323385,-4.20462694728084,0.48383521485253));
#47809=CARTESIAN_POINT('Ctrl Pts',(5.41103940589524,-4.06730520998406,0.491959233542661));
#47810=CARTESIAN_POINT('Ctrl Pts',(5.51158212918542,-3.92616243082783,0.500083252232812));
#47811=CARTESIAN_POINT('Ctrl Pts',(5.61215021905236,-3.78498404184303,0.50820932058441));
#47812=CARTESIAN_POINT('Ctrl Pts',(5.70725910641704,-3.63998298928229,0.516335388936017));
#47813=CARTESIAN_POINT('Ctrl Pts',(5.79661988945616,-3.49163097379452,0.524461457287615));
#47814=CARTESIAN_POINT('Ctrl Pts',(5.88631440177505,-3.34272491872029,0.532617873481364));
#47815=CARTESIAN_POINT('Ctrl Pts',(5.97021760322336,-3.19044314194321,0.540774289675092));
#47816=CARTESIAN_POINT('Ctrl Pts',(6.04808420343757,-3.03528688399119,0.548930705868841));
#47817=CARTESIAN_POINT('Ctrl Pts',(6.12578114329155,-2.88046868968318,0.55706935037992));
#47818=CARTESIAN_POINT('Ctrl Pts',(6.19746765311683,-2.72278888060113,0.565207994891024));
#47819=CARTESIAN_POINT('Ctrl Pts',(6.26294878048974,-2.56276443961635,0.573346639402104));
#47820=CARTESIAN_POINT('Ctrl Pts',(6.32864438641896,-2.40221585049219,0.581511941437192));
#47821=CARTESIAN_POINT('Ctrl Pts',(6.38809378152727,-2.23930759778346,0.589677243472273));
#47822=CARTESIAN_POINT('Ctrl Pts',(6.44115090277373,-2.0745756307489,0.597842545507362));
#47823=CARTESIAN_POINT('Ctrl Pts',(6.49420802402017,-1.9098436637144,0.606007847542448));
#47824=CARTESIAN_POINT('Ctrl Pts',(6.54087282947605,-1.74328834989732,0.614173149577535));
#47825=CARTESIAN_POINT('Ctrl Pts',(6.58105109452538,-1.5754540587546,0.62233845161262));
#47826=CARTESIAN_POINT('Ctrl Pts',(6.62169554697867,-1.40567239053157,0.630598495442894));
#47827=CARTESIAN_POINT('Ctrl Pts',(6.65581859810969,-1.23409558594309,0.638858539273176));
#47828=CARTESIAN_POINT('Ctrl Pts',(6.68326332567506,-1.06126354864695,0.647118583103449));
#47829=CARTESIAN_POINT('Ctrl Pts',(6.71067819738982,-0.888619527335835,
0.655369641213821));
#47830=CARTESIAN_POINT('Ctrl Pts',(6.73142915937007,-0.714723340715225,
0.663620699324172));
#47831=CARTESIAN_POINT('Ctrl Pts',(6.74540960430284,-0.540128012770085,
0.671871757434545));
#47832=CARTESIAN_POINT('Ctrl Pts',(6.75937757270251,-0.365688498491826,
0.680115452073999));
#47833=CARTESIAN_POINT('Ctrl Pts',(6.76658703108541,-0.190551437647277,
0.688359146713446));
#47834=CARTESIAN_POINT('Ctrl Pts',(6.76698275302029,-0.0152780995526872,
0.696602841352899));
#47835=CARTESIAN_POINT('Ctrl Pts',(6.76737819911042,0.159873061259471,0.704840789583804));
#47836=CARTESIAN_POINT('Ctrl Pts',(6.76096936991359,0.335159956271986,0.713078737814734));
#47837=CARTESIAN_POINT('Ctrl Pts',(6.74775300467988,0.51001802696937,0.72131668604564));
#47838=CARTESIAN_POINT('Ctrl Pts',(6.73454327084701,0.684788361444416,0.729550500830175));
#47839=CARTESIAN_POINT('Ctrl Pts',(6.71453283348665,0.859129946988257,0.7377843156147));
#47840=CARTESIAN_POINT('Ctrl Pts',(6.68777049571708,1.03247992552696,0.746018130399236));
#47841=CARTESIAN_POINT('Ctrl Pts',(6.6610128684915,1.20579939205632,0.754250495917751));
#47842=CARTESIAN_POINT('Ctrl Pts',(6.62750575669221,1.37812724775876,0.762482861436278));
#47843=CARTESIAN_POINT('Ctrl Pts',(6.58734968078777,1.54890709309026,0.770715226954792));
#47844=CARTESIAN_POINT('Ctrl Pts',(6.54719622948158,1.71967577626327,0.778947054406483));
#47845=CARTESIAN_POINT('Ctrl Pts',(6.50039476023779,1.88889630470125,0.78717888185817));
#47846=CARTESIAN_POINT('Ctrl Pts',(6.44709664380496,2.05602379982304,0.795410709309863));
#47847=CARTESIAN_POINT('Ctrl Pts',(6.39379257744239,2.22316995220555,0.803643455720766));
#47848=CARTESIAN_POINT('Ctrl Pts',(6.33399052677082,2.38822226729607,0.811876202131666));
#47849=CARTESIAN_POINT('Ctrl Pts',(6.26789136840603,2.55065222910948,0.820108948542568));
#47850=CARTESIAN_POINT('Ctrl Pts',(6.2017731318378,2.71312907309105,0.828344071171487));
#47851=CARTESIAN_POINT('Ctrl Pts',(6.12935430059118,2.87298172707546,0.836579193800416));
#47852=CARTESIAN_POINT('Ctrl Pts',(6.05088344068903,3.0297027225778,0.844814316429336));
#47853=CARTESIAN_POINT('Ctrl Pts',(5.97233329027532,3.18658207607343,0.853057760199208));
#47854=CARTESIAN_POINT('Ctrl Pts',(5.88771905286392,3.3403231310681,0.861301203969076));
#47855=CARTESIAN_POINT('Ctrl Pts',(5.79733520580429,3.49044316835874,0.869544647738948));
#47856=CARTESIAN_POINT('Ctrl Pts',(5.70690374895223,3.64064228154674,0.877792433752036));
#47857=CARTESIAN_POINT('Ctrl Pts',(5.61069681733334,3.78721627718881,0.886040219765133));
#47858=CARTESIAN_POINT('Ctrl Pts',(5.50905157702439,3.92971242226261,0.894288005778222));
#47859=CARTESIAN_POINT('Ctrl Pts',(5.40726414965501,4.07240789893255,0.902547329256762));
#47860=CARTESIAN_POINT('Ctrl Pts',(5.30002342783129,4.2110138442777,0.910806652735291));
#47861=CARTESIAN_POINT('Ctrl Pts',(5.18770691809457,4.34511057764399,0.91906597621383));
#47862=CARTESIAN_POINT('Ctrl Pts',(5.09342187217554,4.45767921686428,0.925999335301106));
#47863=CARTESIAN_POINT('Ctrl Pts',(4.99556072735516,4.56707079875741,0.932932694388378));
#47864=CARTESIAN_POINT('Ctrl Pts',(4.89436596278416,4.67305797335534,0.939866053475654));
#47865=CARTESIAN_POINT('Ctrl Pts',(4.77535419221126,4.79770593671977,0.948020144692652));
#47866=CARTESIAN_POINT('Ctrl Pts',(4.65139416642594,4.91799660289649,0.956174235909639));
#47867=CARTESIAN_POINT('Ctrl Pts',(4.52283974904205,5.03350867730307,0.964328327126637));
#47868=CARTESIAN_POINT('Ctrl Pts',(4.39446997400465,5.14885484204353,0.972470706645458));
#47869=CARTESIAN_POINT('Ctrl Pts',(4.261519223839,5.25943584696624,0.980613086164297));
#47870=CARTESIAN_POINT('Ctrl Pts',(4.12437998102941,5.36486521471731,0.988755465683113));
#47871=CARTESIAN_POINT('Ctrl Pts',(3.98735447350243,5.47020714550512,0.99689109238766));
#47872=CARTESIAN_POINT('Ctrl Pts',(3.84614767331955,5.57040571944288,1.00502671909223));
#47873=CARTESIAN_POINT('Ctrl Pts',(3.70118757133341,5.6651124933056,1.01316234579679));
#47874=CARTESIAN_POINT('Ctrl Pts',(3.55634029040894,5.75974555779153,1.02129164062085));
#47875=CARTESIAN_POINT('Ctrl Pts',(3.40774583104385,5.84889513669293,1.02942093544488));
#47876=CARTESIAN_POINT('Ctrl Pts',(3.25586358768148,5.93225431841976,1.03755023026893));
#47877=CARTESIAN_POINT('Ctrl Pts',(3.20398124987265,5.9607294655474,1.04032716331174));
#47878=CARTESIAN_POINT('Ctrl Pts',(3.15171552704348,5.98852930994894,1.04310409635457));
#47879=CARTESIAN_POINT('Ctrl Pts',(3.09908550384726,6.0156427786101,1.04588102939738));
#47880=CARTESIAN_POINT('Ctrl Pts',(3.0990855038472,6.01564277861013,-0.954225446716826));
#47881=CARTESIAN_POINT('Ctrl Pts',(2.92900571023975,6.10326297852299,-0.945195402684114));
#47882=CARTESIAN_POINT('Ctrl Pts',(2.75515599357988,6.18369314046508,-0.936165358651385));
#47883=CARTESIAN_POINT('Ctrl Pts',(2.57813708152171,6.2566363318386,-0.927135314618674));
#47884=CARTESIAN_POINT('Ctrl Pts',(2.40129499313276,6.32950666047336,-0.918114290670318));
#47885=CARTESIAN_POINT('Ctrl Pts',(2.22129025081137,6.39490485694901,-0.909093266721976));
#47886=CARTESIAN_POINT('Ctrl Pts',(2.03874463708718,6.45258160000695,-0.900072242773618));
#47887=CARTESIAN_POINT('Ctrl Pts',(1.85652788528628,6.51015443651647,-0.891067470496419));
#47888=CARTESIAN_POINT('Ctrl Pts',(1.67177963047401,6.56003352206036,-0.882062698219208));
#47889=CARTESIAN_POINT('Ctrl Pts',(1.48513782241612,6.60201898273771,-0.873057925942007));
#47890=CARTESIAN_POINT('Ctrl Pts',(1.29873687580939,6.64395026113356,-0.864064774332975));
#47891=CARTESIAN_POINT('Ctrl Pts',(1.1104474857551,6.67800818943961,-0.855071622723939));
#47892=CARTESIAN_POINT('Ctrl Pts',(0.920921277242054,6.70404303395517,-0.846078471114907));
#47893=CARTESIAN_POINT('Ctrl Pts',(0.731796195377596,6.7300227764877,-0.837104353246874));
#47894=CARTESIAN_POINT('Ctrl Pts',(0.541439757278538,6.74801329436519,-0.828130235378856));
#47895=CARTESIAN_POINT('Ctrl Pts',(0.350512111891381,6.75791611811048,-0.819156117510822));
#47896=CARTESIAN_POINT('Ctrl Pts',(0.261011179120108,6.76255825340983,-0.814949330597593));
#47897=CARTESIAN_POINT('Ctrl Pts',(0.171384886256927,6.76542389053578,-0.810742543684355));
#47898=CARTESIAN_POINT('Ctrl Pts',(0.0817019711920329,6.76650676404771,
-0.806535756771126));
#47899=CARTESIAN_POINT('Ctrl Pts',(-0.0917704497586113,6.76860135128945,
-0.798398627087806));
#47900=CARTESIAN_POINT('Ctrl Pts',(-0.265375328847117,6.76402127081696,
-0.790261497404494));
#47901=CARTESIAN_POINT('Ctrl Pts',(-0.438558221892025,6.75277392528514,
-0.782124367721174));
#47902=CARTESIAN_POINT('Ctrl Pts',(-0.61173098952734,6.74152723734704,-0.773987713787909));
#47903=CARTESIAN_POINT('Ctrl Pts',(-0.784481456414752,6.72361408456344,
-0.765851059854628));
#47904=CARTESIAN_POINT('Ctrl Pts',(-0.956258271735937,6.69909390274063,
-0.757714405921362));
#47905=CARTESIAN_POINT('Ctrl Pts',(-1.12805752486441,6.67457051804602,-0.749576689163218));
#47906=CARTESIAN_POINT('Ctrl Pts',(-1.298882512385,6.64343843838427,-0.741438972405071));
#47907=CARTESIAN_POINT('Ctrl Pts',(-1.46819009767355,6.60580856800236,-0.733301255646928));
#47908=CARTESIAN_POINT('Ctrl Pts',(-1.63762256907882,6.56815094075192,-0.725157536276185));
#47909=CARTESIAN_POINT('Ctrl Pts',(-1.80553504645514,6.52398602910561,-0.717013816905453));
#47910=CARTESIAN_POINT('Ctrl Pts',(-1.97139698273959,6.4734753368222,-0.708870097534707));
#47911=CARTESIAN_POINT('Ctrl Pts',(-2.13732761100616,6.42294372545602,-0.700723005429758));
#47912=CARTESIAN_POINT('Ctrl Pts',(-2.30120566108843,6.36606121397866,-0.692575913324796));
#47913=CARTESIAN_POINT('Ctrl Pts',(-2.46251891230449,6.30303812510624,-0.684428821219846));
#47914=CARTESIAN_POINT('Ctrl Pts',(-2.62400769448509,6.23994645846047,-0.676272863960146));
#47915=CARTESIAN_POINT('Ctrl Pts',(-2.78292576961112,6.17070101395603,-0.668116906700458));
#47916=CARTESIAN_POINT('Ctrl Pts',(-2.93878324221061,6.09555920775954,-0.659960949440759));
#47917=CARTESIAN_POINT('Ctrl Pts',(-3.01642570140689,6.05812632421383,-0.655897951573662));
#47918=CARTESIAN_POINT('Ctrl Pts',(-3.09330902488021,6.01923086615666,-0.651834953706578));
#47919=CARTESIAN_POINT('Ctrl Pts',(-3.16937523825415,5.97890872978853,-0.647771955839481));
#47920=CARTESIAN_POINT('Ctrl Pts',(-3.32713024121956,5.89528397103979,-0.639345636030166));
#47921=CARTESIAN_POINT('Ctrl Pts',(-3.48169452813347,5.80534763426989,-0.630919316220838));
#47922=CARTESIAN_POINT('Ctrl Pts',(-3.63254823534196,5.70936794381953,-0.622492996411523));
#47923=CARTESIAN_POINT('Ctrl Pts',(-3.78328574887108,5.61346218084225,-0.614073166897478));
#47924=CARTESIAN_POINT('Ctrl Pts',(-3.93031809795312,5.51152252199718,-0.605653337383427));
#47925=CARTESIAN_POINT('Ctrl Pts',(-4.07315087405494,5.40386259606825,-0.597233507869383));
#47926=CARTESIAN_POINT('Ctrl Pts',(-4.2158961409155,5.29626863005895,-0.588818836925468));
#47927=CARTESIAN_POINT('Ctrl Pts',(-4.35444669709763,5.18296158477958,-0.580404165981556));
#47928=CARTESIAN_POINT('Ctrl Pts',(-4.4883376319278,5.06429800681405,-0.571989495037641));
#47929=CARTESIAN_POINT('Ctrl Pts',(-4.62216761181995,4.94568845140838,-0.563578654941174));
#47930=CARTESIAN_POINT('Ctrl Pts',(-4.75134194942648,4.82172744728789,-0.555167814844717));
#47931=CARTESIAN_POINT('Ctrl Pts',(-4.87542902751879,4.69281160900661,-0.546756974748249));
#47932=CARTESIAN_POINT('Ctrl Pts',(-4.99947913152118,4.5639341836356,-0.538348640820536));
#47933=CARTESIAN_POINT('Ctrl Pts',(-5.11844476660789,4.43010510941468,-0.529940306892819));
#47934=CARTESIAN_POINT('Ctrl Pts',(-5.23193112488908,4.29175788045143,-0.521531972965107));
#47935=CARTESIAN_POINT('Ctrl Pts',(-5.34542017002875,4.15340737603347,-0.51312343996498));
#47936=CARTESIAN_POINT('Ctrl Pts',(-5.45342946142394,4.01053875793179,-0.504714906964856));
#47937=CARTESIAN_POINT('Ctrl Pts',(-5.55560403496423,3.86361913323366,-0.496306373964728));
#47938=CARTESIAN_POINT('Ctrl Pts',(-5.65778282591142,3.71669344421036,-0.487897493889944));
#47939=CARTESIAN_POINT('Ctrl Pts',(-5.75412622721796,3.56571669032804,-0.479488613815146));
#47940=CARTESIAN_POINT('Ctrl Pts',(-5.84432216496291,3.41118563436868,-0.47107973374036));
#47941=CARTESIAN_POINT('Ctrl Pts',(-5.9345347280865,3.25662609445114,-0.462669303697597));
#47942=CARTESIAN_POINT('Ctrl Pts',(-6.01859739958445,3.09851123585628,-0.454258873654861));
#47943=CARTESIAN_POINT('Ctrl Pts',(-6.09624352368068,2.93736342660922,-0.4458484436121));
#47944=CARTESIAN_POINT('Ctrl Pts',(-6.17391507030227,2.77616285511141,-0.437435259866257));
#47945=CARTESIAN_POINT('Ctrl Pts',(-6.24516573563743,2.61192765508278,-0.42902207612041));
#47946=CARTESIAN_POINT('Ctrl Pts',(-6.30977642014614,2.44520153111513,-0.420608892374567));
#47947=CARTESIAN_POINT('Ctrl Pts',(-6.3744472030143,2.27832032495629,-0.412187883010642));
#47948=CARTESIAN_POINT('Ctrl Pts',(-6.43246554287891,2.10894387818012,-0.403766873646707));
#47949=CARTESIAN_POINT('Ctrl Pts',(-6.48366140323119,1.93763355881604,-0.395345864282781));
#47950=CARTESIAN_POINT('Ctrl Pts',(-6.53488294260128,1.76623731295888,-0.386920631076383));
#47951=CARTESIAN_POINT('Ctrl Pts',(-6.57927509001139,1.59290558337106,-0.378495397869984));
#47952=CARTESIAN_POINT('Ctrl Pts',(-6.61671853072273,1.4182118618847,-0.370070164663588));
#47953=CARTESIAN_POINT('Ctrl Pts',(-6.65420523124043,1.2433163102134,-0.361635197470407));
#47954=CARTESIAN_POINT('Ctrl Pts',(-6.68472712177001,1.06705595191768,-0.353200230277231));
#47955=CARTESIAN_POINT('Ctrl Pts',(-6.70821634980292,0.890012586560914,
-0.344765263084049));
#47956=CARTESIAN_POINT('Ctrl Pts',(-6.72169535679295,0.788418410888559,
-0.339924960048193));
#47957=CARTESIAN_POINT('Ctrl Pts',(-6.73285953853334,0.686566488305788,
-0.335084657012332));
#47958=CARTESIAN_POINT('Ctrl Pts',(-6.74170381834428,0.5845670412555,-0.330244353976475));
#47959=CARTESIAN_POINT('Ctrl Pts',(-6.75840709403868,0.391931244878789,
-0.321102974714318));
#47960=CARTESIAN_POINT('Ctrl Pts',(-6.76686237902982,0.198465732430607,
-0.311961595452164));
#47961=CARTESIAN_POINT('Ctrl Pts',(-6.76699833344597,0.00474922514552044,
-0.302820216190007));
#47962=CARTESIAN_POINT('',(-6.76699942930229,-0.00277917658345995,-0.697179783782191));
#47963=CARTESIAN_POINT('Ctrl Pts',(3.09908550384728,6.01564277861008,-1.34871979865154));
#47964=CARTESIAN_POINT('Ctrl Pts',(2.94374847892273,6.09566792968225,-1.34050698664135));
#47965=CARTESIAN_POINT('Ctrl Pts',(2.78541162564976,6.16962008736427,-1.33229417463114));
#47966=CARTESIAN_POINT('Ctrl Pts',(2.62459578153322,6.23728995506526,-1.32408136262094));
#47967=CARTESIAN_POINT('Ctrl Pts',(2.46368013222434,6.30500181989781,-1.31586345359256));
#47968=CARTESIAN_POINT('Ctrl Pts',(2.30028276042722,6.36642349734732,-1.30764554456416));
#47969=CARTESIAN_POINT('Ctrl Pts',(2.1349406106516,6.42139529923136,-1.29942763553576));
#47970=CARTESIAN_POINT('Ctrl Pts',(1.96935243679418,6.47644889748191,-1.29119749850909));
#47971=CARTESIAN_POINT('Ctrl Pts',(1.80181404729578,6.52503334608869,-1.28296736148243));
#47972=CARTESIAN_POINT('Ctrl Pts',(1.63287470142026,6.5670396077275,-1.27473722445576));
#47973=CARTESIAN_POINT('Ctrl Pts',(1.51420469579376,6.5965465486902,-1.26895603475006));
#47974=CARTESIAN_POINT('Ctrl Pts',(1.39484363862823,6.62280872975009,-1.26317484504439));
#47975=CARTESIAN_POINT('Ctrl Pts',(1.27498338669229,6.64580366574718,-1.2573936553387));
#47976=CARTESIAN_POINT('Ctrl Pts',(1.10764786172967,6.67790663253063,-1.24932260260283));
#47977=CARTESIAN_POINT('Ctrl Pts',(0.938793560500144,6.70374396058503,-1.24125154986695));
#47978=CARTESIAN_POINT('Ctrl Pts',(0.768940524153764,6.72317034369308,-1.23318049713107));
#47979=CARTESIAN_POINT('Ctrl Pts',(0.599298848692328,6.74257255309419,-1.22511948781206));
#47980=CARTESIAN_POINT('Ctrl Pts',(0.428661276890571,6.75557964920356,-1.21705847849305));
#47981=CARTESIAN_POINT('Ctrl Pts',(0.257560676775405,6.76209667912098,-1.20899746917404));
#47982=CARTESIAN_POINT('Ctrl Pts',(0.0866354732782866,6.76860702837798,
-1.20094472326129));
#47983=CARTESIAN_POINT('Ctrl Pts',(-0.0847514443693596,6.76864053714096,
-1.19289197734856));
#47984=CARTESIAN_POINT('Ctrl Pts',(-0.256059497801806,6.76215369047358,
-1.18483923143582));
#47985=CARTESIAN_POINT('Ctrl Pts',(-0.427229449118924,6.75567207325823,
-1.17679297734423));
#47986=CARTESIAN_POINT('Ctrl Pts',(-0.598320291927199,6.74268057687285,
-1.16874672325262));
#47987=CARTESIAN_POINT('Ctrl Pts',(-0.768788941225106,6.72318767876147,
-1.16070046916104));
#47988=CARTESIAN_POINT('Ctrl Pts',(-0.9391574503223,6.70370623156928,-1.15265894176555));
#47989=CARTESIAN_POINT('Ctrl Pts',(-1.10890412388516,6.67773102786735,-1.14461741437007));
#47990=CARTESIAN_POINT('Ctrl Pts',(-1.27748860541604,6.64532255522877,-1.13657588697458));
#47991=CARTESIAN_POINT('Ctrl Pts',(-1.44931658276778,6.61229055695717,-1.12837964391212));
#47992=CARTESIAN_POINT('Ctrl Pts',(-1.61993679679775,6.57257523889413,-1.12018340084964));
#47993=CARTESIAN_POINT('Ctrl Pts',(-1.78878499137808,6.52629582953612,-1.11198715778718));
#47994=CARTESIAN_POINT('Ctrl Pts',(-1.95439325914239,6.48090444802929,-1.10394818752089));
#47995=CARTESIAN_POINT('Ctrl Pts',(-2.1182965290554,6.4291987268512,-1.0959092172546));
#47996=CARTESIAN_POINT('Ctrl Pts',(-2.27997544670536,6.37134216334523,-1.0878702469883));
#47997=CARTESIAN_POINT('Ctrl Pts',(-2.44167165546222,6.31347941224203,-1.07983041697668));
#47998=CARTESIAN_POINT('Ctrl Pts',(-2.6011426866065,6.24946463474063,-1.07179058696506));
#47999=CARTESIAN_POINT('Ctrl Pts',(-2.75788731040707,6.17951022194281,-1.06375075695344));
#48000=CARTESIAN_POINT('Ctrl Pts',(-2.91467973129993,6.10953447752006,-1.05570847530751));
#48001=CARTESIAN_POINT('Ctrl Pts',(-3.06874374914964,6.03361564470674,-1.04766619366157));
#48002=CARTESIAN_POINT('Ctrl Pts',(-3.21960110107852,5.95201291580705,-1.03962391201564));
#48003=CARTESIAN_POINT('Ctrl Pts',(-3.37553950094233,5.86766171378452,-1.03131075713731));
#48004=CARTESIAN_POINT('Ctrl Pts',(-3.52805106989464,5.77723725642645,-1.02299760225897));
#48005=CARTESIAN_POINT('Ctrl Pts',(-3.67663933634794,5.68107491505076,-1.01468444738064));
#48006=CARTESIAN_POINT('Ctrl Pts',(-3.82063922158787,5.58788205095032,-1.00662800135676));
#48007=CARTESIAN_POINT('Ctrl Pts',(-3.96095424620564,5.48930067774289,-0.998571555332877));
#48008=CARTESIAN_POINT('Ctrl Pts',(-4.09716604848102,5.38567724350192,-0.990515109309001));
#48009=CARTESIAN_POINT('Ctrl Pts',(-4.23988818588854,5.27710105719995,-0.982073600003433));
#48010=CARTESIAN_POINT('Ctrl Pts',(-4.37810486731001,5.16298931304757,-0.973632090697874));
#48011=CARTESIAN_POINT('Ctrl Pts',(-4.51137852757536,5.04378357792362,-0.965190581392307));
#48012=CARTESIAN_POINT('Ctrl Pts',(-4.64465218784067,4.92457784279971,-0.956749072086742));
#48013=CARTESIAN_POINT('Ctrl Pts',(-4.77298255617914,4.80027849925549,-0.94830756278117));
#48014=CARTESIAN_POINT('Ctrl Pts',(-4.89598113101639,4.67136572799984,-0.939866053475605));
#48015=CARTESIAN_POINT('Ctrl Pts',(-5.01696362412722,4.54456597864526,-0.931562909778558));
#48016=CARTESIAN_POINT('Ctrl Pts',(-5.13317976522407,4.41289279758091,-0.923259766081505));
#48017=CARTESIAN_POINT('Ctrl Pts',(-5.24421808414461,4.27673540050477,-0.914956622384459));
#48018=CARTESIAN_POINT('Ctrl Pts',(-5.35512072254373,4.14074437758496,-0.906663624508037));
#48019=CARTESIAN_POINT('Ctrl Pts',(-5.46085792174848,4.00028032354014,-0.898370626631615));
#48020=CARTESIAN_POINT('Ctrl Pts',(-5.56105499227057,3.8557692323248,-0.890077628755193));
#48021=CARTESIAN_POINT('Ctrl Pts',(-5.66112294863427,3.71144435840927,-0.881795317253492));
#48022=CARTESIAN_POINT('Ctrl Pts',(-5.75566480980538,3.56308313093797,-0.873513005751797));
#48023=CARTESIAN_POINT('Ctrl Pts',(-5.84434627259084,3.41114433087396,-0.865230694250094));
#48024=CARTESIAN_POINT('Ctrl Pts',(-5.93296115248566,3.25931960791458,-0.856954601187101));
#48025=CARTESIAN_POINT('Ctrl Pts',(-6.01572422155528,3.10392296416771,-0.848678508124099));
#48026=CARTESIAN_POINT('Ctrl Pts',(-6.09234417361033,2.94544249142235,-0.840402415061106));
#48027=CARTESIAN_POINT('Ctrl Pts',(-6.16891973497529,2.78705383624359,-0.832131116852098));
#48028=CARTESIAN_POINT('Ctrl Pts',(-6.2393591169355,2.6255852264934,-0.823859818643093));
#48029=CARTESIAN_POINT('Ctrl Pts',(-6.30341664058509,2.46154984820437,-0.815588520434083));
#48030=CARTESIAN_POINT('Ctrl Pts',(-6.36744803186293,2.29758138841675,-0.807320596514733));
#48031=CARTESIAN_POINT('Ctrl Pts',(-6.42510262495094,2.13104857317411,-0.79905267259539));
#48032=CARTESIAN_POINT('Ctrl Pts',(-6.47618257374036,1.96248522837287,-0.790784748676039));
#48033=CARTESIAN_POINT('Ctrl Pts',(-6.52725782163957,1.79393739646454,-0.782517585654132));
#48034=CARTESIAN_POINT('Ctrl Pts',(-6.57175952260472,1.62335974133626,-0.774250422632216));
#48035=CARTESIAN_POINT('Ctrl Pts',(-6.60953936200882,1.45130231931742,-0.765983259610309));
#48036=CARTESIAN_POINT('Ctrl Pts',(-6.64731619469459,1.27925859053315,-0.757716754532716));
#48037=CARTESIAN_POINT('Ctrl Pts',(-6.67837215988471,1.10573567334515,-0.74945024945513));
#48038=CARTESIAN_POINT('Ctrl Pts',(-6.70260986472482,0.931294798274735,
-0.741183744377537));
#48039=CARTESIAN_POINT('Ctrl Pts',(-6.72685689179225,0.756786830321425,
-0.732914059863605));
#48040=CARTESIAN_POINT('Ctrl Pts',(-6.74428037073407,0.581360547257899,
-0.724644375349675));
#48041=CARTESIAN_POINT('Ctrl Pts',(-6.75483461391262,0.405583947769132,
-0.716374690835742));
#48042=CARTESIAN_POINT('Ctrl Pts',(-6.76300049239713,0.269584584521214,
-0.709976388493866));
#48043=CARTESIAN_POINT('Ctrl Pts',(-6.76705534748704,0.133375685775319,
-0.70357808615199));
#48044=CARTESIAN_POINT('Ctrl Pts',(-6.76699942930254,-0.00277917598916038,
-0.697179783810114));
#48045=CARTESIAN_POINT('Ctrl Pts',(-6.76699942930229,-0.00277917658345176,
-0.697179783782168));
#48046=CARTESIAN_POINT('Ctrl Pts',(-6.76690970559949,-0.221246851251606,
-0.686913369374764));
#48047=CARTESIAN_POINT('Ctrl Pts',(-6.75623640357004,-0.439364788743829,
-0.676646954967357));
#48048=CARTESIAN_POINT('Ctrl Pts',(-6.7351046007485,-0.656243108136276,
-0.666380540559935));
#48049=CARTESIAN_POINT('Ctrl Pts',(-6.7137419144094,-0.875491013772146,
-0.656001956552447));
#48050=CARTESIAN_POINT('Ctrl Pts',(-6.68169095530472,-1.09347220153135,
-0.645623372544961));
#48051=CARTESIAN_POINT('Ctrl Pts',(-6.63913111398288,-1.30928493894359,
-0.63524478853747));
#48052=CARTESIAN_POINT('Ctrl Pts',(-6.62148928374299,-1.39874325360786,
-0.630942676229158));
#48053=CARTESIAN_POINT('Ctrl Pts',(-6.60204235066164,-1.48782916916932,
-0.62664056392084));
#48054=CARTESIAN_POINT('Ctrl Pts',(-6.58080558754353,-1.5764792478672,-0.622338451612528));
#48055=CARTESIAN_POINT('Ctrl Pts',(-6.53908299118297,-1.75064474711359,
-0.613886349268152));
#48056=CARTESIAN_POINT('Ctrl Pts',(-6.49040676320739,-1.92330031190699,
-0.605434246923772));
#48057=CARTESIAN_POINT('Ctrl Pts',(-6.4349041551301,-2.09387141780229,-0.5969821445794));
#48058=CARTESIAN_POINT('Ctrl Pts',(-6.3794505223416,-2.26429201240706,-0.588537500337764));
#48059=CARTESIAN_POINT('Ctrl Pts',(-6.31718261765681,-2.43263150061118,
-0.580092856096124));
#48060=CARTESIAN_POINT('Ctrl Pts',(-6.24827810907183,-2.59832824556363,
-0.571648211854487));
#48061=CARTESIAN_POINT('Ctrl Pts',(-6.17942505415503,-2.7639012583321,-0.563209873556128));
#48062=CARTESIAN_POINT('Ctrl Pts',(-6.10394540134535,-2.92683515686584,
-0.554771535257758));
#48063=CARTESIAN_POINT('Ctrl Pts',(-6.02206588901574,-3.08658572347393,
-0.546333196959402));
#48064=CARTESIAN_POINT('Ctrl Pts',(-5.94024510928763,-3.24622170016688,
-0.537900911525146));
#48065=CARTESIAN_POINT('Ctrl Pts',(-5.85203377767385,-3.40267860546137,
-0.529468626090902));
#48066=CARTESIAN_POINT('Ctrl Pts',(-5.75770585330553,-3.55543419385189,
-0.521036340656643));
#48067=CARTESIAN_POINT('Ctrl Pts',(-5.66341858833023,-3.70812393801288,
-0.51260768990013));
#48068=CARTESIAN_POINT('Ctrl Pts',(-5.56302016037904,-3.85711526441339,
-0.504179039143616));
#48069=CARTESIAN_POINT('Ctrl Pts',(-5.45682970571519,-4.0019118634503,-0.495750388387101));
#48070=CARTESIAN_POINT('Ctrl Pts',(-5.3506723618518,-4.14666331406674,-0.487324365732841));
#48071=CARTESIAN_POINT('Ctrl Pts',(-5.23872678862464,-4.2872223788229,-0.478898343078576));
#48072=CARTESIAN_POINT('Ctrl Pts',(-5.12135475846663,-4.42312270211118,
-0.470472320424314));
#48073=CARTESIAN_POINT('Ctrl Pts',(-5.08932725136838,-4.4602060563218,-0.468173097176611));
#48074=CARTESIAN_POINT('Ctrl Pts',(-5.05689593330575,-4.49694270786391,
-0.465873873928905));
#48075=CARTESIAN_POINT('Ctrl Pts',(-5.02406868047268,-4.53332360348272,
-0.463574650681203));
#48076=CARTESIAN_POINT('Ctrl Pts',(-4.901002160078,-4.66971242210901,-0.454955062373151));
#48077=CARTESIAN_POINT('Ctrl Pts',(-4.77242363098732,-4.80103706814503,
-0.446335474065095));
#48078=CARTESIAN_POINT('Ctrl Pts',(-4.63877664921645,-4.92686920860339,
-0.437715885757044));
#48079=CARTESIAN_POINT('Ctrl Pts',(-4.50504919667541,-5.05277711440356,
-0.429091107470883));
#48080=CARTESIAN_POINT('Ctrl Pts',(-4.36624742236036,-5.17318570617981,
-0.420466329184711));
#48081=CARTESIAN_POINT('Ctrl Pts',(-4.22284924252844,-5.28770586122914,
-0.411841550898551));
#48082=CARTESIAN_POINT('Ctrl Pts',(-4.07455550072935,-5.4061356929298,-0.402922325802797));
#48083=CARTESIAN_POINT('Ctrl Pts',(-3.92134625974652,-5.5182677169265,-0.394003100707058));
#48084=CARTESIAN_POINT('Ctrl Pts',(-3.76378360987677,-5.6237195820936,-0.385083875611301));
#48085=CARTESIAN_POINT('Ctrl Pts',(-3.611137779954,-5.72588076996802,-0.376442979319348));
#48086=CARTESIAN_POINT('Ctrl Pts',(-3.45440642855516,-5.82177230803757,
-0.367802083027394));
#48087=CARTESIAN_POINT('Ctrl Pts',(-3.29412709115138,-5.91109259844088,
-0.359161186735442));
#48088=CARTESIAN_POINT('Ctrl Pts',(-3.12610370357964,-6.00472848448555,
-0.350102797237785));
#48089=CARTESIAN_POINT('Ctrl Pts',(-2.95418133405112,-6.09114222573036,
-0.341044407740149));
#48090=CARTESIAN_POINT('Ctrl Pts',(-2.77900494902321,-6.170042179216,-0.331986018242496));
#48091=CARTESIAN_POINT('Ctrl Pts',(-2.60382856399525,-6.24894213270166,
-0.32292762874484));
#48092=CARTESIAN_POINT('Ctrl Pts',(-2.42539853061243,-6.32032818726296,
-0.313869239247172));
#48093=CARTESIAN_POINT('Ctrl Pts',(-2.24438075491975,-6.38396773385846,
-0.304810849749515));
#48094=CARTESIAN_POINT('Ctrl Pts',(-2.06386608615943,-6.44743040557555,
-0.295777636445384));
#48095=CARTESIAN_POINT('Ctrl Pts',(-1.88061033434157,-6.50324941191704,
-0.286744423141259));
#48096=CARTESIAN_POINT('Ctrl Pts',(-1.69524999163123,-6.55121488472744,
-0.277711209837129));
#48097=CARTESIAN_POINT('Ctrl Pts',(-1.510059729892,-6.59913634588963,-0.268686285132753));
#48098=CARTESIAN_POINT('Ctrl Pts',(-1.32276896481906,-6.63921860024135,
-0.259661360428383));
#48099=CARTESIAN_POINT('Ctrl Pts',(-1.1340283502408,-6.67130187451071,-0.250636435724005));
#48100=CARTESIAN_POINT('Ctrl Pts',(-0.945616935672086,-6.70332918936604,
-0.241627252227767));
#48101=CARTESIAN_POINT('Ctrl Pts',(-0.755760957629054,-6.72738534371772,
-0.232618068731527));
#48102=CARTESIAN_POINT('Ctrl Pts',(-0.565120088508994,-6.74336179405818,
-0.223608885235294));
#48103=CARTESIAN_POINT('Ctrl Pts',(-0.374714945004879,-6.75931848967022,
-0.214610841508506));
#48104=CARTESIAN_POINT('Ctrl Pts',(-0.18352708569595,-6.76721539860972,
-0.205612797781702));
#48105=CARTESIAN_POINT('Ctrl Pts',(0.00777736804904949,-6.7669955307024,
-0.196614754054913));
#48106=CARTESIAN_POINT('Ctrl Pts',(0.198658389228101,-6.76677614944989,
-0.187636626564621));
#48107=CARTESIAN_POINT('Ctrl Pts',(0.389655250132718,-6.75847585301212,
-0.178658499074348));
#48108=CARTESIAN_POINT('Ctrl Pts',(0.580100937286119,-6.74208957983797,
-0.169680371584057));
#48109=CARTESIAN_POINT('Ctrl Pts',(0.747205729784349,-6.72771159722512,
-0.161802597328769));
#48110=CARTESIAN_POINT('Ctrl Pts',(0.913885991250512,-6.70710894989072,
-0.153924823073464));
#48111=CARTESIAN_POINT('Ctrl Pts',(1.07968995621285,-6.68031126508736,-0.146047048818176));
#48112=CARTESIAN_POINT('Ctrl Pts',(1.25095258969113,-6.65263133552967,-0.137909919134849));
#48113=CARTESIAN_POINT('Ctrl Pts',(1.42120128441979,-6.61835287109931,-0.129772789451537));
#48114=CARTESIAN_POINT('Ctrl Pts',(1.58989107614523,-6.57757822956092,-0.121635659768209));
#48115=CARTESIAN_POINT('Ctrl Pts',(1.75857100515743,-6.5368059719759,-0.113499005834931));
#48116=CARTESIAN_POINT('Ctrl Pts',(1.9256918583268,-6.48953837960548,-0.105362351901639));
#48117=CARTESIAN_POINT('Ctrl Pts',(2.09072064053307,-6.43592854242875,-0.0972256979683621));
#48118=CARTESIAN_POINT('Ctrl Pts',(2.25577097910605,-6.38231170263529,-0.0890879812102037));
#48119=CARTESIAN_POINT('Ctrl Pts',(2.41872835612831,-6.32235108206134,-0.0809502644520282));
#48120=CARTESIAN_POINT('Ctrl Pts',(2.57907669378534,-6.25624906853726,-0.0728125476938715));
#48121=CARTESIAN_POINT('Ctrl Pts',(2.73954330896164,-6.19009829627771,-0.0646688283231229));
#48122=CARTESIAN_POINT('Ctrl Pts',(2.8973967035762,-6.11779722237087,-0.0565251089523754));
#48123=CARTESIAN_POINT('Ctrl Pts',(3.05214187870714,-6.03959592623894,-0.0483813895816212));
#48124=CARTESIAN_POINT('Ctrl Pts',(3.20695114179602,-5.96136224291709,-0.040234297476667));
#48125=CARTESIAN_POINT('Ctrl Pts',(3.35864930069323,-5.8772236429884,-0.032087205371719));
#48126=CARTESIAN_POINT('Ctrl Pts',(3.50676778194066,-5.78747515964803,-0.023940113266768));
#48127=CARTESIAN_POINT('Ctrl Pts',(3.6550474364314,-5.6976290176359,-0.0157841560070632));
#48128=CARTESIAN_POINT('Ctrl Pts',(3.79973932923221,-5.6021610002471,-0.00762819874735902));
#48129=CARTESIAN_POINT('Ctrl Pts',(3.94040495610507,-5.50140870885836,0.000527758512347987));
#48130=CARTESIAN_POINT('Ctrl Pts',(4.01047939663398,-5.45121762374378,0.00459075637939762));
#48131=CARTESIAN_POINT('Ctrl Pts',(4.07955517102849,-5.39971578419021,0.0086537542464415));
#48132=CARTESIAN_POINT('Ctrl Pts',(4.14758131819055,-5.34694849507611,0.0127167521134908));
#48133=CARTESIAN_POINT('Ctrl Pts',(4.28866189222471,-5.23751352412726,0.0211430719227959));
#48134=CARTESIAN_POINT('Ctrl Pts',(4.42551682084227,-5.12240752092213,0.0295693917321155));
#48135=CARTESIAN_POINT('Ctrl Pts',(4.55767992858152,-5.0019838732852,0.0379957115414271));
#48136=CARTESIAN_POINT('Ctrl Pts',(4.68974123890343,-4.8816529808545,0.04641554105546));
#48137=CARTESIAN_POINT('Ctrl Pts',(4.81711768504375,-4.75601283324789,0.0548353705694841));
#48138=CARTESIAN_POINT('Ctrl Pts',(4.93937595472497,-4.62545718582334,0.0632552000835176));
#48139=CARTESIAN_POINT('Ctrl Pts',(5.06155932053113,-4.49498152582156,0.0716698710274222));
#48140=CARTESIAN_POINT('Ctrl Pts',(5.17863053259408,-4.35959661368453,0.0800845419713343));
#48141=CARTESIAN_POINT('Ctrl Pts',(5.29019269833248,-4.21973342931869,0.088499212915238));
#48142=CARTESIAN_POINT('Ctrl Pts',(5.4017040744868,-4.07993391880605,0.0969100530116977));
#48143=CARTESIAN_POINT('Ctrl Pts',(5.5077111961529,-3.93566046249943,0.105320893108149));
#48144=CARTESIAN_POINT('Ctrl Pts',(5.60785684119223,-3.78737780643726,0.113731733204609));
#48145=CARTESIAN_POINT('Ctrl Pts',(5.70797264594431,-3.63913933399435,0.122140067132336));
#48146=CARTESIAN_POINT('Ctrl Pts',(5.80223026949453,-3.48689432146133,0.130548401060059));
#48147=CARTESIAN_POINT('Ctrl Pts',(5.89031507729034,-3.33113753697534,0.138956734987786));
#48148=CARTESIAN_POINT('Ctrl Pts',(5.9784019705473,-3.17537706485317,0.14736526798791));
#48149=CARTESIAN_POINT('Ctrl Pts',(6.06031558521371,-3.01610494300437,0.155773800988043));
#48150=CARTESIAN_POINT('Ctrl Pts',(6.13578630374197,-2.85384222318132,0.164182333988165));
#48151=CARTESIAN_POINT('Ctrl Pts',(6.21126013743586,-2.69157280572429,0.172591214062936));
#48152=CARTESIAN_POINT('Ctrl Pts',(6.28029040316456,-2.52631284807733,0.181000094137698));
#48153=CARTESIAN_POINT('Ctrl Pts',(6.34265482316743,-2.35860526458986,0.189408974212469));
#48154=CARTESIAN_POINT('Ctrl Pts',(6.40503073850055,-2.19086676837908,0.197819404255213));
#48155=CARTESIAN_POINT('Ctrl Pts',(6.4607382416948,-2.02068006109688,0.206229834297953));
#48156=CARTESIAN_POINT('Ctrl Pts',(6.50960419080739,-1.84860549577862,0.214640264340694));
#48157=CARTESIAN_POINT('Ctrl Pts',(6.55848613937721,-1.67647459062251,0.223053448086541));
#48158=CARTESIAN_POINT('Ctrl Pts',(6.60052197647211,-1.50245491748494,0.231466631832394));
#48159=CARTESIAN_POINT('Ctrl Pts',(6.63558907049047,-1.32711969602874,0.239879815578242));
#48160=CARTESIAN_POINT('Ctrl Pts',(6.67068878256316,-1.15162138453218,0.248300824942154));
#48161=CARTESIAN_POINT('Ctrl Pts',(6.69880673379692,-0.974805408722592,
0.256721834306079));
#48162=CARTESIAN_POINT('Ctrl Pts',(6.71987165761963,-0.797253977801603,
0.265142843669992));
#48163=CARTESIAN_POINT('Ctrl Pts',(6.7409471472684,-0.619613489946317,0.273568076876392));
#48164=CARTESIAN_POINT('Ctrl Pts',(6.75496252317796,-0.441237144900999,
0.281993310082783));
#48165=CARTESIAN_POINT('Ctrl Pts',(6.76189856815725,-0.262710399400144,
0.290418543289185));
#48166=CARTESIAN_POINT('Ctrl Pts',(6.7688426266085,-0.0839773952787056,
0.298853510482359));
#48167=CARTESIAN_POINT('Ctrl Pts',(6.76869100669955,0.0949060212790336,
0.307288477675536));
#48168=CARTESIAN_POINT('Ctrl Pts',(6.76147661581355,0.273355032524567,0.315723444868709));
#48169=CARTESIAN_POINT('Ctrl Pts',(6.75733672560317,0.375755820946249,0.320563747904648));
#48170=CARTESIAN_POINT('Ctrl Pts',(6.75087209684535,0.478013640515783,0.325404050940573));
#48171=CARTESIAN_POINT('Ctrl Pts',(6.7420966267274,0.580019030611108,0.330244353976511));
#48172=CARTESIAN_POINT('Ctrl Pts',(6.72709792733164,0.754362759462393,0.338517215628905));
#48173=CARTESIAN_POINT('Ctrl Pts',(6.70531184881675,0.928363414331154,0.346790077281274));
#48174=CARTESIAN_POINT('Ctrl Pts',(6.67675688288832,1.10145654785085,0.355062938933656));
#48175=CARTESIAN_POINT('Ctrl Pts',(6.64823478984464,1.27435041408216,0.363326276749506));
#48176=CARTESIAN_POINT('Ctrl Pts',(6.61295938424434,1.44633849500936,0.371589614565336));
#48177=CARTESIAN_POINT('Ctrl Pts',(6.57100105581381,1.61685933973668,0.379852952381185));
#48178=CARTESIAN_POINT('Ctrl Pts',(6.52908375851575,1.78721343179226,0.388108209462619));
#48179=CARTESIAN_POINT('Ctrl Pts',(6.48049663861083,1.95610280542443,0.396363466544053));
#48180=CARTESIAN_POINT('Ctrl Pts',(6.42536150878182,2.12297397098151,0.404618723625489));
#48181=CARTESIAN_POINT('Ctrl Pts',(6.37027977715849,2.28968352232187,0.412865985515531));
#48182=CARTESIAN_POINT('Ctrl Pts',(6.3086627871622,2.45437842876475,0.421113247405568));
#48183=CARTESIAN_POINT('Ctrl Pts',(6.24068272489409,2.61651832158853,0.429360509295606));
#48184=CARTESIAN_POINT('Ctrl Pts',(6.17274088431909,2.7785670514887,0.437603134174403));
#48185=CARTESIAN_POINT('Ctrl Pts',(6.09844323291158,2.93806330498765,0.445845759053206));
#48186=CARTESIAN_POINT('Ctrl Pts',(6.01801099791469,3.09448422664874,0.454088383932003));
#48187=CARTESIAN_POINT('Ctrl Pts',(5.93761260647178,3.25083933091827,0.46232754055308));
#48188=CARTESIAN_POINT('Ctrl Pts',(5.85108493604182,3.40412136909221,0.470566697174174));
#48189=CARTESIAN_POINT('Ctrl Pts',(5.7586963544244,3.55382966636545,0.478805853795251));
#48190=CARTESIAN_POINT('Ctrl Pts',(5.72056234903276,3.61562276801768,0.482206620832802));
#48191=CARTESIAN_POINT('Ctrl Pts',(5.68143037765305,3.676807299254,0.485607387870354));
#48192=CARTESIAN_POINT('Ctrl Pts',(5.64132157314919,3.73734931580146,0.489008154907907));
#48193=CARTESIAN_POINT('Ctrl Pts',(5.53726608791621,3.89441530135636,0.497830867741997));
#48194=CARTESIAN_POINT('Ctrl Pts',(5.42674759486663,4.04698209985476,0.506653580576097));
#48195=CARTESIAN_POINT('Ctrl Pts',(5.31018113334372,4.19455186296229,0.515476293410202));
#48196=CARTESIAN_POINT('Ctrl Pts',(5.19340607508605,4.34238570349254,0.524314794568539));
#48197=CARTESIAN_POINT('Ctrl Pts',(5.07056158678431,4.48520443187774,0.533153295726877));
#48198=CARTESIAN_POINT('Ctrl Pts',(4.94210115344296,4.6225453149902,0.541991796885213));
#48199=CARTESIAN_POINT('Ctrl Pts',(4.81328318041853,4.76026845444839,0.550854897952025));
#48200=CARTESIAN_POINT('Ctrl Pts',(4.67881816800654,4.89248304563406,0.559717999018851));
#48201=CARTESIAN_POINT('Ctrl Pts',(4.53919667414657,5.01876305013663,0.568581100085666));
#48202=CARTESIAN_POINT('Ctrl Pts',(4.39938827955337,5.14521209612974,0.577456065515498));
#48203=CARTESIAN_POINT('Ctrl Pts',(4.25440981792345,5.26571051468527,0.5863310309453));
#48204=CARTESIAN_POINT('Ctrl Pts',(4.10478382286784,5.379873489918,0.595205996375128));
#48205=CARTESIAN_POINT('Ctrl Pts',(3.95482057865104,5.49429378252144,0.604100965512506));
#48206=CARTESIAN_POINT('Ctrl Pts',(3.80018906105163,5.6023499083688,0.612995934649882));
#48207=CARTESIAN_POINT('Ctrl Pts',(3.64144198757417,5.70369961087818,0.621890903787261));
#48208=CARTESIAN_POINT('Ctrl Pts',(3.48747700623195,5.80199625795376,0.630517921138043));
#48209=CARTESIAN_POINT('Ctrl Pts',(3.32964101985645,5.89398457502353,0.639144938488834));
#48210=CARTESIAN_POINT('Ctrl Pts',(3.16845894722699,5.97939435894115,0.647771955839616));
#48211=CARTESIAN_POINT('Ctrl Pts',(3.14540941730174,5.99160821956599,0.649005645736694));
#48212=CARTESIAN_POINT('Ctrl Pts',(3.12228440987943,6.00369137191337,0.650239335633784));
#48213=CARTESIAN_POINT('Ctrl Pts',(3.09908550384723,6.01564277861011,0.651473025530862));
#48214=CARTESIAN_POINT('Origin',(0.,0.,-63.6971797838103));
#48215=CARTESIAN_POINT('',(3.09908550384731,6.01564277861007,3.04562247039131));
#48216=CARTESIAN_POINT('',(3.09908550384727,6.01564277861009,2.6515053192028));
#48217=CARTESIAN_POINT('',(3.09908550384721,6.01564277861012,-63.6971797838103));
#48218=CARTESIAN_POINT('',(-6.76699874199977,0.004126229935696,1.69717978377767));
#48219=CARTESIAN_POINT('Ctrl Pts',(-6.7669987420002,0.0041262292468995,
1.69717978380999));
#48220=CARTESIAN_POINT('Ctrl Pts',(-6.76710297099132,-0.166808881138621,
1.70519840959001));
#48221=CARTESIAN_POINT('Ctrl Pts',(-6.76072618644486,-0.337884134911409,
1.71321703537002));
#48222=CARTESIAN_POINT('Ctrl Pts',(-6.74786314866394,-0.508558675968804,
1.72123566115003));
#48223=CARTESIAN_POINT('Ctrl Pts',(-6.74120626970332,-0.596886159789519,
1.72538546014442));
#48224=CARTESIAN_POINT('Ctrl Pts',(-6.7328130489101,-0.685106279448968,
1.72953525913879));
#48225=CARTESIAN_POINT('Ctrl Pts',(-6.72268824459125,-0.773144078445009,
1.73368505813318));
#48226=CARTESIAN_POINT('Ctrl Pts',(-6.70258469082633,-0.947949691445093,
1.74192479339818));
#48227=CARTESIAN_POINT('Ctrl Pts',(-6.67566140789129,-1.12194795613973,
1.75016452866318));
#48228=CARTESIAN_POINT('Ctrl Pts',(-6.64201440311397,-1.29457856803925,
1.75840426392818));
#48229=CARTESIAN_POINT('Ctrl Pts',(-6.60835701093335,-1.46726247394813,
1.76664654293977));
#48230=CARTESIAN_POINT('Ctrl Pts',(-6.56797182808259,-1.63857753976916,
1.77488882195136));
#48231=CARTESIAN_POINT('Ctrl Pts',(-6.52100572584818,-1.807974923348,1.78313110096295));
#48232=CARTESIAN_POINT('Ctrl Pts',(-6.4740169939614,-1.97745392757924,1.7913773513475));
#48233=CARTESIAN_POINT('Ctrl Pts',(-6.4204411183472,-2.14501306905879,1.79962360173205));
#48234=CARTESIAN_POINT('Ctrl Pts',(-6.36047448242523,-2.31011977144421,
1.8078698521166));
#48235=CARTESIAN_POINT('Ctrl Pts',(-6.30043566332169,-2.47542521646204,
1.81612602869727));
#48236=CARTESIAN_POINT('Ctrl Pts',(-6.23399083852102,-2.63827199441728,
1.82438220527795));
#48237=CARTESIAN_POINT('Ctrl Pts',(-6.16138450155594,-2.79814760582538,
1.83263838185863));
#48238=CARTESIAN_POINT('Ctrl Pts',(-6.08872815499652,-2.95813333592013,
1.84090024510605));
#48239=CARTESIAN_POINT('Ctrl Pts',(-6.00990199294824,-3.11514350533717,
1.84916210835345));
#48240=CARTESIAN_POINT('Ctrl Pts',(-5.92519591535356,-3.26869123116232,
1.85742397160087));
#48241=CARTESIAN_POINT('Ctrl Pts',(-5.84036956708222,-3.42245697308987,
1.8656975655282));
#48242=CARTESIAN_POINT('Ctrl Pts',(-5.74964680847141,-3.57275015056186,
1.87397115945553));
#48243=CARTESIAN_POINT('Ctrl Pts',(-5.65336077724304,-3.71911292142763,
1.88224475338286));
#48244=CARTESIAN_POINT('Ctrl Pts',(-5.61377649472611,-3.77928432114158,
1.88564612194351));
#48245=CARTESIAN_POINT('Ctrl Pts',(-5.57325242186237,-3.83879182045804,
1.88904749050416));
#48246=CARTESIAN_POINT('Ctrl Pts',(-5.53181362420354,-3.89760529390498,
1.89244885906481));
#48247=CARTESIAN_POINT('Ctrl Pts',(-5.42905042189326,-4.04345558908385,
1.90088384138278));
#48248=CARTESIAN_POINT('Ctrl Pts',(-5.32042193225358,-4.18537206677828,
1.90931882370074));
#48249=CARTESIAN_POINT('Ctrl Pts',(-5.20625440608239,-4.32286988690935,
1.91775380601871));
#48250=CARTESIAN_POINT('Ctrl Pts',(-5.09219484559422,-4.46023767841879,
1.92618081156204));
#48251=CARTESIAN_POINT('Ctrl Pts',(-4.97260690208883,-4.5931948844967,1.93460781710537));
#48252=CARTESIAN_POINT('Ctrl Pts',(-4.84785902237663,-4.72128710196294,
1.9430348226487));
#48253=CARTESIAN_POINT('Ctrl Pts',(-4.72320942905771,-4.84927839809814,
1.95145518872061));
#48254=CARTESIAN_POINT('Ctrl Pts',(-4.59340823641803,-4.97241210706217,
1.95987555479253));
#48255=CARTESIAN_POINT('Ctrl Pts',(-4.45886316091591,-5.09026800003958,
1.96829592086445));
#48256=CARTESIAN_POINT('Ctrl Pts',(-4.32440288737786,-5.20804961002177,
1.97671097969209));
#48257=CARTESIAN_POINT('Ctrl Pts',(-4.18520494336179,-5.32055981555433,
1.98512603851973));
#48258=CARTESIAN_POINT('Ctrl Pts',(-4.04171305541096,-5.42741601295871,
1.99354109734738));
#48259=CARTESIAN_POINT('Ctrl Pts',(-3.89828901883082,-5.5342216824931,2.00195217704223));
#48260=CARTESIAN_POINT('Ctrl Pts',(-3.75057535512656,-5.63537847480804,
2.01036325673709));
#48261=CARTESIAN_POINT('Ctrl Pts',(-3.59904823634381,-5.73054454589357,
2.01877433643195));
#48262=CARTESIAN_POINT('Ctrl Pts',(-3.44755742646226,-5.8256878133021,2.02718340066539));
#48263=CARTESIAN_POINT('Ctrl Pts',(-3.29225526556584,-5.91484304125412,
2.03559246489883));
#48264=CARTESIAN_POINT('Ctrl Pts',(-3.13364664840334,-5.99771187061787,
2.04400152913227));
#48265=CARTESIAN_POINT('Ctrl Pts',(-2.97505735390578,-6.08057060439758,
2.05240956892245));
#48266=CARTESIAN_POINT('Ctrl Pts',(-2.81316270309042,-6.15714431105671,
2.06081760871261));
#48267=CARTESIAN_POINT('Ctrl Pts',(-2.64849218286932,-6.22718059456124,
2.06922564850278));
#48268=CARTESIAN_POINT('Ctrl Pts',(-2.48381817102483,-6.29721836309373,
2.07763386657446));
#48269=CARTESIAN_POINT('Ctrl Pts',(-2.31636848099018,-6.36071830128286,
2.08604208464614));
#48270=CARTESIAN_POINT('Ctrl Pts',(-2.14669288550721,-6.41747603465044,
2.09445030271782));
#48271=CARTESIAN_POINT('Ctrl Pts',(-1.97698942264425,-6.47424308986137,
2.1028599017483));
#48272=CARTESIAN_POINT('Ctrl Pts',(-1.80505964350623,-6.52426562694529,
2.11126950077879));
#48273=CARTESIAN_POINT('Ctrl Pts',(-1.63146912695812,-6.56738893988947,
2.11967909980928));
#48274=CARTESIAN_POINT('Ctrl Pts',(-1.45776002175846,-6.61054171259696,
2.1280944438714));
#48275=CARTESIAN_POINT('Ctrl Pts',(-1.28238823770533,-6.64678576226753,
2.13650978793351));
#48276=CARTESIAN_POINT('Ctrl Pts',(-1.10593119819516,-6.67601716481156,
2.14492513199563));
#48277=CARTESIAN_POINT('Ctrl Pts',(-0.929410368622567,-6.7052591346472,
2.15334351824482));
#48278=CARTESIAN_POINT('Ctrl Pts',(-0.751803832989001,-6.72748335415473,
2.16176190449402));
#48279=CARTESIAN_POINT('Ctrl Pts',(-0.573695352906521,-6.74263766207658,
2.1701802907432));
#48280=CARTESIAN_POINT('Ctrl Pts',(-0.395419202031871,-6.75780623621872,
2.17860660203611));
#48281=CARTESIAN_POINT('Ctrl Pts',(-0.216640497220458,-6.76589157901934,
2.187032913329));
#48282=CARTESIAN_POINT('Ctrl Pts',(-0.0379453377691904,-6.76689361164645,
2.1954592246219));
#48283=CARTESIAN_POINT('Ctrl Pts',(0.0646760729647106,-6.76746906093177,
2.20029830339055));
#48284=CARTESIAN_POINT('Ctrl Pts',(0.167269944912153,-6.76570939935171,
2.2051373821592));
#48285=CARTESIAN_POINT('Ctrl Pts',(0.269725823615944,-6.76162236301871,
2.20997646092785));
#48286=CARTESIAN_POINT('Ctrl Pts',(0.442402428732244,-6.75473417302027,
2.2181321246558));
#48287=CARTESIAN_POINT('Ctrl Pts',(0.615031731835564,-6.74121836881216,
2.22628778838376));
#48288=CARTESIAN_POINT('Ctrl Pts',(0.787061651744364,-6.72107305096094,
2.23444345211172));
#48289=CARTESIAN_POINT('Ctrl Pts',(0.958941008873126,-6.70094536454885,
2.24259197789876));
#48290=CARTESIAN_POINT('Ctrl Pts',(1.13022166734705,-6.67419975683062,2.2507405036858));
#48291=CARTESIAN_POINT('Ctrl Pts',(1.30035287488392,-6.64088634150451,2.25888902947284));
#48292=CARTESIAN_POINT('Ctrl Pts',(1.47036736483711,-6.60759578066463,2.26703196500837));
#48293=CARTESIAN_POINT('Ctrl Pts',(1.63923361758765,-6.56774645349893,2.27517490054391));
#48294=CARTESIAN_POINT('Ctrl Pts',(1.80640734694751,-6.52144013979229,2.28331783607943));
#48295=CARTESIAN_POINT('Ctrl Pts',(1.97349951886859,-6.47515641710136,2.29145679899935));
#48296=CARTESIAN_POINT('Ctrl Pts',(2.13890046121281,-6.42242207865703,2.29959576191926));
#48297=CARTESIAN_POINT('Ctrl Pts',(2.30207741597558,-6.36338970760515,2.30773472483918));
#48298=CARTESIAN_POINT('Ctrl Pts',(2.46520773901468,-6.30437420646741,2.31587136185548));
#48299=CARTESIAN_POINT('Ctrl Pts',(2.62611499811908,-6.23906438240821,2.32400799887178));
#48300=CARTESIAN_POINT('Ctrl Pts',(2.78428290701581,-6.16766225515791,2.33214463588808));
#48301=CARTESIAN_POINT('Ctrl Pts',(2.94245684475139,-6.09625740629411,2.34028158304614));
#48302=CARTESIAN_POINT('Ctrl Pts',(3.09789088966155,-6.01875993661228,2.34841853020418));
#48303=CARTESIAN_POINT('Ctrl Pts',(3.25008982849438,-5.93541953923372,2.35655547736224));
#48304=CARTESIAN_POINT('Ctrl Pts',(3.32606063320038,-5.89381979417688,2.36061707219455));
#48305=CARTESIAN_POINT('Ctrl Pts',(3.40122575489734,-5.85076498187504,2.36467866702688));
#48306=CARTESIAN_POINT('Ctrl Pts',(3.47552596350473,-5.80629040584473,2.3687402618592));
#48307=CARTESIAN_POINT('Ctrl Pts',(3.63969370392998,-5.70802297443215,2.37771443378472));
#48308=CARTESIAN_POINT('Ctrl Pts',(3.7995540908287,-5.60287161391884,2.38668860571026));
#48309=CARTESIAN_POINT('Ctrl Pts',(3.95457002635816,-5.49123528057482,2.39566277763578));
#48310=CARTESIAN_POINT('Ctrl Pts',(4.10984646873757,-5.3794113405216,2.40465203080602));
#48311=CARTESIAN_POINT('Ctrl Pts',(4.26026199279593,-5.2610807871186,2.41364128397626));
#48312=CARTESIAN_POINT('Ctrl Pts',(4.40531210531596,-5.13668319587228,2.4226305371465));
#48313=CARTESIAN_POINT('Ctrl Pts',(4.5506972519056,-5.01199827336838,2.43164055352761));
#48314=CARTESIAN_POINT('Ctrl Pts',(4.69069200782386,-4.88121843270496,2.44065056990872));
#48315=CARTESIAN_POINT('Ctrl Pts',(4.82482635548035,-4.74482240336372,2.44966058628982));
#48316=CARTESIAN_POINT('Ctrl Pts',(4.95909489252592,-4.60828992202363,2.45867961638453));
#48317=CARTESIAN_POINT('Ctrl Pts',(5.08749114456103,-4.46613020390667,2.46769864647925));
#48318=CARTESIAN_POINT('Ctrl Pts',(5.20958400989011,-4.31885672879957,2.47671767657395));
#48319=CARTESIAN_POINT('Ctrl Pts',(5.33184918371774,-4.17137540803904,2.48574943513998));
#48320=CARTESIAN_POINT('Ctrl Pts',(5.44779302950886,-4.01876608561737,2.494781193706));
#48321=CARTESIAN_POINT('Ctrl Pts',(5.5570251635486,-3.86157485123462,2.50381295227203));
#48322=CARTESIAN_POINT('Ctrl Pts',(5.65253371598365,-3.72413262891281,2.51170998911167));
#48323=CARTESIAN_POINT('Ctrl Pts',(5.74291168395272,-3.58318802975742,2.51960702595129));
#48324=CARTESIAN_POINT('Ctrl Pts',(5.82792588108913,-3.4391232784725,2.52750406279092));
#48325=CARTESIAN_POINT('Ctrl Pts',(5.92109086185467,-3.28124623870097,2.53615823244789));
#48326=CARTESIAN_POINT('Ctrl Pts',(6.00789619768168,-3.11948068244951,2.54481240210485));
#48327=CARTESIAN_POINT('Ctrl Pts',(6.08802720130508,-2.9543550558742,2.55346657176182));
#48328=CARTESIAN_POINT('Ctrl Pts',(6.16808425728699,-2.78938181289679,2.56211275505388));
#48329=CARTESIAN_POINT('Ctrl Pts',(6.24147913375015,-2.62105495666394,2.57075893834593));
#48330=CARTESIAN_POINT('Ctrl Pts',(6.30794276905849,-2.4499279626721,2.57940512163799));
#48331=CARTESIAN_POINT('Ctrl Pts',(6.37639769764787,-2.27367389382561,2.58831035014502));
#48332=CARTESIAN_POINT('Ctrl Pts',(6.43749942211724,-2.09444956361584,2.59721557865208));
#48333=CARTESIAN_POINT('Ctrl Pts',(6.49100618115909,-1.91288466880639,2.6061208071591));
#48334=CARTESIAN_POINT('Ctrl Pts',(6.54285762426688,-1.73693677021995,2.61475053838488));
#48335=CARTESIAN_POINT('Ctrl Pts',(6.5875768975266,-1.55879127692548,2.62338026961067));
#48336=CARTESIAN_POINT('Ctrl Pts',(6.62499347012686,-1.37903970964452,2.63201000083646));
#48337=CARTESIAN_POINT('Ctrl Pts',(6.66420178404938,-1.19068050439851,2.64105297798411));
#48338=CARTESIAN_POINT('Ctrl Pts',(6.69539069388701,-1.00055794336212,2.65009595513175));
#48339=CARTESIAN_POINT('Ctrl Pts',(6.71842324907516,-0.809368918532445,
2.6591389322794));
#48340=CARTESIAN_POINT('Ctrl Pts',(6.7414558042633,-0.618179893702837,2.66818190942705));
#48341=CARTESIAN_POINT('Ctrl Pts',(6.75633192426425,-0.425924783021438,
2.6772248865747));
#48342=CARTESIAN_POINT('Ctrl Pts',(6.76297676298404,-0.233311601378899,
2.68626786372235));
#48343=CARTESIAN_POINT('Ctrl Pts',(6.76916879388631,-0.0538239082668467,
2.69469461361171));
#48344=CARTESIAN_POINT('Ctrl Pts',(6.76821062399756,0.125895236555421,2.70312136350109));
#48345=CARTESIAN_POINT('Ctrl Pts',(6.76011154818979,0.30525539476169,2.71154811339045));
#48346=CARTESIAN_POINT('Ctrl Pts',(6.75201056628867,0.484657764846474,2.71997684649028));
#48347=CARTESIAN_POINT('Ctrl Pts',(6.73676534253674,0.66370064882653,2.7284055795901));
#48348=CARTESIAN_POINT('Ctrl Pts',(6.71443720104782,0.841796931085577,2.73683431268992));
#48349=CARTESIAN_POINT('Ctrl Pts',(6.69210078749759,1.0199591939086,2.74526616844091));
#48350=CARTESIAN_POINT('Ctrl Pts',(6.66267626524027,1.19717382711612,2.75369802419192));
#48351=CARTESIAN_POINT('Ctrl Pts',(6.62627645457056,1.37286173652115,2.76212987994292));
#48352=CARTESIAN_POINT('Ctrl Pts',(6.58984306320376,1.54871172705679,2.77056951451442));
#48353=CARTESIAN_POINT('Ctrl Pts',(6.54642159402834,1.72303185506663,2.77900914908593));
#48354=CARTESIAN_POINT('Ctrl Pts',(6.49617561294783,1.89525497116927,2.78744878365744));
#48355=CARTESIAN_POINT('Ctrl Pts',(6.44590318059714,2.06756875164107,2.79589286115253));
#48356=CARTESIAN_POINT('Ctrl Pts',(6.38879917133256,2.23778300296788,2.8043369386476));
#48357=CARTESIAN_POINT('Ctrl Pts',(6.32507629851579,2.40534796192855,2.81278101614269));
#48358=CARTESIAN_POINT('Ctrl Pts',(6.2612863409453,2.57308932621288,2.82123398320654));
#48359=CARTESIAN_POINT('Ctrl Pts',(6.19086372552568,2.73817552016933,2.82968695027037));
#48360=CARTESIAN_POINT('Ctrl Pts',(6.11406878487783,2.90007791167454,2.83813991733422));
#48361=CARTESIAN_POINT('Ctrl Pts',(6.09319834879832,2.94407786120928,2.84043716644073));
#48362=CARTESIAN_POINT('Ctrl Pts',(6.07185752517465,2.98784280561122,2.84273441554726));
#48363=CARTESIAN_POINT('Ctrl Pts',(6.05005211393966,3.03136246902514,2.84503166465377));
#48364=CARTESIAN_POINT('Ctrl Pts',(5.97071873144858,3.18969757521933,2.85338961489284));
#48365=CARTESIAN_POINT('Ctrl Pts',(5.88508860599053,3.34507034491326,2.8617475651319));
#48366=CARTESIAN_POINT('Ctrl Pts',(5.79340883242674,3.49695626228866,2.87010551537097));
#48367=CARTESIAN_POINT('Ctrl Pts',(5.70226108570057,3.64796077059028,2.87841496359414));
#48368=CARTESIAN_POINT('Ctrl Pts',(5.60513388527962,3.79551847850857,2.88672441181733));
#48369=CARTESIAN_POINT('Ctrl Pts',(5.50231710724092,3.93913638395066,2.8950338600405));
#48370=CARTESIAN_POINT('Ctrl Pts',(5.39956497794379,4.08266398587391,2.90333808348051));
#48371=CARTESIAN_POINT('Ctrl Pts',(5.29113060003837,4.22225643876606,2.91164230692051));
#48372=CARTESIAN_POINT('Ctrl Pts',(5.1773477978745,4.35744865487181,2.91994653036052));
#48373=CARTESIAN_POINT('Ctrl Pts',(5.06361763577753,4.49257832613627,2.92824691196442));
#48374=CARTESIAN_POINT('Ctrl Pts',(4.9445442035622,4.62331155151054,2.93654729356831));
#48375=CARTESIAN_POINT('Ctrl Pts',(4.8205024599883,4.74921520182512,2.94484767517221));
#48376=CARTESIAN_POINT('Ctrl Pts',(4.69500339757764,4.87659804580412,2.95324557477381));
#48377=CARTESIAN_POINT('Ctrl Pts',(4.56441876193443,4.99903682580213,2.96164347437542));
#48378=CARTESIAN_POINT('Ctrl Pts',(4.42917678438174,5.11611982000948,2.97004137397701));
#48379=CARTESIAN_POINT('Ctrl Pts',(4.29554593048381,5.23180801664768,2.97833923027147));
#48380=CARTESIAN_POINT('Ctrl Pts',(4.15736837259501,5.34226711638402,2.98663708656591));
#48381=CARTESIAN_POINT('Ctrl Pts',(4.01509197128691,5.44713919981007,2.99493494286037));
#48382=CARTESIAN_POINT('Ctrl Pts',(3.87024253161636,5.55390787249001,3.00338286411553));
#48383=CARTESIAN_POINT('Ctrl Pts',(3.72114486015774,5.65488527325917,3.0118307853707));
#48384=CARTESIAN_POINT('Ctrl Pts',(3.56830396325748,5.74973876152656,3.02027870662586));
#48385=CARTESIAN_POINT('Ctrl Pts',(3.41546306635722,5.84459224979395,3.02872662788102));
#48386=CARTESIAN_POINT('Ctrl Pts',(3.25887927574339,5.93332164015267,3.03717454913619));
#48387=CARTESIAN_POINT('Ctrl Pts',(3.0990855038473,6.01564277861008,3.04562247039135));
#48388=CARTESIAN_POINT('Ctrl Pts',(3.09908550384726,6.0156427786101,1.04588102939738));
#48389=CARTESIAN_POINT('Ctrl Pts',(2.94511050341158,6.09496625398363,1.05400525660668));
#48390=CARTESIAN_POINT('Ctrl Pts',(2.78801560534586,6.16841149912689,1.06212948381596));
#48391=CARTESIAN_POINT('Ctrl Pts',(2.62829577678531,6.23573173811482,1.07025371102526));
#48392=CARTESIAN_POINT('Ctrl Pts',(2.46858314112875,6.30304894536888,1.07837757236398));
#48393=CARTESIAN_POINT('Ctrl Pts',(2.30624614327927,6.36424154462215,1.08650143370269));
#48394=CARTESIAN_POINT('Ctrl Pts',(2.14180121197924,6.41911026298538,1.09462529504141));
#48395=CARTESIAN_POINT('Ctrl Pts',(1.97735210139803,6.47398037580814,1.10274936284378));
#48396=CARTESIAN_POINT('Ctrl Pts',(1.81079529740787,6.52252617097112,1.11087343064615));
#48397=CARTESIAN_POINT('Ctrl Pts',(1.64266370095001,6.56459785254064,1.11899749844852));
#48398=CARTESIAN_POINT('Ctrl Pts',(1.47449585096053,6.60667860585558,1.12712331801056));
#48399=CARTESIAN_POINT('Ctrl Pts',(1.30475288709302,6.64228237665215,1.13524913757259));
#48400=CARTESIAN_POINT('Ctrl Pts',(1.13397920245994,6.67131022876229,1.14337495713463));
#48401=CARTESIAN_POINT('Ctrl Pts',(0.96313620896442,6.70034986188783,1.15150407457778));
#48402=CARTESIAN_POINT('Ctrl Pts',(0.791262021954657,6.72280820051437,1.15963319202093));
#48403=CARTESIAN_POINT('Ctrl Pts',(0.618907432297392,6.73863803674356,1.16776230946408));
#48404=CARTESIAN_POINT('Ctrl Pts',(0.446347403748565,6.75448674142305,1.17590111644831));
#48405=CARTESIAN_POINT('Ctrl Pts',(0.273306193277052,6.76369113041661,1.18403992343255));
#48406=CARTESIAN_POINT('Ctrl Pts',(0.100336820484199,6.7662560934726,1.19217873041679));
#48407=CARTESIAN_POINT('Ctrl Pts',(-0.0727451131579683,6.76882272569358,
1.20032283377813));
#48408=CARTESIAN_POINT('Ctrl Pts',(-0.245754751500726,6.76474133226017,
1.20846693713949));
#48409=CARTESIAN_POINT('Ctrl Pts',(-0.418143228922062,6.75406879148463,
1.21661104050084));
#48410=CARTESIAN_POINT('Ctrl Pts',(-0.590796825776929,6.74337983721089,
1.22476766882964));
#48411=CARTESIAN_POINT('Ctrl Pts',(-0.762826990860979,6.7260795249096,1.2329242971584));
#48412=CARTESIAN_POINT('Ctrl Pts',(-0.933693007081257,6.70227620801527,
1.2410809254872));
#48413=CARTESIAN_POINT('Ctrl Pts',(-1.04760000602917,6.68640784254145,1.24651850210436));
#48414=CARTESIAN_POINT('Ctrl Pts',(-1.16098986786002,6.66765049645239,1.25195607872154));
#48415=CARTESIAN_POINT('Ctrl Pts',(-1.27370620471547,6.64604856317416,1.2573936553387));
#48416=CARTESIAN_POINT('Ctrl Pts',(-1.44372401441086,6.61346488024396,1.26559552644534));
#48417=CARTESIAN_POINT('Ctrl Pts',(-1.61275339964681,6.57430259382322,1.27379739755197));
#48418=CARTESIAN_POINT('Ctrl Pts',(-1.78024430706333,6.52863072988269,1.28199926865861));
#48419=CARTESIAN_POINT('Ctrl Pts',(-1.9475318094701,6.48301433095859,1.29019117921456));
#48420=CARTESIAN_POINT('Ctrl Pts',(-2.11328420892936,6.43090418777637,1.29838308977052));
#48421=CARTESIAN_POINT('Ctrl Pts',(-2.27695920292253,6.37242071651161,1.30657500032648));
#48422=CARTESIAN_POINT('Ctrl Pts',(-2.44046892556389,6.31399629912014,1.31475863907439));
#48423=CARTESIAN_POINT('Ctrl Pts',(-2.6019050818716,6.24921148879263,1.3229422778223));
#48424=CARTESIAN_POINT('Ctrl Pts',(-2.76073810189435,6.17823713795034,1.33112591657022));
#48425=CARTESIAN_POINT('Ctrl Pts',(-2.91944323475257,6.10731993333925,1.33930296611926));
#48426=CARTESIAN_POINT('Ctrl Pts',(-3.0755490771151,6.0302232598561,1.34748001566831));
#48427=CARTESIAN_POINT('Ctrl Pts',(-3.22854365472601,5.9471669616321,1.35565706521736));
#48428=CARTESIAN_POINT('Ctrl Pts',(-3.3814463376797,5.86416055033988,1.36382920330368));
#48429=CARTESIAN_POINT('Ctrl Pts',(-3.53124116147165,5.77520181624719,1.37200134139002));
#48430=CARTESIAN_POINT('Ctrl Pts',(-3.67743844357896,5.68055767453228,1.38017347947634));
#48431=CARTESIAN_POINT('Ctrl Pts',(-3.82359233340284,5.58594162380075,1.38834319202009));
#48432=CARTESIAN_POINT('Ctrl Pts',(-3.96615050295292,5.48564371890684,1.39651290456383));
#48433=CARTESIAN_POINT('Ctrl Pts',(-4.10464990705188,5.37997566356382,1.40468261710758));
#48434=CARTESIAN_POINT('Ctrl Pts',(-4.24313025833367,5.27432214455873,1.41285120577617));
#48435=CARTESIAN_POINT('Ctrl Pts',(-4.37755266819308,5.16330016469292,1.42101979444476));
#48436=CARTESIAN_POINT('Ctrl Pts',(-4.50748503267875,5.04726338525909,1.42918838311336));
#48437=CARTESIAN_POINT('Ctrl Pts',(-4.63742359469937,4.93122107108418,1.43735736140861));
#48438=CARTESIAN_POINT('Ctrl Pts',(-4.76287141501455,4.81016372158861,1.44552633970388));
#48439=CARTESIAN_POINT('Ctrl Pts',(-4.88343129243093,4.68448372951666,1.45369531799913));
#48440=CARTESIAN_POINT('Ctrl Pts',(-5.00401925598966,4.55877445849866,1.46186619937435));
#48441=CARTESIAN_POINT('Ctrl Pts',(-5.11971675875143,4.42844066108668,1.47003708074955));
#48442=CARTESIAN_POINT('Ctrl Pts',(-5.23016511913173,4.29390985310798,1.47820796212477));
#48443=CARTESIAN_POINT('Ctrl Pts',(-5.34072043420266,4.15924876975989,1.48638675592247));
#48444=CARTESIAN_POINT('Ctrl Pts',(-5.44601622193107,4.02038283582922,1.49456554972017));
#48445=CARTESIAN_POINT('Ctrl Pts',(-5.54573504425719,3.87777150163566,1.50274434351788));
#48446=CARTESIAN_POINT('Ctrl Pts',(-5.64550296165731,3.73508995488,1.51092716402264));
#48447=CARTESIAN_POINT('Ctrl Pts',(-5.73968824483146,3.58865963579089,1.51910998452742));
#48448=CARTESIAN_POINT('Ctrl Pts',(-5.82801821818632,3.43896679956181,1.52729280503219));
#48449=CARTESIAN_POINT('Ctrl Pts',(-5.91647344082183,3.28906170333373,1.53548722853357));
#48450=CARTESIAN_POINT('Ctrl Pts',(-5.99905658974666,3.1358851631107,1.54368165203496));
#48451=CARTESIAN_POINT('Ctrl Pts',(-6.07554161380753,2.97994682819895,1.55187607553634));
#48452=CARTESIAN_POINT('Ctrl Pts',(-6.14724123871581,2.83376500686494,1.55955780275815));
#48453=CARTESIAN_POINT('Ctrl Pts',(-6.21358230576481,2.68515659461769,1.56723952997996));
#48454=CARTESIAN_POINT('Ctrl Pts',(-6.27441812645904,2.53455443310303,1.57492125720177));
#48455=CARTESIAN_POINT('Ctrl Pts',(-6.34885486612547,2.35028250643317,1.58432036981129));
#48456=CARTESIAN_POINT('Ctrl Pts',(-6.4152027678741,2.16264824857119,1.59371948242081));
#48457=CARTESIAN_POINT('Ctrl Pts',(-6.47319209011458,1.97232684017583,1.60311859503034));
#48458=CARTESIAN_POINT('Ctrl Pts',(-6.53096545521913,1.7827142047869,1.61248270455031));
#48459=CARTESIAN_POINT('Ctrl Pts',(-6.580442309698,1.59043454498714,1.62184681407032));
#48460=CARTESIAN_POINT('Ctrl Pts',(-6.62140321499279,1.39617637298556,1.63121092359029));
#48461=CARTESIAN_POINT('Ctrl Pts',(-6.66224919727079,1.20246322641746,1.64054876045569));
#48462=CARTESIAN_POINT('Ctrl Pts',(-6.6946268655054,1.00678280225882,1.64988659732106));
#48463=CARTESIAN_POINT('Ctrl Pts',(-6.71836691624296,0.809836390101164,
1.65922443418647));
#48464=CARTESIAN_POINT('Ctrl Pts',(-6.74199049957226,0.613856186417202,
1.66851646012795));
#48465=CARTESIAN_POINT('Ctrl Pts',(-6.75706093789863,0.416622543517127,
1.67780848606946));
#48466=CARTESIAN_POINT('Ctrl Pts',(-6.76346042492071,0.218842593046833,
1.68710051201094));
#48467=CARTESIAN_POINT('Ctrl Pts',(-6.76577431460309,0.147330456965178,
1.69046026926653));
#48468=CARTESIAN_POINT('Ctrl Pts',(-6.76695507065543,0.0757470404218229,
1.69382002652209));
#48469=CARTESIAN_POINT('Ctrl Pts',(-6.76699874199978,0.00412622993574791,
1.69717978377767));
#48470=CARTESIAN_POINT('',(-6.76699985285232,0.0014112039775177,1.30282021622242));
#48471=CARTESIAN_POINT('Ctrl Pts',(3.09908550384723,6.01564277861011,0.651473025530862));
#48472=CARTESIAN_POINT('Ctrl Pts',(2.94500347134394,6.09502139381515,0.659666922542915));
#48473=CARTESIAN_POINT('Ctrl Pts',(2.78765915579723,6.16858476961951,0.667860819554956));
#48474=CARTESIAN_POINT('Ctrl Pts',(2.62753232127271,6.23605347160103,0.676054716567009));
#48475=CARTESIAN_POINT('Ctrl Pts',(2.46757388614715,6.30345121927376,0.68423999636424));
#48476=CARTESIAN_POINT('Ctrl Pts',(2.30483908880748,6.36476691599561,0.692425276161489));
#48477=CARTESIAN_POINT('Ctrl Pts',(2.13983261521718,6.41976676981749,0.700610555958718));
#48478=CARTESIAN_POINT('Ctrl Pts',(1.97496591280073,6.47472003519975,0.708788902293637));
#48479=CARTESIAN_POINT('Ctrl Pts',(1.80783170699304,6.523367997734,0.716967248628545));
#48480=CARTESIAN_POINT('Ctrl Pts',(1.63895505841475,6.56552475560764,0.725145594963465));
#48481=CARTESIAN_POINT('Ctrl Pts',(1.47018691803207,6.60765442652895,0.733318686471199));
#48482=CARTESIAN_POINT('Ctrl Pts',(1.29967891415012,6.64330111242377,0.741491777978916));
#48483=CARTESIAN_POINT('Ctrl Pts',(1.12797173330277,6.6723285866982,0.749664869486651));
#48484=CARTESIAN_POINT('Ctrl Pts',(0.956339766498883,6.70134334587416,0.757834380880514));
#48485=CARTESIAN_POINT('Ctrl Pts',(0.783510024817833,6.72374460921029,0.76600389227438));
#48486=CARTESIAN_POINT('Ctrl Pts',(0.610033917780788,6.739447130081,0.774173403668243));
#48487=CARTESIAN_POINT('Ctrl Pts',(0.436567554066994,6.75514876901622,0.782342456219724));
#48488=CARTESIAN_POINT('Ctrl Pts',(0.262455256200104,6.76415237287407,0.790511508771234));
#48489=CARTESIAN_POINT('Ctrl Pts',(0.0882544452816943,6.7664244733011,0.798680561322712));
#48490=CARTESIAN_POINT('Ctrl Pts',(-0.0859486866819264,6.76869660400151,
0.806849722718346));
#48491=CARTESIAN_POINT('Ctrl Pts',(-0.260239972500771,6.76423704688248,
0.815018884113973));
#48492=CARTESIAN_POINT('Ctrl Pts',(-0.434061269699222,6.7530644757878,0.82318804550961));
#48493=CARTESIAN_POINT('Ctrl Pts',(-0.60791708683003,6.74188968588331,0.831358829254771));
#48494=CARTESIAN_POINT('Ctrl Pts',(-0.781302368596437,6.72399924954581,
0.839529612999922));
#48495=CARTESIAN_POINT('Ctrl Pts',(-0.953663358242854,6.69946379937566,
0.847700396745083));
#48496=CARTESIAN_POINT('Ctrl Pts',(-1.12609051198966,6.6749189307983,0.855874317003656));
#48497=CARTESIAN_POINT('Ctrl Pts',(-1.29749223279426,6.64372401867423,0.864048237262222));
#48498=CARTESIAN_POINT('Ctrl Pts',(-1.46732421200396,6.6060009579826,0.872222157520795));
#48499=CARTESIAN_POINT('Ctrl Pts',(-1.63735500078733,6.56823373773015,0.880405646375398));
#48500=CARTESIAN_POINT('Ctrl Pts',(-1.80581202409021,6.5239231819788,0.888589135230002));
#48501=CARTESIAN_POINT('Ctrl Pts',(-1.97216443620976,6.47324157100208,0.896772624084605));
#48502=CARTESIAN_POINT('Ctrl Pts',(-2.13862045505929,6.42252839477231,0.904961209736478));
#48503=CARTESIAN_POINT('Ctrl Pts',(-2.30296890969443,6.36543637371573,0.913149795388368));
#48504=CARTESIAN_POINT('Ctrl Pts',(-2.46469843567633,6.3021861779207,0.921338381040243));
#48505=CARTESIAN_POINT('Ctrl Pts',(-2.62667820868644,6.23883811395078,0.929539637039182));
#48506=CARTESIAN_POINT('Ctrl Pts',(-2.78603062590047,6.16931298165621,0.937740893038129));
#48507=CARTESIAN_POINT('Ctrl Pts',(-2.94226734446068,6.09387822931508,0.945942149037066));
#48508=CARTESIAN_POINT('Ctrl Pts',(-3.06518908596394,6.0345287293186,0.952394618592198));
#48509=CARTESIAN_POINT('Ctrl Pts',(-3.18618266288592,5.97152211066172,0.958847088147319));
#48510=CARTESIAN_POINT('Ctrl Pts',(-3.30502313505015,5.90500728846149,0.965299557702451));
#48511=CARTESIAN_POINT('Ctrl Pts',(-3.45525352507588,5.82092357943833,0.973456349746807));
#48512=CARTESIAN_POINT('Ctrl Pts',(-3.60252087704555,5.73096435441098,0.981613141791164));
#48513=CARTESIAN_POINT('Ctrl Pts',(-3.74632795874808,5.63536297193912,0.989769933835518));
#48514=CARTESIAN_POINT('Ctrl Pts',(-3.8899575636659,5.53987957410176,0.997916659329544));
#48515=CARTESIAN_POINT('Ctrl Pts',(-4.03013509782365,5.43876807929148,1.00606338482358));
#48516=CARTESIAN_POINT('Ctrl Pts',(-4.16638652809531,5.33230834615797,1.01421011031761));
#48517=CARTESIAN_POINT('Ctrl Pts',(-4.30249845329929,5.2259576149795,1.02234849454513));
#48518=CARTESIAN_POINT('Ctrl Pts',(-4.43469199163253,5.11426977035619,1.03048687877263));
#48519=CARTESIAN_POINT('Ctrl Pts',(-4.56252080310049,4.99756870100605,1.03862526300016));
#48520=CARTESIAN_POINT('Ctrl Pts',(-4.6902455927495,4.8809625981769,1.04675702454598));
#48521=CARTESIAN_POINT('Ctrl Pts',(-4.81361245903754,4.75935163870093,1.0548887860918));
#48522=CARTESIAN_POINT('Ctrl Pts',(-4.93220697932092,4.63310083131568,1.06302054763762));
#48523=CARTESIAN_POINT('Ctrl Pts',(-5.05072990096972,4.50692624486713,1.07114739982488));
#48524=CARTESIAN_POINT('Ctrl Pts',(-5.16448596484937,4.37611765467796,1.07927425201212));
#48525=CARTESIAN_POINT('Ctrl Pts',(-5.27309657678577,4.2410778691142,1.08740110419939));
#48526=CARTESIAN_POINT('Ctrl Pts',(-5.38191968449378,4.10577387931734,1.09554385650631));
#48527=CARTESIAN_POINT('Ctrl Pts',(-5.48557692486534,3.96622238171489,1.10368660881325));
#48528=CARTESIAN_POINT('Ctrl Pts',(-5.58372674065851,3.82286341446501,1.11182936112017));
#48529=CARTESIAN_POINT('Ctrl Pts',(-5.68164466879755,3.67984314550352,1.11995287545181));
#48530=CARTESIAN_POINT('Ctrl Pts',(-5.77408096657034,3.53303368568106,1.12807638978344));
#48531=CARTESIAN_POINT('Ctrl Pts',(-5.86073894005466,3.38290231554608,1.13619990411507));
#48532=CARTESIAN_POINT('Ctrl Pts',(-5.94740229380722,3.23276162431794,1.14432392280522));
#48533=CARTESIAN_POINT('Ctrl Pts',(-6.02828642574991,3.07929892872288,1.15244794149537));
#48534=CARTESIAN_POINT('Ctrl Pts',(-6.10313995500485,2.92300730235547,1.16057196018551));
#48535=CARTESIAN_POINT('Ctrl Pts',(-6.17801236954316,2.7666762441579,1.16869802853712));
#48536=CARTESIAN_POINT('Ctrl Pts',(-6.24685099393633,2.60751516382964,1.17682409688876));
#48537=CARTESIAN_POINT('Ctrl Pts',(-6.30945208222826,2.44603831165121,1.18495016524038));
#48538=CARTESIAN_POINT('Ctrl Pts',(-6.37228696229546,2.28395840350418,1.19310658143415));
#48539=CARTESIAN_POINT('Ctrl Pts',(-6.42883749442711,2.11954573955337,1.20126299762787));
#48540=CARTESIAN_POINT('Ctrl Pts',(-6.47894796318552,1.95333619490711,1.20941941382164));
#48541=CARTESIAN_POINT('Ctrl Pts',(-6.52894924828666,1.78748879746097,1.21755805833271));
#48542=CARTESIAN_POINT('Ctrl Pts',(-6.57253845972189,1.61985270788154,1.2256967028438));
#48543=CARTESIAN_POINT('Ctrl Pts',(-6.60961217372183,1.45097067957562,1.23383534735487));
#48544=CARTESIAN_POINT('Ctrl Pts',(-6.64680731991122,1.28153549076212,1.24200064938998));
#48545=CARTESIAN_POINT('Ctrl Pts',(-6.67744416759231,1.11084655455454,1.25016595142508));
#48546=CARTESIAN_POINT('Ctrl Pts',(-6.70147071035139,0.939456927326899,
1.25833125346018));
#48547=CARTESIAN_POINT('Ctrl Pts',(-6.72549725311047,0.768067300099262,
1.26649655549529));
#48548=CARTESIAN_POINT('Ctrl Pts',(-6.74291351265852,0.595977351140993,
1.27466185753042));
#48549=CARTESIAN_POINT('Ctrl Pts',(-6.75371999706329,0.423739544139386,
1.28282715956553));
#48550=CARTESIAN_POINT('Ctrl Pts',(-6.7625400282018,0.283162575341534,1.28949151177365));
#48551=CARTESIAN_POINT('Ctrl Pts',(-6.76697046679597,0.1423230389344,1.29615586398178));
#48552=CARTESIAN_POINT('Ctrl Pts',(-6.76699985285218,0.00141120466605954,
1.30282021618987));
#48553=CARTESIAN_POINT('Ctrl Pts',(-6.76699985285232,0.00141120397761236,
1.30282021622243));
#48554=CARTESIAN_POINT('Ctrl Pts',(-6.76703593212785,-0.171595998423697,
1.31100250224065));
#48555=CARTESIAN_POINT('Ctrl Pts',(-6.76043302341163,-0.344846684814409,
1.31918478825889));
#48556=CARTESIAN_POINT('Ctrl Pts',(-6.74716121089084,-0.517788175077523,
1.32736707427711));
#48557=CARTESIAN_POINT('Ctrl Pts',(-6.7339035463615,-0.690545306593661,
1.33554063783089));
#48558=CARTESIAN_POINT('Ctrl Pts',(-6.71399116002272,-0.862993539468723,
1.34371420138467));
#48559=CARTESIAN_POINT('Ctrl Pts',(-6.68744612489619,-1.03457881604588,
1.35188776493845));
#48560=CARTESIAN_POINT('Ctrl Pts',(-6.66092390272815,-1.20601663123258,
1.36005430408391));
#48561=CARTESIAN_POINT('Ctrl Pts',(-6.62778043765355,-1.37659261032166,
1.36822084322936));
#48562=CARTESIAN_POINT('Ctrl Pts',(-6.58808971705167,-1.54575641033057,
1.37638738237482));
#48563=CARTESIAN_POINT('Ctrl Pts',(-6.54842490917863,-1.71480976901683,
1.38454858986311));
#48564=CARTESIAN_POINT('Ctrl Pts',(-6.50222144160911,-1.8824524327505,1.39270979735142));
#48565=CARTESIAN_POINT('Ctrl Pts',(-6.44960463395322,-2.04814283332223,
1.40087100483971));
#48566=CARTESIAN_POINT('Ctrl Pts',(-6.39601677912313,-2.21689106279759,
1.40918282803092));
#48567=CARTESIAN_POINT('Ctrl Pts',(-6.33577661045198,-2.38361388714914,
1.41749465122212));
#48568=CARTESIAN_POINT('Ctrl Pts',(-6.26907034096874,-2.54775313953022,
1.42580647441332));
#48569=CARTESIAN_POINT('Ctrl Pts',(-6.20360850721721,-2.70883029966387,
1.43396323677059));
#48570=CARTESIAN_POINT('Ctrl Pts',(-6.13191986236707,-2.86741909194896,
1.44211999912783));
#48571=CARTESIAN_POINT('Ctrl Pts',(-6.05422965113859,-3.02301047488663,
1.4502767614851));
#48572=CARTESIAN_POINT('Ctrl Pts',(-5.97653869147967,-3.17860335671747,
1.45843360242072));
#48573=CARTESIAN_POINT('Ctrl Pts',(-5.89284621213306,-3.33119844676367,
1.46659044335637));
#48574=CARTESIAN_POINT('Ctrl Pts',(-5.80342409808935,-3.48031000597875,
1.47474728429199));
#48575=CARTESIAN_POINT('Ctrl Pts',(-5.71398439523565,-3.62945089457071,
1.48290572963081));
#48576=CARTESIAN_POINT('Ctrl Pts',(-5.61881300015372,-3.77510657663525,
1.49106417496961));
#48577=CARTESIAN_POINT('Ctrl Pts',(-5.51822591717691,-3.91681908275032,
1.49922262030843));
#48578=CARTESIAN_POINT('Ctrl Pts',(-5.41431940631598,-4.06320817785083,
1.50765029873511));
#48579=CARTESIAN_POINT('Ctrl Pts',(-5.30463388482756,-4.20538904208645,
1.51607797716176));
#48580=CARTESIAN_POINT('Ctrl Pts',(-5.18956329734131,-4.34289325022939,
1.52450565558844));
#48581=CARTESIAN_POINT('Ctrl Pts',(-5.07800877693082,-4.47619591539258,
1.53267582005531));
#48582=CARTESIAN_POINT('Ctrl Pts',(-4.96139372600185,-4.60510328713949,
1.54084598452221));
#48583=CARTESIAN_POINT('Ctrl Pts',(-4.84011482850923,-4.72922588240878,
1.54901614898908));
#48584=CARTESIAN_POINT('Ctrl Pts',(-4.71310207903707,-4.85921677466381,
1.55757258439566));
#48585=CARTESIAN_POINT('Ctrl Pts',(-4.58097411048328,-4.98395914907564,
1.56612901980223));
#48586=CARTESIAN_POINT('Ctrl Pts',(-4.44422528968739,-5.10305306404931,
1.57468545520881));
#48587=CARTESIAN_POINT('Ctrl Pts',(-4.30747646889149,-5.22214697902299,
1.58324189061539));
#48588=CARTESIAN_POINT('Ctrl Pts',(-4.16610718824954,-5.33559220394104,
1.59179832602198));
#48589=CARTESIAN_POINT('Ctrl Pts',(-4.02064581935871,-5.4430410796974,1.60035476142856));
#48590=CARTESIAN_POINT('Ctrl Pts',(-3.88205876894149,-5.54541205884647,
1.60850683062828));
#48591=CARTESIAN_POINT('Ctrl Pts',(-3.73934588974453,-5.6426443928679,1.61665889982797));
#48592=CARTESIAN_POINT('Ctrl Pts',(-3.59292772261526,-5.73438395820011,
1.62481096902769));
#48593=CARTESIAN_POINT('Ctrl Pts',(-3.44667627812929,-5.82601906202233,
1.63295375567353));
#48594=CARTESIAN_POINT('Ctrl Pts',(-3.29672825103698,-5.91217365526322,
1.64109654231937));
#48595=CARTESIAN_POINT('Ctrl Pts',(-3.14353663765987,-5.99253422248802,
1.64923932896521));
#48596=CARTESIAN_POINT('Ctrl Pts',(-2.99048726144911,-6.07282017558013,
1.65737455509991));
#48597=CARTESIAN_POINT('Ctrl Pts',(-2.83420061636461,-6.14732264439639,
1.6655097812346));
#48598=CARTESIAN_POINT('Ctrl Pts',(-2.67515802192827,-6.21577175881747,
1.6736450073693));
#48599=CARTESIAN_POINT('Ctrl Pts',(-2.51622968654349,-6.28417169816743,
1.68177438901168));
#48600=CARTESIAN_POINT('Ctrl Pts',(-2.35454967862933,-6.34652679859568,
1.68990377065407));
#48601=CARTESIAN_POINT('Ctrl Pts',(-2.19062322316334,-6.40261344250436,
1.69803315229645));
#48602=CARTESIAN_POINT('Ctrl Pts',(-2.02678011070006,-6.45867157100774,
1.7061584008227));
#48603=CARTESIAN_POINT('Ctrl Pts',(-1.86069317044212,-6.50846747201788,
1.71428364934896));
#48604=CARTESIAN_POINT('Ctrl Pts',(-1.69288687471926,-6.551825930945,1.72240889787521));
#48605=CARTESIAN_POINT('Ctrl Pts',(-1.52467828578781,-6.59528833599336,
1.7305536256009));
#48606=CARTESIAN_POINT('Ctrl Pts',(-1.35474243399278,-6.63228226671296,
1.73869835332659));
#48607=CARTESIAN_POINT('Ctrl Pts',(-1.18362257516338,-6.66268163726616,
1.74684308105228));
#48608=CARTESIAN_POINT('Ctrl Pts',(-1.01294189042843,-6.69300298872721,
1.75496690557334));
#48609=CARTESIAN_POINT('Ctrl Pts',(-0.841083633217064,-6.71676353994614,
1.76309073009443));
#48610=CARTESIAN_POINT('Ctrl Pts',(-0.668596442072254,-6.73388949995828,
1.7712145546155));
#48611=CARTESIAN_POINT('Ctrl Pts',(-0.496083192992632,-6.75101804721847,
1.77933960641662));
#48612=CARTESIAN_POINT('Ctrl Pts',(-0.322941184776123,-6.76150997075938,
1.78746465821772));
#48613=CARTESIAN_POINT('Ctrl Pts',(-0.149723408568824,-6.76534344293965,
1.79558971001885));
#48614=CARTESIAN_POINT('Ctrl Pts',(0.0235534855205549,-6.76917822345421,
1.80371753483706));
#48615=CARTESIAN_POINT('Ctrl Pts',(0.196905833599724,-6.76635001921679,
1.81184535965528));
#48616=CARTESIAN_POINT('Ctrl Pts',(0.369781457612505,-6.7568891269286,1.8199731844735));
#48617=CARTESIAN_POINT('Ctrl Pts',(0.543322254846379,-6.74739183198253,
1.82813228270834));
#48618=CARTESIAN_POINT('Ctrl Pts',(0.71638228217314,-6.73121073379521,1.83629138094319));
#48619=CARTESIAN_POINT('Ctrl Pts',(0.888409896509298,-6.70842879188446,
1.84445047917804));
#48620=CARTESIAN_POINT('Ctrl Pts',(1.06008050677724,-6.68569412869681,1.85259264506586));
#48621=CARTESIAN_POINT('Ctrl Pts',(1.23072263383571,-6.65638610654844,1.86073481095369));
#48622=CARTESIAN_POINT('Ctrl Pts',(1.39980035596695,-6.62063803295685,1.86887697684152));
#48623=CARTESIAN_POINT('Ctrl Pts',(1.56940549599356,-6.58477844749073,1.87704454124987));
#48624=CARTESIAN_POINT('Ctrl Pts',(1.73743610402486,-6.54243868313282,1.88521210565824));
#48625=CARTESIAN_POINT('Ctrl Pts',(1.90336891080001,-6.49380287577318,1.89337967006659));
#48626=CARTESIAN_POINT('Ctrl Pts',(2.06930171757522,-6.44516706841352,1.90154723447495));
#48627=CARTESIAN_POINT('Ctrl Pts',(2.23313639867561,-6.39023539501033,1.90971479888331));
#48628=CARTESIAN_POINT('Ctrl Pts',(2.3943724109838,-6.32923927162812,1.91788236329167));
#48629=CARTESIAN_POINT('Ctrl Pts',(2.55628567234072,-6.26798694266289,1.9260842343983));
#48630=CARTESIAN_POINT('Ctrl Pts',(2.71609718244165,-6.20042290644401,1.93428610550492));
#48631=CARTESIAN_POINT('Ctrl Pts',(2.87327686873585,-6.12670947863431,1.94248797661156));
#48632=CARTESIAN_POINT('Ctrl Pts',(3.03026567221649,-6.05308557019464,1.9506798871675));
#48633=CARTESIAN_POINT('Ctrl Pts',(3.18462869154788,-5.97332729029976,1.95887179772344));
#48634=CARTESIAN_POINT('Ctrl Pts',(3.33585230157968,-5.88764625483271,1.96706370827938));
#48635=CARTESIAN_POINT('Ctrl Pts',(3.48692321308562,-5.80205173606637,1.97524734702734));
#48636=CARTESIAN_POINT('Ctrl Pts',(3.63486071542537,-5.71054654706401,1.9834309857753));
#48637=CARTESIAN_POINT('Ctrl Pts',(3.77917237523593,-5.61338980993246,1.99161462452325));
#48638=CARTESIAN_POINT('Ctrl Pts',(3.9233678400085,-5.51631130023436,1.99979167407241));
#48639=CARTESIAN_POINT('Ctrl Pts',(4.06394297796849,-5.4135905055032,2.00796872362158));
#48640=CARTESIAN_POINT('Ctrl Pts',(4.20043109097176,-5.30553179709611,2.01614577317073));
#48641=CARTESIAN_POINT('Ctrl Pts',(4.33683722375847,-5.19753799306875,2.02431791125707));
#48642=CARTESIAN_POINT('Ctrl Pts',(4.4691609387328,-5.08421288525191,2.03249004934339));
#48643=CARTESIAN_POINT('Ctrl Pts',(4.59696557014832,-4.96590339685248,2.04066218742972));
#48644=CARTESIAN_POINT('Ctrl Pts',(4.72473226833609,-4.84762902346193,2.04883189997347));
#48645=CARTESIAN_POINT('Ctrl Pts',(4.84798228667743,-4.72437345802782,2.05700161251722));
#48646=CARTESIAN_POINT('Ctrl Pts',(4.96631288172423,-4.59652318179948,2.06517132506097));
#48647=CARTESIAN_POINT('Ctrl Pts',(5.08462719849755,-4.46869049342963,2.07333991372958));
#48648=CARTESIAN_POINT('Ctrl Pts',(5.19802319349817,-4.33626461754554,2.08150850239818));
#48649=CARTESIAN_POINT('Ctrl Pts',(5.30613580032696,-4.19966806646533,2.08967709106679));
#48650=CARTESIAN_POINT('Ctrl Pts',(5.41425356392816,-4.06306499998096,2.09784606936205));
#48651=CARTESIAN_POINT('Ctrl Pts',(5.51708721291567,-3.92229114543175,2.10601504765731));
#48652=CARTESIAN_POINT('Ctrl Pts',(5.61431270765535,-3.77780118860954,2.11418402595257));
#48653=CARTESIAN_POINT('Ctrl Pts',(5.71156085246089,-3.63327757079085,2.12235490732784));
#48654=CARTESIAN_POINT('Ctrl Pts',(5.80319803940902,-3.48503642649626,2.13052578870311));
#48655=CARTESIAN_POINT('Ctrl Pts',(5.888944200231,-3.33356043991492,2.13869667007839));
#48656=CARTESIAN_POINT('Ctrl Pts',(5.97477339491605,-3.18193776879156,2.14687546387608));
#48657=CARTESIAN_POINT('Ctrl Pts',(6.05469998805779,-3.0270743120676,2.15505425767378));
#48658=CARTESIAN_POINT('Ctrl Pts',(6.12849001961643,-2.86947714391696,2.16323305147148));
#48659=CARTESIAN_POINT('Ctrl Pts',(6.20231638059613,-2.711802385152,2.17141587197627));
#48660=CARTESIAN_POINT('Ctrl Pts',(6.27000001694408,-2.5513915648,2.17959869248106));
#48661=CARTESIAN_POINT('Ctrl Pts',(6.33135566415787,-2.38877049000863,2.18778151298585));
#48662=CARTESIAN_POINT('Ctrl Pts',(6.39279831185822,-2.22591882336021,2.19597593648723));
#48663=CARTESIAN_POINT('Ctrl Pts',(6.44789492419247,-2.06085098194257,2.20417035998862));
#48664=CARTESIAN_POINT('Ctrl Pts',(6.49651018178799,-1.89410782637236,2.21236478349));
#48665=CARTESIAN_POINT('Ctrl Pts',(6.54208375357042,-1.7377972040399,2.22004651071159));
#48666=CARTESIAN_POINT('Ctrl Pts',(6.58196205937282,-1.58001470154794,2.22772823793315));
#48667=CARTESIAN_POINT('Ctrl Pts',(6.61607479780713,-1.42121190180121,2.23540996515473));
#48668=CARTESIAN_POINT('Ctrl Pts',(6.65558914655382,-1.23726333891385,2.2443080619462));
#48669=CARTESIAN_POINT('Ctrl Pts',(6.68745532321374,-1.05153737755717,2.25320615873768));
#48670=CARTESIAN_POINT('Ctrl Pts',(6.71153051444414,-0.864665920275071,
2.26210425552915));
#48671=CARTESIAN_POINT('Ctrl Pts',(6.73556882002407,-0.678080769140777,
2.27098871952805));
#48672=CARTESIAN_POINT('Ctrl Pts',(6.75183992159552,-0.490353885417766,
2.27987318352692));
#48673=CARTESIAN_POINT('Ctrl Pts',(6.76025210269091,-0.302126642425282,
2.28875764752581));
#48674=CARTESIAN_POINT('Ctrl Pts',(6.76864382875009,-0.114357092274315,
2.29762050808671));
#48675=CARTESIAN_POINT('Ctrl Pts',(6.76921476013823,0.0739101251375437,
2.30648336864763));
#48676=CARTESIAN_POINT('Ctrl Pts',(6.76192497390255,0.262029859582791,2.31534622920853));
#48677=CARTESIAN_POINT('Ctrl Pts',(6.75464621330479,0.449865067155732,2.32419568489193));
#48678=CARTESIAN_POINT('Ctrl Pts',(6.73953045916144,0.637552973558179,2.33304514057532));
#48679=CARTESIAN_POINT('Ctrl Pts',(6.71658963936422,0.82444685479736,2.34189459625873));
#48680=CARTESIAN_POINT('Ctrl Pts',(6.69370541990664,1.01087962535048,2.35072221827612));
#48681=CARTESIAN_POINT('Ctrl Pts',(6.66303469078023,1.19652201798138,2.35954984029351));
#48682=CARTESIAN_POINT('Ctrl Pts',(6.6246410713492,1.38073157267928,2.3683774623109));
#48683=CARTESIAN_POINT('Ctrl Pts',(6.58724279776656,1.56016553658314,2.37697623023597));
#48684=CARTESIAN_POINT('Ctrl Pts',(6.54251707201548,1.73823975977284,2.38557499816104));
#48685=CARTESIAN_POINT('Ctrl Pts',(6.49057015165411,1.91436362963172,2.3941737660861));
#48686=CARTESIAN_POINT('Ctrl Pts',(6.44079222121798,2.08313362948909,2.40241350135111));
#48687=CARTESIAN_POINT('Ctrl Pts',(6.38443398140809,2.24993892942386,2.41065323661612));
#48688=CARTESIAN_POINT('Ctrl Pts',(6.32168608733571,2.41424398377341,2.41889297188114));
#48689=CARTESIAN_POINT('Ctrl Pts',(6.25891882191981,2.57859976189143,2.42713525089275));
#48690=CARTESIAN_POINT('Ctrl Pts',(6.18975809724076,2.74045342707464,2.43537752990436));
#48691=CARTESIAN_POINT('Ctrl Pts',(6.11444271380599,2.89928944736205,2.44361980891597));
#48692=CARTESIAN_POINT('Ctrl Pts',(6.03909104120139,3.05820199952183,2.45186605930035));
#48693=CARTESIAN_POINT('Ctrl Pts',(5.957578951542,3.21409369134424,2.46011230968473));
#48694=CARTESIAN_POINT('Ctrl Pts',(5.87019123532304,3.36647350512915,2.46835856006911));
#48695=CARTESIAN_POINT('Ctrl Pts',(5.78269832855263,3.51903674190916,2.47661473664978));
#48696=CARTESIAN_POINT('Ctrl Pts',(5.68931584344398,3.66807935094485,2.48487091323046));
#48697=CARTESIAN_POINT('Ctrl Pts',(5.59037252578222,3.81313834301607,2.49312708981114));
#48698=CARTESIAN_POINT('Ctrl Pts',(5.4913610582128,3.95829724842301,2.50138895305854));
#48699=CARTESIAN_POINT('Ctrl Pts',(5.38678133114394,4.09946678412285,2.50965081630594));
#48700=CARTESIAN_POINT('Ctrl Pts',(5.2770024321496,4.23621698347561,2.51791267955333));
#48701=CARTESIAN_POINT('Ctrl Pts',(5.16706766260978,4.3731613488144,2.5261862734807));
#48702=CARTESIAN_POINT('Ctrl Pts',(5.05191920593846,4.50567357863123,2.53445986740805));
#48703=CARTESIAN_POINT('Ctrl Pts',(4.93196376787249,4.63335973051878,2.54273346133542));
#48704=CARTESIAN_POINT('Ctrl Pts',(4.88264872300639,4.68585295975988,2.54613482989619));
#48705=CARTESIAN_POINT('Ctrl Pts',(4.83252163703819,4.73753098419086,2.54953619845697));
#48706=CARTESIAN_POINT('Ctrl Pts',(4.78161236962705,4.78836842219034,2.55293756701775));
#48707=CARTESIAN_POINT('Ctrl Pts',(4.65537813259575,4.91442455155208,2.56137157494924));
#48708=CARTESIAN_POINT('Ctrl Pts',(4.5240411366395,5.03560058765171,2.56980558288074));
#48709=CARTESIAN_POINT('Ctrl Pts',(4.38800578918041,5.15147495326525,2.57823959081223));
#48710=CARTESIAN_POINT('Ctrl Pts',(4.25208352366071,5.26725299613449,2.58666658781611));
#48711=CARTESIAN_POINT('Ctrl Pts',(4.11147094151205,5.37773793266703,2.59509358481999));
#48712=CARTESIAN_POINT('Ctrl Pts',(3.96660893953291,5.48254525934968,2.60352058182387));
#48713=CARTESIAN_POINT('Ctrl Pts',(3.82187371122521,5.58726086557137,2.61194020407568));
#48714=CARTESIAN_POINT('Ctrl Pts',(3.67289674888787,5.68630857373254,2.62035982632747));
#48715=CARTESIAN_POINT('Ctrl Pts',(3.52015165274744,5.77934436953358,2.62877944857928));
#48716=CARTESIAN_POINT('Ctrl Pts',(3.38272405843464,5.86305039954687,2.63635473878712));
#48717=CARTESIAN_POINT('Ctrl Pts',(3.2422467575683,5.94189023337968,2.64393002899497));
#48718=CARTESIAN_POINT('Ctrl Pts',(3.09908550384727,6.01564277861009,2.65150531920281));
#48719=CARTESIAN_POINT('Origin',(0.,0.,-63.6971797838103));
#48720=CARTESIAN_POINT('',(3.09908550384713,6.01564277861016,5.04570102894007));
#48721=CARTESIAN_POINT('',(3.09908550384716,6.01564277861015,4.65139679042609));
#48722=CARTESIAN_POINT('',(3.09908550384721,6.01564277861012,-63.6971797838103));
#48723=CARTESIAN_POINT('',(-6.76699851873671,-0.00447743399645792,3.6971797838519));
#48724=CARTESIAN_POINT('Ctrl Pts',(-6.76699851873671,-0.00447743399636642,
3.69717978385191));
#48725=CARTESIAN_POINT('Ctrl Pts',(-6.76686776413152,-0.202094243171143,
3.70644559443041));
#48726=CARTESIAN_POINT('Ctrl Pts',(-6.75807649647211,-0.399395897026799,
3.71571140500891));
#48727=CARTESIAN_POINT('Ctrl Pts',(-6.74073150822531,-0.595674184448696,
3.7249772155874));
#48728=CARTESIAN_POINT('Ctrl Pts',(-6.72332256944408,-0.79267614496839,
3.73427718897591));
#48729=CARTESIAN_POINT('Ctrl Pts',(-6.69729681504176,-0.988647016979515,
3.74357716236443));
#48730=CARTESIAN_POINT('Ctrl Pts',(-6.66281218223202,-1.18288749435462,
3.75287713575294));
#48731=CARTESIAN_POINT('Ctrl Pts',(-6.62816067813818,-1.37806790222179,
3.76222211175204));
#48732=CARTESIAN_POINT('Ctrl Pts',(-6.58496831618429,-1.57150096816226,
3.77156708775114));
#48733=CARTESIAN_POINT('Ctrl Pts',(-6.53344434709676,-1.76249651443324,
3.78091206375024));
#48734=CARTESIAN_POINT('Ctrl Pts',(-6.50274784322497,-1.87628618610319,
3.78647953258112));
#48735=CARTESIAN_POINT('Ctrl Pts',(-6.46909501792016,-1.98921105644742,
3.79204700141197));
#48736=CARTESIAN_POINT('Ctrl Pts',(-6.43253814042731,-2.10112876139182,
3.79761447024285));
#48737=CARTESIAN_POINT('Ctrl Pts',(-6.37387008642234,-2.28073912223503,
3.80654938439423));
#48738=CARTESIAN_POINT('Ctrl Pts',(-6.30763797513442,-2.45800506845748,
3.8154842985456));
#48739=CARTESIAN_POINT('Ctrl Pts',(-6.23404071453184,-2.63230419396379,
3.82441921269698));
#48740=CARTESIAN_POINT('Ctrl Pts',(-6.16055367844835,-2.80634227663877,
3.83334074528216));
#48741=CARTESIAN_POINT('Ctrl Pts',(-6.07972360312658,-2.97742216707847,
3.84226227786734));
#48742=CARTESIAN_POINT('Ctrl Pts',(-5.9917982268079,-3.14493926956019,3.85118381045251));
#48743=CARTESIAN_POINT('Ctrl Pts',(-5.90408727843435,-3.31204783983466,
3.86008358565682));
#48744=CARTESIAN_POINT('Ctrl Pts',(-5.80931568407483,-3.47561073504441,
3.86898336086114));
#48745=CARTESIAN_POINT('Ctrl Pts',(-5.70777771719143,-3.63504642764477,
3.87788313606545));
#48746=CARTESIAN_POINT('Ctrl Pts',(-5.60639602489657,-3.79423673669034,
3.88676921384454));
#48747=CARTESIAN_POINT('Ctrl Pts',(-5.49826887131707,-3.94931229701519,
3.89565529162364));
#48748=CARTESIAN_POINT('Ctrl Pts',(-5.38373602133471,-4.09971650880682,
3.90454136940274));
#48749=CARTESIAN_POINT('Ctrl Pts',(-5.26949589102941,-4.24973632195375,
3.91340473640655));
#48750=CARTESIAN_POINT('Ctrl Pts',(-5.14888288868192,-4.39510840494872,
3.9222681034104));
#48751=CARTESIAN_POINT('Ctrl Pts',(-5.02227914829755,-4.53530607088162,
3.93113147041421));
#48752=CARTESIAN_POINT('Ctrl Pts',(-4.90207127817228,-4.66842111761849,
3.93954707066767));
#48753=CARTESIAN_POINT('Ctrl Pts',(-4.77646309170414,-4.79687137201919,
3.9479626709211));
#48754=CARTESIAN_POINT('Ctrl Pts',(-4.64581777032901,-4.92023030405033,
3.95637827117456));
#48755=CARTESIAN_POINT('Ctrl Pts',(-4.51835837990954,-5.04058099180545,
3.96458864768887));
#48756=CARTESIAN_POINT('Ctrl Pts',(-4.38622634044855,-5.15596923144747,
3.97279902420316));
#48757=CARTESIAN_POINT('Ctrl Pts',(-4.24985108100136,-5.26602836958856,
3.98100940071744));
#48758=CARTESIAN_POINT('Ctrl Pts',(-4.11344336853475,-5.37611369834049,
3.98922173104292));
#48759=CARTESIAN_POINT('Ctrl Pts',(-3.97279070135292,-5.4808671755143,3.99743406136838));
#48760=CARTESIAN_POINT('Ctrl Pts',(-3.8283542946149,-5.57996347612631,4.00564639169386));
#48761=CARTESIAN_POINT('Ctrl Pts',(-3.6838577994082,-5.67910100280515,4.01386213851497));
#48762=CARTESIAN_POINT('Ctrl Pts',(-3.53557472192143,-5.77257646303051,
4.02207788533611));
#48763=CARTESIAN_POINT('Ctrl Pts',(-3.38399391700499,-5.86010871654044,
4.03029363215722));
#48764=CARTESIAN_POINT('Ctrl Pts',(-3.23224285304114,-5.94773928829131,
4.03851860709418));
#48765=CARTESIAN_POINT('Ctrl Pts',(-3.07718697174119,-6.02941314203681,
4.04674358203113));
#48766=CARTESIAN_POINT('Ctrl Pts',(-2.91933917756931,-6.1048953935599,4.05496855696809));
#48767=CARTESIAN_POINT('Ctrl Pts',(-2.76139025085872,-6.18042600630188,
4.0631988016182));
#48768=CARTESIAN_POINT('Ctrl Pts',(-2.60064617143321,-6.24975696832185,
4.07142904626831));
#48769=CARTESIAN_POINT('Ctrl Pts',(-2.43763827545052,-6.31270216611386,
4.07965929091841));
#48770=CARTESIAN_POINT('Ctrl Pts',(-2.27440686957213,-6.37573367183904,
4.08790082055022));
#48771=CARTESIAN_POINT('Ctrl Pts',(-2.10890578288484,-6.43236180945014,
4.09614235018204));
#48772=CARTESIAN_POINT('Ctrl Pts',(-1.94168086722592,-6.48245049420733,
4.10438387981385));
#48773=CARTESIAN_POINT('Ctrl Pts',(-1.86891776461991,-6.50424514181726,
4.10796994391122));
#48774=CARTESIAN_POINT('Ctrl Pts',(-1.79582841503726,-6.52480232806352,
4.11155600800859));
#48775=CARTESIAN_POINT('Ctrl Pts',(-1.72245825573738,-6.54411388632886,
4.11514207210595));
#48776=CARTESIAN_POINT('Ctrl Pts',(-1.54960436937608,-6.58961028336151,
4.12359053564869));
#48777=CARTESIAN_POINT('Ctrl Pts',(-1.37479715599412,-6.62829333036955,
4.13203899919145));
#48778=CARTESIAN_POINT('Ctrl Pts',(-1.19860077262665,-6.66000339248103,
4.1404874627342));
#48779=CARTESIAN_POINT('Ctrl Pts',(-1.02256534778356,-6.6916844868878,4.14892820845551));
#48780=CARTESIAN_POINT('Ctrl Pts',(-0.845143609124331,-6.71640523485003,
4.15736895417682));
#48781=CARTESIAN_POINT('Ctrl Pts',(-0.666912211242663,-6.73405651167968,
4.16580969989813));
#48782=CARTESIAN_POINT('Ctrl Pts',(-0.488816221044837,-6.75169437831033,
4.17424403293435));
#48783=CARTESIAN_POINT('Ctrl Pts',(-0.309912128539771,-6.76227344797985,
4.18267836597059));
#48784=CARTESIAN_POINT('Ctrl Pts',(-0.130784456218596,-6.76573605944036,
4.19111269900681));
#48785=CARTESIAN_POINT('Ctrl Pts',(0.0482346374308115,-6.76919657203057,
4.19954191955166));
#48786=CARTESIAN_POINT('Ctrl Pts',(0.227476708134517,-6.76554922029455,
4.2079711400965));
#48787=CARTESIAN_POINT('Ctrl Pts',(0.406354063323646,-6.75478832941643,
4.21640036064136));
#48788=CARTESIAN_POINT('Ctrl Pts',(0.585150432551974,-6.74403231048582,
4.22482576489251));
#48789=CARTESIAN_POINT('Ctrl Pts',(0.763582083236608,-6.72616919437579,
4.23325116914365));
#48790=CARTESIAN_POINT('Ctrl Pts',(0.941062878659978,-6.70124538115179,
4.2416765733948));
#48791=CARTESIAN_POINT('Ctrl Pts',(1.11850467810437,-6.6763270441738,4.25010012642094));
#48792=CARTESIAN_POINT('Ctrl Pts',(1.29499570857545,-6.64435114693832,4.2585236794471));
#48793=CARTESIAN_POINT('Ctrl Pts',(1.46995596456517,-6.60541584324858,4.26694723247324));
#48794=CARTESIAN_POINT('Ctrl Pts',(1.64489663942007,-6.56648489710521,4.27536984275541));
#48795=CARTESIAN_POINT('Ctrl Pts',(1.81830655595167,-6.52059616966518,4.28379245303755));
#48796=CARTESIAN_POINT('Ctrl Pts',(1.9896165852714,-6.46789879664277,4.29221506331972));
#48797=CARTESIAN_POINT('Ctrl Pts',(2.16093133193039,-6.4151999725005,4.30063790553407));
#48798=CARTESIAN_POINT('Ctrl Pts',(2.33014575753758,-6.35569222737254,4.30906074774842));
#48799=CARTESIAN_POINT('Ctrl Pts',(2.49670620794372,-6.28957447775407,4.31748358996278));
#48800=CARTESIAN_POINT('Ctrl Pts',(2.66329447389768,-6.22344568649022,4.32590783878938));
#48801=CARTESIAN_POINT('Ctrl Pts',(2.82722757139699,-6.15070481350569,4.33433208761599));
#48802=CARTESIAN_POINT('Ctrl Pts',(2.98797178732154,-6.07159893258527,4.34275633644259));
#48803=CARTESIAN_POINT('Ctrl Pts',(3.14882456704112,-5.99243962495463,4.35118627485758));
#48804=CARTESIAN_POINT('Ctrl Pts',(3.30648386213934,-5.90690686675807,4.35961621327255));
#48805=CARTESIAN_POINT('Ctrl Pts',(3.46043963705768,-5.81529419017475,4.36804615168754));
#48806=CARTESIAN_POINT('Ctrl Pts',(3.61445045025472,-5.72364876260154,4.37647910375563));
#48807=CARTESIAN_POINT('Ctrl Pts',(3.76475481996355,-5.62591925847709,4.38491205582374));
#48808=CARTESIAN_POINT('Ctrl Pts',(3.91087120384815,-5.52244288579895,4.39334500789184));
#48809=CARTESIAN_POINT('Ctrl Pts',(4.05712202136199,-5.41887131021507,4.40178571865421));
#48810=CARTESIAN_POINT('Ctrl Pts',(4.1991768860085,-5.30954249988483,4.41022642941658));
#48811=CARTESIAN_POINT('Ctrl Pts',(4.33658601516312,-5.19483500537713,4.41866714017895));
#48812=CARTESIAN_POINT('Ctrl Pts',(4.41256997860826,-5.13140450317413,4.42333465144232));
#48813=CARTESIAN_POINT('Ctrl Pts',(4.48713396538458,-5.06632998999995,4.4280021627057));
#48814=CARTESIAN_POINT('Ctrl Pts',(4.56020668196633,-4.99968039156001,4.43266967396907));
#48815=CARTESIAN_POINT('Ctrl Pts',(4.68766484965754,-4.88342584277769,4.44081104958964));
#48816=CARTESIAN_POINT('Ctrl Pts',(4.81083698689081,-4.76214595966299,4.44895242521021));
#48817=CARTESIAN_POINT('Ctrl Pts',(4.92930031154187,-4.63619320549017,4.45709380083078));
#48818=CARTESIAN_POINT('Ctrl Pts',(5.04766022586806,-4.51035039939848,4.46522806959105));
#48819=CARTESIAN_POINT('Ctrl Pts',(5.16131926047743,-4.37984310656541,4.47336233835132));
#48820=CARTESIAN_POINT('Ctrl Pts',(5.26988909277935,-4.24506277336452,4.48149660711159));
#48821=CARTESIAN_POINT('Ctrl Pts',(5.37838486178295,-4.11037438353145,4.48962532690158));
#48822=CARTESIAN_POINT('Ctrl Pts',(5.48179811185529,-3.97141904080256,4.49775404669156));
#48823=CARTESIAN_POINT('Ctrl Pts',(5.57977870456578,-3.8286235918505,4.50588276648155));
#48824=CARTESIAN_POINT('Ctrl Pts',(5.67771257065771,-3.68589624157279,4.51400760971212));
#48825=CARTESIAN_POINT('Ctrl Pts',(5.77021873195068,-3.5393327330905,4.52213245294268));
#48826=CARTESIAN_POINT('Ctrl Pts',(5.85698856180224,-3.38939138886581,4.53025729617325));
#48827=CARTESIAN_POINT('Ctrl Pts',(5.94373409947056,-3.23949202239556,4.53837986476319));
#48828=CARTESIAN_POINT('Ctrl Pts',(6.02474632197434,-3.08621702072262,4.54650243335314));
#48829=CARTESIAN_POINT('Ctrl Pts',(6.09976103573944,-2.93005192904066,4.55462500194308));
#48830=CARTESIAN_POINT('Ctrl Pts',(6.17477973512309,-2.77387854012668,4.56274800209449));
#48831=CARTESIAN_POINT('Ctrl Pts',(6.24380012715659,-2.61481508271665,4.57087100224589));
#48832=CARTESIAN_POINT('Ctrl Pts',(6.30660484032441,-2.45337000633754,4.57899400239729));
#48833=CARTESIAN_POINT('Ctrl Pts',(6.33866432113846,-2.37095827212793,4.58314049323168));
#48834=CARTESIAN_POINT('Ctrl Pts',(6.36910493527291,-2.28792628966559,4.58728698406607));
#48835=CARTESIAN_POINT('Ctrl Pts',(6.39790266492223,-2.20434355085161,4.59143347490046));
#48836=CARTESIAN_POINT('Ctrl Pts',(6.46029499361516,-2.02325560480029,4.60041714209268));
#48837=CARTESIAN_POINT('Ctrl Pts',(6.51494192559734,-1.83967109875961,4.60940080928488));
#48838=CARTESIAN_POINT('Ctrl Pts',(6.56168958327112,-1.65424267046623,4.6183844764771));
#48839=CARTESIAN_POINT('Ctrl Pts',(6.60851755533095,-1.46849566855624,4.62738357797665));
#48840=CARTESIAN_POINT('Ctrl Pts',(6.64741906944594,-1.28089864450445,4.63638267947621));
#48841=CARTESIAN_POINT('Ctrl Pts',(6.67829134828466,-1.09211431060412,4.64538178097575));
#48842=CARTESIAN_POINT('Ctrl Pts',(6.70923601581433,-0.902887319040711,
4.6544019833853));
#48843=CARTESIAN_POINT('Ctrl Pts',(6.73211374025193,-0.712467684336141,
4.66342218579482));
#48844=CARTESIAN_POINT('Ctrl Pts',(6.74687333082256,-0.521525893734312,
4.67244238820436));
#48845=CARTESIAN_POINT('Ctrl Pts',(6.7616478695633,-0.33039072172708,4.68147172606515));
#48846=CARTESIAN_POINT('Ctrl Pts',(6.76828783679952,-0.13873257604197,4.69050106392597));
#48847=CARTESIAN_POINT('Ctrl Pts',(6.7667941920583,0.0527765319631494,4.69953040178676));
#48848=CARTESIAN_POINT('Ctrl Pts',(6.76529844154432,0.244555633664026,4.70857246940398));
#48849=CARTESIAN_POINT('Ctrl Pts',(6.75564615263741,0.436185038294863,4.7176145370212));
#48850=CARTESIAN_POINT('Ctrl Pts',(6.73789043526874,0.626994005006506,4.72665660463842));
#48851=CARTESIAN_POINT('Ctrl Pts',(6.72248166218426,0.792581911678803,4.73450349503633));
#48852=CARTESIAN_POINT('Ctrl Pts',(6.70097092684326,0.957551909317143,4.74235038543425));
#48853=CARTESIAN_POINT('Ctrl Pts',(6.67342442468385,1.12147021718506,4.75019727583216));
#48854=CARTESIAN_POINT('Ctrl Pts',(6.64304648950995,1.30223725981751,4.75885072760054));
#48855=CARTESIAN_POINT('Ctrl Pts',(6.60530011697497,1.48188441432217,4.76750417936893));
#48856=CARTESIAN_POINT('Ctrl Pts',(6.56028481952129,1.65980483393636,4.77615763113732));
#48857=CARTESIAN_POINT('Ctrl Pts',(6.51531099087796,1.83756135042082,4.78480311120786));
#48858=CARTESIAN_POINT('Ctrl Pts',(6.46308166746408,2.01359401099816,4.7934485912784));
#48859=CARTESIAN_POINT('Ctrl Pts',(6.40374738637307,2.18730619976264,4.80209407134893));
#48860=CARTESIAN_POINT('Ctrl Pts',(6.34262800292173,2.36624460906066,4.81099965513348));
#48861=CARTESIAN_POINT('Ctrl Pts',(6.27396951615173,2.54272041893106,4.819905238918));
#48862=CARTESIAN_POINT('Ctrl Pts',(6.19799251255383,2.7160960613216,4.82881082270255));
#48863=CARTESIAN_POINT('Ctrl Pts',(6.12437450848591,2.88408858724872,4.83743989824162));
#48864=CARTESIAN_POINT('Ctrl Pts',(6.04388575616793,3.04917026101768,4.8460689737807));
#48865=CARTESIAN_POINT('Ctrl Pts',(5.95677668112415,3.21077881069618,4.85469804931977));
#48866=CARTESIAN_POINT('Ctrl Pts',(5.86548064930897,3.3801551849217,4.86374188722706));
#48867=CARTESIAN_POINT('Ctrl Pts',(5.76691229103232,3.54571600631978,4.87278572513433));
#48868=CARTESIAN_POINT('Ctrl Pts',(5.66141575166245,3.70683971690553,4.88182956304162));
#48869=CARTESIAN_POINT('Ctrl Pts',(5.55591921229258,3.86796342749129,4.89087340094891));
#48870=CARTESIAN_POINT('Ctrl Pts',(5.44349467392716,4.02464968591883,4.89991723885619));
#48871=CARTESIAN_POINT('Ctrl Pts',(5.32454098894455,4.17630844850442,4.90896107676348));
#48872=CARTESIAN_POINT('Ctrl Pts',(5.21372353180683,4.31759401208191,4.91738633168347));
#48873=CARTESIAN_POINT('Ctrl Pts',(5.09728824589692,4.45445456856581,4.92581158660348));
#48874=CARTESIAN_POINT('Ctrl Pts',(4.97562218340768,4.58644447126327,4.93423684152347));
#48875=CARTESIAN_POINT('Ctrl Pts',(4.85392901435793,4.71846378061868,4.94266397354607));
#48876=CARTESIAN_POINT('Ctrl Pts',(4.72700297008946,4.8456100292338,4.95109110556866));
#48877=CARTESIAN_POINT('Ctrl Pts',(4.59526875740729,4.96747360810266,4.95951823759125));
#48878=CARTESIAN_POINT('Ctrl Pts',(4.46343886480488,5.08942569774841,4.96795149032694));
#48879=CARTESIAN_POINT('Ctrl Pts',(4.32679406965878,5.20608722611458,4.97638474306262));
#48880=CARTESIAN_POINT('Ctrl Pts',(4.18579381123436,5.31708747058314,4.98481799579831));
#48881=CARTESIAN_POINT('Ctrl Pts',(4.04473729166143,5.42813200575943,4.99325461352417));
#48882=CARTESIAN_POINT('Ctrl Pts',(3.89932210751482,5.53351055251236,5.00169123125004));
#48883=CARTESIAN_POINT('Ctrl Pts',(3.75003810094601,5.63289474794739,5.0101278489759));
#48884=CARTESIAN_POINT('Ctrl Pts',(3.60061690377252,5.73237027652774,5.01857221987448));
#48885=CARTESIAN_POINT('Ctrl Pts',(3.44732006085961,5.82584027050847,5.02701659077309));
#48886=CARTESIAN_POINT('Ctrl Pts',(3.29066442005884,5.91302094318622,5.03546096167167));
#48887=CARTESIAN_POINT('Ctrl Pts',(3.2273415935653,5.94826082718493,5.03887431742781));
#48888=CARTESIAN_POINT('Ctrl Pts',(3.16347023679114,5.98247362281432,5.04228767318394));
#48889=CARTESIAN_POINT('Ctrl Pts',(3.09908550384713,6.01564277861016,5.04570102894007));
#48890=CARTESIAN_POINT('Ctrl Pts',(3.0990855038473,6.01564277861008,3.04562247039135));
#48891=CARTESIAN_POINT('Ctrl Pts',(2.94198259178318,6.09657766376005,3.05392813220987));
#48892=CARTESIAN_POINT('Ctrl Pts',(2.78177728831488,6.17131830222165,3.06223379402837));
#48893=CARTESIAN_POINT('Ctrl Pts',(2.61899753780536,6.23964268984767,3.07053945584688));
#48894=CARTESIAN_POINT('Ctrl Pts',(2.45602509856137,6.30804795571404,3.07885494940098));
#48895=CARTESIAN_POINT('Ctrl Pts',(2.29047244483192,6.37002166148446,3.08717044295508));
#48896=CARTESIAN_POINT('Ctrl Pts',(2.12288585117006,6.42539062337085,3.09548593650918));
#48897=CARTESIAN_POINT('Ctrl Pts',(1.95519200029967,6.48079502198377,3.1038067520679));
#48898=CARTESIAN_POINT('Ctrl Pts',(1.78546194739057,6.52958615091888,3.1121275676266));
#48899=CARTESIAN_POINT('Ctrl Pts',(1.61425441948635,6.5716414744848,3.12044838318532));
#48900=CARTESIAN_POINT('Ctrl Pts',(1.44279498787196,6.6137586755404,3.12878144145518));
#48901=CARTESIAN_POINT('Ctrl Pts',(1.26985407772748,6.64912019672616,3.13711449972508));
#48902=CARTESIAN_POINT('Ctrl Pts',(1.09599913746674,6.67765489454735,3.14544755799494));
#48903=CARTESIAN_POINT('Ctrl Pts',(0.97699700697648,6.6971866365187,3.15115146083559));
#48904=CARTESIAN_POINT('Ctrl Pts',(0.857566756986758,6.71352090508499,3.15685536367623));
#48905=CARTESIAN_POINT('Ctrl Pts',(0.737890778038132,6.72664895766728,3.16255926651688));
#48906=CARTESIAN_POINT('Ctrl Pts',(0.568537405535535,6.74522645332459,3.17063085440759));
#48907=CARTESIAN_POINT('Ctrl Pts',(0.398170534689765,6.75743827932392,3.17870244229829));
#48908=CARTESIAN_POINT('Ctrl Pts',(0.227320024121162,6.76318080540758,3.186774030189));
#48909=CARTESIAN_POINT('Ctrl Pts',(0.0566839668140396,6.76891612341534,
3.19483548654225));
#48910=CARTESIAN_POINT('Ctrl Pts',(-0.114434154292643,6.76819828652658,
3.20289694289552));
#48911=CARTESIAN_POINT('Ctrl Pts',(-0.285495674491022,6.76097487200233,
3.21095839924877));
#48912=CARTESIAN_POINT('Ctrl Pts',(-0.456379988047669,6.75375894038264,
3.21901150455026));
#48913=CARTESIAN_POINT('Ctrl Pts',(-0.627207447921226,6.74005085810645,
3.22706460985174));
#48914=CARTESIAN_POINT('Ctrl Pts',(-0.797435769424155,6.71985008714056,
3.23511771515324));
#48915=CARTESIAN_POINT('Ctrl Pts',(-0.967525020543475,6.69966581947413,
3.24316424135888));
#48916=CARTESIAN_POINT('Ctrl Pts',(-1.13701573904788,6.67299946420441,3.25121076756455));
#48917=CARTESIAN_POINT('Ctrl Pts',(-1.30536725142705,6.63990250974378,3.25925729377019));
#48918=CARTESIAN_POINT('Ctrl Pts',(-1.47361805046999,6.60682535495502,3.26729900628282));
#48919=CARTESIAN_POINT('Ctrl Pts',(-1.64073063505616,6.56732533099749,3.27534071879545));
#48920=CARTESIAN_POINT('Ctrl Pts',(-1.80617116299231,6.52150555699948,3.28338243130808));
#48921=CARTESIAN_POINT('Ctrl Pts',(-1.97478619091406,6.47480658566263,3.29157844951941));
#48922=CARTESIAN_POINT('Ctrl Pts',(-2.14166395004368,6.4215429198229,3.29977446773074));
#48923=CARTESIAN_POINT('Ctrl Pts',(-2.30625148463374,6.3618781102458,3.30797048594206));
#48924=CARTESIAN_POINT('Ctrl Pts',(-2.46768464545086,6.30335679620113,3.31600942479162));
#48925=CARTESIAN_POINT('Ctrl Pts',(-2.62691421728593,6.23867763171685,3.32404836364116));
#48926=CARTESIAN_POINT('Ctrl Pts',(-2.78343544430358,6.16804475724638,3.33208730249072));
#48927=CARTESIAN_POINT('Ctrl Pts',(-2.93997183450435,6.09740504013079,3.3401270201222));
#48928=CARTESIAN_POINT('Ctrl Pts',(-3.0937990169911,6.02081061809264,3.3481667377537));
#48929=CARTESIAN_POINT('Ctrl Pts',(-3.24443416750943,5.93851293950745,3.35620645538518));
#48930=CARTESIAN_POINT('Ctrl Pts',(-3.39511373456322,5.85619099448944,3.36424854362141));
#48931=CARTESIAN_POINT('Ctrl Pts',(-3.54259906864289,5.76816262455319,3.37229063185763));
#48932=CARTESIAN_POINT('Ctrl Pts',(-3.68643393892883,5.67472411786808,3.38033272009386));
#48933=CARTESIAN_POINT('Ctrl Pts',(-3.83511137773307,5.57813976504727,3.38864556578436));
#48934=CARTESIAN_POINT('Ctrl Pts',(-3.97988789073937,5.47577486069885,3.39695841147487));
#48935=CARTESIAN_POINT('Ctrl Pts',(-4.12029512519974,5.36800308133809,3.40527125716537));
#48936=CARTESIAN_POINT('Ctrl Pts',(-4.25636500106121,5.26356050973309,3.41332730844726));
#48937=CARTESIAN_POINT('Ctrl Pts',(-4.38833129304228,5.15404043836785,3.42138335972915));
#48938=CARTESIAN_POINT('Ctrl Pts',(-4.51580438545681,5.03982140083248,3.42943941101105));
#48939=CARTESIAN_POINT('Ctrl Pts',(-4.64937246961748,4.92014110023488,3.43788065390585));
#48940=CARTESIAN_POINT('Ctrl Pts',(-4.77800678073316,4.79530178657098,3.44632189680064));
#48941=CARTESIAN_POINT('Ctrl Pts',(-4.90130605290549,4.66577838905279,3.45476313969544));
#48942=CARTESIAN_POINT('Ctrl Pts',(-5.02460532507778,4.53625499153463,3.46320438259025));
#48943=CARTESIAN_POINT('Ctrl Pts',(-5.1425693182831,4.40204791278835,3.47164562548506));
#48944=CARTESIAN_POINT('Ctrl Pts',(-5.25484872399403,4.26366671867518,3.48008686837986));
#48945=CARTESIAN_POINT('Ctrl Pts',(-5.36544908633879,4.12735489805491,3.48840187964033));
#48946=CARTESIAN_POINT('Ctrl Pts',(-5.47089587792703,3.98654743576582,3.49671689090081));
#48947=CARTESIAN_POINT('Ctrl Pts',(-5.57080753044914,3.84166532361828,3.50503190216128));
#48948=CARTESIAN_POINT('Ctrl Pts',(-5.67054849216198,3.69703073059735,3.51333270791153));
#48949=CARTESIAN_POINT('Ctrl Pts',(-5.76477296970168,3.54833565032679,3.52163351366177));
#48950=CARTESIAN_POINT('Ctrl Pts',(-5.85313928068442,3.39603438747447,3.52993431941202));
#48951=CARTESIAN_POINT('Ctrl Pts',(-5.94141619507938,3.24388720158953,3.53822672757611));
#48952=CARTESIAN_POINT('Ctrl Pts',(-6.02384657241075,3.08814139897192,3.5465191357402));
#48953=CARTESIAN_POINT('Ctrl Pts',(-6.10013110229294,2.92928140246689,3.55481154390429));
#48954=CARTESIAN_POINT('Ctrl Pts',(-6.1763513325648,2.77055530776197,3.56309696246493));
#48955=CARTESIAN_POINT('Ctrl Pts',(-6.24643588385274,2.60872056119268,3.57138238102557));
#48956=CARTESIAN_POINT('Ctrl Pts',(-6.31013052885371,2.44428756672132,3.5796677995862));
#48957=CARTESIAN_POINT('Ctrl Pts',(-6.3737822314333,2.27996543166265,3.58794763218376));
#48958=CARTESIAN_POINT('Ctrl Pts',(-6.43105248490995,2.11304886338099,3.59622746478131));
#48959=CARTESIAN_POINT('Ctrl Pts',(-6.4817344408519,1.94406986455588,3.60450729737887));
#48960=CARTESIAN_POINT('Ctrl Pts',(-6.53239046240314,1.77517733373101,3.61278289311521));
#48961=CARTESIAN_POINT('Ctrl Pts',(-6.57646480485888,1.60422480958536,3.62105848885156));
#48962=CARTESIAN_POINT('Ctrl Pts',(-6.61379985985277,1.4317612977768,3.6293340845879));
#48963=CARTESIAN_POINT('Ctrl Pts',(-6.65112325433395,1.25935164990315,3.6376070956839));
#48964=CARTESIAN_POINT('Ctrl Pts',(-6.68171148249384,1.08543229603188,3.64588010677991));
#48965=CARTESIAN_POINT('Ctrl Pts',(-6.70545756805903,0.910564551780863,
3.65415311787591));
#48966=CARTESIAN_POINT('Ctrl Pts',(-6.729203618725,0.735697064530014,3.6624261168132));
#48967=CARTESIAN_POINT('Ctrl Pts',(-6.74610749360351,0.559881535000381,
3.67069911575047));
#48968=CARTESIAN_POINT('Ctrl Pts',(-6.7561137723544,0.383686975284884,3.67897211468777));
#48969=CARTESIAN_POINT('Ctrl Pts',(-6.76345456110672,0.254427429915391,
3.6850413377285));
#48970=CARTESIAN_POINT('Ctrl Pts',(-6.76708416463921,0.124964074613623,
3.69111056076924));
#48971=CARTESIAN_POINT('Ctrl Pts',(-6.7669985187373,-0.00447743310165752,
3.69717978380997));
#48972=CARTESIAN_POINT('',(-6.76706252418698,0.0012438250213078,3.30292897675432));
#48973=CARTESIAN_POINT('Ctrl Pts',(3.09908550384727,6.01564277861009,2.65150531920281));
#48974=CARTESIAN_POINT('Ctrl Pts',(2.94012272934183,6.09753581120053,2.65991673722147));
#48975=CARTESIAN_POINT('Ctrl Pts',(2.77785065443283,6.17315569312117,2.6683281552401));
#48976=CARTESIAN_POINT('Ctrl Pts',(2.61279470237935,6.24224261329359,2.67673957325876));
#48977=CARTESIAN_POINT('Ctrl Pts',(2.44778162890434,6.31131158592222,2.68514880614175));
#48978=CARTESIAN_POINT('Ctrl Pts',(2.27998642812488,6.37385084902689,2.69355803902475));
#48979=CARTESIAN_POINT('Ctrl Pts',(2.10995579167536,6.42964816744864,2.70196727190773));
#48980=CARTESIAN_POINT('Ctrl Pts',(1.9399483019024,6.48543789004819,2.71037536002177));
#48981=CARTESIAN_POINT('Ctrl Pts',(1.7677063014232,6.53448739297538,2.7187834481358));
#48982=CARTESIAN_POINT('Ctrl Pts',(1.5937932815841,6.57663378755252,2.72719153624983));
#48983=CARTESIAN_POINT('Ctrl Pts',(1.41987906201742,6.61878047287381,2.73559968236651));
#48984=CARTESIAN_POINT('Ctrl Pts',(1.24429412590556,6.65402387628327,2.74400782848317));
#48985=CARTESIAN_POINT('Ctrl Pts',(1.06761418108446,6.68225178815849,2.75241597459986));
#48986=CARTESIAN_POINT('Ctrl Pts',(0.890907746284581,6.71048393230121,2.76082538136676));
#48987=CARTESIAN_POINT('Ctrl Pts',(0.713106306489074,6.73169843567122,2.76923478813368));
#48988=CARTESIAN_POINT('Ctrl Pts',(0.534793098444444,6.74583466606292,2.77764419490059));
#48989=CARTESIAN_POINT('Ctrl Pts',(0.356359160763974,6.75998046760173,2.78605929538266));
#48990=CARTESIAN_POINT('Ctrl Pts',(0.177413096882429,6.76703839267651,2.79447439586472));
#48991=CARTESIAN_POINT('Ctrl Pts',(-0.0014584028518669,6.76699984284477,
2.80288949634679));
#48992=CARTESIAN_POINT('Ctrl Pts',(-0.180392226196036,6.76696127958124,
2.81130752887472));
#48993=CARTESIAN_POINT('Ctrl Pts',(-0.35925109842801,6.75982131768624,2.81972556140265));
#48994=CARTESIAN_POINT('Ctrl Pts',(-0.537450480721161,6.74562346864785,
2.82814359393058));
#48995=CARTESIAN_POINT('Ctrl Pts',(-0.715820944584164,6.73141198886467,
2.83656970824981));
#48996=CARTESIAN_POINT('Ctrl Pts',(-0.893530319532771,6.71012911523428,
2.84499582256906));
#48997=CARTESIAN_POINT('Ctrl Pts',(-1.07000016315762,6.68187014621226,2.8534219368883));
#48998=CARTESIAN_POINT('Ctrl Pts',(-1.18898013307135,6.6628173085434,2.85910301421913));
#48999=CARTESIAN_POINT('Ctrl Pts',(-1.30739680774279,6.6405943749332,2.86478409154997));
#49000=CARTESIAN_POINT('Ctrl Pts',(-1.42507603784582,6.61524355457588,2.8704651688808));
#49001=CARTESIAN_POINT('Ctrl Pts',(-1.59401445790201,6.57885032244354,2.87862083260878));
#49002=CARTESIAN_POINT('Ctrl Pts',(-1.76176990886751,6.53593573372507,2.88677649633676));
#49003=CARTESIAN_POINT('Ctrl Pts',(-1.92779815956372,6.486592576691,2.89493216006474));
#49004=CARTESIAN_POINT('Ctrl Pts',(-2.09368110021672,6.43729260541748,2.90308068585178));
#49005=CARTESIAN_POINT('Ctrl Pts',(-2.25783950261943,6.38157536912555,2.9112292116388));
#49006=CARTESIAN_POINT('Ctrl Pts',(-2.41973936295995,6.31958467111109,2.91937773742583));
#49007=CARTESIAN_POINT('Ctrl Pts',(-2.58152815278813,6.25763650147543,2.92752067296139));
#49008=CARTESIAN_POINT('Ctrl Pts',(-2.74106114652839,6.18942356940207,2.93566360849696));
#49009=CARTESIAN_POINT('Ctrl Pts',(-2.89781956935012,6.11513947048565,2.94380654403251));
#49010=CARTESIAN_POINT('Ctrl Pts',(-3.0545015159481,6.04089161183796,2.95194550695244));
#49011=CARTESIAN_POINT('Ctrl Pts',(-3.20841125861373,5.96057864095412,2.96008446987237));
#49012=CARTESIAN_POINT('Ctrl Pts',(-3.35905009070085,5.87444222783428,2.9682234327923));
#49013=CARTESIAN_POINT('Ctrl Pts',(-3.50964587413398,5.78833043025743,2.97636006980865));
#49014=CARTESIAN_POINT('Ctrl Pts',(-3.65697229301819,5.69639868682647,2.98449670682498));
#49015=CARTESIAN_POINT('Ctrl Pts',(-3.80055534488504,5.59893454779263,2.99263334384133));
#49016=CARTESIAN_POINT('Ctrl Pts',(-3.94414386966314,5.50146669374801,3.00077029099939));
#49017=CARTESIAN_POINT('Ctrl Pts',(-4.08398843838153,5.39846622421434,3.00890723815746));
#49018=CARTESIAN_POINT('Ctrl Pts',(-4.21964398358273,5.29026404367628,3.01704418531551));
#49019=CARTESIAN_POINT('Ctrl Pts',(-4.28735707679175,5.23625442449465,3.02110578014773));
#49020=CARTESIAN_POINT('Ctrl Pts',(-4.35402693308373,5.18094942794208,3.02516737497994));
#49021=CARTESIAN_POINT('Ctrl Pts',(-4.41960125263066,5.12439399029246,3.02922896981215));
#49022=CARTESIAN_POINT('Ctrl Pts',(-4.56448897329967,4.99943366269614,3.03820314173778));
#49023=CARTESIAN_POINT('Ctrl Pts',(-4.70395281213403,4.86842988574425,3.04717731366341));
#49024=CARTESIAN_POINT('Ctrl Pts',(-4.83753202993561,4.73186779816883,3.05615148558904));
#49025=CARTESIAN_POINT('Ctrl Pts',(-4.97133572982691,4.59507621574158,3.06514073875934));
#49026=CARTESIAN_POINT('Ctrl Pts',(-5.09923487511697,4.45270782605835,3.07412999192963));
#49027=CARTESIAN_POINT('Ctrl Pts',(-5.22080781295147,4.30528219519056,3.08311924509994));
#49028=CARTESIAN_POINT('Ctrl Pts',(-5.34266155771033,4.15751604332598,3.09212926148104));
#49029=CARTESIAN_POINT('Ctrl Pts',(-5.45815970544682,4.00466946574594,3.10113927786215));
#49030=CARTESIAN_POINT('Ctrl Pts',(-5.56692128171149,3.84729469149787,3.11014929424324));
#49031=CARTESIAN_POINT('Ctrl Pts',(-5.67579166418284,3.68976247789667,3.11916832433799));
#49032=CARTESIAN_POINT('Ctrl Pts',(-5.77791188001264,3.52769321951944,3.12818735443274));
#49033=CARTESIAN_POINT('Ctrl Pts',(-5.87294525261792,3.3616667086064,3.13720638452749));
#49034=CARTESIAN_POINT('Ctrl Pts',(-5.96811274491677,3.19540588605992,3.1462381430935));
#49035=CARTESIAN_POINT('Ctrl Pts',(-6.0561732759664,3.02517685346559,3.15526990165949));
#49036=CARTESIAN_POINT('Ctrl Pts',(-6.13683587545888,2.85158454857661,3.1643016602255));
#49037=CARTESIAN_POINT('Ctrl Pts',(-6.20736427976691,2.69980183464221,3.17219869706493));
#49038=CARTESIAN_POINT('Ctrl Pts',(-6.27223756172802,2.54544829755473,3.18009573390438));
#49039=CARTESIAN_POINT('Ctrl Pts',(-6.33129152425901,2.38894048373877,3.1879927707438));
#49040=CARTESIAN_POINT('Ctrl Pts',(-6.39738835287652,2.21376730815948,3.1968316203009));
#49041=CARTESIAN_POINT('Ctrl Pts',(-6.45624613323741,2.0357566951229,3.20567046985799));
#49042=CARTESIAN_POINT('Ctrl Pts',(-6.50763970763448,1.85550921194668,3.21450931941509));
#49043=CARTESIAN_POINT('Ctrl Pts',(-6.55895606112458,1.67553255784385,3.22333488824619));
#49044=CARTESIAN_POINT('Ctrl Pts',(-6.60283052208568,1.49332600640725,3.23216045707728));
#49045=CARTESIAN_POINT('Ctrl Pts',(-6.63908756720368,1.30950573691053,3.24098602590838));
#49046=CARTESIAN_POINT('Ctrl Pts',(-6.6753082553054,1.12586979452889,3.24980274483602));
#49047=CARTESIAN_POINT('Ctrl Pts',(-6.70392671212931,0.94062363059039,3.25861946376365));
#49048=CARTESIAN_POINT('Ctrl Pts',(-6.72481789286447,0.754395988728612,
3.26743618269128));
#49049=CARTESIAN_POINT('Ctrl Pts',(-6.74567962581321,0.568430849589584,
3.27624047374999));
#49050=CARTESIAN_POINT('Ctrl Pts',(-6.75883579085114,0.38148726583158,3.28504476480866));
#49051=CARTESIAN_POINT('Ctrl Pts',(-6.76421279127097,0.194201736362655,
3.29384905586735));
#49052=CARTESIAN_POINT('Ctrl Pts',(-6.76603909515312,0.130590008106184,
3.29683944264152));
#49053=CARTESIAN_POINT('Ctrl Pts',(-6.76696840997942,0.0669389024656748,
3.2998298294157));
#49054=CARTESIAN_POINT('Ctrl Pts',(-6.76699920820775,0.00327354788297447,
3.30282021618987));
#49055=CARTESIAN_POINT('Ctrl Pts',(-6.767,2.04925086815431E-12,3.30282021618987));
#49056=CARTESIAN_POINT('Ctrl Pts',(-6.76700000000006,-0.186007249558088,
3.31156972800262));
#49057=CARTESIAN_POINT('Ctrl Pts',(-6.75932637294257,-0.372014355814404,
3.32031923981535));
#49058=CARTESIAN_POINT('Ctrl Pts',(-6.74400518263375,-0.55738953758491,
3.3290687516281));
#49059=CARTESIAN_POINT('Ctrl Pts',(-6.72868405703744,-0.742763936381449,
3.3378182264853));
#49060=CARTESIAN_POINT('Ctrl Pts',(-6.70571545643581,-0.927506130403824,
3.34656770134251));
#49061=CARTESIAN_POINT('Ctrl Pts',(-6.67517739401592,-1.11098864009441,
3.35531717619972));
#49062=CARTESIAN_POINT('Ctrl Pts',(-6.6446394580441,-1.29447039004436,3.36406661482823));
#49063=CARTESIAN_POINT('Ctrl Pts',(-6.60653217002748,-1.47669218339172,
3.37281605345675));
#49064=CARTESIAN_POINT('Ctrl Pts',(-6.56098496085507,-1.65703510627676,
3.38156549208526));
#49065=CARTESIAN_POINT('Ctrl Pts',(-6.51543793649584,-1.83737729739912,
3.39031489521189));
#49066=CARTESIAN_POINT('Ctrl Pts',(-6.46245112156923,-2.01584035544866,
3.39906429833851));
#49067=CARTESIAN_POINT('Ctrl Pts',(-6.40220448361743,-2.19181813797332,
3.40781370146514));
#49068=CARTESIAN_POINT('Ctrl Pts',(-6.34195808511996,-2.36779522106242,
3.41656306981668));
#49069=CARTESIAN_POINT('Ctrl Pts',(-6.27445201416373,-2.54128677725699,
3.42531243816824));
#49070=CARTESIAN_POINT('Ctrl Pts',(-6.19991555052738,-2.71170355428628,
3.43406180651978));
#49071=CARTESIAN_POINT('Ctrl Pts',(-6.12537937695124,-2.88211966813509,
3.44281114082297));
#49072=CARTESIAN_POINT('Ctrl Pts',(-6.04381298028344,-3.04946076419884,
3.45156047512614));
#49073=CARTESIAN_POINT('Ctrl Pts',(-5.9554933930886,-3.21315848424538,3.46030980942933));
#49074=CARTESIAN_POINT('Ctrl Pts',(-5.86717414225678,-3.37685558085311,
3.46905911041089));
#49075=CARTESIAN_POINT('Ctrl Pts',(-5.77210188843925,-3.53690907700231,
3.47780841139246));
#49076=CARTESIAN_POINT('Ctrl Pts',(-5.6705995331122,-3.69277537024224,3.48655771237402));
#49077=CARTESIAN_POINT('Ctrl Pts',(-5.56909755592538,-3.84864108281273,
3.49530698076065));
#49078=CARTESIAN_POINT('Ctrl Pts',(-5.46116568154777,-4.00031938355088,
3.50405624914725));
#49079=CARTESIAN_POINT('Ctrl Pts',(-5.34717048488167,-4.14729511918435,
3.51280551753388));
#49080=CARTESIAN_POINT('Ctrl Pts',(-5.23317570343074,-4.29427031947461,
3.52155475405224));
#49081=CARTESIAN_POINT('Ctrl Pts',(-5.11311781951294,-4.43654276249848,
3.53030399057061));
#49082=CARTESIAN_POINT('Ctrl Pts',(-4.98740458928968,-4.57362924412684,
3.53905322708897));
#49083=CARTESIAN_POINT('Ctrl Pts',(-4.86169180652458,-4.71071523781559,
3.54780243246568));
#49084=CARTESIAN_POINT('Ctrl Pts',(-4.73032391141284,-4.84261509584771,
3.55655163784241));
#49085=CARTESIAN_POINT('Ctrl Pts',(-4.59374706947033,-4.9688808459987,3.56530084321912));
#49086=CARTESIAN_POINT('Ctrl Pts',(-4.45717070231229,-5.09514615720986,
3.57405001818082));
#49087=CARTESIAN_POINT('Ctrl Pts',(-4.315385634971,-5.21577720520799,3.58279919314252));
#49088=CARTESIAN_POINT('Ctrl Pts',(-4.16887340951796,-5.33036429293666,
3.59154836810421));
#49089=CARTESIAN_POINT('Ctrl Pts',(-4.02236168122269,-5.44495099183866,
3.60029751337747));
#49090=CARTESIAN_POINT('Ctrl Pts',(-3.87112305262959,-5.55349359498083,
3.60904665865072));
#49091=CARTESIAN_POINT('Ctrl Pts',(-3.71567116928768,-5.65562346357361,
3.61779580392397));
#49092=CARTESIAN_POINT('Ctrl Pts',(-3.56021980053059,-5.75775299409084,
3.62654492023535));
#49093=CARTESIAN_POINT('Ctrl Pts',(-3.40055544441806,-5.85346967520042,
3.63529403654672));
#49094=CARTESIAN_POINT('Ctrl Pts',(-3.23722035886538,-5.94244843041549,
3.6440431528581));
#49095=CARTESIAN_POINT('Ctrl Pts',(-3.07388580043206,-6.03142689847594,
3.6527922409341));
#49096=CARTESIAN_POINT('Ctrl Pts',(-2.90688078788962,-6.11366734708025,
3.66154132901011));
#49097=CARTESIAN_POINT('Ctrl Pts',(-2.73677250610157,-6.18889047001533,
3.67029041708611));
#49098=CARTESIAN_POINT('Ctrl Pts',(-2.56666475916696,-6.26411335643431,
3.67903947765328));
#49099=CARTESIAN_POINT('Ctrl Pts',(-2.39345402456853,-6.33231884545347,
3.68778853822045));
#49100=CARTESIAN_POINT('Ctrl Pts',(-2.21772855943823,-6.39327529804967,
3.69653759878761));
#49101=CARTESIAN_POINT('Ctrl Pts',(-2.04200363223381,-6.45423156404768,
3.7052866325724));
#49102=CARTESIAN_POINT('Ctrl Pts',(-1.86376426060856,-6.50793874412503,
3.7140356663572));
#49103=CARTESIAN_POINT('Ctrl Pts',(-1.68361577621544,-6.55421443943349,
3.72278470014199));
#49104=CARTESIAN_POINT('Ctrl Pts',(-1.50346782833056,-6.60048999692624,
3.73153370787089));
#49105=CARTESIAN_POINT('Ctrl Pts',(-1.32141105657213,-6.63933404265197,
3.74028271559977));
#49106=CARTESIAN_POINT('Ctrl Pts',(-1.13806375346346,-6.67061465631561,
3.74903172332867));
#49107=CARTESIAN_POINT('Ctrl Pts',(-0.954716981167858,-6.70189517941802,
3.75778070572811));
#49108=CARTESIAN_POINT('Ctrl Pts',(-0.770079967439874,-6.72561226609032,
3.76652968812759));
#49109=CARTESIAN_POINT('Ctrl Pts',(-0.584779764070404,-6.74168536996008,
3.77527867052703));
#49110=CARTESIAN_POINT('Ctrl Pts',(-0.39148958759023,-6.75845153117888,
3.78440490094265));
#49111=CARTESIAN_POINT('Ctrl Pts',(-0.197478091802452,-6.76689985146402,
3.79353113135825));
#49112=CARTESIAN_POINT('Ctrl Pts',(-0.00346214752819375,-6.76699911434415,
3.80265736177387));
#49113=CARTESIAN_POINT('Ctrl Pts',(0.18449079848745,-6.76709527525927,3.81149839748899));
#49114=CARTESIAN_POINT('Ctrl Pts',(0.372447602157554,-6.75935633790748,
3.82033943320412));
#49115=CARTESIAN_POINT('Ctrl Pts',(0.559756448196956,-6.7438091401449,3.82918046891925));
#49116=CARTESIAN_POINT('Ctrl Pts',(0.745136131046012,-6.72842206873125,
3.83793044753255));
#49117=CARTESIAN_POINT('Ctrl Pts',(0.929880851947613,-6.70538686355687,
3.84668042614584));
#49118=CARTESIAN_POINT('Ctrl Pts',(1.11336305057711,-6.67478177303271,3.85543040475915));
#49119=CARTESIAN_POINT('Ctrl Pts',(1.29684337090384,-6.6441769958121,3.86418029379913));
#49120=CARTESIAN_POINT('Ctrl Pts',(1.47906091205463,-6.60600253547999,3.87293018283914));
#49121=CARTESIAN_POINT('Ctrl Pts',(1.65939671095507,-6.5603880644114,3.88168007187913));
#49122=CARTESIAN_POINT('Ctrl Pts',(1.83973072369444,-6.51477404513769,3.89042987425462));
#49123=CARTESIAN_POINT('Ctrl Pts',(2.01818275357318,-6.46172023288573,3.89917967663011));
#49124=CARTESIAN_POINT('Ctrl Pts',(2.19414664033606,-6.40140683918012,3.9079294790056));
#49125=CARTESIAN_POINT('Ctrl Pts',(2.37010884271534,-6.34109402281395,3.91667919762514));
#49126=CARTESIAN_POINT('Ctrl Pts',(2.54358267848075,-6.27352185699683,3.92542891624467));
#49127=CARTESIAN_POINT('Ctrl Pts',(2.71397890842005,-6.19891986435146,3.93417863486421));
#49128=CARTESIAN_POINT('Ctrl Pts',(2.884373563892,-6.12431856103122,3.94292827263603));
#49129=CARTESIAN_POINT('Ctrl Pts',(3.05169040787425,-6.04268767582429,3.95167791040785));
#49130=CARTESIAN_POINT('Ctrl Pts',(3.21536112512301,-5.95430447953812,3.96042754817967));
#49131=CARTESIAN_POINT('Ctrl Pts',(3.37903038443089,-5.86592207054901,3.96917710801174));
#49132=CARTESIAN_POINT('Ctrl Pts',(3.53905332980219,-5.77078760703226,3.9779266678438));
#49133=CARTESIAN_POINT('Ctrl Pts',(3.69488643042137,-5.66922422085139,3.98667622767587));
#49134=CARTESIAN_POINT('Ctrl Pts',(3.85071819468991,-5.56766170562986,3.99542571247587));
#49135=CARTESIAN_POINT('Ctrl Pts',(4.00235994599477,-5.45967053456066,4.00417519727587));
#49136=CARTESIAN_POINT('Ctrl Pts',(4.14929662974557,-5.34561750206486,4.01292468207588));
#49137=CARTESIAN_POINT('Ctrl Pts',(4.29623210225293,-5.23156540974262,4.02167409475123));
#49138=CARTESIAN_POINT('Ctrl Pts',(4.43846235842358,-5.11145173171977,4.03042350742659));
#49139=CARTESIAN_POINT('Ctrl Pts',(4.57550431797661,-4.98568443006348,4.03917292010195));
#49140=CARTESIAN_POINT('Ctrl Pts',(4.71254519337732,-4.85991812336459,4.04792226355985));
#49141=CARTESIAN_POINT('Ctrl Pts',(4.84439764315226,-4.72849847630854,4.05667160701774));
#49142=CARTESIAN_POINT('Ctrl Pts',(4.97061384196931,-4.59187184425079,4.06542095047564));
#49143=CARTESIAN_POINT('Ctrl Pts',(5.09682908420441,-4.45524624767479,4.074170227623));
#49144=CARTESIAN_POINT('Ctrl Pts',(5.21740796650395,-4.31341395556621,4.08291950477036));
#49145=CARTESIAN_POINT('Ctrl Pts',(5.33194095942466,-4.16685668162582,4.09166878191772));
#49146=CARTESIAN_POINT('Ctrl Pts',(5.44647312235341,-4.02030046974933,4.10041799566126));
#49147=CARTESIAN_POINT('Ctrl Pts',(5.55495930712489,-3.86901957035258,4.10916720940481));
#49148=CARTESIAN_POINT('Ctrl Pts',(5.65703106079989,-3.71352778058079,4.11791642314834));
#49149=CARTESIAN_POINT('Ctrl Pts',(5.75910210868923,-3.558037065973,4.12666557639454));
#49150=CARTESIAN_POINT('Ctrl Pts',(5.85475865698729,-3.3983357588059,4.13541472964074));
#49151=CARTESIAN_POINT('Ctrl Pts',(5.94367583069235,-3.23496624706404,4.14416388288694));
#49152=CARTESIAN_POINT('Ctrl Pts',(6.03259241910246,-3.07159781069769,4.15291297854207));
#49153=CARTESIAN_POINT('Ctrl Pts',(6.11476958471132,-2.90456146975489,4.16166207419719));
#49154=CARTESIAN_POINT('Ctrl Pts',(6.18992823574544,-2.73442451647898,4.17041116985231));
#49155=CARTESIAN_POINT('Ctrl Pts',(6.26508641701081,-2.56428862662059,4.17916021082243));
#49156=CARTESIAN_POINT('Ctrl Pts',(6.33322605570431,-2.39105242530922,4.18790925179253));
#49157=CARTESIAN_POINT('Ctrl Pts',(6.39411573747889,-2.21530425353376,4.19665829276265));
#49158=CARTESIAN_POINT('Ctrl Pts',(6.45500505889232,-2.03955712188223,4.20540728195364));
#49159=CARTESIAN_POINT('Ctrl Pts',(6.50864441545021,-1.8612983202525,4.21415627114463));
#49160=CARTESIAN_POINT('Ctrl Pts',(6.55485164049985,-1.68113324012004,4.22290526033562));
#49161=CARTESIAN_POINT('Ctrl Pts',(6.60199852639179,-1.49730435912592,4.23183216721251));
#49162=CARTESIAN_POINT('Ctrl Pts',(6.64140767441071,-1.31149113173343,4.24075907408939));
#49163=CARTESIAN_POINT('Ctrl Pts',(6.67293975269654,-1.12435050446122,4.24968598096628));
#49164=CARTESIAN_POINT('Ctrl Pts',(6.7038466483155,-0.940920291560661,4.25843589515027));
#49165=CARTESIAN_POINT('Ctrl Pts',(6.727185858897,-0.756215114274866,4.26718580933427));
#49166=CARTESIAN_POINT('Ctrl Pts',(6.7428781045189,-0.570862389372079,4.27593572351826));
#49167=CARTESIAN_POINT('Ctrl Pts',(6.75857004154141,-0.385513309565091,
4.28468546562884));
#49168=CARTESIAN_POINT('Ctrl Pts',(6.76661529035565,-0.199516993256255,
4.29343520773942));
#49169=CARTESIAN_POINT('Ctrl Pts',(6.76698652348897,-0.0135052182021578,
4.30218494985));
#49170=CARTESIAN_POINT('Ctrl Pts',(6.76735774981516,0.172503146040806,4.31093453152064));
#49171=CARTESIAN_POINT('Ctrl Pts',(6.76005524147469,0.358526681835397,4.31968411319129));
#49172=CARTESIAN_POINT('Ctrl Pts',(6.74510380214866,0.543933542116802,4.32843369486193));
#49173=CARTESIAN_POINT('Ctrl Pts',(6.73015261710958,0.729337249086645,4.33718312772386));
#49174=CARTESIAN_POINT('Ctrl Pts',(6.70755278444579,0.91412401585657,4.34593256058577));
#49175=CARTESIAN_POINT('Ctrl Pts',(6.67738106408258,1.09766621749575,4.3546819934477));
#49176=CARTESIAN_POINT('Ctrl Pts',(6.64720981677218,1.28120554143509,4.36343128913005));
#49177=CARTESIAN_POINT('Ctrl Pts',(6.60946696581482,1.46350005650805,4.37218058481241));
#49178=CARTESIAN_POINT('Ctrl Pts',(6.56428070010948,1.64393062206717,4.38092988049476));
#49179=CARTESIAN_POINT('Ctrl Pts',(6.51909508282691,1.8243585984483,4.38967905062475));
#49180=CARTESIAN_POINT('Ctrl Pts',(6.46646633415608,2.00292240086736,4.39842822075474));
#49181=CARTESIAN_POINT('Ctrl Pts',(6.40657319597136,2.17901557696621,4.40717739088473));
#49182=CARTESIAN_POINT('Ctrl Pts',(6.34668083768231,2.35510646007606,4.41592644708781));
#49183=CARTESIAN_POINT('Ctrl Pts',(6.27952437143814,2.52872650996707,4.42467550329088));
#49184=CARTESIAN_POINT('Ctrl Pts',(6.20533187335057,2.69928607998106,4.43342455949396));
#49185=CARTESIAN_POINT('Ctrl Pts',(6.12831449784172,2.87633970115568,4.4425067357828));
#49186=CARTESIAN_POINT('Ctrl Pts',(6.04371489463072,3.0500949056251,4.45158891207163));
#49187=CARTESIAN_POINT('Ctrl Pts',(5.95184265120409,3.21991584599782,4.46067108836047));
#49188=CARTESIAN_POINT('Ctrl Pts',(5.86333281335406,3.38352155905451,4.46942086871489));
#49189=CARTESIAN_POINT('Ctrl Pts',(5.76807337235593,3.54347560903973,4.47817064906932));
#49190=CARTESIAN_POINT('Ctrl Pts',(5.66638790086259,3.69923467178795,4.48692042942373));
#49191=CARTESIAN_POINT('Ctrl Pts',(5.56470608502642,3.85498813489909,4.495669895218));
#49192=CARTESIAN_POINT('Ctrl Pts',(5.45659885766848,4.00654667256403,4.50441936101225));
#49193=CARTESIAN_POINT('Ctrl Pts',(5.34243340580399,4.1533955150635,4.51316882680652));
#49194=CARTESIAN_POINT('Ctrl Pts',(5.22827145140479,4.3002398588401,4.52191802456039));
#49195=CARTESIAN_POINT('Ctrl Pts',(5.10805181977968,4.44237456993183,4.53066722231426));
#49196=CARTESIAN_POINT('Ctrl Pts',(4.98218281282423,4.57931691626588,4.53941642006814));
#49197=CARTESIAN_POINT('Ctrl Pts',(4.85631699296099,4.71625579512295,4.54816539628614));
#49198=CARTESIAN_POINT('Ctrl Pts',(4.72480227791707,4.84800236135897,4.55691437250414));
#49199=CARTESIAN_POINT('Ctrl Pts',(4.58808530847982,4.9741091867903,4.56566334872214));
#49200=CARTESIAN_POINT('Ctrl Pts',(4.45135945056829,5.10022421089132,4.57441289374334));
#49201=CARTESIAN_POINT('Ctrl Pts',(4.30943087207889,5.22069856612111,4.58316243876453));
#49202=CARTESIAN_POINT('Ctrl Pts',(4.16278164322307,5.33512305301809,4.59191198378574));
#49203=CARTESIAN_POINT('Ctrl Pts',(4.01614103534237,5.4495408133154,4.60066101445299));
#49204=CARTESIAN_POINT('Ctrl Pts',(3.86478055833267,5.55790924068439,4.60941004512025));
#49205=CARTESIAN_POINT('Ctrl Pts',(3.70921425811814,5.65986029751381,4.6181590757875));
#49206=CARTESIAN_POINT('Ctrl Pts',(3.55364584529982,5.76181273884739,4.62690822526735));
#49207=CARTESIAN_POINT('Ctrl Pts',(3.39387173464207,5.85734747818143,4.63565737474719));
#49208=CARTESIAN_POINT('Ctrl Pts',(3.23043456092267,5.94614005448882,4.64440652422704));
#49209=CARTESIAN_POINT('Ctrl Pts',(3.18690768806298,5.96978744811331,4.64673661296005));
#49210=CARTESIAN_POINT('Ctrl Pts',(3.14312114982832,5.99295688499326,4.64906670169307));
#49211=CARTESIAN_POINT('Ctrl Pts',(3.09908550384716,6.01564277861015,4.65139679042609));
#49212=CARTESIAN_POINT('Origin',(0.,0.,-63.6971797838103));
#49213=CARTESIAN_POINT('',(3.09908550384722,6.01564277861012,7.04591868117257));
#49214=CARTESIAN_POINT('',(3.09908550384729,6.01564277861008,6.6512241499329));
#49215=CARTESIAN_POINT('',(3.09908550384721,6.01564277861012,-63.6971797838103));
#49216=CARTESIAN_POINT('',(-6.76699915828328,-0.00337517308289641,5.69717978377259));
#49217=CARTESIAN_POINT('Ctrl Pts',(-6.76699915828289,-0.00337517387210557,
5.69717978380996));
#49218=CARTESIAN_POINT('Ctrl Pts',(-6.76697949862955,-0.0427914714202488,
5.69904654968036));
#49219=CARTESIAN_POINT('Ctrl Pts',(-6.76661545789972,-0.0822029254710357,
5.70091331555085));
#49220=CARTESIAN_POINT('Ctrl Pts',(-6.76590726115161,-0.121605647467519,
5.70278008142134));
#49221=CARTESIAN_POINT('Ctrl Pts',(-6.76278486510318,-0.295329833278017,
5.71101053770748));
#49222=CARTESIAN_POINT('Ctrl Pts',(-6.75296268258051,-0.469187948267381,
5.71924099399363));
#49223=CARTESIAN_POINT('Ctrl Pts',(-6.73641782758042,-0.642622635966649,
5.72747145027979));
#49224=CARTESIAN_POINT('Ctrl Pts',(-6.71989261229359,-0.815851446519408,
5.73569213653161));
#49225=CARTESIAN_POINT('Ctrl Pts',(-6.69666064861334,-0.98865747724068,
5.74391282278344));
#49226=CARTESIAN_POINT('Ctrl Pts',(-6.66675102227233,-1.16048257506558,
5.75213350903526));
#49227=CARTESIAN_POINT('Ctrl Pts',(-6.63687089961681,-1.3321381798454,5.76034608617401));
#49228=CARTESIAN_POINT('Ctrl Pts',(-6.60032629336207,-1.50281442795062,
5.76855866331277));
#49229=CARTESIAN_POINT('Ctrl Pts',(-6.55719813960777,-1.67195740314293,
5.77677124045152));
#49230=CARTESIAN_POINT('Ctrl Pts',(-6.51410387892953,-1.84096745412623,
5.78497736358106));
#49231=CARTESIAN_POINT('Ctrl Pts',(-6.46443646400532,-2.00844628634816,
5.79318348671062));
#49232=CARTESIAN_POINT('Ctrl Pts',(-6.408328064148,-2.17384921792042,5.80138960984016));
#49233=CARTESIAN_POINT('Ctrl Pts',(-6.35225250799491,-2.33915532896351,
5.80959092942011));
#49234=CARTESIAN_POINT('Ctrl Pts',(-6.28974359265882,-2.50238762147196,
5.81779224900005));
#49235=CARTESIAN_POINT('Ctrl Pts',(-6.22098361389318,-2.66301556053895,
5.82599356858));
#49236=CARTESIAN_POINT('Ctrl Pts',(-6.15224336072521,-2.82359741928192,
5.834192535397));
#49237=CARTESIAN_POINT('Ctrl Pts',(-6.07725575340116,-2.98157608203589,
5.842391502214));
#49238=CARTESIAN_POINT('Ctrl Pts',(-5.99625169893546,-3.13643979107102,
5.850590469031));
#49239=CARTESIAN_POINT('Ctrl Pts',(-5.91525834141358,-3.29128304966812,
5.85878835313816));
#49240=CARTESIAN_POINT('Ctrl Pts',(-5.82825028453694,-3.44301185574427,
5.86698623724531));
#49241=CARTESIAN_POINT('Ctrl Pts',(-5.73550499072217,-3.59113791177687,
5.87518412135246));
#49242=CARTESIAN_POINT('Ctrl Pts',(-5.64275509688695,-3.73927131462846,
5.88338241206175));
#49243=CARTESIAN_POINT('Ctrl Pts',(-5.54426758949399,-3.88380130744567,
5.89158070277106));
#49244=CARTESIAN_POINT('Ctrl Pts',(-5.44036399118967,-4.02426746667849,
5.89977899348035));
#49245=CARTESIAN_POINT('Ctrl Pts',(-5.33643636509712,-4.16476610882027,
5.90797918005077));
#49246=CARTESIAN_POINT('Ctrl Pts',(-5.22709036675116,-4.30119875739443,
5.91617936662118));
#49247=CARTESIAN_POINT('Ctrl Pts',(-5.11268865573878,-4.43313700549396,
5.9243795531916));
#49248=CARTESIAN_POINT('Ctrl Pts',(-4.99817878689707,-4.56519999084082,
5.93258749239414));
#49249=CARTESIAN_POINT('Ctrl Pts',(-4.87860389115694,-4.69275981518642,
5.94079543159667));
#49250=CARTESIAN_POINT('Ctrl Pts',(-4.75436509247631,-4.81542330096148,
5.9490033707992));
#49251=CARTESIAN_POINT('Ctrl Pts',(-4.63006602179254,-4.93814629450769,
5.95721529192158));
#49252=CARTESIAN_POINT('Ctrl Pts',(-4.50109880166452,-5.05596797183455,
5.96542721304397));
#49253=CARTESIAN_POINT('Ctrl Pts',(-4.36789861035503,-5.16853467915797,
5.97363913416635));
#49254=CARTESIAN_POINT('Ctrl Pts',(-4.23451575612425,-5.28125575385428,
5.98186231663518));
#49255=CARTESIAN_POINT('Ctrl Pts',(-4.09688861259461,-5.38870723610298,
5.99008549910399));
#49256=CARTESIAN_POINT('Ctrl Pts',(-3.95548335788428,-5.49057742004432,
5.99830868157282));
#49257=CARTESIAN_POINT('Ctrl Pts',(-3.82938560711906,-5.5814198791266,6.00564168214324));
#49258=CARTESIAN_POINT('Ctrl Pts',(-3.70028400509378,-5.66782453499294,
6.01297468271367));
#49259=CARTESIAN_POINT('Ctrl Pts',(-3.56852566469042,-5.74960116707636,
6.02030768328409));
#49260=CARTESIAN_POINT('Ctrl Pts',(-3.4079794778143,-5.8492451548222,6.02924286929461));
#49261=CARTESIAN_POINT('Ctrl Pts',(-3.24315549910538,-5.94222435605987,
6.03817805530512));
#49262=CARTESIAN_POINT('Ctrl Pts',(-3.07460673310888,-6.02819064369414,
6.04711324131564));
#49263=CARTESIAN_POINT('Ctrl Pts',(-2.90631040097667,-6.11402818044698,
6.05603504518409));
#49264=CARTESIAN_POINT('Ctrl Pts',(-2.73430064234891,-6.19287364395915,
6.06495684905255));
#49265=CARTESIAN_POINT('Ctrl Pts',(-2.55915635159388,-6.26442397735791,
6.073878652921));
#49266=CARTESIAN_POINT('Ctrl Pts',(-2.38443927900038,-6.33579978264753,
6.08277869440924));
#49267=CARTESIAN_POINT('Ctrl Pts',(-2.20660317282507,-6.39991587517573,
6.09167873589749));
#49268=CARTESIAN_POINT('Ctrl Pts',(-2.02624767534499,-6.45651681312448,
6.10057877738573));
#49269=CARTESIAN_POINT('Ctrl Pts',(-1.84616983754887,-6.51303061317744,
6.10946511714189));
#49270=CARTESIAN_POINT('Ctrl Pts',(-1.66358059057379,-6.56205226019557,
6.11835145689805));
#49271=CARTESIAN_POINT('Ctrl Pts',(-1.47909832937744,-6.60337467754427,
6.1272377966542));
#49272=CARTESIAN_POINT('Ctrl Pts',(-1.2950877565163,-6.64459144082021,6.13610141561986));
#49273=CARTESIAN_POINT('Ctrl Pts',(-1.10919407888226,-6.67814819944702,
6.14496503458552));
#49274=CARTESIAN_POINT('Ctrl Pts',(-0.922048844575116,-6.70388804562082,
6.15382865355119));
#49275=CARTESIAN_POINT('Ctrl Pts',(-0.744390957219133,-6.7283230076386,
6.16224293043939));
#49276=CARTESIAN_POINT('Ctrl Pts',(-0.565605501815782,-6.74571381361739,
6.1706572073276));
#49277=CARTESIAN_POINT('Ctrl Pts',(-0.386244720236502,-6.75596802953429,
6.17907148421581));
#49278=CARTESIAN_POINT('Ctrl Pts',(-0.211233057546137,-6.76597360244382,
6.18728173271928));
#49279=CARTESIAN_POINT('Ctrl Pts',(-0.0358417702284699,-6.76917385162462,
6.19549198122275));
#49280=CARTESIAN_POINT('Ctrl Pts',(0.139364509554821,-6.76556476086635,
6.20370222972622));
#49281=CARTESIAN_POINT('Ctrl Pts',(0.31461243945397,-6.7619548121534,6.21191442997366));
#49282=CARTESIAN_POINT('Ctrl Pts',(0.489674918318395,-6.75153230587871,
6.22012663022108));
#49283=CARTESIAN_POINT('Ctrl Pts',(0.663989605743369,-6.73434531364889,
6.22833883046853));
#49284=CARTESIAN_POINT('Ctrl Pts',(0.838376771885889,-6.71715117519879,
6.23655444528621));
#49285=CARTESIAN_POINT('Ctrl Pts',(1.01201517321715,-6.693186982332,6.24477006010389));
#49286=CARTESIAN_POINT('Ctrl Pts',(1.18434977292205,-6.66255240995367,6.25298567492156));
#49287=CARTESIAN_POINT('Ctrl Pts',(1.35687789691903,-6.63188343627728,6.26121051551887));
#49288=CARTESIAN_POINT('Ctrl Pts',(1.52809894439632,-6.59452918436298,6.26943535611618));
#49289=CARTESIAN_POINT('Ctrl Pts',(1.6974692629602,-6.55064020545362,6.2776601967135));
#49290=CARTESIAN_POINT('Ctrl Pts',(1.86694806915528,-6.50672311411347,6.28589030560977));
#49291=CARTESIAN_POINT('Ctrl Pts',(2.03457344333143,-6.45626305408508,6.29412041450605));
#49292=CARTESIAN_POINT('Ctrl Pts',(2.19981903502714,-6.39945975947441,6.30235052340232));
#49293=CARTESIAN_POINT('Ctrl Pts',(2.36529118100769,-6.34257858666042,6.31059191590633));
#49294=CARTESIAN_POINT('Ctrl Pts',(2.52837669668185,-6.27933693688937,6.31883330841034));
#49295=CARTESIAN_POINT('Ctrl Pts',(2.68857033994664,-6.20998216802264,6.32707470091434));
#49296=CARTESIAN_POINT('Ctrl Pts',(2.75829064474062,-6.17979722731116,6.33066156232529));
#49297=CARTESIAN_POINT('Ctrl Pts',(2.82746349428713,-6.14845491737255,6.33424842373623));
#49298=CARTESIAN_POINT('Ctrl Pts',(2.89604883868045,-6.11597826385752,6.33783528514718));
#49299=CARTESIAN_POINT('Ctrl Pts',(3.05759478607773,-6.03948274128214,6.34628377993772));
#49300=CARTESIAN_POINT('Ctrl Pts',(3.21624791209868,-5.95651654239338,6.35473227472826));
#49301=CARTESIAN_POINT('Ctrl Pts',(3.37147378993975,-5.86732080968386,6.36318076951881));
#49302=CARTESIAN_POINT('Ctrl Pts',(3.52655787794422,-5.77820655210299,6.37162154709935));
#49303=CARTESIAN_POINT('Ctrl Pts',(3.67822067026002,-5.68287426856504,6.38006232467991));
#49304=CARTESIAN_POINT('Ctrl Pts',(3.82595070324274,-5.58161179377036,6.38850310226046));
#49305=CARTESIAN_POINT('Ctrl Pts',(3.97356851111394,-5.48042624438007,6.3969374676905));
#49306=CARTESIAN_POINT('Ctrl Pts',(4.11725924134089,-5.37331967226206,6.40537183312054));
#49307=CARTESIAN_POINT('Ctrl Pts',(4.25653854931731,-5.26062435250567,6.41380619855059));
#49308=CARTESIAN_POINT('Ctrl Pts',(4.39573344069351,-5.14799733690654,6.42223545194737));
#49309=CARTESIAN_POINT('Ctrl Pts',(4.53052198199207,-5.02978853632031,6.43066470534415));
#49310=CARTESIAN_POINT('Ctrl Pts',(4.660450878617,-4.90637204133543,6.43909395874094));
#49311=CARTESIAN_POINT('Ctrl Pts',(4.79032095660291,-4.783011416834,6.4475193962259));
#49312=CARTESIAN_POINT('Ctrl Pts',(4.91533553530226,-4.65444802811535,6.45594483371087));
#49313=CARTESIAN_POINT('Ctrl Pts',(5.03507604279997,-4.52109480582102,6.46437027119583));
#49314=CARTESIAN_POINT('Ctrl Pts',(5.15479024652157,-4.38777087765092,6.47279385783829));
#49315=CARTESIAN_POINT('Ctrl Pts',(5.26923246448506,-4.24965945989318,6.48121744448073));
#49316=CARTESIAN_POINT('Ctrl Pts',(5.37802214117491,-4.10720913139719,6.48964103112318));
#49317=CARTESIAN_POINT('Ctrl Pts',(5.48679964486749,-3.96477474234979,6.49806367521024));
#49318=CARTESIAN_POINT('Ctrl Pts',(5.58992566587883,-3.81800267535937,6.5064863192973));
#49319=CARTESIAN_POINT('Ctrl Pts',(5.68706079874458,-3.6673735112997,6.51490896338436));
#49320=CARTESIAN_POINT('Ctrl Pts',(5.78419860779792,-3.51674019722873,6.5233318395252));
#49321=CARTESIAN_POINT('Ctrl Pts',(5.87534501926892,-3.36224985462393,6.53175471566604));
#49322=CARTESIAN_POINT('Ctrl Pts',(5.96020452225528,-3.20441118661255,6.54017759180688));
#49323=CARTESIAN_POINT('Ctrl Pts',(6.04507819724907,-3.04654615866864,6.54860187461473));
#49324=CARTESIAN_POINT('Ctrl Pts',(6.12366271314895,-2.88533198435989,6.55702615742259));
#49325=CARTESIAN_POINT('Ctrl Pts',(6.19570882530371,-2.72130137104544,6.56545044023044));
#49326=CARTESIAN_POINT('Ctrl Pts',(6.26780359474061,-2.55715997751545,6.57388041248763));
#49327=CARTESIAN_POINT('Ctrl Pts',(6.33335100247243,-2.39019864968037,6.58231038474483));
#49328=CARTESIAN_POINT('Ctrl Pts',(6.392149834919,-2.22097039330673,6.59074035700202));
#49329=CARTESIAN_POINT('Ctrl Pts',(6.45096968699995,-2.05168164056049,6.59917334283835));
#49330=CARTESIAN_POINT('Ctrl Pts',(6.50303604976619,-1.88012466031485,6.60760632867468));
#49331=CARTESIAN_POINT('Ctrl Pts',(6.54819763334468,-1.70686752698011,6.61603931451101));
#49332=CARTESIAN_POINT('Ctrl Pts',(6.59340076530773,-1.53345099812744,6.62448005864346));
#49333=CARTESIAN_POINT('Ctrl Pts',(6.63168634815482,-1.35833151540637,6.63292080277589));
#49334=CARTESIAN_POINT('Ctrl Pts',(6.66295401245846,-1.18208833335911,6.64136154690834));
#49335=CARTESIAN_POINT('Ctrl Pts',(6.68024274100485,-1.08463876044005,6.64602866027563));
#49336=CARTESIAN_POINT('Ctrl Pts',(6.69538680924868,-0.986845782646499,
6.65069577364292));
#49337=CARTESIAN_POINT('Ctrl Pts',(6.70837605612388,-0.888808016178895,
6.65536288701021));
#49338=CARTESIAN_POINT('Ctrl Pts',(6.73103465036691,-0.717789789161911,
6.66350425418043));
#49339=CARTESIAN_POINT('Ctrl Pts',(6.74717813261609,-0.545686580013392,
6.67164562135067));
#49340=CARTESIAN_POINT('Ctrl Pts',(6.75670999377169,-0.373040292818122,
6.67978698852089));
#49341=CARTESIAN_POINT('Ctrl Pts',(6.76623353433732,-0.200544712703207,
6.68792124889665));
#49342=CARTESIAN_POINT('Ctrl Pts',(6.76915692190001,-0.0275073611784341,
6.69605550927243));
#49343=CARTESIAN_POINT('Ctrl Pts',(6.76543511410328,0.145522221184218,6.7041897696482));
#49344=CARTESIAN_POINT('Ctrl Pts',(6.76171584518942,0.318433769014059,6.71231848112526));
#49345=CARTESIAN_POINT('Ctrl Pts',(6.75136041403936,0.491337193762728,6.7204471926023));
#49346=CARTESIAN_POINT('Ctrl Pts',(6.73437578768639,0.663680457918825,6.72857590407938));
#49347=CARTESIAN_POINT('Ctrl Pts',(6.71739926098773,0.835941534758323,6.73670073912422));
#49348=CARTESIAN_POINT('Ctrl Pts',(6.69379987025165,1.00764261944256,6.74482557416907));
#49349=CARTESIAN_POINT('Ctrl Pts',(6.66363661077261,1.17823432286236,6.75295040921391));
#49350=CARTESIAN_POINT('Ctrl Pts',(6.6334817955826,1.34877826865671,6.76107296968841));
#49351=CARTESIAN_POINT('Ctrl Pts',(6.59676683623637,1.51821309179151,6.76919553016291));
#49352=CARTESIAN_POINT('Ctrl Pts',(6.55360225270403,1.68599718663843,6.77731809063741));
#49353=CARTESIAN_POINT('Ctrl Pts',(6.51043537508505,1.8537901987786,6.78544108280512));
#49354=CARTESIAN_POINT('Ctrl Pts',(6.46081827591302,2.01993195187524,6.79356407497283));
#49355=CARTESIAN_POINT('Ctrl Pts',(6.40491204692447,2.18389346607424,6.80168706714053));
#49356=CARTESIAN_POINT('Ctrl Pts',(6.37637361860923,2.26759082867735,6.80583360740764));
#49357=CARTESIAN_POINT('Ctrl Pts',(6.34619717801268,2.35072030385674,6.80998014767477));
#49358=CARTESIAN_POINT('Ctrl Pts',(6.31440909758854,2.43321325581854,6.81412668794188));
#49359=CARTESIAN_POINT('Ctrl Pts',(6.24553884434618,2.61193780969269,6.82311034705137));
#49360=CARTESIAN_POINT('Ctrl Pts',(6.16913507327727,2.78758505283654,6.83209400616087));
#49361=CARTESIAN_POINT('Ctrl Pts',(6.0855002992279,2.95955657288337,6.84107766527036));
#49362=CARTESIAN_POINT('Ctrl Pts',(6.00172184149015,3.13182353824678,6.85007675821453));
#49363=CARTESIAN_POINT('Ctrl Pts',(5.91068765571257,3.30040194380193,6.85907585115871));
#49364=CARTESIAN_POINT('Ctrl Pts',(5.81274584040255,3.4647185736915,6.86807494410289));
#49365=CARTESIAN_POINT('Ctrl Pts',(5.7145743788657,3.6294204802266,6.87709513740887));
#49366=CARTESIAN_POINT('Ctrl Pts',(5.60946300447908,3.78984041127712,6.88611533071484));
#49367=CARTESIAN_POINT('Ctrl Pts',(5.49780429068075,3.94543242007418,6.89513552402083));
#49368=CARTESIAN_POINT('Ctrl Pts',(5.38603249445696,4.10118200476601,6.90416485253268));
#49369=CARTESIAN_POINT('Ctrl Pts',(5.26770025628819,4.25209370862804,6.91319418104454));
#49370=CARTESIAN_POINT('Ctrl Pts',(5.14324103084691,4.39765399941979,6.92222350955639));
#49371=CARTESIAN_POINT('Ctrl Pts',(5.01860634297532,4.54341950089229,6.9312655676021));
#49372=CARTESIAN_POINT('Ctrl Pts',(4.88782755191063,4.68381832229776,6.9403076256478));
#49373=CARTESIAN_POINT('Ctrl Pts',(4.75137719411006,4.81837148415218,6.94934968369351));
#49374=CARTESIAN_POINT('Ctrl Pts',(4.63296199580585,4.93514024606876,6.95719661875341));
#49375=CARTESIAN_POINT('Ctrl Pts',(4.51027606519611,5.04750702371292,6.96504355381332));
#49376=CARTESIAN_POINT('Ctrl Pts',(4.3836493741138,5.15518255397728,6.97289048887322));
#49377=CARTESIAN_POINT('Ctrl Pts',(4.24400118439036,5.27393076377734,6.98154435376242));
#49378=CARTESIAN_POINT('Ctrl Pts',(4.09943611034982,5.38707693006477,6.99019821865163));
#49379=CARTESIAN_POINT('Ctrl Pts',(3.95042111681411,5.49422078186062,6.99885208354083));
#49380=CARTESIAN_POINT('Ctrl Pts',(3.8015765489339,5.60124209524111,7.00749605116693));
#49381=CARTESIAN_POINT('Ctrl Pts',(3.64829246275145,5.7022746152954,7.01614001879301));
#49382=CARTESIAN_POINT('Ctrl Pts',(3.4910679425598,5.79695899764966,7.02478398641911));
#49383=CARTESIAN_POINT('Ctrl Pts',(3.36292878294622,5.87412747727749,7.03182888467026));
#49384=CARTESIAN_POINT('Ctrl Pts',(3.23217292507896,5.94707998107329,7.03887378292142));
#49385=CARTESIAN_POINT('Ctrl Pts',(3.09908550384722,6.01564277861012,7.04591868117257));
#49386=CARTESIAN_POINT('Ctrl Pts',(3.09908550384713,6.01564277861016,5.04570102894007));
#49387=CARTESIAN_POINT('Ctrl Pts',(2.96060988807933,6.08698141842904,5.05304231185843));
#49388=CARTESIAN_POINT('Ctrl Pts',(2.81975889686845,6.15349062528649,5.06038359477678));
#49389=CARTESIAN_POINT('Ctrl Pts',(2.67689005748957,6.21502603535283,5.06772487769516));
#49390=CARTESIAN_POINT('Ctrl Pts',(2.51502762950118,6.28474222345865,5.07604214185773));
#49391=CARTESIAN_POINT('Ctrl Pts',(2.35028361639528,6.34819853892449,5.08435940602031));
#49392=CARTESIAN_POINT('Ctrl Pts',(2.18317710810674,6.40515625997045,5.0926766701829));
#49393=CARTESIAN_POINT('Ctrl Pts',(2.01621154182683,6.46206594138173,5.10098691934691));
#49394=CARTESIAN_POINT('Ctrl Pts',(1.84688777793817,6.51248783712324,5.10929716851094));
#49395=CARTESIAN_POINT('Ctrl Pts',(1.67574511035961,6.55623118301253,5.11760741767495));
#49396=CARTESIAN_POINT('Ctrl Pts',(1.50471544614211,6.5999456457181,5.12591217968546));
#49397=CARTESIAN_POINT('Ctrl Pts',(1.33186960724448,6.63699025972096,5.13421694169597));
#49398=CARTESIAN_POINT('Ctrl Pts',(1.15776250433495,6.66722393380904,5.14252170370648));
#49399=CARTESIAN_POINT('Ctrl Pts',(0.983738490705086,6.69744317945532,5.15082250242841));
#49400=CARTESIAN_POINT('Ctrl Pts',(0.808454754614934,6.72085790351684,5.15912330115034));
#49401=CARTESIAN_POINT('Ctrl Pts',(0.632477093025629,6.73737795635645,5.16742409987226));
#49402=CARTESIAN_POINT('Ctrl Pts',(0.456551210467332,6.75389314839544,5.17572245619718));
#49403=CARTESIAN_POINT('Ctrl Pts',(0.279932155294058,6.76351768047052,5.1840208125221));
#49404=CARTESIAN_POINT('Ctrl Pts',(0.10319178066811,6.76621315481581,5.19231916884702));
#49405=CARTESIAN_POINT('Ctrl Pts',(-0.0735665763870974,6.76890890341184,
5.20061836948726));
#49406=CARTESIAN_POINT('Ctrl Pts',(-0.250445929904685,6.76467417280375,
5.2089175701275));
#49407=CARTESIAN_POINT('Ctrl Pts',(-0.42687288964805,6.75352267606199,5.21721677076773));
#49408=CARTESIAN_POINT('Ctrl Pts',(-0.603317735450877,6.74237004878818,
5.22551681277596));
#49409=CARTESIAN_POINT('Ctrl Pts',(-0.779309748703458,6.72429927912349,
5.23381685478417));
#49410=CARTESIAN_POINT('Ctrl Pts',(-0.954279217350867,6.6993761034392,5.2421168967924));
#49411=CARTESIAN_POINT('Ctrl Pts',(-1.12929546965289,6.67444626375089,5.25041915808094));
#49412=CARTESIAN_POINT('Ctrl Pts',(-1.30328828795574,6.64266041533566,5.25872141936948));
#49413=CARTESIAN_POINT('Ctrl Pts',(-1.47569653483271,6.60413572975925,5.26702368065803));
#49414=CARTESIAN_POINT('Ctrl Pts',(-1.64817950415611,6.56559434742496,5.27532954018091));
#49415=CARTESIAN_POINT('Ctrl Pts',(-1.81907619401594,6.52030838287258,5.2836353997038));
#49416=CARTESIAN_POINT('Ctrl Pts',(-1.98783885772199,6.46844538322235,5.29194125922669));
#49417=CARTESIAN_POINT('Ctrl Pts',(-2.15680101067289,6.41652107788751,5.30025693685512));
#49418=CARTESIAN_POINT('Ctrl Pts',(-2.32362376455614,6.35800430652203,5.30857261448358));
#49419=CARTESIAN_POINT('Ctrl Pts',(-2.48777653396244,6.29311186274849,5.31688829211201));
#49420=CARTESIAN_POINT('Ctrl Pts',(-2.6520331285876,6.2281783750608,5.32520922933523));
#49421=CARTESIAN_POINT('Ctrl Pts',(-2.8136160531346,6.15686131328763,5.33353016655844));
#49422=CARTESIAN_POINT('Ctrl Pts',(-2.97201757871664,6.07942435694362,5.34185110378165));
#49423=CARTESIAN_POINT('Ctrl Pts',(-3.13065453812543,6.00187230525001,5.35018440849997));
#49424=CARTESIAN_POINT('Ctrl Pts',(-3.28610034261774,5.91818234570724,5.35851771321829));
#49425=CARTESIAN_POINT('Ctrl Pts',(-3.43787343049739,5.82866324948355,5.36685101793661));
#49426=CARTESIAN_POINT('Ctrl Pts',(-3.54958768017435,5.76277173468273,5.37298483847715));
#49427=CARTESIAN_POINT('Ctrl Pts',(-3.65931267820274,5.69372300525311,5.37911865901768));
#49428=CARTESIAN_POINT('Ctrl Pts',(-3.76686754625777,5.62165437295375,5.38525247955822));
#49429=CARTESIAN_POINT('Ctrl Pts',(-3.90796295367395,5.52711143668235,5.39329910658529));
#49430=CARTESIAN_POINT('Ctrl Pts',(-4.04576267621236,5.42707475399575,5.40134573361236));
#49431=CARTESIAN_POINT('Ctrl Pts',(-4.17979619976959,5.32180352215222,5.40939236063943));
#49432=CARTESIAN_POINT('Ctrl Pts',(-4.31366165359394,5.21666429391006,5.41742889769484));
#49433=CARTESIAN_POINT('Ctrl Pts',(-4.4437700129408,5.1063038040983,5.42546543475023));
#49434=CARTESIAN_POINT('Ctrl Pts',(-4.56967686955862,4.99102617783367,5.43350197180564));
#49435=CARTESIAN_POINT('Ctrl Pts',(-4.69545376133827,4.87586754459646,5.44153021330618));
#49436=CARTESIAN_POINT('Ctrl Pts',(-4.81703750576381,4.75580212563093,5.44955845480673));
#49437=CARTESIAN_POINT('Ctrl Pts',(-4.93401423702517,4.63117614746329,5.45758669630726));
#49438=CARTESIAN_POINT('Ctrl Pts',(-5.05089610727587,4.50665123338008,5.46560842739248));
#49439=CARTESIAN_POINT('Ctrl Pts',(-5.1631781441165,4.37757339245244,5.4736301584777));
#49440=CARTESIAN_POINT('Ctrl Pts',(-5.27048114814646,4.24432768139229,5.48165188956293));
#49441=CARTESIAN_POINT('Ctrl Pts',(-5.37772084964118,4.11116057755657,5.48966888829308));
#49442=CARTESIAN_POINT('Ctrl Pts',(-5.47998713047492,3.97383078937911,5.49768588702323));
#49443=CARTESIAN_POINT('Ctrl Pts',(-5.57693922378061,3.83275852282105,5.50570288575338));
#49444=CARTESIAN_POINT('Ctrl Pts',(-5.67386901811393,3.69171870287106,5.51371804057458));
#49445=CARTESIAN_POINT('Ctrl Pts',(-5.76548683904399,3.54693842249234,5.52173319539578));
#49446=CARTESIAN_POINT('Ctrl Pts',(-5.85149359751363,3.39886917639632,5.52974835021698));
#49447=CARTESIAN_POINT('Ctrl Pts',(-5.9374922841178,3.2508138268249,5.53776275280367));
#49448=CARTESIAN_POINT('Ctrl Pts',(-6.01788076646333,3.09947044990491,5.54577715539037));
#49449=CARTESIAN_POINT('Ctrl Pts',(-6.0924046714446,2.94531735460885,5.55379155797706));
#49450=CARTESIAN_POINT('Ctrl Pts',(-6.16693648268986,2.7911479051635,5.56180681081419));
#49451=CARTESIAN_POINT('Ctrl Pts',(-6.23560231446444,2.63416848215493,5.56982206365131));
#49452=CARTESIAN_POINT('Ctrl Pts',(-6.29819500581745,2.47487952609741,5.57783731648844));
#49453=CARTESIAN_POINT('Ctrl Pts',(-6.36080685614849,2.31554181333134,5.5858550227119));
#49454=CARTESIAN_POINT('Ctrl Pts',(-6.41734172925842,2.15389351004909,5.59387272893535));
#49455=CARTESIAN_POINT('Ctrl Pts',(-6.46764166901062,1.99045227053492,5.60189043515881));
#49456=CARTESIAN_POINT('Ctrl Pts',(-6.51799867509558,1.82682560351907,5.60991723763752));
#49457=CARTESIAN_POINT('Ctrl Pts',(-6.56210650942972,1.66140229693687,5.61794404011624));
#49458=CARTESIAN_POINT('Ctrl Pts',(-6.59985770159272,1.49471312255139,5.62597084259495));
#49459=CARTESIAN_POINT('Ctrl Pts',(-6.6376307381098,1.32792749512324,5.63400228970356));
#49460=CARTESIAN_POINT('Ctrl Pts',(-6.66903973921222,1.15987490950143,5.64203373681217));
#49461=CARTESIAN_POINT('Ctrl Pts',(-6.69402897970091,0.991092840718971,
5.65006518392077));
#49462=CARTESIAN_POINT('Ctrl Pts',(-6.71905865329892,0.822037679049174,
5.65810962607735));
#49463=CARTESIAN_POINT('Ctrl Pts',(-6.73764777526922,0.652251048843681,
5.66615406823393));
#49464=CARTESIAN_POINT('Ctrl Pts',(-6.74979270623879,0.482273182756081,
5.67419851039051));
#49465=CARTESIAN_POINT('Ctrl Pts',(-6.76135787439611,0.320409553456583,
5.6818589348512));
#49466=CARTESIAN_POINT('Ctrl Pts',(-6.76707983323911,0.158372786142489,
5.68951935931186));
#49467=CARTESIAN_POINT('Ctrl Pts',(-6.76699915828328,-0.00337517308298123,
5.69717978377255));
#49468=CARTESIAN_POINT('',(-6.76699945935947,-0.00162771900841451,5.30282021618985));
#49469=CARTESIAN_POINT('Ctrl Pts',(3.09908550384716,6.01564277861015,4.65139679042609));
#49470=CARTESIAN_POINT('Ctrl Pts',(2.93373232018321,6.10082796552484,4.66014623832538));
#49471=CARTESIAN_POINT('Ctrl Pts',(2.76486502144414,6.17919158180196,4.66889568622467));
#49472=CARTESIAN_POINT('Ctrl Pts',(2.59305716434336,6.25046746591386,4.67764513412396));
#49473=CARTESIAN_POINT('Ctrl Pts',(2.42125069459268,6.3217427744723,4.68639451137138));
#49474=CARTESIAN_POINT('Ctrl Pts',(2.24650397871045,6.3859303555783,4.6951438886188));
#49475=CARTESIAN_POINT('Ctrl Pts',(2.06941053323759,6.44281220003543,4.70389326586621));
#49476=CARTESIAN_POINT('Ctrl Pts',(1.89231845896674,6.49969360406688,4.71264257536881));
#49477=CARTESIAN_POINT('Ctrl Pts',(1.71287996431498,6.54926929700883,4.7213918848714));
#49478=CARTESIAN_POINT('Ctrl Pts',(1.531704491735,6.5913709006548,4.730141194374));
#49479=CARTESIAN_POINT('Ctrl Pts',(1.35053036178162,6.63347219230085,4.73889043903859));
#49480=CARTESIAN_POINT('Ctrl Pts',(1.16761955878833,6.66809944062456,4.74763968370318));
#49481=CARTESIAN_POINT('Ctrl Pts',(0.983593309310341,6.69513503985393,4.75638892836777));
#49482=CARTESIAN_POINT('Ctrl Pts',(0.799568362459814,6.72217044771216,4.76513811110095));
#49483=CARTESIAN_POINT('Ctrl Pts',(0.614428268438406,6.74161427235979,4.77388729383413));
#49484=CARTESIAN_POINT('Ctrl Pts',(0.428801816330058,6.75340047696803,4.7826364765673));
#49485=CARTESIAN_POINT('Ctrl Pts',(0.243176616522525,6.76518660206243,4.79138560027544));
#49486=CARTESIAN_POINT('Ctrl Pts',(0.0570653511651543,6.76931519233997,
4.80013472398358));
#49487=CARTESIAN_POINT('Ctrl Pts',(-0.128899900800383,6.76577222610794,
4.80888384769172));
#49488=CARTESIAN_POINT('Ctrl Pts',(-0.314863959942484,6.76222928260131,
4.81763291528098));
#49489=CARTESIAN_POINT('Ctrl Pts',(-0.500681721081251,6.75101488651273,
4.82638198287024));
#49490=CARTESIAN_POINT('Ctrl Pts',(-0.685722110173975,6.73216712415984,
4.83513105045951));
#49491=CARTESIAN_POINT('Ctrl Pts',(-0.870761373828219,6.71331947644137,
4.84388006483587));
#49492=CARTESIAN_POINT('Ctrl Pts',(-1.05502298984397,6.68683858439988,4.85262907921223));
#49493=CARTESIAN_POINT('Ctrl Pts',(-1.23788117676106,6.65281438131417,4.86137809358858));
#49494=CARTESIAN_POINT('Ctrl Pts',(-1.4300964145184,6.61704912302367,4.87057480447611));
#49495=CARTESIAN_POINT('Ctrl Pts',(-1.62076048992743,6.57294837083153,4.87977151536364));
#49496=CARTESIAN_POINT('Ctrl Pts',(-1.80915798961179,6.52067760042036,4.88896822625117));
#49497=CARTESIAN_POINT('Ctrl Pts',(-1.98840443003052,6.47094578577396,4.89771822395767));
#49498=CARTESIAN_POINT('Ctrl Pts',(-2.16559895952225,6.41381888474464,4.90646822166418));
#49499=CARTESIAN_POINT('Ctrl Pts',(-2.34013966242349,6.34949095285225,4.91521821937069));
#49500=CARTESIAN_POINT('Ctrl Pts',(-2.51467682554032,6.28516432556678,4.92396803962228));
#49501=CARTESIAN_POINT('Ctrl Pts',(-2.68656000078851,6.21363705879657,4.93271785987386));
#49502=CARTESIAN_POINT('Ctrl Pts',(-2.85520533840889,6.13515211510859,4.94146768012546));
#49503=CARTESIAN_POINT('Ctrl Pts',(-3.02384747998326,6.05666865881122,4.9502173345567));
#49504=CARTESIAN_POINT('Ctrl Pts',(-3.18925164684535,5.97122791039845,4.95896698898793));
#49505=CARTESIAN_POINT('Ctrl Pts',(-3.35085601829155,5.8791200825191,4.96771664341918));
#49506=CARTESIAN_POINT('Ctrl Pts',(-3.51245754191412,5.78701387778178,4.97646614366232));
#49507=CARTESIAN_POINT('Ctrl Pts',(-3.67025915510926,5.68824097060989,4.98521564390547));
#49508=CARTESIAN_POINT('Ctrl Pts',(-3.82372487928822,5.58313684656863,4.9939651441486));
#49509=CARTESIAN_POINT('Ctrl Pts',(-3.97718810300776,5.47803443501788,5.00271450183372));
#49510=CARTESIAN_POINT('Ctrl Pts',(-4.12631534262996,5.36660117496398,5.01146385951883));
#49511=CARTESIAN_POINT('Ctrl Pts',(-4.27060009886188,5.24921554097381,5.02021321720395));
#49512=CARTESIAN_POINT('Ctrl Pts',(-4.41488269594184,5.13183166360317,5.02896244395913));
#49513=CARTESIAN_POINT('Ctrl Pts',(-4.55432273235067,5.00849577139491,5.03771167071432));
#49514=CARTESIAN_POINT('Ctrl Pts',(-4.68844662480192,4.87962675277356,5.0464608974695));
#49515=CARTESIAN_POINT('Ctrl Pts',(-4.82256868835141,4.75075949139898,5.05521000492099));
#49516=CARTESIAN_POINT('Ctrl Pts',(-4.95137454637844,4.61635945312545,5.06395911237248));
#49517=CARTESIAN_POINT('Ctrl Pts',(-5.07442674461058,4.47688309134613,5.07270821982397));
#49518=CARTESIAN_POINT('Ctrl Pts',(-5.19747742838508,4.33740844616388,5.08145721959633));
#49519=CARTESIAN_POINT('Ctrl Pts',(-5.31477440450886,4.19285781736081,5.09020621936869));
#49520=CARTESIAN_POINT('Ctrl Pts',(-5.42591931531102,4.04372211999474,5.09895521914106));
#49521=CARTESIAN_POINT('Ctrl Pts',(-5.53707636462934,3.89457013500869,5.10770517442164));
#49522=CARTESIAN_POINT('Ctrl Pts',(-5.64207983273426,3.74083230916487,5.11645512970222));
#49523=CARTESIAN_POINT('Ctrl Pts',(-5.74057303468706,3.58303087251894,5.1252050849828));
#49524=CARTESIAN_POINT('Ctrl Pts',(-5.83906243363735,3.42523552887483,5.13395470241161));
#49525=CARTESIAN_POINT('Ctrl Pts',(-5.93104191768405,3.26337713157031,5.14270431984042));
#49526=CARTESIAN_POINT('Ctrl Pts',(-6.01619906699645,3.09800545291178,5.15145393726924));
#49527=CARTESIAN_POINT('Ctrl Pts',(-6.10135338095373,2.93263928039616,5.16020326337463));
#49528=CARTESIAN_POINT('Ctrl Pts',(-6.1796856835283,2.76376031540244,5.16895258948003));
#49529=CARTESIAN_POINT('Ctrl Pts',(-6.25092992694879,2.5919421383156,5.17770191558542));
#49530=CARTESIAN_POINT('Ctrl Pts',(-6.32217217691096,2.42012876880839,5.18645099687921));
#49531=CARTESIAN_POINT('Ctrl Pts',(-6.38632665483843,2.24537661647691,5.19520007817299));
#49532=CARTESIAN_POINT('Ctrl Pts',(-6.44317547869343,2.06827917621478,5.20394915946679));
#49533=CARTESIAN_POINT('Ctrl Pts',(-6.50002944235931,1.89116572423442,5.21269903178175));
#49534=CARTESIAN_POINT('Ctrl Pts',(-6.54957634250395,1.71170683289213,5.22144890409672));
#49535=CARTESIAN_POINT('Ctrl Pts',(-6.59164787708393,1.53051209225375,5.23019877641168));
#49536=CARTESIAN_POINT('Ctrl Pts',(-6.63371649075007,1.34932993148038,5.23894804124648));
#49537=CARTESIAN_POINT('Ctrl Pts',(-6.66831071257123,1.16641244174009,5.24769730608128));
#49538=CARTESIAN_POINT('Ctrl Pts',(-6.69531304840333,0.98238087516003,5.25644657091607));
#49539=CARTESIAN_POINT('Ctrl Pts',(-6.72231677033044,0.79833986179583,5.26519628487173));
#49540=CARTESIAN_POINT('Ctrl Pts',(-6.7417277847789,0.613184940730109,5.27394599882738));
#49541=CARTESIAN_POINT('Ctrl Pts',(-6.75348015835518,0.427545027690477,
5.28269571278304));
#49542=CARTESIAN_POINT('Ctrl Pts',(-6.76249038365217,0.285219953547529,
5.28940388058531));
#49543=CARTESIAN_POINT('Ctrl Pts',(-6.76699999999996,0.1426099957588,5.29611204838757));
#49544=CARTESIAN_POINT('Ctrl Pts',(-6.767,2.19816073760199E-12,5.30282021618984));
#49545=CARTESIAN_POINT('Ctrl Pts',(-6.76699850691525,-0.00449526492710441,
5.30282021618984));
#49546=CARTESIAN_POINT('Ctrl Pts',(-6.76686712558602,-0.202271652565106,
5.3121201420737));
#49547=CARTESIAN_POINT('Ctrl Pts',(-6.75806106437177,-0.39986068289801,
5.32142006795755));
#49548=CARTESIAN_POINT('Ctrl Pts',(-6.74065422882093,-0.596548042892271,
5.33071999384141));
#49549=CARTESIAN_POINT('Ctrl Pts',(-6.72321584937777,-0.793591830962378,
5.34003677263686));
#49550=CARTESIAN_POINT('Ctrl Pts',(-6.69714555455995,-0.989730505222333,
5.34935355143229));
#49551=CARTESIAN_POINT('Ctrl Pts',(-6.6625689230473,-1.18425687485627,5.35867033022774));
#49552=CARTESIAN_POINT('Ctrl Pts',(-6.6279234183554,-1.37917072149241,5.36800566711135));
#49553=CARTESIAN_POINT('Ctrl Pts',(-6.58473771102242,-1.57246566374954,
5.37734100399497));
#49554=CARTESIAN_POINT('Ctrl Pts',(-6.53318870196399,-1.76344389888935,
5.38667634087858));
#49555=CARTESIAN_POINT('Ctrl Pts',(-6.48899557088559,-1.92717015343461,
5.39467955518074));
#49556=CARTESIAN_POINT('Ctrl Pts',(-6.43865651999273,-2.08919386410022,
5.40268276948291));
#49557=CARTESIAN_POINT('Ctrl Pts',(-6.38231203820803,-2.24908471315442,
5.41068598378507));
#49558=CARTESIAN_POINT('Ctrl Pts',(-6.32138973410239,-2.42196622029136,
5.41933943555346));
#49559=CARTESIAN_POINT('Ctrl Pts',(-6.25340012608952,-2.59248103478967,
5.42799288732183));
#49560=CARTESIAN_POINT('Ctrl Pts',(-6.17854530260445,-2.76004835893586,
5.43664633909022));
#49561=CARTESIAN_POINT('Ctrl Pts',(-6.10375943657722,-2.9274613173892,5.44529181916075));
#49562=CARTESIAN_POINT('Ctrl Pts',(-6.02212109271198,-3.09193192456616,
5.45393729923131));
#49563=CARTESIAN_POINT('Ctrl Pts',(-5.93388087430132,-3.25289821076544,
5.46258277930184));
#49564=CARTESIAN_POINT('Ctrl Pts',(-5.84298590354066,-3.41870725046482,
5.47148836308639));
#49565=CARTESIAN_POINT('Ctrl Pts',(-5.74508571091698,-3.58079750791184,
5.48039394687094));
#49566=CARTESIAN_POINT('Ctrl Pts',(-5.64050693340576,-3.73857867834844,
5.48929953065549));
#49567=CARTESIAN_POINT('Ctrl Pts',(-5.53917520796711,-3.89146092293535,
5.49792860619455));
#49568=CARTESIAN_POINT('Ctrl Pts',(-5.43157357537333,-4.04029736648063,
5.5065576817336));
#49569=CARTESIAN_POINT('Ctrl Pts',(-5.31804515951534,-4.18457700148479,
5.51518675727266));
#49570=CARTESIAN_POINT('Ctrl Pts',(-5.19905992335141,-4.33579153499937,
5.52423059517995));
#49571=CARTESIAN_POINT('Ctrl Pts',(-5.07356426827074,-4.48200010995743,
5.53327443308723));
#49572=CARTESIAN_POINT('Ctrl Pts',(-4.94200381528476,-4.6226493799239,5.54231827099453));
#49573=CARTESIAN_POINT('Ctrl Pts',(-4.81044336229875,-4.76329864989043,
5.55136210890182));
#49574=CARTESIAN_POINT('Ctrl Pts',(-4.67281834933547,-4.89838830979678,
5.56040594680911));
#49575=CARTESIAN_POINT('Ctrl Pts',(-4.52962289084241,-5.02740544085679,
5.56944978471641));
#49576=CARTESIAN_POINT('Ctrl Pts',(-4.39621318227486,-5.14760574634184,
5.57787558112254));
#49577=CARTESIAN_POINT('Ctrl Pts',(-4.25802693377784,-5.26248265905892,
5.58630137752867));
#49578=CARTESIAN_POINT('Ctrl Pts',(-4.11552196541618,-5.37166342506462,
5.5947271739348));
#49579=CARTESIAN_POINT('Ctrl Pts',(-3.97298392881197,-5.48086952643998,
5.60315492554489));
#49580=CARTESIAN_POINT('Ctrl Pts',(-3.82612543733519,-5.584376644035,5.61158267715496));
#49581=CARTESIAN_POINT('Ctrl Pts',(-3.6754352504014,-5.68185398616568,5.62001042876506));
#49582=CARTESIAN_POINT('Ctrl Pts',(-3.52468969024317,-5.77936714771402,
5.62844127727078));
#49583=CARTESIAN_POINT('Ctrl Pts',(-3.37010990539355,-5.87084593587486,
5.63687212577652));
#49584=CARTESIAN_POINT('Ctrl Pts',(-3.2122116538631,-5.95600413790875,5.64530297428225));
#49585=CARTESIAN_POINT('Ctrl Pts',(-3.0541683115073,-6.04124059080164,5.65374156979439));
#49586=CARTESIAN_POINT('Ctrl Pts',(-2.89280070223597,-6.12014469643793,
5.66218016530653));
#49587=CARTESIAN_POINT('Ctrl Pts',(-2.72864809358529,-6.19247677277625,
5.67061876081867));
#49588=CARTESIAN_POINT('Ctrl Pts',(-2.56440940912534,-6.26484677749145,
5.67906178123118));
#49589=CARTESIAN_POINT('Ctrl Pts',(-2.3973831189156,-6.33063775359861,5.68750480164366));
#49590=CARTESIAN_POINT('Ctrl Pts',(-2.22812680736587,-6.38965882737862,
5.69594782205617));
#49591=CARTESIAN_POINT('Ctrl Pts',(-2.0586926790306,-6.4487419073404,5.70439971251161));
#49592=CARTESIAN_POINT('Ctrl Pts',(-1.88702416464294,-6.50104077596697,
5.71285160296706));
#49593=CARTESIAN_POINT('Ctrl Pts',(-1.71369331326014,-6.54641460863025,
5.7213034934225));
#49594=CARTESIAN_POINT('Ctrl Pts',(-1.66645606399572,-6.55878018017448,
5.7236068574977));
#49595=CARTESIAN_POINT('Ctrl Pts',(-1.61909540894081,-6.57063171786553,
5.72591022157289));
#49596=CARTESIAN_POINT('Ctrl Pts',(-1.57162304102097,-6.58196703250115,
5.72821358564809));
#49597=CARTESIAN_POINT('Ctrl Pts',(-1.40020410266727,-6.62289795054643,
5.73653084981068));
#49598=CARTESIAN_POINT('Ctrl Pts',(-1.22701956688522,-6.65716762216335,
5.74484811397329));
#49599=CARTESIAN_POINT('Ctrl Pts',(-1.05262176761499,-6.68462986367556,
5.75316537813588));
#49600=CARTESIAN_POINT('Ctrl Pts',(-0.878371060019486,-6.71206894281351,
5.76147562729988));
#49601=CARTESIAN_POINT('Ctrl Pts',(-0.702909469604499,-6.73271197739186,
5.76978587646388));
#49602=CARTESIAN_POINT('Ctrl Pts',(-0.526801012309971,-6.74646349530102,
5.77809612562788));
#49603=CARTESIAN_POINT('Ctrl Pts',(-0.35080883722523,-6.76020593325504,
5.78640088763839));
#49604=CARTESIAN_POINT('Ctrl Pts',(-0.174170991962337,-6.7670658947502,
5.7947056496489));
#49605=CARTESIAN_POINT('Ctrl Pts',(0.00254163895903234,-6.76699952268887,
5.80301041165941));
#49606=CARTESIAN_POINT('Ctrl Pts',(0.179169937162344,-6.76693318230234,
5.81131121038134));
#49607=CARTESIAN_POINT('Ctrl Pts',(0.355872602784891,-6.75994709595507,
5.81961200910326));
#49608=CARTESIAN_POINT('Ctrl Pts',(0.532076760645481,-6.74604946029756,
5.82791280782519));
#49609=CARTESIAN_POINT('Ctrl Pts',(0.708229072831554,-6.73215591383014,
5.8362111641501));
#49610=CARTESIAN_POINT('Ctrl Pts',(0.883882823289214,-6.7113548989976,5.84450952047502));
#49611=CARTESIAN_POINT('Ctrl Pts',(1.0584680436725,-6.68370663633018,5.85280787679993));
#49612=CARTESIAN_POINT('Ctrl Pts',(1.23307102720931,-6.6560555605934,5.86110707744017));
#49613=CARTESIAN_POINT('Ctrl Pts',(1.40660491873926,-6.62155589197754,5.8694062780804));
#49614=CARTESIAN_POINT('Ctrl Pts',(1.57850717050345,-6.58031945369442,5.87770547872064));
#49615=CARTESIAN_POINT('Ctrl Pts',(1.75042684961498,-6.53907883488588,5.88600552072887));
#49616=CARTESIAN_POINT('Ctrl Pts',(1.92071422071009,-6.49110016576597,5.8943055627371));
#49617=CARTESIAN_POINT('Ctrl Pts',(2.08881927963228,-6.43654589178361,5.90260560474533));
#49618=CARTESIAN_POINT('Ctrl Pts',(2.25696928679073,-6.3819770309803,5.91090786603388));
#49619=CARTESIAN_POINT('Ctrl Pts',(2.42293548783468,-6.32082916845419,5.91921012732243));
#49620=CARTESIAN_POINT('Ctrl Pts',(2.58618514530947,-6.25331395295172,5.92751238861098));
#49621=CARTESIAN_POINT('Ctrl Pts',(2.74950555586026,-6.18576947607591,5.93581824813387));
#49622=CARTESIAN_POINT('Ctrl Pts',(2.91010675505354,-6.11185227910375,5.94412410765676));
#49623=CARTESIAN_POINT('Ctrl Pts',(3.06747783523843,-6.03182134436366,5.95242996717965));
#49624=CARTESIAN_POINT('Ctrl Pts',(3.22503493902153,-5.9516958074741,5.96074564480809));
#49625=CARTESIAN_POINT('Ctrl Pts',(3.37935398466859,-5.86544225163518,5.96906132243655));
#49626=CARTESIAN_POINT('Ctrl Pts',(3.52994941545288,-5.77336523392933,5.97737700006499));
#49627=CARTESIAN_POINT('Ctrl Pts',(3.68064009655534,-5.68122997829961,5.9856979372882));
#49628=CARTESIAN_POINT('Ctrl Pts',(3.82760217695544,-5.58326410807159,5.9940188745114));
#49629=CARTESIAN_POINT('Ctrl Pts',(3.97038065700308,-5.47981445292592,6.0023398117346));
#49630=CARTESIAN_POINT('Ctrl Pts',(4.11337135018338,-5.37621103948709,6.01067311645292));
#49631=CARTESIAN_POINT('Ctrl Pts',(4.2521657429859,-5.26710776735871,6.01900642117124));
#49632=CARTESIAN_POINT('Ctrl Pts',(4.38634234683893,-5.15289140350615,6.02733972588956));
#49633=CARTESIAN_POINT('Ctrl Pts',(4.48510451102092,-5.06882119338642,6.03347354643007));
#49634=CARTESIAN_POINT('Ctrl Pts',(4.58136554754155,-4.98198159944445,6.03960736697059));
#49635=CARTESIAN_POINT('Ctrl Pts',(4.6749708000818,-4.89253891332328,6.0457411875111));
#49636=CARTESIAN_POINT('Ctrl Pts',(4.79814471550554,-4.77484246406876,6.0538126009412));
#49637=CARTESIAN_POINT('Ctrl Pts',(4.91709761676779,-4.65227487782898,6.06188401437129));
#49638=CARTESIAN_POINT('Ctrl Pts',(5.03140928200621,-4.52517509461698,6.06995542780139));
#49639=CARTESIAN_POINT('Ctrl Pts',(5.14557743843213,-4.39823487463869,6.07801670824152));
#49640=CARTESIAN_POINT('Ctrl Pts',(5.25511570620615,-4.26677405271283,6.08607798868166));
#49641=CARTESIAN_POINT('Ctrl Pts',(5.35963739888591,-4.1311712567338,6.0941392691218));
#49642=CARTESIAN_POINT('Ctrl Pts',(5.46405079534005,-3.99570896049804,6.10219219716902));
#49643=CARTESIAN_POINT('Ctrl Pts',(5.56345773458674,-3.85611352341332,6.11024512521624));
#49644=CARTESIAN_POINT('Ctrl Pts',(5.6575089208742,-3.71279972665222,6.11829805326346));
#49645=CARTESIAN_POINT('Ctrl Pts',(5.75148325460727,-3.56960303666878,6.12634440097804));
#49646=CARTESIAN_POINT('Ctrl Pts',(5.84011034227156,-3.42269434469623,6.13439074869264));
#49647=CARTESIAN_POINT('Ctrl Pts',(5.92308175312647,-3.27252067155889,6.14243709640722));
#49648=CARTESIAN_POINT('Ctrl Pts',(6.00600351495872,-3.12243686041164,6.15047862929106));
#49649=CARTESIAN_POINT('Ctrl Pts',(6.08327615720387,-2.96909228302733,6.15852016217489));
#49650=CARTESIAN_POINT('Ctrl Pts',(6.15463516987641,-2.81296194885754,6.16656169505873));
#49651=CARTESIAN_POINT('Ctrl Pts',(6.22736603805992,-2.65383005607113,6.17475782398854));
#49652=CARTESIAN_POINT('Ctrl Pts',(6.2939533711383,-2.49180453750885,6.18295395291833));
#49653=CARTESIAN_POINT('Ctrl Pts',(6.3541666018031,-2.32741397188599,6.19115008184814));
#49654=CARTESIAN_POINT('Ctrl Pts',(6.41322369269179,-2.16617983001973,6.19918883887544));
#49655=CARTESIAN_POINT('Ctrl Pts',(6.46614912570988,-2.0026710103283,6.20722759590274));
#49656=CARTESIAN_POINT('Ctrl Pts',(6.51277444295866,-1.83740525065771,6.21526635293004));
#49657=CARTESIAN_POINT('Ctrl Pts',(6.55940427304571,-1.67212349500706,6.22330588802412));
#49658=CARTESIAN_POINT('Ctrl Pts',(6.5997326716581,-1.50508482020148,6.23134542311823));
#49659=CARTESIAN_POINT('Ctrl Pts',(6.63364150784911,-1.33682061075577,6.23938495821231));
#49660=CARTESIAN_POINT('Ctrl Pts',(6.66756034001819,-1.1685067987422,6.24742686327911));
#49661=CARTESIAN_POINT('Ctrl Pts',(6.69505576921223,-0.998967098891834,
6.25546876834588));
#49662=CARTESIAN_POINT('Ctrl Pts',(6.71606110128753,-0.828741385338382,
6.26351067341267));
#49663=CARTESIAN_POINT('Ctrl Pts',(6.73777498972122,-0.652773581573344,
6.27182384974279));
#49664=CARTESIAN_POINT('Ctrl Pts',(6.75255321792446,-0.476073106315516,
6.28013702607293));
#49665=CARTESIAN_POINT('Ctrl Pts',(6.76038053759128,-0.299239013093287,
6.28845020240306));
#49666=CARTESIAN_POINT('Ctrl Pts',(6.76796558691103,-0.127878269493019,
6.2965060702035));
#49667=CARTESIAN_POINT('Ctrl Pts',(6.7690236753614,0.0436075749619817,6.30456193800392));
#49668=CARTESIAN_POINT('Ctrl Pts',(6.76359393379158,0.214676730871604,6.31261780580436));
#49669=CARTESIAN_POINT('Ctrl Pts',(6.75790404914573,0.393941941024649,6.32105963639933));
#49670=CARTESIAN_POINT('Ctrl Pts',(6.74508940122597,0.572749067923802,6.32950146699429));
#49671=CARTESIAN_POINT('Ctrl Pts',(6.72525545491745,0.750485220442785,6.33794329758925));
#49672=CARTESIAN_POINT('Ctrl Pts',(6.70542150860894,0.928221372961769,6.34638512818421));
#49673=CARTESIAN_POINT('Ctrl Pts',(6.67856841781384,1.1048861080945,6.35482695877917));
#49674=CARTESIAN_POINT('Ctrl Pts',(6.64486161298533,1.27988403547902,6.36326878937413));
#49675=CARTESIAN_POINT('Ctrl Pts',(6.61199655583655,1.45051180377893,6.3714998052285));
#49676=CARTESIAN_POINT('Ctrl Pts',(6.57250706355629,1.62012263742595,6.37973082108288));
#49677=CARTESIAN_POINT('Ctrl Pts',(6.52646616979,1.78816339706041,6.38796183693725));
#49678=CARTESIAN_POINT('Ctrl Pts',(6.48048053554156,1.9560024696598,6.39618297370522));
#49679=CARTESIAN_POINT('Ctrl Pts',(6.42795925162016,2.12227487825813,6.40440411047317));
#49680=CARTESIAN_POINT('Ctrl Pts',(6.36902669903641,2.28643563367993,6.41262524724114));
#49681=CARTESIAN_POINT('Ctrl Pts',(6.31015305450766,2.45043229658609,6.42083816628977));
#49682=CARTESIAN_POINT('Ctrl Pts',(6.24488102496868,2.61232117491342,6.42905108533843));
#49683=CARTESIAN_POINT('Ctrl Pts',(6.17338535119798,2.77157036815129,6.43726400438706));
#49684=CARTESIAN_POINT('Ctrl Pts',(6.10194680368452,2.93069231857991,6.44547036117393));
#49685=CARTESIAN_POINT('Ctrl Pts',(6.0242946634999,3.08717845949579,6.45367671796081));
#49686=CARTESIAN_POINT('Ctrl Pts',(5.94065256135273,3.2405147963392,6.46188307474767));
#49687=CARTESIAN_POINT('Ctrl Pts',(5.85706221792892,3.39375624684144,6.47008435334378));
#49688=CARTESIAN_POINT('Ctrl Pts',(5.76748946947354,3.54385146309567,6.47828563193988));
#49689=CARTESIAN_POINT('Ctrl Pts',(5.67220488218159,3.69030903510199,6.48648691053599));
#49690=CARTESIAN_POINT('Ctrl Pts',(5.57695197524829,3.83671791268103,6.49468546235901));
#49691=CARTESIAN_POINT('Ctrl Pts',(5.47599120643469,3.97949125429586,6.502884014182));
#49692=CARTESIAN_POINT('Ctrl Pts',(5.36963776826787,4.11816454717283,6.51108256600503));
#49693=CARTESIAN_POINT('Ctrl Pts',(5.26330037137964,4.25681692397073,6.51927988124129));
#49694=CARTESIAN_POINT('Ctrl Pts',(5.15157214349014,4.39137019951896,6.52747719647758));
#49695=CARTESIAN_POINT('Ctrl Pts',(5.0348100912214,4.52139097461557,6.53567451171385));
#49696=CARTESIAN_POINT('Ctrl Pts',(4.91804444064793,4.6514157566165,6.54387207957019));
#49697=CARTESIAN_POINT('Ctrl Pts',(4.79624489699761,4.77690749391079,6.55206964742652));
#49698=CARTESIAN_POINT('Ctrl Pts',(4.66980706179267,4.89746781568101,6.56026721528286));
#49699=CARTESIAN_POINT('Ctrl Pts',(4.54329344311045,5.01810039810321,6.56846969654346));
#49700=CARTESIAN_POINT('Ctrl Pts',(4.41213623779877,5.13379541143023,6.57667217780403));
#49701=CARTESIAN_POINT('Ctrl Pts',(4.27676655490759,5.24419267712619,6.58487465906462));
#49702=CARTESIAN_POINT('Ctrl Pts',(4.14135426349279,5.35462469110847,6.59307972211169));
#49703=CARTESIAN_POINT('Ctrl Pts',(4.00172713568375,5.45975541490273,6.6012847851588));
#49704=CARTESIAN_POINT('Ctrl Pts',(3.8583472856512,5.55926660840331,6.60948984820587));
#49705=CARTESIAN_POINT('Ctrl Pts',(3.71482347932203,5.65887771317375,6.61770314930375));
#49706=CARTESIAN_POINT('Ctrl Pts',(3.56753972349512,5.75285781936648,6.62591645040162));
#49707=CARTESIAN_POINT('Ctrl Pts',(3.41698563581462,5.84093298751463,6.6341297514995));
#49708=CARTESIAN_POINT('Ctrl Pts',(3.31253589305714,5.90203679942786,6.63982788431064));
#49709=CARTESIAN_POINT('Ctrl Pts',(3.20651263816237,5.96029942014812,6.64552601712176));
#49710=CARTESIAN_POINT('Ctrl Pts',(3.09908550384729,6.01564277861008,6.6512241499329));
#49711=CARTESIAN_POINT('Origin',(0.,0.,-63.6971797838103));
#49712=CARTESIAN_POINT('',(3.09908550384729,6.01564277861008,9.04575635804621));
#49713=CARTESIAN_POINT('',(3.09908550384719,6.01564277861013,8.6513967904261));
#49714=CARTESIAN_POINT('',(3.09908550384721,6.01564277861012,-63.6971797838103));
#49715=CARTESIAN_POINT('',(-6.76699807574441,0.00297333156401857,7.69717978380994));
#49716=CARTESIAN_POINT('Ctrl Pts',(-6.767,2.65028120476538E-12,7.69717978380994));
#49717=CARTESIAN_POINT('Ctrl Pts',(-6.76700000000007,-0.186007249557489,
7.70592929562269));
#49718=CARTESIAN_POINT('Ctrl Pts',(-6.7593263729426,-0.372014355813802,
7.71467880743544));
#49719=CARTESIAN_POINT('Ctrl Pts',(-6.7440051826338,-0.557389537584311,
7.72342831924819));
#49720=CARTESIAN_POINT('Ctrl Pts',(-6.72868405703751,-0.742763936380853,
7.73217779410539));
#49721=CARTESIAN_POINT('Ctrl Pts',(-6.70571545643589,-0.927506130403236,
7.7409272689626));
#49722=CARTESIAN_POINT('Ctrl Pts',(-6.67517739401602,-1.11098864009382,
7.7496767438198));
#49723=CARTESIAN_POINT('Ctrl Pts',(-6.6446394580442,-1.29447039004384,7.75842618244832));
#49724=CARTESIAN_POINT('Ctrl Pts',(-6.60653217002758,-1.47669218339127,
7.76717562107683));
#49725=CARTESIAN_POINT('Ctrl Pts',(-6.56098496085516,-1.65703510627638,
7.77592505970534));
#49726=CARTESIAN_POINT('Ctrl Pts',(-6.51543793649591,-1.83737729739887,
7.78467446283198));
#49727=CARTESIAN_POINT('Ctrl Pts',(-6.46245112156928,-2.01584035544853,
7.79342386595862));
#49728=CARTESIAN_POINT('Ctrl Pts',(-6.40220448361744,-2.19181813797332,
7.80217326908526));
#49729=CARTESIAN_POINT('Ctrl Pts',(-6.34195808511996,-2.36779522106242,
7.8109226374368));
#49730=CARTESIAN_POINT('Ctrl Pts',(-6.27445201416373,-2.54128677725698,
7.81967200578835));
#49731=CARTESIAN_POINT('Ctrl Pts',(-6.19991555052738,-2.71170355428628,
7.82842137413989));
#49732=CARTESIAN_POINT('Ctrl Pts',(-6.12537937695135,-2.88211966813485,
7.83717070844307));
#49733=CARTESIAN_POINT('Ctrl Pts',(-6.04381298028366,-3.04946076419838,
7.84592004274624));
#49734=CARTESIAN_POINT('Ctrl Pts',(-5.95549339308896,-3.21315848424471,
7.85466937704942));
#49735=CARTESIAN_POINT('Ctrl Pts',(-5.86717414225719,-3.37685558085239,
7.86341867803098));
#49736=CARTESIAN_POINT('Ctrl Pts',(-5.77210188843971,-3.53690907700155,
7.87216797901254));
#49737=CARTESIAN_POINT('Ctrl Pts',(-5.67059953311272,-3.69277537024145,
7.88091727999409));
#49738=CARTESIAN_POINT('Ctrl Pts',(-5.56909755592581,-3.84864108281211,
7.88966654838073));
#49739=CARTESIAN_POINT('Ctrl Pts',(-5.4611656815481,-4.00031938355043,7.89841581676734));
#49740=CARTESIAN_POINT('Ctrl Pts',(-5.3471704848819,-4.14729511918406,7.90716508515398));
#49741=CARTESIAN_POINT('Ctrl Pts',(-5.23317570343097,-4.29427031947433,
7.91591432167234));
#49742=CARTESIAN_POINT('Ctrl Pts',(-5.11311781951318,-4.4365427624982,7.92466355819071));
#49743=CARTESIAN_POINT('Ctrl Pts',(-4.98740458928993,-4.57362924412657,
7.93341279470907));
#49744=CARTESIAN_POINT('Ctrl Pts',(-4.86169180652478,-4.71071523781538,
7.94216200008579));
#49745=CARTESIAN_POINT('Ctrl Pts',(-4.730323911413,-4.84261509584755,7.9509112054625));
#49746=CARTESIAN_POINT('Ctrl Pts',(-4.59374706947045,-4.96888084599859,
7.95966041083922));
#49747=CARTESIAN_POINT('Ctrl Pts',(-4.45717070231241,-5.09514615720975,
7.96840958580092));
#49748=CARTESIAN_POINT('Ctrl Pts',(-4.31538563497112,-5.21577720520789,
7.97715876076261));
#49749=CARTESIAN_POINT('Ctrl Pts',(-4.16887340951809,-5.33036429293656,
7.98590793572431));
#49750=CARTESIAN_POINT('Ctrl Pts',(-4.02236168122281,-5.44495099183856,
7.99465708099757));
#49751=CARTESIAN_POINT('Ctrl Pts',(-3.87112305262972,-5.55349359498074,
8.00340622627082));
#49752=CARTESIAN_POINT('Ctrl Pts',(-3.71567116928781,-5.65562346357352,
8.01215537154407));
#49753=CARTESIAN_POINT('Ctrl Pts',(-3.56021980053088,-5.75775299409066,
8.02090448785544));
#49754=CARTESIAN_POINT('Ctrl Pts',(-3.40055544441852,-5.85346967520014,
8.02965360416682));
#49755=CARTESIAN_POINT('Ctrl Pts',(-3.23722035886602,-5.94244843041514,
8.03840272047819));
#49756=CARTESIAN_POINT('Ctrl Pts',(-3.0738858004326,-6.03142689847568,8.04715180855419));
#49757=CARTESIAN_POINT('Ctrl Pts',(-2.90688078789005,-6.11366734708005,
8.0559008966302));
#49758=CARTESIAN_POINT('Ctrl Pts',(-2.73677250610187,-6.18889047001519,
8.06464998470621));
#49759=CARTESIAN_POINT('Ctrl Pts',(-2.56666475916727,-6.26411335643419,
8.07339904527338));
#49760=CARTESIAN_POINT('Ctrl Pts',(-2.39345402456884,-6.33231884545335,
8.08214810584053));
#49761=CARTESIAN_POINT('Ctrl Pts',(-2.21772855943854,-6.39327529804956,
8.0908971664077));
#49762=CARTESIAN_POINT('Ctrl Pts',(-2.04200363223406,-6.4542315640476,8.09964620019249));
#49763=CARTESIAN_POINT('Ctrl Pts',(-1.86376426060876,-6.50793874412497,
8.10839523397729));
#49764=CARTESIAN_POINT('Ctrl Pts',(-1.68361577621558,-6.55421443943346,
8.11714426776209));
#49765=CARTESIAN_POINT('Ctrl Pts',(-1.50346782833082,-6.60048999692618,
8.12589327549098));
#49766=CARTESIAN_POINT('Ctrl Pts',(-1.32141105657251,-6.63933404265189,
8.13464228321988));
#49767=CARTESIAN_POINT('Ctrl Pts',(-1.13806375346396,-6.67061465631553,
8.14339129094877));
#49768=CARTESIAN_POINT('Ctrl Pts',(-0.954716981167985,-6.70189517941801,
8.15214027334823));
#49769=CARTESIAN_POINT('Ctrl Pts',(-0.77007996743962,-6.72561226609036,
8.1608892557477));
#49770=CARTESIAN_POINT('Ctrl Pts',(-0.584779764069763,-6.74168536996014,
8.16963823814716));
#49771=CARTESIAN_POINT('Ctrl Pts',(-0.39148958758965,-6.75845153117892,
8.17876446856277));
#49772=CARTESIAN_POINT('Ctrl Pts',(-0.197478091801936,-6.76689985146404,
8.1878906989784));
#49773=CARTESIAN_POINT('Ctrl Pts',(-0.00346214752773997,-6.76699911434415,
8.19701692939401));
#49774=CARTESIAN_POINT('Ctrl Pts',(0.184490798487905,-6.76709527525926,
8.20585796510914));
#49775=CARTESIAN_POINT('Ctrl Pts',(0.372447602158016,-6.75935633790745,
8.21469900082425));
#49776=CARTESIAN_POINT('Ctrl Pts',(0.559756448197419,-6.74380914014487,
8.22354003653938));
#49777=CARTESIAN_POINT('Ctrl Pts',(0.745136131046603,-6.72842206873119,
8.23229001515269));
#49778=CARTESIAN_POINT('Ctrl Pts',(0.929880851948329,-6.70538686355678,
8.24103999376599));
#49779=CARTESIAN_POINT('Ctrl Pts',(1.11336305057795,-6.67478177303257,8.2497899723793));
#49780=CARTESIAN_POINT('Ctrl Pts',(1.29684337090462,-6.64417699581195,8.25853986141929));
#49781=CARTESIAN_POINT('Ctrl Pts',(1.47906091205535,-6.60600253547983,8.26728975045928));
#49782=CARTESIAN_POINT('Ctrl Pts',(1.65939671095571,-6.56038806441123,8.27603963949926));
#49783=CARTESIAN_POINT('Ctrl Pts',(1.83973072369515,-6.51477404513749,8.28478944187476));
#49784=CARTESIAN_POINT('Ctrl Pts',(2.01818275357394,-6.46172023288549,8.29353924425025));
#49785=CARTESIAN_POINT('Ctrl Pts',(2.19414664033687,-6.40140683917984,8.30228904662575));
#49786=CARTESIAN_POINT('Ctrl Pts',(2.37010884271615,-6.34109402281364,8.31103876524528));
#49787=CARTESIAN_POINT('Ctrl Pts',(2.54358267848155,-6.2735218569965,8.31978848386482));
#49788=CARTESIAN_POINT('Ctrl Pts',(2.71397890842085,-6.19891986435111,8.32853820248435));
#49789=CARTESIAN_POINT('Ctrl Pts',(2.88437356389273,-6.12431856103087,8.33728784025617));
#49790=CARTESIAN_POINT('Ctrl Pts',(3.05169040787491,-6.04268767582396,8.34603747802799));
#49791=CARTESIAN_POINT('Ctrl Pts',(3.2153611251236,-5.9543044795378,8.35478711579981));
#49792=CARTESIAN_POINT('Ctrl Pts',(3.37903038443137,-5.86592207054873,8.36353667563187));
#49793=CARTESIAN_POINT('Ctrl Pts',(3.53905332980255,-5.77078760703204,8.37228623546392));
#49794=CARTESIAN_POINT('Ctrl Pts',(3.69488643042162,-5.66922422085123,8.38103579529599));
#49795=CARTESIAN_POINT('Ctrl Pts',(3.85071819469011,-5.56766170562973,8.38978528009599));
#49796=CARTESIAN_POINT('Ctrl Pts',(4.00235994599491,-5.45967053456056,8.39853476489598));
#49797=CARTESIAN_POINT('Ctrl Pts',(4.14929662974566,-5.34561750206479,8.40728424969598));
#49798=CARTESIAN_POINT('Ctrl Pts',(4.29623210225307,-5.23156540974251,8.41603366237134));
#49799=CARTESIAN_POINT('Ctrl Pts',(4.43846235842376,-5.11145173171961,8.42478307504672));
#49800=CARTESIAN_POINT('Ctrl Pts',(4.57550431797684,-4.98568443006327,8.43353248772208));
#49801=CARTESIAN_POINT('Ctrl Pts',(4.71254519337745,-4.85991812336446,8.44228183117997));
#49802=CARTESIAN_POINT('Ctrl Pts',(4.84439764315229,-4.72849847630849,8.45103117463786));
#49803=CARTESIAN_POINT('Ctrl Pts',(4.97061384196926,-4.59187184425084,8.45978051809576));
#49804=CARTESIAN_POINT('Ctrl Pts',(5.0968290842045,-4.4552462476747,8.46852979524312));
#49805=CARTESIAN_POINT('Ctrl Pts',(5.21740796650416,-4.31341395556596,8.47727907239049));
#49806=CARTESIAN_POINT('Ctrl Pts',(5.33194095942497,-4.16685668162541,8.48602834953786));
#49807=CARTESIAN_POINT('Ctrl Pts',(5.44647312235371,-4.02030046974891,8.4947775632814));
#49808=CARTESIAN_POINT('Ctrl Pts',(5.55495930712519,-3.86901957035216,8.50352677702493));
#49809=CARTESIAN_POINT('Ctrl Pts',(5.65703106080017,-3.71352778058036,8.51227599076847));
#49810=CARTESIAN_POINT('Ctrl Pts',(5.7591021086894,-3.55803706597272,8.52102514401466));
#49811=CARTESIAN_POINT('Ctrl Pts',(5.85475865698736,-3.39833575880577,8.52977429726085));
#49812=CARTESIAN_POINT('Ctrl Pts',(5.94367583069233,-3.23496624706408,8.53852345050704));
#49813=CARTESIAN_POINT('Ctrl Pts',(6.03259241910241,-3.07159781069779,8.54727254616217));
#49814=CARTESIAN_POINT('Ctrl Pts',(6.11476958471124,-2.90456146975505,8.55602164181729));
#49815=CARTESIAN_POINT('Ctrl Pts',(6.18992823574535,-2.7344245164792,8.56477073747241));
#49816=CARTESIAN_POINT('Ctrl Pts',(6.26508641701077,-2.56428862662069,8.57351977844253));
#49817=CARTESIAN_POINT('Ctrl Pts',(6.33322605570432,-2.3910524253092,8.58226881941264));
#49818=CARTESIAN_POINT('Ctrl Pts',(6.39411573747894,-2.21530425353361,8.59101786038276));
#49819=CARTESIAN_POINT('Ctrl Pts',(6.45500505889243,-2.03955712188191,8.59976684957376));
#49820=CARTESIAN_POINT('Ctrl Pts',(6.50864441545036,-1.86129832025199,8.60851583876477));
#49821=CARTESIAN_POINT('Ctrl Pts',(6.55485164050003,-1.68113324011933,8.61726482795576));
#49822=CARTESIAN_POINT('Ctrl Pts',(6.60199852639196,-1.4973043591252,8.62619173483265));
#49823=CARTESIAN_POINT('Ctrl Pts',(6.64140767441085,-1.31149113173271,8.63511864170954));
#49824=CARTESIAN_POINT('Ctrl Pts',(6.67293975269667,-1.1243505044605,8.64404554858642));
#49825=CARTESIAN_POINT('Ctrl Pts',(6.7038466483156,-0.94092029155993,8.65279546277041));
#49826=CARTESIAN_POINT('Ctrl Pts',(6.72718585889709,-0.756215114274129,
8.6615453769544));
#49827=CARTESIAN_POINT('Ctrl Pts',(6.74287810451896,-0.570862389371339,
8.67029529113839));
#49828=CARTESIAN_POINT('Ctrl Pts',(6.75857004154145,-0.385513309564348,
8.67904503324897));
#49829=CARTESIAN_POINT('Ctrl Pts',(6.76661529035567,-0.199516993255511,
8.68779477535956));
#49830=CARTESIAN_POINT('Ctrl Pts',(6.76698652348897,-0.0135052182014118,
8.69654451747014));
#49831=CARTESIAN_POINT('Ctrl Pts',(6.76735774981515,0.17250314604149,8.70529409914078));
#49832=CARTESIAN_POINT('Ctrl Pts',(6.76005524147466,0.358526681836017,8.71404368081143));
#49833=CARTESIAN_POINT('Ctrl Pts',(6.74510380214861,0.543933542117359,8.72279326248207));
#49834=CARTESIAN_POINT('Ctrl Pts',(6.73015261710952,0.729337249087202,8.731542695344));
#49835=CARTESIAN_POINT('Ctrl Pts',(6.70755278444572,0.914124015857128,8.74029212820592));
#49836=CARTESIAN_POINT('Ctrl Pts',(6.67738106408249,1.0976662174963,8.74904156106784));
#49837=CARTESIAN_POINT('Ctrl Pts',(6.64720981677208,1.28120554143558,8.75779085675019));
#49838=CARTESIAN_POINT('Ctrl Pts',(6.60946696581472,1.46350005650848,8.76654015243254));
#49839=CARTESIAN_POINT('Ctrl Pts',(6.56428070010939,1.64393062206754,8.77528944811489));
#49840=CARTESIAN_POINT('Ctrl Pts',(6.51909508282681,1.82435859844867,8.78403861824488));
#49841=CARTESIAN_POINT('Ctrl Pts',(6.46646633415597,2.00292240086772,8.79278778837485));
#49842=CARTESIAN_POINT('Ctrl Pts',(6.40657319597123,2.17901557696657,8.80153695850484));
#49843=CARTESIAN_POINT('Ctrl Pts',(6.34668083768224,2.35510646007624,8.81028601470791));
#49844=CARTESIAN_POINT('Ctrl Pts',(6.27952437143814,2.52872650996707,8.81903507091099));
#49845=CARTESIAN_POINT('Ctrl Pts',(6.20533187335065,2.69928607998089,8.82778412711406));
#49846=CARTESIAN_POINT('Ctrl Pts',(6.1283144978418,2.87633970115551,8.8368663034029));
#49847=CARTESIAN_POINT('Ctrl Pts',(6.0437148946308,3.05009490562493,8.84594847969175));
#49848=CARTESIAN_POINT('Ctrl Pts',(5.95184265120418,3.21991584599766,8.85503065598058));
#49849=CARTESIAN_POINT('Ctrl Pts',(5.86333281335415,3.38352155905435,8.863780436335));
#49850=CARTESIAN_POINT('Ctrl Pts',(5.76807337235603,3.54347560903958,8.87253021668942));
#49851=CARTESIAN_POINT('Ctrl Pts',(5.66638790086269,3.6992346717878,8.88127999704383));
#49852=CARTESIAN_POINT('Ctrl Pts',(5.56470608502652,3.85498813489894,8.8900294628381));
#49853=CARTESIAN_POINT('Ctrl Pts',(5.45659885766858,4.00654667256389,8.89877892863237));
#49854=CARTESIAN_POINT('Ctrl Pts',(5.3424334058041,4.15339551506336,8.90752839442663));
#49855=CARTESIAN_POINT('Ctrl Pts',(5.22827145140486,4.30023985884002,8.91627759218051));
#49856=CARTESIAN_POINT('Ctrl Pts',(5.10805181977971,4.4423745699318,8.92502678993438));
#49857=CARTESIAN_POINT('Ctrl Pts',(4.98218281282421,4.5793169162659,8.93377598768825));
#49858=CARTESIAN_POINT('Ctrl Pts',(4.85631699296106,4.71625579512287,8.94252496390624));
#49859=CARTESIAN_POINT('Ctrl Pts',(4.72480227791723,4.84800236135881,8.95127394012425));
#49860=CARTESIAN_POINT('Ctrl Pts',(4.58808530848008,4.97410918679006,8.96002291634224));
#49861=CARTESIAN_POINT('Ctrl Pts',(4.4513594505686,5.10022421089105,8.96877246136344));
#49862=CARTESIAN_POINT('Ctrl Pts',(4.30943087207926,5.22069856612081,8.97752200638464));
#49863=CARTESIAN_POINT('Ctrl Pts',(4.16278164322349,5.33512305301776,8.98627155140584));
#49864=CARTESIAN_POINT('Ctrl Pts',(4.01614103534265,5.4495408133152,8.9950205820731));
#49865=CARTESIAN_POINT('Ctrl Pts',(3.8647805583328,5.5579092406843,9.00376961274037));
#49866=CARTESIAN_POINT('Ctrl Pts',(3.70921425811811,5.65986029751383,9.01251864340763));
#49867=CARTESIAN_POINT('Ctrl Pts',(3.55364584529979,5.76181273884741,9.02126779288748));
#49868=CARTESIAN_POINT('Ctrl Pts',(3.39387173464203,5.85734747818145,9.03001694236732));
#49869=CARTESIAN_POINT('Ctrl Pts',(3.23043456092263,5.94614005448885,9.03876609184717));
#49870=CARTESIAN_POINT('Ctrl Pts',(3.186907688063,5.9697874481133,9.04109618058018));
#49871=CARTESIAN_POINT('Ctrl Pts',(3.1431211498284,5.99295688499322,9.04342626931319));
#49872=CARTESIAN_POINT('Ctrl Pts',(3.09908550384729,6.01564277861008,9.04575635804621));
#49873=CARTESIAN_POINT('Ctrl Pts',(3.09908550384722,6.01564277861012,7.04591868117257));
#49874=CARTESIAN_POINT('Ctrl Pts',(2.93604628566889,6.09963587730468,7.05454905880241));
#49875=CARTESIAN_POINT('Ctrl Pts',(2.76950740353687,6.17703973348651,7.06317943643227));
#49876=CARTESIAN_POINT('Ctrl Pts',(2.60001743979206,6.24757539472531,7.07180981406212));
#49877=CARTESIAN_POINT('Ctrl Pts',(2.43064033119356,6.3180640896884,7.08043444514209));
#49878=CARTESIAN_POINT('Ctrl Pts',(2.25831633964846,6.38169359341765,7.08905907622205));
#49879=CARTESIAN_POINT('Ctrl Pts',(2.08361602112917,6.43823215459756,7.09768370730202));
#49880=CARTESIAN_POINT('Ctrl Pts',(1.90904874164956,6.4947276601268,7.10630177049108));
#49881=CARTESIAN_POINT('Ctrl Pts',(1.73210903495208,6.54414290516573,7.11491983368014));
#49882=CARTESIAN_POINT('Ctrl Pts',(1.55338505763979,6.58629515453881,7.12353789686919));
#49883=CARTESIAN_POINT('Ctrl Pts',(1.49727832789166,6.59952798932359,7.1262433611811));
#49884=CARTESIAN_POINT('Ctrl Pts',(1.44099587813452,6.61204540909544,7.12894882549301));
#49885=CARTESIAN_POINT('Ctrl Pts',(1.38455622043201,6.62384277232356,7.13165428980491));
#49886=CARTESIAN_POINT('Ctrl Pts',(1.20878280736886,6.66058400861317,7.14008007967293));
#49887=CARTESIAN_POINT('Ctrl Pts',(1.0315604014241,6.69032138189369,7.14850586954092));
#49888=CARTESIAN_POINT('Ctrl Pts',(0.85347220600288,6.71296314555507,7.15693165940894));
#49889=CARTESIAN_POINT('Ctrl Pts',(0.675342688121898,6.73561016286825,7.16535940434401));
#49890=CARTESIAN_POINT('Ctrl Pts',(0.496347309072643,6.75115824602896,7.17378714927912));
#49891=CARTESIAN_POINT('Ctrl Pts',(0.317074893630531,6.75956747964167,7.18221489421418));
#49892=CARTESIAN_POINT('Ctrl Pts',(0.137736604564098,6.76797980322611,7.19064573592297));
#49893=CARTESIAN_POINT('Ctrl Pts',(-0.0418785928876334,6.76924803137516,
7.19907657763173));
#49894=CARTESIAN_POINT('Ctrl Pts',(-0.22118097478846,6.76338435817392,7.20750741934052));
#49895=CARTESIAN_POINT('Ctrl Pts',(-0.400648112698848,6.75751529700522,
7.21594600791703));
#49896=CARTESIAN_POINT('Ctrl Pts',(-0.579801529226361,6.74450125243955,
7.22438459649354));
#49897=CARTESIAN_POINT('Ctrl Pts',(-0.758054598562708,6.72440645898193,
7.23282318507006));
#49898=CARTESIAN_POINT('Ctrl Pts',(-0.936401135934701,6.70430112870226,
7.24126619846967));
#49899=CARTESIAN_POINT('Ctrl Pts',(-1.1138460564091,6.67710768954954,7.2497092118693));
#49900=CARTESIAN_POINT('Ctrl Pts',(-1.28981146573857,6.64294177174912,7.25815222526892));
#49901=CARTESIAN_POINT('Ctrl Pts',(-1.46596173899787,6.6087399602702,7.2666041086427));
#49902=CARTESIAN_POINT('Ctrl Pts',(-1.64062907266469,6.56755110853779,7.27505599201648));
#49903=CARTESIAN_POINT('Ctrl Pts',(-1.81324825739576,6.51954137628187,7.28350787539027));
#49904=CARTESIAN_POINT('Ctrl Pts',(-1.8602924362528,6.50645720817712,7.28581128050561));
#49905=CARTESIAN_POINT('Ctrl Pts',(-1.90718459024933,6.49286671192376,7.28811468562096));
#49906=CARTESIAN_POINT('Ctrl Pts',(-1.95391351250368,6.47877387980593,7.2904180907363));
#49907=CARTESIAN_POINT('Ctrl Pts',(-2.12264494513047,6.42788668535989,7.29873535606751));
#49908=CARTESIAN_POINT('Ctrl Pts',(-2.28955019583296,6.37035459592245,7.30705262139872));
#49909=CARTESIAN_POINT('Ctrl Pts',(-2.45407839486155,6.30632922006723,7.31536988672994));
#49910=CARTESIAN_POINT('Ctrl Pts',(-2.61846782701356,6.24235784469024,7.3236801370878));
#49911=CARTESIAN_POINT('Ctrl Pts',(-2.78048387941258,6.17190421984677,7.33199038744566));
#49912=CARTESIAN_POINT('Ctrl Pts',(-2.9395911052866,6.09516965586028,7.34030063780352));
#49913=CARTESIAN_POINT('Ctrl Pts',(-3.09859327511113,6.01848575852396,7.34860540103113));
#49914=CARTESIAN_POINT('Ctrl Pts',(-3.25469013329891,5.93552933645976,7.35691016425877));
#49915=CARTESIAN_POINT('Ctrl Pts',(-3.40736627027555,5.84654976034486,7.36521492748638));
#49916=CARTESIAN_POINT('Ctrl Pts',(-3.55996954589234,5.75761264779396,7.37351572744668));
#49917=CARTESIAN_POINT('Ctrl Pts',(-3.70915505374586,5.66265828441473,7.38181652740696));
#49918=CARTESIAN_POINT('Ctrl Pts',(-3.85443185757403,5.56198202579965,7.39011732736726));
#49919=CARTESIAN_POINT('Ctrl Pts',(-3.9996659160247,5.46133538956451,7.39841568494986));
#49920=CARTESIAN_POINT('Ctrl Pts',(-4.14099327733758,5.35497041184807,7.40671404253244));
#49921=CARTESIAN_POINT('Ctrl Pts',(-4.27795169579387,5.24322594291476,7.41501240011503));
#49922=CARTESIAN_POINT('Ctrl Pts',(-4.41492404945482,5.13147010423828,7.42331160203646));
#49923=CARTESIAN_POINT('Ctrl Pts',(-4.54752629780061,5.01433389473508,7.4316108039579));
#49924=CARTESIAN_POINT('Ctrl Pts',(-4.67532857434755,4.89219702402605,7.43991000587933));
#49925=CARTESIAN_POINT('Ctrl Pts',(-4.80314380762242,4.77004777095384,7.44821004918249));
#49926=CARTESIAN_POINT('Ctrl Pts',(-4.92615784717814,4.64289708623193,7.45651009248565));
#49927=CARTESIAN_POINT('Ctrl Pts',(-5.04397713955261,4.51116211365438,7.46481013578881));
#49928=CARTESIAN_POINT('Ctrl Pts',(-5.16182793482981,4.37939191735462,7.47311239838434));
#49929=CARTESIAN_POINT('Ctrl Pts',(-5.27448098258482,4.24303524948044,7.48141466097987));
#49930=CARTESIAN_POINT('Ctrl Pts',(-5.38158240991591,4.10254308512216,7.4897169235754));
#49931=CARTESIAN_POINT('Ctrl Pts',(-5.48873025557395,3.96199003071432,7.4980227844156));
#49932=CARTESIAN_POINT('Ctrl Pts',(-5.59032147462727,3.81729818415243,7.50632864525581));
#49933=CARTESIAN_POINT('Ctrl Pts',(-5.68604487717728,3.66894843991109,7.514634506096));
#49934=CARTESIAN_POINT('Ctrl Pts',(-5.78188143154271,3.52042333580549,7.52295018504972));
#49935=CARTESIAN_POINT('Ctrl Pts',(-5.87183612232255,3.36823198765155,7.53126586400344));
#49936=CARTESIAN_POINT('Ctrl Pts',(-5.95564260041542,3.21288191754958,7.53958154295715));
#49937=CARTESIAN_POINT('Ctrl Pts',(-6.03950208543819,3.05743358976558,7.54790248151157));
#49938=CARTESIAN_POINT('Ctrl Pts',(-6.11720544988682,2.89882286774888,7.55622342006601));
#49939=CARTESIAN_POINT('Ctrl Pts',(-6.18853402279732,2.7375784278592,7.56454435862044));
#49940=CARTESIAN_POINT('Ctrl Pts',(-6.2599686120612,2.57609432878636,7.57287766466697));
#49941=CARTESIAN_POINT('Ctrl Pts',(-6.32500934646575,2.41196901207523,7.58121097071347));
#49942=CARTESIAN_POINT('Ctrl Pts',(-6.38348661080446,2.24574880378019,7.58954427675999));
#49943=CARTESIAN_POINT('Ctrl Pts',(-6.42652933007401,2.12340091621269,7.59567808203977));
#49944=CARTESIAN_POINT('Ctrl Pts',(-6.46601711060719,1.99991839314941,7.60181188731956));
#49945=CARTESIAN_POINT('Ctrl Pts',(-6.50189998196639,1.87552276032725,7.60794569259934));
#49946=CARTESIAN_POINT('Ctrl Pts',(-6.55964575326826,1.67533471818333,7.61781673422672));
#49947=CARTESIAN_POINT('Ctrl Pts',(-6.60820101134001,1.47227423754519,7.62768777585408));
#49948=CARTESIAN_POINT('Ctrl Pts',(-6.64730986736617,1.26710714906689,7.63755881748146));
#49949=CARTESIAN_POINT('Ctrl Pts',(-6.68667936649135,1.06057271336363,7.64749564520288));
#49950=CARTESIAN_POINT('Ctrl Pts',(-6.71647593457217,0.851903446939668,
7.65743247292432));
#49951=CARTESIAN_POINT('Ctrl Pts',(-6.7364861811604,0.641905702603612,7.66736930064573));
#49952=CARTESIAN_POINT('Ctrl Pts',(-6.75649642774862,0.431907958267619,
7.67730612836714));
#49953=CARTESIAN_POINT('Ctrl Pts',(-6.7667201599113,0.22058172300754,7.68724295608853));
#49954=CARTESIAN_POINT('Ctrl Pts',(-6.76699433154345,0.00875881606655957,
7.69717978380994));
#49955=CARTESIAN_POINT('',(-6.767,2.34075020651148E-12,7.30282021618984));
#49956=CARTESIAN_POINT('Ctrl Pts',(3.09908550384729,6.01564277861008,6.6512241499329));
#49957=CARTESIAN_POINT('Ctrl Pts',(2.94401248051215,6.09553192368441,6.65944950834));
#49958=CARTESIAN_POINT('Ctrl Pts',(2.78601358709771,6.1693358723004,6.66767486674707));
#49959=CARTESIAN_POINT('Ctrl Pts',(2.62561376615818,6.23686149845904,6.67590022515418));
#49960=CARTESIAN_POINT('Ctrl Pts',(2.59378762865569,6.25025976692641,6.67753228051521));
#49961=CARTESIAN_POINT('Ctrl Pts',(2.561867014533,6.26341101841259,6.67916433587622));
#49962=CARTESIAN_POINT('Ctrl Pts',(2.52985608944668,6.27631397929466,6.68079639123724));
#49963=CARTESIAN_POINT('Ctrl Pts',(2.3546024939825,6.34695518321549,6.68973157724778));
#49964=CARTESIAN_POINT('Ctrl Pts',(2.17627719690743,6.41029683020603,6.69866676325832));
#49965=CARTESIAN_POINT('Ctrl Pts',(1.99548470311922,6.46609076642272,6.70760194926886));
#49966=CARTESIAN_POINT('Ctrl Pts',(1.81496298050897,6.52180114059812,6.71652375313731));
#49967=CARTESIAN_POINT('Ctrl Pts',(1.6319816804589,6.56998628365692,6.72544555700577));
#49968=CARTESIAN_POINT('Ctrl Pts',(1.44716308657288,6.61044688359727,6.73436736087422));
#49969=CARTESIAN_POINT('Ctrl Pts',(1.26279530875128,6.65080879060827,6.74326740236247));
#49970=CARTESIAN_POINT('Ctrl Pts',(1.07659943348155,6.68348370473627,6.7521674438507));
#49971=CARTESIAN_POINT('Ctrl Pts',(0.889210020969436,6.70832278133719,6.76106748533896));
#49972=CARTESIAN_POINT('Ctrl Pts',(0.702109096946915,6.73312361784976,6.76995382509512));
#49973=CARTESIAN_POINT('Ctrl Pts',(0.513818555767998,6.75011264636526,6.77884016485127));
#49974=CARTESIAN_POINT('Ctrl Pts',(0.324983139942513,6.7591918865167,6.78772650460743));
#49975=CARTESIAN_POINT('Ctrl Pts',(0.136630542694427,6.76824791266564,6.79659012357311));
#49976=CARTESIAN_POINT('Ctrl Pts',(-0.0522638920024719,6.76943449366325,
6.8054537425388));
#49977=CARTESIAN_POINT('Ctrl Pts',(-0.241051065202706,6.76270533026278,
6.81431736150448));
#49978=CARTESIAN_POINT('Ctrl Pts',(-0.420267653187079,6.75631730249491,
6.82273163839255));
#49979=CARTESIAN_POINT('Ctrl Pts',(-0.599387323621606,6.7427961021518,6.8311459152806));
#49980=CARTESIAN_POINT('Ctrl Pts',(-0.777850164000041,6.72214535117808,
6.83956019216866));
#49981=CARTESIAN_POINT('Ctrl Pts',(-0.951985658663627,6.70199533715636,
6.84777044067212));
#49982=CARTESIAN_POINT('Ctrl Pts',(-1.12532831860155,6.67507568806264,6.85598068917558));
#49983=CARTESIAN_POINT('Ctrl Pts',(-1.29732118457894,6.64147925872262,6.86419093767904));
#49984=CARTESIAN_POINT('Ctrl Pts',(-1.46935493677815,6.60787484282423,6.87240313792648));
#49985=CARTESIAN_POINT('Ctrl Pts',(-1.64003790639215,6.56759055274846,6.88061533817391));
#49986=CARTESIAN_POINT('Ctrl Pts',(-1.80882432295702,6.52077016683452,6.88882753842135));
#49987=CARTESIAN_POINT('Ctrl Pts',(-1.97768091962694,6.47393031336111,6.89704315323904));
#49988=CARTESIAN_POINT('Ctrl Pts',(-2.14463904952465,6.42054904494424,6.90525876805674));
#49989=CARTESIAN_POINT('Ctrl Pts',(-2.30916898549506,6.36081972676696,6.91347438287443));
#49990=CARTESIAN_POINT('Ctrl Pts',(-2.47388368145781,6.30102333515224,6.92169922347173));
#49991=CARTESIAN_POINT('Ctrl Pts',(-2.63616440256881,6.23486477719519,6.92992406406903));
#49992=CARTESIAN_POINT('Ctrl Pts',(-2.7955013607369,6.16258558902983,6.93814890466633));
#49993=CARTESIAN_POINT('Ctrl Pts',(-2.95494037981667,6.09026010350871,6.94637901356259));
#49994=CARTESIAN_POINT('Ctrl Pts',(-3.11143155976109,6.01180633160917,6.95460912245886));
#49995=CARTESIAN_POINT('Ctrl Pts',(-3.26449059105997,5.92751129740644,6.96283923135512));
#49996=CARTESIAN_POINT('Ctrl Pts',(-3.41775946867916,5.84310069339644,6.9710806238591));
#49997=CARTESIAN_POINT('Ctrl Pts',(-3.56758649486585,5.75283301417291,6.97932201636308));
#49998=CARTESIAN_POINT('Ctrl Pts',(-3.71351632142453,5.65703858308511,6.98756340886706));
#49999=CARTESIAN_POINT('Ctrl Pts',(-3.77702865424248,5.61534643602491,6.99115027027805));
#50000=CARTESIAN_POINT('Ctrl Pts',(-3.83980319701256,5.57260792544221,6.99473713168906));
#50001=CARTESIAN_POINT('Ctrl Pts',(-3.90180444088853,5.52885260294237,6.99832399310006));
#50002=CARTESIAN_POINT('Ctrl Pts',(-4.04691716796378,5.42644410635298,7.00671897372387));
#50003=CARTESIAN_POINT('Ctrl Pts',(-4.18813387617185,5.31822146221833,7.01511395434766));
#50004=CARTESIAN_POINT('Ctrl Pts',(-4.32497312565706,5.20450732176872,7.02350893497146));
#50005=CARTESIAN_POINT('Ctrl Pts',(-4.46168406247309,5.09089980982621,7.03189604371365));
#50006=CARTESIAN_POINT('Ctrl Pts',(-4.59402546078445,4.97181127976229,7.04028315245586));
#50007=CARTESIAN_POINT('Ctrl Pts',(-4.72154622672205,4.84760664956706,7.04867026119805));
#50008=CARTESIAN_POINT('Ctrl Pts',(-4.84896882731571,4.72349763195816,7.05705091355325));
#50009=CARTESIAN_POINT('Ctrl Pts',(-4.97157794932228,4.59428060019929,7.06543156590843));
#50010=CARTESIAN_POINT('Ctrl Pts',(-5.08895663059961,4.4603597850259,7.07381221826363));
#50011=CARTESIAN_POINT('Ctrl Pts',(-5.20626464185742,4.32651959937159,7.08218782489111));
#50012=CARTESIAN_POINT('Ctrl Pts',(-5.31834826629925,4.18798153057609,7.09056343151859));
#50013=CARTESIAN_POINT('Ctrl Pts',(-5.42482816582768,4.04518582654032,7.09893903814607));
#50014=CARTESIAN_POINT('Ctrl Pts',(-5.53282654890704,3.90035374823408,7.10743408723123));
#50015=CARTESIAN_POINT('Ctrl Pts',(-5.63505990996985,3.75114192589885,7.11592913631642));
#50016=CARTESIAN_POINT('Ctrl Pts',(-5.73117487541204,3.59804440598581,7.12442418540158));
#50017=CARTESIAN_POINT('Ctrl Pts',(-5.82588046173029,3.44719182730019,7.13279466757062));
#50018=CARTESIAN_POINT('Ctrl Pts',(-5.91464568360222,3.29256703035907,7.14116514973963));
#50019=CARTESIAN_POINT('Ctrl Pts',(-5.99717618495803,3.13467172229762,7.14953563190868));
#50020=CARTESIAN_POINT('Ctrl Pts',(-6.07970145403767,2.97678642449714,7.15790558340514));
#50021=CARTESIAN_POINT('Ctrl Pts',(-6.15599263309959,2.81563133004938,7.1662755349016));
#50022=CARTESIAN_POINT('Ctrl Pts',(-6.22580144058283,2.65173253222055,7.17464548639806));
#50023=CARTESIAN_POINT('Ctrl Pts',(-6.29561644392233,2.48781918761132,7.18301618076664));
#50024=CARTESIAN_POINT('Ctrl Pts',(-6.35894779614614,2.32116196708482,7.19138687513521));
#50025=CARTESIAN_POINT('Ctrl Pts',(-6.41559534740355,2.15230698051507,7.19975756950379));
#50026=CARTESIAN_POINT('Ctrl Pts',(-6.47371723375101,1.9790572967995,7.2083461233943));
#50027=CARTESIAN_POINT('Ctrl Pts',(-6.5248025468967,1.80349424587402,7.2169346772848));
#50028=CARTESIAN_POINT('Ctrl Pts',(-6.56868967529199,1.62622413882972,7.2255232311753));
#50029=CARTESIAN_POINT('Ctrl Pts',(-6.61150605251964,1.45327903961906,7.23390224289609));
#50030=CARTESIAN_POINT('Ctrl Pts',(-6.64747135569544,1.27870955593672,7.24228125461689));
#50031=CARTESIAN_POINT('Ctrl Pts',(-6.67648739447263,1.10308887740201,7.25066026633768));
#50032=CARTESIAN_POINT('Ctrl Pts',(-6.70659188208925,0.920880320859626,
7.25935359131304));
#50033=CARTESIAN_POINT('Ctrl Pts',(-6.72921558440873,0.737540577943572,
7.2680469162884));
#50034=CARTESIAN_POINT('Ctrl Pts',(-6.74430784407182,0.553715364055754,
7.27674024126377));
#50035=CARTESIAN_POINT('Ctrl Pts',(-6.7594001037349,0.369890150168001,7.28543356623913));
#50036=CARTESIAN_POINT('Ctrl Pts',(-6.76696093792726,0.185579872223753,
7.2941268912145));
#50037=CARTESIAN_POINT('Ctrl Pts',(-6.76699984893368,0.00142987115423253,
7.30282021618986));
#50038=CARTESIAN_POINT('Ctrl Pts',(-6.767,2.53308028912622E-12,7.30282021618984));
#50039=CARTESIAN_POINT('Ctrl Pts',(-6.76700000000007,-0.186007249557542,
7.31156972800259));
#50040=CARTESIAN_POINT('Ctrl Pts',(-6.7593263729426,-0.372014355813791,
7.32031923981533));
#50041=CARTESIAN_POINT('Ctrl Pts',(-6.74400518263381,-0.557389537584237,
7.32906875162807));
#50042=CARTESIAN_POINT('Ctrl Pts',(-6.72868405703753,-0.742763936380651,
7.33781822648527));
#50043=CARTESIAN_POINT('Ctrl Pts',(-6.70571545643593,-0.927506130402907,
7.34656770134246));
#50044=CARTESIAN_POINT('Ctrl Pts',(-6.6751773940161,-1.11098864009337,7.35531717619966));
#50045=CARTESIAN_POINT('Ctrl Pts',(-6.64463945804429,-1.29447039004339,
7.36406661482818));
#50046=CARTESIAN_POINT('Ctrl Pts',(-6.60653217002768,-1.47669218339082,
7.37281605345669));
#50047=CARTESIAN_POINT('Ctrl Pts',(-6.56098496085528,-1.65703510627594,
7.3815654920852));
#50048=CARTESIAN_POINT('Ctrl Pts',(-6.51543793649603,-1.83737729739843,
7.39031489521184));
#50049=CARTESIAN_POINT('Ctrl Pts',(-6.46245112156941,-2.01584035544809,
7.39906429833849));
#50050=CARTESIAN_POINT('Ctrl Pts',(-6.40220448361758,-2.19181813797288,
7.40781370146513));
#50051=CARTESIAN_POINT('Ctrl Pts',(-6.34195808512014,-2.36779522106193,
7.41656306981667));
#50052=CARTESIAN_POINT('Ctrl Pts',(-6.27445201416395,-2.54128677725644,
7.4253124381682));
#50053=CARTESIAN_POINT('Ctrl Pts',(-6.19991555052764,-2.71170355428568,
7.43406180651974));
#50054=CARTESIAN_POINT('Ctrl Pts',(-6.12537937695157,-2.88211966813438,
7.44281114082292));
#50055=CARTESIAN_POINT('Ctrl Pts',(-6.04381298028384,-3.04946076419803,
7.45156047512609));
#50056=CARTESIAN_POINT('Ctrl Pts',(-5.95549339308909,-3.21315848424447,
7.46030980942928));
#50057=CARTESIAN_POINT('Ctrl Pts',(-5.86717414225738,-3.37685558085204,
7.46905911041083));
#50058=CARTESIAN_POINT('Ctrl Pts',(-5.77210188843998,-3.5369090770011,7.47780841139239));
#50059=CARTESIAN_POINT('Ctrl Pts',(-5.67059953311307,-3.6927753702409,7.48655771237394));
#50060=CARTESIAN_POINT('Ctrl Pts',(-5.56909755592636,-3.84864108281131,
7.49530698076056));
#50061=CARTESIAN_POINT('Ctrl Pts',(-5.46116568154886,-4.00031938354938,
7.50405624914717));
#50062=CARTESIAN_POINT('Ctrl Pts',(-5.34717048488289,-4.14729511918278,
7.51280551753379));
#50063=CARTESIAN_POINT('Ctrl Pts',(-5.23317570343208,-4.29427031947298,
7.52155475405215));
#50064=CARTESIAN_POINT('Ctrl Pts',(-5.11311781951441,-4.43654276249679,
7.5303039905705));
#50065=CARTESIAN_POINT('Ctrl Pts',(-4.98740458929128,-4.5736292441251,7.53905322708886));
#50066=CARTESIAN_POINT('Ctrl Pts',(-4.861691806526,-4.71071523781413,7.54780243246559));
#50067=CARTESIAN_POINT('Ctrl Pts',(-4.73032391141408,-4.84261509584652,
7.55655163784232));
#50068=CARTESIAN_POINT('Ctrl Pts',(-4.59374706947136,-4.96888084599775,
7.56530084321905));
#50069=CARTESIAN_POINT('Ctrl Pts',(-4.45717070231348,-5.09514615720881,
7.57405001818074));
#50070=CARTESIAN_POINT('Ctrl Pts',(-4.31538563497237,-5.21577720520685,
7.58279919314242));
#50071=CARTESIAN_POINT('Ctrl Pts',(-4.16887340951951,-5.33036429293545,
7.59154836810411));
#50072=CARTESIAN_POINT('Ctrl Pts',(-4.02236168122442,-5.44495099183737,
7.60029751337736));
#50073=CARTESIAN_POINT('Ctrl Pts',(-3.87112305263152,-5.55349359497948,
7.6090466586506));
#50074=CARTESIAN_POINT('Ctrl Pts',(-3.71567116928981,-5.65562346357221,
7.61779580392384));
#50075=CARTESIAN_POINT('Ctrl Pts',(-3.56021980053318,-5.75775299408923,
7.6265449202352));
#50076=CARTESIAN_POINT('Ctrl Pts',(-3.40055544442113,-5.85346967519861,
7.63529403654655));
#50077=CARTESIAN_POINT('Ctrl Pts',(-3.23722035886896,-5.94244843041354,
7.6440431528579));
#50078=CARTESIAN_POINT('Ctrl Pts',(-3.07388580043524,-6.03142689847434,
7.65279224093393));
#50079=CARTESIAN_POINT('Ctrl Pts',(-2.90688078789238,-6.11366734707895,
7.66154132900996));
#50080=CARTESIAN_POINT('Ctrl Pts',(-2.73677250610388,-6.18889047001431,
7.67029041708598));
#50081=CARTESIAN_POINT('Ctrl Pts',(-2.5666647591693,-6.26411335643336,7.67903947765315));
#50082=CARTESIAN_POINT('Ctrl Pts',(-2.39345402457089,-6.33231884545257,
7.68778853822033));
#50083=CARTESIAN_POINT('Ctrl Pts',(-2.21772855944062,-6.39327529804884,
7.6965375987875));
#50084=CARTESIAN_POINT('Ctrl Pts',(-2.04200363223591,-6.45423156404703,
7.7052866325723));
#50085=CARTESIAN_POINT('Ctrl Pts',(-1.86376426061038,-6.50793874412452,
7.7140356663571));
#50086=CARTESIAN_POINT('Ctrl Pts',(-1.68361577621695,-6.5542144394331,7.7227847001419));
#50087=CARTESIAN_POINT('Ctrl Pts',(-1.50346782833202,-6.60048999692591,
7.73153370787081));
#50088=CARTESIAN_POINT('Ctrl Pts',(-1.32141105657353,-6.63933404265169,
7.74028271559971));
#50089=CARTESIAN_POINT('Ctrl Pts',(-1.1380637534648,-6.67061465631539,7.74903172332861));
#50090=CARTESIAN_POINT('Ctrl Pts',(-0.954716981169521,-6.70189517941778,
7.75778070572804));
#50091=CARTESIAN_POINT('Ctrl Pts',(-0.770079967441858,-6.72561226609009,
7.76652968812747));
#50092=CARTESIAN_POINT('Ctrl Pts',(-0.58477976407271,-6.74168536995988,
7.7752786705269));
#50093=CARTESIAN_POINT('Ctrl Pts',(-0.391489587592541,-6.75845153117875,
7.78440490094252));
#50094=CARTESIAN_POINT('Ctrl Pts',(-0.197478091804768,-6.76689985146396,
7.79353113135814));
#50095=CARTESIAN_POINT('Ctrl Pts',(-0.00346214753050771,-6.76699911434415,
7.80265736177375));
#50096=CARTESIAN_POINT('Ctrl Pts',(0.184490798485202,-6.76709527525933,
7.81149839748888));
#50097=CARTESIAN_POINT('Ctrl Pts',(0.372447602155378,-6.7593563379076,7.82033943320402));
#50098=CARTESIAN_POINT('Ctrl Pts',(0.559756448194851,-6.74380914014508,
7.82918046891915));
#50099=CARTESIAN_POINT('Ctrl Pts',(0.745136131043977,-6.72842206873148,
7.83793044753245));
#50100=CARTESIAN_POINT('Ctrl Pts',(0.92988085194565,-6.70538686355715,7.84668042614576));
#50101=CARTESIAN_POINT('Ctrl Pts',(1.11336305057522,-6.67478177303302,7.85543040475906));
#50102=CARTESIAN_POINT('Ctrl Pts',(1.2968433709019,-6.64417699581248,7.86418029379905));
#50103=CARTESIAN_POINT('Ctrl Pts',(1.47906091205264,-6.60600253548043,7.87293018283903));
#50104=CARTESIAN_POINT('Ctrl Pts',(1.65939671095303,-6.56038806441191,7.88168007187902));
#50105=CARTESIAN_POINT('Ctrl Pts',(1.83973072369242,-6.51477404513826,7.89042987425451));
#50106=CARTESIAN_POINT('Ctrl Pts',(2.01818275357117,-6.46172023288635,7.89917967663001));
#50107=CARTESIAN_POINT('Ctrl Pts',(2.19414664033407,-6.4014068391808,7.9079294790055));
#50108=CARTESIAN_POINT('Ctrl Pts',(2.37010884271337,-6.34109402281468,7.91667919762504));
#50109=CARTESIAN_POINT('Ctrl Pts',(2.54358267847881,-6.27352185699761,7.92542891624456));
#50110=CARTESIAN_POINT('Ctrl Pts',(2.71397890841814,-6.1989198643523,7.9341786348641));
#50111=CARTESIAN_POINT('Ctrl Pts',(2.88437356389017,-6.12431856103208,7.94292827263592));
#50112=CARTESIAN_POINT('Ctrl Pts',(3.0516904078725,-6.04268767582518,7.95167791040775));
#50113=CARTESIAN_POINT('Ctrl Pts',(3.21536112512134,-5.95430447953902,7.96042754817957));
#50114=CARTESIAN_POINT('Ctrl Pts',(3.37903038442914,-5.86592207055001,7.96917710801163));
#50115=CARTESIAN_POINT('Ctrl Pts',(3.53905332980035,-5.77078760703338,7.9779266678437));
#50116=CARTESIAN_POINT('Ctrl Pts',(3.69488643041946,-5.66922422085263,7.98667622767576));
#50117=CARTESIAN_POINT('Ctrl Pts',(3.85071819468793,-5.56766170563123,7.99542571247575));
#50118=CARTESIAN_POINT('Ctrl Pts',(4.00235994599273,-5.45967053456216,8.00417519727574));
#50119=CARTESIAN_POINT('Ctrl Pts',(4.14929662974347,-5.34561750206648,8.01292468207573));
#50120=CARTESIAN_POINT('Ctrl Pts',(4.29623210225092,-5.23156540974426,8.02167409475109));
#50121=CARTESIAN_POINT('Ctrl Pts',(4.43846235842167,-5.11145173172143,8.03042350742646));
#50122=CARTESIAN_POINT('Ctrl Pts',(4.5755043179748,-4.98568443006514,8.03917292010182));
#50123=CARTESIAN_POINT('Ctrl Pts',(4.71254519337551,-4.85991812336635,8.04792226355972));
#50124=CARTESIAN_POINT('Ctrl Pts',(4.84439764315045,-4.72849847631039,8.05667160701763));
#50125=CARTESIAN_POINT('Ctrl Pts',(4.97061384196751,-4.59187184425273,8.06542095047553));
#50126=CARTESIAN_POINT('Ctrl Pts',(5.09682908420275,-4.45524624767669,8.0741702276229));
#50127=CARTESIAN_POINT('Ctrl Pts',(5.21740796650244,-4.31341395556805,8.08291950477024));
#50128=CARTESIAN_POINT('Ctrl Pts',(5.33194095942327,-4.1668566816276,8.0916687819176));
#50129=CARTESIAN_POINT('Ctrl Pts',(5.44647312235203,-4.0203004697512,8.10041799566114));
#50130=CARTESIAN_POINT('Ctrl Pts',(5.55495930712353,-3.86901957035454,8.10916720940468));
#50131=CARTESIAN_POINT('Ctrl Pts',(5.65703106079855,-3.71352778058284,8.11791642314822));
#50132=CARTESIAN_POINT('Ctrl Pts',(5.75910210868784,-3.55803706597524,8.12666557639441));
#50133=CARTESIAN_POINT('Ctrl Pts',(5.85475865698587,-3.39833575880834,8.1354147296406));
#50134=CARTESIAN_POINT('Ctrl Pts',(5.94367583069091,-3.23496624706669,8.14416388288679));
#50135=CARTESIAN_POINT('Ctrl Pts',(6.03259241910106,-3.07159781070043,8.15291297854191));
#50136=CARTESIAN_POINT('Ctrl Pts',(6.11476958470997,-2.90456146975773,8.16166207419705));
#50137=CARTESIAN_POINT('Ctrl Pts',(6.18992823574415,-2.73442451648191,8.17041116985217));
#50138=CARTESIAN_POINT('Ctrl Pts',(6.2650864170096,-2.56428862662355,8.17916021082229));
#50139=CARTESIAN_POINT('Ctrl Pts',(6.33322605570318,-2.39105242531221,8.18790925179239));
#50140=CARTESIAN_POINT('Ctrl Pts',(6.39411573747785,-2.21530425353678,8.19665829276251));
#50141=CARTESIAN_POINT('Ctrl Pts',(6.4550050588915,-2.03955712188486,8.20540728195352));
#50142=CARTESIAN_POINT('Ctrl Pts',(6.50864441544959,-1.86129832025472,8.21415627114451));
#50143=CARTESIAN_POINT('Ctrl Pts',(6.55485164049939,-1.68113324012183,8.22290526033552));
#50144=CARTESIAN_POINT('Ctrl Pts',(6.6019985263914,-1.49730435912765,8.23183216721241));
#50145=CARTESIAN_POINT('Ctrl Pts',(6.64140767441038,-1.31149113173512,8.2407590740893));
#50146=CARTESIAN_POINT('Ctrl Pts',(6.67293975269627,-1.12435050446285,8.24968598096619));
#50147=CARTESIAN_POINT('Ctrl Pts',(6.70384664831528,-0.94092029156223,8.25843589515019));
#50148=CARTESIAN_POINT('Ctrl Pts',(6.72718585889684,-0.756215114276376,
8.26718580933418));
#50149=CARTESIAN_POINT('Ctrl Pts',(6.74287810451878,-0.570862389373527,
8.27593572351817));
#50150=CARTESIAN_POINT('Ctrl Pts',(6.75857004154132,-0.385513309566605,
8.28468546562875));
#50151=CARTESIAN_POINT('Ctrl Pts',(6.7666152903556,-0.199516993257833,8.29343520773934));
#50152=CARTESIAN_POINT('Ctrl Pts',(6.76698652348897,-0.0135052182037979,
8.30218494984992));
#50153=CARTESIAN_POINT('Ctrl Pts',(6.76735774981521,0.172503146039168,8.31093453152056));
#50154=CARTESIAN_POINT('Ctrl Pts',(6.76005524147478,0.358526681833763,8.3196841131912));
#50155=CARTESIAN_POINT('Ctrl Pts',(6.74510380214879,0.543933542115173,8.32843369486184));
#50156=CARTESIAN_POINT('Ctrl Pts',(6.73015261710976,0.729337249085021,8.33718312772377));
#50157=CARTESIAN_POINT('Ctrl Pts',(6.70755278444601,0.914124015854953,8.3459325605857));
#50158=CARTESIAN_POINT('Ctrl Pts',(6.67738106408284,1.09766621749414,8.35468199344763));
#50159=CARTESIAN_POINT('Ctrl Pts',(6.64720981677249,1.28120554143349,8.36343128912998));
#50160=CARTESIAN_POINT('Ctrl Pts',(6.60946696581517,1.46350005650646,8.37218058481233));
#50161=CARTESIAN_POINT('Ctrl Pts',(6.56428070010988,1.6439306220656,8.38092988049468));
#50162=CARTESIAN_POINT('Ctrl Pts',(6.51909508282735,1.82435859844674,8.38967905062466));
#50163=CARTESIAN_POINT('Ctrl Pts',(6.46646633415656,2.00292240086581,8.39842822075465));
#50164=CARTESIAN_POINT('Ctrl Pts',(6.40657319597188,2.17901557696468,8.40717739088464));
#50165=CARTESIAN_POINT('Ctrl Pts',(6.34668083768289,2.35510646007448,8.41592644708772));
#50166=CARTESIAN_POINT('Ctrl Pts',(6.27952437143879,2.52872650996545,8.42467550329079));
#50167=CARTESIAN_POINT('Ctrl Pts',(6.20533187335129,2.6992860799794,8.43342455949387));
#50168=CARTESIAN_POINT('Ctrl Pts',(6.12831449784246,2.8763397011541,8.44250673578271));
#50169=CARTESIAN_POINT('Ctrl Pts',(6.04371489463147,3.0500949056236,8.45158891207156));
#50170=CARTESIAN_POINT('Ctrl Pts',(5.95184265120486,3.21991584599641,8.4606710883604));
#50171=CARTESIAN_POINT('Ctrl Pts',(5.86333281335483,3.38352155905317,8.46942086871482));
#50172=CARTESIAN_POINT('Ctrl Pts',(5.76807337235671,3.54347560903848,8.47817064906924));
#50173=CARTESIAN_POINT('Ctrl Pts',(5.66638790086336,3.69923467178677,8.48692042942366));
#50174=CARTESIAN_POINT('Ctrl Pts',(5.56470608502723,3.85498813489793,8.49566989521793));
#50175=CARTESIAN_POINT('Ctrl Pts',(5.45659885766931,4.0065466725629,8.5044193610122));
#50176=CARTESIAN_POINT('Ctrl Pts',(5.34243340580486,4.15339551506239,8.51316882680646));
#50177=CARTESIAN_POINT('Ctrl Pts',(5.22827145140568,4.30023985883902,8.52191802456033));
#50178=CARTESIAN_POINT('Ctrl Pts',(5.1080518197806,4.44237456993077,8.53066722231419));
#50179=CARTESIAN_POINT('Ctrl Pts',(4.98218281282518,4.57931691626485,8.53941642006806));
#50180=CARTESIAN_POINT('Ctrl Pts',(4.85631699296184,4.71625579512209,8.54816539628607));
#50181=CARTESIAN_POINT('Ctrl Pts',(4.7248022779178,4.84800236135827,8.55691437250409));
#50182=CARTESIAN_POINT('Ctrl Pts',(4.58808530848042,4.97410918678974,8.5656633487221));
#50183=CARTESIAN_POINT('Ctrl Pts',(4.45135945056895,5.10022421089074,8.5744128937433));
#50184=CARTESIAN_POINT('Ctrl Pts',(4.30943087207962,5.22069856612051,8.58316243876449));
#50185=CARTESIAN_POINT('Ctrl Pts',(4.16278164322386,5.33512305301747,8.59191198378569));
#50186=CARTESIAN_POINT('Ctrl Pts',(4.01614103534297,5.44954081331496,8.60066101445296));
#50187=CARTESIAN_POINT('Ctrl Pts',(3.86478055833308,5.55790924068411,8.60941004512022));
#50188=CARTESIAN_POINT('Ctrl Pts',(3.70921425811833,5.65986029751368,8.61815907578749));
#50189=CARTESIAN_POINT('Ctrl Pts',(3.55364584530002,5.76181273884727,8.62690822526733));
#50190=CARTESIAN_POINT('Ctrl Pts',(3.39387173464226,5.85734747818132,8.63565737474718));
#50191=CARTESIAN_POINT('Ctrl Pts',(3.23043456092287,5.94614005448872,8.64440652422702));
#50192=CARTESIAN_POINT('Ctrl Pts',(3.18690768806312,5.96978744811324,8.64673661296004));
#50193=CARTESIAN_POINT('Ctrl Pts',(3.14312114982841,5.99295688499321,8.64906670169307));
#50194=CARTESIAN_POINT('Ctrl Pts',(3.09908550384719,6.01564277861013,8.65139679042609));
#50195=CARTESIAN_POINT('Origin',(0.,0.,-63.6971797838103));
#50196=CARTESIAN_POINT('',(3.09908550384726,6.0156427786101,11.0457658645337));
#50197=CARTESIAN_POINT('',(3.09908550384714,6.01564277861016,10.6513967904261));
#50198=CARTESIAN_POINT('',(3.09908550384721,6.01564277861012,-63.6971797838103));
#50199=CARTESIAN_POINT('',(-6.76842911963828,-0.00288457139099718,9.69470657721669));
#50200=CARTESIAN_POINT('Ctrl Pts',(-6.76699802906409,-0.00516475002166228,
9.69717978380996));
#50201=CARTESIAN_POINT('Ctrl Pts',(-6.76684617121268,-0.204133098312014,
9.70651087210626));
#50202=CARTESIAN_POINT('Ctrl Pts',(-6.75791508724367,-0.402765009104481,
9.71584196040255));
#50203=CARTESIAN_POINT('Ctrl Pts',(-6.74031724594989,-0.60034358824799,
9.72517304869886));
#50204=CARTESIAN_POINT('Ctrl Pts',(-6.72258670926816,-0.799411995932042,
9.73457449746501));
#50205=CARTESIAN_POINT('Ctrl Pts',(-6.69605829151014,-0.997410976137869,
9.74397594623116));
#50206=CARTESIAN_POINT('Ctrl Pts',(-6.66089694743609,-1.19362509006664,
9.7533773949973));
#50207=CARTESIAN_POINT('Ctrl Pts',(-6.62561182536618,-1.39052993384153,
9.76281193955421));
#50208=CARTESIAN_POINT('Ctrl Pts',(-6.58163298569832,-1.58563718982377,
9.7722464841111));
#50209=CARTESIAN_POINT('Ctrl Pts',(-6.52917590122111,-1.77824381087451,
9.781681028668));
#50210=CARTESIAN_POINT('Ctrl Pts',(-6.47649039451653,-1.97168912957352,
9.79115665556304));
#50211=CARTESIAN_POINT('Ctrl Pts',(-6.41525272681293,-2.16261185559198,
9.80063228245812));
#50212=CARTESIAN_POINT('Ctrl Pts',(-6.34572897970457,-2.35032183245989,
9.81010790935316));
#50213=CARTESIAN_POINT('Ctrl Pts',(-6.29551623179225,-2.48589326152001,
9.81695157478234));
#50214=CARTESIAN_POINT('Ctrl Pts',(-6.24098222467483,-2.61978928377327,
9.82379524021147));
#50215=CARTESIAN_POINT('Ctrl Pts',(-6.18224224289037,-2.75175759292526,
9.83063890564064));
#50216=CARTESIAN_POINT('Ctrl Pts',(-6.11296435785666,-2.90740090556831,
9.83871031888266));
#50217=CARTESIAN_POINT('Ctrl Pts',(-6.03767742973509,-3.06071262367723,
9.8467817321247));
#50218=CARTESIAN_POINT('Ctrl Pts',(-5.95655887786007,-3.21118285598724,
9.85485314536672));
#50219=CARTESIAN_POINT('Ctrl Pts',(-5.8755421636081,-3.36146418538362,9.86291442561795));
#50220=CARTESIAN_POINT('Ctrl Pts',(-5.78870856749346,-3.50891080276374,
9.87097570586917));
#50221=CARTESIAN_POINT('Ctrl Pts',(-5.69628417944841,-3.65303100821301,
9.8790369861204));
#50222=CARTESIAN_POINT('Ctrl Pts',(-5.60395555347136,-3.7970018889093,9.88708991397802));
#50223=CARTESIAN_POINT('Ctrl Pts',(-5.50604786281596,-3.93765290509485,
9.89514284183564));
#50224=CARTESIAN_POINT('Ctrl Pts',(-5.40283384014468,-4.07451536943813,
9.90319576969327));
#50225=CARTESIAN_POINT('Ctrl Pts',(-5.29970415731547,-4.21126599860311,
9.91124211721766));
#50226=CARTESIAN_POINT('Ctrl Pts',(-5.19127699599953,-4.34423394128255,
9.91928846474205));
#50227=CARTESIAN_POINT('Ctrl Pts',(-5.07786921845359,-4.47297811310111,
9.92733481226644));
#50228=CARTESIAN_POINT('Ctrl Pts',(-4.96452930266831,-4.60164524605723,
9.93537634495959));
#50229=CARTESIAN_POINT('Ctrl Pts',(-4.84621494955229,-4.7260933604144,9.94341787765274));
#50230=CARTESIAN_POINT('Ctrl Pts',(-4.72328417905465,-4.84591328480938,
9.95145941034589));
#50231=CARTESIAN_POINT('Ctrl Pts',(-4.5979900967641,-4.96803671579757,9.95965553939413));
#50232=CARTESIAN_POINT('Ctrl Pts',(-4.46790053134225,-5.08535187909609,
9.96785166844238));
#50233=CARTESIAN_POINT('Ctrl Pts',(-4.33343537934581,-5.19746349799919,
9.97604779749062));
#50234=CARTESIAN_POINT('Ctrl Pts',(-4.20155206547098,-5.3074224844376,9.98408655432672));
#50235=CARTESIAN_POINT('Ctrl Pts',(-4.06545998304518,-5.41237570910219,
9.9921253111628));
#50236=CARTESIAN_POINT('Ctrl Pts',(-3.92558976240521,-5.5119900233309,10.0001640679989));
#50237=CARTESIAN_POINT('Ctrl Pts',(-3.78570600380607,-5.61161397917248,
10.0082036029017));
#50238=CARTESIAN_POINT('Ctrl Pts',(-3.64204368301207,-5.70589777888392,
10.0162431378045));
#50239=CARTESIAN_POINT('Ctrl Pts',(-3.49506324561321,-5.79455105328822,
10.0242826727073));
#50240=CARTESIAN_POINT('Ctrl Pts',(-3.34803947988359,-5.88323046177176,
10.0323245775828));
#50241=CARTESIAN_POINT('Ctrl Pts',(-3.19769597020124,-5.96627584832997,
10.0403664824583));
#50242=CARTESIAN_POINT('Ctrl Pts',(-3.04451849647632,-6.04344240682523,
10.0484083873339));
#50243=CARTESIAN_POINT('Ctrl Pts',(-2.88617399696951,-6.12321196945387,
10.0567215640147));
#50244=CARTESIAN_POINT('Ctrl Pts',(-2.72480138680157,-6.19669895739926,
10.0650347406955));
#50245=CARTESIAN_POINT('Ctrl Pts',(-2.56095950535423,-6.26368704613631,
10.0733479173763));
#50246=CARTESIAN_POINT('Ctrl Pts',(-2.40218885044364,-6.32860172256725,
10.0814037849868));
#50247=CARTESIAN_POINT('Ctrl Pts',(-2.24109987559649,-6.38741375553719,
10.0894596525974));
#50248=CARTESIAN_POINT('Ctrl Pts',(-2.07821584240643,-6.43997732234912,
10.0975155202079));
#50249=CARTESIAN_POINT('Ctrl Pts',(-1.90752789388964,-6.4950592552442,10.1059573514238));
#50250=CARTESIAN_POINT('Ctrl Pts',(-1.73486911782119,-6.54327912242878,
10.1143991826398));
#50251=CARTESIAN_POINT('Ctrl Pts',(-1.56085207914365,-6.58452957978267,
10.1228410138558));
#50252=CARTESIAN_POINT('Ctrl Pts',(-1.38683504046617,-6.62578003713655,
10.1312828450717));
#50253=CARTESIAN_POINT('Ctrl Pts',(-1.21146020813647,-6.66006108019321,
10.1397246762877));
#50254=CARTESIAN_POINT('Ctrl Pts',(-1.0353438881606,-6.68732771989294,10.1481665075036));
#50255=CARTESIAN_POINT('Ctrl Pts',(-0.863637347590903,-6.71391162975685,
10.1563969635702));
#50256=CARTESIAN_POINT('Ctrl Pts',(-0.690654969195276,-6.73391699050144,
10.1646274196367));
#50257=CARTESIAN_POINT('Ctrl Pts',(-0.516942018526933,-6.74722609295711,
10.1728578757033));
#50258=CARTESIAN_POINT('Ctrl Pts',(-0.343435275367393,-6.76051939672391,
10.1810785617335));
#50259=CARTESIAN_POINT('Ctrl Pts',(-0.169200040751129,-6.76713224302291,
10.1892992477637));
#50260=CARTESIAN_POINT('Ctrl Pts',(0.00520876157270132,-6.7669979953302,
10.1975199337939));
#50261=CARTESIAN_POINT('Ctrl Pts',(0.179445522171758,-6.76686388006316,
10.2057325107093));
#50262=CARTESIAN_POINT('Ctrl Pts',(0.3538551534552,-6.75999592547768,10.2139450876247));
#50263=CARTESIAN_POINT('Ctrl Pts',(0.527878053718226,-6.74637930748062,
10.2221576645401));
#50264=CARTESIAN_POINT('Ctrl Pts',(0.701764194754424,-6.73277339036342,
10.2303637874447));
#50265=CARTESIAN_POINT('Ctrl Pts',(0.875263854289261,-6.71242940120123,
10.2385699103494));
#50266=CARTESIAN_POINT('Ctrl Pts',(1.04781778217753,-6.68538457348211,10.246776033254));
#50267=CARTESIAN_POINT('Ctrl Pts',(1.22027070358692,-6.65835557677219,10.2549773526078));
#50268=CARTESIAN_POINT('Ctrl Pts',(1.39177864292623,-6.62463361077684,10.2631786719614));
#50269=CARTESIAN_POINT('Ctrl Pts',(1.56178773107372,-6.58430771479186,10.2713799913152));
#50270=CARTESIAN_POINT('Ctrl Pts',(1.73174804764207,-6.54399338735095,10.2795789579047));
#50271=CARTESIAN_POINT('Ctrl Pts',(1.9002100201813,-6.49707898234912,10.2877779244942));
#50272=CARTESIAN_POINT('Ctrl Pts',(2.06662998149656,-6.44370464248475,10.2959768910837));
#50273=CARTESIAN_POINT('Ctrl Pts',(2.23302796630399,-6.39033735094312,10.3041747749627));
#50274=CARTESIAN_POINT('Ctrl Pts',(2.3973841353217,-6.33051193223582,10.3123726588416));
#50275=CARTESIAN_POINT('Ctrl Pts',(2.55916998855588,-6.26441840633868,10.3205705427205));
#50276=CARTESIAN_POINT('Ctrl Pts',(2.72096386610309,-6.19832160231104,10.3287688332011));
#50277=CARTESIAN_POINT('Ctrl Pts',(2.88018684186813,-6.12595620732234,10.3369671236816));
#50278=CARTESIAN_POINT('Ctrl Pts',(3.03633035802638,-6.04756041366495,10.3451654141622));
#50279=CARTESIAN_POINT('Ctrl Pts',(3.19250998248926,-5.96914649092178,10.3533656005035));
#50280=CARTESIAN_POINT('Ctrl Pts',(3.34560840857727,-5.88469955288408,10.3615657868448));
#50281=CARTESIAN_POINT('Ctrl Pts',(3.49514160158241,-5.7945037910841,10.3697659731861));
#50282=CARTESIAN_POINT('Ctrl Pts',(3.64481616648852,-5.70422275626848,10.3779739121602));
#50283=CARTESIAN_POINT('Ctrl Pts',(3.79091845666016,-5.60818222450421,10.3861818511343));
#50284=CARTESIAN_POINT('Ctrl Pts',(3.93299258232579,-5.50671030174735,10.3943897901084));
#50285=CARTESIAN_POINT('Ctrl Pts',(4.07513563245421,-5.40518915188645,10.4026017110024));
#50286=CARTESIAN_POINT('Ctrl Pts',(4.21324633853173,-5.29823157703008,10.4108136318963));
#50287=CARTESIAN_POINT('Ctrl Pts',(4.34690194006119,-5.18620598544758,10.4190255527903));
#50288=CARTESIAN_POINT('Ctrl Pts',(4.48074082907466,-5.07402676851312,10.4272487350328));
#50289=CARTESIAN_POINT('Ctrl Pts',(4.61011213816752,-4.95676588637834,10.4354719172754));
#50290=CARTESIAN_POINT('Ctrl Pts',(4.7346291461588,-4.83482945390461,10.443695099518));
#50291=CARTESIAN_POINT('Ctrl Pts',(4.84566689303691,-4.72609292913055,10.4510281028009));
#50292=CARTESIAN_POINT('Ctrl Pts',(4.95284484943451,-4.61363897515007,10.4583611060838));
#50293=CARTESIAN_POINT('Ctrl Pts',(5.05591632381215,-4.49777713171849,10.4656941093667));
#50294=CARTESIAN_POINT('Ctrl Pts',(5.1815078229504,-4.35660070344525,10.474629296149));
#50295=CARTESIAN_POINT('Ctrl Pts',(5.30126275186575,-4.21007139260991,10.4835644829313));
#50296=CARTESIAN_POINT('Ctrl Pts',(5.4147436786938,-4.05867464747367,10.4924996697136));
#50297=CARTESIAN_POINT('Ctrl Pts',(5.52805464619939,-3.90750464782625,10.5014214743502));
#50298=CARTESIAN_POINT('Ctrl Pts',(5.63511020633228,-3.75148196600656,10.5103432789868));
#50299=CARTESIAN_POINT('Ctrl Pts',(5.73551291545298,-3.59112525494058,10.5192650836234));
#50300=CARTESIAN_POINT('Ctrl Pts',(5.83567071855538,-3.43115969192189,10.5281651258627));
#50301=CARTESIAN_POINT('Ctrl Pts',(5.92920792189058,-3.26688141757251,10.537065168102));
#50302=CARTESIAN_POINT('Ctrl Pts',(6.01577045540629,-3.09883765755175,10.5459652103413));
#50303=CARTESIAN_POINT('Ctrl Pts',(6.10219972462893,-2.93105260337027,10.5548515508347));
#50304=CARTESIAN_POINT('Ctrl Pts',(6.18167562506326,-2.75951385558025,10.5637378913281));
#50305=CARTESIAN_POINT('Ctrl Pts',(6.25388854000848,-2.5847953747155,10.5726242318215));
#50306=CARTESIAN_POINT('Ctrl Pts',(6.32591681913538,-2.41052361850816,10.5814878514934));
#50307=CARTESIAN_POINT('Ctrl Pts',(6.39071907004853,-2.2330885902073,10.5903514711654));
#50308=CARTESIAN_POINT('Ctrl Pts',(6.4480328625905,-2.05308577583914,10.5992150908373));
#50309=CARTESIAN_POINT('Ctrl Pts',(6.50244109802557,-1.88220831216498,10.6076293639909));
#50310=CARTESIAN_POINT('Ctrl Pts',(6.55010112360273,-1.70901716807654,10.6160436371445));
#50311=CARTESIAN_POINT('Ctrl Pts',(6.59082757677796,-1.53404069476112,10.6244579102981));
#50312=CARTESIAN_POINT('Ctrl Pts',(6.63056651595371,-1.36330696058711,10.6326681585026));
#50313=CARTESIAN_POINT('Ctrl Pts',(6.66366486677742,-1.19103728197648,10.6408784067072));
#50314=CARTESIAN_POINT('Ctrl Pts',(6.69002227061687,-1.01778731503707,10.6490886549117));
#50315=CARTESIAN_POINT('Ctrl Pts',(6.71638594013664,-0.84449616312675,10.6573008548559));
#50316=CARTESIAN_POINT('Ctrl Pts',(6.73600541657981,-0.670224610522699,
10.6655130548002));
#50317=CARTESIAN_POINT('Ctrl Pts',(6.74883205562075,-0.495534948339518,
10.6737252547444));
#50318=CARTESIAN_POINT('Ctrl Pts',(6.76166402787439,-0.320772651608627,
10.6819408692549));
#50319=CARTESIAN_POINT('Ctrl Pts',(6.76769750984418,-0.145592253658605,
10.6901564837653));
#50320=CARTESIAN_POINT('Ctrl Pts',(6.76693594979251,0.02944234035846,10.6983720982758));
#50321=CARTESIAN_POINT('Ctrl Pts',(6.76617353454229,0.204673490551597,10.7065969385613));
#50322=CARTESIAN_POINT('Ctrl Pts',(6.7586008381732,0.379758153708125,10.7148217788467));
#50323=CARTESIAN_POINT('Ctrl Pts',(6.74427338198156,0.554134955669637,10.7230466191321));
#50324=CARTESIAN_POINT('Ctrl Pts',(6.72993674855619,0.728623452034429,10.7312767277137));
#50325=CARTESIAN_POINT('Ctrl Pts',(6.70883677312071,0.90240283091759,10.7395068362952));
#50326=CARTESIAN_POINT('Ctrl Pts',(6.68108039171039,1.07492036891251,10.7477369448767));
#50327=CARTESIAN_POINT('Ctrl Pts',(6.65328595587521,1.24767443109938,10.7559783370635));
#50328=CARTESIAN_POINT('Ctrl Pts',(6.61881695570913,1.41916284896096,10.7642197292501));
#50329=CARTESIAN_POINT('Ctrl Pts',(6.57783085565331,1.58884556657195,10.7724611214368));
#50330=CARTESIAN_POINT('Ctrl Pts',(6.559992663597,1.66269579631466,10.7760479847012));
#50331=CARTESIAN_POINT('Ctrl Pts',(6.54092062560285,1.7362042097666,10.7796348479655));
#50332=CARTESIAN_POINT('Ctrl Pts',(6.52063059142613,1.8093274137529,10.7832217112298));
#50333=CARTESIAN_POINT('Ctrl Pts',(6.47283500247094,1.98157781857599,10.7916709942978));
#50334=CARTESIAN_POINT('Ctrl Pts',(6.41816856105709,2.15208230878793,10.8001202773659));
#50335=CARTESIAN_POINT('Ctrl Pts',(6.3567776680875,2.32027297499756,10.808569560434));
#50336=CARTESIAN_POINT('Ctrl Pts',(6.2954439444839,2.48830701612346,10.8170109752314));
#50337=CARTESIAN_POINT('Ctrl Pts',(6.22739836603516,2.65403121662498,10.8254523900289));
#50338=CARTESIAN_POINT('Ctrl Pts',(6.1528372684843,2.81689235640105,10.8338938048264));
#50339=CARTESIAN_POINT('Ctrl Pts',(6.07486152976478,2.98721197480637,10.8427218073142));
#50340=CARTESIAN_POINT('Ctrl Pts',(5.98975953431458,3.15439976562703,10.851549809802));
#50341=CARTESIAN_POINT('Ctrl Pts',(5.8978131589271,3.31784402020143,10.8603778122898));
#50342=CARTESIAN_POINT('Ctrl Pts',(5.8100258909488,3.473895028361,10.8688064884268));
#50343=CARTESIAN_POINT('Ctrl Pts',(5.71599996201079,3.62653336835884,10.8772351645638));
#50344=CARTESIAN_POINT('Ctrl Pts',(5.61602866345865,3.77524979984251,10.8856638407007));
#50345=CARTESIAN_POINT('Ctrl Pts',(5.51609820318497,3.92390548065944,10.8940890737233));
#50346=CARTESIAN_POINT('Ctrl Pts',(5.41022740046718,4.06864217043807,10.9025143067458));
#50347=CARTESIAN_POINT('Ctrl Pts',(5.2987536581543,4.20897834042852,10.9109395397683));
#50348=CARTESIAN_POINT('Ctrl Pts',(5.18730989897394,4.34927676414892,10.9193625066529));
#50349=CARTESIAN_POINT('Ctrl Pts',(5.07026641222063,4.4851767672602,10.9277854735375));
#50350=CARTESIAN_POINT('Ctrl Pts',(4.9480020163163,4.61622844392799,10.936208440422));
#50351=CARTESIAN_POINT('Ctrl Pts',(4.82575345400299,4.74726314902662,10.9446303165081));
#50352=CARTESIAN_POINT('Ctrl Pts',(4.69828555868826,4.8734505366306,10.9530521925942));
#50353=CARTESIAN_POINT('Ctrl Pts',(4.56601551626838,4.99437596754554,10.9614740686804));
#50354=CARTESIAN_POINT('Ctrl Pts',(4.43371847846059,5.11532607849275,10.9698976636123));
#50355=CARTESIAN_POINT('Ctrl Pts',(4.29661757959628,5.23101186001651,10.9783212585443));
#50356=CARTESIAN_POINT('Ctrl Pts',(4.1551652661537,5.34105706868499,10.9867448534763));
#50357=CARTESIAN_POINT('Ctrl Pts',(4.01369811032806,5.45111382423525,10.9951693322836));
#50358=CARTESIAN_POINT('Ctrl Pts',(3.86787889546673,5.55552862572213,11.003593811091));
#50359=CARTESIAN_POINT('Ctrl Pts',(3.71819135113202,5.65396693272671,11.0120182898984));
#50360=CARTESIAN_POINT('Ctrl Pts',(3.56843267028355,5.7524520208981,11.0204467722991));
#50361=CARTESIAN_POINT('Ctrl Pts',(3.41480226851862,5.84495476121324,11.0288752546998));
#50362=CARTESIAN_POINT('Ctrl Pts',(3.25781157025836,5.93118476973115,11.0373037371005));
#50363=CARTESIAN_POINT('Ctrl Pts',(3.20527244433795,5.96004284429127,11.0401244462449));
#50364=CARTESIAN_POINT('Ctrl Pts',(3.15235716997192,5.98819875403474,11.0429451553893));
#50365=CARTESIAN_POINT('Ctrl Pts',(3.09908550384726,6.0156427786101,11.0457658645337));
#50366=CARTESIAN_POINT('Ctrl Pts',(3.09908550384729,6.01564277861008,9.04575635804621));
#50367=CARTESIAN_POINT('Ctrl Pts',(2.93373232018328,6.10082796552481,9.0545058059455));
#50368=CARTESIAN_POINT('Ctrl Pts',(2.76486502144416,6.17919158180196,9.06325525384478));
#50369=CARTESIAN_POINT('Ctrl Pts',(2.59305716434331,6.25046746591388,9.07200470174408));
#50370=CARTESIAN_POINT('Ctrl Pts',(2.42125069459257,6.32174277447235,9.0807540789915));
#50371=CARTESIAN_POINT('Ctrl Pts',(2.24650397871028,6.38593035557837,9.08950345623892));
#50372=CARTESIAN_POINT('Ctrl Pts',(2.06941053323735,6.4428122000355,9.09825283348634));
#50373=CARTESIAN_POINT('Ctrl Pts',(1.89231845896656,6.49969360406693,9.10700214298893));
#50374=CARTESIAN_POINT('Ctrl Pts',(1.71287996431486,6.54926929700886,9.11575145249154));
#50375=CARTESIAN_POINT('Ctrl Pts',(1.53170449173494,6.59137090065481,9.12450076199413));
#50376=CARTESIAN_POINT('Ctrl Pts',(1.35053036178163,6.63347219230085,9.13325000665872));
#50377=CARTESIAN_POINT('Ctrl Pts',(1.1676195587884,6.66809944062455,9.14199925132329));
#50378=CARTESIAN_POINT('Ctrl Pts',(0.983593309310468,6.69513503985392,9.15074849598788));
#50379=CARTESIAN_POINT('Ctrl Pts',(0.799568362460066,6.72217044771213,9.15949767872105));
#50380=CARTESIAN_POINT('Ctrl Pts',(0.614428268438786,6.74161427235975,9.16824686145422));
#50381=CARTESIAN_POINT('Ctrl Pts',(0.428801816330565,6.753400476968,9.17699604418739));
#50382=CARTESIAN_POINT('Ctrl Pts',(0.243176616523095,6.76518660206241,9.18574516789552));
#50383=CARTESIAN_POINT('Ctrl Pts',(0.0570653511657863,6.76931519233996,
9.19449429160367));
#50384=CARTESIAN_POINT('Ctrl Pts',(-0.128899900799689,6.76577222610796,
9.2032434153118));
#50385=CARTESIAN_POINT('Ctrl Pts',(-0.3148639599416,6.76222928260135,9.21199248290106));
#50386=CARTESIAN_POINT('Ctrl Pts',(-0.500681721080178,6.7510148865128,9.22074155049031));
#50387=CARTESIAN_POINT('Ctrl Pts',(-0.685722110172717,6.73216712415997,
9.22949061807957));
#50388=CARTESIAN_POINT('Ctrl Pts',(-0.870761373826965,6.71331947644153,
9.23823963245592));
#50389=CARTESIAN_POINT('Ctrl Pts',(-1.05502298984272,6.68683858440007,9.24698864683228));
#50390=CARTESIAN_POINT('Ctrl Pts',(-1.23788117675982,6.6528143813144,9.25573766120864));
#50391=CARTESIAN_POINT('Ctrl Pts',(-1.43009641451717,6.61704912302394,9.26493437209617));
#50392=CARTESIAN_POINT('Ctrl Pts',(-1.62076048992621,6.57294837083183,9.2741310829837));
#50393=CARTESIAN_POINT('Ctrl Pts',(-1.80915798961058,6.5206776004207,9.28332779387122));
#50394=CARTESIAN_POINT('Ctrl Pts',(-1.98840443002939,6.47094578577431,9.29207779157773));
#50395=CARTESIAN_POINT('Ctrl Pts',(-2.16559895952119,6.413818884745,9.30082778928424));
#50396=CARTESIAN_POINT('Ctrl Pts',(-2.3401396624225,6.34949095285261,9.30957778699074));
#50397=CARTESIAN_POINT('Ctrl Pts',(-2.51467682553946,6.28516432556712,9.31832760724234));
#50398=CARTESIAN_POINT('Ctrl Pts',(-2.68656000078778,6.21363705879689,9.32707742749393));
#50399=CARTESIAN_POINT('Ctrl Pts',(-2.85520533840828,6.13515211510887,9.33582724774553));
#50400=CARTESIAN_POINT('Ctrl Pts',(-3.02384747998267,6.05666865881151,9.34457690217677));
#50401=CARTESIAN_POINT('Ctrl Pts',(-3.18925164684476,5.97122791039876,9.35332655660802));
#50402=CARTESIAN_POINT('Ctrl Pts',(-3.35085601829097,5.87912008251942,9.36207621103927));
#50403=CARTESIAN_POINT('Ctrl Pts',(-3.51245754191361,5.78701387778209,9.37082571128241));
#50404=CARTESIAN_POINT('Ctrl Pts',(-3.67025915510882,5.68824097061018,9.37957521152556));
#50405=CARTESIAN_POINT('Ctrl Pts',(-3.82372487928783,5.5831368465689,9.3883247117687));
#50406=CARTESIAN_POINT('Ctrl Pts',(-3.97718810300744,5.47803443501812,9.39707406945382));
#50407=CARTESIAN_POINT('Ctrl Pts',(-4.12631534262969,5.36660117496419,9.40582342713893));
#50408=CARTESIAN_POINT('Ctrl Pts',(-4.27060009886167,5.24921554097398,9.41457278482405));
#50409=CARTESIAN_POINT('Ctrl Pts',(-4.41488269594169,5.1318316636033,9.42332201157923));
#50410=CARTESIAN_POINT('Ctrl Pts',(-4.55432273235057,5.008495771395,9.43207123833443));
#50411=CARTESIAN_POINT('Ctrl Pts',(-4.68844662480187,4.87962675277361,9.44082046508962));
#50412=CARTESIAN_POINT('Ctrl Pts',(-4.82256868835141,4.75075949139899,9.44956957254111));
#50413=CARTESIAN_POINT('Ctrl Pts',(-4.95137454637848,4.6163594531254,9.4583186799926));
#50414=CARTESIAN_POINT('Ctrl Pts',(-5.07442674461067,4.47688309134603,9.46706778744409));
#50415=CARTESIAN_POINT('Ctrl Pts',(-5.19747742838507,4.33740844616388,9.47581678721645));
#50416=CARTESIAN_POINT('Ctrl Pts',(-5.31477440450878,4.1928578173609,9.48456578698882));
#50417=CARTESIAN_POINT('Ctrl Pts',(-5.42591931531087,4.04372211999494,9.49331478676118));
#50418=CARTESIAN_POINT('Ctrl Pts',(-5.53707636462923,3.89457013500884,9.50206474204176));
#50419=CARTESIAN_POINT('Ctrl Pts',(-5.64207983273419,3.74083230916498,9.51081469732233));
#50420=CARTESIAN_POINT('Ctrl Pts',(-5.74057303468702,3.583030872519,9.51956465260291));
#50421=CARTESIAN_POINT('Ctrl Pts',(-5.83906243363725,3.42523552887499,9.52831427003172));
#50422=CARTESIAN_POINT('Ctrl Pts',(-5.9310419176839,3.26337713157057,9.53706388746053));
#50423=CARTESIAN_POINT('Ctrl Pts',(-6.01619906699625,3.09800545291216,9.54581350488934));
#50424=CARTESIAN_POINT('Ctrl Pts',(-6.10135338095357,2.93263928039649,9.55456283099473));
#50425=CARTESIAN_POINT('Ctrl Pts',(-6.17968568352818,2.76376031540271,9.56331215710014));
#50426=CARTESIAN_POINT('Ctrl Pts',(-6.2509299269487,2.59194213831582,9.57206148320553));
#50427=CARTESIAN_POINT('Ctrl Pts',(-6.32217217691088,2.42012876880861,9.58081056449933));
#50428=CARTESIAN_POINT('Ctrl Pts',(-6.38632665483835,2.24537661647713,9.58955964579312));
#50429=CARTESIAN_POINT('Ctrl Pts',(-6.44317547869336,2.068279176215,9.59830872708692));
#50430=CARTESIAN_POINT('Ctrl Pts',(-6.50002944235922,1.8911657242347,9.60705859940188));
#50431=CARTESIAN_POINT('Ctrl Pts',(-6.54957634250385,1.71170683289247,9.61580847171683));
#50432=CARTESIAN_POINT('Ctrl Pts',(-6.59164787708383,1.53051209225416,9.6245583440318));
#50433=CARTESIAN_POINT('Ctrl Pts',(-6.63371649074996,1.34932993148091,9.63330760886658));
#50434=CARTESIAN_POINT('Ctrl Pts',(-6.66831071257111,1.16641244174075,9.64205687370137));
#50435=CARTESIAN_POINT('Ctrl Pts',(-6.69531304840321,0.982380875160824,
9.65080613853615));
#50436=CARTESIAN_POINT('Ctrl Pts',(-6.72231677033034,0.798339861796689,
9.65955585249181));
#50437=CARTESIAN_POINT('Ctrl Pts',(-6.74172778477882,0.613184940731031,
9.66830556644746));
#50438=CARTESIAN_POINT('Ctrl Pts',(-6.75348015835512,0.427545027691463,
9.67705528040311));
#50439=CARTESIAN_POINT('Ctrl Pts',(-6.76249038365214,0.285219953548324,
9.68376344820539));
#50440=CARTESIAN_POINT('Ctrl Pts',(-6.76699999999995,0.142609995759399,
9.69047161600768));
#50441=CARTESIAN_POINT('Ctrl Pts',(-6.767,2.60385621481446E-12,9.69717978380996));
#50442=CARTESIAN_POINT('',(-6.767,5.79285625171286E-10,9.30282021616271));
#50443=CARTESIAN_POINT('Ctrl Pts',(3.09908550384719,6.01564277861013,8.65139679042609));
#50444=CARTESIAN_POINT('Ctrl Pts',(2.93373232018324,6.10082796552483,8.66014623832538));
#50445=CARTESIAN_POINT('Ctrl Pts',(2.76486502144417,6.17919158180195,8.66889568622467));
#50446=CARTESIAN_POINT('Ctrl Pts',(2.59305716434338,6.25046746591385,8.67764513412396));
#50447=CARTESIAN_POINT('Ctrl Pts',(2.4212506945927,6.32174277447229,8.68639451137138));
#50448=CARTESIAN_POINT('Ctrl Pts',(2.24650397871047,6.38593035557829,8.6951438886188));
#50449=CARTESIAN_POINT('Ctrl Pts',(2.06941053323761,6.44281220003542,8.70389326586621));
#50450=CARTESIAN_POINT('Ctrl Pts',(1.89231845896676,6.49969360406687,8.71264257536881));
#50451=CARTESIAN_POINT('Ctrl Pts',(1.712879964315,6.54926929700882,8.7213918848714));
#50452=CARTESIAN_POINT('Ctrl Pts',(1.53170449173501,6.59137090065479,8.730141194374));
#50453=CARTESIAN_POINT('Ctrl Pts',(1.3505303617817,6.63347219230083,8.73889043903859));
#50454=CARTESIAN_POINT('Ctrl Pts',(1.16761955878848,6.66809944062453,8.74763968370318));
#50455=CARTESIAN_POINT('Ctrl Pts',(0.983593309310546,6.69513503985391,8.75638892836777));
#50456=CARTESIAN_POINT('Ctrl Pts',(0.799568362460019,6.72217044771214,8.76513811110095));
#50457=CARTESIAN_POINT('Ctrl Pts',(0.614428268438608,6.74161427235977,8.77388729383413));
#50458=CARTESIAN_POINT('Ctrl Pts',(0.428801816330259,6.75340047696802,8.7826364765673));
#50459=CARTESIAN_POINT('Ctrl Pts',(0.243176616522789,6.76518660206242,8.79138560027544));
#50460=CARTESIAN_POINT('Ctrl Pts',(0.0570653511654812,6.76931519233997,
8.80013472398356));
#50461=CARTESIAN_POINT('Ctrl Pts',(-0.128899900799994,6.76577222610795,
8.80888384769169));
#50462=CARTESIAN_POINT('Ctrl Pts',(-0.314863959941904,6.76222928260133,
8.81763291528095));
#50463=CARTESIAN_POINT('Ctrl Pts',(-0.500681721080484,6.75101488651278,
8.82638198287021));
#50464=CARTESIAN_POINT('Ctrl Pts',(-0.685722110173022,6.73216712415994,
8.83513105045947));
#50465=CARTESIAN_POINT('Ctrl Pts',(-0.870761373827397,6.71331947644148,
8.84388006483583));
#50466=CARTESIAN_POINT('Ctrl Pts',(-1.05502298984328,6.68683858439999,8.85262907921219));
#50467=CARTESIAN_POINT('Ctrl Pts',(-1.2378811767605,6.65281438131428,8.86137809358856));
#50468=CARTESIAN_POINT('Ctrl Pts',(-1.430096414506,6.617049123026,8.87057480447552));
#50469=CARTESIAN_POINT('Ctrl Pts',(-1.62076048990337,6.57294837083711,8.87977151536247));
#50470=CARTESIAN_POINT('Ctrl Pts',(-1.8091579895764,6.52067760043018,8.88896822624943));
#50471=CARTESIAN_POINT('Ctrl Pts',(-1.98840442999547,6.47094578578474,8.89771822395594));
#50472=CARTESIAN_POINT('Ctrl Pts',(-2.16559895948757,6.41381888475635,8.90646822166245));
#50473=CARTESIAN_POINT('Ctrl Pts',(-2.34013966238922,6.34949095286488,8.91521821936895));
#50474=CARTESIAN_POINT('Ctrl Pts',(-2.5146768255064,6.28516432558035,8.92396803962054));
#50475=CARTESIAN_POINT('Ctrl Pts',(-2.68656000075498,6.21363705881107,8.93271785987215));
#50476=CARTESIAN_POINT('Ctrl Pts',(-2.85520533837578,6.135152115124,8.94146768012374));
#50477=CARTESIAN_POINT('Ctrl Pts',(-3.02384747995052,6.05666865882756,8.95021733455498));
#50478=CARTESIAN_POINT('Ctrl Pts',(-3.18925164681301,5.97122791041572,8.95896698898622));
#50479=CARTESIAN_POINT('Ctrl Pts',(-3.35085601825965,5.87912008253727,8.96771664341746));
#50480=CARTESIAN_POINT('Ctrl Pts',(-3.51245754188273,5.78701387780083,8.9764661436606));
#50481=CARTESIAN_POINT('Ctrl Pts',(-3.67025915507841,5.68824097062979,8.98521564390373));
#50482=CARTESIAN_POINT('Ctrl Pts',(-3.82372487925794,5.58313684658937,8.99396514414687));
#50483=CARTESIAN_POINT('Ctrl Pts',(-3.97718810297827,5.47803443503931,9.002714501832));
#50484=CARTESIAN_POINT('Ctrl Pts',(-4.12631534260126,5.36660117498606,9.01146385951711));
#50485=CARTESIAN_POINT('Ctrl Pts',(-4.27060009883401,5.24921554099648,9.02021321720224));
#50486=CARTESIAN_POINT('Ctrl Pts',(-4.41488269591464,5.13183166362657,9.02896244395743));
#50487=CARTESIAN_POINT('Ctrl Pts',(-4.55432273232418,5.008495771419,9.03771167071264));
#50488=CARTESIAN_POINT('Ctrl Pts',(-4.68844662477616,4.87962675279832,9.04646089746782));
#50489=CARTESIAN_POINT('Ctrl Pts',(-4.82256868832633,4.75075949142444,9.05521000491931));
#50490=CARTESIAN_POINT('Ctrl Pts',(-4.95137454635407,4.61635945315159,9.0639591123708));
#50491=CARTESIAN_POINT('Ctrl Pts',(-5.07442674458695,4.47688309137292,9.07270821982229));
#50492=CARTESIAN_POINT('Ctrl Pts',(-5.19747742836243,4.33740844619103,9.08145721959467));
#50493=CARTESIAN_POINT('Ctrl Pts',(-5.31477440448721,4.19285781738826,9.09020621936706));
#50494=CARTESIAN_POINT('Ctrl Pts',(-5.42591931529037,4.04372212002246,9.09895521913944));
#50495=CARTESIAN_POINT('Ctrl Pts',(-5.53707636460948,3.89457013503692,9.10770517442002));
#50496=CARTESIAN_POINT('Ctrl Pts',(-5.64207983271522,3.74083230919359,9.11645512970061));
#50497=CARTESIAN_POINT('Ctrl Pts',(-5.74057303466886,3.5830308725481,9.12520508498119));
#50498=CARTESIAN_POINT('Ctrl Pts',(-5.83906243361988,3.4252355289046,9.13395470241));
#50499=CARTESIAN_POINT('Ctrl Pts',(-5.93104191766735,3.26337713160065,9.14270431983881));
#50500=CARTESIAN_POINT('Ctrl Pts',(-6.01619906698054,3.09800545294267,9.15145393726762));
#50501=CARTESIAN_POINT('Ctrl Pts',(-6.10135338093861,2.93263928042761,9.160203263373));
#50502=CARTESIAN_POINT('Ctrl Pts',(-6.179685683514,2.7637603154344,9.16895258947838));
#50503=CARTESIAN_POINT('Ctrl Pts',(-6.25092992693533,2.59194213834805,9.17770191558377));
#50504=CARTESIAN_POINT('Ctrl Pts',(-6.32217217689837,2.42012876884127,9.18645099687756));
#50505=CARTESIAN_POINT('Ctrl Pts',(-6.38632665482673,2.24537661651018,9.19520007817135));
#50506=CARTESIAN_POINT('Ctrl Pts',(-6.44317547868264,2.06827917624841,9.20394915946514));
#50507=CARTESIAN_POINT('Ctrl Pts',(-6.5000294423494,1.89116572426846,9.2126990317801));
#50508=CARTESIAN_POINT('Ctrl Pts',(-6.54957634249494,1.71170683292655,9.22144890409506));
#50509=CARTESIAN_POINT('Ctrl Pts',(-6.59164787707586,1.53051209228852,9.23019877641002));
#50510=CARTESIAN_POINT('Ctrl Pts',(-6.63371649074297,1.34932993151531,9.23894804124482));
#50511=CARTESIAN_POINT('Ctrl Pts',(-6.6683107125651,1.16641244177513,9.24769730607961));
#50512=CARTESIAN_POINT('Ctrl Pts',(-6.69531304839817,0.982380875195151,
9.25644657091441));
#50513=CARTESIAN_POINT('Ctrl Pts',(-6.72231677032625,0.79833986183109,9.26519628487006));
#50514=CARTESIAN_POINT('Ctrl Pts',(-6.74172778477569,0.613184940765469,
9.27394599882572));
#50515=CARTESIAN_POINT('Ctrl Pts',(-6.75348015835294,0.427545027725897,
9.28269571278138));
#50516=CARTESIAN_POINT('Ctrl Pts',(-6.76249038363927,0.285219953763168,
9.28940388057515));
#50517=CARTESIAN_POINT('Ctrl Pts',(-6.76699999998779,0.142609996155356,
9.29611204836894));
#50518=CARTESIAN_POINT('Ctrl Pts',(-6.767,5.79286453889775E-10,9.30282021616271));
#50519=CARTESIAN_POINT('Ctrl Pts',(-6.767,2.48800301388039E-12,9.30282021618984));
#50520=CARTESIAN_POINT('Ctrl Pts',(-6.76700000000007,-0.18600724955762,
9.31156972800259));
#50521=CARTESIAN_POINT('Ctrl Pts',(-6.75932637294259,-0.372014355813903,
9.32031923981534));
#50522=CARTESIAN_POINT('Ctrl Pts',(-6.74400518263379,-0.55738953758438,
9.32906875162809));
#50523=CARTESIAN_POINT('Ctrl Pts',(-6.7286840570375,-0.742763936380955,
9.33781822648529));
#50524=CARTESIAN_POINT('Ctrl Pts',(-6.70571545643587,-0.927506130403373,
9.3465677013425));
#50525=CARTESIAN_POINT('Ctrl Pts',(-6.67517739401599,-1.11098864009399,
9.3553171761997));
#50526=CARTESIAN_POINT('Ctrl Pts',(-6.64463945804417,-1.29447039004398,
9.36406661482822));
#50527=CARTESIAN_POINT('Ctrl Pts',(-6.60653217002755,-1.47669218339137,
9.37281605345672));
#50528=CARTESIAN_POINT('Ctrl Pts',(-6.56098496085515,-1.65703510627646,
9.38156549208523));
#50529=CARTESIAN_POINT('Ctrl Pts',(-6.5154379364959,-1.83737729739891,9.39031489521187));
#50530=CARTESIAN_POINT('Ctrl Pts',(-6.46245112156927,-2.01584035544854,
9.39906429833851));
#50531=CARTESIAN_POINT('Ctrl Pts',(-6.40220448361744,-2.1918181379733,9.40781370146514));
#50532=CARTESIAN_POINT('Ctrl Pts',(-6.34195808511996,-2.36779522106244,
9.41656306981669));
#50533=CARTESIAN_POINT('Ctrl Pts',(-6.27445201416371,-2.54128677725703,
9.42531243816822));
#50534=CARTESIAN_POINT('Ctrl Pts',(-6.19991555052734,-2.71170355428635,
9.43406180651976));
#50535=CARTESIAN_POINT('Ctrl Pts',(-6.12537937695127,-2.88211966813502,
9.44281114082295));
#50536=CARTESIAN_POINT('Ctrl Pts',(-6.04381298028354,-3.04946076419863,
9.45156047512612));
#50537=CARTESIAN_POINT('Ctrl Pts',(-5.95549339308879,-3.21315848424503,
9.4603098094293));
#50538=CARTESIAN_POINT('Ctrl Pts',(-5.86717414225702,-3.37685558085269,
9.46905911041086));
#50539=CARTESIAN_POINT('Ctrl Pts',(-5.77210188843955,-3.53690907700182,
9.47780841139242));
#50540=CARTESIAN_POINT('Ctrl Pts',(-5.67059953311257,-3.69277537024168,
9.48655771237398));
#50541=CARTESIAN_POINT('Ctrl Pts',(-5.56909755592581,-3.8486410828121,9.4953069807606));
#50542=CARTESIAN_POINT('Ctrl Pts',(-5.46116568154827,-4.00031938355018,
9.50405624914723));
#50543=CARTESIAN_POINT('Ctrl Pts',(-5.34717048488226,-4.1472951191836,9.51280551753385));
#50544=CARTESIAN_POINT('Ctrl Pts',(-5.2331757034314,-4.2942703194738,9.52155475405221));
#50545=CARTESIAN_POINT('Ctrl Pts',(-5.11311781951369,-4.43654276249762,
9.53030399057056));
#50546=CARTESIAN_POINT('Ctrl Pts',(-4.98740458929052,-4.57362924412593,
9.53905322708891));
#50547=CARTESIAN_POINT('Ctrl Pts',(-4.86169180652541,-4.71071523781473,
9.54780243246563));
#50548=CARTESIAN_POINT('Ctrl Pts',(-4.73032391141367,-4.8426150958469,9.55655163784235));
#50549=CARTESIAN_POINT('Ctrl Pts',(-4.59374706947116,-4.96888084599793,
9.56530084321906));
#50550=CARTESIAN_POINT('Ctrl Pts',(-4.4571707023134,-5.09514615720887,9.57405001818075));
#50551=CARTESIAN_POINT('Ctrl Pts',(-4.3153856349724,-5.21577720520682,9.58279919314242));
#50552=CARTESIAN_POINT('Ctrl Pts',(-4.16887340951967,-5.33036429293532,
9.5915483681041));
#50553=CARTESIAN_POINT('Ctrl Pts',(-4.02236168122451,-5.4449509918373,9.60029751337735));
#50554=CARTESIAN_POINT('Ctrl Pts',(-3.87112305263153,-5.55349359497947,
9.60904665865059));
#50555=CARTESIAN_POINT('Ctrl Pts',(-3.71567116928974,-5.65562346357226,
9.61779580392384));
#50556=CARTESIAN_POINT('Ctrl Pts',(-3.56021980053292,-5.75775299408939,
9.62654492023521));
#50557=CARTESIAN_POINT('Ctrl Pts',(-3.40055544442068,-5.85346967519888,
9.63529403654658));
#50558=CARTESIAN_POINT('Ctrl Pts',(-3.23722035886829,-5.9424484304139,9.64404315285795));
#50559=CARTESIAN_POINT('Ctrl Pts',(-3.07388580043488,-6.03142689847452,
9.65279224093395));
#50560=CARTESIAN_POINT('Ctrl Pts',(-2.90688078789233,-6.11366734707897,
9.66154132900997));
#50561=CARTESIAN_POINT('Ctrl Pts',(-2.73677250610415,-6.18889047001419,
9.67029041708598));
#50562=CARTESIAN_POINT('Ctrl Pts',(-2.56666475916967,-6.26411335643321,
9.67903947765314));
#50563=CARTESIAN_POINT('Ctrl Pts',(-2.39345402457135,-6.3323188454524,9.68778853822029));
#50564=CARTESIAN_POINT('Ctrl Pts',(-2.21772855944117,-6.39327529804865,
9.69653759878746));
#50565=CARTESIAN_POINT('Ctrl Pts',(-2.04200363223662,-6.4542315640468,9.70528663257226));
#50566=CARTESIAN_POINT('Ctrl Pts',(-1.86376426061124,-6.50793874412426,
9.71403566635705));
#50567=CARTESIAN_POINT('Ctrl Pts',(-1.68361577621798,-6.55421443943284,
9.72278470014184));
#50568=CARTESIAN_POINT('Ctrl Pts',(-1.50346782833284,-6.60048999692573,
9.73153370787076));
#50569=CARTESIAN_POINT('Ctrl Pts',(-1.32141105657414,-6.63933404265158,
9.74028271559967));
#50570=CARTESIAN_POINT('Ctrl Pts',(-1.13806375346518,-6.67061465631532,
9.74903172332859));
#50571=CARTESIAN_POINT('Ctrl Pts',(-0.954716981169746,-6.70189517941775,
9.75778070572802));
#50572=CARTESIAN_POINT('Ctrl Pts',(-0.770079967441923,-6.72561226609008,
9.76652968812746));
#50573=CARTESIAN_POINT('Ctrl Pts',(-0.584779764072615,-6.74168536995989,
9.7752786705269));
#50574=CARTESIAN_POINT('Ctrl Pts',(-0.391489587592477,-6.75845153117875,
9.78440490094252));
#50575=CARTESIAN_POINT('Ctrl Pts',(-0.197478091804735,-6.76689985146396,
9.79353113135812));
#50576=CARTESIAN_POINT('Ctrl Pts',(-0.00346214753050771,-6.76699911434415,
9.80265736177374));
#50577=CARTESIAN_POINT('Ctrl Pts',(0.18449079848517,-6.76709527525933,9.81149839748887));
#50578=CARTESIAN_POINT('Ctrl Pts',(0.372447602155317,-6.7593563379076,9.820339433204));
#50579=CARTESIAN_POINT('Ctrl Pts',(0.559756448194758,-6.74380914014509,
9.82918046891913));
#50580=CARTESIAN_POINT('Ctrl Pts',(0.745136131043981,-6.72842206873148,
9.83793044753244));
#50581=CARTESIAN_POINT('Ctrl Pts',(0.929880851945746,-6.70538686355714,
9.84668042614576));
#50582=CARTESIAN_POINT('Ctrl Pts',(1.11336305057541,-6.67478177303299,9.85543040475908));
#50583=CARTESIAN_POINT('Ctrl Pts',(1.29684337090212,-6.64417699581243,9.86418029379906));
#50584=CARTESIAN_POINT('Ctrl Pts',(1.4790609120529,-6.60600253548038,9.87293018283905));
#50585=CARTESIAN_POINT('Ctrl Pts',(1.65939671095331,-6.56038806441184,9.88168007187903));
#50586=CARTESIAN_POINT('Ctrl Pts',(1.83973072369273,-6.51477404513818,9.89042987425453));
#50587=CARTESIAN_POINT('Ctrl Pts',(2.01818275357152,-6.46172023288625,9.89917967663001));
#50588=CARTESIAN_POINT('Ctrl Pts',(2.19414664033445,-6.40140683918067,9.9079294790055));
#50589=CARTESIAN_POINT('Ctrl Pts',(2.37010884271371,-6.34109402281455,9.91667919762504));
#50590=CARTESIAN_POINT('Ctrl Pts',(2.54358267847912,-6.27352185699749,9.92542891624459));
#50591=CARTESIAN_POINT('Ctrl Pts',(2.71397890841841,-6.19891986435218,9.93417863486413));
#50592=CARTESIAN_POINT('Ctrl Pts',(2.88437356389041,-6.12431856103197,9.94292827263594));
#50593=CARTESIAN_POINT('Ctrl Pts',(3.05169040787271,-6.04268767582507,9.95167791040775));
#50594=CARTESIAN_POINT('Ctrl Pts',(3.21536112512152,-5.95430447953892,9.96042754817957));
#50595=CARTESIAN_POINT('Ctrl Pts',(3.3790303844294,-5.86592207054986,9.96917710801164));
#50596=CARTESIAN_POINT('Ctrl Pts',(3.5390533298007,-5.77078760703318,9.9779266678437));
#50597=CARTESIAN_POINT('Ctrl Pts',(3.69488643041988,-5.66922422085236,9.98667622767577));
#50598=CARTESIAN_POINT('Ctrl Pts',(3.85071819468837,-5.56766170563093,9.99542571247577));
#50599=CARTESIAN_POINT('Ctrl Pts',(4.00235994599318,-5.45967053456182,10.0041751972758));
#50600=CARTESIAN_POINT('Ctrl Pts',(4.14929662974394,-5.34561750206612,10.0129246820758));
#50601=CARTESIAN_POINT('Ctrl Pts',(4.29623210225136,-5.2315654097439,10.0216740947511));
#50602=CARTESIAN_POINT('Ctrl Pts',(4.43846235842208,-5.11145173172108,10.0304235074265));
#50603=CARTESIAN_POINT('Ctrl Pts',(4.57550431797517,-4.9856844300648,10.0391729201018));
#50604=CARTESIAN_POINT('Ctrl Pts',(4.71254519337589,-4.85991812336597,10.0479222635597));
#50605=CARTESIAN_POINT('Ctrl Pts',(4.84439764315085,-4.72849847630998,10.0566716070176));
#50606=CARTESIAN_POINT('Ctrl Pts',(4.97061384196792,-4.59187184425229,10.0654209504755));
#50607=CARTESIAN_POINT('Ctrl Pts',(5.09682908420313,-4.45524624767625,10.0741702276229));
#50608=CARTESIAN_POINT('Ctrl Pts',(5.21740796650278,-4.31341395556763,10.0829195047703));
#50609=CARTESIAN_POINT('Ctrl Pts',(5.33194095942358,-4.16685668162719,10.0916687819176));
#50610=CARTESIAN_POINT('Ctrl Pts',(5.44647312235243,-4.02030046975066,10.1004179956612));
#50611=CARTESIAN_POINT('Ctrl Pts',(5.55495930712401,-3.86901957035386,10.1091672094047));
#50612=CARTESIAN_POINT('Ctrl Pts',(5.65703106079909,-3.713527780582,10.1179164231483));
#50613=CARTESIAN_POINT('Ctrl Pts',(5.75910210868842,-3.55803706597431,10.1266655763945));
#50614=CARTESIAN_POINT('Ctrl Pts',(5.85475865698647,-3.39833575880731,10.1354147296406));
#50615=CARTESIAN_POINT('Ctrl Pts',(5.94367583069153,-3.23496624706556,10.1441638828868));
#50616=CARTESIAN_POINT('Ctrl Pts',(6.03259241910163,-3.07159781069931,10.152912978542));
#50617=CARTESIAN_POINT('Ctrl Pts',(6.11476958471049,-2.90456146975662,10.1616620741971));
#50618=CARTESIAN_POINT('Ctrl Pts',(6.18992823574463,-2.73442451648082,10.1704111698522));
#50619=CARTESIAN_POINT('Ctrl Pts',(6.26508641701014,-2.56428862662224,10.1791602108223));
#50620=CARTESIAN_POINT('Ctrl Pts',(6.33322605570376,-2.39105242531068,10.1879092517925));
#50621=CARTESIAN_POINT('Ctrl Pts',(6.39411573747846,-2.21530425353501,10.1966582927626));
#50622=CARTESIAN_POINT('Ctrl Pts',(6.45500505889195,-2.03955712188341,10.2054072819536));
#50623=CARTESIAN_POINT('Ctrl Pts',(6.5086444154499,-1.86129832025359,10.2141562711446));
#50624=CARTESIAN_POINT('Ctrl Pts',(6.55485164049959,-1.68113324012104,10.2229052603356));
#50625=CARTESIAN_POINT('Ctrl Pts',(6.60199852639157,-1.49730435912689,10.2318321672125));
#50626=CARTESIAN_POINT('Ctrl Pts',(6.64140767441052,-1.31149113173438,10.2407590740893));
#50627=CARTESIAN_POINT('Ctrl Pts',(6.67293975269639,-1.12435050446214,10.2496859809662));
#50628=CARTESIAN_POINT('Ctrl Pts',(6.70384664831538,-0.940920291561549,
10.2584358951502));
#50629=CARTESIAN_POINT('Ctrl Pts',(6.72718585889691,-0.756215114275723,
10.2671858093342));
#50630=CARTESIAN_POINT('Ctrl Pts',(6.74287810451883,-0.570862389372904,
10.2759357235182));
#50631=CARTESIAN_POINT('Ctrl Pts',(6.75857004154136,-0.385513309565947,
10.2846854656288));
#50632=CARTESIAN_POINT('Ctrl Pts',(6.76661529035562,-0.199516993257141,
10.2934352077394));
#50633=CARTESIAN_POINT('Ctrl Pts',(6.76698652348897,-0.0135052182030729,
10.3021849498499));
#50634=CARTESIAN_POINT('Ctrl Pts',(6.76735774981519,0.172503146039862,10.3109345315206));
#50635=CARTESIAN_POINT('Ctrl Pts',(6.76005524147474,0.358526681834424,10.3196841131912));
#50636=CARTESIAN_POINT('Ctrl Pts',(6.74510380214874,0.543933542115802,10.3284336948619));
#50637=CARTESIAN_POINT('Ctrl Pts',(6.73015261710969,0.729337249085682,10.3371831277238));
#50638=CARTESIAN_POINT('Ctrl Pts',(6.70755278444592,0.914124015855645,10.3459325605857));
#50639=CARTESIAN_POINT('Ctrl Pts',(6.67738106408273,1.09766621749486,10.3546819934477));
#50640=CARTESIAN_POINT('Ctrl Pts',(6.64720981677235,1.28120554143418,10.36343128913));
#50641=CARTESIAN_POINT('Ctrl Pts',(6.60946696581502,1.46350005650712,10.3721805848124));
#50642=CARTESIAN_POINT('Ctrl Pts',(6.56428070010972,1.64393062206621,10.3809298804947));
#50643=CARTESIAN_POINT('Ctrl Pts',(6.5190950828272,1.82435859844726,10.3896790506247));
#50644=CARTESIAN_POINT('Ctrl Pts',(6.46646633415642,2.00292240086623,10.3984282207547));
#50645=CARTESIAN_POINT('Ctrl Pts',(6.40657319597176,2.17901557696501,10.4071773908847));
#50646=CARTESIAN_POINT('Ctrl Pts',(6.34668083768276,2.35510646007485,10.4159264470877));
#50647=CARTESIAN_POINT('Ctrl Pts',(6.27952437143864,2.52872650996584,10.4246755032908));
#50648=CARTESIAN_POINT('Ctrl Pts',(6.20533187335111,2.69928607997982,10.4334245594939));
#50649=CARTESIAN_POINT('Ctrl Pts',(6.12831449784228,2.87633970115448,10.4425067357827));
#50650=CARTESIAN_POINT('Ctrl Pts',(6.0437148946313,3.05009490562395,10.4515889120716));
#50651=CARTESIAN_POINT('Ctrl Pts',(5.95184265120469,3.21991584599672,10.4606710883604));
#50652=CARTESIAN_POINT('Ctrl Pts',(5.86333281335467,3.38352155905345,10.4694208687148));
#50653=CARTESIAN_POINT('Ctrl Pts',(5.76807337235655,3.54347560903872,10.4781706490692));
#50654=CARTESIAN_POINT('Ctrl Pts',(5.66638790086322,3.69923467178698,10.4869204294237));
#50655=CARTESIAN_POINT('Ctrl Pts',(5.56470608502706,3.85498813489817,10.4956698952179));
#50656=CARTESIAN_POINT('Ctrl Pts',(5.45659885766912,4.00654667256316,10.5044193610122));
#50657=CARTESIAN_POINT('Ctrl Pts',(5.34243340580464,4.15339551506267,10.5131688268065));
#50658=CARTESIAN_POINT('Ctrl Pts',(5.22827145140547,4.30023985883927,10.5219180245603));
#50659=CARTESIAN_POINT('Ctrl Pts',(5.1080518197804,4.44237456993099,10.5306672223142));
#50660=CARTESIAN_POINT('Ctrl Pts',(4.982182812825,4.57931691626505,10.5394164200681));
#50661=CARTESIAN_POINT('Ctrl Pts',(4.8563169929618,4.71625579512211,10.5481653962861));
#50662=CARTESIAN_POINT('Ctrl Pts',(4.72480227791793,4.84800236135813,10.5569143725041));
#50663=CARTESIAN_POINT('Ctrl Pts',(4.58808530848072,4.97410918678947,10.5656633487221));
#50664=CARTESIAN_POINT('Ctrl Pts',(4.45135945056924,5.1002242108905,10.5744128937433));
#50665=CARTESIAN_POINT('Ctrl Pts',(4.30943087207988,5.2206985661203,10.5831624387645));
#50666=CARTESIAN_POINT('Ctrl Pts',(4.1627816432241,5.33512305301729,10.5919119837857));
#50667=CARTESIAN_POINT('Ctrl Pts',(4.01614103534319,5.4495408133148,10.6006610144529));
#50668=CARTESIAN_POINT('Ctrl Pts',(3.86478055833327,5.55790924068398,10.6094100451202));
#50669=CARTESIAN_POINT('Ctrl Pts',(3.70921425811851,5.65986029751357,10.6181590757875));
#50670=CARTESIAN_POINT('Ctrl Pts',(3.55364584530017,5.76181273884718,10.6269082252673));
#50671=CARTESIAN_POINT('Ctrl Pts',(3.39387173464239,5.85734747818125,10.6356573747472));
#50672=CARTESIAN_POINT('Ctrl Pts',(3.23043456092297,5.94614005448866,10.644406524227));
#50673=CARTESIAN_POINT('Ctrl Pts',(3.18690768806317,5.96978744811321,10.64673661296));
#50674=CARTESIAN_POINT('Ctrl Pts',(3.14312114982841,5.99295688499321,10.6490667016931));
#50675=CARTESIAN_POINT('Ctrl Pts',(3.09908550384714,6.01564277861016,10.6513967904261));
#50676=CARTESIAN_POINT('Origin',(0.,0.,-63.6971797838103));
#50677=CARTESIAN_POINT('',(3.09908550384717,6.01564277861014,13.0457845165097));
#50678=CARTESIAN_POINT('',(3.09908550384725,6.0156427786101,12.6512833602796));
#50679=CARTESIAN_POINT('',(3.09908550384721,6.01564277861012,-63.6971797838103));
#50680=CARTESIAN_POINT('',(-6.76699966570739,-0.00212704398872074,11.6971797837775));
#50681=CARTESIAN_POINT('Ctrl Pts',(-6.76699966570717,-0.00212704467573977,
11.6971797838099));
#50682=CARTESIAN_POINT('Ctrl Pts',(-6.76692897361369,-0.22702752675126,
11.7077762688185));
#50683=CARTESIAN_POINT('Ctrl Pts',(-6.75564229943246,-0.451681332267032,
11.7183727538272));
#50684=CARTESIAN_POINT('Ctrl Pts',(-6.73323789820075,-0.675126955641032,
11.7289692388358));
#50685=CARTESIAN_POINT('Ctrl Pts',(-6.72842056772625,-0.723171596501596,
11.7312476648302));
#50686=CARTESIAN_POINT('Ctrl Pts',(-6.72308942464251,-0.771160425130636,
11.7335260908246));
#50687=CARTESIAN_POINT('Ctrl Pts',(-6.71724575091993,-0.819083952808324,
11.7358045168189));
#50688=CARTESIAN_POINT('Ctrl Pts',(-6.69591375023501,-0.994026082327715,
11.7441217821523));
#50689=CARTESIAN_POINT('Ctrl Pts',(-6.6677226297911,-1.16830334640407,11.7524390474857));
#50690=CARTESIAN_POINT('Ctrl Pts',(-6.6327277204654,-1.34134707893591,11.7607563128191));
#50691=CARTESIAN_POINT('Ctrl Pts',(-6.59776232665293,-1.51424486239472,
11.7690665631792));
#50692=CARTESIAN_POINT('Ctrl Pts',(-6.55600464577617,-1.68591084794382,
11.7773768135394));
#50693=CARTESIAN_POINT('Ctrl Pts',(-6.50756161391943,-1.85578308027698,
11.7856870638994));
#50694=CARTESIAN_POINT('Ctrl Pts',(-6.45915056824995,-2.02554314859347,
11.7939918271293));
#50695=CARTESIAN_POINT('Ctrl Pts',(-6.40406306257704,-2.19351149035547,
11.8022965903592));
#50696=CARTESIAN_POINT('Ctrl Pts',(-6.34245680869598,-2.35913768776348,
11.810601353589));
#50697=CARTESIAN_POINT('Ctrl Pts',(-6.28087995505695,-2.52468484367839,
11.8189021535516));
#50698=CARTESIAN_POINT('Ctrl Pts',(-6.21279067400815,-2.68789175744743,
11.8272029535143));
#50699=CARTESIAN_POINT('Ctrl Pts',(-6.13839616548183,-2.84822427410448,
11.8355037534769));
#50700=CARTESIAN_POINT('Ctrl Pts',(-6.06402354635039,-3.00850961548154,
11.8438021110618));
#50701=CARTESIAN_POINT('Ctrl Pts',(-5.98334954395937,-3.16592193042428,
11.8521004686467));
#50702=CARTESIAN_POINT('Ctrl Pts',(-5.89662911271887,-3.31994790727751,
11.8603988262316));
#50703=CARTESIAN_POINT('Ctrl Pts',(-5.80989985787322,-3.47398955592091,
11.8686980281554));
#50704=CARTESIAN_POINT('Ctrl Pts',(-5.71712310901313,-3.62464387126268,
11.8769972300792));
#50705=CARTESIAN_POINT('Ctrl Pts',(-5.61859960818609,-3.77142246942597,
11.885296432003));
#50706=CARTESIAN_POINT('Ctrl Pts',(-5.52006611894369,-3.91821594815677,
11.8935964753085));
#50707=CARTESIAN_POINT('Ctrl Pts',(-5.41578490998046,-4.06113263727009,
11.901896518614));
#50708=CARTESIAN_POINT('Ctrl Pts',(-5.30609980771636,-4.19971354148737,
11.9101965619195));
#50709=CARTESIAN_POINT('Ctrl Pts',(-5.19638537749535,-4.33833149991442,
11.9184988245175));
#50710=CARTESIAN_POINT('Ctrl Pts',(-5.08126439006012,-4.47261108999051,
11.9268010871154));
#50711=CARTESIAN_POINT('Ctrl Pts',(-4.96112078117622,-4.60212663825991,
11.9351033497133));
#50712=CARTESIAN_POINT('Ctrl Pts',(-4.84092510141443,-4.73169831925547,
11.9434092105559));
#50713=CARTESIAN_POINT('Ctrl Pts',(-4.71570269820271,-4.85650158844747,
11.9517150713985));
#50714=CARTESIAN_POINT('Ctrl Pts',(-4.58587427479379,-4.9761477204545,11.9600209322411));
#50715=CARTESIAN_POINT('Ctrl Pts',(-4.45589238502848,-5.09593528263109,
11.9683366111973));
#50716=CARTESIAN_POINT('Ctrl Pts',(-4.32129385294283,-5.21055329179029,
11.9766522901534));
#50717=CARTESIAN_POINT('Ctrl Pts',(-4.1825332742568,-5.31965265874895,11.9849679691095));
#50718=CARTESIAN_POINT('Ctrl Pts',(-4.04368493060976,-5.4288210301884,11.9932889076664));
#50719=CARTESIAN_POINT('Ctrl Pts',(-3.90066957185888,-5.53246359462947,
12.0016098462233));
#50720=CARTESIAN_POINT('Ctrl Pts',(-3.75397077761656,-5.63027462925219,
12.0099307847801));
#50721=CARTESIAN_POINT('Ctrl Pts',(-3.60705394352661,-5.72823104136896,
12.018264090829));
#50722=CARTESIAN_POINT('Ctrl Pts',(-3.45644302955745,-5.8203384207047,12.026597396878));
#50723=CARTESIAN_POINT('Ctrl Pts',(-3.3026473813108,-5.90633636654068,12.0349307029269));
#50724=CARTESIAN_POINT('Ctrl Pts',(-3.18944470408375,-5.96963593200723,
12.0410645081785));
#50725=CARTESIAN_POINT('Ctrl Pts',(-3.07451710530569,-6.0296264745796,12.0471983134301));
#50726=CARTESIAN_POINT('Ctrl Pts',(-2.95807432651365,-6.08622093575486,
12.0533321186817));
#50727=CARTESIAN_POINT('Ctrl Pts',(-2.8048484335932,-6.16069302357251,12.0614035319237));
#50728=CARTESIAN_POINT('Ctrl Pts',(-2.64852642815876,-6.22951188052598,
12.0694749451657));
#50729=CARTESIAN_POINT('Ctrl Pts',(-2.48957238179492,-6.29240163656167,
12.0775463584078));
#50730=CARTESIAN_POINT('Ctrl Pts',(-2.33081788907027,-6.35521243971776,
12.085607638659));
#50731=CARTESIAN_POINT('Ctrl Pts',(-2.16943827254946,-6.41210881713044,
12.0936689189102));
#50732=CARTESIAN_POINT('Ctrl Pts',(-2.00592312754502,-6.4628601568021,12.1017301991615));
#50733=CARTESIAN_POINT('Ctrl Pts',(-1.84257740263408,-6.5135589123739,12.1097831270191));
#50734=CARTESIAN_POINT('Ctrl Pts',(-1.67710090565475,-6.55812519100345,
12.1178360548767));
#50735=CARTESIAN_POINT('Ctrl Pts',(-1.51000409965097,-6.5963760216529,12.1258889827343));
#50736=CARTESIAN_POINT('Ctrl Pts',(-1.34304383437945,-6.63459559619068,
12.1339353302587));
#50737=CARTESIAN_POINT('Ctrl Pts',(-1.17446625702939,-6.66650991125675,
12.1419816777831));
#50738=CARTESIAN_POINT('Ctrl Pts',(-1.00479781975984,-6.69198553057356,
12.1500280253074));
#50739=CARTESIAN_POINT('Ctrl Pts',(-0.835230909908369,-6.71744590560631,
12.1580695580006));
#50740=CARTESIAN_POINT('Ctrl Pts',(-0.664574807488492,-6.73647519952897,
12.1661110906938));
#50741=CARTESIAN_POINT('Ctrl Pts',(-0.493366904661608,-6.7489908947475,
12.174152623387));
#50742=CARTESIAN_POINT('Ctrl Pts',(-0.318867574845682,-6.76174720092118,
12.1823487524352));
#50743=CARTESIAN_POINT('Ctrl Pts',(-0.143795398482077,-6.76773682818488,
12.1905448814834));
#50744=CARTESIAN_POINT('Ctrl Pts',(0.031273837992906,-6.76692773325216,
12.1987410105317));
#50745=CARTESIAN_POINT('Ctrl Pts',(0.20298160555235,-6.76613417358721,12.2067797673678));
#50746=CARTESIAN_POINT('Ctrl Pts',(0.374686158268147,-6.75880063125281,
12.2148185242039));
#50747=CARTESIAN_POINT('Ctrl Pts',(0.545843502883641,-6.74494950836251,
12.22285728104));
#50748=CARTESIAN_POINT('Ctrl Pts',(0.717017413721061,-6.73109704482992,
12.2308968159428));
#50749=CARTESIAN_POINT('Ctrl Pts',(0.887643638714671,-6.71072577466029,
12.2389363508456));
#50750=CARTESIAN_POINT('Ctrl Pts',(1.05718291976407,-6.68391002887974,12.2469758857484));
#50751=CARTESIAN_POINT('Ctrl Pts',(1.22677217926078,-6.6570863780914,12.2550177906239));
#50752=CARTESIAN_POINT('Ctrl Pts',(1.39527348834118,-6.62381452857332,12.2630596954994));
#50753=CARTESIAN_POINT('Ctrl Pts',(1.56215754477672,-6.58421998457655,12.2711016003749));
#50754=CARTESIAN_POINT('Ctrl Pts',(1.73467098131165,-6.54328982624501,12.2794147770557));
#50755=CARTESIAN_POINT('Ctrl Pts',(1.90545572464091,-6.49560305495819,12.2877279537366));
#50756=CARTESIAN_POINT('Ctrl Pts',(2.07394491517358,-6.44135401051873,12.2960411304174));
#50757=CARTESIAN_POINT('Ctrl Pts',(2.23721903586767,-6.38878408006001,12.3040969980279));
#50758=CARTESIAN_POINT('Ctrl Pts',(2.39833726918149,-6.33005224939568,12.3121528656384));
#50759=CARTESIAN_POINT('Ctrl Pts',(2.55680537338761,-6.26538388948485,12.320208733249));
#50760=CARTESIAN_POINT('Ctrl Pts',(2.72286582193264,-6.1976172123528,12.328650564465));
#50761=CARTESIAN_POINT('Ctrl Pts',(2.88601551180843,-6.12333136418268,12.337092395681));
#50762=CARTESIAN_POINT('Ctrl Pts',(3.0457166531056,-6.04283865985145,12.3455342268969));
#50763=CARTESIAN_POINT('Ctrl Pts',(3.2054177944027,-5.96234595552025,12.3539760581129));
#50764=CARTESIAN_POINT('Ctrl Pts',(3.36167002544971,-5.87564669358153,12.3624178893289));
#50765=CARTESIAN_POINT('Ctrl Pts',(3.5139728457726,-5.78310330524822,12.3708597205448));
#50766=CARTESIAN_POINT('Ctrl Pts',(3.66246215329503,-5.69287711232376,12.3790901766114));
#50767=CARTESIAN_POINT('Ctrl Pts',(3.80769153283813,-5.59679618283451,12.387320632678));
#50768=CARTESIAN_POINT('Ctrl Pts',(3.94916801048369,-5.49512156598671,12.3955510887446));
#50769=CARTESIAN_POINT('Ctrl Pts',(4.09047654721358,-5.39356764290044,12.4037717747748));
#50770=CARTESIAN_POINT('Ctrl Pts',(4.22804076450014,-5.28643346142516,12.411992460805));
#50771=CARTESIAN_POINT('Ctrl Pts',(4.36139318572993,-5.17402536517444,12.4202131468352));
#50772=CARTESIAN_POINT('Ctrl Pts',(4.49461406439839,-5.06172815141659,12.4284257237506));
#50773=CARTESIAN_POINT('Ctrl Pts',(4.62363114867729,-4.94416761276181,12.436638300666));
#50774=CARTESIAN_POINT('Ctrl Pts',(4.74800674596515,-4.82169274635677,12.4448508775814));
#50775=CARTESIAN_POINT('Ctrl Pts',(4.87228460030948,-4.69931412916951,12.453057000486));
#50776=CARTESIAN_POINT('Ctrl Pts',(4.99192797856486,-4.57202912693668,12.4612631233907));
#50777=CARTESIAN_POINT('Ctrl Pts',(5.1065329780435,-4.44022633929332,12.4694692462953));
#50778=CARTESIAN_POINT('Ctrl Pts',(5.22107089213271,-4.30850070396773,12.4776705656491));
#50779=CARTESIAN_POINT('Ctrl Pts',(5.3305760681249,-4.17226282128462,12.4858718850028));
#50780=CARTESIAN_POINT('Ctrl Pts',(5.43468207912903,-4.03193746216305,12.4940732043565));
#50781=CARTESIAN_POINT('Ctrl Pts',(5.53875822458536,-3.89165235906205,12.502272170946));
#50782=CARTESIAN_POINT('Ctrl Pts',(5.63743807373739,-3.74728240041451,12.5104711375355));
#50783=CARTESIAN_POINT('Ctrl Pts',(5.73039591163477,-3.59928488674063,12.5186701041251));
#50784=CARTESIAN_POINT('Ctrl Pts',(5.82334147402965,-3.45130691680714,12.526867988004));
#50785=CARTESIAN_POINT('Ctrl Pts',(5.91056633870804,-3.29970264905851,12.535065871883));
#50786=CARTESIAN_POINT('Ctrl Pts',(5.99178851202737,-3.14495777827571,12.5432637557619));
#50787=CARTESIAN_POINT('Ctrl Pts',(6.07301471383325,-2.99020523240117,12.5514620462424));
#50788=CARTESIAN_POINT('Ctrl Pts',(6.14823746442675,-2.83231209069919,12.559660336723));
#50789=CARTESIAN_POINT('Ctrl Pts',(6.21722104690627,-2.67178806305923,12.5678586272035));
#50790=CARTESIAN_POINT('Ctrl Pts',(6.28622058189078,-2.51122691411791,12.5760588135448));
#50791=CARTESIAN_POINT('Ctrl Pts',(6.34897793354415,-2.34803399690603,12.5842589998862));
#50792=CARTESIAN_POINT('Ctrl Pts',(6.40530576726585,-2.1827384240515,12.5924591862275));
#50793=CARTESIAN_POINT('Ctrl Pts',(6.46168685453462,-2.01728657720262,12.6006671252016));
#50794=CARTESIAN_POINT('Ctrl Pts',(6.51162616367455,-1.84972844299934,12.6088750641757));
#50795=CARTESIAN_POINT('Ctrl Pts',(6.55498617095785,-1.68060860956719,12.6170830031498));
#50796=CARTESIAN_POINT('Ctrl Pts',(6.59836721349436,-1.51140673098,12.6252949240438));
#50797=CARTESIAN_POINT('Ctrl Pts',(6.63516251493869,-1.3406419929803,12.6335068449378));
#50798=CARTESIAN_POINT('Ctrl Pts',(6.66528585000365,-1.16886848607579,12.6417187658317));
#50799=CARTESIAN_POINT('Ctrl Pts',(6.69545049445055,-0.996859419018739,
12.6499419480743));
#50800=CARTESIAN_POINT('Ctrl Pts',(6.71892483917329,-0.823839173858465,
12.6581651303169));
#50801=CARTESIAN_POINT('Ctrl Pts',(6.73567451233863,-0.650367483682722,
12.6663883125594));
#50802=CARTESIAN_POINT('Ctrl Pts',(6.75061099370125,-0.495674514949851,
12.6737213158422));
#50803=CARTESIAN_POINT('Ctrl Pts',(6.76020064985613,-0.340622766822271,
12.681054319125));
#50804=CARTESIAN_POINT('Ctrl Pts',(6.76445405791795,-0.18560791555702,12.6883873224078));
#50805=CARTESIAN_POINT('Ctrl Pts',(6.76963679056211,0.00327603780625371,
12.6973225091901));
#50806=CARTESIAN_POINT('Ctrl Pts',(6.76690717688361,0.192497154869291,12.7062576959724));
#50807=CARTESIAN_POINT('Ctrl Pts',(6.75624313107965,0.381402351512242,12.7151928827547));
#50808=CARTESIAN_POINT('Ctrl Pts',(6.74559505671733,0.570024626609443,12.7241146873913));
#50809=CARTESIAN_POINT('Ctrl Pts',(6.72703627610263,0.758331668059542,12.7330364920279));
#50810=CARTESIAN_POINT('Ctrl Pts',(6.70059667928441,0.945670736336247,12.7419582966646));
#50811=CARTESIAN_POINT('Ctrl Pts',(6.67422157491306,1.13255284019742,12.7508583389038));
#50812=CARTESIAN_POINT('Ctrl Pts',(6.64000405656431,1.31847142794225,12.7597583811431));
#50813=CARTESIAN_POINT('Ctrl Pts',(6.59802559765879,1.50277982839781,12.7686584233824));
#50814=CARTESIAN_POINT('Ctrl Pts',(6.55611176520797,1.686804483361,12.7775447638758));
#50815=CARTESIAN_POINT('Ctrl Pts',(6.50646088260922,1.86922364518446,12.7864311043692));
#50816=CARTESIAN_POINT('Ctrl Pts',(6.44920564933973,2.04939881246294,12.7953174448626));
#50817=CARTESIAN_POINT('Ctrl Pts',(6.39209680770747,2.22911330328934,12.8041810645345));
#50818=CARTESIAN_POINT('Ctrl Pts',(6.32742249070003,2.40659500294075,12.8130446842065));
#50819=CARTESIAN_POINT('Ctrl Pts',(6.25536536056838,2.58121932539667,12.8219083038784));
#50820=CARTESIAN_POINT('Ctrl Pts',(6.18696120988939,2.74699096303567,12.8303225770321));
#50821=CARTESIAN_POINT('Ctrl Pts',(6.11190422848109,2.91018747026337,12.8387368501858));
#50822=CARTESIAN_POINT('Ctrl Pts',(6.03039281295544,3.07028525082857,12.8471511233395));
#50823=CARTESIAN_POINT('Ctrl Pts',(5.9508578441299,3.22650106310683,12.855361371544));
#50824=CARTESIAN_POINT('Ctrl Pts',(5.8652531850374,3.37961600469497,12.8635716197486));
#50825=CARTESIAN_POINT('Ctrl Pts',(5.77385985034016,3.5291403243042,12.8717818679531));
#50826=CARTESIAN_POINT('Ctrl Pts',(5.68244478962528,3.67870018882505,12.8799940678974));
#50827=CARTESIAN_POINT('Ctrl Pts',(5.58523849739068,3.82466742711152,12.8882062678416));
#50828=CARTESIAN_POINT('Ctrl Pts',(5.48256582694271,3.96658051137752,12.8964184677858));
#50829=CARTESIAN_POINT('Ctrl Pts',(5.37985046602956,4.1085526019551,12.9046340822963));
#50830=CARTESIAN_POINT('Ctrl Pts',(5.27166440730891,4.24646689211029,12.9128496968067));
#50831=CARTESIAN_POINT('Ctrl Pts',(5.15837339904699,4.37989416264874,12.9210653113172));
#50832=CARTESIAN_POINT('Ctrl Pts',(5.04495516994897,4.51347126616313,12.9292901516026));
#50833=CARTESIAN_POINT('Ctrl Pts',(4.92642077185495,4.64255101465771,12.9375149918881));
#50834=CARTESIAN_POINT('Ctrl Pts',(4.80317416396026,4.7667396562708,12.9457398321735));
#50835=CARTESIAN_POINT('Ctrl Pts',(4.67984861232892,4.89100784502589,12.9539699407551));
#50836=CARTESIAN_POINT('Ctrl Pts',(4.55180509367817,5.01037843947844,12.9622000493366));
#50837=CARTESIAN_POINT('Ctrl Pts',(4.41948133383884,5.12449741339091,12.9704301579182));
#50838=CARTESIAN_POINT('Ctrl Pts',(4.28697615609421,5.23877284616782,12.9786715501049));
#50839=CARTESIAN_POINT('Ctrl Pts',(4.1501792934497,5.34778205588775,12.9869129422916));
#50840=CARTESIAN_POINT('Ctrl Pts',(4.00955897379088,5.451213244379,12.9951543344783));
#50841=CARTESIAN_POINT('Ctrl Pts',(3.94835743801168,5.49622912543012,12.9987411977425));
#50842=CARTESIAN_POINT('Ctrl Pts',(3.88643199844304,5.54018898684203,13.0023280610067));
#50843=CARTESIAN_POINT('Ctrl Pts',(3.82382272336396,5.58306983480284,13.0059149242709));
#50844=CARTESIAN_POINT('Ctrl Pts',(3.67635322098209,5.68407112099415,13.0143633999962));
#50845=CARTESIAN_POINT('Ctrl Pts',(3.52475190117989,5.77931344038154,13.0228118757215));
#50846=CARTESIAN_POINT('Ctrl Pts',(3.36949632418923,5.86845665582317,13.0312603514468));
#50847=CARTESIAN_POINT('Ctrl Pts',(3.28052731169263,5.91954006295315,13.0361017398011));
#50848=CARTESIAN_POINT('Ctrl Pts',(3.19035890213008,5.96862135863634,13.0409431281554));
#50849=CARTESIAN_POINT('Ctrl Pts',(3.09908550384717,6.01564277861014,13.0457845165097));
#50850=CARTESIAN_POINT('Ctrl Pts',(3.09908550384726,6.0156427786101,11.0457658645337));
#50851=CARTESIAN_POINT('Ctrl Pts',(2.9397938181652,6.09770525674393,11.0542002828111));
#50852=CARTESIAN_POINT('Ctrl Pts',(2.77731417815122,6.17339906158248,11.0626347010885));
#50853=CARTESIAN_POINT('Ctrl Pts',(2.61218824820048,6.24249642018026,11.0710691193659));
#50854=CARTESIAN_POINT('Ctrl Pts',(2.44692139132781,6.31165275000117,11.0795107360077));
#50855=CARTESIAN_POINT('Ctrl Pts',(2.27900404382807,6.37420126766874,11.0879523526494));
#50856=CARTESIAN_POINT('Ctrl Pts',(2.10899567926727,6.42996315890161,11.0963939692912));
#50857=CARTESIAN_POINT('Ctrl Pts',(2.07975780109613,6.43955303635659,11.0978457505584));
#50858=CARTESIAN_POINT('Ctrl Pts',(2.05045810985601,6.44894230753634,11.0992975318256));
#50859=CARTESIAN_POINT('Ctrl Pts',(2.02109948945974,6.45813021343683,11.1007493130928));
#50860=CARTESIAN_POINT('Ctrl Pts',(1.85646083827064,6.50965458393826,11.1088906803107));
#50861=CARTESIAN_POINT('Ctrl Pts',(1.68964079039257,6.55494474398137,11.1170320475285));
#50862=CARTESIAN_POINT('Ctrl Pts',(1.52115681601926,6.59381308053831,11.1251734147464));
#50863=CARTESIAN_POINT('Ctrl Pts',(1.35281991534155,6.63264748799358,11.1333076751698));
#50864=CARTESIAN_POINT('Ctrl Pts',(1.18282233360269,6.66507114858489,11.1414419355933));
#50865=CARTESIAN_POINT('Ctrl Pts',(1.01169785243365,6.69094585655729,11.1495761960168));
#50866=CARTESIAN_POINT('Ctrl Pts',(0.84069010620479,6.71680291373848,11.1577049075416));
#50867=CARTESIAN_POINT('Ctrl Pts',(0.668557351521036,6.73611985836785,11.1658336190664));
#50868=CARTESIAN_POINT('Ctrl Pts',(0.49584471001288,6.74880930413301,11.1739623305912));
#50869=CARTESIAN_POINT('Ctrl Pts',(0.323214431971352,6.76149269853601,11.1820871656837));
#50870=CARTESIAN_POINT('Ctrl Pts',(0.150005182080456,6.76755486103975,11.1902120007762));
#50871=CARTESIAN_POINT('Ctrl Pts',(-0.0232316446019987,6.76696012184859,
11.1983368358687));
#50872=CARTESIAN_POINT('Ctrl Pts',(-0.196419973149235,6.76636554915634,
11.2064593963909));
#50873=CARTESIAN_POINT('Ctrl Pts',(-0.369635497385828,6.75911778882147,
11.214581956913));
#50874=CARTESIAN_POINT('Ctrl Pts',(-0.542325694487193,6.74523326810119,
11.2227045174352));
#50875=CARTESIAN_POINT('Ctrl Pts',(-0.715025069624446,6.73134800945465,
11.2308275096504));
#50876=CARTESIAN_POINT('Ctrl Pts',(-0.887198696654032,6.71082531120946,
11.2389505018656));
#50877=CARTESIAN_POINT('Ctrl Pts',(-1.05829785887319,6.68373358549729,11.2470734940807));
#50878=CARTESIAN_POINT('Ctrl Pts',(-1.1456387670123,6.66990408512997,11.2512200340619));
#50879=CARTESIAN_POINT('Ctrl Pts',(-1.23269978871727,6.65436366597106,11.255366574043));
#50880=CARTESIAN_POINT('Ctrl Pts',(-1.31940879331736,6.63712659485389,11.2595131140241));
#50881=CARTESIAN_POINT('Ctrl Pts',(-1.50726761912444,6.59978173136066,11.2684967730525));
#50882=CARTESIAN_POINT('Ctrl Pts',(-1.69338053795594,6.55448856373644,11.2774804320809));
#50883=CARTESIAN_POINT('Ctrl Pts',(-1.87710627446768,6.50144299631659,11.2864640911093));
#50884=CARTESIAN_POINT('Ctrl Pts',(-2.0611476498483,6.4483062971739,11.2954631839687));
#50885=CARTESIAN_POINT('Ctrl Pts',(-2.2427934160623,6.38739064456191,11.3044622768281));
#50886=CARTESIAN_POINT('Ctrl Pts',(-2.42141934168466,6.31894115906419,11.3134613696876));
#50887=CARTESIAN_POINT('Ctrl Pts',(-2.60046409518568,6.25033117865115,11.322481562905));
#50888=CARTESIAN_POINT('Ctrl Pts',(-2.7764746166958,6.17415210727052,11.3315017561224));
#50889=CARTESIAN_POINT('Ctrl Pts',(-2.94884595015438,6.09069754316024,11.3405219493398));
#50890=CARTESIAN_POINT('Ctrl Pts',(-3.12139185275069,6.00715846040637,11.3495512777615));
#50891=CARTESIAN_POINT('Ctrl Pts',(-3.2902909919746,5.91632927451426,11.3585806061832));
#50892=CARTESIAN_POINT('Ctrl Pts',(-3.45496337058348,5.81854939894184,11.3676099346049));
#50893=CARTESIAN_POINT('Ctrl Pts',(-3.61986790405356,5.72063167345413,11.3766519925597));
#50894=CARTESIAN_POINT('Ctrl Pts',(-3.78053355632665,5.61574378709345,11.3856940505145));
#50895=CARTESIAN_POINT('Ctrl Pts',(-3.93640770303687,5.50426956057495,11.3947361084692));
#50896=CARTESIAN_POINT('Ctrl Pts',(-4.07167938353012,5.40752929754162,11.4025830439648));
#50897=CARTESIAN_POINT('Ctrl Pts',(-4.20334286747106,5.30582944319444,11.4104299794603));
#50898=CARTESIAN_POINT('Ctrl Pts',(-4.33105680174991,5.19944573777012,11.4182769149559));
#50899=CARTESIAN_POINT('Ctrl Pts',(-4.47189751232059,5.08212763344809,11.4269303792567));
#50900=CARTESIAN_POINT('Ctrl Pts',(-4.60805834060706,4.95900892120961,11.4355838435575));
#50901=CARTESIAN_POINT('Ctrl Pts',(-4.73906523145384,4.83048131473721,11.4442373078582));
#50902=CARTESIAN_POINT('Ctrl Pts',(-4.86995143815756,4.70207210847984,11.4528828005484));
#50903=CARTESIAN_POINT('Ctrl Pts',(-4.99569296083439,4.56826415827005,11.4615282932386));
#50904=CARTESIAN_POINT('Ctrl Pts',(-5.11585029001451,4.42948809798135,11.4701737859288));
#50905=CARTESIAN_POINT('Ctrl Pts',(-5.23962234617609,4.28653719814747,11.4790793634253));
#50906=CARTESIAN_POINT('Ctrl Pts',(-5.35746872426019,4.13831480601132,11.4879849409218));
#50907=CARTESIAN_POINT('Ctrl Pts',(-5.46894983688847,3.98533269396642,11.4968905184184));
#50908=CARTESIAN_POINT('Ctrl Pts',(-5.57696982220859,3.83710018078338,11.5055196065909));
#50909=CARTESIAN_POINT('Ctrl Pts',(-5.67901364914984,3.68439932452288,11.5141486947635));
#50910=CARTESIAN_POINT('Ctrl Pts',(-5.77472180219839,3.52772973840324,11.522777782936));
#50911=CARTESIAN_POINT('Ctrl Pts',(-5.87502991100254,3.3635302487023,11.5318216050946));
#50912=CARTESIAN_POINT('Ctrl Pts',(-5.96837809447859,3.19497138617176,11.5408654272531));
#50913=CARTESIAN_POINT('Ctrl Pts',(-6.05440284903171,3.02266358393333,11.5499092494116));
#50914=CARTESIAN_POINT('Ctrl Pts',(-6.14042760358484,2.8503557816949,11.5589530715702));
#50915=CARTESIAN_POINT('Ctrl Pts',(-6.2191287261133,2.67429936902006,11.5679968937287));
#50916=CARTESIAN_POINT('Ctrl Pts',(-6.29019749782052,2.49513615628736,11.5770407158872));
#50917=CARTESIAN_POINT('Ctrl Pts',(-6.35419382912098,2.33380245030844,11.5851845380637));
#50918=CARTESIAN_POINT('Ctrl Pts',(-6.41198934629365,2.16997942501787,11.5933283602401));
#50919=CARTESIAN_POINT('Ctrl Pts',(-6.46339792467016,2.00418967849092,11.6014721824165));
#50920=CARTESIAN_POINT('Ctrl Pts',(-6.51482563647354,1.8383382277486,11.6096190355895));
#50921=CARTESIAN_POINT('Ctrl Pts',(-6.55986154742279,1.67051894024127,11.6177658887625));
#50922=CARTESIAN_POINT('Ctrl Pts',(-6.59836929786719,1.50126999868901,11.6259127419355));
#50923=CARTESIAN_POINT('Ctrl Pts',(-6.63688350849126,1.33199266340928,11.6340609618499));
#50924=CARTESIAN_POINT('Ctrl Pts',(-6.66886730313274,1.16128555336923,11.6422091817643));
#50925=CARTESIAN_POINT('Ctrl Pts',(-6.694235521968,0.989696810352488,11.6503574016787));
#50926=CARTESIAN_POINT('Ctrl Pts',(-6.71962615788893,0.817956439837697,
11.658512821915));
#50927=CARTESIAN_POINT('Ctrl Pts',(-6.73838949092252,0.64533324160695,11.6666682421514));
#50928=CARTESIAN_POINT('Ctrl Pts',(-6.75049221241431,0.472381085707059,
11.6748236623878));
#50929=CARTESIAN_POINT('Ctrl Pts',(-6.76155111160754,0.314345518364135,
11.682275702851));
#50930=CARTESIAN_POINT('Ctrl Pts',(-6.76704938032223,0.156035544008866,
11.6897277433143));
#50931=CARTESIAN_POINT('Ctrl Pts',(-6.76699966570739,-0.00212704398872441,
11.6971797837775));
#50932=CARTESIAN_POINT('',(-6.767,2.82623737238828E-12,11.3028202161898));
#50933=CARTESIAN_POINT('Ctrl Pts',(3.09908550384714,6.01564277861016,10.6513967904261));
#50934=CARTESIAN_POINT('Ctrl Pts',(2.93373232018321,6.10082796552484,10.6601462383254));
#50935=CARTESIAN_POINT('Ctrl Pts',(2.76486502144417,6.17919158180194,10.6688956862247));
#50936=CARTESIAN_POINT('Ctrl Pts',(2.59305716434341,6.25046746591383,10.6776451341239));
#50937=CARTESIAN_POINT('Ctrl Pts',(2.4212506945927,6.32174277447229,10.6863945113714));
#50938=CARTESIAN_POINT('Ctrl Pts',(2.24650397871044,6.38593035557831,10.6951438886188));
#50939=CARTESIAN_POINT('Ctrl Pts',(2.06941053323755,6.44281220003544,10.7038932658662));
#50940=CARTESIAN_POINT('Ctrl Pts',(1.89231845896654,6.49969360406694,10.7126425753688));
#50941=CARTESIAN_POINT('Ctrl Pts',(1.71287996431462,6.54926929700892,10.7213918848714));
#50942=CARTESIAN_POINT('Ctrl Pts',(1.53170449173448,6.59137090065492,10.730141194374));
#50943=CARTESIAN_POINT('Ctrl Pts',(1.35053036178113,6.63347219230095,10.7388904390386));
#50944=CARTESIAN_POINT('Ctrl Pts',(1.16761955878787,6.66809944062464,10.7476396837032));
#50945=CARTESIAN_POINT('Ctrl Pts',(0.983593309309904,6.695135039854,10.7563889283678));
#50946=CARTESIAN_POINT('Ctrl Pts',(0.799568362459278,6.72217044771223,10.765138111101));
#50947=CARTESIAN_POINT('Ctrl Pts',(0.614428268437771,6.74161427235985,10.7738872938342));
#50948=CARTESIAN_POINT('Ctrl Pts',(0.428801816329323,6.75340047696808,10.7826364765673));
#50949=CARTESIAN_POINT('Ctrl Pts',(0.243176616522011,6.76518660206244,10.7913856002755));
#50950=CARTESIAN_POINT('Ctrl Pts',(0.0570653511648604,6.76931519233997,
10.8001347239836));
#50951=CARTESIAN_POINT('Ctrl Pts',(-0.128899900800456,6.76577222610794,
10.8088838476917));
#50952=CARTESIAN_POINT('Ctrl Pts',(-0.314863959942527,6.76222928260131,
10.817632915281));
#50953=CARTESIAN_POINT('Ctrl Pts',(-0.500681721081265,6.75101488651272,
10.8263819828702));
#50954=CARTESIAN_POINT('Ctrl Pts',(-0.68572211017396,6.73216712415984,10.8351310504595));
#50955=CARTESIAN_POINT('Ctrl Pts',(-0.870761373828175,6.71331947644137,
10.8438800648359));
#50956=CARTESIAN_POINT('Ctrl Pts',(-1.05502298984389,6.68683858439989,10.8526290792122));
#50957=CARTESIAN_POINT('Ctrl Pts',(-1.23788117676096,6.65281438131419,10.8613780935886));
#50958=CARTESIAN_POINT('Ctrl Pts',(-1.43009641451827,6.6170491230237,10.8705748044761));
#50959=CARTESIAN_POINT('Ctrl Pts',(-1.62076048992727,6.57294837083157,10.8797715153636));
#50960=CARTESIAN_POINT('Ctrl Pts',(-1.8091579896116,6.52067760042041,10.8889682262511));
#50961=CARTESIAN_POINT('Ctrl Pts',(-1.98840443003043,6.47094578577399,10.8977182239576));
#50962=CARTESIAN_POINT('Ctrl Pts',(-2.16559895952225,6.41381888474464,10.9064682216642));
#50963=CARTESIAN_POINT('Ctrl Pts',(-2.34013966242358,6.34949095285221,10.9152182193707));
#50964=CARTESIAN_POINT('Ctrl Pts',(-2.51467682554045,6.28516432556673,10.9239680396223));
#50965=CARTESIAN_POINT('Ctrl Pts',(-2.68656000078867,6.2136370587965,10.9327178598739));
#50966=CARTESIAN_POINT('Ctrl Pts',(-2.85520533840907,6.1351521151085,10.9414676801255));
#50967=CARTESIAN_POINT('Ctrl Pts',(-3.02384747998342,6.05666865881114,10.9502173345567));
#50968=CARTESIAN_POINT('Ctrl Pts',(-3.18925164684548,5.97122791039838,10.9589669889879));
#50969=CARTESIAN_POINT('Ctrl Pts',(-3.35085601829165,5.87912008251904,10.9677166434192));
#50970=CARTESIAN_POINT('Ctrl Pts',(-3.51245754191425,5.7870138777817,10.9764661436623));
#50971=CARTESIAN_POINT('Ctrl Pts',(-3.67025915510942,5.68824097060979,10.9852156439055));
#50972=CARTESIAN_POINT('Ctrl Pts',(-3.8237248792884,5.58313684656851,10.9939651441486));
#50973=CARTESIAN_POINT('Ctrl Pts',(-3.97718810300802,5.4780344350177,11.0027145018337));
#50974=CARTESIAN_POINT('Ctrl Pts',(-4.12631534263029,5.36660117496373,11.0114638595188));
#50975=CARTESIAN_POINT('Ctrl Pts',(-4.27060009886228,5.24921554097348,11.020213217204));
#50976=CARTESIAN_POINT('Ctrl Pts',(-4.41488269594226,5.13183166360281,11.0289624439591));
#50977=CARTESIAN_POINT('Ctrl Pts',(-4.5543227323511,5.00849577139452,11.0377116707143));
#50978=CARTESIAN_POINT('Ctrl Pts',(-4.68844662480237,4.87962675277313,11.0464608974695));
#50979=CARTESIAN_POINT('Ctrl Pts',(-4.82256868835201,4.75075949139838,11.055210004921));
#50980=CARTESIAN_POINT('Ctrl Pts',(-4.95137454637918,4.61635945312466,11.0639591123725));
#50981=CARTESIAN_POINT('Ctrl Pts',(-5.07442674461144,4.47688309134515,11.072708219824));
#50982=CARTESIAN_POINT('Ctrl Pts',(-5.19747742838585,4.33740844616295,11.0814572195964));
#50983=CARTESIAN_POINT('Ctrl Pts',(-5.31477440450955,4.19285781735993,11.0902062193687));
#50984=CARTESIAN_POINT('Ctrl Pts',(-5.42591931531163,4.04372211999392,11.0989552191411));
#50985=CARTESIAN_POINT('Ctrl Pts',(-5.53707636462999,3.89457013500777,11.1077051744217));
#50986=CARTESIAN_POINT('Ctrl Pts',(-5.64207983273493,3.74083230916387,11.1164551297023));
#50987=CARTESIAN_POINT('Ctrl Pts',(-5.74057303468775,3.58303087251783,11.1252050849829));
#50988=CARTESIAN_POINT('Ctrl Pts',(-5.83906243363789,3.42523552887389,11.1339547024117));
#50989=CARTESIAN_POINT('Ctrl Pts',(-5.93104191768447,3.26337713156954,11.1427043198405));
#50990=CARTESIAN_POINT('Ctrl Pts',(-6.01619906699674,3.0980054529112,11.1514539372693));
#50991=CARTESIAN_POINT('Ctrl Pts',(-6.10135338095403,2.93263928039554,11.1602032633747));
#50992=CARTESIAN_POINT('Ctrl Pts',(-6.1796856835286,2.76376031540178,11.16895258948));
#50993=CARTESIAN_POINT('Ctrl Pts',(-6.25092992694908,2.59194213831491,11.1777019155854));
#50994=CARTESIAN_POINT('Ctrl Pts',(-6.32217217691122,2.42012876880772,11.1864509968792));
#50995=CARTESIAN_POINT('Ctrl Pts',(-6.38632665483866,2.24537661647625,11.195200078173));
#50996=CARTESIAN_POINT('Ctrl Pts',(-6.44317547869363,2.06827917621415,11.2039491594668));
#50997=CARTESIAN_POINT('Ctrl Pts',(-6.50002944235945,1.89116572423393,11.2126990317818));
#50998=CARTESIAN_POINT('Ctrl Pts',(-6.54957634250403,1.71170683289178,11.2214489040967));
#50999=CARTESIAN_POINT('Ctrl Pts',(-6.59164787708397,1.53051209225356,11.2301987764117));
#51000=CARTESIAN_POINT('Ctrl Pts',(-6.63371649075016,1.34932993147997,11.2389480412465));
#51001=CARTESIAN_POINT('Ctrl Pts',(-6.66831071257135,1.16641244173945,11.2476973060813));
#51002=CARTESIAN_POINT('Ctrl Pts',(-6.69531304840345,0.982380875159165,
11.2564465709161));
#51003=CARTESIAN_POINT('Ctrl Pts',(-6.72231677033054,0.79833986179499,11.2651962848718));
#51004=CARTESIAN_POINT('Ctrl Pts',(-6.74172778477898,0.613184940729295,
11.2739459988274));
#51005=CARTESIAN_POINT('Ctrl Pts',(-6.75348015835523,0.427545027689691,
11.2826957127831));
#51006=CARTESIAN_POINT('Ctrl Pts',(-6.76249038365217,0.285219953547213,
11.2894038805853));
#51007=CARTESIAN_POINT('Ctrl Pts',(-6.76699999999994,0.142609995758956,
11.2961120483876));
#51008=CARTESIAN_POINT('Ctrl Pts',(-6.767,2.82623743936056E-12,11.3028202161898));
#51009=CARTESIAN_POINT('Ctrl Pts',(-6.76699999572935,-0.000240414293744514,
11.3028202161898));
#51010=CARTESIAN_POINT('Ctrl Pts',(-6.76699367167169,-0.178245213700239,
11.3111542497933));
#51011=CARTESIAN_POINT('Ctrl Pts',(-6.75995944046259,-0.35617527161172,
11.3194882833967));
#51012=CARTESIAN_POINT('Ctrl Pts',(-6.74594087271596,-0.533451723982817,
11.3278223170002));
#51013=CARTESIAN_POINT('Ctrl Pts',(-6.73191375254288,-0.710836328901932,
11.3361614350182));
#51014=CARTESIAN_POINT('Ctrl Pts',(-6.7108938272577,-0.887566193870075,
11.3445005530362));
#51015=CARTESIAN_POINT('Ctrl Pts',(-6.68297634044918,-1.06306925127034,
11.3528396710542));
#51016=CARTESIAN_POINT('Ctrl Pts',(-6.65501988782158,-1.23881726698042,
11.3611904283922));
#51017=CARTESIAN_POINT('Ctrl Pts',(-6.62014669057205,-1.41333471678057,
11.3695411857303));
#51018=CARTESIAN_POINT('Ctrl Pts',(-6.57850306471982,-1.58606003274529,
11.3778919430683));
#51019=CARTESIAN_POINT('Ctrl Pts',(-6.53682765482578,-1.75891717941763,
11.3862490740305));
#51020=CARTESIAN_POINT('Ctrl Pts',(-6.48837160213316,-1.92997913682426,
11.3946062049927));
#51021=CARTESIAN_POINT('Ctrl Pts',(-6.43333069050316,-2.09870084257621,
11.4029633359549));
#51022=CARTESIAN_POINT('Ctrl Pts',(-6.378201535987,-2.26769304694154,11.4113338652664));
#51023=CARTESIAN_POINT('Ctrl Pts',(-6.31646654296931,-2.43433718232206,
11.4197043945778));
#51024=CARTESIAN_POINT('Ctrl Pts',(-6.24836964538579,-2.59810811449821,
11.4280749238893));
#51025=CARTESIAN_POINT('Ctrl Pts',(-6.20596974919273,-2.7000785532424,11.4332867556537));
#51026=CARTESIAN_POINT('Ctrl Pts',(-6.16110438861522,-2.80093556954357,
11.4384985874182));
#51027=CARTESIAN_POINT('Ctrl Pts',(-6.11384123733026,-2.9005575885888,11.4437104191826));
#51028=CARTESIAN_POINT('Ctrl Pts',(-6.03722662134645,-3.06204708992703,
11.4521589140111));
#51029=CARTESIAN_POINT('Ctrl Pts',(-5.95414346373569,-3.22063899955504,
11.4606074088395));
#51030=CARTESIAN_POINT('Ctrl Pts',(-5.86483330098463,-3.37579906861497,
11.4690559036679));
#51031=CARTESIAN_POINT('Ctrl Pts',(-5.77560471787926,-3.530817407965,11.477496681287));
#51032=CARTESIAN_POINT('Ctrl Pts',(-5.68016063310411,-3.68240986772118,
11.4859374589062));
#51033=CARTESIAN_POINT('Ctrl Pts',(-5.57878925840906,-3.83006519660693,
11.4943782365254));
#51034=CARTESIAN_POINT('Ctrl Pts',(-5.47749489183758,-3.97760835714293,
11.5028126019947));
#51035=CARTESIAN_POINT('Ctrl Pts',(-5.37028239968252,-4.12122007525554,
11.511246967464));
#51036=CARTESIAN_POINT('Ctrl Pts',(-5.25748441407456,-4.26041625146687,
11.5196813329333));
#51037=CARTESIAN_POINT('Ctrl Pts',(-5.1447547948415,-4.39952806147331,11.5281105863699));
#51038=CARTESIAN_POINT('Ctrl Pts',(-5.02644664106432,-4.53422940688327,
11.5365398398065));
#51039=CARTESIAN_POINT('Ctrl Pts',(-4.90293437746686,-4.66406726905323,
11.5449690932431));
#51040=CARTESIAN_POINT('Ctrl Pts',(-4.77947802770037,-4.79384635380248,
11.5533945307683));
#51041=CARTESIAN_POINT('Ctrl Pts',(-4.6508224952366,-4.9187661043324,11.5618199682935));
#51042=CARTESIAN_POINT('Ctrl Pts',(-4.51738101923936,-5.03840825330937,
11.5702454058187));
#51043=CARTESIAN_POINT('Ctrl Pts',(-4.38396885674569,-5.1580241201238,11.5786689925019));
#51044=CARTESIAN_POINT('Ctrl Pts',(-4.24577309316775,-5.272364472556,11.5870925791851));
#51045=CARTESIAN_POINT('Ctrl Pts',(-4.10324258783639,-5.38104908594651,
11.5955161658683));
#51046=CARTESIAN_POINT('Ctrl Pts',(-3.9607280309213,-5.48972153809861,11.6039388099963));
#51047=CARTESIAN_POINT('Ctrl Pts',(-3.81387996426694,-5.59273931070984,
11.6123614541243));
#51048=CARTESIAN_POINT('Ctrl Pts',(-3.66317921887819,-5.68976335275721,
11.6207840982523));
#51049=CARTESIAN_POINT('Ctrl Pts',(-3.51247432150342,-5.78679006793314,
11.6292069744342));
#51050=CARTESIAN_POINT('Ctrl Pts',(-3.35791681430515,-5.87782254315894,
11.6376298506161));
#51051=CARTESIAN_POINT('Ctrl Pts',(-3.20001561816885,-5.9625656426974,11.6460527267981));
#51052=CARTESIAN_POINT('Ctrl Pts',(-3.04208805165652,-6.04732289480376,
11.6544770096471));
#51053=CARTESIAN_POINT('Ctrl Pts',(-2.88081597690753,-6.12578852000872,
11.6629012924961));
#51054=CARTESIAN_POINT('Ctrl Pts',(-2.71673228491875,-6.19771366651285,
11.6713255753451));
#51055=CARTESIAN_POINT('Ctrl Pts',(-2.55253777687123,-6.26968738860157,
11.6797555476432));
#51056=CARTESIAN_POINT('Ctrl Pts',(-2.38552816289065,-6.33511167145496,
11.6881855199414));
#51057=CARTESIAN_POINT('Ctrl Pts',(-2.21625659696054,-6.39378570929844,
11.6966154922395));
#51058=CARTESIAN_POINT('Ctrl Pts',(-2.04692451917771,-6.45248072216342,
11.7050484781167));
#51059=CARTESIAN_POINT('Ctrl Pts',(-1.87532919410823,-6.50442057503272,
11.7134814639939));
#51060=CARTESIAN_POINT('Ctrl Pts',(-1.70203880756469,-6.54945439693596,
11.7219144498711));
#51061=CARTESIAN_POINT('Ctrl Pts',(-1.52858899492133,-6.59452964968097,
11.7303551940439));
#51062=CARTESIAN_POINT('Ctrl Pts',(-1.35344132944133,-6.63268609947081,
11.7387959382167));
#51063=CARTESIAN_POINT('Ctrl Pts',(-1.17717513952058,-6.66382380401033,
11.7472366823896));
#51064=CARTESIAN_POINT('Ctrl Pts',(-1.07971285546168,-6.68104067246444,
11.751903795275));
#51065=CARTESIAN_POINT('Ctrl Pts',(-0.981908748035641,-6.69611262843616,
11.7565709081603));
#51066=CARTESIAN_POINT('Ctrl Pts',(-0.883861440877113,-6.70902958357844,
11.7612380210457));
#51067=CARTESIAN_POINT('Ctrl Pts',(-0.712826552306661,-6.73156207373501,
11.7693793882636));
#51068=CARTESIAN_POINT('Ctrl Pts',(-0.540711485736337,-6.74757865359124,
11.7775207554814));
#51069=CARTESIAN_POINT('Ctrl Pts',(-0.368058216269429,-6.75698321364176,
11.7856621226993));
#51070=CARTESIAN_POINT('Ctrl Pts',(-0.195555659975322,-6.76637956422664,
11.7937963831228));
#51071=CARTESIAN_POINT('Ctrl Pts',(-0.0225161989652834,-6.76917536405671,
11.8019306435463));
#51072=CARTESIAN_POINT('Ctrl Pts',(0.150510593120949,-6.76532597598655,
11.8100649039698));
#51073=CARTESIAN_POINT('Ctrl Pts',(0.323419352579259,-6.76147921382989,
11.8181936154946));
#51074=CARTESIAN_POINT('Ctrl Pts',(0.496315095855285,-6.75099629715473,
11.8263223270194));
#51075=CARTESIAN_POINT('Ctrl Pts',(0.668645790719264,-6.73388460003239,
11.8344510385443));
#51076=CARTESIAN_POINT('Ctrl Pts',(0.840894304259591,-6.71678106316218,
11.8425758736368));
#51077=CARTESIAN_POINT('Ctrl Pts',(1.01257794249337,-6.69305507688452,11.8507007087293));
#51078=CARTESIAN_POINT('Ctrl Pts',(1.18314735995491,-6.662766041565,11.8588255438218));
#51079=CARTESIAN_POINT('Ctrl Pts',(1.35366902602979,-6.63248548574584,11.866948104344));
#51080=CARTESIAN_POINT('Ctrl Pts',(1.52307673268356,-6.59564560527994,11.8750706648661));
#51081=CARTESIAN_POINT('Ctrl Pts',(1.69082895592043,-6.55235731945542,11.8831932253883));
#51082=CARTESIAN_POINT('Ctrl Pts',(1.85859009475282,-6.50906673297081,11.8913162176035));
#51083=CARTESIAN_POINT('Ctrl Pts',(2.02469521897243,-6.45932714415243,11.8994392098187));
#51084=CARTESIAN_POINT('Ctrl Pts',(2.18861546764281,-6.40330003473167,11.9075622020339));
#51085=CARTESIAN_POINT('Ctrl Pts',(2.27229175918843,-6.37469990277496,11.9117087420149));
#51086=CARTESIAN_POINT('Ctrl Pts',(2.3553989557734,-6.34446217793446,11.915855281996));
#51087=CARTESIAN_POINT('Ctrl Pts',(2.43786844108258,-6.31261328325865,11.9200018219771));
#51088=CARTESIAN_POINT('Ctrl Pts',(2.61654216414868,-6.24361126916906,11.9289854810055));
#51089=CARTESIAN_POINT('Ctrl Pts',(2.7921330226587,-6.167078008446,11.9379691400338));
#51090=CARTESIAN_POINT('Ctrl Pts',(2.96404282747277,-6.08331645707399,11.9469527990622));
#51091=CARTESIAN_POINT('Ctrl Pts',(3.13624797151036,-5.99941100424407,11.9559518919216));
#51092=CARTESIAN_POINT('Ctrl Pts',(3.30475920691669,-5.90825254518361,11.964950984781));
#51093=CARTESIAN_POINT('Ctrl Pts',(3.46900357466484,-5.81018960094785,11.9739500776404));
#51094=CARTESIAN_POINT('Ctrl Pts',(3.63363304955753,-5.71189672651141,11.9829702708578));
#51095=CARTESIAN_POINT('Ctrl Pts',(3.79397543317875,-5.60666709849133,11.9919904640751));
#51096=CARTESIAN_POINT('Ctrl Pts',(3.94948506837573,-5.49489369275486,12.0010106572925));
#51097=CARTESIAN_POINT('Ctrl Pts',(4.10515219601855,-5.3830070884566,12.0100399857142));
#51098=CARTESIAN_POINT('Ctrl Pts',(4.25597660700428,-5.26456361125743,12.0190693141359));
#51099=CARTESIAN_POINT('Ctrl Pts',(4.40144508884287,-5.13999709434753,12.0280986425576));
#51100=CARTESIAN_POINT('Ctrl Pts',(4.54711865191911,-5.01525496375737,12.0371407005124));
#51101=CARTESIAN_POINT('Ctrl Pts',(4.68742100623655,-4.8843726887987,12.0461827584671));
#51102=CARTESIAN_POINT('Ctrl Pts',(4.8218735208686,-4.74782315895888,12.0552248164218));
#51103=CARTESIAN_POINT('Ctrl Pts',(4.93855494613993,-4.62932188878596,12.0630717519175));
#51104=CARTESIAN_POINT('Ctrl Pts',(5.05083123888825,-4.50655313272352,12.0709186874131));
#51105=CARTESIAN_POINT('Ctrl Pts',(5.15841337933475,-4.37984707585782,12.0787656229088));
#51106=CARTESIAN_POINT('Ctrl Pts',(5.27705309700226,-4.24011783501058,12.0874190872096));
#51107=CARTESIAN_POINT('Ctrl Pts',(5.39008766652695,-4.09547629687063,12.0960725515104));
#51108=CARTESIAN_POINT('Ctrl Pts',(5.49711721599856,-3.94638965556777,12.1047260158113));
#51109=CARTESIAN_POINT('Ctrl Pts',(5.60404816936307,-3.79744035355602,12.1133715085014));
#51110=CARTESIAN_POINT('Ctrl Pts',(5.70498495941745,-3.64405436176327,12.1220170011916));
#51111=CARTESIAN_POINT('Ctrl Pts',(5.79956842159314,-3.4867312949609,12.1306624938818));
#51112=CARTESIAN_POINT('Ctrl Pts',(5.89699726486195,-3.32467543376197,12.1395680713784));
#51113=CARTESIAN_POINT('Ctrl Pts',(5.98768433488902,-3.15844215885032,12.1484736488749));
#51114=CARTESIAN_POINT('Ctrl Pts',(6.07128430232286,-2.98861103530855,12.1573792263714));
#51115=CARTESIAN_POINT('Ctrl Pts',(6.15228876166216,-2.82405261783819,12.166008314544));
#51116=CARTESIAN_POINT('Ctrl Pts',(6.22663942259502,-2.65611669750417,12.1746374027165));
#51117=CARTESIAN_POINT('Ctrl Pts',(6.2940677570571,-2.48535713119347,12.1832664908891));
#51118=CARTESIAN_POINT('Ctrl Pts',(6.36473685362026,-2.30639046418374,12.1923103130476));
#51119=CARTESIAN_POINT('Ctrl Pts',(6.42780163725656,-2.12432232704686,12.2013541352061));
#51120=CARTESIAN_POINT('Ctrl Pts',(6.48300865200716,-1.93981643925407,12.2103979573646));
#51121=CARTESIAN_POINT('Ctrl Pts',(6.53821566675777,-1.75531055146122,12.2194417795231));
#51122=CARTESIAN_POINT('Ctrl Pts',(6.58556476898538,-1.56836727223152,12.2284856016816));
#51123=CARTESIAN_POINT('Ctrl Pts',(6.62486185615985,-1.37967184025708,12.2375294238401));
#51124=CARTESIAN_POINT('Ctrl Pts',(6.66147347815302,-1.20387138470126,12.2459552136899));
#51125=CARTESIAN_POINT('Ctrl Pts',(6.69108017067793,-1.0266271008646,12.2543810035397));
#51126=CARTESIAN_POINT('Ctrl Pts',(6.71359061716581,-0.848522259639202,
12.2628067933895));
#51127=CARTESIAN_POINT('Ctrl Pts',(6.73610628683456,-0.670376092098958,
12.271234538306));
#51128=CARTESIAN_POINT('Ctrl Pts',(6.75152238588159,-0.491369297929553,
12.2796622832225));
#51129=CARTESIAN_POINT('Ctrl Pts',(6.75979943308341,-0.312090731174892,
12.288090028139));
#51130=CARTESIAN_POINT('Ctrl Pts',(6.76807952168481,-0.132746288541368,
12.2965208698289));
#51131=CARTESIAN_POINT('Ctrl Pts',(6.7692153126499,0.0468697948018875,12.3049517115188));
#51132=CARTESIAN_POINT('Ctrl Pts',(6.76321943488462,0.226167804072546,12.3133825532087));
#51133=CARTESIAN_POINT('Ctrl Pts',(6.75721804767299,0.405630565328126,12.321821141766));
#51134=CARTESIAN_POINT('Ctrl Pts',(6.74407191035636,0.584774337033546,12.3302597303234));
#51135=CARTESIAN_POINT('Ctrl Pts',(6.72384568996211,0.763012540904812,12.3386983188807));
#51136=CARTESIAN_POINT('Ctrl Pts',(6.70360886383172,0.941344205013449,12.347141332261));
#51137=CARTESIAN_POINT('Ctrl Pts',(6.67628459558111,1.11876902615511,12.3555843456412));
#51138=CARTESIAN_POINT('Ctrl Pts',(6.64198894150593,1.29470919550026,12.3640273590214));
#51139=CARTESIAN_POINT('Ctrl Pts',(6.60765725745575,1.47083420225629,12.3724792423757));
#51140=CARTESIAN_POINT('Ctrl Pts',(6.56633962850735,1.64547111803245,12.38093112573));
#51141=CARTESIAN_POINT('Ctrl Pts',(6.51820263109422,1.8180548561571,12.3893830090843));
#51142=CARTESIAN_POINT('Ctrl Pts',(6.50508377853655,1.86508937712808,12.3916864143135));
#51143=CARTESIAN_POINT('Ctrl Pts',(6.49145871001122,1.91197149993074,12.3939898195427));
#51144=CARTESIAN_POINT('Ctrl Pts',(6.4773314260651,1.95869002062843,12.3962932247719));
#51145=CARTESIAN_POINT('Ctrl Pts',(6.42631507109697,2.12739963562528,12.4046112666019));
#51146=CARTESIAN_POINT('Ctrl Pts',(6.36865392812675,2.29427782756339,12.4129293084319));
#51147=CARTESIAN_POINT('Ctrl Pts',(6.30450005681102,2.45877368492302,12.4212473502619));
#51148=CARTESIAN_POINT('Ctrl Pts',(6.24040189617653,2.62312669546625,12.4295581687745));
#51149=CARTESIAN_POINT('Ctrl Pts',(6.16982236764962,2.78510117112147,12.4378689872871));
#51150=CARTESIAN_POINT('Ctrl Pts',(6.09296322397741,2.9441617060309,12.4461798057997));
#51151=CARTESIAN_POINT('Ctrl Pts',(6.01392927394398,3.10772301790209,12.4547257872363));
#51152=CARTESIAN_POINT('Ctrl Pts',(5.92825518985636,3.26820269193904,12.463271768673));
#51153=CARTESIAN_POINT('Ctrl Pts',(5.83621387980417,3.42503964198682,12.4718177501097));
#51154=CARTESIAN_POINT('Ctrl Pts',(5.74681276250543,3.57737774495436,12.4801185912039));
#51155=CARTESIAN_POINT('Ctrl Pts',(5.65140485702718,3.72627890193112,12.4884194322982));
#51156=CARTESIAN_POINT('Ctrl Pts',(5.55028720305213,3.87125315158229,12.4967202733924));
#51157=CARTESIAN_POINT('Ctrl Pts',(5.44919593882082,4.01618956577005,12.5050189481284));
#51158=CARTESIAN_POINT('Ctrl Pts',(5.34239809400194,4.15720082965892,12.5133176228644));
#51159=CARTESIAN_POINT('Ctrl Pts',(5.23023413478742,4.29382578772177,12.5216162976004));
#51160=CARTESIAN_POINT('Ctrl Pts',(5.1180808301031,4.43043776768764,12.5299141840396));
#51161=CARTESIAN_POINT('Ctrl Pts',(5.00056264787511,4.56266400379488,12.5382120704789));
#51162=CARTESIAN_POINT('Ctrl Pts',(4.87806057260666,4.69007612411359,12.5465099569181));
#51163=CARTESIAN_POINT('Ctrl Pts',(4.74916269563243,4.82414039832184,12.5552410738649));
#51164=CARTESIAN_POINT('Ctrl Pts',(4.61474685148551,4.95287409026204,12.5639721908117));
#51165=CARTESIAN_POINT('Ctrl Pts',(4.47530120284403,5.0758219180565,12.5727033077585));
#51166=CARTESIAN_POINT('Ctrl Pts',(4.34269155605801,5.19274251167682,12.5810064018001));
#51167=CARTESIAN_POINT('Ctrl Pts',(4.2055337520006,5.30443073289881,12.5893094958417));
#51168=CARTESIAN_POINT('Ctrl Pts',(4.06428169622938,5.41053632218607,12.5976125898833));
#51169=CARTESIAN_POINT('Ctrl Pts',(3.92298254815063,5.51667728622959,12.6059184521101));
#51170=CARTESIAN_POINT('Ctrl Pts',(3.77758671001731,5.61723170586951,12.614224314337));
#51171=CARTESIAN_POINT('Ctrl Pts',(3.62857748778439,5.71189236725836,12.6225301765638));
#51172=CARTESIAN_POINT('Ctrl Pts',(3.47945071810508,5.80662770267647,12.6308425909549));
#51173=CARTESIAN_POINT('Ctrl Pts',(3.32670517036247,5.89545981713876,12.6391550053459));
#51174=CARTESIAN_POINT('Ctrl Pts',(3.17084976882889,5.97812685910209,12.647467419737));
#51175=CARTESIAN_POINT('Ctrl Pts',(3.14700050283917,5.99077671437157,12.6487393999178));
#51176=CARTESIAN_POINT('Ctrl Pts',(3.12307845892274,6.00328230076835,12.6500113800987));
#51177=CARTESIAN_POINT('Ctrl Pts',(3.09908550384725,6.0156427786101,12.6512833602796));
#51178=CARTESIAN_POINT('Origin',(0.,0.,-63.6971797838103));
#51179=CARTESIAN_POINT('',(3.09908550384723,6.01564277861011,15.0459090623666));
#51180=CARTESIAN_POINT('',(3.09908550384726,6.0156427786101,14.6514674425353));
#51181=CARTESIAN_POINT('',(3.09908550384721,6.01564277861012,-63.6971797838103));
#51182=CARTESIAN_POINT('',(-6.7669990707839,0.00354626703724618,13.697179783782));
#51183=CARTESIAN_POINT('Ctrl Pts',(-6.76699907078421,0.00354626644463786,
13.6971797838099));
#51184=CARTESIAN_POINT('Ctrl Pts',(-6.76709416588778,-0.177914570622926,
13.7057259625698));
#51185=CARTESIAN_POINT('Ctrl Pts',(-6.75988576497314,-0.359512959521169,
13.7142721413297));
#51186=CARTESIAN_POINT('Ctrl Pts',(-6.74536894644925,-0.540635529981356,
13.7228183200896));
#51187=CARTESIAN_POINT('Ctrl Pts',(-6.73108277756305,-0.718880344879146,
13.7312287133789));
#51188=CARTESIAN_POINT('Ctrl Pts',(-6.70971871563235,-0.896663999759646,
13.7396391066682));
#51189=CARTESIAN_POINT('Ctrl Pts',(-6.68132449676958,-1.07340205369036,
13.7480494999575));
#51190=CARTESIAN_POINT('Ctrl Pts',(-6.65224264257796,-1.25442025106941,
13.7566635714526));
#51191=CARTESIAN_POINT('Ctrl Pts',(-6.6157858083811,-1.43434120511028,13.7652776429478));
#51192=CARTESIAN_POINT('Ctrl Pts',(-6.57206171372395,-1.61254266021207,
13.773891714443));
#51193=CARTESIAN_POINT('Ctrl Pts',(-6.52833761906682,-1.79074411531379,
13.7825057859381));
#51194=CARTESIAN_POINT('Ctrl Pts',(-6.47734633166832,-1.96722569930743,
13.7911198574333));
#51195=CARTESIAN_POINT('Ctrl Pts',(-6.41925196146298,-2.14137648610742,
13.7997339289284));
#51196=CARTESIAN_POINT('Ctrl Pts',(-6.36242738610591,-2.31172078062388,
13.8081597187782));
#51197=CARTESIAN_POINT('Ctrl Pts',(-6.29882283260392,-2.47978788974719,
13.8165855086281));
#51198=CARTESIAN_POINT('Ctrl Pts',(-6.22865289128799,-2.64502781835083,
13.8250112984779));
#51199=CARTESIAN_POINT('Ctrl Pts',(-6.15846666818502,-2.81030608817692,
13.8334390433944));
#51200=CARTESIAN_POINT('Ctrl Pts',(-6.08171214942431,-2.97275556438013,
13.8418667883109));
#51201=CARTESIAN_POINT('Ctrl Pts',(-5.99865152927202,-3.13184751071353,
13.8502945332274));
#51202=CARTESIAN_POINT('Ctrl Pts',(-5.915560388509,-3.2909979153555,13.8587253749174));
#51203=CARTESIAN_POINT('Ctrl Pts',(-5.82615867946626,-3.44678803647088,
13.8671562166073));
#51204=CARTESIAN_POINT('Ctrl Pts',(-5.73075406147579,-3.59871461592591,
13.8755870582973));
#51205=CARTESIAN_POINT('Ctrl Pts',(-5.63526177881876,-3.75078079651566,
13.8840256468546));
#51206=CARTESIAN_POINT('Ctrl Pts',(-5.53375574337052,-3.89897606174041,
13.892464235412));
#51207=CARTESIAN_POINT('Ctrl Pts',(-5.42658700588314,-4.04282604963165,
13.9009028239694));
#51208=CARTESIAN_POINT('Ctrl Pts',(-5.31936207384588,-4.18675146609945,
13.9093458373496));
#51209=CARTESIAN_POINT('Ctrl Pts',(-5.20646872196533,-4.32632680021686,
13.9177888507299));
#51210=CARTESIAN_POINT('Ctrl Pts',(-5.08829799717866,-4.46111112750037,
13.9262318641102));
#51211=CARTESIAN_POINT('Ctrl Pts',(-4.97000312580897,-4.59603705511432,
13.9346837474645));
#51212=CARTESIAN_POINT('Ctrl Pts',(-4.84642003064305,-4.72616167770075,
13.9431356308188));
#51213=CARTESIAN_POINT('Ctrl Pts',(-4.71797701471852,-4.85108048671507,
13.9515875141731));
#51214=CARTESIAN_POINT('Ctrl Pts',(-4.68297223506109,-4.88512480865146,
13.9538909194021));
#51215=CARTESIAN_POINT('Ctrl Pts',(-4.64760668654054,-4.91878270383548,
13.9561943246311));
#51216=CARTESIAN_POINT('Ctrl Pts',(-4.61188946415064,-4.95204650326068,
13.9584977298601));
#51217=CARTESIAN_POINT('Ctrl Pts',(-4.48291970587711,-5.07215730371138,
13.9668149951935));
#51218=CARTESIAN_POINT('Ctrl Pts',(-4.34913020695709,-5.18734269351666,
13.9751322605269));
#51219=CARTESIAN_POINT('Ctrl Pts',(-4.21092947632851,-5.29720321918914,
13.9834495258603));
#51220=CARTESIAN_POINT('Ctrl Pts',(-4.072845307382,-5.40697108596171,13.9917597762204));
#51221=CARTESIAN_POINT('Ctrl Pts',(-3.93035759035839,-5.5114228212473,14.0000700265805));
#51222=CARTESIAN_POINT('Ctrl Pts',(-3.7839099957345,-5.61019733558282,14.0083802769406));
#51223=CARTESIAN_POINT('Ctrl Pts',(-3.63755909819999,-5.70890663062903,
14.0166850401705));
#51224=CARTESIAN_POINT('Ctrl Pts',(-3.48725382047601,-5.80194598038974,
14.0249898034004));
#51225=CARTESIAN_POINT('Ctrl Pts',(-3.33346925191896,-5.8889958181774,14.0332945666303));
#51226=CARTESIAN_POINT('Ctrl Pts',(-3.17975807369543,-5.97600411332727,
14.0415953665929));
#51227=CARTESIAN_POINT('Ctrl Pts',(-3.02257121576365,-6.0570284219602,14.0498961665555));
#51228=CARTESIAN_POINT('Ctrl Pts',(-2.86241115851228,-6.131793486381,14.0581969665182));
#51229=CARTESIAN_POINT('Ctrl Pts',(-2.7022982257973,-6.20653655237684,14.0664953241031));
#51230=CARTESIAN_POINT('Ctrl Pts',(-2.53921415233772,-6.27502389822606,
14.074793681688));
#51231=CARTESIAN_POINT('Ctrl Pts',(-2.37368453368196,-6.33702696337637,
14.083092039273));
#51232=CARTESIAN_POINT('Ctrl Pts',(-2.20813807276732,-6.39903633719628,
14.0913912411968));
#51233=CARTESIAN_POINT('Ctrl Pts',(-2.04014589254418,-6.45455998300652,
14.0996904431206));
#51234=CARTESIAN_POINT('Ctrl Pts',(-1.87025256883398,-6.50341789590442,
14.1079896450443));
#51235=CARTESIAN_POINT('Ctrl Pts',(-1.70034202116121,-6.55228076206855,
14.1162896883499));
#51236=CARTESIAN_POINT('Ctrl Pts',(-1.52853028014549,-6.59447645164882,
14.1245897316554));
#51237=CARTESIAN_POINT('Ctrl Pts',(-1.35537596122062,-6.62987518764458,
14.132889774961));
#51238=CARTESIAN_POINT('Ctrl Pts',(-1.18217534373489,-6.66528338866867,
14.1411920375589));
#51239=CARTESIAN_POINT('Ctrl Pts',(-1.0076317737392,-6.69389094417816,14.1494943001568));
#51240=CARTESIAN_POINT('Ctrl Pts',(-0.832313097425561,-6.71561939867455,
14.1577965627548));
#51241=CARTESIAN_POINT('Ctrl Pts',(-0.656918437066145,-6.73735727039856,
14.1661024235974));
#51242=CARTESIAN_POINT('Ctrl Pts',(-0.480748345908473,-6.75221005629532,
14.17440828444));
#51243=CARTESIAN_POINT('Ctrl Pts',(-0.304375009054581,-6.76015124489556,
14.1827141452827));
#51244=CARTESIAN_POINT('Ctrl Pts',(-0.12779318647331,-6.76810182054099,
14.1910298242388));
#51245=CARTESIAN_POINT('Ctrl Pts',(0.048992013903208,-6.76912445982801,
14.1993455031949));
#51246=CARTESIAN_POINT('Ctrl Pts',(0.225407998656858,-6.763244800696,14.2076611821511));
#51247=CARTESIAN_POINT('Ctrl Pts',(0.401935565115987,-6.75736142272642,
14.2159821207079));
#51248=CARTESIAN_POINT('Ctrl Pts',(0.578093103757538,-6.74456706528404,
14.2243030592648));
#51249=CARTESIAN_POINT('Ctrl Pts',(0.753313770290341,-6.72493920890672,
14.2326239978217));
#51250=CARTESIAN_POINT('Ctrl Pts',(0.928794869007725,-6.70528217945515,
14.2409573038706));
#51251=CARTESIAN_POINT('Ctrl Pts',(1.10333596904297,-6.67877140554487,14.2492906099196));
#51252=CARTESIAN_POINT('Ctrl Pts',(1.27637969656503,-6.64553563455923,14.2576239159685));
#51253=CARTESIAN_POINT('Ctrl Pts',(1.40375009654633,-6.62107214486939,14.26375772122));
#51254=CARTESIAN_POINT('Ctrl Pts',(1.53030947374522,-6.59296623442997,14.2698915264716));
#51255=CARTESIAN_POINT('Ctrl Pts',(1.65584129774007,-6.5612863522863,14.2760253317231));
#51256=CARTESIAN_POINT('Ctrl Pts',(1.82102737472401,-6.51959911088335,14.2840967449651));
#51257=CARTESIAN_POINT('Ctrl Pts',(1.98494203352834,-6.47159297497934,14.2921681582071));
#51258=CARTESIAN_POINT('Ctrl Pts',(2.14705257811262,-6.41735570362279,14.3002395714491));
#51259=CARTESIAN_POINT('Ctrl Pts',(2.30895960633557,-6.36318652266802,14.3083008517004));
#51260=CARTESIAN_POINT('Ctrl Pts',(2.46906667773576,-6.30280188820965,14.3163621319516));
#51261=CARTESIAN_POINT('Ctrl Pts',(2.62685071084514,-6.23634062114413,14.3244234122028));
#51262=CARTESIAN_POINT('Ctrl Pts',(2.7844712619378,-6.16994821543144,14.3324763400604));
#51263=CARTESIAN_POINT('Ctrl Pts',(2.93977322379651,-6.09749185003728,14.340529267918));
#51264=CARTESIAN_POINT('Ctrl Pts',(3.092248226194,-6.01916023275673,14.3485821957756));
#51265=CARTESIAN_POINT('Ctrl Pts',(3.2445986358545,-5.94089262302127,14.3566285433));
#51266=CARTESIAN_POINT('Ctrl Pts',(3.39412635370123,-5.85675948634532,14.3646748908244));
#51267=CARTESIAN_POINT('Ctrl Pts',(3.54034267279721,-5.76699772491468,14.3727212383487));
#51268=CARTESIAN_POINT('Ctrl Pts',(3.68647149792179,-5.67728967577167,14.3807627710419));
#51269=CARTESIAN_POINT('Ctrl Pts',(3.82929255183924,-5.58195990141865,14.388804303735));
#51270=CARTESIAN_POINT('Ctrl Pts',(3.96834154507748,-5.48129130603475,14.3968458364282));
#51271=CARTESIAN_POINT('Ctrl Pts',(4.11006371870998,-5.37868738333038,14.4050419654764));
#51272=CARTESIAN_POINT('Ctrl Pts',(4.24786697040222,-5.27053745778933,14.4132380945247));
#51273=CARTESIAN_POINT('Ctrl Pts',(4.38129013694641,-5.15718777396132,14.421434223573));
#51274=CARTESIAN_POINT('Ctrl Pts',(4.51215147232026,-5.04601449443175,14.4294729804091));
#51275=CARTESIAN_POINT('Ctrl Pts',(4.63879911983766,-4.92983959333512,14.4375117372451));
#51276=CARTESIAN_POINT('Ctrl Pts',(4.76083129951727,-4.80903049871144,14.4455504940812));
#51277=CARTESIAN_POINT('Ctrl Pts',(4.8828752906221,-4.68820971104423,14.453590028984));
#51278=CARTESIAN_POINT('Ctrl Pts',(5.00030265887253,-4.5627540994133,14.4616295638868));
#51279=CARTESIAN_POINT('Ctrl Pts',(5.1127486852055,-4.43306777321635,14.4696690987896));
#51280=CARTESIAN_POINT('Ctrl Pts',(5.22522785947751,-4.30334321681622,14.4777110036651));
#51281=CARTESIAN_POINT('Ctrl Pts',(5.33272252439571,-4.16938574540773,14.4857529085406));
#51282=CARTESIAN_POINT('Ctrl Pts',(5.43490852954296,-4.03163220985015,14.4937948134161));
#51283=CARTESIAN_POINT('Ctrl Pts',(5.54054150186107,-3.88923193314583,14.502107990097));
#51284=CARTESIAN_POINT('Ctrl Pts',(5.64050114311577,-3.74277536337125,14.5104211667778));
#51285=CARTESIAN_POINT('Ctrl Pts',(5.73447889264906,-3.59277620090126,14.5187343434586));
#51286=CARTESIAN_POINT('Ctrl Pts',(5.82554784711029,-3.44741980575408,14.5267902110692));
#51287=CARTESIAN_POINT('Ctrl Pts',(5.91099957511724,-3.29873720683962,14.5348460786797));
#51288=CARTESIAN_POINT('Ctrl Pts',(5.99060105698889,-3.14721908611454,14.5429019462902));
#51289=CARTESIAN_POINT('Ctrl Pts',(6.07401631490912,-2.98844160078769,14.5513437775062));
#51290=CARTESIAN_POINT('Ctrl Pts',(6.15100674604125,-2.82655064347649,14.5597856087222));
#51291=CARTESIAN_POINT('Ctrl Pts',(6.22136199727863,-2.66213145783924,14.5682274399382));
#51292=CARTESIAN_POINT('Ctrl Pts',(6.29171724851601,-2.49771227220198,14.5766692711542));
#51293=CARTESIAN_POINT('Ctrl Pts',(6.35543723539127,-2.3307653195474,14.5851111023702));
#51294=CARTESIAN_POINT('Ctrl Pts',(6.41237240559569,-2.16189017573857,14.5935529335862));
#51295=CARTESIAN_POINT('Ctrl Pts',(6.46788197514518,-1.99724349940867,14.6017833896528));
#51296=CARTESIAN_POINT('Ctrl Pts',(6.51712741399373,-1.83021654216366,14.6100138457193));
#51297=CARTESIAN_POINT('Ctrl Pts',(6.55989964640253,-1.66132646675118,14.6182443017859));
#51298=CARTESIAN_POINT('Ctrl Pts',(6.60262110565111,-1.49263687381008,14.6264649878161));
#51299=CARTESIAN_POINT('Ctrl Pts',(6.63888457201858,-1.32208891068805,14.6346856738463));
#51300=CARTESIAN_POINT('Ctrl Pts',(6.66852964355521,-1.15021797630948,14.6429063598765));
#51301=CARTESIAN_POINT('Ctrl Pts',(6.69814547236329,-0.978516580232526,
14.6511189367919));
#51302=CARTESIAN_POINT('Ctrl Pts',(6.72115584739485,-0.805495162698951,
14.6593315137073));
#51303=CARTESIAN_POINT('Ctrl Pts',(6.73745061970401,-0.63170257799859,14.6675440906227));
#51304=CARTESIAN_POINT('Ctrl Pts',(6.75373258645454,-0.458046571526462,
14.6757502135273));
#51305=CARTESIAN_POINT('Ctrl Pts',(6.76330942894072,-0.283620960328507,
14.6839563364319));
#51306=CARTESIAN_POINT('Ctrl Pts',(6.76612235147591,-0.108983140246803,
14.6921624593366));
#51307=CARTESIAN_POINT('Ctrl Pts',(6.76893362743368,0.065552453524236,14.7003637786903));
#51308=CARTESIAN_POINT('Ctrl Pts',(6.76498886514755,0.240299651204914,14.708565098044));
#51309=CARTESIAN_POINT('Ctrl Pts',(6.75428123280918,0.414697514004833,14.7167664173976));
#51310=CARTESIAN_POINT('Ctrl Pts',(6.74357667223676,0.589045346190983,14.7249653839872));
#51311=CARTESIAN_POINT('Ctrl Pts',(6.72611312406623,0.763043685475608,14.7331643505767));
#51312=CARTESIAN_POINT('Ctrl Pts',(6.70193585136313,0.936132920163386,14.7413633171662));
#51313=CARTESIAN_POINT('Ctrl Pts',(6.67776177137814,1.10919929763553,14.7495612010452));
#51314=CARTESIAN_POINT('Ctrl Pts',(6.64687578138272,1.28135645444196,14.7577590849241));
#51315=CARTESIAN_POINT('Ctrl Pts',(6.60937487893045,1.45205120769313,14.765956968803));
#51316=CARTESIAN_POINT('Ctrl Pts',(6.571872116495,1.62275442712379,14.7741552592835));
#51317=CARTESIAN_POINT('Ctrl Pts',(6.5277538648852,1.79199474820034,14.782353549764));
#51318=CARTESIAN_POINT('Ctrl Pts',(6.47716799146005,1.95923041279106,14.7905518402446));
#51319=CARTESIAN_POINT('Ctrl Pts',(6.42657042001371,2.1265047507547,14.7987520265859));
#51320=CARTESIAN_POINT('Ctrl Pts',(6.36950235167999,2.29177316573873,14.8069522129272));
#51321=CARTESIAN_POINT('Ctrl Pts',(6.30616116457238,2.4545102090721,14.8151523992686));
#51322=CARTESIAN_POINT('Ctrl Pts',(6.24276009334236,2.61740110751092,14.8233603382427));
#51323=CARTESIAN_POINT('Ctrl Pts',(6.17307418462033,2.77775551830354,14.8315682772168));
#51324=CARTESIAN_POINT('Ctrl Pts',(6.09734889143322,2.93506822682849,14.8397762161909));
#51325=CARTESIAN_POINT('Ctrl Pts',(6.02158686161215,3.09245725251441,14.8479881370849));
#51326=CARTESIAN_POINT('Ctrl Pts',(5.93977977364929,3.24680131722539,14.8562000579788));
#51327=CARTESIAN_POINT('Ctrl Pts',(5.85221844740126,3.39762096825064,14.8644119788728));
#51328=CARTESIAN_POINT('Ctrl Pts',(5.76453704466559,3.5486474445347,14.8726351611154));
#51329=CARTESIAN_POINT('Ctrl Pts',(5.67108582560821,3.69613954517809,14.8808583433579));
#51330=CARTESIAN_POINT('Ctrl Pts',(5.57219891614664,3.83964688987077,14.8890815256005));
#51331=CARTESIAN_POINT('Ctrl Pts',(5.48401674891213,3.96761922451014,14.8964145288833));
#51332=CARTESIAN_POINT('Ctrl Pts',(5.39151274046028,4.09242312878907,14.9037475321662));
#51333=CARTESIAN_POINT('Ctrl Pts',(5.29494976727265,4.21376268459192,14.9110805354491));
#51334=CARTESIAN_POINT('Ctrl Pts',(5.17726978944369,4.36163754557937,14.9200171664916));
#51335=CARTESIAN_POINT('Ctrl Pts',(5.05331699973582,4.50467388222966,14.9289537975341));
#51336=CARTESIAN_POINT('Ctrl Pts',(4.92349523383776,4.6423575564983,14.9378904285766));
#51337=CARTESIAN_POINT('Ctrl Pts',(4.79273035422974,4.78104145873289,14.9468919813925));
#51338=CARTESIAN_POINT('Ctrl Pts',(4.65601100815203,4.9142943786491,14.9558935342083));
#51339=CARTESIAN_POINT('Ctrl Pts',(4.51379255778441,5.04162332441547,14.9648950870241));
#51340=CARTESIAN_POINT('Ctrl Pts',(4.37312634939398,5.1675625395666,14.973798392474));
#51341=CARTESIAN_POINT('Ctrl Pts',(4.22708064891526,5.28770623900974,14.9827016979239));
#51342=CARTESIAN_POINT('Ctrl Pts',(4.07613507253603,5.40161196962922,14.9916050033737));
#51343=CARTESIAN_POINT('Ctrl Pts',(3.92269098500821,5.51740311315492,15.0006556798726));
#51344=CARTESIAN_POINT('Ctrl Pts',(3.76418354441934,5.62674775083,15.0097063563714));
#51345=CARTESIAN_POINT('Ctrl Pts',(3.60115508114248,5.72922080928652,15.0187570328702));
#51346=CARTESIAN_POINT('Ctrl Pts',(3.43812661786561,5.83169386774304,15.027807709369));
#51347=CARTESIAN_POINT('Ctrl Pts',(3.27057733268523,5.92729513890819,15.0368583858678));
#51348=CARTESIAN_POINT('Ctrl Pts',(3.09908550384722,6.01564277861011,15.0459090623666));
#51349=CARTESIAN_POINT('Ctrl Pts',(3.09908550384717,6.01564277861014,13.0457845165097));
#51350=CARTESIAN_POINT('Ctrl Pts',(2.94002611072669,6.09758558632192,13.0542214576994));
#51351=CARTESIAN_POINT('Ctrl Pts',(2.77760959688775,6.17327019142043,13.062658398889));
#51352=CARTESIAN_POINT('Ctrl Pts',(2.61235697521166,6.24242581326066,13.0710953400787));
#51353=CARTESIAN_POINT('Ctrl Pts',(2.44721533292437,6.31153499197299,13.0795266152368));
#51354=CARTESIAN_POINT('Ctrl Pts',(2.27924168670711,6.37412380057255,13.0879578903949));
#51355=CARTESIAN_POINT('Ctrl Pts',(2.10897936049659,6.42996851135365,13.0963891655529));
#51356=CARTESIAN_POINT('Ctrl Pts',(1.93880524877013,6.48578428847421,13.1048160723894));
#51357=CARTESIAN_POINT('Ctrl Pts',(1.76634513758492,6.53486283106964,13.113242979226));
#51358=CARTESIAN_POINT('Ctrl Pts',(1.59216031042803,6.57702931009872,13.1216698860625));
#51359=CARTESIAN_POINT('Ctrl Pts',(1.41802841216451,6.61918297615719,13.1300942322463));
#51360=CARTESIAN_POINT('Ctrl Pts',(1.24217316610256,6.65442868615755,13.1385185784301));
#51361=CARTESIAN_POINT('Ctrl Pts',(1.06516941800624,6.68264192598588,13.1469429246139));
#51362=CARTESIAN_POINT('Ctrl Pts',(0.888196003982625,6.71085033076141,13.1553658270727));
#51363=CARTESIAN_POINT('Ctrl Pts',(0.710074809391342,6.73202861530033,13.1637887295315));
#51364=CARTESIAN_POINT('Ctrl Pts',(0.531389593725857,6.7461036235504,13.1722116319904));
#51365=CARTESIAN_POINT('Ctrl Pts',(0.352710082313214,6.76017818247731,13.1806342655609));
#51366=CARTESIAN_POINT('Ctrl Pts',(0.173466918097244,6.76714989123629,13.1890568991314));
#51367=CARTESIAN_POINT('Ctrl Pts',(-0.00575193952454701,6.76699755542971,
13.1974795327019));
#51368=CARTESIAN_POINT('Ctrl Pts',(-0.184990067383262,6.76684520324346,
13.2059030719034));
#51369=CARTESIAN_POINT('Ctrl Pts',(-0.364203550049273,6.75956728013755,
13.2143266111049));
#51370=CARTESIAN_POINT('Ctrl Pts',(-0.54280497774089,6.74519471595444,13.2227501503064));
#51371=CARTESIAN_POINT('Ctrl Pts',(-0.721522516916806,6.73081280795039,
13.2311791657778));
#51372=CARTESIAN_POINT('Ctrl Pts',(-0.899626873024427,6.70932706658896,
13.2396081812493));
#51373=CARTESIAN_POINT('Ctrl Pts',(-1.07653522714635,6.68082037662389,13.2480371967207));
#51374=CARTESIAN_POINT('Ctrl Pts',(-1.25349717761354,6.65230505024136,13.2564687658558));
#51375=CARTESIAN_POINT('Ctrl Pts',(-1.42926207521128,6.61676459281632,13.2649003349909));
#51376=CARTESIAN_POINT('Ctrl Pts',(-1.60325725162761,6.57433306009845,13.273331904126));
#51377=CARTESIAN_POINT('Ctrl Pts',(-1.77742662637449,6.53185904630546,13.2817719146747));
#51378=CARTESIAN_POINT('Ctrl Pts',(-1.94982241538522,6.48248025198872,13.2902119252235));
#51379=CARTESIAN_POINT('Ctrl Pts',(-2.11988577858572,6.42638104112649,13.2986519357723));
#51380=CARTESIAN_POINT('Ctrl Pts',(-2.28639312073834,6.3714548634846,13.3069154658928));
#51381=CARTESIAN_POINT('Ctrl Pts',(-2.45066434411047,6.31008666730127,13.3151789960134));
#51382=CARTESIAN_POINT('Ctrl Pts',(-2.61219368322618,6.24249414587737,13.323442526134));
#51383=CARTESIAN_POINT('Ctrl Pts',(-2.77133507280265,6.17590087035688,13.3315838933519));
#51384=CARTESIAN_POINT('Ctrl Pts',(-2.92813109737699,6.10313320137953,13.3397252605697));
#51385=CARTESIAN_POINT('Ctrl Pts',(-3.08206503653218,6.02438080723537,13.3478666277876));
#51386=CARTESIAN_POINT('Ctrl Pts',(-3.23586460306598,5.94569715794177,13.356000888211));
#51387=CARTESIAN_POINT('Ctrl Pts',(-3.38680673358627,5.86103934792309,13.3641351486345));
#51388=CARTESIAN_POINT('Ctrl Pts',(-3.53439404226829,5.77064534987019,13.372269409058));
#51389=CARTESIAN_POINT('Ctrl Pts',(-3.68188067221889,5.68031301533791,13.3803981205828));
#51390=CARTESIAN_POINT('Ctrl Pts',(-3.8260167258597,5.58425247387798,13.3885268321075));
#51391=CARTESIAN_POINT('Ctrl Pts',(-3.96632886489278,5.4827478818124,13.3966555436323));
#51392=CARTESIAN_POINT('Ctrl Pts',(-4.10657409166014,5.38129169541067,13.4047803787248));
#51393=CARTESIAN_POINT('Ctrl Pts',(-4.24299873920578,5.27439684238225,13.4129052138174));
#51394=CARTESIAN_POINT('Ctrl Pts',(-4.37515797079932,5.16239108655584,13.4210300489099));
#51395=CARTESIAN_POINT('Ctrl Pts',(-4.50728020404572,5.05041668705457,13.429152609432));
#51396=CARTESIAN_POINT('Ctrl Pts',(-4.6351391213156,4.93333447174832,13.4372751699542));
#51397=CARTESIAN_POINT('Ctrl Pts',(-4.75832256938735,4.81151278972206,13.4453977304764));
#51398=CARTESIAN_POINT('Ctrl Pts',(-4.88151256433965,4.68968463318959,13.4535207226915));
#51399=CARTESIAN_POINT('Ctrl Pts',(-5.00002633065173,4.56311676134893,13.4616437149067));
#51400=CARTESIAN_POINT('Ctrl Pts',(-5.11348810125801,4.43221484568299,13.4697667071219));
#51401=CARTESIAN_POINT('Ctrl Pts',(-5.17140687745421,4.36539340691471,13.4739132471031));
#51402=CARTESIAN_POINT('Ctrl Pts',(-5.22800981914079,4.29744318159846,13.4780597870842));
#51403=CARTESIAN_POINT('Ctrl Pts',(-5.28325092638768,4.22842153159117,13.4822063270654));
#51404=CARTESIAN_POINT('Ctrl Pts',(-5.40293318535753,4.0788831279929,13.4911899860938));
#51405=CARTESIAN_POINT('Ctrl Pts',(-5.51616158888885,3.92438776164471,13.5001736451222));
#51406=CARTESIAN_POINT('Ctrl Pts',(-5.62257164882376,3.76549824775464,13.5091573041505));
#51407=CARTESIAN_POINT('Ctrl Pts',(-5.72916452011397,3.60633576336352,13.5181563970099));
#51408=CARTESIAN_POINT('Ctrl Pts',(-5.82891550203853,3.44276424163258,13.5271554898693));
#51409=CARTESIAN_POINT('Ctrl Pts',(-5.92150483796006,3.27537317782503,13.5361545827287));
#51410=CARTESIAN_POINT('Ctrl Pts',(-6.01431127000053,3.10758962874974,13.5451747759461));
#51411=CARTESIAN_POINT('Ctrl Pts',(-6.09992234188846,2.93596882881938,13.5541949691634));
#51412=CARTESIAN_POINT('Ctrl Pts',(-6.1780642601733,2.76112495138655,13.5632151623808));
#51413=CARTESIAN_POINT('Ctrl Pts',(-6.25628531671751,2.58610400074608,13.5722444908025));
#51414=CARTESIAN_POINT('Ctrl Pts',(-6.32702201589748,2.40785367219275,13.5812738192242));
#51415=CARTESIAN_POINT('Ctrl Pts',(-6.39004916142147,2.22700712046836,13.5903031476459));
#51416=CARTESIAN_POINT('Ctrl Pts',(-6.45316516251637,2.04590561155897,13.5993452056006));
#51417=CARTESIAN_POINT('Ctrl Pts',(-6.508549798691,1.86220078690502,13.6083872635554));
#51418=CARTESIAN_POINT('Ctrl Pts',(-6.55602741117472,1.67654215095407,13.6174293215101));
#51419=CARTESIAN_POINT('Ctrl Pts',(-6.59722973088013,1.51542270803466,13.6252762570057));
#51420=CARTESIAN_POINT('Ctrl Pts',(-6.63247786449317,1.35283211035126,13.6331231925014));
#51421=CARTESIAN_POINT('Ctrl Pts',(-6.66168820007206,1.18920112891837,13.640970127997));
#51422=CARTESIAN_POINT('Ctrl Pts',(-6.69711427398505,0.99075071307011,13.6504868319769));
#51423=CARTESIAN_POINT('Ctrl Pts',(-6.72368001736206,0.790651468887019,
13.6600035359568));
#51424=CARTESIAN_POINT('Ctrl Pts',(-6.7412618041006,0.589642509131079,13.6695202399368));
#51425=CARTESIAN_POINT('Ctrl Pts',(-6.75829515942328,0.394903653206785,
13.6787400878852));
#51426=CARTESIAN_POINT('Ctrl Pts',(-6.7668964796064,0.199311108068396,13.6879599358336));
#51427=CARTESIAN_POINT('Ctrl Pts',(-6.7669990707839,0.00354626703724167,
13.697179783782));
#51428=CARTESIAN_POINT('',(-6.76699798626915,-0.00522052001777089,13.302820216157));
#51429=CARTESIAN_POINT('Ctrl Pts',(3.09908550384725,6.0156427786101,12.6512833602796));
#51430=CARTESIAN_POINT('Ctrl Pts',(2.94210374532802,6.09651524895113,12.6596057067752));
#51431=CARTESIAN_POINT('Ctrl Pts',(2.78208499805338,6.17117181071805,12.6679280532708));
#51432=CARTESIAN_POINT('Ctrl Pts',(2.6195623649851,6.23940558194077,12.6762503997664));
#51433=CARTESIAN_POINT('Ctrl Pts',(2.45680893777207,6.30773625015917,12.6845845646088));
#51434=CARTESIAN_POINT('Ctrl Pts',(2.29154484584409,6.36962578316633,12.6929187294512));
#51435=CARTESIAN_POINT('Ctrl Pts',(2.12431953451885,6.42491677107662,12.7012528942936));
#51436=CARTESIAN_POINT('Ctrl Pts',(2.04026086604636,6.45270973366963,12.705442205074));
#51437=CARTESIAN_POINT('Ctrl Pts',(1.95570683751969,6.4788362144871,12.7096315158543));
#51438=CARTESIAN_POINT('Ctrl Pts',(1.87072815952385,6.50328110673101,12.7138208266347));
#51439=CARTESIAN_POINT('Ctrl Pts',(1.70700241492626,6.55037831133143,12.7218922398767));
#51440=CARTESIAN_POINT('Ctrl Pts',(1.54119570789558,6.59137514485665,12.7299636531187));
#51441=CARTESIAN_POINT('Ctrl Pts',(1.37381253820462,6.62607939205921,12.7380350663608));
#51442=CARTESIAN_POINT('Ctrl Pts',(1.2066395042192,6.6607400709539,12.746096346612));
#51443=CARTESIAN_POINT('Ctrl Pts',(1.03789430607367,6.68912380738644,12.7541576268632));
#51444=CARTESIAN_POINT('Ctrl Pts',(0.868098829367446,6.71108735023252,12.7622189071144));
#51445=CARTESIAN_POINT('Ctrl Pts',(0.698479279885125,6.73302813637626,12.770271834972));
#51446=CARTESIAN_POINT('Ctrl Pts',(0.527811984151826,6.74856191925419,12.7783247628297));
#51447=CARTESIAN_POINT('Ctrl Pts',(0.356631217975381,6.75759596116588,12.7863776906873));
#51448=CARTESIAN_POINT('Ctrl Pts',(0.185590329679652,6.76662262104123,12.7944240382117));
#51449=CARTESIAN_POINT('Ctrl Pts',(0.014037176588647,6.76916009143369,12.802470385736));
#51450=CARTESIAN_POINT('Ctrl Pts',(-0.157486706361212,6.76516717733712,
12.8105167332604));
#51451=CARTESIAN_POINT('Ctrl Pts',(-0.32890795161737,6.76117665254918,12.8185582659536));
#51452=CARTESIAN_POINT('Ctrl Pts',(-0.500299589675203,6.7506635310307,12.8265997986467));
#51453=CARTESIAN_POINT('Ctrl Pts',(-0.67111803809773,6.73363865818028,12.8346413313399));
#51454=CARTESIAN_POINT('Ctrl Pts',(-0.845220426351066,6.71628648661836,
12.8428374603881));
#51455=CARTESIAN_POINT('Ctrl Pts',(-1.01872696642979,6.69216962278029,12.8510335894364));
#51456=CARTESIAN_POINT('Ctrl Pts',(-1.19106490449715,6.66135522197062,12.8592297184846));
#51457=CARTESIAN_POINT('Ctrl Pts',(-1.36009381675582,6.63113248222351,12.8672684753207));
#51458=CARTESIAN_POINT('Ctrl Pts',(-1.52799821947554,6.59446716054457,12.8753072321568));
#51459=CARTESIAN_POINT('Ctrl Pts',(-1.69424601636151,6.55147460012196,12.8833459889929));
#51460=CARTESIAN_POINT('Ctrl Pts',(-1.86050990427714,6.50847787847389,12.8913855238957));
#51461=CARTESIAN_POINT('Ctrl Pts',(-2.02511650546706,6.45915279207153,12.8994250587985));
#51462=CARTESIAN_POINT('Ctrl Pts',(-2.18754729237714,6.40366503212133,12.9074645937013));
#51463=CARTESIAN_POINT('Ctrl Pts',(-2.35002596222311,6.3481609149466,12.9155064985768));
#51464=CARTESIAN_POINT('Ctrl Pts',(-2.51032718785764,6.28649062880948,12.9235484034523));
#51465=CARTESIAN_POINT('Ctrl Pts',(-2.6679510243003,6.21886857329651,12.9315903083278));
#51466=CARTESIAN_POINT('Ctrl Pts',(-2.83089187248764,6.14896547151873,12.9399034850087));
#51467=CARTESIAN_POINT('Ctrl Pts',(-2.99097114177248,6.07270221526078,12.9482166616895));
#51468=CARTESIAN_POINT('Ctrl Pts',(-3.14766368850354,5.99036745985389,12.9565298383704));
#51469=CARTESIAN_POINT('Ctrl Pts',(-3.29950629458373,5.91058112608898,12.9645857059809));
#51470=CARTESIAN_POINT('Ctrl Pts',(-3.44816842299859,5.82509379009984,12.9726415735914));
#51471=CARTESIAN_POINT('Ctrl Pts',(-3.59320179316167,5.73421222781471,12.9806974412019));
#51472=CARTESIAN_POINT('Ctrl Pts',(-3.74518383790148,5.63897645104341,12.9891392724179));
#51473=CARTESIAN_POINT('Ctrl Pts',(-3.8931804549649,5.53781712185059,12.9975811036339));
#51474=CARTESIAN_POINT('Ctrl Pts',(-4.03671536784392,5.43113413929473,13.0060229348499));
#51475=CARTESIAN_POINT('Ctrl Pts',(-4.18025028072295,5.32445115673887,13.0144647660659));
#51476=CARTESIAN_POINT('Ctrl Pts',(-4.31932318429191,5.21224487696434,13.0229065972819));
#51477=CARTESIAN_POINT('Ctrl Pts',(-4.45350313218815,5.09495817957227,13.0313484284979));
#51478=CARTESIAN_POINT('Ctrl Pts',(-4.58315933088935,4.98162569151799,13.0395056514116));
#51479=CARTESIAN_POINT('Ctrl Pts',(-4.70869264445891,4.86316062911941,13.0476628743253));
#51480=CARTESIAN_POINT('Ctrl Pts',(-4.82966607146199,4.73989605773892,13.055820097239));
#51481=CARTESIAN_POINT('Ctrl Pts',(-4.95049448812238,4.61677924308634,13.0639675421236));
#51482=CARTESIAN_POINT('Ctrl Pts',(-5.06677364563792,4.48887463075528,13.0721149870082));
#51483=CARTESIAN_POINT('Ctrl Pts',(-5.17809910981238,4.35655581956208,13.0802624318929));
#51484=CARTESIAN_POINT('Ctrl Pts',(-5.28931456857467,4.22436775819753,13.0884018259417));
#51485=CARTESIAN_POINT('Ctrl Pts',(-5.39558584606881,4.08777446054306,13.0965412199905));
#51486=CARTESIAN_POINT('Ctrl Pts',(-5.49654494194717,3.94718668182226,13.1046806140393));
#51487=CARTESIAN_POINT('Ctrl Pts',(-5.59894811720977,3.80458799055156,13.1129364307942));
#51488=CARTESIAN_POINT('Ctrl Pts',(-5.69588569719101,3.6578799265307,13.1211922475492));
#51489=CARTESIAN_POINT('Ctrl Pts',(-5.78701486954364,3.50752731987662,13.1294480643041));
#51490=CARTESIAN_POINT('Ctrl Pts',(-5.87673678152078,3.35949653026787,13.137576390778));
#51491=CARTESIAN_POINT('Ctrl Pts',(-5.9608281827451,3.2079332702881,13.1457047172519));
#51492=CARTESIAN_POINT('Ctrl Pts',(-6.03900474827512,3.05331142373499,13.1538330437259));
#51493=CARTESIAN_POINT('Ctrl Pts',(-6.117158453127,2.89873479226958,13.1619589932848));
#51494=CARTESIAN_POINT('Ctrl Pts',(-6.18940060090174,2.7411016810502,13.1700849428437));
#51495=CARTESIAN_POINT('Ctrl Pts',(-6.25549260177143,2.5809109456126,13.1782108924026));
#51496=CARTESIAN_POINT('Ctrl Pts',(-6.32157786448275,2.42073654181168,13.1863360135112));
#51497=CARTESIAN_POINT('Ctrl Pts',(-6.38151409000943,2.25800537143498,13.1944611346199));
#51498=CARTESIAN_POINT('Ctrl Pts',(-6.43511068145649,2.0932366128569,13.2025862557285));
#51499=CARTESIAN_POINT('Ctrl Pts',(-6.49020933326299,1.92385016098802,13.2109390857642));
#51500=CARTESIAN_POINT('Ctrl Pts',(-6.53860766597136,1.75231062191697,13.2192919157999));
#51501=CARTESIAN_POINT('Ctrl Pts',(-6.58015348247487,1.57919889408327,13.2276447458356));
#51502=CARTESIAN_POINT('Ctrl Pts',(-6.62059538367987,1.41068692383746,13.2357756325413));
#51503=CARTESIAN_POINT('Ctrl Pts',(-6.65454425660174,1.24068562579775,13.243906519247));
#51504=CARTESIAN_POINT('Ctrl Pts',(-6.68191166322437,1.06974086809197,13.2520374059527));
#51505=CARTESIAN_POINT('Ctrl Pts',(-6.71039961430526,0.891796864766862,
13.2605012076534));
#51506=CARTESIAN_POINT('Ctrl Pts',(-6.73175569899097,0.71283094874556,13.2689650093542));
#51507=CARTESIAN_POINT('Ctrl Pts',(-6.74593991475798,0.533463838020057,
13.2774288110549));
#51508=CARTESIAN_POINT('Ctrl Pts',(-6.76012413052499,0.354096727294553,
13.2858926127556));
#51509=CARTESIAN_POINT('Ctrl Pts',(-6.7671365028122,0.17432886676091,13.2943564144563));
#51510=CARTESIAN_POINT('Ctrl Pts',(-6.76699798626915,-0.00522052001777006,
13.302820216157));
#51511=CARTESIAN_POINT('Ctrl Pts',(-6.76699798626862,-0.00522052071405314,
13.3028202161898));
#51512=CARTESIAN_POINT('Ctrl Pts',(-6.76680254782566,-0.258553784264194,
13.3147621255739));
#51513=CARTESIAN_POINT('Ctrl Pts',(-6.75237781066175,-0.511376352775485,
13.3267040349581));
#51514=CARTESIAN_POINT('Ctrl Pts',(-6.72391519900023,-0.762399761708883,
13.3386459443422));
#51515=CARTESIAN_POINT('Ctrl Pts',(-6.7157876610372,-0.834079841877793,
13.3420559730151));
#51516=CARTESIAN_POINT('Ctrl Pts',(-6.70651576063321,-0.905613394825189,
13.345466001688));
#51517=CARTESIAN_POINT('Ctrl Pts',(-6.69610462071302,-0.976970781787121,
13.3488760303609));
#51518=CARTESIAN_POINT('Ctrl Pts',(-6.66882465074012,-1.16394621277629,
13.3578112171431));
#51519=CARTESIAN_POINT('Ctrl Pts',(-6.63369169714627,-1.34989716734416,
13.3667464039253));
#51520=CARTESIAN_POINT('Ctrl Pts',(-6.59079597868481,-1.53417644596446,
13.3756815907075));
#51521=CARTESIAN_POINT('Ctrl Pts',(-6.54796450473953,-1.7181797312334,13.3846033953441));
#51522=CARTESIAN_POINT('Ctrl Pts',(-6.4973935226934,-1.9005160851843,13.3935251999807));
#51523=CARTESIAN_POINT('Ctrl Pts',(-6.43922439836573,-2.08054755953608,
13.4024470046173));
#51524=CARTESIAN_POINT('Ctrl Pts',(-6.38119716232729,-2.26013989442687,
13.4113470468565));
#51525=CARTESIAN_POINT('Ctrl Pts',(-6.31560885333637,-2.43743832519912,
13.4202470890957));
#51526=CARTESIAN_POINT('Ctrl Pts',(-6.24265061621746,-2.61181972652015,
13.429147131335));
#51527=CARTESIAN_POINT('Ctrl Pts',(-6.16980469937722,-2.78593266511011,
13.4380334718283));
#51528=CARTESIAN_POINT('Ctrl Pts',(-6.08961158617208,-2.95713729512159,
13.4469198123217));
#51529=CARTESIAN_POINT('Ctrl Pts',(-6.00231148810044,-3.12482732320003,
13.4558061528151));
#51530=CARTESIAN_POINT('Ctrl Pts',(-5.91523460114094,-3.29208859714774,
13.464669772487));
#51531=CARTESIAN_POINT('Ctrl Pts',(-5.82108710798822,-3.45585297216316,
13.4735333921588));
#51532=CARTESIAN_POINT('Ctrl Pts',(-5.7201560570988,-3.61553643079916,13.4823970118307));
#51533=CARTESIAN_POINT('Ctrl Pts',(-5.62434176639866,-3.76712464068034,
13.4908112849846));
#51534=CARTESIAN_POINT('Ctrl Pts',(-5.52241469626898,-3.91503516365269,
13.4992255581386));
#51535=CARTESIAN_POINT('Ctrl Pts',(-5.41466008086214,-4.05878617430359,
13.5076398312925));
#51536=CARTESIAN_POINT('Ctrl Pts',(-5.30951824371354,-4.19905158469682,
13.515850079497));
#51537=CARTESIAN_POINT('Ctrl Pts',(-5.19892827514438,-4.33522133848849,
13.5240603277016));
#51538=CARTESIAN_POINT('Ctrl Pts',(-5.08325100083917,-4.46686111967538,
13.5322705759061));
#51539=CARTESIAN_POINT('Ctrl Pts',(-4.96754622773981,-4.59853219426252,
13.5404827758503));
#51540=CARTESIAN_POINT('Ctrl Pts',(-4.84675197448823,-4.72567088343414,
13.5486949757945));
#51541=CARTESIAN_POINT('Ctrl Pts',(-4.72126741702553,-4.8478781932855,13.5569071757387));
#51542=CARTESIAN_POINT('Ctrl Pts',(-4.59573068409985,-4.97013631594683,
13.5651227902492));
#51543=CARTESIAN_POINT('Ctrl Pts',(-4.46550001654741,-5.08745872624941,
13.5733384047596));
#51544=CARTESIAN_POINT('Ctrl Pts',(-4.33100934004682,-5.19948527225794,
13.5815540192701));
#51545=CARTESIAN_POINT('Ctrl Pts',(-4.19636763641176,-5.31163761916708,
13.5897788595555));
#51546=CARTESIAN_POINT('Ctrl Pts',(-4.05745664262412,-5.41848199575201,
13.5980036998409));
#51547=CARTESIAN_POINT('Ctrl Pts',(-3.91474184822035,-5.51969974380784,
13.6062285401263));
#51548=CARTESIAN_POINT('Ctrl Pts',(-3.7719356400296,-5.62098232534992,13.6144586487079));
#51549=CARTESIAN_POINT('Ctrl Pts',(-3.62532107159179,-5.71663089988303,
13.6226887572894));
#51550=CARTESIAN_POINT('Ctrl Pts',(-3.47539008769781,-5.80637173614744,
13.630918865871));
#51551=CARTESIAN_POINT('Ctrl Pts',(-3.32525354612426,-5.89623560847542,
13.6391602580577));
#51552=CARTESIAN_POINT('Ctrl Pts',(-3.17179181859186,-5.98017539413079,
13.6474016502444));
#51553=CARTESIAN_POINT('Ctrl Pts',(-3.01551965984233,-6.05796419443895,
13.6556430424311));
#51554=CARTESIAN_POINT('Ctrl Pts',(-2.94750604603211,-6.09181985667115,
13.6592299056953));
#51555=CARTESIAN_POINT('Ctrl Pts',(-2.87896031322669,-6.12451101748651,
13.6628167689596));
#51556=CARTESIAN_POINT('Ctrl Pts',(-2.80992587884854,-6.15602189367267,
13.6664036322238));
#51557=CARTESIAN_POINT('Ctrl Pts',(-2.64732222801011,-6.23024258592781,
13.6748521270522));
#51558=CARTESIAN_POINT('Ctrl Pts',(-2.4816353628965,-6.29808112664666,13.6833006218806));
#51559=CARTESIAN_POINT('Ctrl Pts',(-2.31339409499536,-6.35928429630573,
13.6917491167091));
#51560=CARTESIAN_POINT('Ctrl Pts',(-2.14530650571936,-6.42043156042458,
13.7001898943282));
#51561=CARTESIAN_POINT('Ctrl Pts',(-1.97466947648193,-6.47495542149956,
13.7086306719474));
#51562=CARTESIAN_POINT('Ctrl Pts',(-1.80203272105282,-6.52265031043785,
13.7170714495666));
#51563=CARTESIAN_POINT('Ctrl Pts',(-1.62952711144905,-6.57030896731444,
13.7255058150359));
#51564=CARTESIAN_POINT('Ctrl Pts',(-1.4550251243115,-6.61114890534553,13.7339401805052));
#51565=CARTESIAN_POINT('Ctrl Pts',(-1.27909297551313,-6.64501393226478,
13.7423745459745));
#51566=CARTESIAN_POINT('Ctrl Pts',(-1.1032674584349,-6.67885843373659,13.7508037994111));
#51567=CARTESIAN_POINT('Ctrl Pts',(-0.926013834524638,-6.70573638968763,
13.7592330528477));
#51568=CARTESIAN_POINT('Ctrl Pts',(-0.747910281271728,-6.72554229866767,
13.7676623062843));
#51569=CARTESIAN_POINT('Ctrl Pts',(-0.569887355251328,-6.74533924154009,
13.7760877438095));
#51570=CARTESIAN_POINT('Ctrl Pts',(-0.391015597954095,-6.75807048450108,
13.7845131813347));
#51571=CARTESIAN_POINT('Ctrl Pts',(-0.211880506429093,-6.76368210747632,
13.7929386188599));
#51572=CARTESIAN_POINT('Ctrl Pts',(-0.0327847660661349,-6.76929249772891,
13.8013622055431));
#51573=CARTESIAN_POINT('Ctrl Pts',(0.146573860306079,-6.76778637322521,
13.8097857922263));
#51574=CARTESIAN_POINT('Ctrl Pts',(0.325607119369595,-6.75916185660736,
13.8182093789094));
#51575=CARTESIAN_POINT('Ctrl Pts',(0.504620345550144,-6.7505383050277,13.8266320230374));
#51576=CARTESIAN_POINT('Ctrl Pts',(0.683307944051406,-6.73479796526905,
13.8350546671654));
#51577=CARTESIAN_POINT('Ctrl Pts',(0.861083712811642,-6.71199104882676,
13.8434773112934));
#51578=CARTESIAN_POINT('Ctrl Pts',(1.03886437950728,-6.6891835040266,13.8519001874753));
#51579=CARTESIAN_POINT('Ctrl Pts',(1.21573283573447,-6.65930903718829,13.8603230636573));
#51580=CARTESIAN_POINT('Ctrl Pts',(1.39110966602265,-6.62246954670978,13.8687459398392));
#51581=CARTESIAN_POINT('Ctrl Pts',(1.56651578521461,-6.58562390383193,13.8771702226882));
#51582=CARTESIAN_POINT('Ctrl Pts',(1.74042945570415,-6.54181098736379,13.8855945055372));
#51583=CARTESIAN_POINT('Ctrl Pts',(1.91228272583966,-6.49118354204033,13.8940187883862));
#51584=CARTESIAN_POINT('Ctrl Pts',(2.08425205931978,-6.44052190481218,13.9024487606843));
#51585=CARTESIAN_POINT('Ctrl Pts',(2.25415789174803,-6.38303663665025,13.9108787329825));
#51586=CARTESIAN_POINT('Ctrl Pts',(2.42144770622888,-6.31893028969294,13.9193087052806));
#51587=CARTESIAN_POINT('Ctrl Pts',(2.5887973241183,-6.25480102575129,13.9277416911578));
#51588=CARTESIAN_POINT('Ctrl Pts',(2.75352875025348,-6.18404608850153,13.936174677035));
#51589=CARTESIAN_POINT('Ctrl Pts',(2.91511012103796,-6.10691591412736,13.9446076629122));
#51590=CARTESIAN_POINT('Ctrl Pts',(3.07684014569905,-6.02971478046272,13.953048407085));
#51591=CARTESIAN_POINT('Ctrl Pts',(3.23541402651578,-5.94612684050535,13.9614891512578));
#51592=CARTESIAN_POINT('Ctrl Pts',(3.39032416879734,-5.85644867052283,13.9699298954306));
#51593=CARTESIAN_POINT('Ctrl Pts',(3.47597812374837,-5.80686321524766,13.9745970083161));
#51594=CARTESIAN_POINT('Ctrl Pts',(3.56051245230653,-5.75541659648905,13.9792641212015));
#51595=CARTESIAN_POINT('Ctrl Pts',(3.64384520217654,-5.70216460149784,13.983931234087));
#51596=CARTESIAN_POINT('Ctrl Pts',(3.78921184202792,-5.60927118817199,13.9920726013048));
#51597=CARTESIAN_POINT('Ctrl Pts',(3.93120919044798,-5.51069695212364,14.0002139685227));
#51598=CARTESIAN_POINT('Ctrl Pts',(4.06936069948131,-5.40671734951227,14.0083553357406));
#51599=CARTESIAN_POINT('Ctrl Pts',(4.20739161275435,-5.30282851318583,14.0164895961641));
#51600=CARTESIAN_POINT('Ctrl Pts',(4.34158307856815,-5.19354392110617,14.0246238565875));
#51601=CARTESIAN_POINT('Ctrl Pts',(4.47148587948624,-5.07918330340175,14.032758117011));
#51602=CARTESIAN_POINT('Ctrl Pts',(4.60130006540548,-4.96490069838018,14.0408868285358));
#51603=CARTESIAN_POINT('Ctrl Pts',(4.72683113752287,-4.84554920271323,14.0490155400606));
#51604=CARTESIAN_POINT('Ctrl Pts',(4.84766148843627,-4.72148992305732,14.0571442515854));
#51605=CARTESIAN_POINT('Ctrl Pts',(4.96843421758857,-4.59748980497895,14.065269086678));
#51606=CARTESIAN_POINT('Ctrl Pts',(5.08451043466415,-4.46878663527642,14.0733939217705));
#51607=CARTESIAN_POINT('Ctrl Pts',(5.19550808867569,-4.33577959547133,14.081518756863));
#51608=CARTESIAN_POINT('Ctrl Pts',(5.30647466858273,-4.20280979136,14.0896413173852));
#51609=CARTESIAN_POINT('Ctrl Pts',(5.41236528359747,-4.06553879836356,14.0977638779073));
#51610=CARTESIAN_POINT('Ctrl Pts',(5.51283704096533,-3.92440017834071,14.1058864384295));
#51611=CARTESIAN_POINT('Ctrl Pts',(5.61331413814655,-3.78325405716622,14.1140094306447));
#51612=CARTESIAN_POINT('Ctrl Pts',(5.7083715868624,-3.63824019427199,14.1221324228599));
#51613=CARTESIAN_POINT('Ctrl Pts',(5.79770874095827,-3.48982268246054,14.1302554150751));
#51614=CARTESIAN_POINT('Ctrl Pts',(5.84331263561209,-3.41406006564192,14.1344019550561));
#51615=CARTESIAN_POINT('Ctrl Pts',(5.88742664052992,-3.33741099064498,14.1385484950372));
#51616=CARTESIAN_POINT('Ctrl Pts',(5.93001527222362,-3.25993985699041,14.1426950350183));
#51617=CARTESIAN_POINT('Ctrl Pts',(6.02228539318372,-3.0920952799532,14.1516786940467));
#51618=CARTESIAN_POINT('Ctrl Pts',(6.10734731431897,-2.92047372197738,14.160662353075));
#51619=CARTESIAN_POINT('Ctrl Pts',(6.18493844514299,-2.74569215859904,14.1696460121034));
#51620=CARTESIAN_POINT('Ctrl Pts',(6.26266287670776,-2.57061032234645,14.1786451049628));
#51621=CARTESIAN_POINT('Ctrl Pts',(6.33289076787979,-2.39235784854027,14.1876441978222));
#51622=CARTESIAN_POINT('Ctrl Pts',(6.39540817182099,-2.21157032802606,14.1966432906816));
#51623=CARTESIAN_POINT('Ctrl Pts',(6.45807216160402,-2.03035891129711,14.205663483899));
#51624=CARTESIAN_POINT('Ctrl Pts',(6.51298941293532,-1.84660078194002,14.2146836771164));
#51625=CARTESIAN_POINT('Ctrl Pts',(6.55999549279584,-1.66094796260998,14.2237038703338));
#51626=CARTESIAN_POINT('Ctrl Pts',(6.60704917808271,-1.47510712331225,14.2327331987555));
#51627=CARTESIAN_POINT('Ctrl Pts',(6.6461756330223,-1.28736799376254,14.2417625271772));
#51628=CARTESIAN_POINT('Ctrl Pts',(6.67726155662699,-1.09839296446732,14.2507918555988));
#51629=CARTESIAN_POINT('Ctrl Pts',(6.70839130511806,-0.90915151847199,14.2598339135536));
#51630=CARTESIAN_POINT('Ctrl Pts',(6.73145781792007,-0.718670924939345,
14.2688759715084));
#51631=CARTESIAN_POINT('Ctrl Pts',(6.74639940128629,-0.527621188281867,
14.2779180294631));
#51632=CARTESIAN_POINT('Ctrl Pts',(6.75936609995866,-0.361823206504845,
14.2857649649587));
#51633=CARTESIAN_POINT('Ctrl Pts',(6.76621454360319,-0.19559675795372,14.2936119004544));
#51634=CARTESIAN_POINT('Ctrl Pts',(6.76693621826582,-0.0293805704898146,
14.30145883595));
#51635=CARTESIAN_POINT('Ctrl Pts',(6.76773206856092,0.153919756782495,14.3101123002508));
#51636=CARTESIAN_POINT('Ctrl Pts',(6.7610763336698,0.337369176667206,14.3187657645516));
#51637=CARTESIAN_POINT('Ctrl Pts',(6.74696391042136,0.520352756763833,14.3274192288524));
#51638=CARTESIAN_POINT('Ctrl Pts',(6.73286448760132,0.703167771555361,14.3360647215426));
#51639=CARTESIAN_POINT('Ctrl Pts',(6.71132210038471,0.885517500421605,14.3447102142328));
#51640=CARTESIAN_POINT('Ctrl Pts',(6.68238366679435,1.06678841845987,14.353355706923));
#51641=CARTESIAN_POINT('Ctrl Pts',(6.65257467010642,1.25351256088969,14.3622612844195));
#51642=CARTESIAN_POINT('Ctrl Pts',(6.61491767142006,1.43909164593957,14.371166861916));
#51643=CARTESIAN_POINT('Ctrl Pts',(6.56952165561464,1.62285988810197,14.3800724394126));
#51644=CARTESIAN_POINT('Ctrl Pts',(6.52553503900052,1.80092272182056,14.3887015275851));
#51645=CARTESIAN_POINT('Ctrl Pts',(6.47428280818188,1.97728514116082,14.3973306157577));
#51646=CARTESIAN_POINT('Ctrl Pts',(6.4159161540952,2.15135048367771,14.4059597039302));
#51647=CARTESIAN_POINT('Ctrl Pts',(6.35474426327739,2.33378181016412,14.4150035260888));
#51648=CARTESIAN_POINT('Ctrl Pts',(6.28575726983507,2.51368947601402,14.4240473482473));
#51649=CARTESIAN_POINT('Ctrl Pts',(6.20918863901788,2.69040246897956,14.4330911704058));
#51650=CARTESIAN_POINT('Ctrl Pts',(6.13262000820066,2.86711546194517,14.4421349925643));
#51651=CARTESIAN_POINT('Ctrl Pts',(6.04846986142122,3.04063341469961,14.4511788147229));
#51652=CARTESIAN_POINT('Ctrl Pts',(5.9570309314573,3.21030706968367,14.4602226368814));
#51653=CARTESIAN_POINT('Ctrl Pts',(5.87184071050187,3.3683856491696,14.4686484267312));
#51654=CARTESIAN_POINT('Ctrl Pts',(5.78036136009623,3.5230582739114,14.477074216581));
#51655=CARTESIAN_POINT('Ctrl Pts',(5.68289859464026,3.67381988712509,14.4855000064308));
#51656=CARTESIAN_POINT('Ctrl Pts',(5.58541321454388,3.82461648210493,14.4939277513473));
#51657=CARTESIAN_POINT('Ctrl Pts',(5.48194183119702,3.97149997776411,14.5023554962638));
#51658=CARTESIAN_POINT('Ctrl Pts',(5.37283341293857,4.11399442352696,14.5107832411803));
#51659=CARTESIAN_POINT('Ctrl Pts',(5.26368490281046,4.25654122884956,14.5192140828703));
#51660=CARTESIAN_POINT('Ctrl Pts',(5.14889542917268,4.39469550550699,14.5276449245602));
#51661=CARTESIAN_POINT('Ctrl Pts',(5.02885438368019,4.52801419915403,14.5360757662501));
#51662=CARTESIAN_POINT('Ctrl Pts',(4.90870303578885,4.66145539566383,14.5445143548075));
#51663=CARTESIAN_POINT('Ctrl Pts',(4.78329069707587,4.79005188537434,14.5529529433648));
#51664=CARTESIAN_POINT('Ctrl Pts',(4.65304455351723,4.91339652205922,14.5613915319221));
#51665=CARTESIAN_POINT('Ctrl Pts',(4.52273011463673,5.03680583522075,14.5698345453024));
#51666=CARTESIAN_POINT('Ctrl Pts',(4.38757706164631,5.1549575811245,14.5782775586827));
#51667=CARTESIAN_POINT('Ctrl Pts',(4.24804625123498,5.26748441358572,14.5867205720629));
#51668=CARTESIAN_POINT('Ctrl Pts',(4.1083688539821,5.38012946332748,14.5951724554172));
#51669=CARTESIAN_POINT('Ctrl Pts',(3.9643047748306,5.48713759344893,14.6036243387715));
#51670=CARTESIAN_POINT('Ctrl Pts',(3.81634533099098,5.58818372233979,14.6120762221258));
#51671=CARTESIAN_POINT('Ctrl Pts',(3.77602170815514,5.61572198474927,14.6143796273549));
#51672=CARTESIAN_POINT('Ctrl Pts',(3.73540891556891,5.64281768567938,14.6166830325839));
#51673=CARTESIAN_POINT('Ctrl Pts',(3.69451722846398,5.66946482911596,14.618986437813));
#51674=CARTESIAN_POINT('Ctrl Pts',(3.54685060464839,5.76569205729348,14.6273044138501));
#51675=CARTESIAN_POINT('Ctrl Pts',(3.39527945585105,5.85623945284287,14.6356223898873));
#51676=CARTESIAN_POINT('Ctrl Pts',(3.24027485363508,5.94078343932012,14.6439403659244));
#51677=CARTESIAN_POINT('Ctrl Pts',(3.19351942856848,5.96628519841667,14.6464493914614));
#51678=CARTESIAN_POINT('Ctrl Pts',(3.14645182243516,5.99124101861392,14.6489584169983));
#51679=CARTESIAN_POINT('Ctrl Pts',(3.09908550384726,6.0156427786101,14.6514674425353));
#51680=CARTESIAN_POINT('Origin',(0.,0.,-63.6971797838103));
#51681=CARTESIAN_POINT('',(3.09908550384729,6.01564277861008,17.0455658338557));
#51682=CARTESIAN_POINT('',(3.09908550384718,6.01564277861013,16.6515258479908));
#51683=CARTESIAN_POINT('',(3.09908550384721,6.01564277861012,-63.6971797838103));
#51684=CARTESIAN_POINT('',(-6.76699962369028,-0.00225676218481283,15.6971797837776));
#51685=CARTESIAN_POINT('Ctrl Pts',(-6.76699962369006,-0.00225676287355765,
15.6971797838099));
#51686=CARTESIAN_POINT('Ctrl Pts',(-6.76698132045164,-0.0571398030595781,
15.6997530359089));
#51687=CARTESIAN_POINT('Ctrl Pts',(-6.76629528591052,-0.112013453905497,
15.7023262880079));
#51688=CARTESIAN_POINT('Ctrl Pts',(-6.7649424930389,-0.166859419502339,
15.7048995401069));
#51689=CARTESIAN_POINT('Ctrl Pts',(-6.76021966393885,-0.358335977203184,
15.7138831991354));
#51690=CARTESIAN_POINT('Ctrl Pts',(-6.74736714906962,-0.549449300788106,
15.7228668581638));
#51691=CARTESIAN_POINT('Ctrl Pts',(-6.72646848946574,-0.739534083206774,
15.7318505171923));
#51692=CARTESIAN_POINT('Ctrl Pts',(-6.70553392618607,-0.929945429267811,
15.7408496100518));
#51693=CARTESIAN_POINT('Ctrl Pts',(-6.67652561563581,-1.11932446463432,
15.7498487029113));
#51694=CARTESIAN_POINT('Ctrl Pts',(-6.63957850243178,-1.30701427308417,
15.7588477957708));
#51695=CARTESIAN_POINT('Ctrl Pts',(-6.60254475857209,-1.49514416168525,
15.7678679889883));
#51696=CARTESIAN_POINT('Ctrl Pts',(-6.55753501457225,-1.68157666299484,
15.7768881822058));
#51697=CARTESIAN_POINT('Ctrl Pts',(-6.50473527186347,-1.86566557640304,
15.7859083754233));
#51698=CARTESIAN_POINT('Ctrl Pts',(-6.45188205619393,-2.04994092593268,
15.7949377038451));
#51699=CARTESIAN_POINT('Ctrl Pts',(-6.39122315256914,-2.23186771794581,
15.8039670322669));
#51700=CARTESIAN_POINT('Ctrl Pts',(-6.32299396624546,-2.41081652201563,
15.8129963606887));
#51701=CARTESIAN_POINT('Ctrl Pts',(-6.25466859052188,-2.59001760782884,
15.8220384186436));
#51702=CARTESIAN_POINT('Ctrl Pts',(-6.17875167741203,-2.76623208745566,
15.8310804765984));
#51703=CARTESIAN_POINT('Ctrl Pts',(-6.09552706086693,-2.93884991965207,
15.8401225345533));
#51704=CARTESIAN_POINT('Ctrl Pts',(-6.02330255170285,-3.08865221037933,
15.8479694700483));
#51705=CARTESIAN_POINT('Ctrl Pts',(-5.9455752328829,-3.23574604873654,15.8558164055433));
#51706=CARTESIAN_POINT('Ctrl Pts',(-5.86255851577818,-3.37974801561844,
15.8636633410382));
#51707=CARTESIAN_POINT('Ctrl Pts',(-5.77100912069394,-3.53855088591681,
15.8723168053389));
#51708=CARTESIAN_POINT('Ctrl Pts',(-5.67294527554543,-3.69373294266671,
15.8809702696397));
#51709=CARTESIAN_POINT('Ctrl Pts',(-5.56867200572264,-3.84476021263759,
15.8896237339404));
#51710=CARTESIAN_POINT('Ctrl Pts',(-5.46449479290955,-3.9956483556015,15.8982692266305));
#51711=CARTESIAN_POINT('Ctrl Pts',(-5.35411973653381,-4.14238909634571,
15.9069147193207));
#51712=CARTESIAN_POINT('Ctrl Pts',(-5.23789610881431,-4.28447585513887,
15.9155602120108));
#51713=CARTESIAN_POINT('Ctrl Pts',(-5.11817609276777,-4.43083705016001,
15.9244657895074));
#51714=CARTESIAN_POINT('Ctrl Pts',(-4.99225027491115,-4.57225958993237,
15.933371367004));
#51715=CARTESIAN_POINT('Ctrl Pts',(-4.86054786135095,-4.70822296493239,
15.9422769445006));
#51716=CARTESIAN_POINT('Ctrl Pts',(-4.7329343809704,-4.83996511770704,15.9509060326731));
#51717=CARTESIAN_POINT('Ctrl Pts',(-4.59989783696624,-4.96658175199479,
15.9595351208455));
#51718=CARTESIAN_POINT('Ctrl Pts',(-4.4618691257133,-5.08763333044024,15.968164209018));
#51719=CARTESIAN_POINT('Ctrl Pts',(-4.31720643454498,-5.21450292843281,
15.9772080311766));
#51720=CARTESIAN_POINT('Ctrl Pts',(-4.16706008848616,-5.33525908049973,
15.9862518533353));
#51721=CARTESIAN_POINT('Ctrl Pts',(-4.0119694957848,-5.44943939913935,15.995295675494));
#51722=CARTESIAN_POINT('Ctrl Pts',(-3.85687890308344,-5.56361971777898,
16.0043394976526));
#51723=CARTESIAN_POINT('Ctrl Pts',(-3.69684435350022,-5.67122394665413,
16.0133833198112));
#51724=CARTESIAN_POINT('Ctrl Pts',(-3.53244552541382,-5.7718383215388,16.0224271419699));
#51725=CARTESIAN_POINT('Ctrl Pts',(-3.37928130427869,-5.86557696033318,
16.0308529318197));
#51726=CARTESIAN_POINT('Ctrl Pts',(-3.22239609884637,-5.95320757548475,
16.0392787216696));
#51727=CARTESIAN_POINT('Ctrl Pts',(-3.06230824364645,-6.03444754893893,
16.0477045115194));
#51728=CARTESIAN_POINT('Ctrl Pts',(-2.90218324267878,-6.11570637279985,
16.0561322564359));
#51729=CARTESIAN_POINT('Ctrl Pts',(-2.73885440588408,-6.1905714483703,16.0645600013524));
#51730=CARTESIAN_POINT('Ctrl Pts',(-2.57286280017949,-6.25880707574954,
16.072987746269));
#51731=CARTESIAN_POINT('Ctrl Pts',(-2.40681020088744,-6.32706777629853,
16.0814185879589));
#51732=CARTESIAN_POINT('Ctrl Pts',(-2.23809318823863,-6.38869404553378,
16.0898494296489));
#51733=CARTESIAN_POINT('Ctrl Pts',(-2.06727120825433,-6.44349895255076,
16.0982802713388));
#51734=CARTESIAN_POINT('Ctrl Pts',(-1.89629226467413,-6.49835421828199,
16.1067188598962));
#51735=CARTESIAN_POINT('Ctrl Pts',(-1.72320480529395,-6.54637549765692,
16.1151574484536));
#51736=CARTESIAN_POINT('Ctrl Pts',(-1.54858286775491,-6.58742590863047,
16.1235960370109));
#51737=CARTESIAN_POINT('Ctrl Pts',(-1.37386936618862,-6.62849784462546,
16.1320390503912));
#51738=CARTESIAN_POINT('Ctrl Pts',(-1.19762010586276,-6.66259155412601,
16.1404820637715));
#51739=CARTESIAN_POINT('Ctrl Pts',(-1.02041819412114,-6.68962149221513,
16.1489250771518));
#51740=CARTESIAN_POINT('Ctrl Pts',(-0.843030119420576,-6.71667982713815,
16.1573769605061));
#51741=CARTESIAN_POINT('Ctrl Pts',(-0.664687722586519,-6.73665952446968,
16.1658288438604));
#51742=CARTESIAN_POINT('Ctrl Pts',(-0.485979166360038,-6.74952689081716,
16.1742807272147));
#51743=CARTESIAN_POINT('Ctrl Pts',(-0.43727543896636,-6.7530336546571,16.1765841324436));
#51744=CARTESIAN_POINT('Ctrl Pts',(-0.388544518088214,-6.75601245986053,
16.1788875376724));
#51745=CARTESIAN_POINT('Ctrl Pts',(-0.339798300466749,-6.75846329538009,
16.1811909429013));
#51746=CARTESIAN_POINT('Ctrl Pts',(-0.16378271237999,-6.76731291031081,
16.1895082082347));
#51747=CARTESIAN_POINT('Ctrl Pts',(0.0127488507593406,-6.76929060122636,
16.1978254735681));
#51748=CARTESIAN_POINT('Ctrl Pts',(0.18922662558176,-6.76435379649608,16.2061427389015));
#51749=CARTESIAN_POINT('Ctrl Pts',(0.365555554980591,-6.75942115558072,
16.2144529892616));
#51750=CARTESIAN_POINT('Ctrl Pts',(0.541830440502447,-6.74758564794832,
16.2227632396216));
#51751=CARTESIAN_POINT('Ctrl Pts',(0.717479320325822,-6.72885669522727,
16.2310734899817));
#51752=CARTESIAN_POINT('Ctrl Pts',(0.893012221901616,-6.71014010894497,
16.2393782532116));
#51753=CARTESIAN_POINT('Ctrl Pts',(1.06791959669993,-6.68453918402528,16.2476830164414));
#51754=CARTESIAN_POINT('Ctrl Pts',(1.24163218191214,-6.65211534211788,16.2559877796713));
#51755=CARTESIAN_POINT('Ctrl Pts',(1.41526186657815,-6.61970697378254,16.2642885796339));
#51756=CARTESIAN_POINT('Ctrl Pts',(1.58769755676741,-6.58048224122146,16.2725893795965));
#51757=CARTESIAN_POINT('Ctrl Pts',(1.75837756446174,-6.53455410420616,16.2808901795591));
#51758=CARTESIAN_POINT('Ctrl Pts',(1.929007352293,-6.48863948081079,16.289188537144));
#51759=CARTESIAN_POINT('Ctrl Pts',(2.09788215184669,-6.43602547475562,16.2974868947289));
#51760=CARTESIAN_POINT('Ctrl Pts',(2.26445265911187,-6.37687565776856,16.3057852523139));
#51761=CARTESIAN_POINT('Ctrl Pts',(2.4310401145442,-6.31771982242326,16.3140844542376));
#51762=CARTESIAN_POINT('Ctrl Pts',(2.59532247894716,-6.25202695670496,16.3223836561614));
#51763=CARTESIAN_POINT('Ctrl Pts',(2.75676719261827,-6.18001000368961,16.3306828580852));
#51764=CARTESIAN_POINT('Ctrl Pts',(2.91822827372315,-6.1079857495203,16.3389829013907));
#51765=CARTESIAN_POINT('Ctrl Pts',(3.07685081263101,-6.02963627140844,16.3472829446963));
#51766=CARTESIAN_POINT('Ctrl Pts',(3.23212385080766,-5.94522198181365,16.3555829880018));
#51767=CARTESIAN_POINT('Ctrl Pts',(3.38743840639054,-5.86078512125359,16.3638852505997));
#51768=CARTESIAN_POINT('Ctrl Pts',(3.5394013705374,-5.77028038332949,16.3721875131976));
#51769=CARTESIAN_POINT('Ctrl Pts',(3.687527769292,-5.67401339007059,16.3804897757955));
#51770=CARTESIAN_POINT('Ctrl Pts',(3.83571836681454,-5.57770467418553,16.3887956366381));
#51771=CARTESIAN_POINT('Ctrl Pts',(3.9800687934584,-5.47562891508982,16.3971014974808));
#51772=CARTESIAN_POINT('Ctrl Pts',(4.12012420341948,-5.3681342707124,16.4054073583234));
#51773=CARTESIAN_POINT('Ctrl Pts',(4.26034516875616,-5.2605125600815,16.4137230372795));
#51774=CARTESIAN_POINT('Ctrl Pts',(4.39626069742289,-5.14745937821396,16.4220387162356));
#51775=CARTESIAN_POINT('Ctrl Pts',(4.52744921128366,-5.02936304508305,16.4303543951918));
#51776=CARTESIAN_POINT('Ctrl Pts',(4.65872070083473,-4.91119201696189,16.4386753337486));
#51777=CARTESIAN_POINT('Ctrl Pts',(4.78525896426821,-4.78797171875699,16.4469962723055));
#51778=CARTESIAN_POINT('Ctrl Pts',(4.90668020456831,-4.66012643284466,16.4553172108623));
#51779=CARTESIAN_POINT('Ctrl Pts',(5.02828191444139,-4.53209112923774,16.4636505169112));
#51780=CARTESIAN_POINT('Ctrl Pts',(5.14475117255765,-4.3994173614894,16.4719838229601));
#51781=CARTESIAN_POINT('Ctrl Pts',(5.2557444394465,-4.26256253763241,16.4803171290091));
#51782=CARTESIAN_POINT('Ctrl Pts',(5.33744203693728,-4.16182930734253,16.4864509342608));
#51783=CARTESIAN_POINT('Ctrl Pts',(5.41617369798555,-4.05883152237425,16.4925847395126));
#51784=CARTESIAN_POINT('Ctrl Pts',(5.49181783252645,-3.95376098093253,16.4987185447643));
#51785=CARTESIAN_POINT('Ctrl Pts',(5.59135719580181,-3.81549970188449,16.5067899580063));
#51786=CARTESIAN_POINT('Ctrl Pts',(5.6858549415438,-3.6732225761573,16.5148613712484));
#51787=CARTESIAN_POINT('Ctrl Pts',(5.77496001784963,-3.52733976138368,16.5229327844904));
#51788=CARTESIAN_POINT('Ctrl Pts',(5.86395323011254,-3.38164009040082,16.5309940647416));
#51789=CARTESIAN_POINT('Ctrl Pts',(5.94756705165948,-3.2323440514801,16.5390553449929));
#51790=CARTESIAN_POINT('Ctrl Pts',(6.02549066639004,-3.07989467827174,16.5471166252441));
#51791=CARTESIAN_POINT('Ctrl Pts',(6.10333354348565,-2.92760325977174,16.5551695531017));
#51792=CARTESIAN_POINT('Ctrl Pts',(6.17549777806015,-2.77216533810599,16.5632224809594));
#51793=CARTESIAN_POINT('Ctrl Pts',(6.24171593266433,-2.61405264214863,16.571275408817));
#51794=CARTESIAN_POINT('Ctrl Pts',(6.30787997806362,-2.4560691456882,16.5793217563414));
#51795=CARTESIAN_POINT('Ctrl Pts',(6.36810747072865,-2.29541556739407,16.5873681038658));
#51796=CARTESIAN_POINT('Ctrl Pts',(6.42217705079707,-2.13258784771353,16.5954144513901));
#51797=CARTESIAN_POINT('Ctrl Pts',(6.47621427632177,-1.96985756205353,16.6034559840833));
#51798=CARTESIAN_POINT('Ctrl Pts',(6.52410080741377,-1.80495607794764,16.6114975167765));
#51799=CARTESIAN_POINT('Ctrl Pts',(6.5656635874515,-1.63839880871953,16.6195390494696));
#51800=CARTESIAN_POINT('Ctrl Pts',(6.608025401025,-1.46863951971262,16.6277351785179));
#51801=CARTESIAN_POINT('Ctrl Pts',(6.64381769250576,-1.29716049929915,16.6359313075661));
#51802=CARTESIAN_POINT('Ctrl Pts',(6.67291058330975,-1.12452360897969,16.6441274366143));
#51803=CARTESIAN_POINT('Ctrl Pts',(6.70144486741583,-0.955201484590184,
16.6521661934504));
#51804=CARTESIAN_POINT('Ctrl Pts',(6.72353464443878,-0.784765936603242,
16.6602049502865));
#51805=CARTESIAN_POINT('Ctrl Pts',(6.73910910993699,-0.613756795778476,
16.6682437071226));
#51806=CARTESIAN_POINT('Ctrl Pts',(6.75468508287886,-0.442731103076344,
16.6762832420254));
#51807=CARTESIAN_POINT('Ctrl Pts',(6.76374445465041,-0.27113207893276,16.6843227769282));
#51808=CARTESIAN_POINT('Ctrl Pts',(6.76626839571479,-0.0995037544578944,
16.692362311831));
#51809=CARTESIAN_POINT('Ctrl Pts',(6.7687930808112,0.0721751642929305,16.7004042167066));
#51810=CARTESIAN_POINT('Ctrl Pts',(6.76477849490892,0.243883027340105,16.7084461215821));
#51811=CARTESIAN_POINT('Ctrl Pts',(6.75425793013242,0.415076876305283,16.7164880264576));
#51812=CARTESIAN_POINT('Ctrl Pts',(6.74338248269518,0.592045484507614,16.7248012031384));
#51813=CARTESIAN_POINT('Ctrl Pts',(6.72555448240518,0.76846435854144,16.7331143798192));
#51814=CARTESIAN_POINT('Ctrl Pts',(6.70086863396485,0.943741781604503,16.7414275565001));
#51815=CARTESIAN_POINT('Ctrl Pts',(6.67694686079383,1.11359402576181,16.7494834241106));
#51816=CARTESIAN_POINT('Ctrl Pts',(6.64658557937559,1.28237407680473,16.7575392917211));
#51817=CARTESIAN_POINT('Ctrl Pts',(6.60992246821841,1.44955647152551,16.7655951593317));
#51818=CARTESIAN_POINT('Ctrl Pts',(6.57150279560167,1.62474871980245,16.7740369905476));
#51819=CARTESIAN_POINT('Ctrl Pts',(6.52616270811494,1.79818598515055,16.7824788217636));
#51820=CARTESIAN_POINT('Ctrl Pts',(6.47411811650042,1.96928505138314,16.7909206529795));
#51821=CARTESIAN_POINT('Ctrl Pts',(6.42207352488591,2.14038411761566,16.7993624841955));
#51822=CARTESIAN_POINT('Ctrl Pts',(6.36332466156437,2.30914457739854,16.8078043154114));
#51823=CARTESIAN_POINT('Ctrl Pts',(6.29814318431123,2.47501139995638,16.8162461466274));
#51824=CARTESIAN_POINT('Ctrl Pts',(6.23458005286255,2.63676002992794,16.8244783814564));
#51825=CARTESIAN_POINT('Ctrl Pts',(6.16468883442206,2.79629523656879,16.8327106162853));
#51826=CARTESIAN_POINT('Ctrl Pts',(6.08864269601374,2.95308637196385,16.8409428511143));
#51827=CARTESIAN_POINT('Ctrl Pts',(6.00988326236478,3.11547175120014,16.8494688087285));
#51828=CARTESIAN_POINT('Ctrl Pts',(5.92452164224108,3.27491325502656,16.8579947663427));
#51829=CARTESIAN_POINT('Ctrl Pts',(5.83280655248278,3.43083906957379,16.866520723957));
#51830=CARTESIAN_POINT('Ctrl Pts',(5.74447415848501,3.58101392652816,16.8747322216415));
#51831=CARTESIAN_POINT('Ctrl Pts',(5.65024876378823,3.72792742854062,16.8829437193261));
#51832=CARTESIAN_POINT('Ctrl Pts',(5.55040114885524,3.87108978025393,16.8911552170106));
#51833=CARTESIAN_POINT('Ctrl Pts',(5.4506260637312,4.01414813811596,16.899360749822));
#51834=CARTESIAN_POINT('Ctrl Pts',(5.34523709463131,4.15346047881291,16.9075662826334));
#51835=CARTESIAN_POINT('Ctrl Pts',(5.23454974979036,4.28856361932171,16.9157718154448));
#51836=CARTESIAN_POINT('Ctrl Pts',(5.12392269914392,4.42359316573496,16.923972878495));
#51837=CARTESIAN_POINT('Ctrl Pts',(5.008003247532,4.55441780195135,16.9321739415453));
#51838=CARTESIAN_POINT('Ctrl Pts',(4.88714885980716,4.68060519827143,16.9403750045955));
#51839=CARTESIAN_POINT('Ctrl Pts',(4.7663383495365,4.80674678093259,16.9485730901638));
#51840=CARTESIAN_POINT('Ctrl Pts',(4.64059672034411,4.92825421936213,16.956771175732));
#51841=CARTESIAN_POINT('Ctrl Pts',(4.51032021251044,5.04472998094247,16.9649692613002));
#51842=CARTESIAN_POINT('Ctrl Pts',(4.38004966843678,5.16120041052934,16.9731669715789));
#51843=CARTESIAN_POINT('Ctrl Pts',(4.24524492243483,5.27263937874268,16.9813646818575));
#51844=CARTESIAN_POINT('Ctrl Pts',(4.10633760909274,5.37868761317764,16.9895623921362));
#51845=CARTESIAN_POINT('Ctrl Pts',(3.96743304694315,5.48473374722565,16.9977599400513));
#51846=CARTESIAN_POINT('Ctrl Pts',(3.82442636712194,5.58538914637848,17.0059574879665));
#51847=CARTESIAN_POINT('Ctrl Pts',(3.67778050834567,5.6803362164957,17.0141550358816));
#51848=CARTESIAN_POINT('Ctrl Pts',(3.53108214213304,5.77531728298543,17.0223555189783));
#51849=CARTESIAN_POINT('Ctrl Pts',(3.38074229823093,5.86458574775904,17.0305560020751));
#51850=CARTESIAN_POINT('Ctrl Pts',(3.22725130109749,5.94786836098149,17.0387564851718));
#51851=CARTESIAN_POINT('Ctrl Pts',(3.18476706746597,5.97091986278722,17.0410262680665));
#51852=CARTESIAN_POINT('Ctrl Pts',(3.14204156470054,5.99351305608632,17.0432960509611));
#51853=CARTESIAN_POINT('Ctrl Pts',(3.09908550384729,6.01564277861008,17.0455658338557));
#51854=CARTESIAN_POINT('Ctrl Pts',(3.09908550384722,6.01564277861011,15.0459090623666));
#51855=CARTESIAN_POINT('Ctrl Pts',(2.94791065649508,6.09352369594803,15.053887487038));
#51856=CARTESIAN_POINT('Ctrl Pts',(2.79367270731465,6.16576841633157,15.0618659117094));
#51857=CARTESIAN_POINT('Ctrl Pts',(2.63678901268786,6.23214511244472,15.0698443363808));
#51858=CARTESIAN_POINT('Ctrl Pts',(2.47534685772831,6.30045047002248,15.0780545845853));
#51859=CARTESIAN_POINT('Ctrl Pts',(2.31125754215692,6.36247497736568,15.0862648327899));
#51860=CARTESIAN_POINT('Ctrl Pts',(2.14505142902513,6.41802488050937,15.0944750809944));
#51861=CARTESIAN_POINT('Ctrl Pts',(1.97880580538659,6.47358798897253,15.1026872809386));
#51862=CARTESIAN_POINT('Ctrl Pts',(1.81044271925723,6.52267331398955,15.1108994808828));
#51863=CARTESIAN_POINT('Ctrl Pts',(1.64050790061722,6.56513692378251,15.119111680827));
#51864=CARTESIAN_POINT('Ctrl Pts',(1.47050242445597,6.6076181896005,15.1273272953375));
#51865=CARTESIAN_POINT('Ctrl Pts',(1.29892425888759,6.643472168885,15.135542909848));
#51866=CARTESIAN_POINT('Ctrl Pts',(1.12632961815818,6.67260598201779,15.1437585243584));
#51867=CARTESIAN_POINT('Ctrl Pts',(0.953541161212214,6.70177251114578,15.1519833646439));
#51868=CARTESIAN_POINT('Ctrl Pts',(0.779734300361377,6.72420374214697,15.1602082049293));
#51869=CARTESIAN_POINT('Ctrl Pts',(0.605471646608188,6.73985853598973,15.1684330452147));
#51870=CARTESIAN_POINT('Ctrl Pts',(0.431097371567741,6.75552335727211,15.1766631537963));
#51871=CARTESIAN_POINT('Ctrl Pts',(0.256267076202778,6.76440307072837,15.1848932623778));
#51872=CARTESIAN_POINT('Ctrl Pts',(0.0815436259758152,6.76650867412898,
15.1931233709594));
#51873=CARTESIAN_POINT('Ctrl Pts',(-0.0934193727826761,6.76861716434417,
15.2013647631461));
#51874=CARTESIAN_POINT('Ctrl Pts',(-0.268274879042422,6.76393300338852,
15.2096061553328));
#51875=CARTESIAN_POINT('Ctrl Pts',(-0.442463881960391,6.75251913830391,
15.2178475475195));
#51876=CARTESIAN_POINT('Ctrl Pts',(-0.518275361554963,6.74755153423326,
15.2214344107837));
#51877=CARTESIAN_POINT('Ctrl Pts',(-0.593960701927358,6.74130984104823,
15.2250212740479));
#51878=CARTESIAN_POINT('Ctrl Pts',(-0.66947444095361,6.73380226713778,15.2286081373121));
#51879=CARTESIAN_POINT('Ctrl Pts',(-0.847339440716848,6.71611893362755,
15.2370566321405));
#51880=CARTESIAN_POINT('Ctrl Pts',(-1.02465734435062,6.69136886435576,15.245505126969));
#51881=CARTESIAN_POINT('Ctrl Pts',(-1.20084374890138,6.65959933409845,15.2539536217974));
#51882=CARTESIAN_POINT('Ctrl Pts',(-1.37686921740663,6.62785882346147,15.2623943994166));
#51883=CARTESIAN_POINT('Ctrl Pts',(-1.55176492044309,6.58911169152856,15.2708351770357));
#51884=CARTESIAN_POINT('Ctrl Pts',(-1.72495236976604,6.54345690916037,15.2792759546549));
#51885=CARTESIAN_POINT('Ctrl Pts',(-1.89800825492073,6.49783680905982,15.2877103201242));
#51886=CARTESIAN_POINT('Ctrl Pts',(-2.0693581520363,6.44531960414918,15.2961446855935));
#51887=CARTESIAN_POINT('Ctrl Pts',(-2.23843415879977,6.38605523909075,15.3045790510627));
#51888=CARTESIAN_POINT('Ctrl Pts',(-2.40740768932165,6.32682679390946,15.3130083044993));
#51889=CARTESIAN_POINT('Ctrl Pts',(-2.57410976335735,6.26085945185644,15.3214375579359));
#51890=CARTESIAN_POINT('Ctrl Pts',(-2.73798764947457,6.18835298212091,15.3298668113725));
#51891=CARTESIAN_POINT('Ctrl Pts',(-2.90179134829885,6.11587933596419,15.3382922488977));
#51892=CARTESIAN_POINT('Ctrl Pts',(-3.06277310414549,6.03687259960411,15.3467176864229));
#51893=CARTESIAN_POINT('Ctrl Pts',(-3.22039981611449,5.95158080045712,15.3551431239481));
#51894=CARTESIAN_POINT('Ctrl Pts',(-3.37799190173474,5.8663077376242,15.3635667106312));
#51895=CARTESIAN_POINT('Ctrl Pts',(-3.5322301186995,5.77475252099084,15.3719902973144));
#51896=CARTESIAN_POINT('Ctrl Pts',(-3.68260517224159,5.67720953861838,15.3804138839976));
#51897=CARTESIAN_POINT('Ctrl Pts',(-3.83296339960315,5.57967747079452,15.3888365281256));
#51898=CARTESIAN_POINT('Ctrl Pts',(-3.9794590456418,5.47615915432116,15.3972591722536));
#51899=CARTESIAN_POINT('Ctrl Pts',(-4.12161079945174,5.36699295861684,15.4056818163816));
#51900=CARTESIAN_POINT('Ctrl Pts',(-4.26376646971315,5.25782375525278,15.4141046925635));
#51901=CARTESIAN_POINT('Ctrl Pts',(-4.40157774494995,5.14300656579612,15.4225275687454));
#51902=CARTESIAN_POINT('Ctrl Pts',(-4.53459518798329,5.0229210108381,15.4309504449274));
#51903=CARTESIAN_POINT('Ctrl Pts',(-4.66763484566817,4.90281540092564,15.4393747277764));
#51904=CARTESIAN_POINT('Ctrl Pts',(-4.79587882796318,4.77743989519189,15.4477990106255));
#51905=CARTESIAN_POINT('Ctrl Pts',(-4.91891319035554,4.64721228541868,15.4562232934745));
#51906=CARTESIAN_POINT('Ctrl Pts',(-5.04203064560674,4.51689672473334,15.4646532657726));
#51907=CARTESIAN_POINT('Ctrl Pts',(-5.15993122124276,4.38172275455596,15.4730832380708));
#51908=CARTESIAN_POINT('Ctrl Pts',(-5.27223937418251,4.24214344186046,15.4815132103689));
#51909=CARTESIAN_POINT('Ctrl Pts',(-5.38458767547467,4.10251423181297,15.4899461962462));
#51910=CARTESIAN_POINT('Ctrl Pts',(-5.49133936356548,3.95847680267804,15.4983791821234));
#51911=CARTESIAN_POINT('Ctrl Pts',(-5.59216083866854,3.81051520853309,15.5068121680006));
#51912=CARTESIAN_POINT('Ctrl Pts',(-5.69307506891403,3.66241749062359,15.5152529121734));
#51913=CARTESIAN_POINT('Ctrl Pts',(-5.78804800305449,3.51038867373545,15.5236936563462));
#51914=CARTESIAN_POINT('Ctrl Pts',(-5.87679023152679,3.35494047259133,15.532134400519));
#51915=CARTESIAN_POINT('Ctrl Pts',(-5.92585817974336,3.26898901052635,15.5368015134044));
#51916=CARTESIAN_POINT('Ctrl Pts',(-5.97302204020799,3.18199258788588,15.5414686262898));
#51917=CARTESIAN_POINT('Ctrl Pts',(-6.01823906458843,3.09404065284569,15.5461357391752));
#51918=CARTESIAN_POINT('Ctrl Pts',(-6.09744684373968,2.93997307449344,15.5543112361648));
#51919=CARTESIAN_POINT('Ctrl Pts',(-6.17083323312904,2.78267001192737,15.5624867331544));
#51920=CARTESIAN_POINT('Ctrl Pts',(-6.23812381222279,2.62261325844644,15.5706622301439));
#51921=CARTESIAN_POINT('Ctrl Pts',(-6.30535387216047,2.46270045527436,15.5788303743334));
#51922=CARTESIAN_POINT('Ctrl Pts',(-6.36649889697672,2.30003922375514,15.5869985185228));
#51923=CARTESIAN_POINT('Ctrl Pts',(-6.42133040351226,2.13513579168377,15.5951666627123));
#51924=CARTESIAN_POINT('Ctrl Pts',(-6.47839694748146,1.96351057925462,15.6036677561344));
#51925=CARTESIAN_POINT('Ctrl Pts',(-6.52862424305058,1.78945686915077,15.6121688495565));
#51926=CARTESIAN_POINT('Ctrl Pts',(-6.57180970945634,1.61356937957296,15.6206699429786));
#51927=CARTESIAN_POINT('Ctrl Pts',(-6.61325069369425,1.44478688652871,15.628827633698));
#51928=CARTESIAN_POINT('Ctrl Pts',(-6.64820750101947,1.27431625047136,15.6369853244174));
#51929=CARTESIAN_POINT('Ctrl Pts',(-6.67655179969668,1.10269899155074,15.6451430151368));
#51930=CARTESIAN_POINT('Ctrl Pts',(-6.70488750477797,0.931133764588747,
15.6532982325582));
#51931=CARTESIAN_POINT('Ctrl Pts',(-6.7266146365196,0.758422964707003,15.6614534499795));
#51932=CARTESIAN_POINT('Ctrl Pts',(-6.74165602440339,0.585117978381655,
15.6696086674009));
#51933=CARTESIAN_POINT('Ctrl Pts',(-6.75669650310326,0.411823467559594,
15.6777633918762));
#51934=CARTESIAN_POINT('Ctrl Pts',(-6.76505201088149,0.237935202829579,
15.6859181163516));
#51935=CARTESIAN_POINT('Ctrl Pts',(-6.76669725855707,0.0640094605216243,
15.6940728408269));
#51936=CARTESIAN_POINT('Ctrl Pts',(-6.76690620453611,0.0419209415431688,
15.6951084884771));
#51937=CARTESIAN_POINT('Ctrl Pts',(-6.76700699012752,0.0198318204418481,
15.6961441361274));
#51938=CARTESIAN_POINT('Ctrl Pts',(-6.76699962369028,-0.0022567621848848,
15.6971797837776));
#51939=CARTESIAN_POINT('',(-6.76699885577408,0.00393521947970883,15.302820216215));
#51940=CARTESIAN_POINT('Ctrl Pts',(3.09908550384726,6.0156427786101,14.6514674425353));
#51941=CARTESIAN_POINT('Ctrl Pts',(2.94223581389065,6.09644721104014,14.6597758753902));
#51942=CARTESIAN_POINT('Ctrl Pts',(2.7821086280402,6.17117268014464,14.668084308245));
#51943=CARTESIAN_POINT('Ctrl Pts',(2.61921061121263,6.239553251164,14.6763927410999));
#51944=CARTESIAN_POINT('Ctrl Pts',(2.45641114893688,6.30789245141248,14.684696147289));
#51945=CARTESIAN_POINT('Ctrl Pts',(2.29084451598339,6.36989426874963,14.6929995534781));
#51946=CARTESIAN_POINT('Ctrl Pts',(2.12303989010122,6.42533972837538,14.7013029596673));
#51947=CARTESIAN_POINT('Ctrl Pts',(1.95530607309647,6.48076179156177,14.7096028620503));
#51948=CARTESIAN_POINT('Ctrl Pts',(1.78533647498609,6.52963290194865,14.7179027644333));
#51949=CARTESIAN_POINT('Ctrl Pts',(1.6136782828608,6.5717829695923,14.7262026668164));
#51950=CARTESIAN_POINT('Ctrl Pts',(1.44206111582549,6.61392296366885,14.7345005855816));
#51951=CARTESIAN_POINT('Ctrl Pts',(1.26875649672477,6.64934503422806,14.7427985043469));
#51952=CARTESIAN_POINT('Ctrl Pts',(1.09432495510236,6.67792946149031,14.7510964231121));
#51953=CARTESIAN_POINT('Ctrl Pts',(0.919864152507174,6.70651868380361,14.7593957338571));
#51954=CARTESIAN_POINT('Ctrl Pts',(0.744276391991946,6.72826790884433,14.7676950446021));
#51955=CARTESIAN_POINT('Ctrl Pts',(0.568131141044132,6.7431087790852,14.7759943553472));
#51956=CARTESIAN_POINT('Ctrl Pts',(0.391959205880474,6.75795189756713,14.7842949233534));
#51957=CARTESIAN_POINT('Ctrl Pts',(0.215229958711135,6.76588454577244,14.7925954913597));
#51958=CARTESIAN_POINT('Ctrl Pts',(0.0385166028543294,6.76689038416499,
14.800896059366));
#51959=CARTESIAN_POINT('Ctrl Pts',(-0.138252858901103,6.76789654190786,
14.8091992627748));
#51960=CARTESIAN_POINT('Ctrl Pts',(-0.315006071414334,6.76197150467151,
14.8175024661836));
#51961=CARTESIAN_POINT('Ctrl Pts',(-0.491171025936373,6.74915105945041,
14.8258056695924));
#51962=CARTESIAN_POINT('Ctrl Pts',(-0.667421161029729,6.73632441519358,
14.834112887827));
#51963=CARTESIAN_POINT('Ctrl Pts',(-0.843082124584112,6.71659574321202,
14.8424201060617));
#51964=CARTESIAN_POINT('Ctrl Pts',(-1.01758801963393,6.69005258740897,14.8507273242963));
#51965=CARTESIAN_POINT('Ctrl Pts',(-1.19230221256526,6.66347774853229,14.8590444583906));
#51966=CARTESIAN_POINT('Ctrl Pts',(-1.36585823866266,6.63007222923399,14.8673615924849));
#51967=CARTESIAN_POINT('Ctrl Pts',(-1.53770026841016,6.58997472563676,14.8756787265792));
#51968=CARTESIAN_POINT('Ctrl Pts',(-1.70965875565764,6.54985004792485,14.8840014972028));
#51969=CARTESIAN_POINT('Ctrl Pts',(-1.8799005955692,6.50302443424873,14.8923242678264));
#51970=CARTESIAN_POINT('Ctrl Pts',(-2.04788593809083,6.44968620822516,14.90064703845));
#51971=CARTESIAN_POINT('Ctrl Pts',(-2.21610664706218,6.39627324931892,14.9089814702159));
#51972=CARTESIAN_POINT('Ctrl Pts',(-2.38206421600202,6.33632956638265,14.9173159019817));
#51973=CARTESIAN_POINT('Ctrl Pts',(-2.54523850425461,6.27009170239636,14.9256503337476));
#51974=CARTESIAN_POINT('Ctrl Pts',(-2.61613625839305,6.24131194888345,14.9292715690571));
#51975=CARTESIAN_POINT('Ctrl Pts',(-2.68650888650556,6.2113445558385,14.9328928043665));
#51976=CARTESIAN_POINT('Ctrl Pts',(-2.7563152404219,6.18021158985823,14.936514039676));
#51977=CARTESIAN_POINT('Ctrl Pts',(-2.91190742961283,6.11081896209426,14.944585452918));
#51978=CARTESIAN_POINT('Ctrl Pts',(-3.06516359421407,6.03541901204667,14.9526568661601));
#51979=CARTESIAN_POINT('Ctrl Pts',(-3.21557397391724,5.95418953496327,14.9607282794021));
#51980=CARTESIAN_POINT('Ctrl Pts',(-3.365795525847,5.87306203476021,14.9687895596533));
#51981=CARTESIAN_POINT('Ctrl Pts',(-3.51317807752925,5.78611974441354,14.9768508399045));
#51982=CARTESIAN_POINT('Ctrl Pts',(-3.65723009588752,5.69358911634257,14.9849121201558));
#51983=CARTESIAN_POINT('Ctrl Pts',(-3.80113286014219,5.6011543604163,14.9929650480134));
#51984=CARTESIAN_POINT('Ctrl Pts',(-3.94171164713815,5.50314298918696,15.001017975871));
#51985=CARTESIAN_POINT('Ctrl Pts',(-4.07849797076714,5.39982808082335,15.0090709037287));
#51986=CARTESIAN_POINT('Ctrl Pts',(-4.21517252143495,5.2965975947392,15.0171172512531));
#51987=CARTESIAN_POINT('Ctrl Pts',(-4.34806048061897,5.18807242072281,15.0251635987774));
#51988=CARTESIAN_POINT('Ctrl Pts',(-4.476720997698,5.07456974617256,15.0332099463018));
#51989=CARTESIAN_POINT('Ctrl Pts',(-4.60530452597265,4.961134990168,15.041251478995));
#51990=CARTESIAN_POINT('Ctrl Pts',(-4.72966536895888,4.84272890902312,15.0492930116881));
#51991=CARTESIAN_POINT('Ctrl Pts',(-4.84939461938599,4.7197098242869,15.0573345443813));
#51992=CARTESIAN_POINT('Ctrl Pts',(-4.97142563322307,4.5943257299397,15.0655306734295));
#51993=CARTESIAN_POINT('Ctrl Pts',(-5.08864484479072,4.46414969907813,15.0737268024778));
#51994=CARTESIAN_POINT('Ctrl Pts',(-5.20065728709588,4.32960191959683,15.081922931526));
#51995=CARTESIAN_POINT('Ctrl Pts',(-5.31051900120609,4.19763756475071,15.0899616883621));
#51996=CARTESIAN_POINT('Ctrl Pts',(-5.41537185162273,4.06146813343074,15.0980004451982));
#51997=CARTESIAN_POINT('Ctrl Pts',(-5.51488300729395,3.92152450149944,15.1060392020343));
#51998=CARTESIAN_POINT('Ctrl Pts',(-5.61440379459327,3.7815673245037,15.1140787369371));
#51999=CARTESIAN_POINT('Ctrl Pts',(-5.70858164114063,3.63783552383456,15.1221182718399));
#52000=CARTESIAN_POINT('Ctrl Pts',(-5.79712651734152,3.49078975905679,15.1301578067427));
#52001=CARTESIAN_POINT('Ctrl Pts',(-5.885697495667,3.34370064669036,15.1381997116182));
#52002=CARTESIAN_POINT('Ctrl Pts',(-5.96863200582886,3.19329594544603,15.1462416164937));
#52003=CARTESIAN_POINT('Ctrl Pts',(-6.04568559993949,3.04006161560655,15.1542835213693));
#52004=CARTESIAN_POINT('Ctrl Pts',(-6.1253383876371,2.88165834209843,15.1625966980501));
#52005=CARTESIAN_POINT('Ctrl Pts',(-6.19870636962145,2.72023159112665,15.1709098747309));
#52006=CARTESIAN_POINT('Ctrl Pts',(-6.26557363347915,2.55634036142509,15.1792230514117));
#52007=CARTESIAN_POINT('Ctrl Pts',(-6.33037122479694,2.39752188568526,15.1872789190223));
#52008=CARTESIAN_POINT('Ctrl Pts',(-6.38906446492972,2.23638959034347,15.1953347866328));
#52009=CARTESIAN_POINT('Ctrl Pts',(-6.44150791704022,2.07346684437157,15.2033906542433));
#52010=CARTESIAN_POINT('Ctrl Pts',(-6.49646398043434,1.90273832830993,15.2118324854593));
#52011=CARTESIAN_POINT('Ctrl Pts',(-6.54455652681935,1.73004404488682,15.2202743166753));
#52012=CARTESIAN_POINT('Ctrl Pts',(-6.58567866377099,1.55599663802708,15.2287161478912));
#52013=CARTESIAN_POINT('Ctrl Pts',(-6.62680080072263,1.38194923116734,15.2371579791072));
#52014=CARTESIAN_POINT('Ctrl Pts',(-6.66095252412015,1.20654916983101,15.2455998103232));
#52015=CARTESIAN_POINT('Ctrl Pts',(-6.68808929934124,1.03041279302872,15.2540416415391));
#52016=CARTESIAN_POINT('Ctrl Pts',(-6.74035652201825,0.691162489599462,
15.2703011664227));
#52017=CARTESIAN_POINT('Ctrl Pts',(-6.766798755653,0.34802710901653,15.2865606913062));
#52018=CARTESIAN_POINT('Ctrl Pts',(-6.76699885577377,0.00393522001405927,
15.3028202161898));
#52019=CARTESIAN_POINT('Ctrl Pts',(-6.76699885577408,0.00393521947970433,
15.3028202162151));
#52020=CARTESIAN_POINT('Ctrl Pts',(-6.76709797409406,-0.166508528672056,
15.3108742693703));
#52021=CARTESIAN_POINT('Ctrl Pts',(-6.76075336727106,-0.33721982332612,
15.3189283225256));
#52022=CARTESIAN_POINT('Ctrl Pts',(-6.74793081125063,-0.507660089601789,
15.3269823756808));
#52023=CARTESIAN_POINT('Ctrl Pts',(-6.73512136567371,-0.677926088946617,
15.3350281939562));
#52024=CARTESIAN_POINT('Ctrl Pts',(-6.71584717939243,-0.847921241071309,
15.3430740122315));
#52025=CARTESIAN_POINT('Ctrl Pts',(-6.69012601859959,-1.01710513480999,
15.3511198305069));
#52026=CARTESIAN_POINT('Ctrl Pts',(-6.66442548622603,-1.18615334274805,
15.3591591960208));
#52027=CARTESIAN_POINT('Ctrl Pts',(-6.63228832647834,-1.35439121892961,
15.3671985615348));
#52028=CARTESIAN_POINT('Ctrl Pts',(-6.59378425325154,-1.52128176928934,
15.3752379270487));
#52029=CARTESIAN_POINT('Ctrl Pts',(-6.5546043610467,-1.69110156301832,15.3834183985635));
#52030=CARTESIAN_POINT('Ctrl Pts',(-6.50883198403785,-1.85952590036126,
15.3915988700782));
#52031=CARTESIAN_POINT('Ctrl Pts',(-6.45659539920556,-2.02599724850693,
15.3997793415929));
#52032=CARTESIAN_POINT('Ctrl Pts',(-6.40530323508075,-2.18945884804641,
15.4078119128052));
#52033=CARTESIAN_POINT('Ctrl Pts',(-6.34777874086579,-2.35103710651839,
15.4158444840175));
#52034=CARTESIAN_POINT('Ctrl Pts',(-6.28419419467783,-2.51021758490723,
15.4238770552298));
#52035=CARTESIAN_POINT('Ctrl Pts',(-6.22061531511023,-2.66938387721793,
15.4319089105836));
#52036=CARTESIAN_POINT('Ctrl Pts',(-6.15097759710344,-2.82615246665587,
15.4399407659375));
#52037=CARTESIAN_POINT('Ctrl Pts',(-6.07550194224933,-2.98002770955652,
15.4479726212914));
#52038=CARTESIAN_POINT('Ctrl Pts',(-6.00001797688494,-3.13391989542759,
15.4560053610207));
#52039=CARTESIAN_POINT('Ctrl Pts',(-5.9186949608861,-3.28491776452564,15.46403810075));
#52040=CARTESIAN_POINT('Ctrl Pts',(-5.83180026134308,-3.43254930216578,
15.4720708404793));
#52041=CARTESIAN_POINT('Ctrl Pts',(-5.74210604203649,-3.58493714150813,
15.4803623740562));
#52042=CARTESIAN_POINT('Ctrl Pts',(-5.64647532842407,-3.73373773384368,
15.4886539076331));
#52043=CARTESIAN_POINT('Ctrl Pts',(-5.54525076988173,-3.8784639870864,15.49694544121));
#52044=CARTESIAN_POINT('Ctrl Pts',(-5.44705977048966,-4.01885299592785,
15.5049884890645));
#52045=CARTESIAN_POINT('Ctrl Pts',(-5.3436056502797,-4.15540808818343,15.513031536919));
#52046=CARTESIAN_POINT('Ctrl Pts',(-5.23524201657913,-4.28771851079854,
15.5210745847735));
#52047=CARTESIAN_POINT('Ctrl Pts',(-5.12185662689373,-4.42616042452312,
15.5294903612116));
#52048=CARTESIAN_POINT('Ctrl Pts',(-5.00309616237061,-4.55995452387688,
15.5379061376497));
#52049=CARTESIAN_POINT('Ctrl Pts',(-4.87940813424595,-4.68867414728881,
15.5463219140878));
#52050=CARTESIAN_POINT('Ctrl Pts',(-4.75572010612129,-4.81739377070075,
15.5547376905258));
#52051=CARTESIAN_POINT('Ctrl Pts',(-4.62710489635256,-4.94103864852683,
15.5631534669639));
#52052=CARTESIAN_POINT('Ctrl Pts',(-4.49404799525706,-5.0592313266272,15.571569243402));
#52053=CARTESIAN_POINT('Ctrl Pts',(-4.3527790021099,-5.18471869703139,15.5805044301843));
#52054=CARTESIAN_POINT('Ctrl Pts',(-4.20616143137451,-5.30436555192128,
15.5894396169665));
#52055=CARTESIAN_POINT('Ctrl Pts',(-4.05468105371477,-5.41773481749029,
15.5983748037488));
#52056=CARTESIAN_POINT('Ctrl Pts',(-3.9034275467992,-5.53093429097109,15.6072966083855));
#52057=CARTESIAN_POINT('Ctrl Pts',(-3.74732597137332,-5.63787478071781,
15.6162184130221));
#52058=CARTESIAN_POINT('Ctrl Pts',(-3.586895273272,-5.73815922562097,15.6251402176587));
#52059=CARTESIAN_POINT('Ctrl Pts',(-3.4268559036905,-5.83819905297992,15.634040259898));
#52060=CARTESIAN_POINT('Ctrl Pts',(-3.26250870556334,-5.93161510245008,
15.6429403021373));
#52061=CARTESIAN_POINT('Ctrl Pts',(-3.09440116547005,-6.01805370756507,
15.6518403443766));
#52062=CARTESIAN_POINT('Ctrl Pts',(-2.92655242940633,-6.10435923917661,
15.6607266848699));
#52063=CARTESIAN_POINT('Ctrl Pts',(-2.75495512773007,-6.18370863615309,
15.6696130253633));
#52064=CARTESIAN_POINT('Ctrl Pts',(-2.58018344911085,-6.25579270508018,
15.6784993658567));
#52065=CARTESIAN_POINT('Ctrl Pts',(-2.40585863116678,-6.32769246762559,
15.6873629855286));
#52066=CARTESIAN_POINT('Ctrl Pts',(-2.22837587000653,-6.39236387152424,
15.6962266052005));
#52067=CARTESIAN_POINT('Ctrl Pts',(-2.04833084499392,-6.44954492576387,
15.7050902248724));
#52068=CARTESIAN_POINT('Ctrl Pts',(-1.87741331056537,-6.50382715214573,
15.7135044980262));
#52069=CARTESIAN_POINT('Ctrl Pts',(-1.70418707205572,-6.55135946454181,
15.72191877118));
#52070=CARTESIAN_POINT('Ctrl Pts',(-1.52918061718334,-6.59195689003128,
15.7303330443337));
#52071=CARTESIAN_POINT('Ctrl Pts',(-1.3584176284331,-6.63156993011715,15.7385432925382));
#52072=CARTESIAN_POINT('Ctrl Pts',(-1.18612359201481,-6.66454125114756,
15.7467535407428));
#52073=CARTESIAN_POINT('Ctrl Pts',(-1.01285423788337,-6.69077090422335,
15.7549637889473));
#52074=CARTESIAN_POINT('Ctrl Pts',(-0.839543694171909,-6.71700679261062,
15.7631759888915));
#52075=CARTESIAN_POINT('Ctrl Pts',(-0.665257722775855,-6.73649776686892,
15.7713881888357));
#52076=CARTESIAN_POINT('Ctrl Pts',(-0.490558650524202,-6.74919559728386,
15.77960038878));
#52077=CARTESIAN_POINT('Ctrl Pts',(-0.315786939811825,-6.76189870735395,
15.7878160032905));
#52078=CARTESIAN_POINT('Ctrl Pts',(-0.140602140771924,-6.76780302070672,
15.796031617801));
#52079=CARTESIAN_POINT('Ctrl Pts',(0.0344318441392134,-6.76691240139173,
15.8042472323115));
#52080=CARTESIAN_POINT('Ctrl Pts',(0.209662384541716,-6.76602078195029,
15.8124720725969));
#52081=CARTESIAN_POINT('Ctrl Pts',(0.384741416475649,-6.75831899125156,
15.8206969128824));
#52082=CARTESIAN_POINT('Ctrl Pts',(0.559107606873107,-6.74386296449866,
15.8289217531678));
#52083=CARTESIAN_POINT('Ctrl Pts',(0.73358548487677,-6.72939767815811,15.8371518617493));
#52084=CARTESIAN_POINT('Ctrl Pts',(0.907349258729725,-6.70816957450446,
15.8453819703309));
#52085=CARTESIAN_POINT('Ctrl Pts',(1.0798462840235,-6.6802859970873,15.8536120789124));
#52086=CARTESIAN_POINT('Ctrl Pts',(1.25257980538611,-6.65236419085759,15.8618534710991));
#52087=CARTESIAN_POINT('Ctrl Pts',(1.42404276136469,-6.61776875531765,15.8700948632858));
#52088=CARTESIAN_POINT('Ctrl Pts',(1.59369521228511,-6.576657553069,15.8783362554725));
#52089=CARTESIAN_POINT('Ctrl Pts',(1.66753226919263,-6.55876491336058,15.8819231187367));
#52090=CARTESIAN_POINT('Ctrl Pts',(1.74102660014215,-6.53963868008357,15.8855099820009));
#52091=CARTESIAN_POINT('Ctrl Pts',(1.81413482365718,-6.51929473498433,15.8890968452651));
#52092=CARTESIAN_POINT('Ctrl Pts',(1.98633387413338,-6.47137662316876,15.8975453400935));
#52093=CARTESIAN_POINT('Ctrl Pts',(2.15678227119935,-6.41659023055404,15.9059938349219));
#52094=CARTESIAN_POINT('Ctrl Pts',(2.32491237193879,-6.35508233328302,15.9144423297504));
#52095=CARTESIAN_POINT('Ctrl Pts',(2.49288889559806,-6.2936306199031,15.9228831073695));
#52096=CARTESIAN_POINT('Ctrl Pts',(2.65855103235927,-6.22546975417097,15.9313238849887));
#52097=CARTESIAN_POINT('Ctrl Pts',(2.8213458302109,-6.1507964286222,15.9397646626079));
#52098=CARTESIAN_POINT('Ctrl Pts',(2.98401695881191,-6.07617982966625,15.9481990280772));
#52099=CARTESIAN_POINT('Ctrl Pts',(3.1438247887736,-5.99506077187894,15.9566333935465));
#52100=CARTESIAN_POINT('Ctrl Pts',(3.30023553719457,-5.90768435167605,15.9650677590158));
#52101=CARTESIAN_POINT('Ctrl Pts',(3.45655148573321,-5.82036088994588,15.9734970124524));
#52102=CARTESIAN_POINT('Ctrl Pts',(3.60947416737169,-5.72678778939718,15.9819262658891));
#52103=CARTESIAN_POINT('Ctrl Pts',(3.75849328831579,-5.62725663193755,15.9903555193258));
#52104=CARTESIAN_POINT('Ctrl Pts',(3.90744494850998,-5.52777053209522,15.998780956851));
#52105=CARTESIAN_POINT('Ctrl Pts',(4.05249629488894,-5.42233193849658,16.0072063943763));
#52106=CARTESIAN_POINT('Ctrl Pts',(4.19316464781808,-5.31127661078659,16.0156318319016));
#52107=CARTESIAN_POINT('Ctrl Pts',(4.3338020996922,-5.20024567894619,16.0240554185847));
#52108=CARTESIAN_POINT('Ctrl Pts',(4.47005821470849,-5.08360067739934,16.0324790052679));
#52109=CARTESIAN_POINT('Ctrl Pts',(4.60148171579809,-4.9617189581007,16.0409025919511));
#52110=CARTESIAN_POINT('Ctrl Pts',(4.7328905112872,-4.83985087672721,16.0493252360791));
#52111=CARTESIAN_POINT('Ctrl Pts',(4.85946752644858,-4.71274747241858,16.0577478802072));
#52112=CARTESIAN_POINT('Ctrl Pts',(4.98079659468887,-4.58082462907452,16.0661705243352));
#52113=CARTESIAN_POINT('Ctrl Pts',(5.10212900569004,-4.44889815109842,16.0745934005171));
#52114=CARTESIAN_POINT('Ctrl Pts',(5.21821295609764,-4.31215221501692,16.083016276699));
#52115=CARTESIAN_POINT('Ctrl Pts',(5.32867075393888,-4.17103787996663,16.091439152881));
#52116=CARTESIAN_POINT('Ctrl Pts',(5.43914699884538,-4.0298999780392,16.0998634357299));
#52117=CARTESIAN_POINT('Ctrl Pts',(5.54399501290666,-3.88439248551719,16.1082877185789));
#52118=CARTESIAN_POINT('Ctrl Pts',(5.64287861602505,-3.73499798190135,16.1167120014279));
#52119=CARTESIAN_POINT('Ctrl Pts',(5.7418290014728,-3.5855025827616,16.1251419737261));
#52120=CARTESIAN_POINT('Ctrl Pts',(5.8348067426431,-3.43211520519866,16.1335719460242));
#52121=CARTESIAN_POINT('Ctrl Pts',(5.9215195404571,-3.27534659722978,16.1420019183224));
#52122=CARTESIAN_POINT('Ctrl Pts',(6.00826333669684,-3.11852194701369,16.1504349041996));
#52123=CARTESIAN_POINT('Ctrl Pts',(6.08873756791653,-2.95831395092299,16.1588678900768));
#52124=CARTESIAN_POINT('Ctrl Pts',(6.16269657023468,-2.79525669361826,16.1673008759539));
#52125=CARTESIAN_POINT('Ctrl Pts',(6.23672361438426,-2.6320494246305,16.1757416201267));
#52126=CARTESIAN_POINT('Ctrl Pts',(6.30422332174809,-2.46598796345006,16.1841823642996));
#52127=CARTESIAN_POINT('Ctrl Pts',(6.36499830694323,-2.29762606892631,16.1926231084724));
#52128=CARTESIAN_POINT('Ctrl Pts',(6.39860241941228,-2.20453428090018,16.1972902213576));
#52129=CARTESIAN_POINT('Ctrl Pts',(6.43015147300926,-2.11073948092309,16.2019573342429));
#52130=CARTESIAN_POINT('Ctrl Pts',(6.45961868919637,-2.01633712215615,16.2066244471281));
#52131=CARTESIAN_POINT('Ctrl Pts',(6.5110216515342,-1.85166052490023,16.214765814346));
#52132=CARTESIAN_POINT('Ctrl Pts',(6.55618879668403,-1.68480712826192,16.2229071815638));
#52133=CARTESIAN_POINT('Ctrl Pts',(6.59493289321892,-1.51629454062829,16.2310485487817));
#52134=CARTESIAN_POINT('Ctrl Pts',(6.63364316910437,-1.34792905166677,16.2391828092052));
#52135=CARTESIAN_POINT('Ctrl Pts',(6.66594147538702,-1.17790760897593,16.2473170696287));
#52136=CARTESIAN_POINT('Ctrl Pts',(6.69168999992635,-1.00676409594586,16.2554513300522));
#52137=CARTESIAN_POINT('Ctrl Pts',(6.71742095975214,-0.835737330839642,
16.263580041577));
#52138=CARTESIAN_POINT('Ctrl Pts',(6.73661097929366,-0.663590379850863,
16.2717087531018));
#52139=CARTESIAN_POINT('Ctrl Pts',(6.74917307420059,-0.49086842889498,16.2798374646266));
#52140=CARTESIAN_POINT('Ctrl Pts',(6.76172917847663,-0.318228845845166,
16.2879622997191));
#52141=CARTESIAN_POINT('Ctrl Pts',(6.76766362575598,-0.145015173182179,
16.2960871348116));
#52142=CARTESIAN_POINT('Ctrl Pts',(6.76694115281663,0.0282211678854143,
16.3042119699041));
#52143=CARTESIAN_POINT('Ctrl Pts',(6.7662188821356,0.201409010953095,16.3123345304262));
#52144=CARTESIAN_POINT('Ctrl Pts',(6.75884340556819,0.374619144061783,16.3204570909483));
#52145=CARTESIAN_POINT('Ctrl Pts',(6.74483155776262,0.547299056649524,16.3285796514704));
#52146=CARTESIAN_POINT('Ctrl Pts',(6.73081896526366,0.719988146726942,16.3367026436856));
#52147=CARTESIAN_POINT('Ctrl Pts',(6.71016932262387,0.892146594810273,16.3448256359007));
#52148=CARTESIAN_POINT('Ctrl Pts',(6.68295144654538,1.06322573478871,16.3529486281159));
#52149=CARTESIAN_POINT('Ctrl Pts',(6.66905755025985,1.15055642218789,16.3570951680972));
#52150=CARTESIAN_POINT('Ctrl Pts',(6.65345294201825,1.23760596170539,16.3612417080785));
#52151=CARTESIAN_POINT('Ctrl Pts',(6.63615194183469,1.32430223320951,16.3653882480598));
#52152=CARTESIAN_POINT('Ctrl Pts',(6.59866857324288,1.5121334722041,16.3743719070882));
#52153=CARTESIAN_POINT('Ctrl Pts',(6.55323819000232,1.69821294411952,16.3833555661166));
#52154=CARTESIAN_POINT('Ctrl Pts',(6.50005716923112,1.88189951823341,16.3923392251451));
#52155=CARTESIAN_POINT('Ctrl Pts',(6.44678478402949,2.06590166393613,16.4013383180045));
#52156=CARTESIAN_POINT('Ctrl Pts',(6.38573521384414,2.24750246541374,16.410337410864));
#52157=CARTESIAN_POINT('Ctrl Pts',(6.3171540394609,2.42607787214733,16.4193365037235));
#52158=CARTESIAN_POINT('Ctrl Pts',(6.24841206138861,2.60507198830713,16.428356696941));
#52159=CARTESIAN_POINT('Ctrl Pts',(6.17210323165745,2.78102629233047,16.4373768901584));
#52160=CARTESIAN_POINT('Ctrl Pts',(6.08852159448198,2.95333604480198,16.4463970833759));
#52161=CARTESIAN_POINT('Ctrl Pts',(6.00485530996999,3.12582030404431,16.4554264117977));
#52162=CARTESIAN_POINT('Ctrl Pts',(5.91390161319471,3.29465242564326,16.4644557402194));
#52163=CARTESIAN_POINT('Ctrl Pts',(5.81600034517519,3.45925266277589,16.4734850686412));
#52164=CARTESIAN_POINT('Ctrl Pts',(5.71796105610107,3.62408495306551,16.482527126596));
#52165=CARTESIAN_POINT('Ctrl Pts',(5.61295473353225,3.7846732239533,16.4915691845509));
#52166=CARTESIAN_POINT('Ctrl Pts',(5.50136560554989,3.94046513422879,16.5006112425057));
#52167=CARTESIAN_POINT('Ctrl Pts',(5.4045256280128,4.07566544777477,16.5084581780009));
#52168=CARTESIAN_POINT('Ctrl Pts',(5.30272872096714,4.20725390885981,16.516305113496));
#52169=CARTESIAN_POINT('Ctrl Pts',(5.19625087626687,4.33488936778043,16.5241520489911));
#52170=CARTESIAN_POINT('Ctrl Pts',(5.0788151465547,4.4756600914712,16.532806531043));
#52171=CARTESIAN_POINT('Ctrl Pts',(4.95558089663504,4.61174555463093,16.5414610130948));
#52172=CARTESIAN_POINT('Ctrl Pts',(4.82694033039609,4.74267182575346,16.5501154951466));
#52173=CARTESIAN_POINT('Ctrl Pts',(4.69846128022556,4.87343371096583,16.5587591109689));
#52174=CARTESIAN_POINT('Ctrl Pts',(4.56458967290304,4.9990491156275,16.5674027267913));
#52175=CARTESIAN_POINT('Ctrl Pts',(4.42575618602506,5.1190791341667,16.5760463426136));
#52176=CARTESIAN_POINT('Ctrl Pts',(4.28703063180706,5.23901583833723,16.5846832386706));
#52177=CARTESIAN_POINT('Ctrl Pts',(4.14335111950464,5.35337561723113,16.5933201347277));
#52178=CARTESIAN_POINT('Ctrl Pts',(3.99518423232107,5.46175722179347,16.6019570307847));
#52179=CARTESIAN_POINT('Ctrl Pts',(3.84716005678295,5.57003443516951,16.6105856079409));
#52180=CARTESIAN_POINT('Ctrl Pts',(3.69465737613545,5.67234478586437,16.619214185097));
#52181=CARTESIAN_POINT('Ctrl Pts',(3.53817498594311,5.76832790060053,16.6278427622532));
#52182=CARTESIAN_POINT('Ctrl Pts',(3.39500785667449,5.85614370516579,16.6357371241658));
#52183=CARTESIAN_POINT('Ctrl Pts',(3.24850999897858,5.93866359220831,16.6436314860783));
#52184=CARTESIAN_POINT('Ctrl Pts',(3.09908550384718,6.01564277861014,16.6515258479909));
#52185=CARTESIAN_POINT('Origin',(0.,0.,-63.6971797838103));
#52186=CARTESIAN_POINT('',(3.0990855038472,6.01564277861012,19.0457563580462));
#52187=CARTESIAN_POINT('',(3.09908550384716,6.01564277861015,18.6513967904261));
#52188=CARTESIAN_POINT('',(3.09908550384721,6.01564277861012,-63.6971797838103));
#52189=CARTESIAN_POINT('',(-6.767,-4.88839462225982E-8,17.6971797861095));
#52190=CARTESIAN_POINT('Ctrl Pts',(-6.767,-4.88839462226118E-8,17.6971797861095));
#52191=CARTESIAN_POINT('Ctrl Pts',(-6.76699999865631,-0.186007298443953,
17.7059292979222));
#52192=CARTESIAN_POINT('Ctrl Pts',(-6.75932637025508,-0.3720144046447,17.7146788097349));
#52193=CARTESIAN_POINT('Ctrl Pts',(-6.7440051786071,-0.557389586304395,
17.7234283215477));
#52194=CARTESIAN_POINT('Ctrl Pts',(-6.72868405167163,-0.742763984990187,
17.7321777964049));
#52195=CARTESIAN_POINT('Ctrl Pts',(-6.70571544973541,-0.927506178846571,
17.7409272712621));
#52196=CARTESIAN_POINT('Ctrl Pts',(-6.67517738599004,-1.11098868831648,
17.7496767461193));
#52197=CARTESIAN_POINT('Ctrl Pts',(-6.64463944869275,-1.2944704380457,17.7584261847478));
#52198=CARTESIAN_POINT('Ctrl Pts',(-6.60653215935977,-1.47669223111764,
17.7671756233763));
#52199=CARTESIAN_POINT('Ctrl Pts',(-6.56098494888459,-1.65703515367352,
17.7759250620048));
#52200=CARTESIAN_POINT('Ctrl Pts',(-6.51543792322256,-1.83737734446685,
17.7846744651314));
#52201=CARTESIAN_POINT('Ctrl Pts',(-6.46245110700674,-2.0158404021336,17.7934238682581));
#52202=CARTESIAN_POINT('Ctrl Pts',(-6.40220446778367,-2.19181818422304,
17.8021732713847));
#52203=CARTESIAN_POINT('Ctrl Pts',(-6.34195806801502,-2.36779526687668,
17.8109226397362));
#52204=CARTESIAN_POINT('Ctrl Pts',(-6.27445199580558,-2.54128682258334,
17.8196720080878));
#52205=CARTESIAN_POINT('Ctrl Pts',(-6.19991553093826,-2.71170359907395,
17.8284213764393));
#52206=CARTESIAN_POINT('Ctrl Pts',(-6.12537935613118,-2.88211971238402,
17.8371707107425));
#52207=CARTESIAN_POINT('Ctrl Pts',(-6.04381295825467,-3.04946080785825,
17.8459200450456));
#52208=CARTESIAN_POINT('Ctrl Pts',(-5.95549336987747,-3.21315852726651,
17.8546693793488));
#52209=CARTESIAN_POINT('Ctrl Pts',(-5.86717411786317,-3.37685562323618,
17.8634186803304));
#52210=CARTESIAN_POINT('Ctrl Pts',(-5.77210186288949,-3.53690911869855,
17.8721679813119));
#52211=CARTESIAN_POINT('Ctrl Pts',(-5.67059950643654,-3.6927754112052,17.8809172822935));
#52212=CARTESIAN_POINT('Ctrl Pts',(-5.56909752812385,-3.84864112304235,
17.8896665506801));
#52213=CARTESIAN_POINT('Ctrl Pts',(-5.46116565265063,-4.00031942300073,
17.8984158190667));
#52214=CARTESIAN_POINT('Ctrl Pts',(-5.34717045492291,-4.14729515781063,
17.9071650874533));
#52215=CARTESIAN_POINT('Ctrl Pts',(-5.23317567241028,-4.29427035727743,
17.9159143239717));
#52216=CARTESIAN_POINT('Ctrl Pts',(-5.11311778746475,-4.43654279943404,
17.9246635604901));
#52217=CARTESIAN_POINT('Ctrl Pts',(-4.98740455625122,-4.57362928015428,
17.9334127970084));
#52218=CARTESIAN_POINT('Ctrl Pts',(-4.86169177249585,-4.71071527293492,
17.9421620023852));
#52219=CARTESIAN_POINT('Ctrl Pts',(-4.73032387643131,-4.84261513001808,
17.9509112077619));
#52220=CARTESIAN_POINT('Ctrl Pts',(-4.5937470335767,-4.96888087918248,17.9596604131386));
#52221=CARTESIAN_POINT('Ctrl Pts',(-4.45717066550651,-5.09514618940709,
17.9684095881003));
#52222=CARTESIAN_POINT('Ctrl Pts',(-4.31538559729377,-5.21577723638106,
17.977158763062));
#52223=CARTESIAN_POINT('Ctrl Pts',(-4.16887337101294,-5.3303643230514,17.9859079380237));
#52224=CARTESIAN_POINT('Ctrl Pts',(-4.02236164188988,-5.44495102089508,
17.9946570832969));
#52225=CARTESIAN_POINT('Ctrl Pts',(-3.87112301251265,-5.55349362294478,
18.0034062285702));
#52226=CARTESIAN_POINT('Ctrl Pts',(-3.71567112843293,-5.65562349041465,
18.0121553738434));
#52227=CARTESIAN_POINT('Ctrl Pts',(-3.56021975893851,-5.75775301980866,
18.0209044901548));
#52228=CARTESIAN_POINT('Ctrl Pts',(-3.40055540213499,-5.85346969976462,
18.0296536064661));
#52229=CARTESIAN_POINT('Ctrl Pts',(-3.23722031594003,-5.94244845379959,
18.0384027227775));
#52230=CARTESIAN_POINT('Ctrl Pts',(-3.07388575686353,-6.03142692068044,
18.0471518108535));
#52231=CARTESIAN_POINT('Ctrl Pts',(-2.90688074372655,-6.11366736807859,
18.0559008989296));
#52232=CARTESIAN_POINT('Ctrl Pts',(-2.73677246139464,-6.18889048978506,
18.0646499870056));
#52233=CARTESIAN_POINT('Ctrl Pts',(-2.56666471391664,-6.26411337497523,
18.0733990475727));
#52234=CARTESIAN_POINT('Ctrl Pts',(-2.39345397882551,-6.33231886274315,
18.0821481081399));
#52235=CARTESIAN_POINT('Ctrl Pts',(-2.21772851325488,-6.39327531406996,
18.0908971687071));
#52236=CARTESIAN_POINT('Ctrl Pts',(-2.04200358560971,-6.45423157879873,
18.0996462024919));
#52237=CARTESIAN_POINT('Ctrl Pts',(-1.86376421359607,-6.50793875758863,
18.1083952362767));
#52238=CARTESIAN_POINT('Ctrl Pts',(-1.68361572886822,-6.55421445159582,
18.1171442700615));
#52239=CARTESIAN_POINT('Ctrl Pts',(-1.50346778064905,-6.6004900077872,18.1258932777904));
#52240=CARTESIAN_POINT('Ctrl Pts',(-1.32141100861001,-6.63933405219776,
18.1346422855193));
#52241=CARTESIAN_POINT('Ctrl Pts',(-1.13806370527537,-6.67061466453691,
18.1433912932482));
#52242=CARTESIAN_POINT('Ctrl Pts',(-0.954716932754182,-6.70189518631477,
18.1521402756477));
#52243=CARTESIAN_POINT('Ctrl Pts',(-0.770079918855252,-6.72561227165323,
18.1608892580471));
#52244=CARTESIAN_POINT('Ctrl Pts',(-0.584779715370058,-6.74168537418439,
18.1696382404465));
#52245=CARTESIAN_POINT('Ctrl Pts',(-0.391489539276155,-6.7584515339629,
18.1787644708382));
#52246=CARTESIAN_POINT('Ctrl Pts',(-0.197478043938523,-6.76689985284623,
18.1878907012298));
#52247=CARTESIAN_POINT('Ctrl Pts',(-0.00346210017286045,-6.76699911436838,
18.1970169316215));
#52248=CARTESIAN_POINT('Ctrl Pts',(0.184490845350193,-6.76709527396796,
18.2058579673134));
#52249=CARTESIAN_POINT('Ctrl Pts',(0.372447648472862,-6.75935633534174,
18.2146990030053));
#52250=CARTESIAN_POINT('Ctrl Pts',(0.559756493915292,-6.74380913635014,
18.2235400386973));
#52251=CARTESIAN_POINT('Ctrl Pts',(0.745136176659968,-6.72842206367975,
18.2322900173106));
#52252=CARTESIAN_POINT('Ctrl Pts',(0.929880897405338,-6.70538685725295,
18.2410399959238));
#52253=CARTESIAN_POINT('Ctrl Pts',(1.11336309582729,-6.67478176548491,18.2497899745372));
#52254=CARTESIAN_POINT('Ctrl Pts',(1.29684341594623,-6.6441769870205,18.2585398635771));
#52255=CARTESIAN_POINT('Ctrl Pts',(1.47906095683791,-6.60600252545316,18.2672897526171));
#52256=CARTESIAN_POINT('Ctrl Pts',(1.6593967554288,-6.56038805316213,18.2760396416571));
#52257=CARTESIAN_POINT('Ctrl Pts',(1.83973076785883,-6.51477403266595,18.2847894440326));
#52258=CARTESIAN_POINT('Ctrl Pts',(2.01818279737779,-6.46172021920427,18.293539246408));
#52259=CARTESIAN_POINT('Ctrl Pts',(2.19414668373167,-6.40140682430584,18.3022890487835));
#52260=CARTESIAN_POINT('Ctrl Pts',(2.3701088857019,-6.34109400674686,18.3110387674031));
#52261=CARTESIAN_POINT('Ctrl Pts',(2.54358272100906,-6.27352183975383,18.3197884860226));
#52262=CARTESIAN_POINT('Ctrl Pts',(2.71397895044246,-6.19891984595343,18.3285382046421));
#52263=CARTESIAN_POINT('Ctrl Pts',(2.88437360540857,-6.12431854147813,18.3372878424139));
#52264=CARTESIAN_POINT('Ctrl Pts',(3.05169044883733,-6.04268765513703,18.3460374801857));
#52265=CARTESIAN_POINT('Ctrl Pts',(3.21536116548682,-5.95430445774141,18.3547871179576));
#52266=CARTESIAN_POINT('Ctrl Pts',(3.37903042419546,-5.86592204764285,18.3635366777896));
#52267=CARTESIAN_POINT('Ctrl Pts',(3.53905336892174,-5.7707875830414,18.3722862376217));
#52268=CARTESIAN_POINT('Ctrl Pts',(3.69488646885232,-5.66922419580422,18.3810357974537));
#52269=CARTESIAN_POINT('Ctrl Pts',(3.85071823243222,-5.56766167952644,18.3897852822537));
#52270=CARTESIAN_POINT('Ctrl Pts',(4.00235998300487,-5.4596705074294,18.3985347670537));
#52271=CARTESIAN_POINT('Ctrl Pts',(4.14929666598237,-5.34561747393766,18.4072842518537));
#52272=CARTESIAN_POINT('Ctrl Pts',(4.29623213771649,-5.23156538061946,18.4160336645291));
#52273=CARTESIAN_POINT('Ctrl Pts',(4.43846239307282,-5.11145170163255,18.4247830772044));
#52274=CARTESIAN_POINT('Ctrl Pts',(4.57550435177322,-4.98568439904737,18.4335324898798));
#52275=CARTESIAN_POINT('Ctrl Pts',(4.71254522632129,-4.85991809141961,18.4422818333377));
#52276=CARTESIAN_POINT('Ctrl Pts',(4.84439767520529,-4.72849844346986,18.4510311767956));
#52277=CARTESIAN_POINT('Ctrl Pts',(4.9706138730961,-4.59187181055662,18.4597805202535));
#52278=CARTESIAN_POINT('Ctrl Pts',(5.09682911440502,-4.4552462131251,18.4685297974008));
#52279=CARTESIAN_POINT('Ctrl Pts',(5.21740799574309,-4.31341392019921,18.4772790745482));
#52280=CARTESIAN_POINT('Ctrl Pts',(5.33194098767029,-4.16685664548249,18.4860283516956));
#52281=CARTESIAN_POINT('Ctrl Pts',(5.44647314960563,-4.02030043282958,18.4947775654391));
#52282=CARTESIAN_POINT('Ctrl Pts',(5.55495933335167,-3.8690195326974,18.5035267791826));
#52283=CARTESIAN_POINT('Ctrl Pts',(5.65703108597267,-3.71352774223364,18.5122759929262));
#52284=CARTESIAN_POINT('Ctrl Pts',(5.75910213280788,-3.55803702693411,18.5210251461724));
#52285=CARTESIAN_POINT('Ctrl Pts',(5.85475868002329,-3.39833571911875,18.5297742994185));
#52286=CARTESIAN_POINT('Ctrl Pts',(5.94367585262084,-3.23496620677433,18.5385234526647));
#52287=CARTESIAN_POINT('Ctrl Pts',(6.03259243992342,-3.07159776980548,18.5472725483198));
#52288=CARTESIAN_POINT('Ctrl Pts',(6.1147696043999,-2.90456142830587,18.5560216439749));
#52289=CARTESIAN_POINT('Ctrl Pts',(6.18992825428066,-2.73442447452074,18.5647707396301));
#52290=CARTESIAN_POINT('Ctrl Pts',(6.26508643439276,-2.56428858415288,18.5735197806002));
#52291=CARTESIAN_POINT('Ctrl Pts',(6.33322607191198,-2.39105238237964,18.5822688215703));
#52292=CARTESIAN_POINT('Ctrl Pts',(6.39411575249527,-2.21530421019144,18.5910178625404));
#52293=CARTESIAN_POINT('Ctrl Pts',(6.45500507271743,-2.03955707812706,18.5997668517314));
#52294=CARTESIAN_POINT('Ctrl Pts',(6.50864442806703,-1.86129827613362,18.6085158409224));
#52295=CARTESIAN_POINT('Ctrl Pts',(6.55485165189545,-1.68113319568781,18.6172648301134));
#52296=CARTESIAN_POINT('Ctrl Pts',(6.6019985363039,-1.49730431529977,18.6261917369453));
#52297=CARTESIAN_POINT('Ctrl Pts',(6.64140768290384,-1.3114910885858,18.6351186437773));
#52298=CARTESIAN_POINT('Ctrl Pts',(6.67293975984165,-1.12435046205555,18.6440455506092));
#52299=CARTESIAN_POINT('Ctrl Pts',(6.70384665429488,-0.940920248958837,
18.6527954647932));
#52300=CARTESIAN_POINT('Ctrl Pts',(6.72718586370259,-0.75621507152498,18.6615453789772));
#52301=CARTESIAN_POINT('Ctrl Pts',(6.74287810814659,-0.57086234652273,18.6702952931611));
#52302=CARTESIAN_POINT('Ctrl Pts',(6.75857004399123,-0.385513266616217,
18.6790450352717));
#52303=CARTESIAN_POINT('Ctrl Pts',(6.76661529162351,-0.199516950256453,
18.6877947773823));
#52304=CARTESIAN_POINT('Ctrl Pts',(6.76698652357479,-0.0135051752001907,
18.6965445194929));
#52305=CARTESIAN_POINT('Ctrl Pts',(6.76735774871896,0.172503189044874,18.7052941011635));
#52306=CARTESIAN_POINT('Ctrl Pts',(6.76005523919639,0.358526724792804,18.7140436828341));
#52307=CARTESIAN_POINT('Ctrl Pts',(6.7451037986922,0.543933584978941,18.7227932645048));
#52308=CARTESIAN_POINT('Ctrl Pts',(6.73015261247498,0.729337291853583,18.7315426973667));
#52309=CARTESIAN_POINT('Ctrl Pts',(6.70755277863699,0.914124058479703,18.7402921302286));
#52310=CARTESIAN_POINT('Ctrl Pts',(6.67738105710749,1.09766625992696,18.7490415630905));
#52311=CARTESIAN_POINT('Ctrl Pts',(6.64720980863084,1.28120558367433,18.7577908587729));
#52312=CARTESIAN_POINT('Ctrl Pts',(6.60946695651515,1.4635000985072,18.7665401544552));
#52313=CARTESIAN_POINT('Ctrl Pts',(6.56428068966336,1.64393066377894,18.7752894501375));
#52314=CARTESIAN_POINT('Ctrl Pts',(6.51909507123432,1.82435863987282,18.7840386202675));
#52315=CARTESIAN_POINT('Ctrl Pts',(6.46646632142887,2.00292244195733,18.7927877903975));
#52316=CARTESIAN_POINT('Ctrl Pts',(6.40657318212524,2.17901561767548,18.8015369605275));
#52317=CARTESIAN_POINT('Ctrl Pts',(6.34668082271735,2.35510650040452,18.8102860167305));
#52318=CARTESIAN_POINT('Ctrl Pts',(6.27952435537005,2.52872654986856,18.8190350729336));
#52319=CARTESIAN_POINT('Ctrl Pts',(6.20533185619881,2.69928611941088,18.8277841291367));
#52320=CARTESIAN_POINT('Ctrl Pts',(6.12831448027958,2.8763397384532,18.8368663053412));
#52321=CARTESIAN_POINT('Ctrl Pts',(6.04371487681997,3.0500949408034,18.8459484815458));
#52322=CARTESIAN_POINT('Ctrl Pts',(5.95184263330165,3.21991587908953,18.8550306577504));
#52323=CARTESIAN_POINT('Ctrl Pts',(5.86333279454217,3.38352159165377,18.8637804381048));
#52324=CARTESIAN_POINT('Ctrl Pts',(5.76807335265492,3.54347564110903,18.8725302184592));
#52325=CARTESIAN_POINT('Ctrl Pts',(5.66638788029581,3.69923470329158,18.8812799988136));
#52326=CARTESIAN_POINT('Ctrl Pts',(5.56470606359391,3.85498816583708,18.8900294646078));
#52327=CARTESIAN_POINT('Ctrl Pts',(5.45659883539358,4.00654670290066,18.898778930402));
#52328=CARTESIAN_POINT('Ctrl Pts',(5.34243338271291,4.15339554476511,18.9075283961963));
#52329=CARTESIAN_POINT('Ctrl Pts',(5.22827142749751,4.30023988790677,18.9162775939502));
#52330=CARTESIAN_POINT('Ctrl Pts',(5.10805179508241,4.44237459832989,18.925026791704));
#52331=CARTESIAN_POINT('Ctrl Pts',(4.98218278736586,4.57931694396395,18.9337759894579));
#52332=CARTESIAN_POINT('Ctrl Pts',(4.85631696674133,4.71625582212127,18.9425249656759));
#52333=CARTESIAN_POINT('Ctrl Pts',(4.72480225096497,4.84800238762615,18.9512739418939));
#52334=CARTESIAN_POINT('Ctrl Pts',(4.58808528082664,4.97410921229741,18.9600229181119));
#52335=CARTESIAN_POINT('Ctrl Pts',(4.45135942221465,5.10022423563771,18.968772463133));
#52336=CARTESIAN_POINT('Ctrl Pts',(4.30943084305619,5.2206985900779,18.9775220081542));
#52337=CARTESIAN_POINT('Ctrl Pts',(4.16278161356498,5.3351230761591,18.9862715531754));
#52338=CARTESIAN_POINT('Ctrl Pts',(4.01614100504849,5.44954083564103,18.9950205838426));
#52339=CARTESIAN_POINT('Ctrl Pts',(3.86478052743664,5.55790926216842,19.0037696145098));
#52340=CARTESIAN_POINT('Ctrl Pts',(3.70921422665565,5.65986031813289,19.0125186451771));
#52341=CARTESIAN_POINT('Ctrl Pts',(3.55364581327177,5.76181275860091,19.0212677946569));
#52342=CARTESIAN_POINT('Ctrl Pts',(3.39387170208419,5.85734749704611,19.0300169441366));
#52343=CARTESIAN_POINT('Ctrl Pts',(3.23043452787251,5.94614007244441,19.0387660936164));
#52344=CARTESIAN_POINT('Ctrl Pts',(3.18690766589811,5.96978745984176,19.0410961817597));
#52345=CARTESIAN_POINT('Ctrl Pts',(3.14312113868286,5.99295689073508,19.0434262699029));
#52346=CARTESIAN_POINT('Ctrl Pts',(3.0990855038472,6.01564277861012,19.0457563580462));
#52347=CARTESIAN_POINT('Ctrl Pts',(3.09908550384729,6.01564277861008,17.0455658338557));
#52348=CARTESIAN_POINT('Ctrl Pts',(2.94372784046354,6.09567856202065,17.0537748772338));
#52349=CARTESIAN_POINT('Ctrl Pts',(2.7853529842944,6.16964826932369,17.0619839206119));
#52350=CARTESIAN_POINT('Ctrl Pts',(2.62448024722065,6.23733856961033,17.0701929639901));
#52351=CARTESIAN_POINT('Ctrl Pts',(2.46352124048431,6.30506516951786,17.0784064095523));
#52352=CARTESIAN_POINT('Ctrl Pts',(2.30006201767863,6.36650552350461,17.0866198551145));
#52353=CARTESIAN_POINT('Ctrl Pts',(2.13463849340305,6.42149573716918,17.0948333006768));
#52354=CARTESIAN_POINT('Ctrl Pts',(1.96900103712844,6.47655706627146,17.1030573681794));
#52355=CARTESIAN_POINT('Ctrl Pts',(1.80139454849196,6.52515149144324,17.1112814356821));
#52356=CARTESIAN_POINT('Ctrl Pts',(1.63236758722803,6.56716567936026,17.1195055031848));
#52357=CARTESIAN_POINT('Ctrl Pts',(1.53461716767009,6.59146301314397,17.1242615849534));
#52358=CARTESIAN_POINT('Ctrl Pts',(1.43639184567715,6.61356057311733,17.1290176667219));
#52359=CARTESIAN_POINT('Ctrl Pts',(1.33779861920245,6.63344434320965,17.1337737484904));
#52360=CARTESIAN_POINT('Ctrl Pts',(1.15257285209219,6.67079971436528,17.1427089352727));
#52361=CARTESIAN_POINT('Ctrl Pts',(0.965663972667169,6.70041647862909,17.151644122055));
#52362=CARTESIAN_POINT('Ctrl Pts',(0.777711705246082,6.72216137142833,17.1605793088373));
#52363=CARTESIAN_POINT('Ctrl Pts',(0.590040932177247,6.7438736971051,17.1695011134739));
#52364=CARTESIAN_POINT('Ctrl Pts',(0.401330145213883,6.75773764608581,17.1784229181105));
#52365=CARTESIAN_POINT('Ctrl Pts',(0.212227603136763,6.76367122533812,17.1873447227472));
#52366=CARTESIAN_POINT('Ctrl Pts',(0.0235863270061176,6.76959033118346,
17.1962447649865));
#52367=CARTESIAN_POINT('Ctrl Pts',(-0.165444539324304,6.76761766664595,
17.2051448072258));
#52368=CARTESIAN_POINT('Ctrl Pts',(-0.354213909340622,6.75772310075144,
17.214044849465));
#52369=CARTESIAN_POINT('Ctrl Pts',(-0.542692666135895,6.74784376768662,
17.2229311899584));
#52370=CARTESIAN_POINT('Ctrl Pts',(-0.730910472961369,6.730066874345,17.2318175304518));
#52371=CARTESIAN_POINT('Ctrl Pts',(-0.918215547135476,6.70441415852263,
17.2407038709452));
#52372=CARTESIAN_POINT('Ctrl Pts',(-1.10504171493065,6.67882703221672,17.2495674906171));
#52373=CARTESIAN_POINT('Ctrl Pts',(-1.29095955165088,6.64540430071771,17.258431110289));
#52374=CARTESIAN_POINT('Ctrl Pts',(-1.4753224553871,6.60421930682428,17.267294729961));
#52375=CARTESIAN_POINT('Ctrl Pts',(-1.6503389710822,6.5651222109114,17.2757090031146));
#52376=CARTESIAN_POINT('Ctrl Pts',(-1.82395402431221,6.51903030575848,17.2841232762682));
#52377=CARTESIAN_POINT('Ctrl Pts',(-1.99561783376145,6.46604967979471,17.2925375494218));
#52378=CARTESIAN_POINT('Ctrl Pts',(-2.16311922783132,6.41435370068241,17.3007477976263));
#52379=CARTESIAN_POINT('Ctrl Pts',(-2.3286015770788,6.35614772948267,17.3089580458309));
#52380=CARTESIAN_POINT('Ctrl Pts',(-2.49153434258356,6.29162503807456,17.3171682940354));
#52381=CARTESIAN_POINT('Ctrl Pts',(-2.65450584045484,6.22708700833641,17.3253804939796));
#52382=CARTESIAN_POINT('Ctrl Pts',(-2.81492621613493,6.15622939780991,17.3335926939238));
#52383=CARTESIAN_POINT('Ctrl Pts',(-2.97228525510381,6.07929349203446,17.341804893868));
#52384=CARTESIAN_POINT('Ctrl Pts',(-3.12970972268787,6.00232559693188,17.3500205083785));
#52385=CARTESIAN_POINT('Ctrl Pts',(-3.28406999819524,5.91927452784803,17.358236122889));
#52386=CARTESIAN_POINT('Ctrl Pts',(-3.43488071919935,5.83042738097925,17.3664517373995));
#52387=CARTESIAN_POINT('Ctrl Pts',(-3.58586079403171,5.74148046265954,17.3746765776849));
#52388=CARTESIAN_POINT('Ctrl Pts',(-3.733283046241,5.6467246472369,17.3829014179704));
#52389=CARTESIAN_POINT('Ctrl Pts',(-3.87669053610912,5.54649073624413,17.3911262582558));
#52390=CARTESIAN_POINT('Ctrl Pts',(-4.02018988345974,5.44619262194697,17.3993563668373));
#52391=CARTESIAN_POINT('Ctrl Pts',(-4.15966905924843,5.34040963177509,17.4075864754188));
#52392=CARTESIAN_POINT('Ctrl Pts',(-4.29470450102172,5.2295126205894,17.4158165840004));
#52393=CARTESIAN_POINT('Ctrl Pts',(-4.42992507845766,5.11846356789977,17.4240579761871));
#52394=CARTESIAN_POINT('Ctrl Pts',(-4.5606894875852,5.00228672537704,17.4322993683738));
#52395=CARTESIAN_POINT('Ctrl Pts',(-4.68661056628652,4.88139021181175,17.4405407605605));
#52396=CARTESIAN_POINT('Ctrl Pts',(-4.74141461894764,4.8287729775543,17.4441276238248));
#52397=CARTESIAN_POINT('Ctrl Pts',(-4.79530175147435,4.77526217089232,17.4477144870891));
#52398=CARTESIAN_POINT('Ctrl Pts',(-4.84824246668574,4.72089334599131,17.4513013503535));
#52399=CARTESIAN_POINT('Ctrl Pts',(-4.97142674868588,4.59438608911196,17.4596473875025));
#52400=CARTESIAN_POINT('Ctrl Pts',(-5.08978376569604,4.46292358682828,17.4679934246516));
#52401=CARTESIAN_POINT('Ctrl Pts',(-5.20290147465994,4.32690481117639,17.4763394618006));
#52402=CARTESIAN_POINT('Ctrl Pts',(-5.31590899936957,4.19101852695755,17.4846773693483));
#52403=CARTESIAN_POINT('Ctrl Pts',(-5.42368716556202,4.05058507736566,17.493015276896));
#52404=CARTESIAN_POINT('Ctrl Pts',(-5.52586131619716,3.90603964574808,17.5013531844437));
#52405=CARTESIAN_POINT('Ctrl Pts',(-5.62793962359984,3.7616298032332,17.5096832707176));
#52406=CARTESIAN_POINT('Ctrl Pts',(-5.72442419844025,3.6131159509024,17.5180133569914));
#52407=CARTESIAN_POINT('Ctrl Pts',(-5.81498115372413,3.46096564297208,17.5263434432652));
#52408=CARTESIAN_POINT('Ctrl Pts',(-5.90548912695851,3.30889763279453,17.5346690238145));
#52409=CARTESIAN_POINT('Ctrl Pts',(-5.99007569229831,3.15319738202128,17.5429946043638));
#52410=CARTESIAN_POINT('Ctrl Pts',(-6.06845038561592,2.99436118685071,17.5513201849131));
#52411=CARTESIAN_POINT('Ctrl Pts',(-6.14679541776859,2.8355851037697,17.5596426146185));
#52412=CARTESIAN_POINT('Ctrl Pts',(-6.21893310991805,2.6736757507284,17.567965044324));
#52413=CARTESIAN_POINT('Ctrl Pts',(-6.28461895029311,2.50915397088675,17.5762874740295));
#52414=CARTESIAN_POINT('Ctrl Pts',(-6.35029059907227,2.34466773640165,17.5846081056524));
#52415=CARTESIAN_POINT('Ctrl Pts',(-6.40951304675221,2.17757052097107,17.5929287372754));
#52416=CARTESIAN_POINT('Ctrl Pts',(-6.46208984800146,2.00840329524636,17.6012493688984));
#52417=CARTESIAN_POINT('Ctrl Pts',(-6.51467647471934,1.83920445582076,17.6095715554677));
#52418=CARTESIAN_POINT('Ctrl Pts',(-6.56061486540809,1.66793516159074,17.617893742037));
#52419=CARTESIAN_POINT('Ctrl Pts',(-6.59975822020709,1.49515231157531,17.6262159286064));
#52420=CARTESIAN_POINT('Ctrl Pts',(-6.63890425509947,1.32235763134818,17.6345386849847));
#52421=CARTESIAN_POINT('Ctrl Pts',(-6.6712542550039,1.14804952700332,17.642861441363));
#52422=CARTESIAN_POINT('Ctrl Pts',(-6.69671245309473,0.97279562116923,17.6511841977414));
#52423=CARTESIAN_POINT('Ctrl Pts',(-6.72218643939624,0.797433029497346,
17.6595121155782));
#52424=CARTESIAN_POINT('Ctrl Pts',(-6.74076003656308,0.621123807099775,
17.667840033415));
#52425=CARTESIAN_POINT('Ctrl Pts',(-6.75238922133331,0.444442126290663,
17.6761679512518));
#52426=CARTESIAN_POINT('Ctrl Pts',(-6.76213058743735,0.296441989510258,
17.6831439601583));
#52427=CARTESIAN_POINT('Ctrl Pts',(-6.76700008639309,0.148180702939684,
17.6901199690648));
#52428=CARTESIAN_POINT('Ctrl Pts',(-6.76699999999885,-3.9452790698771E-6,
17.6970959779713));
#52429=CARTESIAN_POINT('',(-6.767,3.26333198744783E-12,17.3028202161898));
#52430=CARTESIAN_POINT('Ctrl Pts',(3.09908550384718,6.01564277861014,16.6515258479909));
#52431=CARTESIAN_POINT('Ctrl Pts',(2.93597037955409,6.09967498194382,16.6601435101984));
#52432=CARTESIAN_POINT('Ctrl Pts',(2.76936763087946,6.17710392388078,16.668761172406));
#52433=CARTESIAN_POINT('Ctrl Pts',(2.59982817764029,6.24765415550089,16.6773788346136));
#52434=CARTESIAN_POINT('Ctrl Pts',(2.56351738067913,6.26276412009602,16.6792245063833));
#52435=CARTESIAN_POINT('Ctrl Pts',(2.52707196505644,6.27755872568492,16.6810701781531));
#52436=CARTESIAN_POINT('Ctrl Pts',(2.49049748311316,6.292035543972,16.6829158499228));
#52437=CARTESIAN_POINT('Ctrl Pts',(2.32352906339011,6.3581245585959,16.6913416397726));
#52438=CARTESIAN_POINT('Ctrl Pts',(2.15394204162623,6.41755800409971,16.6997674296224));
#52439=CARTESIAN_POINT('Ctrl Pts',(1.98229553397733,6.47014632106366,16.7081932194722));
#52440=CARTESIAN_POINT('Ctrl Pts',(1.81060919856209,6.52274684028694,16.7166209643889));
#52441=CARTESIAN_POINT('Ctrl Pts',(1.63686274142149,6.56849896702093,16.7250487093055));
#52442=CARTESIAN_POINT('Ctrl Pts',(1.46162962989451,6.60726326288082,16.7334764542221));
#52443=CARTESIAN_POINT('Ctrl Pts',(1.28633212899157,6.64604180267438,16.7419072959121));
#52444=CARTESIAN_POINT('Ctrl Pts',(1.10954720801154,6.67782732030957,16.7503381376021));
#52445=CARTESIAN_POINT('Ctrl Pts',(0.931858079315654,6.7025315754582,16.7587689792921));
#52446=CARTESIAN_POINT('Ctrl Pts',(0.754005676991051,6.72725853066401,16.7672075678495));
#52447=CARTESIAN_POINT('Ctrl Pts',(0.575247735563395,6.74489117777599,16.7756461564068));
#52448=CARTESIAN_POINT('Ctrl Pts',(0.396173261575324,6.75539308603228,16.7840847449642));
#52449=CARTESIAN_POINT('Ctrl Pts',(0.217004888846535,6.76590050102518,16.7925277583445));
#52450=CARTESIAN_POINT('Ctrl Pts',(0.0375199835359462,6.76926970846292,
16.8009707717248));
#52451=CARTESIAN_POINT('Ctrl Pts',(-0.141692314662265,6.76551640955557,
16.8094137851052));
#52452=CARTESIAN_POINT('Ctrl Pts',(-0.321092887870196,6.76175916754612,
16.8178656684595));
#52453=CARTESIAN_POINT('Ctrl Pts',(-0.500219950993989,6.7508644867019,16.8263175518138));
#52454=CARTESIAN_POINT('Ctrl Pts',(-0.678488274244354,6.73290001869276,
16.8347694351681));
#52455=CARTESIAN_POINT('Ctrl Pts',(-0.727072024240753,6.72800413362097,
16.8370728403968));
#52456=CARTESIAN_POINT('Ctrl Pts',(-0.775592041482276,6.72258344578304,
16.8393762456255));
#52457=CARTESIAN_POINT('Ctrl Pts',(-0.824036603510481,6.71663998410477,
16.8416796508542));
#52458=CARTESIAN_POINT('Ctrl Pts',(-0.998962956602453,6.69517899792604,
16.8499969161876));
#52459=CARTESIAN_POINT('Ctrl Pts',(-1.17321938694986,6.66685938408274,16.858314181521));
#52460=CARTESIAN_POINT('Ctrl Pts',(-1.34623726940326,6.63173689273554,16.8666314468543));
#52461=CARTESIAN_POINT('Ctrl Pts',(-1.51910922458655,6.59664402450712,16.8749416972144));
#52462=CARTESIAN_POINT('Ctrl Pts',(-1.69074437399089,6.55475977931087,16.8832519475745));
#52463=CARTESIAN_POINT('Ctrl Pts',(-1.86058084131076,6.50619150755243,16.8915621979346));
#52464=CARTESIAN_POINT('Ctrl Pts',(-2.03030516822879,6.4576553046753,16.8998669611645));
#52465=CARTESIAN_POINT('Ctrl Pts',(-2.19823284627887,6.40244396471579,16.9081717243943));
#52466=CARTESIAN_POINT('Ctrl Pts',(-2.36381357409787,6.3407156052697,16.9164764876242));
#52467=CARTESIAN_POINT('Ctrl Pts',(-2.52931528212255,6.27901670433808,16.9247772875867));
#52468=CARTESIAN_POINT('Ctrl Pts',(-2.69247194678431,6.210807103314,16.9330780875493));
#52469=CARTESIAN_POINT('Ctrl Pts',(-2.85274956603841,6.13629439592558,16.9413788875119));
#52470=CARTESIAN_POINT('Ctrl Pts',(-3.01298002616589,6.06180361270985,16.9496772450968));
#52471=CARTESIAN_POINT('Ctrl Pts',(-3.17033281439747,5.98101356633595,16.9579756026817));
#52472=CARTESIAN_POINT('Ctrl Pts',(-3.32429480720481,5.89417958962833,16.9662739602666));
#52473=CARTESIAN_POINT('Ctrl Pts',(-3.47827246529225,5.80733677776248,16.9745731621904));
#52474=CARTESIAN_POINT('Ctrl Pts',(-3.62885833195818,5.71444897113201,16.9828723641142));
#52475=CARTESIAN_POINT('Ctrl Pts',(-3.77556424520675,5.61581727180616,16.9911715660379));
#52476=CARTESIAN_POINT('Ctrl Pts',(-3.92228503165374,5.51717557309581,16.9994716093435));
#52477=CARTESIAN_POINT('Ctrl Pts',(-4.0651247915311,5.41278901472721,17.007771652649));
#52478=CARTESIAN_POINT('Ctrl Pts',(-4.20362478320096,5.30300176146102,17.0160716959545));
#52479=CARTESIAN_POINT('Ctrl Pts',(-4.34216180744667,5.19318515292387,17.0243739585525));
#52480=CARTESIAN_POINT('Ctrl Pts',(-4.47635647806641,5.07796518748133,17.0326762211504));
#52481=CARTESIAN_POINT('Ctrl Pts',(-4.60578340481018,4.95772611465934,17.0409784837484));
#52482=CARTESIAN_POINT('Ctrl Pts',(-4.7352664258707,4.83743492958523,17.049284344591));
#52483=CARTESIAN_POINT('Ctrl Pts',(-4.85997733003502,4.71212053835371,17.0575902054336));
#52484=CARTESIAN_POINT('Ctrl Pts',(-4.97952770222746,4.58220393072474,17.0658960662762));
#52485=CARTESIAN_POINT('Ctrl Pts',(-5.09921939139417,4.45213375249988,17.0742117452323));
#52486=CARTESIAN_POINT('Ctrl Pts',(-5.2137381249279,4.317450744912,17.0825274241885));
#52487=CARTESIAN_POINT('Ctrl Pts',(-5.32273514893061,4.17860976095384,17.0908431031446));
#52488=CARTESIAN_POINT('Ctrl Pts',(-5.43180111268308,4.03968096117887,17.0991640417014));
#52489=CARTESIAN_POINT('Ctrl Pts',(-5.53533819844516,3.89658922181437,17.1074849802583));
#52490=CARTESIAN_POINT('Ctrl Pts',(-5.63304104004112,3.74981834776199,17.1158059188151));
#52491=CARTESIAN_POINT('Ctrl Pts',(-5.73088909832283,3.60282932672896,17.124139224864));
#52492=CARTESIAN_POINT('Ctrl Pts',(-5.82288540163198,3.45215053952877,17.1324725309129));
#52493=CARTESIAN_POINT('Ctrl Pts',(-5.90876992487993,3.29829152362772,17.1408058369619));
#52494=CARTESIAN_POINT('Ctrl Pts',(-5.97198600462747,3.18504220406173,17.1469396422137));
#52495=CARTESIAN_POINT('Ctrl Pts',(-6.03189179053176,3.07007040327827,17.1530734474655));
#52496=CARTESIAN_POINT('Ctrl Pts',(-6.08840037876368,2.95358592694884,17.1592072527174));
#52497=CARTESIAN_POINT('Ctrl Pts',(-6.16789901937184,2.7897107035556,17.1678365459723));
#52498=CARTESIAN_POINT('Ctrl Pts',(-6.2408922449539,2.62238745399539,17.1764658392272));
#52499=CARTESIAN_POINT('Ctrl Pts',(-6.30708074887625,2.45214628991718,17.1850951324822));
#52500=CARTESIAN_POINT('Ctrl Pts',(-6.37313275158236,2.28225621590106,17.193706629459));
#52501=CARTESIAN_POINT('Ctrl Pts',(-6.4324078944947,2.10946050270718,17.2023181264358));
#52502=CARTESIAN_POINT('Ctrl Pts',(-6.48465262896137,1.93431364615575,17.2109296234126));
#52503=CARTESIAN_POINT('Ctrl Pts',(-6.53674933660995,1.75966303926738,17.2195167211363));
#52504=CARTESIAN_POINT('Ctrl Pts',(-6.58185527279857,1.58267486333834,17.2281038188601));
#52505=CARTESIAN_POINT('Ctrl Pts',(-6.61976514174731,1.40392252923987,17.2366909165839));
#52506=CARTESIAN_POINT('Ctrl Pts',(-6.6576116461526,1.2254689711687,17.2452636613821));
#52507=CARTESIAN_POINT('Ctrl Pts',(-6.68828598970659,1.04525742598236,17.2538364061803));
#52508=CARTESIAN_POINT('Ctrl Pts',(-6.71163198982137,0.863877904108215,
17.2624091509785));
#52509=CARTESIAN_POINT('Ctrl Pts',(-6.73492455131497,0.682913557061215,
17.2709622729009));
#52510=CARTESIAN_POINT('Ctrl Pts',(-6.75092218215173,0.50078686477468,17.2795153948233));
#52511=CARTESIAN_POINT('Ctrl Pts',(-6.75951936688239,0.318098929174461,
17.2880685167456));
#52512=CARTESIAN_POINT('Ctrl Pts',(-6.76446193196228,0.213070708971655,
17.2929857498937));
#52513=CARTESIAN_POINT('Ctrl Pts',(-6.76695945626195,0.107857245431671,
17.2979029830418));
#52514=CARTESIAN_POINT('Ctrl Pts',(-6.76699951028476,0.00257445253156413,
17.3028202161898));
#52515=CARTESIAN_POINT('Ctrl Pts',(-6.767,3.26333214810868E-12,17.3028202161898));
#52516=CARTESIAN_POINT('Ctrl Pts',(-6.76700000000009,-0.186007249556681,
17.3115697280026));
#52517=CARTESIAN_POINT('Ctrl Pts',(-6.75932637294265,-0.372014355812802,
17.3203192398153));
#52518=CARTESIAN_POINT('Ctrl Pts',(-6.7440051826339,-0.557389537583119,
17.329068751628));
#52519=CARTESIAN_POINT('Ctrl Pts',(-6.72868405703764,-0.742763936379661,
17.3378182264852));
#52520=CARTESIAN_POINT('Ctrl Pts',(-6.70571545643605,-0.927506130402047,
17.3465677013424));
#52521=CARTESIAN_POINT('Ctrl Pts',(-6.67517739401622,-1.11098864009264,
17.3553171761996));
#52522=CARTESIAN_POINT('Ctrl Pts',(-6.64463945804443,-1.29447039004266,
17.3640666148282));
#52523=CARTESIAN_POINT('Ctrl Pts',(-6.60653217002784,-1.47669218339009,
17.3728160534567));
#52524=CARTESIAN_POINT('Ctrl Pts',(-6.56098496085546,-1.65703510627521,
17.3815654920852));
#52525=CARTESIAN_POINT('Ctrl Pts',(-6.51543793649627,-1.83737729739757,
17.3903148952118));
#52526=CARTESIAN_POINT('Ctrl Pts',(-6.46245112156971,-2.01584035544712,
17.3990642983385));
#52527=CARTESIAN_POINT('Ctrl Pts',(-6.40220448361796,-2.1918181379718,17.4078137014651));
#52528=CARTESIAN_POINT('Ctrl Pts',(-6.34195808512052,-2.36779522106091,
17.4165630698166));
#52529=CARTESIAN_POINT('Ctrl Pts',(-6.27445201416433,-2.5412867772555,17.4253124381682));
#52530=CARTESIAN_POINT('Ctrl Pts',(-6.19991555052802,-2.7117035542848,17.4340618065197));
#52531=CARTESIAN_POINT('Ctrl Pts',(-6.12537937695198,-2.88211966813351,
17.4428111408229));
#52532=CARTESIAN_POINT('Ctrl Pts',(-6.04381298028428,-3.04946076419717,
17.4515604751261));
#52533=CARTESIAN_POINT('Ctrl Pts',(-5.95549339308955,-3.21315848424362,
17.4603098094292));
#52534=CARTESIAN_POINT('Ctrl Pts',(-5.86717414225774,-3.37685558085143,
17.4690591104108));
#52535=CARTESIAN_POINT('Ctrl Pts',(-5.77210188844023,-3.53690907700072,
17.4778084113924));
#52536=CARTESIAN_POINT('Ctrl Pts',(-5.67059953311319,-3.69277537024073,
17.4865577123739));
#52537=CARTESIAN_POINT('Ctrl Pts',(-5.56909755592633,-3.84864108281135,
17.4953069807606));
#52538=CARTESIAN_POINT('Ctrl Pts',(-5.46116568154869,-4.00031938354963,
17.5040562491472));
#52539=CARTESIAN_POINT('Ctrl Pts',(-5.34717048488254,-4.14729511918322,
17.5128055175338));
#52540=CARTESIAN_POINT('Ctrl Pts',(-5.23317570343161,-4.29427031947356,
17.5215547540522));
#52541=CARTESIAN_POINT('Ctrl Pts',(-5.1131178195138,-4.4365427624975,17.5303039905705));
#52542=CARTESIAN_POINT('Ctrl Pts',(-4.98740458929052,-4.57362924412592,
17.5390532270889));
#52543=CARTESIAN_POINT('Ctrl Pts',(-4.86169180652526,-4.71071523781489,
17.5478024324656));
#52544=CARTESIAN_POINT('Ctrl Pts',(-4.73032391141336,-4.84261509584721,
17.5565516378424));
#52545=CARTESIAN_POINT('Ctrl Pts',(-4.59374706947068,-4.96888084599838,
17.5653008432191));
#52546=CARTESIAN_POINT('Ctrl Pts',(-4.45717070231264,-5.09514615720954,
17.5740500181808));
#52547=CARTESIAN_POINT('Ctrl Pts',(-4.31538563497136,-5.21577720520769,
17.5827991931425));
#52548=CARTESIAN_POINT('Ctrl Pts',(-4.16887340951833,-5.33036429293637,
17.5915483681042));
#52549=CARTESIAN_POINT('Ctrl Pts',(-4.02236168122307,-5.44495099183837,
17.6002975133775));
#52550=CARTESIAN_POINT('Ctrl Pts',(-3.87112305262998,-5.55349359498056,
17.6090466586507));
#52551=CARTESIAN_POINT('Ctrl Pts',(-3.71567116928808,-5.65562346357335,
17.6177958039239));
#52552=CARTESIAN_POINT('Ctrl Pts',(-3.56021980053164,-5.75775299409017,
17.6265449202353));
#52553=CARTESIAN_POINT('Ctrl Pts',(-3.40055544441979,-5.85346967519938,
17.6352940365466));
#52554=CARTESIAN_POINT('Ctrl Pts',(-3.23722035886783,-5.94244843041416,
17.644043152858));
#52555=CARTESIAN_POINT('Ctrl Pts',(-3.07388580043432,-6.0314268984748,17.652792240934));
#52556=CARTESIAN_POINT('Ctrl Pts',(-2.90688078789168,-6.11366734707928,
17.66154132901));
#52557=CARTESIAN_POINT('Ctrl Pts',(-2.73677250610341,-6.18889047001451,
17.670290417086));
#52558=CARTESIAN_POINT('Ctrl Pts',(-2.56666475916883,-6.26411335643355,
17.6790394776532));
#52559=CARTESIAN_POINT('Ctrl Pts',(-2.39345402457042,-6.33231884545275,
17.6877885382203));
#52560=CARTESIAN_POINT('Ctrl Pts',(-2.21772855944014,-6.393275298049,17.6965375987875));
#52561=CARTESIAN_POINT('Ctrl Pts',(-2.04200363223574,-6.45423156404707,
17.7052866325723));
#52562=CARTESIAN_POINT('Ctrl Pts',(-1.86376426061051,-6.50793874412447,
17.7140356663571));
#52563=CARTESIAN_POINT('Ctrl Pts',(-1.68361577621741,-6.55421443943299,
17.7227847001419));
#52564=CARTESIAN_POINT('Ctrl Pts',(-1.50346782833254,-6.60048999692579,
17.7315337078708));
#52565=CARTESIAN_POINT('Ctrl Pts',(-1.32141105657412,-6.63933404265157,
17.7402827155997));
#52566=CARTESIAN_POINT('Ctrl Pts',(-1.13806375346546,-6.67061465631527,
17.7490317233286));
#52567=CARTESIAN_POINT('Ctrl Pts',(-0.954716981169866,-6.70189517941774,
17.757780705728));
#52568=CARTESIAN_POINT('Ctrl Pts',(-0.770079967441888,-6.72561226609009,
17.7665296881275));
#52569=CARTESIAN_POINT('Ctrl Pts',(-0.584779764072423,-6.7416853699599,
17.7752786705269));
#52570=CARTESIAN_POINT('Ctrl Pts',(-0.391489587592256,-6.75845153117877,
17.7844049009425));
#52571=CARTESIAN_POINT('Ctrl Pts',(-0.197478091804486,-6.76689985146396,
17.7935311313582));
#52572=CARTESIAN_POINT('Ctrl Pts',(-0.00346214753022823,-6.76699911434415,
17.8026573617738));
#52573=CARTESIAN_POINT('Ctrl Pts',(0.184490798485415,-6.76709527525933,
17.8114983974889));
#52574=CARTESIAN_POINT('Ctrl Pts',(0.372447602155526,-6.75935633790759,
17.820339433204));
#52575=CARTESIAN_POINT('Ctrl Pts',(0.559756448194932,-6.74380914014507,
17.8291804689192));
#52576=CARTESIAN_POINT('Ctrl Pts',(0.745136131044055,-6.72842206873147,
17.8379304475325));
#52577=CARTESIAN_POINT('Ctrl Pts',(0.929880851945723,-6.70538686355714,
17.8466804261458));
#52578=CARTESIAN_POINT('Ctrl Pts',(1.11336305057529,-6.67478177303301,17.8554304047591));
#52579=CARTESIAN_POINT('Ctrl Pts',(1.29684337090197,-6.64417699581246,17.8641802937991));
#52580=CARTESIAN_POINT('Ctrl Pts',(1.47906091205271,-6.60600253548042,17.872930182839));
#52581=CARTESIAN_POINT('Ctrl Pts',(1.65939671095309,-6.5603880644119,17.881680071879));
#52582=CARTESIAN_POINT('Ctrl Pts',(1.8397307236926,-6.51477404513822,17.8904298742545));
#52583=CARTESIAN_POINT('Ctrl Pts',(2.01818275357148,-6.46172023288626,17.89917967663));
#52584=CARTESIAN_POINT('Ctrl Pts',(2.19414664033449,-6.40140683918066,17.9079294790055));
#52585=CARTESIAN_POINT('Ctrl Pts',(2.37010884271373,-6.34109402281455,17.9166791976251));
#52586=CARTESIAN_POINT('Ctrl Pts',(2.54358267847909,-6.27352185699749,17.9254289162446));
#52587=CARTESIAN_POINT('Ctrl Pts',(2.71397890841836,-6.1989198643522,17.9341786348641));
#52588=CARTESIAN_POINT('Ctrl Pts',(2.88437356389044,-6.12431856103195,17.9429282726359));
#52589=CARTESIAN_POINT('Ctrl Pts',(3.05169040787282,-6.04268767582502,17.9516779104078));
#52590=CARTESIAN_POINT('Ctrl Pts',(3.21536112512171,-5.95430447953882,17.9604275481796));
#52591=CARTESIAN_POINT('Ctrl Pts',(3.3790303844295,-5.8659220705498,17.9691771080117));
#52592=CARTESIAN_POINT('Ctrl Pts',(3.53905332980071,-5.77078760703316,17.9779266678437));
#52593=CARTESIAN_POINT('Ctrl Pts',(3.69488643041981,-5.6692242208524,17.9866762276758));
#52594=CARTESIAN_POINT('Ctrl Pts',(3.85071819468833,-5.56766170563095,17.9954257124758));
#52595=CARTESIAN_POINT('Ctrl Pts',(4.00235994599317,-5.45967053456184,18.0041751972758));
#52596=CARTESIAN_POINT('Ctrl Pts',(4.14929662974394,-5.34561750206611,18.0129246820758));
#52597=CARTESIAN_POINT('Ctrl Pts',(4.29623210225124,-5.231565409744,18.0216740947511));
#52598=CARTESIAN_POINT('Ctrl Pts',(4.43846235842183,-5.11145173172129,18.0304235074265));
#52599=CARTESIAN_POINT('Ctrl Pts',(4.57550431797482,-4.98568443006513,18.0391729201018));
#52600=CARTESIAN_POINT('Ctrl Pts',(4.71254519337547,-4.85991812336638,18.0479222635597));
#52601=CARTESIAN_POINT('Ctrl Pts',(4.84439764315037,-4.72849847631046,18.0566716070176));
#52602=CARTESIAN_POINT('Ctrl Pts',(4.97061384196739,-4.59187184425286,18.0654209504755));
#52603=CARTESIAN_POINT('Ctrl Pts',(5.09682908420268,-4.45524624767677,18.0741702276229));
#52604=CARTESIAN_POINT('Ctrl Pts',(5.2174079665024,-4.31341395556809,18.0829195047702));
#52605=CARTESIAN_POINT('Ctrl Pts',(5.33194095942327,-4.16685668162759,18.0916687819176));
#52606=CARTESIAN_POINT('Ctrl Pts',(5.44647312235211,-4.02030046975109,18.1004179956612));
#52607=CARTESIAN_POINT('Ctrl Pts',(5.55495930712368,-3.86901957035433,18.1091672094047));
#52608=CARTESIAN_POINT('Ctrl Pts',(5.65703106079876,-3.71352778058251,18.1179164231482));
#52609=CARTESIAN_POINT('Ctrl Pts',(5.75910210868811,-3.55803706597481,18.1266655763944));
#52610=CARTESIAN_POINT('Ctrl Pts',(5.85475865698619,-3.39833575880779,18.1354147296406));
#52611=CARTESIAN_POINT('Ctrl Pts',(5.94367583069127,-3.23496624706602,18.1441638828868));
#52612=CARTESIAN_POINT('Ctrl Pts',(6.03259241910144,-3.0715978106997,18.152912978542));
#52613=CARTESIAN_POINT('Ctrl Pts',(6.11476958471035,-2.90456146975693,18.1616620741971));
#52614=CARTESIAN_POINT('Ctrl Pts',(6.18992823574453,-2.73442451648105,18.1704111698522));
#52615=CARTESIAN_POINT('Ctrl Pts',(6.26508641701006,-2.56428862662244,18.1791602108223));
#52616=CARTESIAN_POINT('Ctrl Pts',(6.3332260557037,-2.39105242531085,18.1879092517925));
#52617=CARTESIAN_POINT('Ctrl Pts',(6.3941157374784,-2.21530425353517,18.1966582927626));
#52618=CARTESIAN_POINT('Ctrl Pts',(6.45500505889191,-2.03955712188354,18.2054072819536));
#52619=CARTESIAN_POINT('Ctrl Pts',(6.50864441544987,-1.8612983202537,18.2141562711446));
#52620=CARTESIAN_POINT('Ctrl Pts',(6.55485164049957,-1.68113324012112,18.2229052603356));
#52621=CARTESIAN_POINT('Ctrl Pts',(6.60199852639155,-1.497304359127,18.2318321672124));
#52622=CARTESIAN_POINT('Ctrl Pts',(6.64140767441049,-1.31149113173452,18.2407590740894));
#52623=CARTESIAN_POINT('Ctrl Pts',(6.67293975269636,-1.12435050446232,18.2496859809662));
#52624=CARTESIAN_POINT('Ctrl Pts',(6.70384664831534,-0.940920291561764,
18.2584358951502));
#52625=CARTESIAN_POINT('Ctrl Pts',(6.72718585889688,-0.756215114275973,
18.2671858093342));
#52626=CARTESIAN_POINT('Ctrl Pts',(6.74287810451881,-0.57086238937319,18.2759357235182));
#52627=CARTESIAN_POINT('Ctrl Pts',(6.75857004154135,-0.385513309566141,
18.2846854656288));
#52628=CARTESIAN_POINT('Ctrl Pts',(6.76661529035562,-0.199516993257244,
18.2934352077394));
#52629=CARTESIAN_POINT('Ctrl Pts',(6.76698652348897,-0.0135052182030834,
18.30218494985));
#52630=CARTESIAN_POINT('Ctrl Pts',(6.76735774981519,0.17250314603988,18.3109345315206));
#52631=CARTESIAN_POINT('Ctrl Pts',(6.76005524147474,0.358526681834471,18.3196841131912));
#52632=CARTESIAN_POINT('Ctrl Pts',(6.74510380214873,0.543933542115877,18.3284336948619));
#52633=CARTESIAN_POINT('Ctrl Pts',(6.73015261710969,0.729337249085657,18.3371831277238));
#52634=CARTESIAN_POINT('Ctrl Pts',(6.70755278444593,0.914124015855522,18.3459325605857));
#52635=CARTESIAN_POINT('Ctrl Pts',(6.67738106408276,1.09766621749464,18.3546819934477));
#52636=CARTESIAN_POINT('Ctrl Pts',(6.64720981677239,1.28120554143399,18.36343128913));
#52637=CARTESIAN_POINT('Ctrl Pts',(6.60946696581506,1.46350005650695,18.3721805848124));
#52638=CARTESIAN_POINT('Ctrl Pts',(6.56428070010976,1.64393062206608,18.3809298804947));
#52639=CARTESIAN_POINT('Ctrl Pts',(6.51909508282721,1.82435859844722,18.3896790506247));
#52640=CARTESIAN_POINT('Ctrl Pts',(6.46646633415641,2.00292240086628,18.3984282207547));
#52641=CARTESIAN_POINT('Ctrl Pts',(6.40657319597172,2.17901557696514,18.4071773908847));
#52642=CARTESIAN_POINT('Ctrl Pts',(6.3466808376827,2.355106460075,18.4159264470877));
#52643=CARTESIAN_POINT('Ctrl Pts',(6.27952437143856,2.52872650996602,18.4246755032908));
#52644=CARTESIAN_POINT('Ctrl Pts',(6.20533187335102,2.69928607998002,18.4334245594939));
#52645=CARTESIAN_POINT('Ctrl Pts',(6.1283144978422,2.87633970115466,18.4425067357828));
#52646=CARTESIAN_POINT('Ctrl Pts',(6.04371489463123,3.05009490562409,18.4515889120716));
#52647=CARTESIAN_POINT('Ctrl Pts',(5.95184265120463,3.21991584599683,18.4606710883604));
#52648=CARTESIAN_POINT('Ctrl Pts',(5.86333281335462,3.38352155905352,18.4694208687148));
#52649=CARTESIAN_POINT('Ctrl Pts',(5.76807337235653,3.54347560903877,18.4781706490693));
#52650=CARTESIAN_POINT('Ctrl Pts',(5.66638790086321,3.699234671787,18.4869204294237));
#52651=CARTESIAN_POINT('Ctrl Pts',(5.564706085027,3.85498813489826,18.4956698952179));
#52652=CARTESIAN_POINT('Ctrl Pts',(5.456598857669,4.00654667256333,18.5044193610122));
#52653=CARTESIAN_POINT('Ctrl Pts',(5.34243340580445,4.1533955150629,18.5131688268065));
#52654=CARTESIAN_POINT('Ctrl Pts',(5.22827145140523,4.30023985883957,18.5219180245604));
#52655=CARTESIAN_POINT('Ctrl Pts',(5.10805181978009,4.44237456993136,18.5306672223142));
#52656=CARTESIAN_POINT('Ctrl Pts',(4.98218281282461,4.57931691626547,18.5394164200681));
#52657=CARTESIAN_POINT('Ctrl Pts',(4.85631699296121,4.71625579512274,18.5481653962861));
#52658=CARTESIAN_POINT('Ctrl Pts',(4.72480227791711,4.84800236135894,18.5569143725041));
#52659=CARTESIAN_POINT('Ctrl Pts',(4.58808530847967,4.97410918679044,18.5656633487221));
#52660=CARTESIAN_POINT('Ctrl Pts',(4.45135945056814,5.10022421089146,18.5744128937433));
#52661=CARTESIAN_POINT('Ctrl Pts',(4.30943087207873,5.22069856612124,18.5831624387646));
#52662=CARTESIAN_POINT('Ctrl Pts',(4.16278164322291,5.33512305301822,18.5919119837858));
#52663=CARTESIAN_POINT('Ctrl Pts',(4.01614103534205,5.44954081331564,18.600661014453));
#52664=CARTESIAN_POINT('Ctrl Pts',(3.86478055833219,5.55790924068473,18.6094100451203));
#52665=CARTESIAN_POINT('Ctrl Pts',(3.70921425811749,5.65986029751424,18.6181590757875));
#52666=CARTESIAN_POINT('Ctrl Pts',(3.55364584529916,5.76181273884779,18.6269082252674));
#52667=CARTESIAN_POINT('Ctrl Pts',(3.39387173464139,5.85734747818182,18.6356573747472));
#52668=CARTESIAN_POINT('Ctrl Pts',(3.23043456092199,5.94614005448919,18.6444065242271));
#52669=CARTESIAN_POINT('Ctrl Pts',(3.18690768806252,5.96978744811355,18.6467366129601));
#52670=CARTESIAN_POINT('Ctrl Pts',(3.14312114982809,5.99295688499337,18.6490667016931));
#52671=CARTESIAN_POINT('Ctrl Pts',(3.09908550384716,6.01564277861015,18.6513967904261));
#52672=CARTESIAN_POINT('Origin',(0.,0.,-63.6971797838103));
#52673=CARTESIAN_POINT('',(3.0990855038473,6.01564277861008,21.0460278352566));
#52674=CARTESIAN_POINT('',(3.09908550384707,6.01564277861019,20.6515076495525));
#52675=CARTESIAN_POINT('',(3.09908550384721,6.01564277861012,-63.6971797838103));
#52676=CARTESIAN_POINT('',(-6.767,7.50599334255745E-8,19.6971817862495));
#52677=CARTESIAN_POINT('Ctrl Pts',(-6.767,7.50599334255761E-8,19.6971817862495));
#52678=CARTESIAN_POINT('Ctrl Pts',(-6.7670000019611,-0.176801917699121,
19.7055396886733));
#52679=CARTESIAN_POINT('Ctrl Pts',(-6.76006670113114,-0.35378666355907,
19.7138975910971));
#52680=CARTESIAN_POINT('Ctrl Pts',(-6.74618310727778,-0.53037956510401,
19.722255493521));
#52681=CARTESIAN_POINT('Ctrl Pts',(-6.73231304500031,-0.70680035125333,
19.7306052499567));
#52682=CARTESIAN_POINT('Ctrl Pts',(-6.71150621456675,-0.882829712877172,
19.7389550063924));
#52683=CARTESIAN_POINT('Ctrl Pts',(-6.68379765480675,-1.05789314658895,
19.7473047628281));
#52684=CARTESIAN_POINT('Ctrl Pts',(-6.65611120922512,-1.2328168623206,19.7556478553301));
#52685=CARTESIAN_POINT('Ctrl Pts',(-6.62153406509078,-1.40677584781493,
19.7639909478322));
#52686=CARTESIAN_POINT('Ctrl Pts',(-6.58015308656352,-1.57920054375262,
19.7723340403343));
#52687=CARTESIAN_POINT('Ctrl Pts',(-6.53879783380593,-1.75151804652644,
19.7806719460939));
#52688=CARTESIAN_POINT('Ctrl Pts',(-6.49064725738989,-1.92230282704946,
19.7890098518536));
#52689=CARTESIAN_POINT('Ctrl Pts',(-6.43583938430197,-2.09099507877653,
19.7973477576132));
#52690=CARTESIAN_POINT('Ctrl Pts',(-6.38105405776363,-2.25961793484924,
19.8056822333729));
#52691=CARTESIAN_POINT('Ctrl Pts',(-6.31961699868245,-2.42614965081121,
19.8140167091326));
#52692=CARTESIAN_POINT('Ctrl Pts',(-6.25171630185697,-2.59004484152221,
19.8223511848922));
#52693=CARTESIAN_POINT('Ctrl Pts',(-6.18383044630271,-2.7539042091402,19.830683838959));
#52694=CARTESIAN_POINT('Ctrl Pts',(-6.10948389970995,-2.91512788198916,
19.8390164930258));
#52695=CARTESIAN_POINT('Ctrl Pts',(-6.02891329099595,-3.0731894718114,19.8473491470925));
#52696=CARTESIAN_POINT('Ctrl Pts',(-5.94834740506893,-3.23124179657743,
19.8556813127262));
#52697=CARTESIAN_POINT('Ctrl Pts',(-5.86155834060649,-3.38613210120756,
19.86401347836));
#52698=CARTESIAN_POINT('Ctrl Pts',(-5.76882927709368,-3.53735745603224,
19.8723456439937));
#52699=CARTESIAN_POINT('Ctrl Pts',(-5.6760908173443,-3.68859813452304,19.8806786539258));
#52700=CARTESIAN_POINT('Ctrl Pts',(-5.57741133947012,-3.83617283005422,
19.8890116638578));
#52701=CARTESIAN_POINT('Ctrl Pts',(-5.47311817133102,-3.97960632257089,
19.8973446737899));
#52702=CARTESIAN_POINT('Ctrl Pts',(-5.36875617982275,-4.1231344672722,19.9056831826999));
#52703=CARTESIAN_POINT('Ctrl Pts',(-5.25877329786672,-4.2625156692081,19.9140216916098));
#52704=CARTESIAN_POINT('Ctrl Pts',(-5.14353865202304,-4.39730589510726,
19.9223602005197));
#52705=CARTESIAN_POINT('Ctrl Pts',(-5.02826519893037,-4.53214151393333,
19.9307015175659));
#52706=CARTESIAN_POINT('Ctrl Pts',(-4.90773668534676,-4.66238281766333,
19.9390428346121));
#52707=CARTESIAN_POINT('Ctrl Pts',(-4.78236037383168,-4.78762135666602,
19.9473841516583));
#52708=CARTESIAN_POINT('Ctrl Pts',(-4.65685677636424,-4.9129870417501,19.9557339370705));
#52709=CARTESIAN_POINT('Ctrl Pts',(-4.52649579541607,-5.03333957507811,
19.9640837224826));
#52710=CARTESIAN_POINT('Ctrl Pts',(-4.39171998876124,-5.14830890101934,
19.9724335078948));
#52711=CARTESIAN_POINT('Ctrl Pts',(-4.28901518590022,-5.23592033699538,
19.9787963936824));
#52712=CARTESIAN_POINT('Ctrl Pts',(-4.18374738657325,-5.32040648979079,
19.9851592794701));
#52713=CARTESIAN_POINT('Ctrl Pts',(-4.07612420460264,-5.40162017071291,
19.9915221652578));
#52714=CARTESIAN_POINT('Ctrl Pts',(-3.93841941548391,-5.50553377557166,
19.9996635324756));
#52715=CARTESIAN_POINT('Ctrl Pts',(-3.7965628885728,-5.60431055798295,20.0078048996935));
#52716=CARTESIAN_POINT('Ctrl Pts',(-3.65097880291341,-5.69759973854578,
20.0159462669114));
#52717=CARTESIAN_POINT('Ctrl Pts',(-3.50552180108836,-5.79080748474912,
20.0240805273348));
#52718=CARTESIAN_POINT('Ctrl Pts',(-3.35634402349876,-5.87853696802974,
20.0322147877583));
#52719=CARTESIAN_POINT('Ctrl Pts',(-3.20390163287579,-5.96047844781406,
20.0403490481818));
#52720=CARTESIAN_POINT('Ctrl Pts',(-3.05156323294489,-6.04236403008091,
20.0484777597066));
#52721=CARTESIAN_POINT('Ctrl Pts',(-2.89596497497535,-6.11846929732322,
20.0566064712315));
#52722=CARTESIAN_POINT('Ctrl Pts',(-2.73759079890839,-6.1885285502882,20.0647351827564));
#52723=CARTESIAN_POINT('Ctrl Pts',(-2.57929214855954,-6.25855439329,20.0728600178489));
#52724=CARTESIAN_POINT('Ctrl Pts',(-2.41822055028159,-6.32253981577258,
20.0809848529414));
#52725=CARTESIAN_POINT('Ctrl Pts',(-2.25488325185526,-6.38026570923991,
20.0891096880339));
#52726=CARTESIAN_POINT('Ctrl Pts',(-2.0915916801637,-6.43797544218147,20.0972322485561));
#52727=CARTESIAN_POINT('Ctrl Pts',(-1.92603601680998,-6.4894290154097,20.1053548090783));
#52728=CARTESIAN_POINT('Ctrl Pts',(-1.75874209977583,-6.5344560008065,20.1134773696004));
#52729=CARTESIAN_POINT('Ctrl Pts',(-1.59143929150364,-6.57948537927086,
20.1216003618156));
#52730=CARTESIAN_POINT('Ctrl Pts',(-1.42239839745797,-6.61808738865115,
20.1297233540308));
#52731=CARTESIAN_POINT('Ctrl Pts',(-1.25215916183377,-6.65014183558785,
20.137846346246));
#52732=CARTESIAN_POINT('Ctrl Pts',(-1.1652572200179,-6.66650465390303,20.1419928862271));
#52733=CARTESIAN_POINT('Ctrl Pts',(-1.0780432045147,-6.68116213074483,20.1461394262081));
#52734=CARTESIAN_POINT('Ctrl Pts',(-0.99058984092042,-6.69410343265364,
20.1502859661891));
#52735=CARTESIAN_POINT('Ctrl Pts',(-0.801118329007074,-6.72214132551464,
20.1592696252175));
#52736=CARTESIAN_POINT('Ctrl Pts',(-0.61061671185007,-6.74210688210214,
20.1682532842459));
#52737=CARTESIAN_POINT('Ctrl Pts',(-0.419754791226097,-6.75396882693744,
20.1772369432742));
#52738=CARTESIAN_POINT('Ctrl Pts',(-0.228564971845571,-6.76585115046825,
20.1862360361336));
#52739=CARTESIAN_POINT('Ctrl Pts',(-0.0370138505142297,-6.76960202140709,
20.1952351289929));
#52740=CARTESIAN_POINT('Ctrl Pts',(0.154228262328821,-6.76524224570703,
20.2042342218523));
#52741=CARTESIAN_POINT('Ctrl Pts',(0.34591878448494,-6.76087224755126,20.2132544150697));
#52742=CARTESIAN_POINT('Ctrl Pts',(0.537298608434677,-6.74835355818315,
20.222274608287));
#52743=CARTESIAN_POINT('Ctrl Pts',(0.727699264931206,-6.72775912022856,
20.2312948015044));
#52744=CARTESIAN_POINT('Ctrl Pts',(0.918292749769805,-6.70714382524859,
20.2403241299261));
#52745=CARTESIAN_POINT('Ctrl Pts',(1.10790484918032,-6.67843647431839,20.2493534583478));
#52746=CARTESIAN_POINT('Ctrl Pts',(1.29587518300171,-6.64176155173312,20.2583827867695));
#52747=CARTESIAN_POINT('Ctrl Pts',(1.4841105171046,-6.60503492489956,20.2674248447242));
#52748=CARTESIAN_POINT('Ctrl Pts',(1.67069922279195,-6.56031831238033,20.276466902679));
#52749=CARTESIAN_POINT('Ctrl Pts',(1.85499175602118,-6.50778722647671,20.2855089606337));
#52750=CARTESIAN_POINT('Ctrl Pts',(2.01492565910245,-6.46219936974455,20.2933558961294));
#52751=CARTESIAN_POINT('Ctrl Pts',(2.17313038866878,-6.41072707698854,20.3012028316251));
#52752=CARTESIAN_POINT('Ctrl Pts',(2.32919171885851,-6.35351516381294,20.3090497671208));
#52753=CARTESIAN_POINT('Ctrl Pts',(2.5012934457399,-6.29042285873173,20.3177032314216));
#52754=CARTESIAN_POINT('Ctrl Pts',(2.67093975429473,-6.22029356059689,20.3263566957224));
#52755=CARTESIAN_POINT('Ctrl Pts',(2.83755243353247,-6.14333664932616,20.3350101600233));
#52756=CARTESIAN_POINT('Ctrl Pts',(3.00401162841341,-6.0664506311116,20.3436556527135));
#52757=CARTESIAN_POINT('Ctrl Pts',(3.16744249283284,-5.98274967161941,20.3523011454037));
#52758=CARTESIAN_POINT('Ctrl Pts',(3.32728625269314,-5.89249142491011,20.3609466380939));
#52759=CARTESIAN_POINT('Ctrl Pts',(3.49193863767322,-5.79951791379029,20.3698522155904));
#52760=CARTESIAN_POINT('Ctrl Pts',(3.65278441561305,-5.69958652694498,20.3787577930869));
#52761=CARTESIAN_POINT('Ctrl Pts',(3.8092374397924,-5.59303130040266,20.3876633705835));
#52762=CARTESIAN_POINT('Ctrl Pts',(3.96083310453578,-5.48978426836671,20.396292458756));
#52763=CARTESIAN_POINT('Ctrl Pts',(4.10830440336963,-5.38031870236594,20.4049215469286));
#52764=CARTESIAN_POINT('Ctrl Pts',(4.25114468426882,-5.26498412850532,20.4135506351012));
#52765=CARTESIAN_POINT('Ctrl Pts',(4.40085020027326,-5.1441063075975,20.4225944572597));
#52766=CARTESIAN_POINT('Ctrl Pts',(4.54546827328342,-5.01678157922803,20.4316382794181));
#52767=CARTESIAN_POINT('Ctrl Pts',(4.68445121006545,-4.88346248685462,20.4406821015766));
#52768=CARTESIAN_POINT('Ctrl Pts',(4.82343414684748,-4.75014339448122,20.4497259237351));
#52769=CARTESIAN_POINT('Ctrl Pts',(4.95678164535619,-4.61083017984488,20.4587697458936));
#52770=CARTESIAN_POINT('Ctrl Pts',(5.08398704627084,-4.46602336686121,20.4678135680522));
#52771=CARTESIAN_POINT('Ctrl Pts',(5.20249954652553,-4.33111229125269,20.4762393579019));
#52772=CARTESIAN_POINT('Ctrl Pts',(5.31562900031493,-4.19149202381202,20.4846651477517));
#52773=CARTESIAN_POINT('Ctrl Pts',(5.42300844233551,-4.04762503628459,20.4930909376015));
#52774=CARTESIAN_POINT('Ctrl Pts',(5.53041279999891,-3.90372466677633,20.5015186825179));
#52775=CARTESIAN_POINT('Ctrl Pts',(5.63206428741306,-3.75557587813829,20.5099464274344));
#52776=CARTESIAN_POINT('Ctrl Pts',(5.72763828737402,-3.60367155121097,20.5183741723508));
#52777=CARTESIAN_POINT('Ctrl Pts',(5.82324740598551,-3.45171140706374,20.5268050140408));
#52778=CARTESIAN_POINT('Ctrl Pts',(5.91277440794826,-3.29599325354146,20.5352358557307));
#52779=CARTESIAN_POINT('Ctrl Pts',(5.99593959107438,-3.13703640721411,20.5436666974207));
#52780=CARTESIAN_POINT('Ctrl Pts',(6.07918119238835,-2.9779334998347,20.552105285978));
#52781=CARTESIAN_POINT('Ctrl Pts',(6.15604914192404,-2.81558624792901,20.5605438745353));
#52782=CARTESIAN_POINT('Ctrl Pts',(6.2263105602298,-2.65053689043766,20.5689824630926));
#52783=CARTESIAN_POINT('Ctrl Pts',(6.29660882051841,-2.48540098835689,20.5774254764729));
#52784=CARTESIAN_POINT('Ctrl Pts',(6.36029351816141,-2.31756046262265,20.5858684898532));
#52785=CARTESIAN_POINT('Ctrl Pts',(6.41718080857057,-2.14757525365552,20.5943115032334));
#52786=CARTESIAN_POINT('Ctrl Pts',(6.47412786304321,-1.97741146337882,20.6027633865877));
#52787=CARTESIAN_POINT('Ctrl Pts',(6.52426314762407,-1.80509880553376,20.6112152699419));
#52788=CARTESIAN_POINT('Ctrl Pts',(6.56745304480664,-1.63121105448068,20.6196671532962));
#52789=CARTESIAN_POINT('Ctrl Pts',(6.57922365626102,-1.58382114878889,20.6219705585254));
#52790=CARTESIAN_POINT('Ctrl Pts',(6.59047870375266,-1.53631430889342,20.6242739637547));
#52791=CARTESIAN_POINT('Ctrl Pts',(6.60121614522942,-1.48870225497327,20.6265773689839));
#52792=CARTESIAN_POINT('Ctrl Pts',(6.63998750366456,-1.31678196908697,20.6348946343173));
#52793=CARTESIAN_POINT('Ctrl Pts',(6.67207593033756,-1.14318001944469,20.6432118996508));
#52794=CARTESIAN_POINT('Ctrl Pts',(6.69734220124111,-0.968450535378533,
20.6515291649842));
#52795=CARTESIAN_POINT('Ctrl Pts',(6.72258716198922,-0.793868422187867,
20.6598394153443));
#52796=CARTESIAN_POINT('Ctrl Pts',(6.74102138152034,-0.618161011823664,
20.6681496657043));
#52797=CARTESIAN_POINT('Ctrl Pts',(6.75255649033741,-0.441893476759026,
20.6764599160644));
#52798=CARTESIAN_POINT('Ctrl Pts',(6.76408398269993,-0.265742328430808,
20.6847646792943));
#52799=CARTESIAN_POINT('Ctrl Pts',(6.76872141886024,-0.0890321382852432,
20.6930694425242));
#52800=CARTESIAN_POINT('Ctrl Pts',(6.76643212665369,0.0876657024660587,
20.701374205754));
#52801=CARTESIAN_POINT('Ctrl Pts',(6.76414392696195,0.264279218024154,20.7096750057166));
#52802=CARTESIAN_POINT('Ctrl Pts',(6.7549355912046,0.440880048849934,20.7179758056792));
#52803=CARTESIAN_POINT('Ctrl Pts',(6.73882252188824,0.616895468042915,20.7262766056419));
#52804=CARTESIAN_POINT('Ctrl Pts',(6.72271419358492,0.792859097512794,20.7345749632268));
#52805=CARTESIAN_POINT('Ctrl Pts',(6.69970521299222,0.968237312720989,20.7428733208117));
#52806=CARTESIAN_POINT('Ctrl Pts',(6.66986296581343,1.14246094780981,20.7511716783966));
#52807=CARTESIAN_POINT('Ctrl Pts',(6.64001768225444,1.31670230975392,20.7594708803204));
#52808=CARTESIAN_POINT('Ctrl Pts',(6.60333779420146,1.48978851276434,20.7677700822442));
#52809=CARTESIAN_POINT('Ctrl Pts',(6.55994219260918,1.66115846011929,20.776069284168));
#52810=CARTESIAN_POINT('Ctrl Pts',(6.51654219152551,1.8325457811384,20.7843693274735));
#52811=CARTESIAN_POINT('Ctrl Pts',(6.46642520474349,2.00221616218893,20.792669370779));
#52812=CARTESIAN_POINT('Ctrl Pts',(6.40976058365726,2.16962168596135,20.8009694140846));
#52813=CARTESIAN_POINT('Ctrl Pts',(6.35308081140155,2.33707197116365,20.8092716766825));
#52814=CARTESIAN_POINT('Ctrl Pts',(6.28985002702341,2.50225586252743,20.8175739392805));
#52815=CARTESIAN_POINT('Ctrl Pts',(6.22028656411547,2.66464332702982,20.8258762018784));
#52816=CARTESIAN_POINT('Ctrl Pts',(6.1506929520334,2.82710117112143,20.834182062721));
#52817=CARTESIAN_POINT('Ctrl Pts',(6.07476132826883,2.98675985325214,20.8424879235636));
#52818=CARTESIAN_POINT('Ctrl Pts',(5.99275708164464,3.143111763905,20.8507937844063));
#52819=CARTESIAN_POINT('Ctrl Pts',(5.91065590021539,3.29964849354718,20.8591094633624));
#52820=CARTESIAN_POINT('Ctrl Pts',(5.82246791573087,3.45287033355623,20.8674251423185));
#52821=CARTESIAN_POINT('Ctrl Pts',(5.72850376926257,3.6022955966362,20.8757408212746));
#52822=CARTESIAN_POINT('Ctrl Pts',(5.63448019122017,3.75181537000471,20.8840617598315));
#52823=CARTESIAN_POINT('Ctrl Pts',(5.53467336173813,3.89753349101612,20.8923826983883));
#52824=CARTESIAN_POINT('Ctrl Pts',(5.42943580675272,4.03899935879562,20.9007036369451));
#52825=CARTESIAN_POINT('Ctrl Pts',(5.32404183616345,4.18067548867345,20.909036942994));
#52826=CARTESIAN_POINT('Ctrl Pts',(5.21320122733091,4.31808646410224,20.917370249043));
#52827=CARTESIAN_POINT('Ctrl Pts',(5.09730601876832,4.4508156950191,20.9257035550919));
#52828=CARTESIAN_POINT('Ctrl Pts',(5.01200030279605,4.54851224532726,20.9318373603435));
#52829=CARTESIAN_POINT('Ctrl Pts',(4.92395689847716,4.64367304143043,20.9379711655951));
#52830=CARTESIAN_POINT('Ctrl Pts',(4.83334402846156,4.73614553223769,20.9441049708467));
#52831=CARTESIAN_POINT('Ctrl Pts',(4.70787102970677,4.8641935757652,20.9525985428809));
#52832=CARTESIAN_POINT('Ctrl Pts',(4.57706282676204,4.98749972683568,20.961092114915));
#52833=CARTESIAN_POINT('Ctrl Pts',(4.44132178010929,5.10558026531038,20.9695856869492));
#52834=CARTESIAN_POINT('Ctrl Pts',(4.31250030380911,5.21764150001963,20.9776462884804));
#52835=CARTESIAN_POINT('Ctrl Pts',(4.17923668925624,5.32499628093545,20.9857068900117));
#52836=CARTESIAN_POINT('Ctrl Pts',(4.04191632955374,5.42726463191974,20.9937674915429));
#52837=CARTESIAN_POINT('Ctrl Pts',(3.90472119891727,5.52943971945709,21.0018207422224));
#52838=CARTESIAN_POINT('Ctrl Pts',(3.76347697774605,5.62653738171646,21.009873992902));
#52839=CARTESIAN_POINT('Ctrl Pts',(3.61860468201547,5.71821555691072,21.0179272435815));
#52840=CARTESIAN_POINT('Ctrl Pts',(3.47385946705332,5.80981331277502,21.0259734300168));
#52841=CARTESIAN_POINT('Ctrl Pts',(3.32549282799942,5.89600084867242,21.034019616452));
#52842=CARTESIAN_POINT('Ctrl Pts',(3.17395719995998,5.97647761585553,21.0420658028873));
#52843=CARTESIAN_POINT('Ctrl Pts',(3.14908458615611,5.98968683652678,21.0433864803437));
#52844=CARTESIAN_POINT('Ctrl Pts',(3.12412666215165,6.00274229672367,21.0447071578001));
#52845=CARTESIAN_POINT('Ctrl Pts',(3.0990855038473,6.01564277861008,21.0460278352566));
#52846=CARTESIAN_POINT('Ctrl Pts',(3.0990855038472,6.01564277861012,19.0457563580462));
#52847=CARTESIAN_POINT('Ctrl Pts',(2.93373232018331,6.10082796552479,19.0545058059455));
#52848=CARTESIAN_POINT('Ctrl Pts',(2.76486502144431,6.17919158180188,19.0632552538448));
#52849=CARTESIAN_POINT('Ctrl Pts',(2.59305716434359,6.25046746591376,19.0720047017441));
#52850=CARTESIAN_POINT('Ctrl Pts',(2.42125069459297,6.32174277447219,19.0807540789915));
#52851=CARTESIAN_POINT('Ctrl Pts',(2.2465039787108,6.38593035557818,19.0895034562389));
#52852=CARTESIAN_POINT('Ctrl Pts',(2.06941053323801,6.44281220003529,19.0982528334863));
#52853=CARTESIAN_POINT('Ctrl Pts',(1.8923184589671,6.49969360406677,19.1070021429889));
#52854=CARTESIAN_POINT('Ctrl Pts',(1.71287996431529,6.54926929700875,19.1157514524915));
#52855=CARTESIAN_POINT('Ctrl Pts',(1.53170449173525,6.59137090065474,19.1245007619941));
#52856=CARTESIAN_POINT('Ctrl Pts',(1.35053036178188,6.6334721923008,19.1332500066587));
#52857=CARTESIAN_POINT('Ctrl Pts',(1.16761955878859,6.66809944062452,19.1419992513233));
#52858=CARTESIAN_POINT('Ctrl Pts',(0.983593309310603,6.6951350398539,19.1507484959879));
#52859=CARTESIAN_POINT('Ctrl Pts',(0.799568362460142,6.72217044771212,19.1594976787211));
#52860=CARTESIAN_POINT('Ctrl Pts',(0.614428268438801,6.74161427235975,19.1682468614542));
#52861=CARTESIAN_POINT('Ctrl Pts',(0.42880181633052,6.753400476968,19.1769960441874));
#52862=CARTESIAN_POINT('Ctrl Pts',(0.243176616523182,6.7651866020624,19.1857451678955));
#52863=CARTESIAN_POINT('Ctrl Pts',(0.0570653511660035,6.76931519233996,
19.1944942916037));
#52864=CARTESIAN_POINT('Ctrl Pts',(-0.128899900799341,6.76577222610797,
19.2032434153118));
#52865=CARTESIAN_POINT('Ctrl Pts',(-0.314863959941376,6.76222928260136,
19.2119924829011));
#52866=CARTESIAN_POINT('Ctrl Pts',(-0.500681721080079,6.75101488651281,
19.2207415504903));
#52867=CARTESIAN_POINT('Ctrl Pts',(-0.685722110172742,6.73216712415997,
19.2294906180796));
#52868=CARTESIAN_POINT('Ctrl Pts',(-0.870761373826987,6.71331947644153,
19.2382396324559));
#52869=CARTESIAN_POINT('Ctrl Pts',(-1.05502298984274,6.68683858440007,19.2469886468323));
#52870=CARTESIAN_POINT('Ctrl Pts',(-1.23788117675984,6.6528143813144,19.2557376612087));
#52871=CARTESIAN_POINT('Ctrl Pts',(-1.43009641451712,6.61704912302395,19.2649343720962));
#52872=CARTESIAN_POINT('Ctrl Pts',(-1.62076048992609,6.57294837083186,19.2741310829837));
#52873=CARTESIAN_POINT('Ctrl Pts',(-1.8091579896104,6.52067760042075,19.2833277938712));
#52874=CARTESIAN_POINT('Ctrl Pts',(-1.98840443002914,6.47094578577439,19.2920777915777));
#52875=CARTESIAN_POINT('Ctrl Pts',(-2.16559895952088,6.4138188847451,19.3008277892842));
#52876=CARTESIAN_POINT('Ctrl Pts',(-2.34013966242213,6.34949095285274,19.3095777869907));
#52877=CARTESIAN_POINT('Ctrl Pts',(-2.5146768255391,6.28516432556727,19.3183276072423));
#52878=CARTESIAN_POINT('Ctrl Pts',(-2.68656000078742,6.21363705879704,19.3270774274939));
#52879=CARTESIAN_POINT('Ctrl Pts',(-2.85520533840792,6.13515211510904,19.3358272477455));
#52880=CARTESIAN_POINT('Ctrl Pts',(-3.02384747998231,6.05666865881169,19.3445769021768));
#52881=CARTESIAN_POINT('Ctrl Pts',(-3.1892516468444,5.97122791039895,19.353326556608));
#52882=CARTESIAN_POINT('Ctrl Pts',(-3.35085601829061,5.87912008251963,19.3620762110393));
#52883=CARTESIAN_POINT('Ctrl Pts',(-3.5124575419132,5.78701387778234,19.3708257112824));
#52884=CARTESIAN_POINT('Ctrl Pts',(-3.67025915510836,5.68824097061047,19.3795752115255));
#52885=CARTESIAN_POINT('Ctrl Pts',(-3.82372487928733,5.58313684656924,19.3883247117687));
#52886=CARTESIAN_POINT('Ctrl Pts',(-3.9771881030071,5.47803443501837,19.3970740694538));
#52887=CARTESIAN_POINT('Ctrl Pts',(-4.12631534262951,5.36660117496434,19.4058234271389));
#52888=CARTESIAN_POINT('Ctrl Pts',(-4.27060009886163,5.24921554097401,19.414572784824));
#52889=CARTESIAN_POINT('Ctrl Pts',(-4.41488269594165,5.13183166360333,19.4233220115792));
#52890=CARTESIAN_POINT('Ctrl Pts',(-4.55432273235053,5.00849577139504,19.4320712383344));
#52891=CARTESIAN_POINT('Ctrl Pts',(-4.68844662480183,4.87962675277365,19.4408204650896));
#52892=CARTESIAN_POINT('Ctrl Pts',(-4.82256868835128,4.75075949139912,19.4495695725411));
#52893=CARTESIAN_POINT('Ctrl Pts',(-4.95137454637826,4.61635945312563,19.4583186799926));
#52894=CARTESIAN_POINT('Ctrl Pts',(-5.07442674461037,4.47688309134637,19.4670677874441));
#52895=CARTESIAN_POINT('Ctrl Pts',(-5.19747742838517,4.33740844616379,19.4758167872165));
#52896=CARTESIAN_POINT('Ctrl Pts',(-5.31477440450922,4.19285781736036,19.4845657869888));
#52897=CARTESIAN_POINT('Ctrl Pts',(-5.42591931531163,4.04372211999392,19.4933147867612));
#52898=CARTESIAN_POINT('Ctrl Pts',(-5.53707636462996,3.8945701350078,19.5020647420418));
#52899=CARTESIAN_POINT('Ctrl Pts',(-5.64207983273489,3.74083230916393,19.5108146973224));
#52900=CARTESIAN_POINT('Ctrl Pts',(-5.74057303468769,3.58303087251792,19.519564652603));
#52901=CARTESIAN_POINT('Ctrl Pts',(-5.83906243363792,3.42523552887385,19.5283142700318));
#52902=CARTESIAN_POINT('Ctrl Pts',(-5.93104191768457,3.26337713156936,19.5370638874606));
#52903=CARTESIAN_POINT('Ctrl Pts',(-6.01619906699691,3.09800545291088,19.5458135048894));
#52904=CARTESIAN_POINT('Ctrl Pts',(-6.10135338095419,2.9326392803952,19.5545628309948));
#52905=CARTESIAN_POINT('Ctrl Pts',(-6.17968568352877,2.7637603154014,19.5633121571002));
#52906=CARTESIAN_POINT('Ctrl Pts',(-6.25092992694924,2.5919421383145,19.5720614832056));
#52907=CARTESIAN_POINT('Ctrl Pts',(-6.32217217691139,2.42012876880728,19.5808105644994));
#52908=CARTESIAN_POINT('Ctrl Pts',(-6.38632665483883,2.24537661647578,19.5895596457932));
#52909=CARTESIAN_POINT('Ctrl Pts',(-6.44317547869379,2.06827917621365,19.598308727087));
#52910=CARTESIAN_POINT('Ctrl Pts',(-6.50002944235964,1.89116572423327,19.6070585994019));
#52911=CARTESIAN_POINT('Ctrl Pts',(-6.54957634250424,1.71170683289098,19.6158084717169));
#52912=CARTESIAN_POINT('Ctrl Pts',(-6.5916478770842,1.5305120922526,19.6245583440319));
#52913=CARTESIAN_POINT('Ctrl Pts',(-6.63371649075029,1.34932993147928,19.6333076088667));
#52914=CARTESIAN_POINT('Ctrl Pts',(-6.66831071257141,1.16641244173905,19.6420568737015));
#52915=CARTESIAN_POINT('Ctrl Pts',(-6.69531304840347,0.982380875159052,
19.6508061385363));
#52916=CARTESIAN_POINT('Ctrl Pts',(-6.72231677033056,0.798339861794849,
19.6595558524919));
#52917=CARTESIAN_POINT('Ctrl Pts',(-6.74172778477899,0.613184940729128,
19.6683055664476));
#52918=CARTESIAN_POINT('Ctrl Pts',(-6.75348015835525,0.427545027689496,
19.6770552804032));
#52919=CARTESIAN_POINT('Ctrl Pts',(-6.76249038365216,0.28521995354738,19.6837634482055));
#52920=CARTESIAN_POINT('Ctrl Pts',(-6.76699999999992,0.142609995759486,
19.6904716160077));
#52921=CARTESIAN_POINT('Ctrl Pts',(-6.767,3.718767489228E-12,19.6971797838099));
#52922=CARTESIAN_POINT('',(-6.76699844390314,-0.0035429858251562,19.3028202161898));
#52923=CARTESIAN_POINT('Ctrl Pts',(3.09908550384716,6.01564277861015,18.6513967904261));
#52924=CARTESIAN_POINT('Ctrl Pts',(2.93373232018326,6.10082796552481,18.6601462383254));
#52925=CARTESIAN_POINT('Ctrl Pts',(2.76486502144426,6.17919158180191,18.6688956862247));
#52926=CARTESIAN_POINT('Ctrl Pts',(2.59305716434353,6.25046746591379,18.677645134124));
#52927=CARTESIAN_POINT('Ctrl Pts',(2.4212506945928,6.32174277447226,18.6863945113714));
#52928=CARTESIAN_POINT('Ctrl Pts',(2.24650397871051,6.38593035557828,18.6951438886188));
#52929=CARTESIAN_POINT('Ctrl Pts',(2.06941053323759,6.44281220003543,18.7038932658662));
#52930=CARTESIAN_POINT('Ctrl Pts',(1.8923184589668,6.49969360406686,18.7126425753688));
#52931=CARTESIAN_POINT('Ctrl Pts',(1.7128799643151,6.54926929700879,18.7213918848714));
#52932=CARTESIAN_POINT('Ctrl Pts',(1.53170449173519,6.59137090065475,18.730141194374));
#52933=CARTESIAN_POINT('Ctrl Pts',(1.35053036178182,6.63347219230081,18.7388904390386));
#52934=CARTESIAN_POINT('Ctrl Pts',(1.16761955878853,6.66809944062453,18.7476396837032));
#52935=CARTESIAN_POINT('Ctrl Pts',(0.983593309310539,6.69513503985391,18.7563889283678));
#52936=CARTESIAN_POINT('Ctrl Pts',(0.79956836245995,6.72217044771215,18.765138111101));
#52937=CARTESIAN_POINT('Ctrl Pts',(0.614428268438478,6.74161427235978,18.7738872938341));
#52938=CARTESIAN_POINT('Ctrl Pts',(0.428801816330067,6.75340047696803,18.7826364765673));
#52939=CARTESIAN_POINT('Ctrl Pts',(0.243176616522471,6.76518660206243,18.7913856002754));
#52940=CARTESIAN_POINT('Ctrl Pts',(0.0570653511650372,6.76931519233997,
18.8001347239836));
#52941=CARTESIAN_POINT('Ctrl Pts',(-0.128899900800564,6.76577222610794,
18.8088838476917));
#52942=CARTESIAN_POINT('Ctrl Pts',(-0.314863959942471,6.76222928260131,
18.817632915281));
#52943=CARTESIAN_POINT('Ctrl Pts',(-0.500681721081045,6.75101488651274,
18.8263819828703));
#52944=CARTESIAN_POINT('Ctrl Pts',(-0.685722110173579,6.73216712415988,
18.8351310504595));
#52945=CARTESIAN_POINT('Ctrl Pts',(-0.870761373827823,6.71331947644142,
18.8438800648359));
#52946=CARTESIAN_POINT('Ctrl Pts',(-1.05502298984357,6.68683858439994,18.8526290792122));
#52947=CARTESIAN_POINT('Ctrl Pts',(-1.23788117676067,6.65281438131425,18.8613780935886));
#52948=CARTESIAN_POINT('Ctrl Pts',(-1.43009641451794,6.61704912302377,18.8705748044761));
#52949=CARTESIAN_POINT('Ctrl Pts',(-1.62076048992691,6.57294837083166,18.8797715153636));
#52950=CARTESIAN_POINT('Ctrl Pts',(-1.80915798961122,6.52067760042052,18.8889682262512));
#52951=CARTESIAN_POINT('Ctrl Pts',(-1.98840443002995,6.47094578577414,18.8977182239577));
#52952=CARTESIAN_POINT('Ctrl Pts',(-2.16559895952168,6.41381888474483,18.9064682216642));
#52953=CARTESIAN_POINT('Ctrl Pts',(-2.34013966242293,6.34949095285245,18.9152182193707));
#52954=CARTESIAN_POINT('Ctrl Pts',(-2.51467682553989,6.28516432556695,18.9239680396223));
#52955=CARTESIAN_POINT('Ctrl Pts',(-2.6865600007882,6.21363705879671,18.9327178598739));
#52956=CARTESIAN_POINT('Ctrl Pts',(-2.85520533840869,6.13515211510868,18.9414676801255));
#52957=CARTESIAN_POINT('Ctrl Pts',(-3.02384747998307,6.05666865881131,18.9502173345567));
#52958=CARTESIAN_POINT('Ctrl Pts',(-3.18925164684516,5.97122791039855,18.9589669889879));
#52959=CARTESIAN_POINT('Ctrl Pts',(-3.35085601829136,5.87912008251921,18.9677166434192));
#52960=CARTESIAN_POINT('Ctrl Pts',(-3.51245754191393,5.78701387778189,18.9764661436623));
#52961=CARTESIAN_POINT('Ctrl Pts',(-3.67025915510908,5.68824097061001,18.9852156439055));
#52962=CARTESIAN_POINT('Ctrl Pts',(-3.82372487928803,5.58313684656876,18.9939651441486));
#52963=CARTESIAN_POINT('Ctrl Pts',(-3.97718810300769,5.47803443501794,19.0027145018337));
#52964=CARTESIAN_POINT('Ctrl Pts',(-4.12631534262998,5.36660117496397,19.0114638595188));
#52965=CARTESIAN_POINT('Ctrl Pts',(-4.270600098862,5.24921554097371,19.020213217204));
#52966=CARTESIAN_POINT('Ctrl Pts',(-4.41488269594181,5.13183166360319,19.0289624439591));
#52967=CARTESIAN_POINT('Ctrl Pts',(-4.5543227323505,5.00849577139506,19.0377116707143));
#52968=CARTESIAN_POINT('Ctrl Pts',(-4.68844662480162,4.87962675277385,19.0464608974695));
#52969=CARTESIAN_POINT('Ctrl Pts',(-4.82256868835107,4.75075949139933,19.055210004921));
#52970=CARTESIAN_POINT('Ctrl Pts',(-4.95137454637806,4.61635945312585,19.0639591123725));
#52971=CARTESIAN_POINT('Ctrl Pts',(-5.07442674461018,4.47688309134659,19.072708219824));
#52972=CARTESIAN_POINT('Ctrl Pts',(-5.19747742838489,4.33740844616411,19.0814572195963));
#52973=CARTESIAN_POINT('Ctrl Pts',(-5.31477440450888,4.19285781736079,19.0902062193687));
#52974=CARTESIAN_POINT('Ctrl Pts',(-5.42591931531123,4.04372211999446,19.0989552191411));
#52975=CARTESIAN_POINT('Ctrl Pts',(-5.5370763646295,3.89457013500846,19.1077051744216));
#52976=CARTESIAN_POINT('Ctrl Pts',(-5.64207983273437,3.7408323091647,19.1164551297022));
#52977=CARTESIAN_POINT('Ctrl Pts',(-5.74057303468713,3.58303087251882,19.1252050849828));
#52978=CARTESIAN_POINT('Ctrl Pts',(-5.83906243363732,3.42523552887487,19.1339547024116));
#52979=CARTESIAN_POINT('Ctrl Pts',(-5.93104191768394,3.26337713157051,19.1427043198404));
#52980=CARTESIAN_POINT('Ctrl Pts',(-6.01619906699625,3.09800545291216,19.1514539372692));
#52981=CARTESIAN_POINT('Ctrl Pts',(-6.10135338095357,2.93263928039649,19.1602032633746));
#52982=CARTESIAN_POINT('Ctrl Pts',(-6.17968568352818,2.76376031540271,19.16895258948));
#52983=CARTESIAN_POINT('Ctrl Pts',(-6.2509299269487,2.59194213831582,19.1777019155854));
#52984=CARTESIAN_POINT('Ctrl Pts',(-6.32217217691088,2.42012876880862,19.1864509968792));
#52985=CARTESIAN_POINT('Ctrl Pts',(-6.38632665483835,2.24537661647713,19.195200078173));
#52986=CARTESIAN_POINT('Ctrl Pts',(-6.44317547869336,2.06827917621501,19.2039491594668));
#52987=CARTESIAN_POINT('Ctrl Pts',(-6.50002944235924,1.89116572423465,19.2126990317818));
#52988=CARTESIAN_POINT('Ctrl Pts',(-6.54957634250388,1.71170683289236,19.2214489040967));
#52989=CARTESIAN_POINT('Ctrl Pts',(-6.59164787708387,1.53051209225399,19.2301987764117));
#52990=CARTESIAN_POINT('Ctrl Pts',(-6.63371649075001,1.34932993148068,19.2389480412465));
#52991=CARTESIAN_POINT('Ctrl Pts',(-6.66831071257117,1.16641244174045,19.2476973060813));
#52992=CARTESIAN_POINT('Ctrl Pts',(-6.69531304840326,0.982380875160461,
19.2564465709161));
#52993=CARTESIAN_POINT('Ctrl Pts',(-6.72231677033039,0.798339861796263,
19.2651962848717));
#52994=CARTESIAN_POINT('Ctrl Pts',(-6.74172778477886,0.613184940730545,
19.2739459988274));
#52995=CARTESIAN_POINT('Ctrl Pts',(-6.75348015835516,0.427545027690915,
19.2826957127831));
#52996=CARTESIAN_POINT('Ctrl Pts',(-6.76249038365213,0.285219953548288,
19.2894038805853));
#52997=CARTESIAN_POINT('Ctrl Pts',(-6.76699999999993,0.142609995759882,
19.2961120483875));
#52998=CARTESIAN_POINT('Ctrl Pts',(-6.767,3.60156657358884E-12,19.3028202161898));
#52999=CARTESIAN_POINT('Ctrl Pts',(-6.7669973892787,-0.00594419845536852,
19.3028202161898));
#53000=CARTESIAN_POINT('Ctrl Pts',(-6.76678148696253,-0.251731821604794,
19.3144057968282));
#53001=CARTESIAN_POINT('Ctrl Pts',(-6.75317158476609,-0.496930574792495,
19.3259913774667));
#53002=CARTESIAN_POINT('Ctrl Pts',(-6.72637726539961,-0.740363345604933,
19.3375769581052));
#53003=CARTESIAN_POINT('Ctrl Pts',(-6.6982552193013,-0.995858829889866,
19.3497366337563));
#53004=CARTESIAN_POINT('Ctrl Pts',(-6.655609497569,-1.24940987343356,19.3618963094075));
#53005=CARTESIAN_POINT('Ctrl Pts',(-6.59872934408692,-1.49968664843233,
19.3740559850587));
#53006=CARTESIAN_POINT('Ctrl Pts',(-6.58649778794481,-1.55350637705577,
19.3766708119586));
#53007=CARTESIAN_POINT('Ctrl Pts',(-6.57360816990642,-1.60717477434293,
19.3792856388585));
#53008=CARTESIAN_POINT('Ctrl Pts',(-6.56006365577417,-1.66067872636184,
19.3819004657585));
#53009=CARTESIAN_POINT('Ctrl Pts',(-6.51825462790827,-1.8258340209005,19.3899718790005));
#53010=CARTESIAN_POINT('Ctrl Pts',(-6.47012764472255,-1.9897132384509,19.3980432922425));
#53011=CARTESIAN_POINT('Ctrl Pts',(-6.41577085801813,-2.15178374782535,
19.4061147054845));
#53012=CARTESIAN_POINT('Ctrl Pts',(-6.36148231175712,-2.31365079109937,
19.4141759857358));
#53013=CARTESIAN_POINT('Ctrl Pts',(-6.30097964085668,-2.47371329515649,
19.422237265987));
#53014=CARTESIAN_POINT('Ctrl Pts',(-6.23440205186282,-2.63144828102865,
19.4302985462383));
#53015=CARTESIAN_POINT('Ctrl Pts',(-6.16789344474438,-2.7890198357026,19.4383514740959));
#53016=CARTESIAN_POINT('Ctrl Pts',(-6.09532258917428,-2.94426833059145,
19.4464044019535));
#53017=CARTESIAN_POINT('Ctrl Pts',(-6.01687856773649,-3.09668553474732,
19.4544573298111));
#53018=CARTESIAN_POINT('Ctrl Pts',(-5.93849864569332,-3.24897819339498,
19.4625036773355));
#53019=CARTESIAN_POINT('Ctrl Pts',(-5.85425527957901,-3.39844383612653,
19.4705500248599));
#53020=CARTESIAN_POINT('Ctrl Pts',(-5.76438573185665,-3.54459393081457,
19.4785963723843));
#53021=CARTESIAN_POINT('Ctrl Pts',(-5.67456996091978,-3.69065657115916,
19.4866379050775));
#53022=CARTESIAN_POINT('Ctrl Pts',(-5.57913490524292,-3.83340729609017,
19.4946794377706));
#53023=CARTESIAN_POINT('Ctrl Pts',(-5.47836381126608,-3.9723820248574,19.5027209704638));
#53024=CARTESIAN_POINT('Ctrl Pts',(-5.37565541946049,-4.11402850630357,
19.510917099512));
#53025=CARTESIAN_POINT('Ctrl Pts',(-5.26740391589171,-4.25175197760208,
19.5191132285603));
#53026=CARTESIAN_POINT('Ctrl Pts',(-5.15395588504798,-4.38509153096937,
19.5273093576085));
#53027=CARTESIAN_POINT('Ctrl Pts',(-5.04268614684367,-4.51587085860614,
19.5353481144446));
#53028=CARTESIAN_POINT('Ctrl Pts',(-4.92641789533958,-4.64243281165157,
19.5433868712807));
#53029=CARTESIAN_POINT('Ctrl Pts',(-4.80551885472306,-4.76437588115182,
19.5514256281168));
#53030=CARTESIAN_POINT('Ctrl Pts',(-4.6846081123571,-4.88633075345248,19.5594651630196));
#53031=CARTESIAN_POINT('Ctrl Pts',(-4.55906595129381,-5.0036655867268,19.5675046979224));
#53032=CARTESIAN_POINT('Ctrl Pts',(-4.42929674974193,-5.11601595997565,
19.5755442328252));
#53033=CARTESIAN_POINT('Ctrl Pts',(-4.29948929355575,-5.22839945296625,
19.5835861377007));
#53034=CARTESIAN_POINT('Ctrl Pts',(-4.16545259877468,-5.33579531687339,
19.5916280425763));
#53035=CARTESIAN_POINT('Ctrl Pts',(-4.02762375514728,-5.43787972347434,
19.5996699474518));
#53036=CARTESIAN_POINT('Ctrl Pts',(-3.88514563006092,-5.54340767009469,
19.6079831241326));
#53037=CARTESIAN_POINT('Ctrl Pts',(-3.73861539616346,-5.64325929633916,
19.6162963008134));
#53038=CARTESIAN_POINT('Ctrl Pts',(-3.58854698120328,-5.73712642040393,
19.6246094774942));
#53039=CARTESIAN_POINT('Ctrl Pts',(-3.44312347706519,-5.82808817347159,
19.6326653451048));
#53040=CARTESIAN_POINT('Ctrl Pts',(-3.29437791185248,-5.91343024907903,
19.6407212127153));
#53041=CARTESIAN_POINT('Ctrl Pts',(-3.14280113920245,-5.99291998940648,
19.6487770803258));
#53042=CARTESIAN_POINT('Ctrl Pts',(-2.98396219188709,-6.07621815214766,
19.6572189115418));
#53043=CARTESIAN_POINT('Ctrl Pts',(-2.82201451069582,-6.1530891941694,19.6656607427577));
#53044=CARTESIAN_POINT('Ctrl Pts',(-2.65754349422894,-6.22332319394401,
19.6741025739737));
#53045=CARTESIAN_POINT('Ctrl Pts',(-2.49307247776206,-6.29355719371862,
19.6825444051897));
#53046=CARTESIAN_POINT('Ctrl Pts',(-2.32607858739046,-6.35715406711887,
19.6909862364056));
#53047=CARTESIAN_POINT('Ctrl Pts',(-2.15716150908466,-6.41396470396615,
19.6994280676216));
#53048=CARTESIAN_POINT('Ctrl Pts',(-1.99247394825558,-6.46935285835151,
19.7076585236881));
#53049=CARTESIAN_POINT('Ctrl Pts',(-1.82541072593333,-6.51847512866971,
19.7158889797547));
#53050=CARTESIAN_POINT('Ctrl Pts',(-1.65648915888423,-6.56112282056197,
19.7241194358212));
#53051=CARTESIAN_POINT('Ctrl Pts',(-1.48776811168905,-6.6037198871309,19.7323401218515));
#53052=CARTESIAN_POINT('Ctrl Pts',(-1.31719345653477,-6.63985759232926,
19.7405608078817));
#53053=CARTESIAN_POINT('Ctrl Pts',(-1.1453007104705,-6.66937592902033,19.7487814939119));
#53054=CARTESIAN_POINT('Ctrl Pts',(-0.973577524222988,-6.69886514799774,
19.7569940708273));
#53055=CARTESIAN_POINT('Ctrl Pts',(-0.800539187322688,-6.72174794169361,
19.7652066477426));
#53056=CARTESIAN_POINT('Ctrl Pts',(-0.62673463512712,-6.73791456588254,
19.773419224658));
#53057=CARTESIAN_POINT('Ctrl Pts',(-0.453066670565052,-6.75406848522046,
19.7816253475626));
#53058=CARTESIAN_POINT('Ctrl Pts',(-0.278634045422089,-6.76351671465871,
19.7898314704673));
#53059=CARTESIAN_POINT('Ctrl Pts',(-0.103994198741046,-6.7662008695152,
19.7980375933719));
#53060=CARTESIAN_POINT('Ctrl Pts',(0.0705434204438084,-6.76888345316995,
19.8062389127257));
#53061=CARTESIAN_POINT('Ctrl Pts',(0.245287662004282,-6.76480984439387,
19.8144402320794));
#53062=CARTESIAN_POINT('Ctrl Pts',(0.419677582265115,-6.75397362498138,
19.8226415514331));
#53063=CARTESIAN_POINT('Ctrl Pts',(0.594017474189871,-6.74314051422348,
19.8308405180226));
#53064=CARTESIAN_POINT('Ctrl Pts',(0.768002889656946,-6.72554867539881,
19.8390394846121));
#53065=CARTESIAN_POINT('Ctrl Pts',(0.941074250497254,-6.70124378418298,
19.8472384512016));
#53066=CARTESIAN_POINT('Ctrl Pts',(1.11412275648244,-6.67694210253784,19.8554363350806));
#53067=CARTESIAN_POINT('Ctrl Pts',(1.28625709310994,-6.64592918310876,19.8636342189595));
#53068=CARTESIAN_POINT('Ctrl Pts',(1.45692414916047,-6.60830243130511,19.8718321028384));
#53069=CARTESIAN_POINT('Ctrl Pts',(1.62759967001688,-6.57067381327633,19.8800303933189));
#53070=CARTESIAN_POINT('Ctrl Pts',(1.79680741507235,-6.52643078652049,19.8882286837995));
#53071=CARTESIAN_POINT('Ctrl Pts',(1.96400573537052,-6.47572161781463,19.89642697428));
#53072=CARTESIAN_POINT('Ctrl Pts',(2.13124272040526,-6.4250007225756,19.9046271606213));
#53073=CARTESIAN_POINT('Ctrl Pts',(2.29646901206936,-6.3678108112492,19.9128273469627));
#53074=CARTESIAN_POINT('Ctrl Pts',(2.45915930736879,-6.30434964932795,19.921027533304));
#53075=CARTESIAN_POINT('Ctrl Pts',(2.62200341357712,-6.24082848985751,19.9292354722781));
#53076=CARTESIAN_POINT('Ctrl Pts',(2.78230639878598,-6.17102436484951,19.9374434112522));
#53077=CARTESIAN_POINT('Ctrl Pts',(2.9395632294928,-6.09518309977755,19.9456513502263));
#53078=CARTESIAN_POINT('Ctrl Pts',(3.09689635025264,-6.01930504181013,19.9538632711202));
#53079=CARTESIAN_POINT('Ctrl Pts',(3.25118005362063,-5.93738417250636,19.9620751920142));
#53080=CARTESIAN_POINT('Ctrl Pts',(3.40193510144856,-5.84971166516198,19.9702871129082));
#53081=CARTESIAN_POINT('Ctrl Pts',(3.55289688594214,-5.76191892886277,19.9785102951507));
#53082=CARTESIAN_POINT('Ctrl Pts',(3.70032004145717,-5.66835898383597,19.9867334773933));
#53083=CARTESIAN_POINT('Ctrl Pts',(3.8437544341694,-5.56936628799032,19.9949566596358));
#53084=CARTESIAN_POINT('Ctrl Pts',(3.97166171405434,-5.48108978599754,20.0022896629187));
#53085=CARTESIAN_POINT('Ctrl Pts',(4.09639737778694,-5.38849378016287,20.0096226662017));
#53086=CARTESIAN_POINT('Ctrl Pts',(4.21766570116052,-5.29184136508779,20.0169556694846));
#53087=CARTESIAN_POINT('Ctrl Pts',(4.36542986794342,-5.17407142167784,20.0258908562669));
#53088=CARTESIAN_POINT('Ctrl Pts',(4.50835245263275,-5.05003426305525,20.0348260430492));
#53089=CARTESIAN_POINT('Ctrl Pts',(4.64591986172555,-4.92013390452171,20.0437612298314));
#53090=CARTESIAN_POINT('Ctrl Pts',(4.78328123739679,-4.79042809653985,20.0526830344681));
#53091=CARTESIAN_POINT('Ctrl Pts',(4.91530325354397,-4.65487678725042,20.0616048391047));
#53092=CARTESIAN_POINT('Ctrl Pts',(5.04150607776926,-4.51392351151585,20.0705266437414));
#53093=CARTESIAN_POINT('Ctrl Pts',(5.16740106337686,-4.37331405424833,20.0794266859806));
#53094=CARTESIAN_POINT('Ctrl Pts',(5.28750501464005,-4.2273291210464,20.0883267282199));
#53095=CARTESIAN_POINT('Ctrl Pts',(5.40137598380592,-4.07644777736262,20.0972267704592));
#53096=CARTESIAN_POINT('Ctrl Pts',(5.51507164694044,-3.92579871772594,20.1061131109526));
#53097=CARTESIAN_POINT('Ctrl Pts',(5.62255331420112,-3.77026848932627,20.114999451446));
#53098=CARTESIAN_POINT('Ctrl Pts',(5.72341829897401,-3.61037006066823,20.1238857919394));
#53099=CARTESIAN_POINT('Ctrl Pts',(5.82402538958749,-3.45088046438092,20.1327494116114));
#53100=CARTESIAN_POINT('Ctrl Pts',(5.91804941852547,-3.28704517217004,20.1416130312833));
#53101=CARTESIAN_POINT('Ctrl Pts',(6.00513053934645,-3.11940638670382,20.1504766509552));
#53102=CARTESIAN_POINT('Ctrl Pts',(6.08779703048986,-2.96026615006718,20.1588909241088));
#53103=CARTESIAN_POINT('Ctrl Pts',(6.16420688657542,-2.79769867385645,20.1673051972624));
#53104=CARTESIAN_POINT('Ctrl Pts',(6.23408762025623,-2.63219310518208,20.175719470416));
#53105=CARTESIAN_POINT('Ctrl Pts',(6.30227392200353,-2.47070063004526,20.1839297186205));
#53106=CARTESIAN_POINT('Ctrl Pts',(6.36417742337436,-2.30656562611901,20.192139966825));
#53107=CARTESIAN_POINT('Ctrl Pts',(6.41960476151267,-2.14031859917254,20.2003502150296));
#53108=CARTESIAN_POINT('Ctrl Pts',(6.47504527583429,-1.97403205199336,20.2085624149738));
#53109=CARTESIAN_POINT('Ctrl Pts',(6.52400644718736,-1.8056328192079,20.216774614918));
#53110=CARTESIAN_POINT('Ctrl Pts',(6.56634474621996,-1.63566673677421,20.2249868148623));
#53111=CARTESIAN_POINT('Ctrl Pts',(6.60870064917459,-1.46562998381924,20.2332024293727));
#53112=CARTESIAN_POINT('Ctrl Pts',(6.6444281077952,-1.29402542842772,20.2414180438832));
#53113=CARTESIAN_POINT('Ctrl Pts',(6.67343465260615,-1.12140935317816,20.2496336583937));
#53114=CARTESIAN_POINT('Ctrl Pts',(6.70247377049535,-0.94859943764315,20.2578584986791));
#53115=CARTESIAN_POINT('Ctrl Pts',(6.72477684118185,-0.774776084664146,
20.2660833389645));
#53116=CARTESIAN_POINT('Ctrl Pts',(6.74030314047907,-0.600501935424053,
20.27430817925));
#53117=CARTESIAN_POINT('Ctrl Pts',(6.75583938491071,-0.426116157533253,
20.2825382878315));
#53118=CARTESIAN_POINT('Ctrl Pts',(6.76459018712003,-0.251279362352467,
20.2907683964131));
#53119=CARTESIAN_POINT('Ctrl Pts',(6.76656695989601,-0.0765544070821397,
20.2989985049946));
#53120=CARTESIAN_POINT('Ctrl Pts',(6.7685464428578,0.0984100987830904,20.3072398971813));
#53121=CARTESIAN_POINT('Ctrl Pts',(6.76373335575344,0.273262103706231,20.315481289368));
#53122=CARTESIAN_POINT('Ctrl Pts',(6.75219105778701,0.447442643409409,20.3237226815547));
#53123=CARTESIAN_POINT('Ctrl Pts',(6.747167556463,0.523250439600418,20.327309544819));
#53124=CARTESIAN_POINT('Ctrl Pts',(6.74087005937798,0.598931157170586,20.3308964080833));
#53125=CARTESIAN_POINT('Ctrl Pts',(6.73330680843956,0.674439340060628,20.3344832713476));
#53126=CARTESIAN_POINT('Ctrl Pts',(6.71549231908453,0.852291394853806,20.3429317729193));
#53127=CARTESIAN_POINT('Ctrl Pts',(6.69061148799602,1.02959114221899,20.351380274491));
#53128=CARTESIAN_POINT('Ctrl Pts',(6.65871202097412,1.20575421282065,20.3598287760627));
#53129=CARTESIAN_POINT('Ctrl Pts',(6.62684169745718,1.38175634000225,20.3682695590431));
#53130=CARTESIAN_POINT('Ctrl Pts',(6.58796557872047,1.55662353387428,20.3767103420235));
#53131=CARTESIAN_POINT('Ctrl Pts',(6.54218306238557,1.72977737822977,20.3851511250039));
#53132=CARTESIAN_POINT('Ctrl Pts',(6.49643533279525,1.9027996557986,20.3935854944582));
#53133=CARTESIAN_POINT('Ctrl Pts',(6.44379175181674,2.07411085786092,20.4020198639125));
#53134=CARTESIAN_POINT('Ctrl Pts',(6.38440268310488,2.24314319203283,20.4104542333669));
#53135=CARTESIAN_POINT('Ctrl Pts',(6.3250496194929,2.41207304899458,20.418883489417));
#53136=CARTESIAN_POINT('Ctrl Pts',(6.2589593318243,2.57872647876713,20.4273127454671));
#53137=CARTESIAN_POINT('Ctrl Pts',(6.18633199707147,2.74255089688591,20.4357420015173));
#53138=CARTESIAN_POINT('Ctrl Pts',(6.11373755238869,2.90630112535411,20.4441674402881));
#53139=CARTESIAN_POINT('Ctrl Pts',(6.03461209856751,3.06722459248032,20.4525928790589));
#53140=CARTESIAN_POINT('Ctrl Pts',(5.94920405625126,3.22478838020165,20.4610183178298));
#53141=CARTESIAN_POINT('Ctrl Pts',(5.86381485763857,3.38231740438986,20.4694418976835));
#53142=CARTESIAN_POINT('Ctrl Pts',(5.77214599069726,3.53648793298379,20.4778654775372));
#53143=CARTESIAN_POINT('Ctrl Pts',(5.67449221830271,3.68679088970639,20.4862890573909));
#53144=CARTESIAN_POINT('Ctrl Pts',(5.57684939438853,3.83707699517039,20.4947116928326));
#53145=CARTESIAN_POINT('Ctrl Pts',(5.47322318431893,3.98349611368803,20.5031343282742));
#53146=CARTESIAN_POINT('Ctrl Pts',(5.36395231130543,4.12556718549597,20.5115569637159));
#53147=CARTESIAN_POINT('Ctrl Pts',(5.25467845185882,4.26764214018452,20.5199798293529));
#53148=CARTESIAN_POINT('Ctrl Pts',(5.13975982546946,4.40536854721088,20.5284026949898));
#53149=CARTESIAN_POINT('Ctrl Pts',(5.01957638258124,4.53829725111001,20.5368255606267));
#53150=CARTESIAN_POINT('Ctrl Pts',(4.89937289493421,4.67124812548241,20.5452498310687));
#53151=CARTESIAN_POINT('Ctrl Pts',(4.77390306415786,4.79939945453999,20.5536741015108));
#53152=CARTESIAN_POINT('Ctrl Pts',(4.64358498523711,4.92233760370827,20.5620983719528));
#53153=CARTESIAN_POINT('Ctrl Pts',(4.51317933547137,5.04535836457321,20.5705283033168));
#53154=CARTESIAN_POINT('Ctrl Pts',(4.37791917034344,5.16315871655745,20.5789582346808));
#53155=CARTESIAN_POINT('Ctrl Pts',(4.23825782685266,5.27536345602103,20.5873881660448));
#53156=CARTESIAN_POINT('Ctrl Pts',(4.09854656058211,5.38760830373761,20.595821110738));
#53157=CARTESIAN_POINT('Ctrl Pts',(3.95443124273722,5.49425334666627,20.6042540554313));
#53158=CARTESIAN_POINT('Ctrl Pts',(3.80639616587544,5.59496534648864,20.6126870001245));
#53159=CARTESIAN_POINT('Ctrl Pts',(3.65822600690346,5.69576924608063,20.6211276398856));
#53160=CARTESIAN_POINT('Ctrl Pts',(3.50612922199424,5.79062910351373,20.6295682796468));
#53161=CARTESIAN_POINT('Ctrl Pts',(3.3506177196932,5.87925589649557,20.6380089194079));
#53162=CARTESIAN_POINT('Ctrl Pts',(3.26771690240264,5.92650149224458,20.6425084961228));
#53163=CARTESIAN_POINT('Ctrl Pts',(3.18384611222608,5.97197655998786,20.6470080728376));
#53164=CARTESIAN_POINT('Ctrl Pts',(3.09908550384707,6.0156427786102,20.6515076495525));
#53165=CARTESIAN_POINT('Origin',(0.,0.,-63.6971797838103));
#53166=CARTESIAN_POINT('',(3.09908550384706,6.0156427786102,23.0456261631097));
#53167=CARTESIAN_POINT('',(3.09908550384738,6.01564277861003,22.6514909292461));
#53168=CARTESIAN_POINT('',(3.09908550384721,6.01564277861012,-63.6971797838103));
#53169=CARTESIAN_POINT('',(-6.76699855717881,0.00441895236067136,21.6971797837833));
#53170=CARTESIAN_POINT('Ctrl Pts',(-6.76699855717918,0.00441895179320035,
21.6971797838099));
#53171=CARTESIAN_POINT('Ctrl Pts',(-6.76711125264251,-0.168158182668951,
21.7052796560254));
#53172=CARTESIAN_POINT('Ctrl Pts',(-6.76061791801425,-0.340884502066218,
21.7133795282409));
#53173=CARTESIAN_POINT('Ctrl Pts',(-6.7475109834384,-0.513210023653212,
21.7214794004565));
#53174=CARTESIAN_POINT('Ctrl Pts',(-6.73864096822721,-0.62982996929403,
21.7269609254725));
#53175=CARTESIAN_POINT('Ctrl Pts',(-6.72674313303695,-0.74626625523307,
21.7324424504885));
#53176=CARTESIAN_POINT('Ctrl Pts',(-6.71182868254392,-0.862348384459978,
21.7379239755045));
#53177=CARTESIAN_POINT('Ctrl Pts',(-6.68948976408141,-1.03621662190972,
21.746134223709));
#53178=CARTESIAN_POINT('Ctrl Pts',(-6.66039171995952,-1.20920693037894,
21.7543444719136));
#53179=CARTESIAN_POINT('Ctrl Pts',(-6.62463440377626,-1.38076356278109,
21.7625547201181));
#53180=CARTESIAN_POINT('Ctrl Pts',(-6.58886858736612,-1.55236097761478,
21.7707669200624));
#53181=CARTESIAN_POINT('Ctrl Pts',(-6.5464404176516,-1.72252368891705,21.7789791200066));
#53182=CARTESIAN_POINT('Ctrl Pts',(-6.49750052696888,-1.89070777806598,
21.7871913199508));
#53183=CARTESIAN_POINT('Ctrl Pts',(-6.44854028747589,-2.05896179679732,
21.7954069344613));
#53184=CARTESIAN_POINT('Ctrl Pts',(-6.39306303241003,-2.22523521289516,
21.8036225489718));
#53185=CARTESIAN_POINT('Ctrl Pts',(-6.33126877521517,-2.38900077354223,
21.8118381634822));
#53186=CARTESIAN_POINT('Ctrl Pts',(-6.26940512577825,-2.5529502357352,21.8200630037677));
#53187=CARTESIAN_POINT('Ctrl Pts',(-6.20121043147482,-2.71438588443705,
21.8282878440531));
#53188=CARTESIAN_POINT('Ctrl Pts',(-6.12693262206969,-2.87280101027173,
21.8365126843385));
#53189=CARTESIAN_POINT('Ctrl Pts',(-6.05260723514554,-3.03131760650144,
21.8447427929201));
#53190=CARTESIAN_POINT('Ctrl Pts',(-5.97219112883533,-3.18680950768719,
21.8529729015016));
#53191=CARTESIAN_POINT('Ctrl Pts',(-5.88597739674428,-3.3387960532227,21.8612030100832));
#53192=CARTESIAN_POINT('Ctrl Pts',(-5.79964546430348,-3.49099097464454,
21.8694444022699));
#53193=CARTESIAN_POINT('Ctrl Pts',(-5.70750021648081,-3.63967063948447,
21.8776857944566));
#53194=CARTESIAN_POINT('Ctrl Pts',(-5.60987767841737,-3.78438389083276,
21.8859271866433));
#53195=CARTESIAN_POINT('Ctrl Pts',(-5.56738986960998,-3.8473667744696,21.8895140499075));
#53196=CARTESIAN_POINT('Ctrl Pts',(-5.52386505985673,-3.90959876316506,
21.8931009131717));
#53197=CARTESIAN_POINT('Ctrl Pts',(-5.47933324514882,-3.97104472256444,
21.8966877764359));
#53198=CARTESIAN_POINT('Ctrl Pts',(-5.3744430448401,-4.11577448558528,21.9051362712643));
#53199=CARTESIAN_POINT('Ctrl Pts',(-5.2637242651968,-4.25647116895907,21.9135847660927));
#53200=CARTESIAN_POINT('Ctrl Pts',(-5.14751218724185,-4.39265378583342,
21.9220332609211));
#53201=CARTESIAN_POINT('Ctrl Pts',(-5.03140626226963,-4.52871200779777,
21.9304740385403));
#53202=CARTESIAN_POINT('Ctrl Pts',(-4.90981725641308,-4.6602641298948,21.9389148161594));
#53203=CARTESIAN_POINT('Ctrl Pts',(-4.78312212557501,-4.78686032090292,
21.9473555937786));
#53204=CARTESIAN_POINT('Ctrl Pts',(-4.65652324039093,-4.91336034141801,
21.9557899592479));
#53205=CARTESIAN_POINT('Ctrl Pts',(-4.52482619797284,-5.03491170122852,
21.9642243247172));
#53206=CARTESIAN_POINT('Ctrl Pts',(-4.38844665165136,-5.1510993958193,21.9726586901865));
#53207=CARTESIAN_POINT('Ctrl Pts',(-4.25214976438765,-5.267216669547,21.9810879436231));
#53208=CARTESIAN_POINT('Ctrl Pts',(-4.11117628473948,-5.37797654378555,
21.9895171970597));
#53209=CARTESIAN_POINT('Ctrl Pts',(-3.96597726064723,-5.48300222214337,
21.9979464504963));
#53210=CARTESIAN_POINT('Ctrl Pts',(-3.82084396795233,-5.58798035552188,
22.0063718880216));
#53211=CARTESIAN_POINT('Ctrl Pts',(-3.67148921488254,-5.68722927411314,
22.0147973255468));
#53212=CARTESIAN_POINT('Ctrl Pts',(-3.51839584407446,-5.78041345272114,
22.023222763072));
#53213=CARTESIAN_POINT('Ctrl Pts',(-3.36533610376296,-5.87357716127102,
22.0316463497552));
#53214=CARTESIAN_POINT('Ctrl Pts',(-3.20853966636499,-5.96067861065335,
22.0400699364384));
#53215=CARTESIAN_POINT('Ctrl Pts',(-3.048517426255,-6.04142619766389,22.0484935231216));
#53216=CARTESIAN_POINT('Ctrl Pts',(-2.88851309179476,-6.12216474944278,
22.0569161672495));
#53217=CARTESIAN_POINT('Ctrl Pts',(-2.72528397179574,-6.19655070603551,
22.0653388113776));
#53218=CARTESIAN_POINT('Ctrl Pts',(-2.55936485224373,-6.26433879616192,
22.0737614555055));
#53219=CARTESIAN_POINT('Ctrl Pts',(-2.39344116142092,-6.33212875393156,
22.0821843316875));
#53220=CARTESIAN_POINT('Ctrl Pts',(-2.22482763206665,-6.39332035708,22.0906072078694));
#53221=CARTESIAN_POINT('Ctrl Pts',(-2.05407862358452,-6.4477166507325,22.0990300840514));
#53222=CARTESIAN_POINT('Ctrl Pts',(-1.88330109907076,-6.50212202886781,
22.1074543669004));
#53223=CARTESIAN_POINT('Ctrl Pts',(-1.71038770221262,-6.54972973433226,
22.1158786497494));
#53224=CARTESIAN_POINT('Ctrl Pts',(-1.53590788198711,-6.59039270287059,
22.1243029325984));
#53225=CARTESIAN_POINT('Ctrl Pts',(-1.36131022454225,-6.63108313367439,
22.1327329048965));
#53226=CARTESIAN_POINT('Ctrl Pts',(-1.18514435482528,-6.66481937969628,
22.1411628771946));
#53227=CARTESIAN_POINT('Ctrl Pts',(-1.0079908442802,-6.69150532076657,22.1495928494928));
#53228=CARTESIAN_POINT('Ctrl Pts',(-0.83077400421468,-6.71820080163004,
22.1580258353699));
#53229=CARTESIAN_POINT('Ctrl Pts',(-0.652569149889286,-6.73784090846588,
22.1664588212471));
#53230=CARTESIAN_POINT('Ctrl Pts',(-0.473962486645386,-6.7503813641344,
22.1748918071243));
#53231=CARTESIAN_POINT('Ctrl Pts',(-0.295191506358986,-6.76293335694576,
22.1833325512971));
#53232=CARTESIAN_POINT('Ctrl Pts',(-0.116018311720531,-6.76837263141582,
22.1917732954699));
#53233=CARTESIAN_POINT('Ctrl Pts',(0.0629692635081873,-6.76670701832533,
22.2002140396427));
#53234=CARTESIAN_POINT('Ctrl Pts',(0.161936274185537,-6.76578605636302,
22.2048811525281));
#53235=CARTESIAN_POINT('Ctrl Pts',(0.260846564772378,-6.76269385613586,
22.2095482654135));
#53236=CARTESIAN_POINT('Ctrl Pts',(0.359601331876994,-6.75743855925545,
22.2142153782989));
#53237=CARTESIAN_POINT('Ctrl Pts',(0.531870321990595,-6.74827115688209,
22.2223567455168));
#53238=CARTESIAN_POINT('Ctrl Pts',(0.704008070814728,-6.73250022156963,
22.2304981127347));
#53239=CARTESIAN_POINT('Ctrl Pts',(0.875464168136037,-6.71013051216665,
22.2386394799526));
#53240=CARTESIAN_POINT('Ctrl Pts',(1.04677059732388,-6.68778032981873,22.246773740376));
#53241=CARTESIAN_POINT('Ctrl Pts',(1.21739619892367,-6.65884288622386,22.2549080007994));
#53242=CARTESIAN_POINT('Ctrl Pts',(1.38679251798085,-6.62337493367787,22.2630422612229));
#53243=CARTESIAN_POINT('Ctrl Pts',(1.55607328098818,-6.58793117608792,22.2711709727477));
#53244=CARTESIAN_POINT('Ctrl Pts',(1.72412607420585,-6.54596585377698,22.2792996842726));
#53245=CARTESIAN_POINT('Ctrl Pts',(1.89040954964891,-6.49758730103692,22.2874283957974));
#53246=CARTESIAN_POINT('Ctrl Pts',(2.05661372757562,-6.44923181913457,22.2955532308899));
#53247=CARTESIAN_POINT('Ctrl Pts',(2.22104991720915,-6.39446929909738,22.3036780659824));
#53248=CARTESIAN_POINT('Ctrl Pts',(2.38318893864969,-6.33345872984878,22.311802901075));
#53249=CARTESIAN_POINT('Ctrl Pts',(2.54528256881695,-6.27246524067997,22.3199254615971));
#53250=CARTESIAN_POINT('Ctrl Pts',(2.7050799697127,-6.20522731586441,22.3280480221193));
#53251=CARTESIAN_POINT('Ctrl Pts',(2.86206908450194,-6.13195315992696,22.3361705826415));
#53252=CARTESIAN_POINT('Ctrl Pts',(3.01906654285522,-6.05867510965829,22.3442935748566));
#53253=CARTESIAN_POINT('Ctrl Pts',(3.17325508357313,-5.97936033865593,22.3524165670719));
#53254=CARTESIAN_POINT('Ctrl Pts',(3.32414435746671,-5.89426444017591,22.360539559287));
#53255=CARTESIAN_POINT('Ctrl Pts',(3.40116873350251,-5.85082557726341,22.3646860992681));
#53256=CARTESIAN_POINT('Ctrl Pts',(3.47733377062505,-5.80588101977382,22.3688326392492));
#53257=CARTESIAN_POINT('Ctrl Pts',(3.55257685114073,-5.75946930860292,22.3729791792303));
#53258=CARTESIAN_POINT('Ctrl Pts',(3.71559425424743,-5.65891631985014,22.3819628382587));
#53259=CARTESIAN_POINT('Ctrl Pts',(3.8742018412101,-5.55152394140958,22.3909464972871));
#53260=CARTESIAN_POINT('Ctrl Pts',(4.02786701279647,-5.43769954366974,22.3999301563154));
#53261=CARTESIAN_POINT('Ctrl Pts',(4.18179617951964,-5.32367959682047,22.4089292491748));
#53262=CARTESIAN_POINT('Ctrl Pts',(4.33076576751449,-5.20320568691012,22.4179283420343));
#53263=CARTESIAN_POINT('Ctrl Pts',(4.47427632467089,-5.07672535897793,22.4269274348937));
#53264=CARTESIAN_POINT('Ctrl Pts',(4.61812337397992,-4.94994847002155,22.435947628111));
#53265=CARTESIAN_POINT('Ctrl Pts',(4.75648560198327,-4.81713714346964,22.4449678213284));
#53266=CARTESIAN_POINT('Ctrl Pts',(4.88889853712001,-4.67877762815736,22.4539880145458));
#53267=CARTESIAN_POINT('Ctrl Pts',(5.0214455735105,-4.54027798918985,22.4630173429675));
#53268=CARTESIAN_POINT('Ctrl Pts',(5.14803111943441,-4.39621911301956,22.4720466713892));
#53269=CARTESIAN_POINT('Ctrl Pts',(5.26823008096148,-4.24712147389883,22.4810759998109));
#53270=CARTESIAN_POINT('Ctrl Pts',(5.38859849879596,-4.09781363716036,22.4901180577656));
#53271=CARTESIAN_POINT('Ctrl Pts',(5.50256217887023,-3.9434530199379,22.4991601157204));
#53272=CARTESIAN_POINT('Ctrl Pts',(5.60973717586073,-3.78459216003073,22.5082021736752));
#53273=CARTESIAN_POINT('Ctrl Pts',(5.70274645453809,-3.64672853133999,22.5160491091708));
#53274=CARTESIAN_POINT('Ctrl Pts',(5.79064364718261,-3.50547621488624,22.5238960446664));
#53275=CARTESIAN_POINT('Ctrl Pts',(5.87320508241612,-3.36121273648091,22.5317429801621));
#53276=CARTESIAN_POINT('Ctrl Pts',(5.96425240054603,-3.20212147582456,22.5403964444629));
#53277=CARTESIAN_POINT('Ctrl Pts',(6.0488898332124,-3.03922735851312,22.5490499087637));
#53278=CARTESIAN_POINT('Ctrl Pts',(6.12680981952343,-2.87306290139831,22.5577033730645));
#53279=CARTESIAN_POINT('Ctrl Pts',(6.20465802558881,-2.70705151573687,22.5663488657547));
#53280=CARTESIAN_POINT('Ctrl Pts',(6.27580099908149,-2.5377760733746,22.5749943584448));
#53281=CARTESIAN_POINT('Ctrl Pts',(6.33997713483556,-2.36579350953593,22.5836398511349));
#53282=CARTESIAN_POINT('Ctrl Pts',(6.40608389946652,-2.18863714549616,22.5925454286315));
#53283=CARTESIAN_POINT('Ctrl Pts',(6.46479793954806,-2.0086085148415,22.601451006128));
#53284=CARTESIAN_POINT('Ctrl Pts',(6.51588589123277,-1.82634061785687,22.6103565836246));
#53285=CARTESIAN_POINT('Ctrl Pts',(6.56538772756097,-1.64973154846018,22.6189856717971));
#53286=CARTESIAN_POINT('Ctrl Pts',(6.60772980164938,-1.47102048869803,22.6276147599697));
#53287=CARTESIAN_POINT('Ctrl Pts',(6.64274954482154,-1.29080110194142,22.6362438481422));
#53288=CARTESIAN_POINT('Ctrl Pts',(6.67945241805147,-1.10191995357932,22.6452876703008));
#53289=CARTESIAN_POINT('Ctrl Pts',(6.70811163163842,-0.911382232976675,
22.6543314924593));
#53290=CARTESIAN_POINT('Ctrl Pts',(6.72859955155919,-0.719886848579347,
22.6633753146178));
#53291=CARTESIAN_POINT('Ctrl Pts',(6.74908747147996,-0.528391464182019,
22.6724191367763));
#53292=CARTESIAN_POINT('Ctrl Pts',(6.76140402230401,-0.335938795437292,
22.6814629589349));
#53293=CARTESIAN_POINT('Ctrl Pts',(6.76548386034245,-0.143238037705902,
22.6905067810934));
#53294=CARTESIAN_POINT('Ctrl Pts',(6.76928489239844,0.0362940296087281,
22.6989325709432));
#53295=CARTESIAN_POINT('Ctrl Pts',(6.76593505134287,0.215962810871053,22.7073583607931));
#53296=CARTESIAN_POINT('Ctrl Pts',(6.75545136976293,0.395178175976516,22.7157841506429));
#53297=CARTESIAN_POINT('Ctrl Pts',(6.7449652556162,0.574435125075533,22.7242118955594));
#53298=CARTESIAN_POINT('Ctrl Pts',(6.72734201989472,0.753238117308931,22.732639640476));
#53299=CARTESIAN_POINT('Ctrl Pts',(6.70265067643537,0.931001025606562,22.7410673853925));
#53300=CARTESIAN_POINT('Ctrl Pts',(6.67795026014629,1.10882925285302,22.7494982270824));
#53301=CARTESIAN_POINT('Ctrl Pts',(6.64617660317425,1.28561630593951,22.7579290687723));
#53302=CARTESIAN_POINT('Ctrl Pts',(6.60745010600319,1.46078475371237,22.7663599104622));
#53303=CARTESIAN_POINT('Ctrl Pts',(6.568688024124,1.63611415893148,22.7747984990195));
#53304=CARTESIAN_POINT('Ctrl Pts',(6.52296040949227,1.80982166345399,22.7832370875769));
#53305=CARTESIAN_POINT('Ctrl Pts',(6.47043824649797,1.98134244850713,22.7916756761342));
#53306=CARTESIAN_POINT('Ctrl Pts',(6.41788854320256,2.15295317147983,22.8001186895145));
#53307=CARTESIAN_POINT('Ctrl Pts',(6.35853729042603,2.322374573866,22.8085617028947));
#53308=CARTESIAN_POINT('Ctrl Pts',(6.29260438710844,2.48905986817183,22.8170047162749));
#53309=CARTESIAN_POINT('Ctrl Pts',(6.22660221668023,2.65592027699772,22.8254565996292));
#53310=CARTESIAN_POINT('Ctrl Pts',(6.15400471257011,2.82003853073858,22.8339084829835));
#53311=CARTESIAN_POINT('Ctrl Pts',(6.07507911003739,2.98088959989922,22.8423603663378));
#53312=CARTESIAN_POINT('Ctrl Pts',(6.05356938990043,3.0247265979119,22.8446637715669));
#53313=CARTESIAN_POINT('Ctrl Pts',(6.03158991932571,3.06832107925754,22.846967176796));
#53314=CARTESIAN_POINT('Ctrl Pts',(6.00914668281669,3.1116627619961,22.8492705820251));
#53315=CARTESIAN_POINT('Ctrl Pts',(5.92811450439602,3.26814959344361,22.8575871162033));
#53316=CARTESIAN_POINT('Ctrl Pts',(5.84088749743472,3.42162030783587,22.8659036503815));
#53317=CARTESIAN_POINT('Ctrl Pts',(5.74771588976992,3.57156143031118,22.8742201845597));
#53318=CARTESIAN_POINT('Ctrl Pts',(5.6546185525653,3.72138302929165,22.8825300893276));
#53319=CARTESIAN_POINT('Ctrl Pts',(5.55558623646763,3.86768034702241,22.8908399940955));
#53320=CARTESIAN_POINT('Ctrl Pts',(5.4509152148054,4.00996412964044,22.8991498988634));
#53321=CARTESIAN_POINT('Ctrl Pts',(5.34631024165017,4.15215812970679,22.9074545599946));
#53322=CARTESIAN_POINT('Ctrl Pts',(5.23607385703312,4.29034336107764,22.9157592211258));
#53323=CARTESIAN_POINT('Ctrl Pts',(5.12054591546747,4.4240590556173,22.924063882257));
#53324=CARTESIAN_POINT('Ctrl Pts',(5.00507168780598,4.55771257998494,22.9323646821945));
#53325=CARTESIAN_POINT('Ctrl Pts',(4.88431103272458,4.68690044587856,22.9406654821319));
#53326=CARTESIAN_POINT('Ctrl Pts',(4.75864451946989,4.81119437742015,22.9489662820693));
#53327=CARTESIAN_POINT('Ctrl Pts',(4.63300123370041,4.93546533517674,22.957265547734));
#53328=CARTESIAN_POINT('Ctrl Pts',(4.50245414028907,5.05484391326157,22.9655648133987));
#53329=CARTESIAN_POINT('Ctrl Pts',(4.36742142712399,5.16893790617553,22.9738640790634));
#53330=CARTESIAN_POINT('Ctrl Pts',(4.23240744198006,5.28301607511126,22.9821621936824));
#53331=CARTESIAN_POINT('Ctrl Pts',(4.0929093442588,5.39181089714173,22.9904603083013));
#53332=CARTESIAN_POINT('Ctrl Pts',(3.9493792173035,5.49496977224909,22.9987584229203));
#53333=CARTESIAN_POINT('Ctrl Pts',(3.80580495801465,5.59816036642465,23.0070590890257));
#53334=CARTESIAN_POINT('Ctrl Pts',(3.65819647368515,5.69571134619766,23.015359755131));
#53335=CARTESIAN_POINT('Ctrl Pts',(3.50703625399584,5.78731247758049,23.0236604212364));
#53336=CARTESIAN_POINT('Ctrl Pts',(3.37369971107801,5.86811269215449,23.0309823351942));
#53337=CARTESIAN_POINT('Ctrl Pts',(3.23760020729334,5.94428400194773,23.0383042491519));
#53338=CARTESIAN_POINT('Ctrl Pts',(3.09908550384706,6.0156427786102,23.0456261631097));
#53339=CARTESIAN_POINT('Ctrl Pts',(3.0990855038473,6.01564277861008,21.0460278352566));
#53340=CARTESIAN_POINT('Ctrl Pts',(2.94662663691218,6.09418518577089,21.0540685571013));
#53341=CARTESIAN_POINT('Ctrl Pts',(2.79108041138924,6.1669791943634,21.062109278946));
#53342=CARTESIAN_POINT('Ctrl Pts',(2.63293047526607,6.23377623214174,21.0701500007907));
#53343=CARTESIAN_POINT('Ctrl Pts',(2.47480882144445,6.30056132445862,21.0781892846954));
#53344=CARTESIAN_POINT('Ctrl Pts',(2.31408472406724,6.36135142788615,21.0862285686001));
#53345=CARTESIAN_POINT('Ctrl Pts',(2.15126389991249,6.41594518624757,21.0942678525048));
#53346=CARTESIAN_POINT('Ctrl Pts',(1.98845319473804,6.47053555171887,21.1023066367845));
#53347=CARTESIAN_POINT('Ctrl Pts',(1.82354637576793,6.51893021863884,21.1103454210642));
#53348=CARTESIAN_POINT('Ctrl Pts',(1.65706622753046,6.56097710082713,21.1183842053439));
#53349=CARTESIAN_POINT('Ctrl Pts',(1.49056346858335,6.60302969366534,21.1264240814212));
#53350=CARTESIAN_POINT('Ctrl Pts',(1.32248731704382,6.63873269387233,21.1344639574984));
#53351=CARTESIAN_POINT('Ctrl Pts',(1.15337255970195,6.66798475842039,21.1425038335757));
#53352=CARTESIAN_POINT('Ctrl Pts',(0.984201347065698,6.69724658813584,21.1505463935912));
#53353=CARTESIAN_POINT('Ctrl Pts',(0.813991206228209,6.72005313214289,21.1585889536067));
#53354=CARTESIAN_POINT('Ctrl Pts',(0.643283735453474,6.73635472905792,21.1666315136222));
#53355=CARTESIAN_POINT('Ctrl Pts',(0.472377325898346,6.7526753235001,21.1746834462626));
#53356=CARTESIAN_POINT('Ctrl Pts',(0.300972800845152,6.76247579447924,21.1827353789029));
#53357=CARTESIAN_POINT('Ctrl Pts',(0.129614342912238,6.76575857698983,21.1907873115433));
#53358=CARTESIAN_POINT('Ctrl Pts',(-0.0418468513062848,6.76904332766053,
21.198844071641));
#53359=CARTESIAN_POINT('Ctrl Pts',(-0.213261551119682,6.76580261469696,
21.2069008317387));
#53360=CARTESIAN_POINT('Ctrl Pts',(-0.384089513756238,6.75609089973059,
21.2149575918365));
#53361=CARTESIAN_POINT('Ctrl Pts',(-0.555196049055262,6.74636334767144,
21.2230274902582));
#53362=CARTESIAN_POINT('Ctrl Pts',(-0.725713564944908,6.73014374840286,
21.2310973886798));
#53363=CARTESIAN_POINT('Ctrl Pts',(-0.895109663699864,6.70753812437552,
21.2391672871015));
#53364=CARTESIAN_POINT('Ctrl Pts',(-1.05230006604951,6.68656132997271,21.2466557156376));
#53365=CARTESIAN_POINT('Ctrl Pts',(-1.20852472136614,6.66008623194602,21.2541441441737));
#53366=CARTESIAN_POINT('Ctrl Pts',(-1.36337035817365,6.62823583364785,21.2616325727098));
#53367=CARTESIAN_POINT('Ctrl Pts',(-1.53355963149028,6.59322938301115,21.2698630287764));
#53368=CARTESIAN_POINT('Ctrl Pts',(-1.70264886980046,6.55161271349318,21.278093484843));
#53369=CARTESIAN_POINT('Ctrl Pts',(-1.87008600869319,6.50346579295148,21.2863239409096));
#53370=CARTESIAN_POINT('Ctrl Pts',(-2.03732438983509,6.45537602564173,21.2945446269398));
#53371=CARTESIAN_POINT('Ctrl Pts',(-2.20291423545044,6.40077154096288,21.30276531297));
#53372=CARTESIAN_POINT('Ctrl Pts',(-2.36631225253593,6.33978353916743,21.3109859990002));
#53373=CARTESIAN_POINT('Ctrl Pts',(-2.52954908924421,6.27885569764388,21.3191985759156));
#53374=CARTESIAN_POINT('Ctrl Pts',(-2.69059806960531,6.21155700367775,21.3274111528311));
#53375=CARTESIAN_POINT('Ctrl Pts',(-2.8489295973464,6.13806884527729,21.3356237297465));
#53376=CARTESIAN_POINT('Ctrl Pts',(-3.00713669722695,6.06463843895221,21.3438298526512));
#53377=CARTESIAN_POINT('Ctrl Pts',(-3.16263027431438,5.98502840667668,21.3520359755559));
#53378=CARTESIAN_POINT('Ctrl Pts',(-3.31489922795727,5.89946879884014,21.3602420984607));
#53379=CARTESIAN_POINT('Ctrl Pts',(-3.46707904916856,5.81395927433123,21.3684434178144));
#53380=CARTESIAN_POINT('Ctrl Pts',(-3.61603769547434,5.72250728726912,21.3766447371681));
#53381=CARTESIAN_POINT('Ctrl Pts',(-3.76128718727957,5.62538955938223,21.3848460565218));
#53382=CARTESIAN_POINT('Ctrl Pts',(-3.90649501044739,5.52829969227019,21.3930450231113));
#53383=CARTESIAN_POINT('Ctrl Pts',(-4.04799549874984,5.4255475176042,21.4012439897007));
#53384=CARTESIAN_POINT('Ctrl Pts',(-4.18532806637969,5.3174540878859,21.4094429562902));
#53385=CARTESIAN_POINT('Ctrl Pts',(-4.32264249862362,5.20937493239328,21.4176408401692));
#53386=CARTESIAN_POINT('Ctrl Pts',(-4.45578982416256,5.09595614770787,21.4258387240481));
#53387=CARTESIAN_POINT('Ctrl Pts',(-4.58434107624492,4.97756023536165,21.4340366079271));
#53388=CARTESIAN_POINT('Ctrl Pts',(-4.71289870425812,4.85915845077277,21.4422348984076));
#53389=CARTESIAN_POINT('Ctrl Pts',(-4.83685954083583,4.73577928965515,21.4504331888881));
#53390=CARTESIAN_POINT('Ctrl Pts',(-4.95583011811126,4.60782343850341,21.4586314793686));
#53391=CARTESIAN_POINT('Ctrl Pts',(-5.07482820742181,4.47983799746522,21.4668316657099));
#53392=CARTESIAN_POINT('Ctrl Pts',(-5.18883349486172,4.34727402102261,21.4750318520512));
#53393=CARTESIAN_POINT('Ctrl Pts',(-5.29749154609927,4.21056674558269,21.4832320383925));
#53394=CARTESIAN_POINT('Ctrl Pts',(-5.40625232499886,4.07373022414002,21.4914399773667));
#53395=CARTESIAN_POINT('Ctrl Pts',(-5.50965554416134,3.93274285874172,21.4996479163407));
#53396=CARTESIAN_POINT('Ctrl Pts',(-5.60738846940656,3.78807121806947,21.5078558553149));
#53397=CARTESIAN_POINT('Ctrl Pts',(-5.70516880785485,3.6433293928012,21.5160677762088));
#53398=CARTESIAN_POINT('Ctrl Pts',(-5.79727317890153,3.49490003321679,21.5242796971028));
#53399=CARTESIAN_POINT('Ctrl Pts',(-5.88343395903084,3.34327591588291,21.5324916179968));
#53400=CARTESIAN_POINT('Ctrl Pts',(-5.96971289502047,3.19144387009246,21.5407148002393));
#53401=CARTESIAN_POINT('Ctrl Pts',(-6.05003178615456,3.03640862951005,21.5489379824819));
#53402=CARTESIAN_POINT('Ctrl Pts',(-6.12416994087796,2.87868573054559,21.5571611647245));
#53403=CARTESIAN_POINT('Ctrl Pts',(-6.19028246470763,2.73803670906435,21.5644941680073));
#53404=CARTESIAN_POINT('Ctrl Pts',(-6.25148059307092,2.59525087227621,21.57182717129));
#53405=CARTESIAN_POINT('Ctrl Pts',(-6.30764116018424,2.45070438738532,21.5791601745728));
#53406=CARTESIAN_POINT('Ctrl Pts',(-6.38296327955959,2.25683975691834,21.588995142007));
#53407=CARTESIAN_POINT('Ctrl Pts',(-6.44937136978426,2.05942808343972,21.5988301094412));
#53408=CARTESIAN_POINT('Ctrl Pts',(-6.50657387259168,1.85924324403971,21.6086650768754));
#53409=CARTESIAN_POINT('Ctrl Pts',(-6.56154238031078,1.66687645325694,21.6181159480225));
#53410=CARTESIAN_POINT('Ctrl Pts',(-6.60801052598671,1.47194913615589,21.6275668191696));
#53411=CARTESIAN_POINT('Ctrl Pts',(-6.64576820312261,1.27516822041818,21.6370176903167));
#53412=CARTESIAN_POINT('Ctrl Pts',(-6.68341192004839,1.07898122878296,21.6464400368472));
#53413=CARTESIAN_POINT('Ctrl Pts',(-6.71239759196143,0.880951940409592,
21.6558623833778));
#53414=CARTESIAN_POINT('Ctrl Pts',(-6.73256559614496,0.681798719275146,
21.6652847299084));
#53415=CARTESIAN_POINT('Ctrl Pts',(-6.75263041947556,0.483664379287074,
21.6746588710864));
#53416=CARTESIAN_POINT('Ctrl Pts',(-6.76396749901039,0.284417716246836,
21.6840330122644));
#53417=CARTESIAN_POINT('Ctrl Pts',(-6.76646887602599,0.0847817773557425,
21.6934071534424));
#53418=CARTESIAN_POINT('Ctrl Pts',(-6.76680443639516,0.0580005648731028,
21.6946646968893));
#53419=CARTESIAN_POINT('Ctrl Pts',(-6.7669810606732,0.0312123682027215,
21.6959222403363));
#53420=CARTESIAN_POINT('Ctrl Pts',(-6.76699855717881,0.00441895236067369,
21.6971797837833));
#53421=CARTESIAN_POINT('',(-6.76699990728121,0.0011202036125479,21.3028202162152));
#53422=CARTESIAN_POINT('Ctrl Pts',(3.09908550384707,6.0156427786102,20.6515076495525));
#53423=CARTESIAN_POINT('Ctrl Pts',(3.09592568488907,6.01727062612174,20.6516753907719));
#53424=CARTESIAN_POINT('Ctrl Pts',(3.09276462949704,6.01889596023524,20.6518431319913));
#53425=CARTESIAN_POINT('Ctrl Pts',(3.08960234186716,6.02051877906954,20.6520108732107));
#53426=CARTESIAN_POINT('Ctrl Pts',(2.93611982316823,6.09928274719409,20.6601522404286));
#53427=CARTESIAN_POINT('Ctrl Pts',(2.77942780619768,6.1722741082475,20.6682936076464));
#53428=CARTESIAN_POINT('Ctrl Pts',(2.62000433287076,6.23922000699915,20.6764349748643));
#53429=CARTESIAN_POINT('Ctrl Pts',(2.46072002411105,6.30610746707278,20.6845692352878));
#53430=CARTESIAN_POINT('Ctrl Pts',(2.29870934028287,6.36695982847892,20.6927034957112));
#53431=CARTESIAN_POINT('Ctrl Pts',(2.13447479684968,6.42155015098485,20.7008377561347));
#53432=CARTESIAN_POINT('Ctrl Pts',(1.97035228828983,6.47610323394458,20.7089664676595));
#53433=CARTESIAN_POINT('Ctrl Pts',(1.8040092864421,6.52440266790771,20.7170951791843));
#53434=CARTESIAN_POINT('Ctrl Pts',(1.63596812132802,6.56626966442885,20.7252238907091));
#53435=CARTESIAN_POINT('Ctrl Pts',(1.46800709193988,6.60811669535311,20.7333487258017));
#53436=CARTESIAN_POINT('Ctrl Pts',(1.29834986636587,6.64353730902006,20.7414735608941));
#53437=CARTESIAN_POINT('Ctrl Pts',(1.12753374887625,6.67240261413721,20.7495983959867));
#53438=CARTESIAN_POINT('Ctrl Pts',(0.95676545183752,6.70125983833129,20.7577209565088));
#53439=CARTESIAN_POINT('Ctrl Pts',(0.784839269850681,6.72356534917233,20.765843517031));
#53440=CARTESIAN_POINT('Ctrl Pts',(0.612302475373419,6.73924140231314,20.7739660775532));
#53441=CARTESIAN_POINT('Ctrl Pts',(0.439756511013284,6.7549182885955,20.7820890697683));
#53442=CARTESIAN_POINT('Ctrl Pts',(0.266600233536377,6.7639649762837,20.7902120619835));
#53443=CARTESIAN_POINT('Ctrl Pts',(0.093386002451098,6.76635559622359,20.7983350541987));
#53444=CARTESIAN_POINT('Ctrl Pts',(0.00496541611165684,6.76757593484978,
20.8024815941798));
#53445=CARTESIAN_POINT('Ctrl Pts',(-0.0834702254333327,6.76706267811711,
20.806628134161));
#53446=CARTESIAN_POINT('Ctrl Pts',(-0.17184741606916,6.76481762249289,20.8107746741421));
#53447=CARTESIAN_POINT('Ctrl Pts',(-0.363320439401836,6.75995361193963,
20.8197583331705));
#53448=CARTESIAN_POINT('Ctrl Pts',(-0.554424234399817,6.74696018565322,
20.8287419921989));
#53449=CARTESIAN_POINT('Ctrl Pts',(-0.744493555791528,6.72592137520094,
20.8377256512272));
#53450=CARTESIAN_POINT('Ctrl Pts',(-0.934889414263731,6.70484642029519,
20.8467247440866));
#53451=CARTESIAN_POINT('Ctrl Pts',(-1.12424700925004,6.67569848147455,20.855723836946));
#53452=CARTESIAN_POINT('Ctrl Pts',(-1.31190952420657,6.63861298768772,20.8647229298055));
#53453=CARTESIAN_POINT('Ctrl Pts',(-1.50001205531867,6.60144053878145,20.8737431230228));
#53454=CARTESIAN_POINT('Ctrl Pts',(-1.68641131860128,6.55629334344968,20.8827633162402));
#53455=CARTESIAN_POINT('Ctrl Pts',(-1.87046125076591,6.50335787954063,20.8917835094576));
#53456=CARTESIAN_POINT('Ctrl Pts',(-2.05469757957372,6.45036880521912,20.9008128378793));
#53457=CARTESIAN_POINT('Ctrl Pts',(-2.23657959608153,6.38957577674257,20.909842166301));
#53458=CARTESIAN_POINT('Ctrl Pts',(-2.41547804360663,6.32121466340563,20.9188714947227));
#53459=CARTESIAN_POINT('Ctrl Pts',(-2.59462870188254,6.2527571746783,20.9279135526774));
#53460=CARTESIAN_POINT('Ctrl Pts',(-2.77078715726314,6.17671035276352,20.9369556106322));
#53461=CARTESIAN_POINT('Ctrl Pts',(-2.94334357795152,6.0933584813411,20.9459976685869));
#53462=CARTESIAN_POINT('Ctrl Pts',(-3.09309257417237,6.0210235370438,20.9538446040826));
#53463=CARTESIAN_POINT('Ctrl Pts',(-3.24012906133422,5.94318778162752,20.9616915395782));
#53464=CARTESIAN_POINT('Ctrl Pts',(-3.38406977779202,5.86006490911446,20.9695384750738));
#53465=CARTESIAN_POINT('Ctrl Pts',(-3.54280510217386,5.76839844769471,20.9781919393746));
#53466=CARTESIAN_POINT('Ctrl Pts',(-3.69791481064681,5.67022020774096,20.9868454036754));
#53467=CARTESIAN_POINT('Ctrl Pts',(-3.84886515503193,5.56583560827852,20.9954988679762));
#53468=CARTESIAN_POINT('Ctrl Pts',(-3.99967644327402,5.46154716838332,21.0041443606664));
#53469=CARTESIAN_POINT('Ctrl Pts',(-4.14633576052478,5.35106394464301,21.0127898533565));
#53470=CARTESIAN_POINT('Ctrl Pts',(-4.2883367847219,5.23473558270148,21.0214353460467));
#53471=CARTESIAN_POINT('Ctrl Pts',(-4.43460966596699,5.11490768168516,21.0303409235432));
#53472=CARTESIAN_POINT('Ctrl Pts',(-4.57593931753899,4.98887762199869,21.0392465010398));
#53473=CARTESIAN_POINT('Ctrl Pts',(-4.71180554652535,4.85707499342279,21.0481520785363));
#53474=CARTESIAN_POINT('Ctrl Pts',(-4.8434535693575,4.72936440937589,21.0567811667089));
#53475=CARTESIAN_POINT('Ctrl Pts',(-4.96997207647084,4.59623454241351,21.0654102548814));
#53476=CARTESIAN_POINT('Ctrl Pts',(-5.09092184834525,4.45811661288049,21.074039343054));
#53477=CARTESIAN_POINT('Ctrl Pts',(-5.21768474670377,4.31336041539825,21.0830831652125));
#53478=CARTESIAN_POINT('Ctrl Pts',(-5.33833015749739,4.16312507218579,21.092126987371));
#53479=CARTESIAN_POINT('Ctrl Pts',(-5.45239609107579,4.00795033227977,21.1011708095296));
#53480=CARTESIAN_POINT('Ctrl Pts',(-5.56646202465419,3.85277559237374,21.1102146316881));
#53481=CARTESIAN_POINT('Ctrl Pts',(-5.67394822489392,3.69266174572377,21.1192584538466));
#53482=CARTESIAN_POINT('Ctrl Pts',(-5.77444135509975,3.52818877563457,21.1283022760051));
#53483=CARTESIAN_POINT('Ctrl Pts',(-5.86806703477566,3.37495547917563,21.1367280658549));
#53484=CARTESIAN_POINT('Ctrl Pts',(-5.9555819488501,3.21800570310243,21.1451538557046));
#53485=CARTESIAN_POINT('Ctrl Pts',(-6.03670386153248,3.05785799018837,21.1535796455544));
#53486=CARTESIAN_POINT('Ctrl Pts',(-6.11784459722786,2.89767311761693,21.1620073904709));
#53487=CARTESIAN_POINT('Ctrl Pts',(-6.19258922406439,2.73428912443612,21.1704351353874));
#53488=CARTESIAN_POINT('Ctrl Pts',(-6.260702441154,2.56824725120623,21.1788628803039));
#53489=CARTESIAN_POINT('Ctrl Pts',(-6.32884068643314,2.4021443659195,21.1872937219937));
#53490=CARTESIAN_POINT('Ctrl Pts',(-6.39034253763179,2.23338195981157,21.1957245636836));
#53491=CARTESIAN_POINT('Ctrl Pts',(-6.44502147639647,2.06251961658264,21.2041554053735));
#53492=CARTESIAN_POINT('Ctrl Pts',(-6.49975065812689,1.89150027266843,21.2125939939308));
#53493=CARTESIAN_POINT('Ctrl Pts',(-6.54764430067226,1.71837745247793,21.2210325824881));
#53494=CARTESIAN_POINT('Ctrl Pts',(-6.58856594528387,1.5437252944244,21.2294711710454));
#53495=CARTESIAN_POINT('Ctrl Pts',(-6.62950904739746,1.36898155649757,21.2379141844256));
#53496=CARTESIAN_POINT('Ctrl Pts',(-6.66347279254201,1.19270720553275,21.2463571978058));
#53497=CARTESIAN_POINT('Ctrl Pts',(-6.69037206577036,1.01548541179066,21.254800211186));
#53498=CARTESIAN_POINT('Ctrl Pts',(-6.71729959856012,0.838077434201822,
21.2632520945403));
#53499=CARTESIAN_POINT('Ctrl Pts',(-6.73714779202576,0.659720354079816,
21.2717039778945));
#53500=CARTESIAN_POINT('Ctrl Pts',(-6.74988338645799,0.481002358849198,
21.2801558612488));
#53501=CARTESIAN_POINT('Ctrl Pts',(-6.75335423828881,0.432296059017696,
21.2824592664781));
#53502=CARTESIAN_POINT('Ctrl Pts',(-6.75629711157566,0.383562954992505,
21.2847626717074));
#53503=CARTESIAN_POINT('Ctrl Pts',(-6.75871200404307,0.334814943519694,
21.2870660769368));
#53504=CARTESIAN_POINT('Ctrl Pts',(-6.76421755610254,0.223677607766188,
21.2923174566878));
#53505=CARTESIAN_POINT('Ctrl Pts',(-6.76698148391198,0.11241325470507,21.2975688364388));
#53506=CARTESIAN_POINT('Ctrl Pts',(-6.76699990728112,0.00112020415150532,
21.3028202161898));
#53507=CARTESIAN_POINT('Ctrl Pts',(-6.76699990728121,0.00112020361273272,
21.3028202162152));
#53508=CARTESIAN_POINT('Ctrl Pts',(-6.76702891842711,-0.174132241042112,
21.311089529839));
#53509=CARTESIAN_POINT('Ctrl Pts',(-6.76024557647699,-0.34956410759948,
21.3193588434628));
#53510=CARTESIAN_POINT('Ctrl Pts',(-6.74663422670371,-0.524609960894863,
21.3276281570867));
#53511=CARTESIAN_POINT('Ctrl Pts',(-6.73303425497763,-0.699509489246982,
21.3358905581968));
#53512=CARTESIAN_POINT('Ctrl Pts',(-6.71261767259278,-0.874023296891779,
21.344152959307));
#53513=CARTESIAN_POINT('Ctrl Pts',(-6.68542086837122,-1.04758618392313,
21.3524153604172));
#53514=CARTESIAN_POINT('Ctrl Pts',(-6.65824157348432,-1.22103733096294,
21.3606724421838));
#53515=CARTESIAN_POINT('Ctrl Pts',(-6.62429080789634,-1.39353842939799,
21.3689295239503));
#53516=CARTESIAN_POINT('Ctrl Pts',(-6.58365677468221,-1.56452947341401,
21.3771866057169));
#53517=CARTESIAN_POINT('Ctrl Pts',(-6.54304109715321,-1.73544327533718,
21.3854399574971));
#53518=CARTESIAN_POINT('Ctrl Pts',(-6.49574824933605,-1.90484803923695,
21.3936933092772));
#53519=CARTESIAN_POINT('Ctrl Pts',(-6.44191753897369,-2.07219386666963,
21.4019466610573));
#53520=CARTESIAN_POINT('Ctrl Pts',(-6.38684580767145,-2.24339770887946,
21.4103902867966));
#53521=CARTESIAN_POINT('Ctrl Pts',(-6.32493118864368,-2.4124461586262,21.4188339125359));
#53522=CARTESIAN_POINT('Ctrl Pts',(-6.2563770741499,-2.57876615962974,21.4272775382751));
#53523=CARTESIAN_POINT('Ctrl Pts',(-6.18937543192634,-2.74131968809628,
21.435529950184));
#53524=CARTESIAN_POINT('Ctrl Pts',(-6.11603193000432,-2.90126668262016,
21.4437823620929));
#53525=CARTESIAN_POINT('Ctrl Pts',(-6.03658533437643,-3.05809197062342,
21.4520347740018));
#53526=CARTESIAN_POINT('Ctrl Pts',(-5.95712648527414,-3.21494144663166,
21.4602884587244));
#53527=CARTESIAN_POINT('Ctrl Pts',(-5.87156282614231,-3.36866794145217,
21.4685421434471));
#53528=CARTESIAN_POINT('Ctrl Pts',(-5.78017931513017,-3.5187804826305,21.4767958281697));
#53529=CARTESIAN_POINT('Ctrl Pts',(-5.68876579974297,-3.66894231096071,
21.4850522228632));
#53530=CARTESIAN_POINT('Ctrl Pts',(-5.59152880859176,-3.815487519726,21.4933086175567));
#53531=CARTESIAN_POINT('Ctrl Pts',(-5.48879695101422,-3.95795364178726,
21.5015650122502));
#53532=CARTESIAN_POINT('Ctrl Pts',(-5.3819673693051,-4.10610239122495,21.5101507344626));
#53533=CARTESIAN_POINT('Ctrl Pts',(-5.26919579675221,-4.24983960532958,
21.5187364566751));
#53534=CARTESIAN_POINT('Ctrl Pts',(-5.15089773603461,-4.38868334616586,
21.5273221788875));
#53535=CARTESIAN_POINT('Ctrl Pts',(-5.03694290077282,-4.52242954215717,
21.5355926826844));
#53536=CARTESIAN_POINT('Ctrl Pts',(-4.91786044315648,-4.65163497682704,
21.5438631864812));
#53537=CARTESIAN_POINT('Ctrl Pts',(-4.79405905529826,-4.77590690595124,
21.5521336902781));
#53538=CARTESIAN_POINT('Ctrl Pts',(-4.6701689978321,-4.90026784169665,21.5604101176137));
#53539=CARTESIAN_POINT('Ctrl Pts',(-4.54155353013335,-5.01968798830965,
21.5686865449494));
#53540=CARTESIAN_POINT('Ctrl Pts',(-4.40865475228873,-5.13381459298269,
21.5769629722851));
#53541=CARTESIAN_POINT('Ctrl Pts',(-4.27558143402515,-5.24809108395053,
21.5852502693302));
#53542=CARTESIAN_POINT('Ctrl Pts',(-4.13821384871292,-5.35705993324231,
21.5935375663753));
#53543=CARTESIAN_POINT('Ctrl Pts',(-3.99702406363177,-5.46041094009861,
21.6018248634203));
#53544=CARTESIAN_POINT('Ctrl Pts',(-3.98130006073072,-5.47192091959678,
21.6027478018801));
#53545=CARTESIAN_POINT('Ctrl Pts',(-3.96552867784857,-5.48336126855425,
21.6036707403399));
#53546=CARTESIAN_POINT('Ctrl Pts',(-3.94971058607144,-5.49473159365179,
21.6045936787997));
#53547=CARTESIAN_POINT('Ctrl Pts',(-3.81137595055879,-5.59416898472216,
21.6126650920417));
#53548=CARTESIAN_POINT('Ctrl Pts',(-3.66902918682942,-5.68856179859757,
21.6207365052837));
#53549=CARTESIAN_POINT('Ctrl Pts',(-3.52308071124807,-5.77755928589502,
21.6288079185258));
#53550=CARTESIAN_POINT('Ctrl Pts',(-3.3773154618892,-5.86644504421865,21.636869198777));
#53551=CARTESIAN_POINT('Ctrl Pts',(-3.22795781199351,-5.9499487615537,21.6449304790282));
#53552=CARTESIAN_POINT('Ctrl Pts',(-3.07545102426697,-6.02775994854932,
21.6529917592795));
#53553=CARTESIAN_POINT('Ctrl Pts',(-2.92310225073681,-6.10549051439773,
21.6610446871371));
#53554=CARTESIAN_POINT('Ctrl Pts',(-2.76761116196906,-6.17754011923568,
21.6690976149947));
#53555=CARTESIAN_POINT('Ctrl Pts',(-2.60944968390115,-6.2436416735098,21.6771505428523));
#53556=CARTESIAN_POINT('Ctrl Pts',(-2.45141744519182,-6.30968921385726,
21.6851968903767));
#53557=CARTESIAN_POINT('Ctrl Pts',(-2.29071950261418,-6.36979823433429,
21.6932432379011));
#53558=CARTESIAN_POINT('Ctrl Pts',(-2.12785195969749,-6.42374774081389,
21.7012895854255));
#53559=CARTESIAN_POINT('Ctrl Pts',(-1.96508187463137,-6.47766496460017,
21.7093311181186));
#53560=CARTESIAN_POINT('Ctrl Pts',(-1.80014512684374,-6.52542989472095,
21.7173726508118));
#53561=CARTESIAN_POINT('Ctrl Pts',(-1.63355725711915,-6.56686985463496,
21.7254141835049));
#53562=CARTESIAN_POINT('Ctrl Pts',(-1.46376677932882,-6.60910648690023,
21.7336103125531));
#53563=CARTESIAN_POINT('Ctrl Pts',(-1.29226141455064,-6.64477233083709,
21.7418064416014));
#53564=CARTESIAN_POINT('Ctrl Pts',(-1.11960311989676,-6.67373792217805,
21.7500025706496));
#53565=CARTESIAN_POINT('Ctrl Pts',(-0.950260002153118,-6.70214735107228,
21.7580413274857));
#53566=CARTESIAN_POINT('Ctrl Pts',(-0.779808212887768,-6.72411145366687,
21.7660800843218));
#53567=CARTESIAN_POINT('Ctrl Pts',(-0.608787634920312,-6.73955982357662,
21.7741188411579));
#53568=CARTESIAN_POINT('Ctrl Pts',(-0.437750503968559,-6.7550096887253,
21.7821583760607));
#53569=CARTESIAN_POINT('Ctrl Pts',(-0.266144846661902,-6.76394253173664,
21.7901979109635));
#53570=CARTESIAN_POINT('Ctrl Pts',(-0.0945147078463442,-6.76633992421314,
21.7982374458663));
#53571=CARTESIAN_POINT('Ctrl Pts',(0.0771660257802154,-6.76873802341645,
21.8062793507418));
#53572=CARTESIAN_POINT('Ctrl Pts',(0.248870882049254,-6.76459683205694,
21.8143212556174));
#53573=CARTESIAN_POINT('Ctrl Pts',(0.420056927277532,-6.75395004259331,
21.8223631604929));
#53574=CARTESIAN_POINT('Ctrl Pts',(0.597017468505102,-6.74294411262216,
21.8306763371737));
#53575=CARTESIAN_POINT('Ctrl Pts',(0.773423149339626,-6.72498603702747,
21.8389895138545));
#53576=CARTESIAN_POINT('Ctrl Pts',(0.948682322968968,-6.7001709567806,21.8473026905353));
#53577=CARTESIAN_POINT('Ctrl Pts',(1.11851688254776,-6.67612395178014,21.8553585581459));
#53578=CARTESIAN_POINT('Ctrl Pts',(1.28727450121639,-6.64563823085054,21.8634144257564));
#53579=CARTESIAN_POINT('Ctrl Pts',(1.45442981742539,-6.60885185990607,21.8714702933669));
#53580=CARTESIAN_POINT('Ctrl Pts',(1.62959368983613,-6.5703030220186,21.8799121245829));
#53581=CARTESIAN_POINT('Ctrl Pts',(1.80299747711763,-6.52483506515602,21.8883539557989));
#53582=CARTESIAN_POINT('Ctrl Pts',(1.97405812244072,-6.4726643300287,21.8967957870148));
#53583=CARTESIAN_POINT('Ctrl Pts',(2.14511876776381,-6.42049359490137,21.9052376182308));
#53584=CARTESIAN_POINT('Ctrl Pts',(2.31383586396583,-6.36162031423033,21.9136794494468));
#53585=CARTESIAN_POINT('Ctrl Pts',(2.47965458072558,-6.29631655496185,21.9221212806627));
#53586=CARTESIAN_POINT('Ctrl Pts',(2.64132135993411,-6.23264793758592,21.9303517367293));
#53587=CARTESIAN_POINT('Ctrl Pts',(2.80077100940199,-6.16265560244377,21.9385821927959));
#53588=CARTESIAN_POINT('Ctrl Pts',(2.95747335139946,-6.08651298986226,21.9468126488625));
#53589=CARTESIAN_POINT('Ctrl Pts',(3.11398967848306,-6.01046076304871,21.9550333348927));
#53590=CARTESIAN_POINT('Ctrl Pts',(3.26776487260306,-5.92827295135204,21.9632540209229));
#53591=CARTESIAN_POINT('Ctrl Pts',(3.41828618182501,-5.84017196486064,21.9714747069532));
#53592=CARTESIAN_POINT('Ctrl Pts',(3.56865901261323,-5.75215788364899,21.9796872838685));
#53593=CARTESIAN_POINT('Ctrl Pts',(3.71578404334172,-5.65824242369913,21.9878998607839));
#53594=CARTESIAN_POINT('Ctrl Pts',(3.85917062114248,-5.55869509119819,21.9961124376993));
#53595=CARTESIAN_POINT('Ctrl Pts',(4.00244451585767,-5.45922598987312,22.004318560604));
#53596=CARTESIAN_POINT('Ctrl Pts',(4.14198551617762,-5.35413403497812,22.0125246835086));
#53597=CARTESIAN_POINT('Ctrl Pts',(4.27732953458581,-5.24373350319788,22.0207308064133));
#53598=CARTESIAN_POINT('Ctrl Pts',(4.41259432777456,-5.13339759567264,22.028932125767));
#53599=CARTESIAN_POINT('Ctrl Pts',(4.54366675611459,-5.01775952764966,22.0371334451207));
#53600=CARTESIAN_POINT('Ctrl Pts',(4.67011351299529,-4.89717559167923,22.0453347644745));
#53601=CARTESIAN_POINT('Ctrl Pts',(4.79652399529741,-4.77662624838297,22.053533731064));
#53602=CARTESIAN_POINT('Ctrl Pts',(4.91831118749573,-4.6511341075736,22.0617326976535));
#53603=CARTESIAN_POINT('Ctrl Pts',(5.03507637203057,-4.52109443916177,22.069931664243));
#53604=CARTESIAN_POINT('Ctrl Pts',(5.15182613719535,-4.39107194307556,22.078129548122));
#53605=CARTESIAN_POINT('Ctrl Pts',(5.26355497537947,-4.25650338160682,22.0863274320009));
#53606=CARTESIAN_POINT('Ctrl Pts',(5.36990242666848,-4.11781943849655,22.0945253158799));
#53607=CARTESIAN_POINT('Ctrl Pts',(5.47625515261699,-3.9791286168897,22.1027236063604));
#53608=CARTESIAN_POINT('Ctrl Pts',(5.57722574165307,-3.83632229156312,22.110921896841));
#53609=CARTESIAN_POINT('Ctrl Pts',(5.67249525422541,-3.68986267912373,22.1191201873215));
#53610=CARTESIAN_POINT('Ctrl Pts',(5.76778679794314,-3.54336919779044,22.1273203736629));
#53611=CARTESIAN_POINT('Ctrl Pts',(5.85737444387502,-3.39322104724946,22.1355205600042));
#53612=CARTESIAN_POINT('Ctrl Pts',(5.94098363187514,-3.23990778970508,22.1437207463455));
#53613=CARTESIAN_POINT('Ctrl Pts',(6.02467186580247,-3.08644958650479,22.1519286853196));
#53614=CARTESIAN_POINT('Ctrl Pts',(6.10237017748786,-2.92982061314315,22.1601366242937));
#53615=CARTESIAN_POINT('Ctrl Pts',(6.17385046162314,-2.77053415021648,22.1683445632678));
#53616=CARTESIAN_POINT('Ctrl Pts',(6.24536542300995,-2.61117041260061,22.1765564841618));
#53617=CARTESIAN_POINT('Ctrl Pts',(6.31065620858617,-2.44914694741303,22.1847684050558));
#53618=CARTESIAN_POINT('Ctrl Pts',(6.36954364926308,-2.28499512037385,22.1929803259498));
#53619=CARTESIAN_POINT('Ctrl Pts',(6.42851184473591,-2.12061818510889,22.2012035081923));
#53620=CARTESIAN_POINT('Ctrl Pts',(6.48105903842363,-1.95410739707698,22.2094266904349));
#53621=CARTESIAN_POINT('Ctrl Pts',(6.52705620058236,-1.78600849786316,22.2176498726774));
#53622=CARTESIAN_POINT('Ctrl Pts',(6.5680740609629,-1.63610670274193,22.2249828759602));
#53623=CARTESIAN_POINT('Ctrl Pts',(6.60388392501553,-1.48494235595671,22.232315879243));
#53624=CARTESIAN_POINT('Ctrl Pts',(6.63442894834745,-1.33290717206014,22.2396488825258));
#53625=CARTESIAN_POINT('Ctrl Pts',(6.6716477355503,-1.14765391180549,22.2485840693081));
#53626=CARTESIAN_POINT('Ctrl Pts',(6.70112667694405,-0.960723245654245,
22.2575192560904));
#53627=CARTESIAN_POINT('Ctrl Pts',(6.72273297968455,-0.772754996012099,
22.2664544428727));
#53628=CARTESIAN_POINT('Ctrl Pts',(6.74430692286757,-0.585068264659009,
22.2753762475093));
#53629=CARTESIAN_POINT('Ctrl Pts',(6.75803172464734,-0.396347306592092,
22.2842980521459));
#53630=CARTESIAN_POINT('Ctrl Pts',(6.76382586999895,-0.207240440872359,
22.2932198567825));
#53631=CARTESIAN_POINT('Ctrl Pts',(6.76960588205595,-0.0185948516454272,
22.3021198990218));
#53632=CARTESIAN_POINT('Ctrl Pts',(6.7674938386161,0.170434508781644,22.3110199412611));
#53633=CARTESIAN_POINT('Ctrl Pts',(6.75746008878359,0.359196531855262,22.3199199835003));
#53634=CARTESIAN_POINT('Ctrl Pts',(6.74744178605647,0.547667953019138,22.3288063239937));
#53635=CARTESIAN_POINT('Ctrl Pts',(6.72952611760736,0.735872601121292,22.3376926644872));
#53636=CARTESIAN_POINT('Ctrl Pts',(6.70373530180988,0.923158709685429,22.3465790049806));
#53637=CARTESIAN_POINT('Ctrl Pts',(6.67801042862648,1.10996596036162,22.3554426246525));
#53638=CARTESIAN_POINT('Ctrl Pts',(6.64445062212603,1.29585910272873,22.3643062443244));
#53639=CARTESIAN_POINT('Ctrl Pts',(6.60312970185075,1.48019158913179,22.3731698639963));
#53640=CARTESIAN_POINT('Ctrl Pts',(6.56390357042496,1.65517922952111,22.38158413715));
#53641=CARTESIAN_POINT('Ctrl Pts',(6.51768366501041,1.82876025029509,22.3899984103037));
#53642=CARTESIAN_POINT('Ctrl Pts',(6.46457647938154,2.00038494851042,22.3984126834574));
#53643=CARTESIAN_POINT('Ctrl Pts',(6.41275700935809,2.16784817969352,22.406622931662));
#53644=CARTESIAN_POINT('Ctrl Pts',(6.35442903773312,2.33328756654549,22.4148331798665));
#53645=CARTESIAN_POINT('Ctrl Pts',(6.28978622751912,2.4961727127967,22.423043428071));
#53646=CARTESIAN_POINT('Ctrl Pts',(6.22512805042046,2.65909658009432,22.4312556280152));
#53647=CARTESIAN_POINT('Ctrl Pts',(6.15415217528793,2.81946466623393,22.4394678279595));
#53648=CARTESIAN_POINT('Ctrl Pts',(6.07710026379533,2.97676693474293,22.4476800279037));
#53649=CARTESIAN_POINT('Ctrl Pts',(6.00001631474162,3.13413460826189,22.4558956424141));
#53650=CARTESIAN_POINT('Ctrl Pts',(5.91685145270224,3.2884336051883,22.4641112569246));
#53651=CARTESIAN_POINT('Ctrl Pts',(5.82789313167117,3.43917877491416,22.4723268714351));
#53652=CARTESIAN_POINT('Ctrl Pts',(5.73883491434496,3.59009322485788,22.4805517117205));
#53653=CARTESIAN_POINT('Ctrl Pts',(5.64397042480884,3.73744557003128,22.488776552006));
#53654=CARTESIAN_POINT('Ctrl Pts',(5.54363080142423,3.88077911475267,22.4970013922914));
#53655=CARTESIAN_POINT('Ctrl Pts',(5.44322690702313,4.0242044695916,22.5052315008729));
#53656=CARTESIAN_POINT('Ctrl Pts',(5.33734110245925,4.16360560975987,22.5134616094545));
#53657=CARTESIAN_POINT('Ctrl Pts',(5.22634455480093,4.29855924636415,22.521691718036));
#53658=CARTESIAN_POINT('Ctrl Pts',(5.11519582917256,4.43369790647503,22.5299331102227));
#53659=CARTESIAN_POINT('Ctrl Pts',(4.99892260080244,4.56437661858004,22.5381745024094));
#53660=CARTESIAN_POINT('Ctrl Pts',(4.87793327383911,4.69020852158764,22.5464158945961));
#53661=CARTESIAN_POINT('Ctrl Pts',(4.82527564483445,4.74497376271946,22.5500027578603));
#53662=CARTESIAN_POINT('Ctrl Pts',(4.7717251197473,4.79882142510225,22.5535896211245));
#53663=CARTESIAN_POINT('Ctrl Pts',(4.71731727448285,4.85172203777851,22.5571764843888));
#53664=CARTESIAN_POINT('Ctrl Pts',(4.58917628301486,4.97631320518556,22.5656242406398));
#53665=CARTESIAN_POINT('Ctrl Pts',(4.45598542019436,5.09593252264637,22.5740719968909));
#53666=CARTESIAN_POINT('Ctrl Pts',(4.31815736177582,5.21016372093443,22.5825197531419));
#53667=CARTESIAN_POINT('Ctrl Pts',(4.18044024365649,5.32430297246315,22.590960709641));
#53668=CARTESIAN_POINT('Ctrl Pts',(4.03809362238139,5.43306253443922,22.5994016661401));
#53669=CARTESIAN_POINT('Ctrl Pts',(3.8915660252331,5.53606384277236,22.6078426226393));
#53670=CARTESIAN_POINT('Ctrl Pts',(3.7451621432242,5.63897818577292,22.61627645233));
#53671=CARTESIAN_POINT('Ctrl Pts',(3.59458459652159,5.73614377901942,22.6247102820207));
#53672=CARTESIAN_POINT('Ctrl Pts',(3.44031394494327,5.82722309168174,22.6331441117114));
#53673=CARTESIAN_POINT('Ctrl Pts',(3.32844797976623,5.89326724923467,22.6392597175563));
#53674=CARTESIAN_POINT('Ctrl Pts',(3.21464084663881,5.95611200178093,22.6453753234012));
#53675=CARTESIAN_POINT('Ctrl Pts',(3.09908550384738,6.01564277861003,22.6514909292461));
#53676=CARTESIAN_POINT('Origin',(0.,0.,-63.6971797838103));
#53677=CARTESIAN_POINT('',(3.09908550384716,6.01564277861014,25.0456934344376));
#53678=CARTESIAN_POINT('',(3.09908550384736,6.01564277861004,24.6513967904261));
#53679=CARTESIAN_POINT('',(3.09908550384721,6.01564277861012,-63.6971797838103));
#53680=CARTESIAN_POINT('',(-6.76699871332204,-0.00417299626651514,23.6971797838511));
#53681=CARTESIAN_POINT('Ctrl Pts',(-6.76699871332204,-0.00417299626651379,
23.6971797838512));
#53682=CARTESIAN_POINT('Ctrl Pts',(-6.76687805051677,-0.19984176658391,
23.7063512865483));
#53683=CARTESIAN_POINT('Ctrl Pts',(-6.75826665739669,-0.395211573173384,
23.7155227892454));
#53684=CARTESIAN_POINT('Ctrl Pts',(-6.74126652660386,-0.589588515229351,
23.7246942919426));
#53685=CARTESIAN_POINT('Ctrl Pts',(-6.72421153836498,-0.78459268908379,
23.7338953900129));
#53686=CARTESIAN_POINT('Ctrl Pts',(-6.69871368186293,-0.978597396112563,
23.7430964880832));
#53687=CARTESIAN_POINT('Ctrl Pts',(-6.66492609097329,-1.17091810211624,
23.7522975861535));
#53688=CARTESIAN_POINT('Ctrl Pts',(-6.63098536740846,-1.36411044718708,
23.7615403855918));
#53689=CARTESIAN_POINT('Ctrl Pts',(-6.58867968481332,-1.55560330970433,
23.7707831850301));
#53690=CARTESIAN_POINT('Ctrl Pts',(-6.5382134288921,-1.74472179967326,23.7800259844684));
#53691=CARTESIAN_POINT('Ctrl Pts',(-6.49848710569334,-1.89359320133012,
23.787301785517));
#53692=CARTESIAN_POINT('Ctrl Pts',(-6.45370497690736,-2.04099364387838,
23.7945775865655));
#53693=CARTESIAN_POINT('Ctrl Pts',(-6.4039874546103,-2.18660322902761,23.8018533876141));
#53694=CARTESIAN_POINT('Ctrl Pts',(-6.34293089944737,-2.36542186795322,
23.8107885743963));
#53695=CARTESIAN_POINT('Ctrl Pts',(-6.27434173768598,-2.54179536035517,
23.8197237611786));
#53696=CARTESIAN_POINT('Ctrl Pts',(-6.19842717401112,-2.7151039701051,23.8286589479608));
#53697=CARTESIAN_POINT('Ctrl Pts',(-6.12262630686811,-2.8881530171715,23.8375807525974));
#53698=CARTESIAN_POINT('Ctrl Pts',(-6.03952203253638,-3.05814610463433,
23.846502557234));
#53699=CARTESIAN_POINT('Ctrl Pts',(-5.94937014392125,-3.22448195693796,
23.8554243618706));
#53700=CARTESIAN_POINT('Ctrl Pts',(-5.85943815714215,-3.39041207665096,
23.8643244041099));
#53701=CARTESIAN_POINT('Ctrl Pts',(-5.76249298886226,-3.55270253902627,
23.8732244463491));
#53702=CARTESIAN_POINT('Ctrl Pts',(-5.65883665502042,-3.71077575606467,
23.8821244885884));
#53703=CARTESIAN_POINT('Ctrl Pts',(-5.55533990162899,-3.86860561706067,
23.8910108290818));
#53704=CARTESIAN_POINT('Ctrl Pts',(-5.44515273316735,-4.02223096864418,
23.8998971695751));
#53705=CARTESIAN_POINT('Ctrl Pts',(-5.32862232043915,-4.1710997549948,23.9087835100684));
#53706=CARTESIAN_POINT('Ctrl Pts',(-5.21238985563483,-4.31958790984517,
23.9176471297403));
#53707=CARTESIAN_POINT('Ctrl Pts',(-5.08984666846457,-4.46334356458428,
23.9265107494122));
#53708=CARTESIAN_POINT('Ctrl Pts',(-4.96138189572148,-4.60184513915963,
23.9353743690841));
#53709=CARTESIAN_POINT('Ctrl Pts',(-4.83942972172004,-4.7333252933017,23.943788642238));
#53710=CARTESIAN_POINT('Ctrl Pts',(-4.71214156169059,-4.86007060779907,
23.9522029153919));
#53711=CARTESIAN_POINT('Ctrl Pts',(-4.57988605599304,-4.98165963451143,
23.9606171885457));
#53712=CARTESIAN_POINT('Ctrl Pts',(-4.4508374134857,-5.10030043330662,23.9688274367503));
#53713=CARTESIAN_POINT('Ctrl Pts',(-4.3171827310238,-5.21391719638234,23.9770376849548));
#53714=CARTESIAN_POINT('Ctrl Pts',(-4.17935626272777,-5.32214902358044,
23.9852479331593));
#53715=CARTESIAN_POINT('Ctrl Pts',(-4.04149703033263,-5.43040657964148,
23.9934601331035));
#53716=CARTESIAN_POINT('Ctrl Pts',(-3.89946431627269,-5.53327642964444,
24.0016723330477));
#53717=CARTESIAN_POINT('Ctrl Pts',(-3.75372360851034,-5.63043942076568,
24.0098845329919));
#53718=CARTESIAN_POINT('Ctrl Pts',(-3.6079223029414,-5.72764281147214,24.0181001475024));
#53719=CARTESIAN_POINT('Ctrl Pts',(-3.4584102280793,-5.81913441874243,24.0263157620129));
#53720=CARTESIAN_POINT('Ctrl Pts',(-3.30567992154997,-5.90463963813723,
24.0345313765233));
#53721=CARTESIAN_POINT('Ctrl Pts',(-3.1527781055815,-5.99024087614521,24.0427562168087));
#53722=CARTESIAN_POINT('Ctrl Pts',(-2.99665115045636,-6.06984212542071,
24.0509810570942));
#53723=CARTESIAN_POINT('Ctrl Pts',(-2.83781502587742,-6.1432153534533,24.0592058973796));
#53724=CARTESIAN_POINT('Ctrl Pts',(-2.67887716123888,-6.21663557958921,
24.0674360059612));
#53725=CARTESIAN_POINT('Ctrl Pts',(-2.51722699571533,-6.28381969582728,
24.0756661145427));
#53726=CARTESIAN_POINT('Ctrl Pts',(-2.353398280191,-6.34458868129322,24.0838962231243));
#53727=CARTESIAN_POINT('Ctrl Pts',(-2.18934495298402,-6.40544098197063,
24.092137615311));
#53728=CARTESIAN_POINT('Ctrl Pts',(-2.02310744719204,-6.45986047389336,
24.1003790074976));
#53729=CARTESIAN_POINT('Ctrl Pts',(-1.85523336226345,-6.50771835373541,
24.1086203996843));
#53730=CARTESIAN_POINT('Ctrl Pts',(-1.7821702954165,-6.52854731894192,24.1122072629486));
#53731=CARTESIAN_POINT('Ctrl Pts',(-1.70879734349152,-6.54813403400726,
24.1157941262129));
#53732=CARTESIAN_POINT('Ctrl Pts',(-1.63516007992373,-6.5664709329307,24.1193809894771));
#53733=CARTESIAN_POINT('Ctrl Pts',(-1.46171492893776,-6.60966164980822,
24.1278294843055));
#53734=CARTESIAN_POINT('Ctrl Pts',(-1.28640735786213,-6.64601354661873,
24.1362779791339));
#53735=CARTESIAN_POINT('Ctrl Pts',(-1.10980360493438,-6.67537451821804,
24.1447264739624));
#53736=CARTESIAN_POINT('Ctrl Pts',(-0.933361169276194,-6.70470867027534,
24.1531672515816));
#53737=CARTESIAN_POINT('Ctrl Pts',(-0.755625239165976,-6.72706457154169,
24.1616080292007));
#53738=CARTESIAN_POINT('Ctrl Pts',(-0.57717387623315,-6.74234078911724,
24.1700488068199));
#53739=CARTESIAN_POINT('Ctrl Pts',(-0.398858076269871,-6.75760540190936,
24.1784831722892));
#53740=CARTESIAN_POINT('Ctrl Pts',(-0.219828257999102,-6.7658010241223,
24.1869175377585));
#53741=CARTESIAN_POINT('Ctrl Pts',(-0.0406696645354656,-6.76687778657089,
24.1953519032279));
#53742=CARTESIAN_POINT('Ctrl Pts',(0.138380341673131,-6.76795389639839,
24.2037811566645));
#53743=CARTESIAN_POINT('Ctrl Pts',(0.317558634847511,-6.7619197468726,24.2122104101011));
#53744=CARTESIAN_POINT('Ctrl Pts',(0.496277494712585,-6.74877749286801,
24.2206396635377));
#53745=CARTESIAN_POINT('Ctrl Pts',(0.674915448797272,-6.73564118834361,
24.2290651010629));
#53746=CARTESIAN_POINT('Ctrl Pts',(0.853094052309623,-6.71540322015307,
24.2374905385881));
#53747=CARTESIAN_POINT('Ctrl Pts',(1.03022783445546,-6.6881177927062,24.2459159761133));
#53748=CARTESIAN_POINT('Ctrl Pts',(1.20732270507286,-6.66083835913398,24.2543395627965));
#53749=CARTESIAN_POINT('Ctrl Pts',(1.38337288229526,-6.62651460110577,24.2627631494797));
#53750=CARTESIAN_POINT('Ctrl Pts',(1.5577997154205,-6.58525239050378,24.2711867361629));
#53751=CARTESIAN_POINT('Ctrl Pts',(1.73220703109782,-6.54399479692678,24.2796093802909));
#53752=CARTESIAN_POINT('Ctrl Pts',(1.90499104041301,-6.49580037526879,24.2880320244189));
#53753=CARTESIAN_POINT('Ctrl Pts',(2.07558464744206,-6.4408258299152,24.2964546685469));
#53754=CARTESIAN_POINT('Ctrl Pts',(2.24618295452916,-6.38584976994709,24.3048775447289));
#53755=CARTESIAN_POINT('Ctrl Pts',(2.41459042180088,-6.32409331648483,24.3133004209108));
#53756=CARTESIAN_POINT('Ctrl Pts',(2.58025608977679,-6.25576274415597,24.3217232970927));
#53757=CARTESIAN_POINT('Ctrl Pts',(2.74594942483861,-6.18742076024232,24.3301475799417));
#53758=CARTESIAN_POINT('Ctrl Pts',(2.9088997397551,-6.11250259621451,24.3385718627908));
#53759=CARTESIAN_POINT('Ctrl Pts',(3.06857665571365,-6.0312624141227,24.3469961456398));
#53760=CARTESIAN_POINT('Ctrl Pts',(3.22836141155734,-5.9499673654157,24.3554261179379));
#53761=CARTESIAN_POINT('Ctrl Pts',(3.3848680534537,-5.86234191824887,24.3638560902361));
#53762=CARTESIAN_POINT('Ctrl Pts',(3.53759049680964,-5.76868637359339,24.3722860625342));
#53763=CARTESIAN_POINT('Ctrl Pts',(3.69036753597431,-5.6749973485922,24.3807190484114));
#53764=CARTESIAN_POINT('Ctrl Pts',(3.83935739822696,-5.57527410732994,24.3891520342887));
#53765=CARTESIAN_POINT('Ctrl Pts',(3.98408307130611,-5.46986024327241,24.3975850201659));
#53766=CARTESIAN_POINT('Ctrl Pts',(4.12894189112241,-5.36434939910242,24.4060257643387));
#53767=CARTESIAN_POINT('Ctrl Pts',(4.26952841773963,-5.25313767347353,24.4144665085115));
#53768=CARTESIAN_POINT('Ctrl Pts',(4.40539794635658,-5.1366095758036,24.4229072526843));
#53769=CARTESIAN_POINT('Ctrl Pts',(4.48052383747979,-5.07217807841447,24.4275743655696));
#53770=CARTESIAN_POINT('Ctrl Pts',(4.55420822789292,-5.00612190614283,24.4322414784549));
#53771=CARTESIAN_POINT('Ctrl Pts',(4.62638076641204,-4.93851090959337,24.4369085913401));
#53772=CARTESIAN_POINT('Ctrl Pts',(4.75227940087219,-4.82056948319042,24.445049958558));
#53773=CARTESIAN_POINT('Ctrl Pts',(4.87382547408825,-4.69766025222511,24.4531913257758));
#53774=CARTESIAN_POINT('Ctrl Pts',(4.99060093565539,-4.57014127801708,24.4613326929937));
#53775=CARTESIAN_POINT('Ctrl Pts',(5.10727446112596,-4.44273361817504,24.4694669534172));
#53776=CARTESIAN_POINT('Ctrl Pts',(5.21918541867333,-4.31072449294497,24.4776012138406));
#53777=CARTESIAN_POINT('Ctrl Pts',(5.32595073348743,-4.17451048441188,24.4857354742641));
#53778=CARTESIAN_POINT('Ctrl Pts',(5.43264321686007,-4.03838939615543,24.4938641857889));
#53779=CARTESIAN_POINT('Ctrl Pts',(5.53419682124909,-3.89806942245095,24.5019928973137));
#53780=CARTESIAN_POINT('Ctrl Pts',(5.63026712403262,-3.75398203405895,24.5101216088385));
#53781=CARTESIAN_POINT('Ctrl Pts',(5.72629161266432,-3.60996335827949,24.518246443931));
#53782=CARTESIAN_POINT('Ctrl Pts',(5.81683780421136,-3.4621811494102,24.5263712790235));
#53783=CARTESIAN_POINT('Ctrl Pts',(5.90160320331277,-3.31109779841195,24.534496114116));
#53784=CARTESIAN_POINT('Ctrl Pts',(5.98634487210311,-3.16005674362131,24.5426186746382));
#53785=CARTESIAN_POINT('Ctrl Pts',(6.06530879365759,-3.00571670682226,24.5507412351604));
#53786=CARTESIAN_POINT('Ctrl Pts',(6.138237264273,-2.84856670757249,24.5588637956825));
#53787=CARTESIAN_POINT('Ctrl Pts',(6.21116961084736,-2.69140835620808,24.5669867878977));
#53788=CARTESIAN_POINT('Ctrl Pts',(6.27806570803365,-2.53144007444894,24.5751097801129));
#53789=CARTESIAN_POINT('Ctrl Pts',(6.33871497505609,-2.36917316061948,24.583232772328));
#53790=CARTESIAN_POINT('Ctrl Pts',(6.36967457761155,-2.28634084612172,24.5873793123093));
#53791=CARTESIAN_POINT('Ctrl Pts',(6.39900715896981,-2.20290988185016,24.5915258522905));
#53792=CARTESIAN_POINT('Ctrl Pts',(6.42668962807205,-2.11895007596477,24.5956723922718));
#53793=CARTESIAN_POINT('Ctrl Pts',(6.48666490013114,-1.93704750862493,24.6046560513002));
#53794=CARTESIAN_POINT('Ctrl Pts',(6.53886223245715,-1.75275174609116,24.6136397103287));
#53795=CARTESIAN_POINT('Ctrl Pts',(6.58313645147381,-1.56671741589757,24.6226233693571));
#53796=CARTESIAN_POINT('Ctrl Pts',(6.62748673312969,-1.38036348069562,24.6316224622166));
#53797=CARTESIAN_POINT('Ctrl Pts',(6.66388663988868,-1.19226524065869,24.640621555076));
#53798=CARTESIAN_POINT('Ctrl Pts',(6.69224222806581,-1.00308671653687,24.6496206479355));
#53799=CARTESIAN_POINT('Ctrl Pts',(6.7206643021733,-0.813464621641641,24.658640841153));
#53800=CARTESIAN_POINT('Ctrl Pts',(6.74100428323107,-0.622757412103681,
24.6676610343705));
#53801=CARTESIAN_POINT('Ctrl Pts',(6.75321991307334,-0.431636195967978,
24.6766812275879));
#53802=CARTESIAN_POINT('Ctrl Pts',(6.76544791429967,-0.240321421743524,
24.6857105560097));
#53803=CARTESIAN_POINT('Ctrl Pts',(6.76953511770094,-0.0485920421243081,
24.6947398844314));
#53804=CARTESIAN_POINT('Ctrl Pts',(6.76549143108519,0.142880005294184,24.7037692128532));
#53805=CARTESIAN_POINT('Ctrl Pts',(6.76144204368639,0.334621989705024,24.712811270808));
#53806=CARTESIAN_POINT('Ctrl Pts',(6.74923885109273,0.52610567730403,24.7218533287628));
#53807=CARTESIAN_POINT('Ctrl Pts',(6.7289438899742,0.716661095343454,24.7308953867177));
#53808=CARTESIAN_POINT('Ctrl Pts',(6.71133138941633,0.882030094422799,24.7387423222128));
#53809=CARTESIAN_POINT('Ctrl Pts',(6.68762562503935,1.0466999766423,24.746589257708));
#53810=CARTESIAN_POINT('Ctrl Pts',(6.65789856411851,1.21023787327482,24.7544361932031));
#53811=CARTESIAN_POINT('Ctrl Pts',(6.62511607717144,1.3905846279029,24.7630896575039));
#53812=CARTESIAN_POINT('Ctrl Pts',(6.58498069800237,1.56971346366483,24.7717431218046));
#53813=CARTESIAN_POINT('Ctrl Pts',(6.53760001254048,1.7470189111829,24.7803965861053));
#53814=CARTESIAN_POINT('Ctrl Pts',(6.49026297438123,1.92416102411745,24.7890420787955));
#53815=CARTESIAN_POINT('Ctrl Pts',(6.43569402042041,2.09948280635722,24.7976875714856));
#53816=CARTESIAN_POINT('Ctrl Pts',(6.37405162045641,2.27238969803972,24.8063330641757));
#53817=CARTESIAN_POINT('Ctrl Pts',(6.31055481470666,2.45049819674137,24.8152386416723));
#53818=CARTESIAN_POINT('Ctrl Pts',(6.23955237982781,2.62604391898996,24.8241442191689));
#53819=CARTESIAN_POINT('Ctrl Pts',(6.1612733726827,2.79839229327684,24.8330497966655));
#53820=CARTESIAN_POINT('Ctrl Pts',(6.08542467505829,2.96538980901066,24.8416788848379));
#53821=CARTESIAN_POINT('Ctrl Pts',(6.00274458260455,3.12938522489419,24.8503079730104));
#53822=CARTESIAN_POINT('Ctrl Pts',(5.91349098719739,3.28981965225075,24.8589370611829));
#53823=CARTESIAN_POINT('Ctrl Pts',(5.81994765703926,3.45796493019147,24.8679808833416));
#53824=CARTESIAN_POINT('Ctrl Pts',(5.71918348259384,3.62219816265412,24.8770247055002));
#53825=CARTESIAN_POINT('Ctrl Pts',(5.61155085342805,3.78190243388047,24.8860685276589));
#53826=CARTESIAN_POINT('Ctrl Pts',(5.50391822426225,3.94160670510681,24.8951123498175));
#53827=CARTESIAN_POINT('Ctrl Pts',(5.38941732699857,4.09678167621332,24.9041561719762));
#53828=CARTESIAN_POINT('Ctrl Pts',(5.26845483302557,4.24684267101685,24.9131999941348));
#53829=CARTESIAN_POINT('Ctrl Pts',(5.15576715296944,4.38663827886121,24.9216251456378));
#53830=CARTESIAN_POINT('Ctrl Pts',(5.03752120343059,4.52193457477448,24.9300502971407));
#53831=CARTESIAN_POINT('Ctrl Pts',(4.91410992194947,4.65229112104969,24.9384754486437));
#53832=CARTESIAN_POINT('Ctrl Pts',(4.79067136733749,4.78267647531638,24.9469024620531));
#53833=CARTESIAN_POINT('Ctrl Pts',(4.66206543304073,4.9081196631357,24.9553294754625));
#53834=CARTESIAN_POINT('Ctrl Pts',(4.52872222401741,5.02821678308432,24.9637564888719));
#53835=CARTESIAN_POINT('Ctrl Pts',(4.39528593922621,5.1483977328113,24.9721893844762));
#53836=CARTESIAN_POINT('Ctrl Pts',(4.2571060198141,5.26322493735222,24.9806222800805));
#53837=CARTESIAN_POINT('Ctrl Pts',(4.11464674081503,5.37233386884139,24.9890551756848));
#53838=CARTESIAN_POINT('Ctrl Pts',(3.97213064006988,5.48148631985448,24.9974914348597));
#53839=CARTESIAN_POINT('Ctrl Pts',(3.8253320428754,5.5849157532515,25.0059276940347));
#53840=CARTESIAN_POINT('Ctrl Pts',(3.67474505553761,5.68230039480508,25.0143639532097));
#53841=CARTESIAN_POINT('Ctrl Pts',(3.52402872618747,5.77976868186969,25.0228074584473));
#53842=CARTESIAN_POINT('Ctrl Pts',(3.36951778907315,5.87118163235017,25.0312509636848));
#53843=CARTESIAN_POINT('Ctrl Pts',(3.21173266199104,5.95626244451165,25.0396944689224));
#53844=CARTESIAN_POINT('Ctrl Pts',(3.17436478733321,5.97641192997604,25.0416941240941));
#53845=CARTESIAN_POINT('Ctrl Pts',(3.13681337133934,5.9962064703819,25.0436937792658));
#53846=CARTESIAN_POINT('Ctrl Pts',(3.09908550384716,6.01564277861015,25.0456934344376));
#53847=CARTESIAN_POINT('Ctrl Pts',(3.09908550384706,6.0156427786102,23.0456261631097));
#53848=CARTESIAN_POINT('Ctrl Pts',(2.94196606588778,6.0965861774243,23.0539315269246));
#53849=CARTESIAN_POINT('Ctrl Pts',(2.78173892819578,6.17133642383441,23.0622368907394));
#53850=CARTESIAN_POINT('Ctrl Pts',(2.61893168606547,6.23967032973075,23.0705422545543));
#53851=CARTESIAN_POINT('Ctrl Pts',(2.45593279780636,6.30808467387025,23.0788573949049));
#53852=CARTESIAN_POINT('Ctrl Pts',(2.29034805782135,6.3700674512532,23.0871725352556));
#53853=CARTESIAN_POINT('Ctrl Pts',(2.12272356423858,6.42544423910334,23.0954876756062));
#53854=CARTESIAN_POINT('Ctrl Pts',(1.95499601547681,6.48085507248383,23.1038079280873));
#53855=CARTESIAN_POINT('Ctrl Pts',(1.78522654617375,6.52965172074197,23.1121281805683));
#53856=CARTESIAN_POINT('Ctrl Pts',(1.61397385552916,6.5717103857115,23.1204484330494));
#53857=CARTESIAN_POINT('Ctrl Pts',(1.4424607602372,6.61383300454814,23.1287813371998));
#53858=CARTESIAN_POINT('Ctrl Pts',(1.2694602766696,6.64919709226822,23.1371142413502));
#53859=CARTESIAN_POINT('Ctrl Pts',(1.09554010378793,6.67773021924309,23.1454471455006));
#53860=CARTESIAN_POINT('Ctrl Pts',(0.946997402047146,6.70209994990593,23.1525641582964));
#53861=CARTESIAN_POINT('Ctrl Pts',(0.797784048357197,6.72148761566964,23.1596811710922));
#53862=CARTESIAN_POINT('Ctrl Pts',(0.648254563906394,6.73587819221626,23.166798183888));
#53863=CARTESIAN_POINT('Ctrl Pts',(0.478672985863151,6.75219856333698,23.1748695971301));
#53864=CARTESIAN_POINT('Ctrl Pts',(0.308162695173207,6.76214065689063,23.1829410103721));
#53865=CARTESIAN_POINT('Ctrl Pts',(0.137254858684796,6.76560788870944,23.1910124236141));
#53866=CARTESIAN_POINT('Ctrl Pts',(-0.0334384171712378,6.7690707677059,
23.1990737038653));
#53867=CARTESIAN_POINT('Ctrl Pts',(-0.204527877618031,6.76607495143243,
23.2071349841165));
#53868=CARTESIAN_POINT('Ctrl Pts',(-0.375474229969245,6.75657517553302,
23.2151962643678));
#53869=CARTESIAN_POINT('Ctrl Pts',(-0.54624346265954,6.74708524247063,23.2232491922254));
#53870=CARTESIAN_POINT('Ctrl Pts',(-0.716869513095837,6.73110478077824,
23.231302120083));
#53871=CARTESIAN_POINT('Ctrl Pts',(-0.88681015760305,6.70864045424794,23.2393550479406));
#53872=CARTESIAN_POINT('Ctrl Pts',(-1.05661193757673,6.68619448411634,23.247401395465));
#53873=CARTESIAN_POINT('Ctrl Pts',(-1.22572905848472,6.65727524299328,23.2554477429894));
#53874=CARTESIAN_POINT('Ctrl Pts',(-1.39362159845902,6.62194139511281,23.2634940905138));
#53875=CARTESIAN_POINT('Ctrl Pts',(-1.56141367369068,6.58662869055374,23.271535623207));
#53876=CARTESIAN_POINT('Ctrl Pts',(-1.72798226267916,6.54490909703747,23.2795771559002));
#53877=CARTESIAN_POINT('Ctrl Pts',(-1.89279496000941,6.49689281421227,23.2876186885934));
#53878=CARTESIAN_POINT('Ctrl Pts',(-2.06077613818036,6.44795343095465,23.2958148176416));
#53879=CARTESIAN_POINT('Ctrl Pts',(-2.22693283221004,6.39247284335409,23.3040109466899));
#53880=CARTESIAN_POINT('Ctrl Pts',(-2.39071426966323,6.33062195055341,23.3122070757381));
#53881=CARTESIAN_POINT('Ctrl Pts',(-2.55135097294168,6.26995864420546,23.3202458325742));
#53882=CARTESIAN_POINT('Ctrl Pts',(-2.70970245245694,6.20316760287597,23.3282845894103));
#53883=CARTESIAN_POINT('Ctrl Pts',(-2.86526672974682,6.13045965384375,23.3363233462464));
#53884=CARTESIAN_POINT('Ctrl Pts',(-3.02084606401434,6.05774466745062,23.3443628811492));
#53885=CARTESIAN_POINT('Ctrl Pts',(-3.17363732048882,5.97911179106404,23.352402416052));
#53886=CARTESIAN_POINT('Ctrl Pts',(-3.32316107945763,5.89481886405155,23.3604419509548));
#53887=CARTESIAN_POINT('Ctrl Pts',(-3.47272891650268,5.81050108834552,23.3684838558304));
#53888=CARTESIAN_POINT('Ctrl Pts',(-3.6190270136101,5.72052012416416,23.3765257607059));
#53889=CARTESIAN_POINT('Ctrl Pts',(-3.76160313863333,5.62517829294538,23.3845676655814));
#53890=CARTESIAN_POINT('Ctrl Pts',(-3.9089886817515,5.52662036416332,23.3928808422622));
#53891=CARTESIAN_POINT('Ctrl Pts',(-4.05239639633216,5.42233381609275,23.401194018943));
#53892=CARTESIAN_POINT('Ctrl Pts',(-4.19136287490199,5.31269858460777,23.4095071956238));
#53893=CARTESIAN_POINT('Ctrl Pts',(-4.32602806928495,5.20645677787069,23.4175630632344));
#53894=CARTESIAN_POINT('Ctrl Pts',(-4.45652262851063,5.09519275380206,23.4256189308449));
#53895=CARTESIAN_POINT('Ctrl Pts',(-4.58246202668122,4.97929018777021,23.4336747984555));
#53896=CARTESIAN_POINT('Ctrl Pts',(-4.7144352906662,4.85783462925833,23.4421166296714));
#53897=CARTESIAN_POINT('Ctrl Pts',(-4.84140582776385,4.73128546389627,23.4505584608874));
#53898=CARTESIAN_POINT('Ctrl Pts',(-4.96297864168079,4.60012304207402,23.4590002921033));
#53899=CARTESIAN_POINT('Ctrl Pts',(-5.08455145559772,4.46896062025177,23.4674421233193));
#53900=CARTESIAN_POINT('Ctrl Pts',(-5.20072631158247,4.33318534796473,23.4758839545352));
#53901=CARTESIAN_POINT('Ctrl Pts',(-5.31116064737433,4.19331152882568,23.4843257857512));
#53902=CARTESIAN_POINT('Ctrl Pts',(-5.42026318551523,4.05512453672664,23.4926658115739));
#53903=CARTESIAN_POINT('Ctrl Pts',(-5.52411789085058,3.91248865961095,23.5010058373966));
#53904=CARTESIAN_POINT('Ctrl Pts',(-5.62234753441595,3.76583286966468,23.5093458632193));
#53905=CARTESIAN_POINT('Ctrl Pts',(-5.72040644613119,3.61943198051454,23.5176713933359));
#53906=CARTESIAN_POINT('Ctrl Pts',(-5.81285959669981,3.4690253938297,23.5259969234526));
#53907=CARTESIAN_POINT('Ctrl Pts',(-5.89937016156137,3.31507476490039,23.5343224535693));
#53908=CARTESIAN_POINT('Ctrl Pts',(-5.98579102568036,3.16128376370853,23.5426393511422));
#53909=CARTESIAN_POINT('Ctrl Pts',(-6.06628140900166,3.00395633964463,23.5509562487151));
#53910=CARTESIAN_POINT('Ctrl Pts',(-6.14054729391427,2.84358364237842,23.559273146288));
#53911=CARTESIAN_POINT('Ctrl Pts',(-6.21474837457741,2.68335088597866,23.5675827865543));
#53912=CARTESIAN_POINT('Ctrl Pts',(-6.28273563240102,2.5200784629357,23.5758924268205));
#53913=CARTESIAN_POINT('Ctrl Pts',(-6.34426048947774,2.35428287205504,23.5842020670867));
#53914=CARTESIAN_POINT('Ctrl Pts',(-6.40574176168773,2.18860473254404,23.5925058207149));
#53915=CARTESIAN_POINT('Ctrl Pts',(-6.46076963478621,2.0204073104585,23.6008095743431));
#53916=CARTESIAN_POINT('Ctrl Pts',(-6.50914319088074,1.85022807259291,23.6091133279712));
#53917=CARTESIAN_POINT('Ctrl Pts',(-6.55748843617753,1.68014843273855,23.6174122217977));
#53918=CARTESIAN_POINT('Ctrl Pts',(-6.5991870333806,1.50808962186954,23.6257111156243));
#53919=CARTESIAN_POINT('Ctrl Pts',(-6.63408752911016,1.33460543086901,23.6340100094508));
#53920=CARTESIAN_POINT('Ctrl Pts',(-6.66897587017113,1.16118165857611,23.6423060130517));
#53921=CARTESIAN_POINT('Ctrl Pts',(-6.69707076005188,0.986333834813457,
23.6506020166527));
#53922=CARTESIAN_POINT('Ctrl Pts',(-6.71827151180999,0.810627469064775,
23.6588980202536));
#53923=CARTESIAN_POINT('Ctrl Pts',(-6.73947005152071,0.634939436194601,
23.6671931582649));
#53924=CARTESIAN_POINT('Ctrl Pts',(-6.75377584224094,0.458393383404347,
23.6754882962761));
#53925=CARTESIAN_POINT('Ctrl Pts',(-6.76113983933595,0.281561845682635,
23.6837834342873));
#53926=CARTESIAN_POINT('Ctrl Pts',(-6.76510403614756,0.186369654677821,
23.6882488841282));
#53927=CARTESIAN_POINT('Ctrl Pts',(-6.7670574619932,0.0910948258338363,
23.6927143339691));
#53928=CARTESIAN_POINT('Ctrl Pts',(-6.76699871332258,-0.00417299538677052,
23.6971797838099));
#53929=CARTESIAN_POINT('',(-6.76699967020645,0.00131471018405068,23.3028202161898));
#53930=CARTESIAN_POINT('Ctrl Pts',(3.09908550384738,6.01564277861003,22.6514909292461));
#53931=CARTESIAN_POINT('Ctrl Pts',(2.93986815724682,6.09766695939506,22.6599172859334));
#53932=CARTESIAN_POINT('Ctrl Pts',(2.77733107740478,6.17339780661688,22.6683436426207));
#53933=CARTESIAN_POINT('Ctrl Pts',(2.61200124368849,6.24257466939482,22.676769999308));
#53934=CARTESIAN_POINT('Ctrl Pts',(2.44671664424222,6.31173260537158,22.6851940505427));
#53935=CARTESIAN_POINT('Ctrl Pts',(2.27864112082035,6.37434000160425,22.6936181017774));
#53936=CARTESIAN_POINT('Ctrl Pts',(2.10832292993519,6.43018377833087,22.7020421530121));
#53937=CARTESIAN_POINT('Ctrl Pts',(1.93803032010428,6.48601916756421,22.7104649389908));
#53938=CARTESIAN_POINT('Ctrl Pts',(1.7654960309847,6.5350928585057,22.7188877249695));
#53939=CARTESIAN_POINT('Ctrl Pts',(1.59128515308273,6.57724110562921,22.7273105109482));
#53940=CARTESIAN_POINT('Ctrl Pts',(1.41707614735013,6.61938889980362,22.7357332064108));
#53941=CARTESIAN_POINT('Ctrl Pts',(1.24119091286643,6.65461132040979,22.7441559018735));
#53942=CARTESIAN_POINT('Ctrl Pts',(1.06420681222095,6.68279528796315,22.7525785973361));
#53943=CARTESIAN_POINT('Ctrl Pts',(0.887199933301354,6.71098288286008,22.7610023768197));
#53944=CARTESIAN_POINT('Ctrl Pts',(0.709094235577874,6.7321301668121,22.7694261563032));
#53945=CARTESIAN_POINT('Ctrl Pts',(0.530474687802311,6.74617562813192,22.7778499357868));
#53946=CARTESIAN_POINT('Ctrl Pts',(0.351737367345903,6.76023035031738,22.7862792694838));
#53947=CARTESIAN_POINT('Ctrl Pts',(0.172485852483893,6.76717386518292,22.7947086031807));
#53948=CARTESIAN_POINT('Ctrl Pts',(-0.0066913210940973,6.76699669175492,
22.8031379368777));
#53949=CARTESIAN_POINT('Ctrl Pts',(-0.185926256653699,6.76681946121089,
22.811569987969));
#53950=CARTESIAN_POINT('Ctrl Pts',(-0.365086469648003,6.75951697150564,
22.8200020390602));
#53951=CARTESIAN_POINT('Ctrl Pts',(-0.543585453003535,6.74513186344663,
22.8284340901514));
#53952=CARTESIAN_POINT('Ctrl Pts',(-0.72225783924089,6.73073278097081,22.8368743325608));
#53953=CARTESIAN_POINT('Ctrl Pts',(-0.900267379823388,6.70923736226023,
22.8453145749701));
#53954=CARTESIAN_POINT('Ctrl Pts',(-1.07703344825401,6.68074007512207,22.8537548173795));
#53955=CARTESIAN_POINT('Ctrl Pts',(-1.22328200824711,6.65716265868312,22.8607379070036));
#53956=CARTESIAN_POINT('Ctrl Pts',(-1.36867944026832,6.62879329037425,22.8677209966278));
#53957=CARTESIAN_POINT('Ctrl Pts',(-1.51290324157073,6.59571169637097,22.8747040862519));
#53958=CARTESIAN_POINT('Ctrl Pts',(-1.68104929026209,6.55714289381666,22.8828454534698));
#53959=CARTESIAN_POINT('Ctrl Pts',(-1.84793380259225,6.51209085151953,22.8909868206877));
#53960=CARTESIAN_POINT('Ctrl Pts',(-2.01301533523164,6.46065463092729,22.8991281879055));
#53961=CARTESIAN_POINT('Ctrl Pts',(-2.17795276424785,6.40926331024379,22.907262448329));
#53962=CARTESIAN_POINT('Ctrl Pts',(-2.34108999927349,6.35149901234894,22.9153967087524));
#53963=CARTESIAN_POINT('Ctrl Pts',(-2.50189643805424,6.28751168692763,22.9235309691759));
#53964=CARTESIAN_POINT('Ctrl Pts',(-2.6625931804919,6.22356801134805,22.9316596807008));
#53965=CARTESIAN_POINT('Ctrl Pts',(-2.82096195357071,6.15340989493447,22.9397883922256));
#53966=CARTESIAN_POINT('Ctrl Pts',(-2.97648800098441,6.07723688694096,22.9479171037505));
#53967=CARTESIAN_POINT('Ctrl Pts',(-3.13193988089993,6.00110020444743,22.956041938843));
#53968=CARTESIAN_POINT('Ctrl Pts',(-3.28455140667152,5.91895450301538,22.9641667739355));
#53969=CARTESIAN_POINT('Ctrl Pts',(-3.4338284951019,5.83104715006029,22.972291609028));
#53970=CARTESIAN_POINT('Ctrl Pts',(-3.58306379299294,5.74316440701507,22.9804141695502));
#53971=CARTESIAN_POINT('Ctrl Pts',(-3.72896619814001,5.6495234115118,22.9885367300724));
#53972=CARTESIAN_POINT('Ctrl Pts',(-3.8710669353214,5.55041708182921,22.9966592905946));
#53973=CARTESIAN_POINT('Ctrl Pts',(-4.01317522478872,5.45130548490201,23.0047822828098));
#53974=CARTESIAN_POINT('Ctrl Pts',(-4.15148114016511,5.34672817971588,23.012905275025));
#53975=CARTESIAN_POINT('Ctrl Pts',(-4.28554541765919,5.23702104952618,23.0210282672402));
#53976=CARTESIAN_POINT('Ctrl Pts',(-4.35398114576626,5.18101890284396,23.0251748072213));
#53977=CARTESIAN_POINT('Ctrl Pts',(-4.42131209509528,5.12368070100619,23.0293213472023));
#53978=CARTESIAN_POINT('Ctrl Pts',(-4.48748318345132,5.06505515056269,23.0334678871833));
#53979=CARTESIAN_POINT('Ctrl Pts',(-4.63084572138578,4.93804034835539,23.0424515462117));
#53980=CARTESIAN_POINT('Ctrl Pts',(-4.76869106892665,4.80504354482025,23.05143520524));
#53981=CARTESIAN_POINT('Ctrl Pts',(-4.90056436154782,4.66655739687486,23.0604188642684));
#53982=CARTESIAN_POINT('Ctrl Pts',(-5.03266421108922,4.52783333119382,23.0694179571278));
#53983=CARTESIAN_POINT('Ctrl Pts',(-5.15877133406117,4.38360124512236,23.0784170499873));
#53984=CARTESIAN_POINT('Ctrl Pts',(-5.2784704105158,4.2343876918994,23.0874161428467));
#53985=CARTESIAN_POINT('Ctrl Pts',(-5.39845014785484,4.08482427459184,23.0964363360642));
#53986=CARTESIAN_POINT('Ctrl Pts',(-5.5119916259134,3.9302562075175,23.1054565292816));
#53987=CARTESIAN_POINT('Ctrl Pts',(-5.61872062340603,3.77124217680485,23.114476722499));
#53988=CARTESIAN_POINT('Ctrl Pts',(-5.72555771073407,3.61206710456823,23.1235060509207));
#53989=CARTESIAN_POINT('Ctrl Pts',(-5.8255684061678,3.44843727526012,23.1325353793424));
#53990=CARTESIAN_POINT('Ctrl Pts',(-5.91842315118929,3.28093834191786,23.1415647077642));
#53991=CARTESIAN_POINT('Ctrl Pts',(-6.01140880268452,3.11320326884235,23.1506067657189));
#53992=CARTESIAN_POINT('Ctrl Pts',(-6.09721821579471,2.9415883943495,23.1596488236737));
#53993=CARTESIAN_POINT('Ctrl Pts',(-6.17556786884616,2.76670390487939,23.1686908816285));
#53994=CARTESIAN_POINT('Ctrl Pts',(-6.24356175659459,2.61493454939594,23.176537817124));
#53995=CARTESIAN_POINT('Ctrl Pts',(-6.3059382395626,2.46070320449476,23.1843847526195));
#53996=CARTESIAN_POINT('Ctrl Pts',(-6.36254168907972,2.30442015585758,23.192231688115));
#53997=CARTESIAN_POINT('Ctrl Pts',(-6.42901872513224,2.12087597352802,23.2014473987879));
#53998=CARTESIAN_POINT('Ctrl Pts',(-6.48758449919244,1.93435488806567,23.2106631094608));
#53999=CARTESIAN_POINT('Ctrl Pts',(-6.53799515801084,1.7455395480558,23.2198788201337));
#54000=CARTESIAN_POINT('Ctrl Pts',(-6.58641319465717,1.56418766204055,23.2287302540872));
#54001=CARTESIAN_POINT('Ctrl Pts',(-6.62730830956766,1.38071969702469,23.2375816880407));
#54002=CARTESIAN_POINT('Ctrl Pts',(-6.66051430440762,1.19575842074454,23.2464331219941));
#54003=CARTESIAN_POINT('Ctrl Pts',(-6.69368573792491,1.01098965507524,23.2552753432357));
#54004=CARTESIAN_POINT('Ctrl Pts',(-6.71918396897205,0.824730943739976,
23.2641175644772));
#54005=CARTESIAN_POINT('Ctrl Pts',(-6.73689348630898,0.637616776855506,
23.2729597857188));
#54006=CARTESIAN_POINT('Ctrl Pts',(-6.75457764120661,0.450770582926593,
23.281789343696));
#54007=CARTESIAN_POINT('Ctrl Pts',(-6.76449531809539,0.263071646712626,
23.2906189016732));
#54008=CARTESIAN_POINT('Ctrl Pts',(-6.7665825759315,0.0751614469011366,
23.2994484596503));
#54009=CARTESIAN_POINT('Ctrl Pts',(-6.76684826402433,0.0512422636802975,
23.3005723784968));
#54010=CARTESIAN_POINT('Ctrl Pts',(-6.76698714541347,0.0273196671605242,
23.3016962973433));
#54011=CARTESIAN_POINT('Ctrl Pts',(-6.76699914837107,0.00339498825326048,
23.3028202161898));
#54012=CARTESIAN_POINT('Ctrl Pts',(-6.767,3.50975458611922E-12,23.3028202161898));
#54013=CARTESIAN_POINT('Ctrl Pts',(-6.7670000000001,-0.186007249556406,
23.3115697280025));
#54014=CARTESIAN_POINT('Ctrl Pts',(-6.75932637294267,-0.3720143558125,23.3203192398153));
#54015=CARTESIAN_POINT('Ctrl Pts',(-6.74400518263393,-0.55738953758279,
23.329068751628));
#54016=CARTESIAN_POINT('Ctrl Pts',(-6.72868405703767,-0.742763936379368,
23.3378182264852));
#54017=CARTESIAN_POINT('Ctrl Pts',(-6.70571545643609,-0.927506130401786,
23.3465677013424));
#54018=CARTESIAN_POINT('Ctrl Pts',(-6.67517739401625,-1.11098864009241,
23.3553171761996));
#54019=CARTESIAN_POINT('Ctrl Pts',(-6.6446394580445,-1.29447039004228,23.3640666148281));
#54020=CARTESIAN_POINT('Ctrl Pts',(-6.60653217002795,-1.47669218338956,
23.3728160534566));
#54021=CARTESIAN_POINT('Ctrl Pts',(-6.56098496085563,-1.65703510627453,
23.3815654920851));
#54022=CARTESIAN_POINT('Ctrl Pts',(-6.51543793649644,-1.837377297397,23.3903148952118));
#54023=CARTESIAN_POINT('Ctrl Pts',(-6.46245112156986,-2.01584035544665,
23.3990642983384));
#54024=CARTESIAN_POINT('Ctrl Pts',(-6.40220448361808,-2.19181813797142,
23.4078137014651));
#54025=CARTESIAN_POINT('Ctrl Pts',(-6.34195808512073,-2.36779522106033,
23.4165630698166));
#54026=CARTESIAN_POINT('Ctrl Pts',(-6.27445201416464,-2.54128677725471,
23.4253124381681));
#54027=CARTESIAN_POINT('Ctrl Pts',(-6.19991555052845,-2.71170355428383,
23.4340618065196));
#54028=CARTESIAN_POINT('Ctrl Pts',(-6.12537937695242,-2.88211966813258,
23.4428111408228));
#54029=CARTESIAN_POINT('Ctrl Pts',(-6.04381298028472,-3.04946076419628,
23.451560475126));
#54030=CARTESIAN_POINT('Ctrl Pts',(-5.95549339309,-3.21315848424278,23.4603098094292));
#54031=CARTESIAN_POINT('Ctrl Pts',(-5.8671741422582,-3.37685558085064,23.4690591104108));
#54032=CARTESIAN_POINT('Ctrl Pts',(-5.77210188844069,-3.53690907699996,
23.4778084113923));
#54033=CARTESIAN_POINT('Ctrl Pts',(-5.67059953311365,-3.69277537024002,
23.4865577123739));
#54034=CARTESIAN_POINT('Ctrl Pts',(-5.5690975559269,-3.84864108281052,23.4953069807605));
#54035=CARTESIAN_POINT('Ctrl Pts',(-5.46116568154937,-4.00031938354869,
23.5040562491471));
#54036=CARTESIAN_POINT('Ctrl Pts',(-5.34717048488336,-4.14729511918218,
23.5128055175338));
#54037=CARTESIAN_POINT('Ctrl Pts',(-5.23317570343258,-4.29427031947236,
23.5215547540521));
#54038=CARTESIAN_POINT('Ctrl Pts',(-5.11311781951494,-4.43654276249617,
23.5303039905705));
#54039=CARTESIAN_POINT('Ctrl Pts',(-4.98740458929186,-4.57362924412447,
23.5390532270888));
#54040=CARTESIAN_POINT('Ctrl Pts',(-4.86169180652679,-4.71071523781331,
23.5478024324655));
#54041=CARTESIAN_POINT('Ctrl Pts',(-4.73032391141509,-4.84261509584551,
23.5565516378422));
#54042=CARTESIAN_POINT('Ctrl Pts',(-4.59374706947262,-4.96888084599659,
23.565300843219));
#54043=CARTESIAN_POINT('Ctrl Pts',(-4.4571707023148,-5.09514615720765,23.5740500181806));
#54044=CARTESIAN_POINT('Ctrl Pts',(-4.31538563497374,-5.21577720520572,
23.5827991931424));
#54045=CARTESIAN_POINT('Ctrl Pts',(-4.16887340952094,-5.33036429293433,
23.591548368104));
#54046=CARTESIAN_POINT('Ctrl Pts',(-4.0223616812255,-5.44495099183659,23.6002975133773));
#54047=CARTESIAN_POINT('Ctrl Pts',(-3.87112305263222,-5.55349359497901,
23.6090466586506));
#54048=CARTESIAN_POINT('Ctrl Pts',(-3.71567116929011,-5.65562346357201,
23.6177958039238));
#54049=CARTESIAN_POINT('Ctrl Pts',(-3.56021980053325,-5.75775299408919,
23.6265449202352));
#54050=CARTESIAN_POINT('Ctrl Pts',(-3.40055544442095,-5.85346967519873,
23.6352940365466));
#54051=CARTESIAN_POINT('Ctrl Pts',(-3.23722035886851,-5.94244843041378,
23.6440431528579));
#54052=CARTESIAN_POINT('Ctrl Pts',(-3.07388580043516,-6.03142689847437,
23.652792240934));
#54053=CARTESIAN_POINT('Ctrl Pts',(-2.90688078789267,-6.1136673470788,23.6615413290099));
#54054=CARTESIAN_POINT('Ctrl Pts',(-2.73677250610456,-6.18889047001401,
23.670290417086));
#54055=CARTESIAN_POINT('Ctrl Pts',(-2.56666475917031,-6.26411335643293,
23.6790394776531));
#54056=CARTESIAN_POINT('Ctrl Pts',(-2.39345402457224,-6.33231884545205,
23.6877885382203));
#54057=CARTESIAN_POINT('Ctrl Pts',(-2.21772855944231,-6.39327529804825,
23.6965375987874));
#54058=CARTESIAN_POINT('Ctrl Pts',(-2.04200363223765,-6.45423156404647,
23.7052866325722));
#54059=CARTESIAN_POINT('Ctrl Pts',(-1.86376426061217,-6.507938744124,23.714035666357));
#54060=CARTESIAN_POINT('Ctrl Pts',(-1.68361577621879,-6.55421443943263,
23.7227847001418));
#54061=CARTESIAN_POINT('Ctrl Pts',(-1.50346782833402,-6.60048999692545,
23.7315337078707));
#54062=CARTESIAN_POINT('Ctrl Pts',(-1.3214110565757,-6.63933404265125,23.7402827155996));
#54063=CARTESIAN_POINT('Ctrl Pts',(-1.13806375346714,-6.67061465631499,
23.7490317233285));
#54064=CARTESIAN_POINT('Ctrl Pts',(-0.954716981171266,-6.70189517941754,
23.757780705728));
#54065=CARTESIAN_POINT('Ctrl Pts',(-0.770079967443005,-6.72561226608997,
23.7665296881274));
#54066=CARTESIAN_POINT('Ctrl Pts',(-0.584779764073251,-6.74168536995983,
23.7752786705269));
#54067=CARTESIAN_POINT('Ctrl Pts',(-0.391489587593115,-6.75845153117872,
23.7844049009425));
#54068=CARTESIAN_POINT('Ctrl Pts',(-0.197478091805371,-6.76689985146394,
23.7935311313581));
#54069=CARTESIAN_POINT('Ctrl Pts',(-0.0034621475311433,-6.76699911434415,
23.8026573617737));
#54070=CARTESIAN_POINT('Ctrl Pts',(0.184490798484599,-6.76709527525935,
23.8114983974888));
#54071=CARTESIAN_POINT('Ctrl Pts',(0.372447602154806,-6.75935633790763,
23.820339433204));
#54072=CARTESIAN_POINT('Ctrl Pts',(0.559756448194312,-6.74380914014512,
23.8291804689191));
#54073=CARTESIAN_POINT('Ctrl Pts',(0.745136131043408,-6.72842206873154,
23.8379304475324));
#54074=CARTESIAN_POINT('Ctrl Pts',(0.92988085194505,-6.70538686355723,23.8466804261457));
#54075=CARTESIAN_POINT('Ctrl Pts',(1.11336305057459,-6.67478177303313,23.855430404759));
#54076=CARTESIAN_POINT('Ctrl Pts',(1.29684337090112,-6.64417699581263,23.864180293799));
#54077=CARTESIAN_POINT('Ctrl Pts',(1.47906091205171,-6.60600253548064,23.872930182839));
#54078=CARTESIAN_POINT('Ctrl Pts',(1.65939671095195,-6.56038806441219,23.881680071879));
#54079=CARTESIAN_POINT('Ctrl Pts',(1.83973072369144,-6.51477404513854,23.8904298742545));
#54080=CARTESIAN_POINT('Ctrl Pts',(2.0181827535703,-6.46172023288663,23.89917967663));
#54081=CARTESIAN_POINT('Ctrl Pts',(2.1941466403333,-6.40140683918107,23.9079294790055));
#54082=CARTESIAN_POINT('Ctrl Pts',(2.37010884271264,-6.34109402281496,23.916679197625));
#54083=CARTESIAN_POINT('Ctrl Pts',(2.54358267847811,-6.2735218569979,23.9254289162445));
#54084=CARTESIAN_POINT('Ctrl Pts',(2.71397890841748,-6.19891986435259,23.9341786348641));
#54085=CARTESIAN_POINT('Ctrl Pts',(2.88437356388955,-6.12431856103237,23.9429282726359));
#54086=CARTESIAN_POINT('Ctrl Pts',(3.05169040787191,-6.04268767582548,23.9516779104077));
#54087=CARTESIAN_POINT('Ctrl Pts',(3.21536112512079,-5.95430447953932,23.9604275481796));
#54088=CARTESIAN_POINT('Ctrl Pts',(3.37903038442868,-5.86592207055028,23.9691771080116));
#54089=CARTESIAN_POINT('Ctrl Pts',(3.53905332979999,-5.77078760703361,23.9779266678437));
#54090=CARTESIAN_POINT('Ctrl Pts',(3.69488643041918,-5.66922422085281,23.9866762276757));
#54091=CARTESIAN_POINT('Ctrl Pts',(3.85071819468769,-5.5676617056314,23.9954257124757));
#54092=CARTESIAN_POINT('Ctrl Pts',(4.00235994599251,-5.45967053456231,24.0041751972757));
#54093=CARTESIAN_POINT('Ctrl Pts',(4.14929662974328,-5.34561750206663,24.0129246820757));
#54094=CARTESIAN_POINT('Ctrl Pts',(4.29623210225067,-5.23156540974447,24.0216740947511));
#54095=CARTESIAN_POINT('Ctrl Pts',(4.43846235842135,-5.11145173172171,24.0304235074264));
#54096=CARTESIAN_POINT('Ctrl Pts',(4.57550431797442,-4.98568443006549,24.0391729201018));
#54097=CARTESIAN_POINT('Ctrl Pts',(4.71254519337506,-4.85991812336677,24.0479222635597));
#54098=CARTESIAN_POINT('Ctrl Pts',(4.84439764314995,-4.72849847631089,24.0566716070176));
#54099=CARTESIAN_POINT('Ctrl Pts',(4.97061384196697,-4.59187184425332,24.0654209504755));
#54100=CARTESIAN_POINT('Ctrl Pts',(5.09682908420216,-4.45524624767736,24.0741702276228));
#54101=CARTESIAN_POINT('Ctrl Pts',(5.2174079665018,-4.31341395556881,24.0829195047702));
#54102=CARTESIAN_POINT('Ctrl Pts',(5.3319409594226,-4.16685668162845,24.0916687819176));
#54103=CARTESIAN_POINT('Ctrl Pts',(5.44647312235144,-4.02030046975199,24.1004179956611));
#54104=CARTESIAN_POINT('Ctrl Pts',(5.55495930712302,-3.86901957035527,24.1091672094047));
#54105=CARTESIAN_POINT('Ctrl Pts',(5.65703106079811,-3.7135277805835,24.1179164231482));
#54106=CARTESIAN_POINT('Ctrl Pts',(5.75910210868747,-3.55803706597584,24.1266655763944));
#54107=CARTESIAN_POINT('Ctrl Pts',(5.85475865698557,-3.39833575880886,24.1354147296406));
#54108=CARTESIAN_POINT('Ctrl Pts',(5.94367583069067,-3.23496624706713,24.1441638828868));
#54109=CARTESIAN_POINT('Ctrl Pts',(6.03259241910079,-3.07159781070096,24.1529129785419));
#54110=CARTESIAN_POINT('Ctrl Pts',(6.11476958470967,-2.90456146975836,24.161662074197));
#54111=CARTESIAN_POINT('Ctrl Pts',(6.18992823574383,-2.73442451648264,24.1704111698521));
#54112=CARTESIAN_POINT('Ctrl Pts',(6.26508641700944,-2.56428862662396,24.1791602108223));
#54113=CARTESIAN_POINT('Ctrl Pts',(6.33322605570316,-2.39105242531229,24.1879092517924));
#54114=CARTESIAN_POINT('Ctrl Pts',(6.39411573747794,-2.21530425353652,24.1966582927625));
#54115=CARTESIAN_POINT('Ctrl Pts',(6.45500505889155,-2.03955712188469,24.2054072819535));
#54116=CARTESIAN_POINT('Ctrl Pts',(6.5086444154496,-1.86129832025464,24.2141562711445));
#54117=CARTESIAN_POINT('Ctrl Pts',(6.55485164049938,-1.68113324012185,24.2229052603356));
#54118=CARTESIAN_POINT('Ctrl Pts',(6.60199852639141,-1.49730435912764,24.2318321672124));
#54119=CARTESIAN_POINT('Ctrl Pts',(6.64140767441039,-1.31149113173507,24.2407590740893));
#54120=CARTESIAN_POINT('Ctrl Pts',(6.67293975269628,-1.12435050446277,24.2496859809662));
#54121=CARTESIAN_POINT('Ctrl Pts',(6.70384664831528,-0.940920291562243,
24.2584358951502));
#54122=CARTESIAN_POINT('Ctrl Pts',(6.72718585889682,-0.756215114276483,
24.2671858093342));
#54123=CARTESIAN_POINT('Ctrl Pts',(6.74287810451876,-0.570862389373729,
24.2759357235182));
#54124=CARTESIAN_POINT('Ctrl Pts',(6.75857004154131,-0.385513309566711,
24.2846854656288));
#54125=CARTESIAN_POINT('Ctrl Pts',(6.7666152903556,-0.199516993257844,24.2934352077393));
#54126=CARTESIAN_POINT('Ctrl Pts',(6.76698652348897,-0.0135052182037115,
24.3021849498499));
#54127=CARTESIAN_POINT('Ctrl Pts',(6.7673577498152,0.172503146039223,24.3109345315206));
#54128=CARTESIAN_POINT('Ctrl Pts',(6.76005524147477,0.358526681833787,24.3196841131912));
#54129=CARTESIAN_POINT('Ctrl Pts',(6.74510380214879,0.543933542115166,24.3284336948618));
#54130=CARTESIAN_POINT('Ctrl Pts',(6.73015261710976,0.729337249085047,24.3371831277238));
#54131=CARTESIAN_POINT('Ctrl Pts',(6.70755278444601,0.914124015855012,24.3459325605857));
#54132=CARTESIAN_POINT('Ctrl Pts',(6.67738106408283,1.09766621749423,24.3546819934476));
#54133=CARTESIAN_POINT('Ctrl Pts',(6.64720981677245,1.28120554143368,24.36343128913));
#54134=CARTESIAN_POINT('Ctrl Pts',(6.60946696581511,1.46350005650675,24.3721805848124));
#54135=CARTESIAN_POINT('Ctrl Pts',(6.56428070010979,1.64393062206597,24.3809298804947));
#54136=CARTESIAN_POINT('Ctrl Pts',(6.51909508282722,1.8243585984472,24.3896790506247));
#54137=CARTESIAN_POINT('Ctrl Pts',(6.46646633415639,2.00292240086636,24.3984282207547));
#54138=CARTESIAN_POINT('Ctrl Pts',(6.40657319597166,2.17901557696532,24.4071773908847));
#54139=CARTESIAN_POINT('Ctrl Pts',(6.34668083768269,2.35510646007503,24.4159264470877));
#54140=CARTESIAN_POINT('Ctrl Pts',(6.27952437143861,2.5287265099659,24.4246755032908));
#54141=CARTESIAN_POINT('Ctrl Pts',(6.20533187335114,2.69928607997976,24.4334245594939));
#54142=CARTESIAN_POINT('Ctrl Pts',(6.12831449784228,2.87633970115449,24.4425067357827));
#54143=CARTESIAN_POINT('Ctrl Pts',(6.04371489463127,3.05009490562401,24.4515889120716));
#54144=CARTESIAN_POINT('Ctrl Pts',(5.95184265120463,3.21991584599684,24.4606710883604));
#54145=CARTESIAN_POINT('Ctrl Pts',(5.86333281335457,3.38352155905362,24.4694208687148));
#54146=CARTESIAN_POINT('Ctrl Pts',(5.76807337235642,3.54347560903895,24.4781706490693));
#54147=CARTESIAN_POINT('Ctrl Pts',(5.66638790086304,3.69923467178725,24.4869204294237));
#54148=CARTESIAN_POINT('Ctrl Pts',(5.56470608502684,3.85498813489849,24.495669895218));
#54149=CARTESIAN_POINT('Ctrl Pts',(5.45659885766885,4.00654667256353,24.5044193610122));
#54150=CARTESIAN_POINT('Ctrl Pts',(5.34243340580432,4.15339551506308,24.5131688268065));
#54151=CARTESIAN_POINT('Ctrl Pts',(5.2282714514051,4.30023985883972,24.5219180245604));
#54152=CARTESIAN_POINT('Ctrl Pts',(5.10805181977998,4.44237456993148,24.5306672223142));
#54153=CARTESIAN_POINT('Ctrl Pts',(4.98218281282452,4.57931691626557,24.5394164200681));
#54154=CARTESIAN_POINT('Ctrl Pts',(4.85631699296131,4.71625579512262,24.5481653962861));
#54155=CARTESIAN_POINT('Ctrl Pts',(4.72480227791742,4.84800236135863,24.5569143725041));
#54156=CARTESIAN_POINT('Ctrl Pts',(4.5880853084802,4.97410918678995,24.5656633487221));
#54157=CARTESIAN_POINT('Ctrl Pts',(4.4513594505687,5.10022421089096,24.5744128937433));
#54158=CARTESIAN_POINT('Ctrl Pts',(4.30943087207933,5.22069856612075,24.5831624387645));
#54159=CARTESIAN_POINT('Ctrl Pts',(4.16278164322354,5.33512305301772,24.5919119837857));
#54160=CARTESIAN_POINT('Ctrl Pts',(4.01614103534282,5.44954081331506,24.600661014453));
#54161=CARTESIAN_POINT('Ctrl Pts',(3.86478055833311,5.55790924068408,24.6094100451202));
#54162=CARTESIAN_POINT('Ctrl Pts',(3.70921425811856,5.65986029751354,24.6181590757875));
#54163=CARTESIAN_POINT('Ctrl Pts',(3.55364584530038,5.76181273884704,24.6269082252673));
#54164=CARTESIAN_POINT('Ctrl Pts',(3.39387173464277,5.85734747818102,24.6356573747472));
#54165=CARTESIAN_POINT('Ctrl Pts',(3.23043456092353,5.94614005448836,24.644406524227));
#54166=CARTESIAN_POINT('Ctrl Pts',(3.18690768806362,5.96978744811297,24.64673661296));
#54167=CARTESIAN_POINT('Ctrl Pts',(3.14312114982874,5.99295688499304,24.6490667016931));
#54168=CARTESIAN_POINT('Ctrl Pts',(3.09908550384736,6.01564277861004,24.6513967904261));
#54169=CARTESIAN_POINT('Origin',(0.,0.,-63.6971797838103));
#54170=CARTESIAN_POINT('',(3.09908550384735,6.01564277861005,27.0459166703402));
#54171=CARTESIAN_POINT('',(3.09908550384733,6.01564277861006,26.6512146511404));
#54172=CARTESIAN_POINT('',(3.09908550384721,6.01564277861012,-63.6971797838103));
#54173=CARTESIAN_POINT('',(-6.76699883050778,-0.00397843013915454,25.6971797837804));
#54174=CARTESIAN_POINT('Ctrl Pts',(-6.76699883050741,-0.00397843076278133,
25.6971797838099));
#54175=CARTESIAN_POINT('Ctrl Pts',(-6.76695810834549,-0.0732436356925205,
25.7004595221374));
#54176=CARTESIAN_POINT('Ctrl Pts',(-6.765853956984,-0.142489156183605,25.7037392604649));
#54177=CARTESIAN_POINT('Ctrl Pts',(-6.76368796441601,-0.211693457655297,
25.7070189987924));
#54178=CARTESIAN_POINT('Ctrl Pts',(-6.75825243728204,-0.385360654853746,
25.7152494548589));
#54179=CARTESIAN_POINT('Ctrl Pts',(-6.74611593464877,-0.55907255138845,
25.7234799109255));
#54180=CARTESIAN_POINT('Ctrl Pts',(-6.72726299458639,-0.732271535476137,
25.731710366992));
#54181=CARTESIAN_POINT('Ctrl Pts',(-6.70843243407479,-0.905264922163828,
25.7399310530222));
#54182=CARTESIAN_POINT('Ctrl Pts',(-6.68290135018699,-1.07774625585958,
25.7481517390524));
#54183=CARTESIAN_POINT('Ctrl Pts',(-6.65070625872861,-1.24915782033659,
25.7563724250826));
#54184=CARTESIAN_POINT('Ctrl Pts',(-6.61854292540964,-1.42040029964833,
25.764585001998));
#54185=CARTESIAN_POINT('Ctrl Pts',(-6.57972874142569,-1.59057476132321,
25.7727975789134));
#54186=CARTESIAN_POINT('Ctrl Pts',(-6.53435201193211,-1.75912841605119,
25.7810101558288));
#54187=CARTESIAN_POINT('Ctrl Pts',(-6.48901094260993,-1.92754960966345,
25.7892162787335));
#54188=CARTESIAN_POINT('Ctrl Pts',(-6.43711769275813,-2.09435218870091,
25.7974224016381));
#54189=CARTESIAN_POINT('Ctrl Pts',(-6.3788116732331,-2.25899327963258,25.8056285245428));
#54190=CARTESIAN_POINT('Ctrl Pts',(-6.32053978382505,-2.42353799595766,
25.8138298438965));
#54191=CARTESIAN_POINT('Ctrl Pts',(-6.25586272209305,-2.58592340765658,
25.8220311632502));
#54192=CARTESIAN_POINT('Ctrl Pts',(-6.18496983250082,-2.7456214544352,25.8302324826039));
#54193=CARTESIAN_POINT('Ctrl Pts',(-6.1140972803988,-2.90527368762824,25.8384314491934));
#54194=CARTESIAN_POINT('Ctrl Pts',(-6.03701259396966,-3.06223976264625,
25.8466304157829));
#54195=CARTESIAN_POINT('Ctrl Pts',(-5.95395347458101,-3.21601104204024,
25.8548293823724));
#54196=CARTESIAN_POINT('Ctrl Pts',(-5.87090532352427,-3.36976201524217,
25.8630272662513));
#54197=CARTESIAN_POINT('Ctrl Pts',(-5.78188448046673,-3.52031871724852,
25.8712251501303));
#54198=CARTESIAN_POINT('Ctrl Pts',(-5.68717488564158,-3.66719658869383,
25.8794230340092));
#54199=CARTESIAN_POINT('Ctrl Pts',(-5.5924605933759,-3.81408174504061,25.8876213244897));
#54200=CARTESIAN_POINT('Ctrl Pts',(-5.49205718154599,-3.95728740587926,
25.8958196149703));
#54201=CARTESIAN_POINT('Ctrl Pts',(-5.38629227552321,-4.09635747007498,
25.9040179054508));
#54202=CARTESIAN_POINT('Ctrl Pts',(-5.28050291128713,-4.23545969432662,
25.9122180917921));
#54203=CARTESIAN_POINT('Ctrl Pts',(-5.16934980048246,-4.37042413176443,
25.9204182781334));
#54204=CARTESIAN_POINT('Ctrl Pts',(-5.05320127542262,-4.5008272428596,25.9286184644747));
#54205=CARTESIAN_POINT('Ctrl Pts',(-4.93694294104563,-4.63135363986459,
25.9368264034488));
#54206=CARTESIAN_POINT('Ctrl Pts',(-4.81567999566671,-4.75730982674317,
25.9450343424229));
#54207=CARTESIAN_POINT('Ctrl Pts',(-4.68981876342653,-4.87830800239309,
25.953242281397));
#54208=CARTESIAN_POINT('Ctrl Pts',(-4.56389647208926,-4.99936487792401,
25.961454202291));
#54209=CARTESIAN_POINT('Ctrl Pts',(-4.43337171404866,-5.11545870847014,
25.9696661231849));
#54210=CARTESIAN_POINT('Ctrl Pts',(-4.29868433841007,-5.22624166669587,
25.9778780440788));
#54211=CARTESIAN_POINT('Ctrl Pts',(-4.16381226037282,-5.33717654619869,
25.9861012263214));
#54212=CARTESIAN_POINT('Ctrl Pts',(-4.02476644234229,-5.44278578151289,
25.994324408564));
#54213=CARTESIAN_POINT('Ctrl Pts',(-3.88201717192874,-5.54276390231898,
26.0025475908065));
#54214=CARTESIAN_POINT('Ctrl Pts',(-3.75472084822987,-5.63191915468607,
26.0098805940895));
#54215=CARTESIAN_POINT('Ctrl Pts',(-3.62448003363244,-5.71659699308896,
26.0172135973724));
#54216=CARTESIAN_POINT('Ctrl Pts',(-3.49164434372748,-5.79661183597073,
26.0245466006554));
#54217=CARTESIAN_POINT('Ctrl Pts',(-3.32978546342189,-5.89410907399416,
26.0334817874377));
#54218=CARTESIAN_POINT('Ctrl Pts',(-3.16373792203329,-5.98488514976522,
26.04241697422));
#54219=CARTESIAN_POINT('Ctrl Pts',(-2.99405931104218,-6.06859933114402,
26.0513521610023));
#54220=CARTESIAN_POINT('Ctrl Pts',(-2.82463482611953,-6.15218813457645,
26.0602739656389));
#54221=CARTESIAN_POINT('Ctrl Pts',(-2.65159035386039,-6.22873603342583,
26.0691957702756));
#54222=CARTESIAN_POINT('Ctrl Pts',(-2.47550877308883,-6.29794770654379,
26.0781175749122));
#54223=CARTESIAN_POINT('Ctrl Pts',(-2.29985669705086,-6.36699055597734,
26.0870176171515));
#54224=CARTESIAN_POINT('Ctrl Pts',(-2.12118253804638,-6.42873280030971,
26.0959176593908));
#54225=CARTESIAN_POINT('Ctrl Pts',(-1.94008928689499,-6.48292700551806,
26.1048177016301));
#54226=CARTESIAN_POINT('Ctrl Pts',(-1.75927483146609,-6.53703777795075,
26.1137040421236));
#54227=CARTESIAN_POINT('Ctrl Pts',(-1.57604895901434,-6.58362361708434,
26.122590382617));
#54228=CARTESIAN_POINT('Ctrl Pts',(-1.39103276731701,-6.62248569951271,
26.1314767231104));
#54229=CARTESIAN_POINT('Ctrl Pts',(-1.20648962972656,-6.66124841837985,
26.1403403427824));
#54230=CARTESIAN_POINT('Ctrl Pts',(-1.02016555913015,-6.69232673410084,
26.1492039624543));
#54231=CARTESIAN_POINT('Ctrl Pts',(-0.832694137200324,-6.71557216280729,
26.1580675821263));
#54232=CARTESIAN_POINT('Ctrl Pts',(-0.654726691509346,-6.73763915055558,
26.1664818552797));
#54233=CARTESIAN_POINT('Ctrl Pts',(-0.475725582744447,-6.75264759780368,
26.1748961284332));
#54234=CARTESIAN_POINT('Ctrl Pts',(-0.296244233930681,-6.76051243278665,
26.1833104015867));
#54235=CARTESIAN_POINT('Ctrl Pts',(-0.121114856150621,-6.76818656531359,
26.1915206497912));
#54236=CARTESIAN_POINT('Ctrl Pts',(0.0543034891896902,-6.76905092275449,
26.1997308979957));
#54237=CARTESIAN_POINT('Ctrl Pts',(0.229446166549684,-6.76310900818963,
26.2079411462003));
#54238=CARTESIAN_POINT('Ctrl Pts',(0.404630478815592,-6.75716568111322,
26.2161533461445));
#54239=CARTESIAN_POINT('Ctrl Pts',(0.579538636792803,-6.74441287060682,
26.2243655460887));
#54240=CARTESIAN_POINT('Ctrl Pts',(0.753608990122599,-6.72490613243088,
26.2325777460329));
#54241=CARTESIAN_POINT('Ctrl Pts',(0.927751720496305,-6.70539128351109,
26.2407933605433));
#54242=CARTESIAN_POINT('Ctrl Pts',(1.10105559878524,-6.67911695192261,26.2490089750538));
#54243=CARTESIAN_POINT('Ctrl Pts',(1.27296696474913,-6.64619019489041,26.2572245895642));
#54244=CARTESIAN_POINT('Ctrl Pts',(1.4450713796411,-6.61322646255344,26.2654494298496));
#54245=CARTESIAN_POINT('Ctrl Pts',(1.61577980920721,-6.57359545098582,26.2736742701351));
#54246=CARTESIAN_POINT('Ctrl Pts',(1.78455065411568,-6.52745493763805,26.2818991104205));
#54247=CARTESIAN_POINT('Ctrl Pts',(1.95342960261712,-6.48128486968754,26.290129219002));
#54248=CARTESIAN_POINT('Ctrl Pts',(2.1203681538456,-6.42859709499531,26.2983593275835));
#54249=CARTESIAN_POINT('Ctrl Pts',(2.28484266381283,-6.36959833911218,26.3065894361651));
#54250=CARTESIAN_POINT('Ctrl Pts',(2.44954267085703,-6.31051869502943,26.3148308283518));
#54251=CARTESIAN_POINT('Ctrl Pts',(2.61177155981408,-6.24511092010381,26.3230722205384));
#54252=CARTESIAN_POINT('Ctrl Pts',(2.77102742736652,-6.17362907832844,26.3313136127251));
#54253=CARTESIAN_POINT('Ctrl Pts',(2.84033962705722,-6.14251836468543,26.3349004759896));
#54254=CARTESIAN_POINT('Ctrl Pts',(2.90908900729819,-6.11025767345907,26.338487339254));
#54255=CARTESIAN_POINT('Ctrl Pts',(2.97723582829392,-6.07687056162323,26.3420742025185));
#54256=CARTESIAN_POINT('Ctrl Pts',(3.13774879528164,-5.99823058544214,26.3505226973469));
#54257=CARTESIAN_POINT('Ctrl Pts',(3.29528303020821,-5.91315902906587,26.3589711921753));
#54258=CARTESIAN_POINT('Ctrl Pts',(3.44930736484255,-5.82190413033768,26.3674196870038));
#54259=CARTESIAN_POINT('Ctrl Pts',(3.60319100719453,-5.73073258765845,26.375860464623));
#54260=CARTESIAN_POINT('Ctrl Pts',(3.75357085446227,-5.63338913020284,26.3843012422422));
#54261=CARTESIAN_POINT('Ctrl Pts',(3.89993932131773,-5.5301683780912,26.3927420198613));
#54262=CARTESIAN_POINT('Ctrl Pts',(4.04619659740531,-5.42702603900754,26.4011763853307));
#54263=CARTESIAN_POINT('Ctrl Pts',(4.18844829635835,-5.31801549732248,26.4096107508));
#54264=CARTESIAN_POINT('Ctrl Pts',(4.32621454127569,-5.20347544847238,26.4180451162693));
#54265=CARTESIAN_POINT('Ctrl Pts',(4.46389728666329,-5.08900482185426,26.4264743697059));
#54266=CARTESIAN_POINT('Ctrl Pts',(4.59709974245636,-4.96901158256042,26.4349036231425));
#54267=CARTESIAN_POINT('Ctrl Pts',(4.72537363584976,-4.84387582433902,26.4433328765791));
#54268=CARTESIAN_POINT('Ctrl Pts',(4.85358945982906,-4.71879671490227,26.4517583141044));
#54269=CARTESIAN_POINT('Ctrl Pts',(4.97688093208074,-4.5885799610794,26.4601837516296));
#54270=CARTESIAN_POINT('Ctrl Pts',(5.09483501661782,-4.45364403084092,26.4686091891549));
#54271=CARTESIAN_POINT('Ctrl Pts',(5.21276318981455,-4.3187377423976,26.4770327758381));
#54272=CARTESIAN_POINT('Ctrl Pts',(5.32535609176861,-4.17911459354741,26.4854563625213));
#54273=CARTESIAN_POINT('Ctrl Pts',(5.43223917423329,-4.03522819105999,26.4938799492045));
#54274=CARTESIAN_POINT('Ctrl Pts',(5.53911029704153,-3.89135788870647,26.5023025933325));
#54275=CARTESIAN_POINT('Ctrl Pts',(5.64027267527523,-3.7432255513046,26.5107252374605));
#54276=CARTESIAN_POINT('Ctrl Pts',(5.73539333324714,-3.59131623683355,26.5191478815885));
#54277=CARTESIAN_POINT('Ctrl Pts',(5.83051661190702,-3.43940273707907,26.5275707577704));
#54278=CARTESIAN_POINT('Ctrl Pts',(5.91959766182598,-3.28371233556856,26.5359936339524));
#54279=CARTESIAN_POINT('Ctrl Pts',(6.00234777247844,-3.12475762551643,26.5444165101343));
#54280=CARTESIAN_POINT('Ctrl Pts',(6.08511170285861,-2.9657763691456,26.5528407929833));
#54281=CARTESIAN_POINT('Ctrl Pts',(6.16154243263012,-2.80353001331801,26.5612650758323));
#54282=CARTESIAN_POINT('Ctrl Pts',(6.23139783306991,-2.63855453724414,26.5696893586813));
#54283=CARTESIAN_POINT('Ctrl Pts',(6.30130041126432,-2.47346764283354,26.5781193309795));
#54284=CARTESIAN_POINT('Ctrl Pts',(6.36461865641622,-2.30564825247651,26.5865493032777));
#54285=CARTESIAN_POINT('Ctrl Pts',(6.42115873691968,-2.13565200238244,26.5949792755758));
#54286=CARTESIAN_POINT('Ctrl Pts',(6.47771902958934,-1.96559498137276,26.603412261453));
#54287=CARTESIAN_POINT('Ctrl Pts',(6.52749622671926,-1.79335986721838,26.6118452473302));
#54288=CARTESIAN_POINT('Ctrl Pts',(6.57034661664641,-1.61951669862434,26.6202782332074));
#54289=CARTESIAN_POINT('Ctrl Pts',(6.61323642867122,-1.44551359537438,26.6287189773803));
#54290=CARTESIAN_POINT('Ctrl Pts',(6.64918662740134,-1.2698998072055,26.6371597215531));
#54291=CARTESIAN_POINT('Ctrl Pts',(6.67810456598509,-1.09325587387819,26.6456004657259));
#54292=CARTESIAN_POINT('Ctrl Pts',(6.69409406655653,-0.995584725407506,
26.650267578611));
#54293=CARTESIAN_POINT('Ctrl Pts',(6.70793452446345,-0.897598762076486,
26.6549346914961));
#54294=CARTESIAN_POINT('Ctrl Pts',(6.7196170927716,-0.799396726620603,26.6596018043812));
#54295=CARTESIAN_POINT('Ctrl Pts',(6.73999630385679,-0.628091928158219,
26.6677431715991));
#54296=CARTESIAN_POINT('Ctrl Pts',(6.75384653233093,-0.455789002641146,
26.6758845388169));
#54297=CARTESIAN_POINT('Ctrl Pts',(6.7610784939512,-0.283031091278999,26.6840259060347));
#54298=CARTESIAN_POINT('Ctrl Pts',(6.76830414261901,-0.110423984434327,
26.6921601664582));
#54299=CARTESIAN_POINT('Ctrl Pts',(6.76892300890659,0.0626369544499142,
26.7002944268816));
#54300=CARTESIAN_POINT('Ctrl Pts',(6.76289737244261,0.235601633714247,26.708428687305));
#54301=CARTESIAN_POINT('Ctrl Pts',(6.75687584645019,0.408448322721779,26.7165573988298));
#54302=CARTESIAN_POINT('Ctrl Pts',(6.74421885474144,0.581198518511867,26.7246861103546));
#54303=CARTESIAN_POINT('Ctrl Pts',(6.72494071497385,0.753300325293346,26.7328148218794));
#54304=CARTESIAN_POINT('Ctrl Pts',(6.70567176859481,0.925320059903924,26.7409396569719));
#54305=CARTESIAN_POINT('Ctrl Pts',(6.67978800251816,1.09669165823763,26.7490644920644));
#54306=CARTESIAN_POINT('Ctrl Pts',(6.6473557227816,1.26686656550827,26.7571893271568));
#54307=CARTESIAN_POINT('Ctrl Pts',(6.61493252255269,1.43699383183649,26.765311887679));
#54308=CARTESIAN_POINT('Ctrl Pts',(6.5759645294767,1.6059247152823,26.7734344482011));
#54309=CARTESIAN_POINT('Ctrl Pts',(6.53056946604912,1.77311912998167,26.7815570087232));
#54310=CARTESIAN_POINT('Ctrl Pts',(6.48517198999165,1.94032243063054,26.7896800009384));
#54311=CARTESIAN_POINT('Ctrl Pts',(6.43334685333674,2.10578872386958,26.7978029931535));
#54312=CARTESIAN_POINT('Ctrl Pts',(6.37526217773027,2.26899122193144,26.8059259853687));
#54313=CARTESIAN_POINT('Ctrl Pts',(6.34561172093646,2.35230112367231,26.8100725253501));
#54314=CARTESIAN_POINT('Ctrl Pts',(6.31433095963519,2.43502137573639,26.8142190653315));
#54315=CARTESIAN_POINT('Ctrl Pts',(6.28144717792837,2.5170836996206,26.818365605313));
#54316=CARTESIAN_POINT('Ctrl Pts',(6.21020303612765,2.69487528975545,26.8273492643415));
#54317=CARTESIAN_POINT('Ctrl Pts',(6.1314670238083,2.86948952157552,26.8363329233699));
#54318=CARTESIAN_POINT('Ctrl Pts',(6.0455495977747,3.04033206424005,26.8453165823984));
#54319=CARTESIAN_POINT('Ctrl Pts',(5.95948456651342,3.21146811258291,26.8543156752579));
#54320=CARTESIAN_POINT('Ctrl Pts',(5.86621356961772,3.37881930694775,26.8633147681174));
#54321=CARTESIAN_POINT('Ctrl Pts',(5.76609230798076,3.54181711778644,26.8723138609769));
#54322=CARTESIAN_POINT('Ctrl Pts',(5.66573628996394,3.70519711294216,26.8813340541944));
#54323=CARTESIAN_POINT('Ctrl Pts',(5.55849799574921,3.86420309664514,26.8903542474118));
#54324=CARTESIAN_POINT('Ctrl Pts',(5.44477723408637,4.01829439827083,26.8993744406293));
#54325=CARTESIAN_POINT('Ctrl Pts',(5.3309413016762,4.17254175592452,26.9084037690511));
#54326=CARTESIAN_POINT('Ctrl Pts',(5.21060993306272,4.32186429932877,26.9174330974729));
#54327=CARTESIAN_POINT('Ctrl Pts',(5.08422338295535,4.46575431391048,26.9264624258947));
#54328=CARTESIAN_POINT('Ctrl Pts',(4.95765865328782,4.60984718440913,26.9355044838496));
#54329=CARTESIAN_POINT('Ctrl Pts',(4.82502183102855,4.74849203251823,26.9445465418045));
#54330=CARTESIAN_POINT('Ctrl Pts',(4.68679178908261,4.8812162137922,26.9535885997593));
#54331=CARTESIAN_POINT('Ctrl Pts',(4.56683212635577,4.99639774594819,26.9614355352543));
#54332=CARTESIAN_POINT('Ctrl Pts',(4.44266072880168,5.10712081221389,26.9692824707493));
#54333=CARTESIAN_POINT('Ctrl Pts',(4.31461139104306,5.21310056917009,26.9771294062443));
#54334=CARTESIAN_POINT('Ctrl Pts',(4.17338976130643,5.32998234504197,26.9857835472062));
#54335=CARTESIAN_POINT('Ctrl Pts',(4.02732597406175,5.44119673635603,26.9944376881681));
#54336=CARTESIAN_POINT('Ctrl Pts',(3.87689232870796,5.54634968890399,27.0030918291301));
#54337=CARTESIAN_POINT('Ctrl Pts',(3.72662796509449,5.65138431370176,27.0117362316585));
#54338=CARTESIAN_POINT('Ctrl Pts',(3.57200380360275,5.75037093627247,27.020380634187));
#54339=CARTESIAN_POINT('Ctrl Pts',(3.41352374733898,5.84295683933681,27.0290250367155));
#54340=CARTESIAN_POINT('Ctrl Pts',(3.31029752519016,5.90326280604888,27.0346555812571));
#54341=CARTESIAN_POINT('Ctrl Pts',(3.20543607517873,5.96085403431976,27.0402861257987));
#54342=CARTESIAN_POINT('Ctrl Pts',(3.09908550384735,6.01564277861005,27.0459166703402));
#54343=CARTESIAN_POINT('Ctrl Pts',(3.09908550384716,6.01564277861015,25.0456934344376));
#54344=CARTESIAN_POINT('Ctrl Pts',(2.93386957082307,6.10075725795725,25.0544502213138));
#54345=CARTESIAN_POINT('Ctrl Pts',(2.76526825588463,6.17899746639908,25.06320700819));
#54346=CARTESIAN_POINT('Ctrl Pts',(2.59388993472329,6.25012191933415,25.0719637950662));
#54347=CARTESIAN_POINT('Ctrl Pts',(2.43111345179144,6.31767648645075,25.0802810603996));
#54348=CARTESIAN_POINT('Ctrl Pts',(2.26553899905849,6.3789333607424,25.088598325733));
#54349=CARTESIAN_POINT('Ctrl Pts',(2.09768879961298,6.43366075418795,25.0969155910664));
#54350=CARTESIAN_POINT('Ctrl Pts',(1.92998016889498,6.48834198928829,25.1052258414265));
#54351=CARTESIAN_POINT('Ctrl Pts',(1.75999994470735,6.53650460852614,25.1135360917866));
#54352=CARTESIAN_POINT('Ctrl Pts',(1.5882899136827,6.57796504628094,25.1218463421467));
#54353=CARTESIAN_POINT('Ctrl Pts',(1.41669326014494,6.61939810834773,25.1301511053765));
#54354=CARTESIAN_POINT('Ctrl Pts',(1.24336941265814,6.65413772561488,25.1384558686064));
#54355=CARTESIAN_POINT('Ctrl Pts',(1.06887511172934,6.68205020899466,25.1467606318363));
#54356=CARTESIAN_POINT('Ctrl Pts',(0.894464084403035,6.70994937175002,25.1550614317989));
#54357=CARTESIAN_POINT('Ctrl Pts',(0.718884059572879,6.73102783887337,25.1633622317614));
#54358=CARTESIAN_POINT('Ctrl Pts',(0.542701984691165,6.7452030033063,25.171663031724));
#54359=CARTESIAN_POINT('Ctrl Pts',(0.366571748568069,6.75937399692373,25.179961389309));
#54360=CARTESIAN_POINT('Ctrl Pts',(0.189840161791331,6.76664570874752,25.1882597468939));
#54361=CARTESIAN_POINT('Ctrl Pts',(0.0130795383062143,6.7669873596511,25.1965581044788));
#54362=CARTESIAN_POINT('Ctrl Pts',(-0.163699070167067,6.76732904531687,
25.2048573064026));
#54363=CARTESIAN_POINT('Ctrl Pts',(-0.340506373458073,6.76073925297585,
25.2131565083264));
#54364=CARTESIAN_POINT('Ctrl Pts',(-0.516769214631858,6.747239330186,25.2214557102502));
#54365=CARTESIAN_POINT('Ctrl Pts',(-0.693049925516606,6.73373803875987,
25.2297557535557));
#54366=CARTESIAN_POINT('Ctrl Pts',(-0.868785717218181,6.7133252465697,25.2380557968612));
#54367=CARTESIAN_POINT('Ctrl Pts',(-1.04340780343969,6.68607427087982,25.2463558401668));
#54368=CARTESIAN_POINT('Ctrl Pts',(-1.21807658067824,6.65881600873611,25.2546581027647));
#54369=CARTESIAN_POINT('Ctrl Pts',(-1.39163071514237,6.62471597252829,25.2629603653626));
#54370=CARTESIAN_POINT('Ctrl Pts',(-1.5635106793521,6.58389879596823,25.2712626279605));
#54371=CARTESIAN_POINT('Ctrl Pts',(-1.73546513725157,6.54306392902698,25.2795684888031));
#54372=CARTESIAN_POINT('Ctrl Pts',(-1.90574364050117,6.4955061999138,25.2878743496458));
#54373=CARTESIAN_POINT('Ctrl Pts',(-2.07380072200634,6.44140043510773,25.2961802104884));
#54374=CARTESIAN_POINT('Ctrl Pts',(-2.24205645883823,6.3872307134705,25.3044958894446));
#54375=CARTESIAN_POINT('Ctrl Pts',(-2.40808519599487,6.32649759811053,25.3128115684007));
#54376=CARTESIAN_POINT('Ctrl Pts',(-2.57135928194027,6.25942492911127,25.3211272473568));
#54377=CARTESIAN_POINT('Ctrl Pts',(-2.73473663744468,6.19230983718304,25.3294481859136));
#54378=CARTESIAN_POINT('Ctrl Pts',(-2.8953555512352,6.11884733970848,25.3377691244705));
#54379=CARTESIAN_POINT('Ctrl Pts',(-3.05271185063397,6.03930785413353,25.3460900630273));
#54380=CARTESIAN_POINT('Ctrl Pts',(-3.21030203023437,5.95965014824586,25.3544233690762));
#54381=CARTESIAN_POINT('Ctrl Pts',(-3.36461960048107,5.8738975724953,25.3627566751251));
#54382=CARTESIAN_POINT('Ctrl Pts',(-3.51518715403526,5.78236528352417,25.3710899811741));
#54383=CARTESIAN_POINT('Ctrl Pts',(-3.62601376298369,5.71499211476036,25.3772237864258));
#54384=CARTESIAN_POINT('Ctrl Pts',(-3.73480926329466,5.64448851718007,25.3833575916775));
#54385=CARTESIAN_POINT('Ctrl Pts',(-3.84139462256851,5.5709941979598,25.3894913969293));
#54386=CARTESIAN_POINT('Ctrl Pts',(-3.9809256705174,5.47478267839503,25.3975211702539));
#54387=CARTESIAN_POINT('Ctrl Pts',(-4.11710711489268,5.37314122535884,25.4055509435785));
#54388=CARTESIAN_POINT('Ctrl Pts',(-4.24947299795826,5.26633347212495,25.413580716903));
#54389=CARTESIAN_POINT('Ctrl Pts',(-4.38167304827217,5.15965953149601,25.421600430238));
#54390=CARTESIAN_POINT('Ctrl Pts',(-4.51006675783186,5.04783240040823,25.4296201435731));
#54391=CARTESIAN_POINT('Ctrl Pts',(-4.63421478721721,4.93116034072482,25.437639856908));
#54392=CARTESIAN_POINT('Ctrl Pts',(-4.75823499883584,4.8146084018535,25.4456513134721));
#54393=CARTESIAN_POINT('Ctrl Pts',(-4.87801795547243,4.69322171487695,25.453662770036));
#54394=CARTESIAN_POINT('Ctrl Pts',(-4.99315535615592,4.5673502809935,25.4616742266001));
#54395=CARTESIAN_POINT('Ctrl Pts',(-5.10819986744137,4.4415803964038,25.4696792197614));
#54396=CARTESIAN_POINT('Ctrl Pts',(-5.21860602822786,4.31133324155964,25.4776842129228));
#54397=CARTESIAN_POINT('Ctrl Pts',(-5.32400067600738,4.17699722311051,25.4856892060842));
#54398=CARTESIAN_POINT('Ctrl Pts',(-5.42933373903935,4.04273970058085,25.4936895217264));
#54399=CARTESIAN_POINT('Ctrl Pts',(-5.5296608857929,3.9043983655855,25.5016898373686));
#54400=CARTESIAN_POINT('Ctrl Pts',(-5.62464782667414,3.7623962877254,25.5096901530109));
#54401=CARTESIAN_POINT('Ctrl Pts',(-5.71961342979113,3.62042610905937,25.5176886714708));
#54402=CARTESIAN_POINT('Ctrl Pts',(-5.80924099902817,3.47479713290247,25.5256871899307));
#54403=CARTESIAN_POINT('Ctrl Pts',(-5.89323832783158,3.32596317047812,25.5336857083907));
#54404=CARTESIAN_POINT('Ctrl Pts',(-5.97722837469604,3.17714211084298,25.541683533439));
#54405=CARTESIAN_POINT('Ctrl Pts',(-6.0555889660689,3.02511694561341,25.5496813584873));
#54406=CARTESIAN_POINT('Ctrl Pts',(-6.12807296701681,2.870367696118,25.5576791835357));
#54407=CARTESIAN_POINT('Ctrl Pts',(-6.20056526889467,2.71560072460584,25.5656779245018));
#54408=CARTESIAN_POINT('Ctrl Pts',(-6.26717948091634,2.55810938944274,25.5736766654679));
#54409=CARTESIAN_POINT('Ctrl Pts',(-6.32771598043466,2.39839518656785,25.581675406434));
#54410=CARTESIAN_POINT('Ctrl Pts',(-6.38827159765289,2.2386305452265,25.5896766734386));
#54411=CARTESIAN_POINT('Ctrl Pts',(-6.44274554949837,2.07664199166433,25.5976779404432));
#54412=CARTESIAN_POINT('Ctrl Pts',(-6.49098765538635,1.91294753133014,25.6056792074478));
#54413=CARTESIAN_POINT('Ctrl Pts',(-6.53928378200302,1.74906976859098,25.6136894341417));
#54414=CARTESIAN_POINT('Ctrl Pts',(-6.58133402071878,1.58348264631413,25.6216996608354));
#54415=CARTESIAN_POINT('Ctrl Pts',(-6.61703886627128,1.41671650031164,25.6297098875292));
#54416=CARTESIAN_POINT('Ctrl Pts',(-6.65276478283154,1.2498519382342,25.6377248414119));
#54417=CARTESIAN_POINT('Ctrl Pts',(-6.68213778570095,1.08180733729416,25.6457397952946));
#54418=CARTESIAN_POINT('Ctrl Pts',(-6.70511019851716,0.91311895486905,25.6537547491773));
#54419=CARTESIAN_POINT('Ctrl Pts',(-6.7281183001261,0.744168506601595,25.6617821546918));
#54420=CARTESIAN_POINT('Ctrl Pts',(-6.74470591615529,0.574572653351214,
25.6698095602064));
#54421=CARTESIAN_POINT('Ctrl Pts',(-6.75487747544724,0.404869474887251,
25.677836965721));
#54422=CARTESIAN_POINT('Ctrl Pts',(-6.76304726415453,0.268564010679525,
25.6842845717408));
#54423=CARTESIAN_POINT('Ctrl Pts',(-6.76707888580151,0.132189369752193,
25.6907321777606));
#54424=CARTESIAN_POINT('Ctrl Pts',(-6.76699883050778,-0.00397843013914469,
25.6971797837804));
#54425=CARTESIAN_POINT('',(-6.76699952998211,-0.00142798523079344,25.3028202161898));
#54426=CARTESIAN_POINT('Ctrl Pts',(3.09908550384736,6.01564277861004,24.6513967904261));
#54427=CARTESIAN_POINT('Ctrl Pts',(2.93373232018338,6.10082796552476,24.6601462383254));
#54428=CARTESIAN_POINT('Ctrl Pts',(2.76486502144429,6.1791915818019,24.6688956862247));
#54429=CARTESIAN_POINT('Ctrl Pts',(2.59305716434347,6.25046746591381,24.677645134124));
#54430=CARTESIAN_POINT('Ctrl Pts',(2.42125069459276,6.32174277447227,24.6863945113714));
#54431=CARTESIAN_POINT('Ctrl Pts',(2.2465039787105,6.38593035557829,24.6951438886188));
#54432=CARTESIAN_POINT('Ctrl Pts',(2.06941053323761,6.44281220003542,24.7038932658662));
#54433=CARTESIAN_POINT('Ctrl Pts',(1.89231845896684,6.49969360406685,24.7126425753688));
#54434=CARTESIAN_POINT('Ctrl Pts',(1.71287996431518,6.54926929700877,24.7213918848714));
#54435=CARTESIAN_POINT('Ctrl Pts',(1.53170449173529,6.59137090065473,24.730141194374));
#54436=CARTESIAN_POINT('Ctrl Pts',(1.35053036178195,6.63347219230078,24.7388904390386));
#54437=CARTESIAN_POINT('Ctrl Pts',(1.16761955878869,6.6680994406245,24.7476396837032));
#54438=CARTESIAN_POINT('Ctrl Pts',(0.983593309310725,6.69513503985388,24.7563889283678));
#54439=CARTESIAN_POINT('Ctrl Pts',(0.799568362460165,6.72217044771212,24.7651381111009));
#54440=CARTESIAN_POINT('Ctrl Pts',(0.614428268438725,6.74161427235976,24.7738872938341));
#54441=CARTESIAN_POINT('Ctrl Pts',(0.428801816330343,6.75340047696802,24.7826364765673));
#54442=CARTESIAN_POINT('Ctrl Pts',(0.243176616522904,6.76518660206241,24.7913856002754));
#54443=CARTESIAN_POINT('Ctrl Pts',(0.057065351165626,6.76931519233997,24.8001347239836));
#54444=CARTESIAN_POINT('Ctrl Pts',(-0.128899900799819,6.76577222610796,
24.8088838476917));
#54445=CARTESIAN_POINT('Ctrl Pts',(-0.314863959941826,6.76222928260134,
24.817632915281));
#54446=CARTESIAN_POINT('Ctrl Pts',(-0.500681721080501,6.75101488651278,
24.8263819828702));
#54447=CARTESIAN_POINT('Ctrl Pts',(-0.685722110173135,6.73216712415993,
24.8351310504595));
#54448=CARTESIAN_POINT('Ctrl Pts',(-0.870761373827479,6.71331947644147,
24.8438800648359));
#54449=CARTESIAN_POINT('Ctrl Pts',(-1.05502298984333,6.68683858439998,24.8526290792122));
#54450=CARTESIAN_POINT('Ctrl Pts',(-1.23788117676052,6.65281438131427,24.8613780935886));
#54451=CARTESIAN_POINT('Ctrl Pts',(-1.4300964145179,6.61704912302378,24.8705748044761));
#54452=CARTESIAN_POINT('Ctrl Pts',(-1.62076048992696,6.57294837083165,24.8797715153636));
#54453=CARTESIAN_POINT('Ctrl Pts',(-1.80915798961136,6.52067760042048,24.8889682262512));
#54454=CARTESIAN_POINT('Ctrl Pts',(-1.98840443003007,6.4709457857741,24.8977182239577));
#54455=CARTESIAN_POINT('Ctrl Pts',(-2.16559895952177,6.4138188847448,24.9064682216642));
#54456=CARTESIAN_POINT('Ctrl Pts',(-2.34013966242298,6.34949095285243,24.9152182193707));
#54457=CARTESIAN_POINT('Ctrl Pts',(-2.5146768255398,6.28516432556698,24.9239680396222));
#54458=CARTESIAN_POINT('Ctrl Pts',(-2.68656000078796,6.21363705879681,24.9327178598738));
#54459=CARTESIAN_POINT('Ctrl Pts',(-2.85520533840832,6.13515211510886,24.9414676801254));
#54460=CARTESIAN_POINT('Ctrl Pts',(-3.02384747998256,6.05666865881156,24.9502173345567));
#54461=CARTESIAN_POINT('Ctrl Pts',(-3.18925164684452,5.97122791039889,24.9589669889879));
#54462=CARTESIAN_POINT('Ctrl Pts',(-3.35085601829059,5.87912008251964,24.9677166434192));
#54463=CARTESIAN_POINT('Ctrl Pts',(-3.51245754191326,5.7870138777823,24.9764661436623));
#54464=CARTESIAN_POINT('Ctrl Pts',(-3.67025915510851,5.68824097061038,24.9852156439054));
#54465=CARTESIAN_POINT('Ctrl Pts',(-3.82372487928755,5.58313684656909,24.9939651441486));
#54466=CARTESIAN_POINT('Ctrl Pts',(-3.9771881030072,5.4780344350183,25.0027145018337));
#54467=CARTESIAN_POINT('Ctrl Pts',(-4.12631534262948,5.36660117496436,25.0114638595188));
#54468=CARTESIAN_POINT('Ctrl Pts',(-4.27060009886148,5.24921554097413,25.0202132172039));
#54469=CARTESIAN_POINT('Ctrl Pts',(-4.41488269594138,5.13183166360356,25.0289624439591));
#54470=CARTESIAN_POINT('Ctrl Pts',(-4.55432273235015,5.00849577139537,25.0377116707143));
#54471=CARTESIAN_POINT('Ctrl Pts',(-4.68844662480136,4.87962675277411,25.0464608974695));
#54472=CARTESIAN_POINT('Ctrl Pts',(-4.82256868835098,4.75075949139943,25.055210004921));
#54473=CARTESIAN_POINT('Ctrl Pts',(-4.95137454637813,4.61635945312579,25.0639591123725));
#54474=CARTESIAN_POINT('Ctrl Pts',(-5.07442674461039,4.47688309134635,25.072708219824));
#54475=CARTESIAN_POINT('Ctrl Pts',(-5.19747742838508,4.33740844616389,25.0814572195963));
#54476=CARTESIAN_POINT('Ctrl Pts',(-5.31477440450904,4.19285781736059,25.0902062193687));
#54477=CARTESIAN_POINT('Ctrl Pts',(-5.42591931531137,4.04372211999428,25.0989552191411));
#54478=CARTESIAN_POINT('Ctrl Pts',(-5.53707636462969,3.89457013500819,25.1077051744217));
#54479=CARTESIAN_POINT('Ctrl Pts',(-5.64207983273461,3.74083230916434,25.1164551297023));
#54480=CARTESIAN_POINT('Ctrl Pts',(-5.74057303468741,3.58303087251837,25.1252050849828));
#54481=CARTESIAN_POINT('Ctrl Pts',(-5.83906243363764,3.42523552887433,25.1339547024116));
#54482=CARTESIAN_POINT('Ctrl Pts',(-5.93104191768429,3.26337713156987,25.1427043198404));
#54483=CARTESIAN_POINT('Ctrl Pts',(-6.01619906699663,3.09800545291142,25.1514539372693));
#54484=CARTESIAN_POINT('Ctrl Pts',(-6.1013533809538,2.932639280396,25.1602032633746));
#54485=CARTESIAN_POINT('Ctrl Pts',(-6.17968568352828,2.76376031540248,25.16895258948));
#54486=CARTESIAN_POINT('Ctrl Pts',(-6.25092992694868,2.59194213831585,25.1777019155854));
#54487=CARTESIAN_POINT('Ctrl Pts',(-6.32217217691085,2.42012876880867,25.1864509968792));
#54488=CARTESIAN_POINT('Ctrl Pts',(-6.38632665483832,2.24537661647722,25.195200078173));
#54489=CARTESIAN_POINT('Ctrl Pts',(-6.44317547869332,2.06827917621512,25.2039491594668));
#54490=CARTESIAN_POINT('Ctrl Pts',(-6.50002944235916,1.89116572423491,25.2126990317818));
#54491=CARTESIAN_POINT('Ctrl Pts',(-6.54957634250377,1.71170683289277,25.2214489040967));
#54492=CARTESIAN_POINT('Ctrl Pts',(-6.59164787708374,1.53051209225456,25.2301987764117));
#54493=CARTESIAN_POINT('Ctrl Pts',(-6.63371649074992,1.34932993148116,25.2389480412465));
#54494=CARTESIAN_POINT('Ctrl Pts',(-6.6683107125711,1.16641244174083,25.2476973060813));
#54495=CARTESIAN_POINT('Ctrl Pts',(-6.69531304840322,0.982380875160746,
25.2564465709161));
#54496=CARTESIAN_POINT('Ctrl Pts',(-6.72231677033035,0.798339861796578,
25.2651962848717));
#54497=CARTESIAN_POINT('Ctrl Pts',(-6.74172778477883,0.613184940730891,
25.2739459988274));
#54498=CARTESIAN_POINT('Ctrl Pts',(-6.75348015835513,0.427545027691289,
25.282695712783));
#54499=CARTESIAN_POINT('Ctrl Pts',(-6.76249038365212,0.285219953548558,
25.2894038805853));
#54500=CARTESIAN_POINT('Ctrl Pts',(-6.76699999999992,0.142609995760042,
25.2961120483875));
#54501=CARTESIAN_POINT('Ctrl Pts',(-6.767,3.65565930388384E-12,25.3028202161898));
#54502=CARTESIAN_POINT('Ctrl Pts',(-6.7669985337519,-0.00445468289831136,
25.3028202161898));
#54503=CARTESIAN_POINT('Ctrl Pts',(-6.76686772084466,-0.203169332550661,
25.3121622732703));
#54504=CARTESIAN_POINT('Ctrl Pts',(-6.75797960988083,-0.401695375614664,
25.3215043303508));
#54505=CARTESIAN_POINT('Ctrl Pts',(-6.74040959930496,-0.599305793061871,
25.3308463874314));
#54506=CARTESIAN_POINT('Ctrl Pts',(-6.722962658811,-0.795532037736014,25.3401230075718));
#54507=CARTESIAN_POINT('Ctrl Pts',(-6.69695515512968,-0.990855271405463,
25.3493996277122));
#54508=CARTESIAN_POINT('Ctrl Pts',(-6.66251242258052,-1.18457469961173,
25.3586762478526));
#54509=CARTESIAN_POINT('Ctrl Pts',(-6.6277052533626,-1.38034386248957,25.3680510234032));
#54510=CARTESIAN_POINT('Ctrl Pts',(-6.58428339171561,-1.57447489642017,
25.3774257989537));
#54511=CARTESIAN_POINT('Ctrl Pts',(-6.53242827667237,-1.76625870419121,
25.3868005745043));
#54512=CARTESIAN_POINT('Ctrl Pts',(-6.4805731616291,-1.95804251196238,25.3961753500549));
#54513=CARTESIAN_POINT('Ctrl Pts',(-6.42028487035499,-2.14747891495456,
25.4055501256055));
#54514=CARTESIAN_POINT('Ctrl Pts',(-6.3517960376486,-2.33387576706891,25.4149249011561));
#54515=CARTESIAN_POINT('Ctrl Pts',(-6.28857685275979,-2.5059309268791,25.4235783654568));
#54516=CARTESIAN_POINT('Ctrl Pts',(-6.21832248720098,-2.67552548039541,
25.4322318297576));
#54517=CARTESIAN_POINT('Ctrl Pts',(-6.1412427471693,-2.84208137116805,25.4408852940583));
#54518=CARTESIAN_POINT('Ctrl Pts',(-6.06423401334421,-3.00848382989767,
25.4495307867484));
#54519=CARTESIAN_POINT('Ctrl Pts',(-5.98041257299404,-3.1718529340812,25.4581762794385));
#54520=CARTESIAN_POINT('Ctrl Pts',(-5.89003649211402,-3.33163009975075,
25.4668217721287));
#54521=CARTESIAN_POINT('Ctrl Pts',(-5.796941601983,-3.49621388717122,25.4757273496253));
#54522=CARTESIAN_POINT('Ctrl Pts',(-5.6968916447697,-3.65698593828745,25.4846329271219));
#54523=CARTESIAN_POINT('Ctrl Pts',(-5.59022108859942,-3.81336035283559,
25.4935385046184));
#54524=CARTESIAN_POINT('Ctrl Pts',(-5.48686230754852,-3.96487984851949,
25.5021675927909));
#54525=CARTESIAN_POINT('Ctrl Pts',(-5.3772880352706,-4.11227039426033,25.5107966809634));
#54526=CARTESIAN_POINT('Ctrl Pts',(-5.26184817134888,-4.25502559588923,
25.5194257691359));
#54527=CARTESIAN_POINT('Ctrl Pts',(-5.14085999989243,-4.40464194352013,
25.5284695912945));
#54528=CARTESIAN_POINT('Ctrl Pts',(-5.01342867388619,-4.54916609599658,
25.5375134134532));
#54529=CARTESIAN_POINT('Ctrl Pts',(-4.88000714049934,-4.68805069391058,
25.5465572356118));
#54530=CARTESIAN_POINT('Ctrl Pts',(-4.74658560711241,-4.82693529182466,
25.5556010577705));
#54531=CARTESIAN_POINT('Ctrl Pts',(-4.6071741083085,-4.96018003330942,25.5646448799291));
#54532=CARTESIAN_POINT('Ctrl Pts',(-4.46227354144581,-5.08727862823658,
25.5736887020878));
#54533=CARTESIAN_POINT('Ctrl Pts',(-4.32727511886633,-5.20569162135824,
25.5821144919376));
#54534=CARTESIAN_POINT('Ctrl Pts',(-4.1875714748537,-5.31871809721675,25.5905402817875));
#54535=CARTESIAN_POINT('Ctrl Pts',(-4.04362535160469,-5.42599143160583,
25.5989660716373));
#54536=CARTESIAN_POINT('Ctrl Pts',(-3.8996458280128,-5.53328965701711,25.6073938165538));
#54537=CARTESIAN_POINT('Ctrl Pts',(-3.75142212824965,-5.63483188122655,
25.6158215614703));
#54538=CARTESIAN_POINT('Ctrl Pts',(-3.59944737237399,-5.73029385053768,
25.6242493063868));
#54539=CARTESIAN_POINT('Ctrl Pts',(-3.44741677340041,-5.82579089733304,
25.6326801480768));
#54540=CARTESIAN_POINT('Ctrl Pts',(-3.29163265064257,-5.91520305821385,
25.6411109897667));
#54541=CARTESIAN_POINT('Ctrl Pts',(-3.13261452676403,-5.99825101397957,
25.6495418314567));
#54542=CARTESIAN_POINT('Ctrl Pts',(-2.97345028552638,-6.08137528021658,
25.657980420014));
#54543=CARTESIAN_POINT('Ctrl Pts',(-2.81104640017321,-6.15812350423278,
25.6664190085714));
#54544=CARTESIAN_POINT('Ctrl Pts',(-2.64594528120833,-6.22826320645261,
25.6748575971288));
#54545=CARTESIAN_POINT('Ctrl Pts',(-2.48075759051284,-6.29843968683267,
25.683300610509));
#54546=CARTESIAN_POINT('Ctrl Pts',(-2.31287015332307,-6.36200061214593,
25.6917436238893));
#54547=CARTESIAN_POINT('Ctrl Pts',(-2.14284304546279,-6.41876255071893,
25.7001866372696));
#54548=CARTESIAN_POINT('Ctrl Pts',(-1.97263731227475,-6.47558412166472,
25.7086385206239));
#54549=CARTESIAN_POINT('Ctrl Pts',(-1.80028773467195,-6.5255923401309,25.7170904039782));
#54550=CARTESIAN_POINT('Ctrl Pts',(-1.62636818537994,-6.56865401171229,
25.7255422873325));
#54551=CARTESIAN_POINT('Ctrl Pts',(-1.5789696136712,-6.58038967763747,25.7278456925614));
#54552=CARTESIAN_POINT('Ctrl Pts',(-1.53145448793498,-6.59160969352032,
25.7301490977903));
#54553=CARTESIAN_POINT('Ctrl Pts',(-1.48383452985272,-6.60231202595097,
25.7324525030192));
#54554=CARTESIAN_POINT('Ctrl Pts',(-1.31188570314621,-6.64095661067097,
25.7407697683526));
#54555=CARTESIAN_POINT('Ctrl Pts',(-1.13826014071322,-6.67291702549273,
25.749087033686));
#54556=CARTESIAN_POINT('Ctrl Pts',(-0.963512074390253,-6.69805445502679,
25.7574042990194));
#54557=CARTESIAN_POINT('Ctrl Pts',(-0.788911394614725,-6.72317068307331,
25.7657145493795));
#54558=CARTESIAN_POINT('Ctrl Pts',(-0.613190439782572,-6.74147534203104,
25.7740247997395));
#54559=CARTESIAN_POINT('Ctrl Pts',(-0.436914447371334,-6.75288047914949,
25.7823350500996));
#54560=CARTESIAN_POINT('Ctrl Pts',(-0.260754847280388,-6.76427808563172,
25.7906398133295));
#54561=CARTESIAN_POINT('Ctrl Pts',(-0.0840412858169509,-6.76878522558246,
25.7989445765594));
#54562=CARTESIAN_POINT('Ctrl Pts',(0.0926548189229739,-6.76636564815488,
25.8072493397893));
#54563=CARTESIAN_POINT('Ctrl Pts',(0.269266599297139,-6.76394722541789,
25.8155501397518));
#54564=CARTESIAN_POINT('Ctrl Pts',(0.445860592470569,-6.75460867784938,
25.8238509397144));
#54565=CARTESIAN_POINT('Ctrl Pts',(0.621864083055294,-6.73836583024444,
25.832151739677));
#54566=CARTESIAN_POINT('Ctrl Pts',(0.797815787426847,-6.72212776183772,
25.8404500972619));
#54567=CARTESIAN_POINT('Ctrl Pts',(0.973176989590091,-6.69898947466501,
25.8487484548469));
#54568=CARTESIAN_POINT('Ctrl Pts',(1.14737857352802,-6.6690187740783,25.8570468124318));
#54569=CARTESIAN_POINT('Ctrl Pts',(1.32159788207783,-6.6390450240415,25.8653460143556));
#54570=CARTESIAN_POINT('Ctrl Pts',(1.49465699260167,-6.60223752310994,25.8736452162794));
#54571=CARTESIAN_POINT('Ctrl Pts',(1.66599489619299,-6.5587155759233,25.8819444182031));
#54572=CARTESIAN_POINT('Ctrl Pts',(1.83735017019983,-6.51518921643622,25.8902444615087));
#54573=CARTESIAN_POINT('Ctrl Pts',(2.00698355202321,-6.46494713903994,25.8985445048142));
#54574=CARTESIAN_POINT('Ctrl Pts',(2.17434724937158,-6.40815909908222,25.9068445481197));
#54575=CARTESIAN_POINT('Ctrl Pts',(2.34175569696578,-6.35135587495501,25.9151468107177));
#54576=CARTESIAN_POINT('Ctrl Pts',(2.50689292103439,-6.28800331158205,25.9234490733155));
#54577=CARTESIAN_POINT('Ctrl Pts',(2.66922904968405,-6.21832013330954,25.9317513359135));
#54578=CARTESIAN_POINT('Ctrl Pts',(2.83163553567381,-6.14860675397758,25.9400571967561));
#54579=CARTESIAN_POINT('Ctrl Pts',(2.99123818721352,-6.0725574286115,25.9483630575987));
#54580=CARTESIAN_POINT('Ctrl Pts',(3.14752959060519,-5.99043792024129,25.9566689184413));
#54581=CARTESIAN_POINT('Ctrl Pts',(3.30400574146244,-5.90822134081843,25.9649845973974));
#54582=CARTESIAN_POINT('Ctrl Pts',(3.45716251556301,-5.81992040418544,25.9733002763535));
#54583=CARTESIAN_POINT('Ctrl Pts',(3.60651845478899,-5.72584610649522,25.9816159553096));
#54584=CARTESIAN_POINT('Ctrl Pts',(3.75596886045715,-5.63171230756086,25.9899368938665));
#54585=CARTESIAN_POINT('Ctrl Pts',(3.90161335059677,-5.53179806185756,25.9982578324233));
#54586=CARTESIAN_POINT('Ctrl Pts',(4.04300158438589,-5.42645622747048,26.0065787709802));
#54587=CARTESIAN_POINT('Ctrl Pts',(4.18459996488499,-5.3209578224882,26.0149120770291));
#54588=CARTESIAN_POINT('Ctrl Pts',(4.32192917608692,-5.2100159255991,26.023245383078));
#54589=CARTESIAN_POINT('Ctrl Pts',(4.45457291710652,-5.09402288237706,26.031578689127));
#54590=CARTESIAN_POINT('Ctrl Pts',(4.55220654180502,-5.00864515431748,26.0377124943787));
#54591=CARTESIAN_POINT('Ctrl Pts',(4.647302394389,-4.92053160836058,26.0438462996305));
#54592=CARTESIAN_POINT('Ctrl Pts',(4.73970804784577,-4.82985057959209,26.0499801048822));
#54593=CARTESIAN_POINT('Ctrl Pts',(4.86130372692857,-4.71052431696045,26.0580515181242));
#54594=CARTESIAN_POINT('Ctrl Pts',(4.97861389964261,-4.58638355881354,26.0661229313663));
#54595=CARTESIAN_POINT('Ctrl Pts',(5.09122289490461,-4.45777281098972,26.0741943446083));
#54596=CARTESIAN_POINT('Ctrl Pts',(5.20369051890032,-4.32932352330712,26.0822556248595));
#54597=CARTESIAN_POINT('Ctrl Pts',(5.31146846621601,-4.196415688837,26.0903169051108));
#54598=CARTESIAN_POINT('Ctrl Pts',(5.41417512671915,-4.05943305120502,26.098378185362));
#54599=CARTESIAN_POINT('Ctrl Pts',(5.51677537156268,-3.92259234300262,26.1064311132196));
#54600=CARTESIAN_POINT('Ctrl Pts',(5.61431456421166,-3.78168552932459,26.1144840410772));
#54601=CARTESIAN_POINT('Ctrl Pts',(5.70644896334461,-3.63713200595514,26.1225369689349));
#54602=CARTESIAN_POINT('Ctrl Pts',(5.79850807618911,-3.49269660240151,26.1305833164592));
#54603=CARTESIAN_POINT('Ctrl Pts',(5.88517098631676,-3.34462073299806,26.1386296639837));
#54604=CARTESIAN_POINT('Ctrl Pts',(5.96613524311391,-3.19335548614214,26.146676011508));
#54605=CARTESIAN_POINT('Ctrl Pts',(6.04705105193752,-3.04218075447116,26.1547175442012));
#54606=CARTESIAN_POINT('Ctrl Pts',(6.12227482020028,-2.88782077258248,26.1627590768943));
#54607=CARTESIAN_POINT('Ctrl Pts',(6.19154838686063,-2.73075403014691,26.1708006095875));
#54608=CARTESIAN_POINT('Ctrl Pts',(6.26215371965539,-2.57066772081876,26.1789967386357));
#54609=CARTESIAN_POINT('Ctrl Pts',(6.32657752879682,-2.40776985285506,26.187192867684));
#54610=CARTESIAN_POINT('Ctrl Pts',(6.38459630624366,-2.24259202850179,26.1953889967322));
#54611=CARTESIAN_POINT('Ctrl Pts',(6.4415010769077,-2.08058575006514,26.2034277535683));
#54612=CARTESIAN_POINT('Ctrl Pts',(6.49224444280832,-1.91638664810777,26.2114665104044));
#54613=CARTESIAN_POINT('Ctrl Pts',(6.53666485547006,-1.75051465782568,26.2195052672405));
#54614=CARTESIAN_POINT('Ctrl Pts',(6.58108956755827,-1.58462661288805,26.2275448021433));
#54615=CARTESIAN_POINT('Ctrl Pts',(6.61919001109639,-1.41706571796878,26.2355843370461));
#54616=CARTESIAN_POINT('Ctrl Pts',(6.65085514182505,-1.24836488354137,26.2436238719489));
#54617=CARTESIAN_POINT('Ctrl Pts',(6.68252960711064,-1.07961431783208,26.2516657768245));
#54618=CARTESIAN_POINT('Ctrl Pts',(6.70776491467035,-0.909723510592241,
26.2597076817));
#54619=CARTESIAN_POINT('Ctrl Pts',(6.72650156553943,-0.739233176200573,
26.2677495865755));
#54620=CARTESIAN_POINT('Ctrl Pts',(6.74587024640452,-0.562991813724064,
26.2760627632563));
#54621=CARTESIAN_POINT('Ctrl Pts',(6.75829412475733,-0.38611020372354,26.2843759399371));
#54622=CARTESIAN_POINT('Ctrl Pts',(6.76376593097555,-0.209187549759847,
26.2926891166179));
#54623=CARTESIAN_POINT('Ctrl Pts',(6.7690683740941,-0.0377409978145964,
26.3007449842285));
#54624=CARTESIAN_POINT('Ctrl Pts',(6.76784276946827,0.133743727256565,26.308800851839));
#54625=CARTESIAN_POINT('Ctrl Pts',(6.76013545925107,0.30472540520346,26.3168567194496));
#54626=CARTESIAN_POINT('Ctrl Pts',(6.75205888511553,0.483898963661559,26.3252985506655));
#54627=CARTESIAN_POINT('Ctrl Pts',(6.73686427849205,0.662519602094777,26.3337403818815));
#54628=CARTESIAN_POINT('Ctrl Pts',(6.71466525655449,0.839975887999223,26.3421822130974));
#54629=CARTESIAN_POINT('Ctrl Pts',(6.69246623461694,1.01743217390354,26.3506240443134));
#54630=CARTESIAN_POINT('Ctrl Pts',(6.66326295715326,1.19372366636151,26.3590658755293));
#54631=CARTESIAN_POINT('Ctrl Pts',(6.62722876856082,1.3682572306258,26.3675077067453));
#54632=CARTESIAN_POINT('Ctrl Pts',(6.59209409591994,1.53843394015663,26.3757388058167));
#54633=CARTESIAN_POINT('Ctrl Pts',(6.55034898385465,1.70750556831118,26.3839699048881));
#54634=CARTESIAN_POINT('Ctrl Pts',(6.50207382812475,1.87491998058988,26.3922010039595));
#54635=CARTESIAN_POINT('Ctrl Pts',(6.45385670486078,2.04213314087821,26.400422208273));
#54636=CARTESIAN_POINT('Ctrl Pts',(6.39912526794902,2.20769271110237,26.4086434125866));
#54637=CARTESIAN_POINT('Ctrl Pts',(6.33801114870739,2.37105539346107,26.4168646169001));
#54638=CARTESIAN_POINT('Ctrl Pts',(6.27695823368949,2.53425447228129,26.4250775878883));
#54639=CARTESIAN_POINT('Ctrl Pts',(6.20953549166139,2.69526071143631,26.4332905588765));
#54640=CARTESIAN_POINT('Ctrl Pts',(6.13592473550519,2.85354457477284,26.4415035298647));
#54641=CARTESIAN_POINT('Ctrl Pts',(6.06237293462631,3.01170166765429,26.4497099230373));
#54642=CARTESIAN_POINT('Ctrl Pts',(5.98264314217222,3.16714040415081,26.4579163162098));
#54643=CARTESIAN_POINT('Ctrl Pts',(5.89696581801861,3.31934980698331,26.4661227093823));
#54644=CARTESIAN_POINT('Ctrl Pts',(5.81134215802297,3.47146387316146,26.4743239624646));
#54645=CARTESIAN_POINT('Ctrl Pts',(5.71977856480075,3.62035232456767,26.482525215547));
#54646=CARTESIAN_POINT('Ctrl Pts',(5.62255212312826,3.76552740299495,26.4907264686293));
#54647=CARTESIAN_POINT('Ctrl Pts',(5.52535826973602,3.91065382175661,26.4989249728222));
#54648=CARTESIAN_POINT('Ctrl Pts',(5.42250554695334,4.05206904863729,26.5071234770151));
#54649=CARTESIAN_POINT('Ctrl Pts',(5.31431530047584,4.18931281800827,26.515321981208));
#54650=CARTESIAN_POINT('Ctrl Pts',(5.20614166420548,4.32653551664957,26.5235192267028));
#54651=CARTESIAN_POINT('Ctrl Pts',(5.09263235859772,4.45958775218417,26.5317164721977));
#54652=CARTESIAN_POINT('Ctrl Pts',(4.97415012139717,4.58804092939508,26.5399137176925));
#54653=CARTESIAN_POINT('Ctrl Pts',(4.85566455259991,4.71649771857513,26.5481111936853));
#54654=CARTESIAN_POINT('Ctrl Pts',(4.73220601761551,4.84035492916575,26.5563086696782));
#54655=CARTESIAN_POINT('Ctrl Pts',(4.60417537458037,4.95921950715107,26.564506145671));
#54656=CARTESIAN_POINT('Ctrl Pts',(4.47607211847807,5.07815149963482,26.5727082708936));
#54657=CARTESIAN_POINT('Ctrl Pts',(4.3433918367202,5.19208495826923,26.5809103961162));
#54658=CARTESIAN_POINT('Ctrl Pts',(4.2065703390607,5.30066552260513,26.5891125213388));
#54659=CARTESIAN_POINT('Ctrl Pts',(4.06970592182169,5.4092801476131,26.5973172194886));
#54660=CARTESIAN_POINT('Ctrl Pts',(3.92869798623901,5.51253831644174,26.6055219176385));
#54661=CARTESIAN_POINT('Ctrl Pts',(3.78401277938467,5.61012800972077,26.6137266157884));
#54662=CARTESIAN_POINT('Ctrl Pts',(3.63919306417103,5.70780842844307,26.6219389415355));
#54663=CARTESIAN_POINT('Ctrl Pts',(3.49068955190514,5.79980965362521,26.6301512672826));
#54664=CARTESIAN_POINT('Ctrl Pts',(3.33899528572142,5.88586437848598,26.6383635930298));
#54665=CARTESIAN_POINT('Ctrl Pts',(3.25986902722478,5.93075195779596,26.6426472790666));
#54666=CARTESIAN_POINT('Ctrl Pts',(3.1798750075793,5.97402235846659,26.6469309651035));
#54667=CARTESIAN_POINT('Ctrl Pts',(3.09908550384733,6.01564277861006,26.6512146511404));
#54668=CARTESIAN_POINT('Origin',(0.,0.,-63.6971797838103));
#54669=CARTESIAN_POINT('',(3.09908550384738,6.01564277861003,29.0457563580462));
#54670=CARTESIAN_POINT('',(3.09908550384705,6.0156427786102,28.6513967904261));
#54671=CARTESIAN_POINT('',(3.09908550384721,6.01564277861012,-63.6971797838103));
#54672=CARTESIAN_POINT('',(-6.76699784670241,0.00324515999788631,27.6971797838099));
#54673=CARTESIAN_POINT('Ctrl Pts',(-6.767,4.30010947876278E-12,27.6971797838099));
#54674=CARTESIAN_POINT('Ctrl Pts',(-6.76700000000012,-0.186007249555743,
27.7059292956227));
#54675=CARTESIAN_POINT('Ctrl Pts',(-6.7593263729427,-0.372014355811964,
27.7146788074354));
#54676=CARTESIAN_POINT('Ctrl Pts',(-6.74400518263396,-0.557389537582383,
27.7234283192481));
#54677=CARTESIAN_POINT('Ctrl Pts',(-6.72868405703772,-0.742763936378962,
27.7321777941054));
#54678=CARTESIAN_POINT('Ctrl Pts',(-6.70571545643614,-0.927506130401384,
27.7409272689626));
#54679=CARTESIAN_POINT('Ctrl Pts',(-6.67517739401632,-1.11098864009201,
27.7496767438198));
#54680=CARTESIAN_POINT('Ctrl Pts',(-6.64463945804457,-1.29447039004188,
27.7584261824483));
#54681=CARTESIAN_POINT('Ctrl Pts',(-6.60653217002804,-1.47669218338917,
27.7671756210768));
#54682=CARTESIAN_POINT('Ctrl Pts',(-6.56098496085573,-1.65703510627414,
27.7759250597053));
#54683=CARTESIAN_POINT('Ctrl Pts',(-6.51543793649655,-1.83737729739661,
27.7846744628319));
#54684=CARTESIAN_POINT('Ctrl Pts',(-6.46245112156998,-2.01584035544626,
27.7934238659586));
#54685=CARTESIAN_POINT('Ctrl Pts',(-6.40220448361822,-2.19181813797104,
27.8021732690852));
#54686=CARTESIAN_POINT('Ctrl Pts',(-6.34195808512075,-2.36779522106032,
27.8109226374368));
#54687=CARTESIAN_POINT('Ctrl Pts',(-6.27445201416452,-2.54128677725506,
27.8196720057883));
#54688=CARTESIAN_POINT('Ctrl Pts',(-6.19991555052815,-2.71170355428452,
27.8284213741398));
#54689=CARTESIAN_POINT('Ctrl Pts',(-6.12537937695205,-2.88211966813338,
27.837170708443));
#54690=CARTESIAN_POINT('Ctrl Pts',(-6.04381298028427,-3.04946076419718,
27.8459200427462));
#54691=CARTESIAN_POINT('Ctrl Pts',(-5.95549339308946,-3.21315848424378,
27.8546693770494));
#54692=CARTESIAN_POINT('Ctrl Pts',(-5.86717414225764,-3.37685558085162,
27.863418678031));
#54693=CARTESIAN_POINT('Ctrl Pts',(-5.7721018884401,-3.53690907700093,27.8721679790125));
#54694=CARTESIAN_POINT('Ctrl Pts',(-5.67059953311303,-3.69277537024097,
27.8809172799941));
#54695=CARTESIAN_POINT('Ctrl Pts',(-5.56909755592626,-3.84864108281145,
27.8896665483807));
#54696=CARTESIAN_POINT('Ctrl Pts',(-5.4611656815487,-4.0003193835496,27.8984158167673));
#54697=CARTESIAN_POINT('Ctrl Pts',(-5.34717048488266,-4.14729511918307,
27.907165085154));
#54698=CARTESIAN_POINT('Ctrl Pts',(-5.23317570343178,-4.29427031947334,
27.9159143216723));
#54699=CARTESIAN_POINT('Ctrl Pts',(-5.11311781951404,-4.43654276249722,
27.9246635581907));
#54700=CARTESIAN_POINT('Ctrl Pts',(-4.98740458929083,-4.57362924412558,
27.933412794709));
#54701=CARTESIAN_POINT('Ctrl Pts',(-4.86169180652574,-4.7107152378144,27.9421620000858));
#54702=CARTESIAN_POINT('Ctrl Pts',(-4.73032391141401,-4.84261509584657,
27.9509112054625));
#54703=CARTESIAN_POINT('Ctrl Pts',(-4.59374706947151,-4.96888084599762,
27.9596604108392));
#54704=CARTESIAN_POINT('Ctrl Pts',(-4.45717070231365,-5.09514615720865,
27.9684095858009));
#54705=CARTESIAN_POINT('Ctrl Pts',(-4.31538563497257,-5.21577720520669,
27.9771587607626));
#54706=CARTESIAN_POINT('Ctrl Pts',(-4.16887340951974,-5.33036429293527,
27.9859079357243));
#54707=CARTESIAN_POINT('Ctrl Pts',(-4.02236168122458,-5.44495099183725,
27.9946570809975));
#54708=CARTESIAN_POINT('Ctrl Pts',(-3.8711230526316,-5.55349359497943,28.0034062262707));
#54709=CARTESIAN_POINT('Ctrl Pts',(-3.71567116928981,-5.65562346357221,
28.012155371544));
#54710=CARTESIAN_POINT('Ctrl Pts',(-3.56021980053315,-5.75775299408924,
28.0209044878554));
#54711=CARTESIAN_POINT('Ctrl Pts',(-3.40055544442108,-5.85346967519865,
28.0296536041667));
#54712=CARTESIAN_POINT('Ctrl Pts',(-3.23722035886887,-5.94244843041359,
28.0384027204781));
#54713=CARTESIAN_POINT('Ctrl Pts',(-3.07388580043541,-6.03142689847425,
28.0471518085541));
#54714=CARTESIAN_POINT('Ctrl Pts',(-2.90688078789281,-6.11366734707874,
28.0559008966301));
#54715=CARTESIAN_POINT('Ctrl Pts',(-2.73677250610458,-6.188890470014,28.0646499847061));
#54716=CARTESIAN_POINT('Ctrl Pts',(-2.56666475917022,-6.26411335643298,
28.0733990452733));
#54717=CARTESIAN_POINT('Ctrl Pts',(-2.39345402457202,-6.33231884545214,
28.0821481058404));
#54718=CARTESIAN_POINT('Ctrl Pts',(-2.21772855944197,-6.39327529804837,
28.0908971664076));
#54719=CARTESIAN_POINT('Ctrl Pts',(-2.04200363223743,-6.45423156404654,
28.0996462001924));
#54720=CARTESIAN_POINT('Ctrl Pts',(-1.86376426061207,-6.50793874412403,
28.1083952339772));
#54721=CARTESIAN_POINT('Ctrl Pts',(-1.68361577621881,-6.55421443943263,
28.117144267762));
#54722=CARTESIAN_POINT('Ctrl Pts',(-1.50346782833454,-6.60048999692532,
28.1258932754909));
#54723=CARTESIAN_POINT('Ctrl Pts',(-1.32141105657673,-6.63933404265104,
28.1346422832197));
#54724=CARTESIAN_POINT('Ctrl Pts',(-1.13806375346868,-6.67061465631472,
28.1433912909486));
#54725=CARTESIAN_POINT('Ctrl Pts',(-0.954716981173318,-6.70189517941724,
28.152140273348));
#54726=CARTESIAN_POINT('Ctrl Pts',(-0.770079967445574,-6.72561226608966,
28.1608892557475));
#54727=CARTESIAN_POINT('Ctrl Pts',(-0.584779764076339,-6.74168536995957,
28.1696382381469));
#54728=CARTESIAN_POINT('Ctrl Pts',(-0.391489587596211,-6.75845153117854,
28.1787644685625));
#54729=CARTESIAN_POINT('Ctrl Pts',(-0.197478091808471,-6.76689985146385,
28.1878906989781));
#54730=CARTESIAN_POINT('Ctrl Pts',(-0.00346214753424312,-6.76699911434415,
28.1970169293937));
#54731=CARTESIAN_POINT('Ctrl Pts',(0.184490798481499,-6.76709527525944,
28.2058579651089));
#54732=CARTESIAN_POINT('Ctrl Pts',(0.372447602151712,-6.7593563379078,28.214699000824));
#54733=CARTESIAN_POINT('Ctrl Pts',(0.559756448191226,-6.74380914014538,
28.2235400365391));
#54734=CARTESIAN_POINT('Ctrl Pts',(0.745136131040457,-6.72842206873187,
28.2322900151524));
#54735=CARTESIAN_POINT('Ctrl Pts',(0.929880851942236,-6.70538686355763,
28.2410399937658));
#54736=CARTESIAN_POINT('Ctrl Pts',(1.11336305057191,-6.67478177303357,28.2497899723791));
#54737=CARTESIAN_POINT('Ctrl Pts',(1.29684337089858,-6.64417699581312,28.2585398614191));
#54738=CARTESIAN_POINT('Ctrl Pts',(1.47906091204931,-6.60600253548118,28.267289750459));
#54739=CARTESIAN_POINT('Ctrl Pts',(1.65939671094969,-6.56038806441276,28.276039639499));
#54740=CARTESIAN_POINT('Ctrl Pts',(1.83973072368907,-6.51477404513921,28.2847894418745));
#54741=CARTESIAN_POINT('Ctrl Pts',(2.01818275356783,-6.4617202328874,28.29353924425));
#54742=CARTESIAN_POINT('Ctrl Pts',(2.19414664033073,-6.40140683918195,28.3022890466255));
#54743=CARTESIAN_POINT('Ctrl Pts',(2.37010884270997,-6.34109402281595,28.311038765245));
#54744=CARTESIAN_POINT('Ctrl Pts',(2.54358267847536,-6.27352185699901,28.3197884838646));
#54745=CARTESIAN_POINT('Ctrl Pts',(2.71397890841464,-6.19891986435383,28.3285382024841));
#54746=CARTESIAN_POINT('Ctrl Pts',(2.88437356388674,-6.1243185610337,28.3372878402559));
#54747=CARTESIAN_POINT('Ctrl Pts',(3.05169040786914,-6.04268767582687,28.3460374780277));
#54748=CARTESIAN_POINT('Ctrl Pts',(3.21536112511806,-5.95430447954079,28.3547871157996));
#54749=CARTESIAN_POINT('Ctrl Pts',(3.37903038442588,-5.86592207055189,28.3635366756316));
#54750=CARTESIAN_POINT('Ctrl Pts',(3.53905332979713,-5.77078760703536,28.3722862354637));
#54751=CARTESIAN_POINT('Ctrl Pts',(3.69488643041626,-5.66922422085472,28.3810357952957));
#54752=CARTESIAN_POINT('Ctrl Pts',(3.85071819468482,-5.56766170563338,28.3897852800957));
#54753=CARTESIAN_POINT('Ctrl Pts',(4.0023599459897,-5.45967053456438,28.3985347648957));
#54754=CARTESIAN_POINT('Ctrl Pts',(4.14929662974053,-5.34561750206876,28.4072842496957));
#54755=CARTESIAN_POINT('Ctrl Pts',(4.29623210224798,-5.23156540974668,28.4160336623711));
#54756=CARTESIAN_POINT('Ctrl Pts',(4.43846235841872,-5.11145173172399,28.4247830750464));
#54757=CARTESIAN_POINT('Ctrl Pts',(4.57550431797185,-4.98568443006785,28.4335324877218));
#54758=CARTESIAN_POINT('Ctrl Pts',(4.71254519337256,-4.8599181233692,28.4422818311797));
#54759=CARTESIAN_POINT('Ctrl Pts',(4.84439764314752,-4.72849847631338,28.4510311746376));
#54760=CARTESIAN_POINT('Ctrl Pts',(4.97061384196461,-4.59187184425588,28.4597805180955));
#54761=CARTESIAN_POINT('Ctrl Pts',(5.09682908419996,-4.45524624767989,28.4685297952428));
#54762=CARTESIAN_POINT('Ctrl Pts',(5.21740796649975,-4.3134139555713,28.4772790723902));
#54763=CARTESIAN_POINT('Ctrl Pts',(5.33194095942069,-4.16685668163089,28.4860283495376));
#54764=CARTESIAN_POINT('Ctrl Pts',(5.44647312234952,-4.02030046975459,28.4947775632811));
#54765=CARTESIAN_POINT('Ctrl Pts',(5.5549593071211,-3.86901957035803,28.5035267770247));
#54766=CARTESIAN_POINT('Ctrl Pts',(5.6570310607962,-3.71352778058641,28.5122759907682));
#54767=CARTESIAN_POINT('Ctrl Pts',(5.75910210868564,-3.5580370659788,28.5210251440144));
#54768=CARTESIAN_POINT('Ctrl Pts',(5.85475865698382,-3.39833575881187,28.5297742972606));
#54769=CARTESIAN_POINT('Ctrl Pts',(5.943675830689,-3.23496624707019,28.5385234505068));
#54770=CARTESIAN_POINT('Ctrl Pts',(6.03259241909927,-3.07159781070396,28.5472725461619));
#54771=CARTESIAN_POINT('Ctrl Pts',(6.11476958470828,-2.90456146976127,28.556021641817));
#54772=CARTESIAN_POINT('Ctrl Pts',(6.18992823574258,-2.73442451648547,28.5647707374721));
#54773=CARTESIAN_POINT('Ctrl Pts',(6.26508641700816,-2.56428862662706,28.5735197784423));
#54774=CARTESIAN_POINT('Ctrl Pts',(6.33322605570187,-2.39105242531567,28.5822688194124));
#54775=CARTESIAN_POINT('Ctrl Pts',(6.39411573747667,-2.21530425354018,28.5910178603825));
#54776=CARTESIAN_POINT('Ctrl Pts',(6.45500505889026,-2.03955712188874,28.5997668495735));
#54777=CARTESIAN_POINT('Ctrl Pts',(6.50864441544832,-1.8612983202591,28.6085158387645));
#54778=CARTESIAN_POINT('Ctrl Pts',(6.55485164049813,-1.68113324012671,28.6172648279555));
#54779=CARTESIAN_POINT('Ctrl Pts',(6.60199852639029,-1.49730435913254,28.6261917348324));
#54780=CARTESIAN_POINT('Ctrl Pts',(6.64140767440941,-1.31149113174,28.6351186417092));
#54781=CARTESIAN_POINT('Ctrl Pts',(6.67293975269545,-1.12435050446772,28.6440455485861));
#54782=CARTESIAN_POINT('Ctrl Pts',(6.7038466483146,-0.940920291567091,28.6527954627701));
#54783=CARTESIAN_POINT('Ctrl Pts',(6.72718585889629,-0.756215114281222,
28.6615453769541));
#54784=CARTESIAN_POINT('Ctrl Pts',(6.74287810451837,-0.570862389378351,
28.6702952911381));
#54785=CARTESIAN_POINT('Ctrl Pts',(6.75857004154105,-0.385513309571343,
28.6790450332487));
#54786=CARTESIAN_POINT('Ctrl Pts',(6.76661529035546,-0.199516993262481,
28.6877947753593));
#54787=CARTESIAN_POINT('Ctrl Pts',(6.76698652348896,-0.0135052182083492,
28.6965445174699));
#54788=CARTESIAN_POINT('Ctrl Pts',(6.76735774981532,0.172503146034585,28.7052940991405));
#54789=CARTESIAN_POINT('Ctrl Pts',(6.76005524147502,0.358526681829154,28.7140436808111));
#54790=CARTESIAN_POINT('Ctrl Pts',(6.74510380214916,0.543933542110543,28.7227932624818));
#54791=CARTESIAN_POINT('Ctrl Pts',(6.73015261711027,0.729337249080307,28.7315426953437));
#54792=CARTESIAN_POINT('Ctrl Pts',(6.70755278444666,0.91412401585016,28.7402921282056));
#54793=CARTESIAN_POINT('Ctrl Pts',(6.67738106408364,1.09766621748927,28.7490415610676));
#54794=CARTESIAN_POINT('Ctrl Pts',(6.64720981677343,1.28120554142862,28.7577908567499));
#54795=CARTESIAN_POINT('Ctrl Pts',(6.60946696581625,1.46350005650159,28.7665401524323));
#54796=CARTESIAN_POINT('Ctrl Pts',(6.5642807001111,1.64393062206072,28.7752894481146));
#54797=CARTESIAN_POINT('Ctrl Pts',(6.51909508282871,1.82435859844187,28.7840386182446));
#54798=CARTESIAN_POINT('Ctrl Pts',(6.46646633415806,2.00292240086095,28.7927877883746));
#54799=CARTESIAN_POINT('Ctrl Pts',(6.40657319597352,2.17901557695983,28.8015369585046));
#54800=CARTESIAN_POINT('Ctrl Pts',(6.34668083768471,2.3551064600696,28.8102860147076));
#54801=CARTESIAN_POINT('Ctrl Pts',(6.27952437144077,2.52872650996053,28.8190350709107));
#54802=CARTESIAN_POINT('Ctrl Pts',(6.20533187335345,2.69928607997445,28.8277841271138));
#54803=CARTESIAN_POINT('Ctrl Pts',(6.12831449784469,2.87633970114936,28.8368663034026));
#54804=CARTESIAN_POINT('Ctrl Pts',(6.04371489463377,3.05009490561907,28.8459484796915));
#54805=CARTESIAN_POINT('Ctrl Pts',(5.9518426512072,3.21991584599208,28.8550306559803));
#54806=CARTESIAN_POINT('Ctrl Pts',(5.86333281335734,3.38352155904882,28.8637804363347));
#54807=CARTESIAN_POINT('Ctrl Pts',(5.76807337235938,3.54347560903412,28.8725302166892));
#54808=CARTESIAN_POINT('Ctrl Pts',(5.66638790086621,3.6992346717824,28.8812799970436));
#54809=CARTESIAN_POINT('Ctrl Pts',(5.56470608503021,3.85498813489362,28.8900294628378));
#54810=CARTESIAN_POINT('Ctrl Pts',(5.45659885767243,4.00654667255865,28.8987789286321));
#54811=CARTESIAN_POINT('Ctrl Pts',(5.34243340580811,4.1533955150582,28.9075283944264));
#54812=CARTESIAN_POINT('Ctrl Pts',(5.22827145140903,4.30023985883495,28.9162775921802));
#54813=CARTESIAN_POINT('Ctrl Pts',(5.10805181978403,4.44237456992682,28.9250267899341));
#54814=CARTESIAN_POINT('Ctrl Pts',(4.9821828128287,4.57931691626102,28.933775987688));
#54815=CARTESIAN_POINT('Ctrl Pts',(4.85631699296544,4.71625579511838,28.942524963906));
#54816=CARTESIAN_POINT('Ctrl Pts',(4.72480227792148,4.84800236135468,28.951273940124));
#54817=CARTESIAN_POINT('Ctrl Pts',(4.58808530848417,4.97410918678628,28.960022916342));
#54818=CARTESIAN_POINT('Ctrl Pts',(4.45135945057278,5.10022421088741,28.9687724613632));
#54819=CARTESIAN_POINT('Ctrl Pts',(4.3094308720835,5.2206985661173,28.9775220063844));
#54820=CARTESIAN_POINT('Ctrl Pts',(4.16278164322781,5.33512305301439,28.9862715514056));
#54821=CARTESIAN_POINT('Ctrl Pts',(4.01614103534698,5.44954081331201,28.9950205820729));
#54822=CARTESIAN_POINT('Ctrl Pts',(3.86478055833713,5.55790924068129,29.0037696127402));
#54823=CARTESIAN_POINT('Ctrl Pts',(3.70921425812244,5.65986029751099,29.0125186434074));
#54824=CARTESIAN_POINT('Ctrl Pts',(3.55364584530422,5.76181273884467,29.0212677928873));
#54825=CARTESIAN_POINT('Ctrl Pts',(3.39387173464656,5.85734747817882,29.0300169423671));
#54826=CARTESIAN_POINT('Ctrl Pts',(3.23043456092726,5.94614005448633,29.038766091847));
#54827=CARTESIAN_POINT('Ctrl Pts',(3.18690768806613,5.96978744811164,29.0410961805801));
#54828=CARTESIAN_POINT('Ctrl Pts',(3.14312114983002,5.99295688499238,29.0434262693131));
#54829=CARTESIAN_POINT('Ctrl Pts',(3.09908550384738,6.01564277861003,29.0457563580462));
#54830=CARTESIAN_POINT('Ctrl Pts',(3.09908550384735,6.01564277861005,27.0459166703402));
#54831=CARTESIAN_POINT('Ctrl Pts',(2.93605479406775,6.09963149402321,27.0545480454384));
#54832=CARTESIAN_POINT('Ctrl Pts',(2.76952358531319,6.1770322731653,27.0631794205365));
#54833=CARTESIAN_POINT('Ctrl Pts',(2.60004025099926,6.24756590146784,27.0718107956347));
#54834=CARTESIAN_POINT('Ctrl Pts',(2.43067166116671,6.31805177672946,27.0804363270747));
#54835=CARTESIAN_POINT('Ctrl Pts',(2.25835521155813,6.38167965649669,27.0890618585148));
#54836=CARTESIAN_POINT('Ctrl Pts',(2.08366127629973,6.43821750841403,27.0976873899548));
#54837=CARTESIAN_POINT('Ctrl Pts',(1.90910481826852,6.49471086727498,27.1063061334423));
#54838=CARTESIAN_POINT('Ctrl Pts',(1.73217489681239,6.54412523909033,27.1149248769297));
#54839=CARTESIAN_POINT('Ctrl Pts',(1.55345949011609,6.58627759911228,27.1235436204172));
#54840=CARTESIAN_POINT('Ctrl Pts',(1.46810051161555,6.60641062770436,27.1276601493368));
#54841=CARTESIAN_POINT('Ctrl Pts',(1.38233446969443,6.62488772612642,27.1317766782565));
#54842=CARTESIAN_POINT('Ctrl Pts',(1.29622666598318,6.64169296417669,27.1358932071761));
#54843=CARTESIAN_POINT('Ctrl Pts',(1.11997957221407,6.67609024570984,27.1443189970259));
#54844=CARTESIAN_POINT('Ctrl Pts',(0.942376881392607,6.70346498969645,27.1527447868757));
#54845=CARTESIAN_POINT('Ctrl Pts',(0.764002966958121,6.7237332239225,27.1611705767256));
#54846=CARTESIAN_POINT('Ctrl Pts',(0.585587663774305,6.74400616106078,27.1695983216421));
#54847=CARTESIAN_POINT('Ctrl Pts',(0.406401109563409,6.75716926324582,27.1780260665587));
#54848=CARTESIAN_POINT('Ctrl Pts',(0.227032608423332,6.76319045973958,27.1864538114752));
#54849=CARTESIAN_POINT('Ctrl Pts',(0.047598198358595,6.76921386872095,27.1948846531652));
#54850=CARTESIAN_POINT('Ctrl Pts',(-0.132017960781943,6.76809012829394,
27.2033154948552));
#54851=CARTESIAN_POINT('Ctrl Pts',(-0.31122635973812,6.75983928455434,27.2117463365451));
#54852=CARTESIAN_POINT('Ctrl Pts',(-0.490599428339162,6.75158085934247,
27.2201849251025));
#54853=CARTESIAN_POINT('Ctrl Pts',(-0.669563656796403,6.73618226199444,
27.2286235136598));
#54854=CARTESIAN_POINT('Ctrl Pts',(-0.847533326702103,6.71371553315519,
27.2370621022172));
#54855=CARTESIAN_POINT('Ctrl Pts',(-1.02559631603796,6.69123702375618,27.2455051155975));
#54856=CARTESIAN_POINT('Ctrl Pts',(-1.20266337921886,6.66168304044586,27.2539481289778));
#54857=CARTESIAN_POINT('Ctrl Pts',(-1.37815821303781,6.62517689875798,27.2623911423581));
#54858=CARTESIAN_POINT('Ctrl Pts',(-1.5538374164115,6.58863240482382,27.2708430257124));
#54859=CARTESIAN_POINT('Ctrl Pts',(-1.72794076836931,6.54512123785287,27.2792949090668));
#54860=CARTESIAN_POINT('Ctrl Pts',(-1.8999053223626,6.49481706948381,27.2877467924211));
#54861=CARTESIAN_POINT('Ctrl Pts',(-1.94677109608751,6.48110759437712,27.2900501976499));
#54862=CARTESIAN_POINT('Ctrl Pts',(-1.9934781158684,6.46689386041559,27.2923536028787));
#54863=CARTESIAN_POINT('Ctrl Pts',(-2.0400152289791,6.45218000876707,27.2946570081074));
#54864=CARTESIAN_POINT('Ctrl Pts',(-2.20805405808109,6.39905040451516,27.3029742734408));
#54865=CARTESIAN_POINT('Ctrl Pts',(-2.37417838005245,6.33930081292399,27.3112915387742));
#54866=CARTESIAN_POINT('Ctrl Pts',(-2.53783939289301,6.27309016481355,27.3196088041076));
#54867=CARTESIAN_POINT('Ctrl Pts',(-2.70136237026249,6.20693536029006,27.3279190544677));
#54868=CARTESIAN_POINT('Ctrl Pts',(-2.86242585707067,6.13433048632257,27.3362293048278));
#54869=CARTESIAN_POINT('Ctrl Pts',(-3.02049713478366,6.05548396569289,27.3445395551879));
#54870=CARTESIAN_POINT('Ctrl Pts',(-3.17846404046859,5.9766895062054,27.3528443184177));
#54871=CARTESIAN_POINT('Ctrl Pts',(-3.33344236368593,5.89166176691848,27.3611490816476));
#54872=CARTESIAN_POINT('Ctrl Pts',(-3.48492006132125,5.80065695987969,27.3694538448775));
#54873=CARTESIAN_POINT('Ctrl Pts',(-3.63632546952663,5.70969558290173,27.3777546448401));
#54874=CARTESIAN_POINT('Ctrl Pts',(-3.78423328394655,5.612763001541,27.3860554448027));
#54875=CARTESIAN_POINT('Ctrl Pts',(-3.92815654496965,5.51016108278262,27.3943562447653));
#54876=CARTESIAN_POINT('Ctrl Pts',(-4.07203745887423,5.40758935299843,27.4026546023502));
#54877=CARTESIAN_POINT('Ctrl Pts',(-4.21193587341536,5.29935181253114,27.4109529599351));
#54878=CARTESIAN_POINT('Ctrl Pts',(-4.34739409618035,5.18579343712187,27.4192513175201));
#54879=CARTESIAN_POINT('Ctrl Pts',(-4.48286610150874,5.07222350740843,27.4275505194438));
#54880=CARTESIAN_POINT('Ctrl Pts',(-4.61389674099209,4.9533318787011,27.4358497213676));
#54881=CARTESIAN_POINT('Ctrl Pts',(-4.74006124268781,4.82950395129447,27.4441489232914));
#54882=CARTESIAN_POINT('Ctrl Pts',(-4.86623853507252,4.7056634700832,27.4524489665969));
#54883=CARTESIAN_POINT('Ctrl Pts',(-4.98754845759794,4.57688593606884,27.4607490099025));
#54884=CARTESIAN_POINT('Ctrl Pts',(-5.10360304661759,4.44359369683545,27.469049053208));
#54885=CARTESIAN_POINT('Ctrl Pts',(-5.21968866668782,4.31026581749291,27.4773513158059));
#54886=CARTESIAN_POINT('Ctrl Pts',(-5.33051592409775,4.1724210893604,27.4856535784038));
#54887=CARTESIAN_POINT('Ctrl Pts',(-5.43573698275921,4.03051515990993,27.4939558410017));
#54888=CARTESIAN_POINT('Ctrl Pts',(-5.54100364478619,3.88854772767617,27.5022617018443));
#54889=CARTESIAN_POINT('Ctrl Pts',(-5.64065905844078,3.7425158654118,27.510567562687));
#54890=CARTESIAN_POINT('Ctrl Pts',(-5.7343984652765,3.5929045689295,27.5188734235296));
#54891=CARTESIAN_POINT('Ctrl Pts',(-5.82824867870474,3.44311642133918,27.5271891024857));
#54892=CARTESIAN_POINT('Ctrl Pts',(-5.91616872833246,3.2897406809609,27.5355047814418));
#54893=CARTESIAN_POINT('Ctrl Pts',(-5.99789904712273,3.13328837174689,27.5438204603979));
#54894=CARTESIAN_POINT('Ctrl Pts',(-6.07968105968878,2.9767371076932,27.5521413989548));
#54895=CARTESIAN_POINT('Ctrl Pts',(-6.15526538532918,2.81710570815055,27.5604623375116));
#54896=CARTESIAN_POINT('Ctrl Pts',(-6.22444041261873,2.65492571454622,27.5687832760684));
#54897=CARTESIAN_POINT('Ctrl Pts',(-6.29371825542564,2.49250467123652,27.5771165821174));
#54898=CARTESIAN_POINT('Ctrl Pts',(-6.35656763837977,2.32752778862264,27.5854498881663));
#54899=CARTESIAN_POINT('Ctrl Pts',(-6.41282623649688,2.16054360300765,27.5937831942152));
#54900=CARTESIAN_POINT('Ctrl Pts',(-6.45423588622814,2.03763338362067,27.599916999467));
#54901=CARTESIAN_POINT('Ctrl Pts',(-6.49207580302994,1.91363596890389,27.6060508047188));
#54902=CARTESIAN_POINT('Ctrl Pts',(-6.52629897085645,1.78877353038278,27.6121846099706));
#54903=CARTESIAN_POINT('Ctrl Pts',(-6.58230854197514,1.58442390191316,27.6222231839337));
#54904=CARTESIAN_POINT('Ctrl Pts',(-6.62877194642737,1.37723941178004,27.6322617578968));
#54905=CARTESIAN_POINT('Ctrl Pts',(-6.66543459182177,1.1680199921858,27.64230033186));
#54906=CARTESIAN_POINT('Ctrl Pts',(-6.70154781580039,0.96193590634854,27.6521884691195));
#54907=CARTESIAN_POINT('Ctrl Pts',(-6.72815180168886,0.753877410366474,
27.662076606379));
#54908=CARTESIAN_POINT('Ctrl Pts',(-6.7450473860383,0.544632683648273,27.6719647436385));
#54909=CARTESIAN_POINT('Ctrl Pts',(-6.75940879799794,0.366772619229647,
27.6803697570289));
#54910=CARTESIAN_POINT('Ctrl Pts',(-6.76675639309456,0.188055855418755,
27.6887747704194));
#54911=CARTESIAN_POINT('Ctrl Pts',(-6.76699404115812,0.00898036360930988,
27.6971797838099));
#54912=CARTESIAN_POINT('',(-6.767,3.80125455851782E-12,27.3028202161898));
#54913=CARTESIAN_POINT('Ctrl Pts',(3.09908550384733,6.01564277861006,26.6512146511404));
#54914=CARTESIAN_POINT('Ctrl Pts',(2.94396840926309,6.09555462791971,26.6594393944729));
#54915=CARTESIAN_POINT('Ctrl Pts',(2.78591789415201,6.1693808510076,26.6676641378053));
#54916=CARTESIAN_POINT('Ctrl Pts',(2.62545871930722,6.23692676830614,26.6758888811378));
#54917=CARTESIAN_POINT('Ctrl Pts',(2.56597851648579,6.26196519234493,26.6789376902947));
#54918=CARTESIAN_POINT('Ctrl Pts',(2.50616749398762,6.28614113728922,26.6819864994515));
#54919=CARTESIAN_POINT('Ctrl Pts',(2.44605286443358,6.30944644040951,26.6850353086083));
#54920=CARTESIAN_POINT('Ctrl Pts',(2.2698740956819,6.37774761168144,26.6939704953906));
#54921=CARTESIAN_POINT('Ctrl Pts',(2.09072110230475,6.43870896745376,26.702905682173));
#54922=CARTESIAN_POINT('Ctrl Pts',(1.90920164027248,6.4920904258013,26.7118408689553));
#54923=CARTESIAN_POINT('Ctrl Pts',(1.72795403824027,6.54539193523809,26.7207626735919));
#54924=CARTESIAN_POINT('Ctrl Pts',(1.54434728680086,6.59113612638472,26.7296844782285));
#54925=CARTESIAN_POINT('Ctrl Pts',(1.35900626864516,6.62913199157953,26.7386062828652));
#54926=CARTESIAN_POINT('Ctrl Pts',(1.17411734118709,6.66703517584826,26.7475063251045));
#54927=CARTESIAN_POINT('Ctrl Pts',(0.987502842551587,6.69722770356834,26.7564063673438));
#54928=CARTESIAN_POINT('Ctrl Pts',(0.799799258886218,6.71956919344426,26.7653064095831));
#54929=CARTESIAN_POINT('Ctrl Pts',(0.612384647647815,6.74187628826801,26.7741927500766));
#54930=CARTESIAN_POINT('Ctrl Pts',(0.423884551130265,6.7563564248753,26.7830790905699));
#54931=CARTESIAN_POINT('Ctrl Pts',(0.234944959542762,6.76292021733108,26.7919654310633));
#54932=CARTESIAN_POINT('Ctrl Pts',(0.046488453510159,6.76946722731531,26.8008290507353));
#54933=CARTESIAN_POINT('Ctrl Pts',(-0.142405047894484,6.76813827328685,
26.8096926704073));
#54934=CARTESIAN_POINT('Ctrl Pts',(-0.331085886631742,6.75889570386119,
26.8185562900792));
#54935=CARTESIAN_POINT('Ctrl Pts',(-0.51020143701945,6.75012169203915,26.8269705632327));
#54936=CARTESIAN_POINT('Ctrl Pts',(-0.689125089154248,6.73421643709939,
26.8353848363862));
#54937=CARTESIAN_POINT('Ctrl Pts',(-0.86729702919699,6.71119101673809,26.8437991095397));
#54938=CARTESIAN_POINT('Ctrl Pts',(-1.04114874807327,6.68872390487581,26.8520093577442));
#54939=CARTESIAN_POINT('Ctrl Pts',(-1.21411755445475,6.65949831652102,26.8602196059488));
#54940=CARTESIAN_POINT('Ctrl Pts',(-1.38564777503169,6.62361451501744,26.8684298541533));
#54941=CARTESIAN_POINT('Ctrl Pts',(-1.5572187717618,6.58772218321884,26.8766420540975));
#54942=CARTESIAN_POINT('Ctrl Pts',(-1.72735015295138,6.54516855778685,26.8848542540417));
#54943=CARTESIAN_POINT('Ctrl Pts',(-1.89549811119315,6.49610467206796,26.8930664539859));
#54944=CARTESIAN_POINT('Ctrl Pts',(-2.06371598399514,6.44702038598247,26.9012820684964));
#54945=CARTESIAN_POINT('Ctrl Pts',(-2.22994844946578,6.39142054646708,26.9094976830069));
#54946=CARTESIAN_POINT('Ctrl Pts',(-2.39366840240841,6.32950555567428,26.9177132975174));
#54947=CARTESIAN_POINT('Ctrl Pts',(-2.55757220568088,6.26752103706111,26.9259381378028));
#54948=CARTESIAN_POINT('Ctrl Pts',(-2.71895752803241,6.19920732882995,26.9341629780882));
#54949=CARTESIAN_POINT('Ctrl Pts',(-2.87731784303245,6.12481273429377,26.9423878183736));
#54950=CARTESIAN_POINT('Ctrl Pts',(-3.03577959331905,6.05037048743374,26.9506179269551));
#54951=CARTESIAN_POINT('Ctrl Pts',(-3.19121215847159,5.9698397530627,26.9588480355366));
#54952=CARTESIAN_POINT('Ctrl Pts',(-3.3431350941232,5.88351397911502,26.9670781441182));
#54953=CARTESIAN_POINT('Ctrl Pts',(-3.49526631845103,5.79706985120648,26.9753195363048));
#54954=CARTESIAN_POINT('Ctrl Pts',(-3.64387800078042,5.70481500142485,26.9835609284915));
#54955=CARTESIAN_POINT('Ctrl Pts',(-3.78851923208803,5.60708578747455,26.9918023206782));
#54956=CARTESIAN_POINT('Ctrl Pts',(-3.85147077077765,5.56455155060807,26.9953891839426));
#54957=CARTESIAN_POINT('Ctrl Pts',(-3.91367065011081,5.52098086674005,26.998976047207));
#54958=CARTESIAN_POINT('Ctrl Pts',(-3.97508375785953,5.47640375775941,27.0025629104715));
#54959=CARTESIAN_POINT('Ctrl Pts',(-4.11858185142801,5.37224472086962,27.0109439883749));
#54960=CARTESIAN_POINT('Ctrl Pts',(-4.25812341298019,5.26234050420493,27.0193250662783));
#54961=CARTESIAN_POINT('Ctrl Pts',(-4.39323229053872,5.14701846133933,27.0277061441818));
#54962=CARTESIAN_POINT('Ctrl Pts',(-4.52821375403582,5.03180517261425,27.0360793183324));
#54963=CARTESIAN_POINT('Ctrl Pts',(-4.6587706055261,4.91118445998857,27.0444524924829));
#54964=CARTESIAN_POINT('Ctrl Pts',(-4.78445752919904,4.78552558777932,27.0528256666335));
#54965=CARTESIAN_POINT('Ctrl Pts',(-4.91004744550775,4.65996370128369,27.061192378222));
#54966=CARTESIAN_POINT('Ctrl Pts',(-5.03077468462145,4.52937164579121,27.0695590898104));
#54967=CARTESIAN_POINT('Ctrl Pts',(-5.14622853284925,4.39415758566852,27.0779258013989));
#54968=CARTESIAN_POINT('Ctrl Pts',(-5.26161302402364,4.25902475323061,27.0862874868191));
#54969=CARTESIAN_POINT('Ctrl Pts',(-5.37173021773203,4.1192757098648,27.0946491722393));
#54970=CARTESIAN_POINT('Ctrl Pts',(-5.47620746828476,3.97535416841095,27.1030108576596));
#54971=CARTESIAN_POINT('Ctrl Pts',(-5.58064435175422,3.83148823420954,27.1113693123588));
#54972=CARTESIAN_POINT('Ctrl Pts',(-5.67944543449643,3.68345329071489,27.119727767058));
#54973=CARTESIAN_POINT('Ctrl Pts',(-5.77227923171137,3.53172499936697,27.1280862217571));
#54974=CARTESIAN_POINT('Ctrl Pts',(-5.86509355306056,3.38002853952784,27.1364429229124));
#54975=CARTESIAN_POINT('Ctrl Pts',(-5.95194290540346,3.22464056698319,27.1447996240677));
#54976=CARTESIAN_POINT('Ctrl Pts',(-6.03253975024757,3.06606476801829,27.1531563252229));
#54977=CARTESIAN_POINT('Ctrl Pts',(-6.1131321930474,2.9074976301578,27.1615125699513));
#54978=CARTESIAN_POINT('Ctrl Pts',(-6.1874726543895,2.74574331735602,27.1698688146796));
#54979=CARTESIAN_POINT('Ctrl Pts',(-6.25531996334364,2.58132933896365,27.178225059408));
#54980=CARTESIAN_POINT('Ctrl Pts',(-6.32317409415783,2.41689882919858,27.1865821443337));
#54981=CARTESIAN_POINT('Ctrl Pts',(-6.38453364155701,2.2498084366913,27.1949392292595));
#54982=CARTESIAN_POINT('Ctrl Pts',(-6.43920581269364,2.08060508068504,27.2032963141852));
#54983=CARTESIAN_POINT('Ctrl Pts',(-6.49391511153665,1.91128681919052,27.2116590743821));
#54984=CARTESIAN_POINT('Ctrl Pts',(-6.54192785242033,1.73985305173175,27.220021834579));
#54985=CARTESIAN_POINT('Ctrl Pts',(-6.58310103126158,1.56686623940997,27.2283845947759));
#54986=CARTESIAN_POINT('Ctrl Pts',(-6.62428763052127,1.39382304194932,27.2367500808187));
#54987=CARTESIAN_POINT('Ctrl Pts',(-6.65863015074845,1.2192261243188,27.2451155668615));
#54988=CARTESIAN_POINT('Ctrl Pts',(-6.68603679320054,1.04364792912585,27.2534810529043));
#54989=CARTESIAN_POINT('Ctrl Pts',(-6.71347283343644,0.867881399669266,
27.2618555122007));
#54990=CARTESIAN_POINT('Ctrl Pts',(-6.73395808035583,0.691131827904614,
27.2702299714969));
#54991=CARTESIAN_POINT('Ctrl Pts',(-6.74745253910463,0.513977852179009,
27.2786044307932));
#54992=CARTESIAN_POINT('Ctrl Pts',(-6.76045950490944,0.343223637627389,
27.2866763592587));
#54993=CARTESIAN_POINT('Ctrl Pts',(-6.76697195104396,0.172094006548877,
27.2947482877242));
#54994=CARTESIAN_POINT('Ctrl Pts',(-6.76699990953827,0.00110648500407755,
27.3028202161897));
#54995=CARTESIAN_POINT('Ctrl Pts',(-6.767,4.18591371480668E-12,27.3028202161898));
#54996=CARTESIAN_POINT('Ctrl Pts',(-6.76700000000012,-0.186007249555859,
27.3115697280026));
#54997=CARTESIAN_POINT('Ctrl Pts',(-6.75932637294269,-0.372014355812083,
27.3203192398153));
#54998=CARTESIAN_POINT('Ctrl Pts',(-6.74400518263395,-0.557389537582502,
27.329068751628));
#54999=CARTESIAN_POINT('Ctrl Pts',(-6.72868405703772,-0.742763936378955,
27.3378182264852));
#55000=CARTESIAN_POINT('Ctrl Pts',(-6.70571545643616,-0.92750613040125,
27.3465677013424));
#55001=CARTESIAN_POINT('Ctrl Pts',(-6.67517739401636,-1.11098864009176,
27.3553171761996));
#55002=CARTESIAN_POINT('Ctrl Pts',(-6.6446394580446,-1.29447039004176,27.3640666148281));
#55003=CARTESIAN_POINT('Ctrl Pts',(-6.60653217002805,-1.47669218338917,
27.3728160534567));
#55004=CARTESIAN_POINT('Ctrl Pts',(-6.5609849608557,-1.65703510627426,27.3815654920852));
#55005=CARTESIAN_POINT('Ctrl Pts',(-6.51543793649651,-1.83737729739674,
27.3903148952118));
#55006=CARTESIAN_POINT('Ctrl Pts',(-6.46245112156994,-2.01584035544639,
27.3990642983385));
#55007=CARTESIAN_POINT('Ctrl Pts',(-6.40220448361817,-2.19181813797117,
27.4078137014651));
#55008=CARTESIAN_POINT('Ctrl Pts',(-6.34195808512075,-2.36779522106032,
27.4165630698166));
#55009=CARTESIAN_POINT('Ctrl Pts',(-6.27445201416456,-2.54128677725495,
27.4253124381682));
#55010=CARTESIAN_POINT('Ctrl Pts',(-6.19991555052824,-2.71170355428429,
27.4340618065197));
#55011=CARTESIAN_POINT('Ctrl Pts',(-6.1253793769522,-2.88211966813304,27.4428111408229));
#55012=CARTESIAN_POINT('Ctrl Pts',(-6.0438129802845,-3.04946076419673,27.4515604751261));
#55013=CARTESIAN_POINT('Ctrl Pts',(-5.95549339308976,-3.21315848424322,
27.4603098094293));
#55014=CARTESIAN_POINT('Ctrl Pts',(-5.86717414225807,-3.37685558085085,
27.4690591104108));
#55015=CARTESIAN_POINT('Ctrl Pts',(-5.77210188844069,-3.53690907699995,
27.4778084113924));
#55016=CARTESIAN_POINT('Ctrl Pts',(-5.67059953311379,-3.6927753702398,27.4865577123739));
#55017=CARTESIAN_POINT('Ctrl Pts',(-5.56909755592719,-3.8486410828101,27.4953069807605));
#55018=CARTESIAN_POINT('Ctrl Pts',(-5.46116568154982,-4.00031938354806,
27.5040562491472));
#55019=CARTESIAN_POINT('Ctrl Pts',(-5.34717048488398,-4.14729511918137,
27.5128055175338));
#55020=CARTESIAN_POINT('Ctrl Pts',(-5.23317570343323,-4.29427031947158,
27.5215547540521));
#55021=CARTESIAN_POINT('Ctrl Pts',(-5.11311781951561,-4.4365427624954,27.5303039905705));
#55022=CARTESIAN_POINT('Ctrl Pts',(-4.98740458929254,-4.57362924412372,
27.5390532270888));
#55023=CARTESIAN_POINT('Ctrl Pts',(-4.86169180652732,-4.71071523781276,
27.5478024324655));
#55024=CARTESIAN_POINT('Ctrl Pts',(-4.73032391141546,-4.84261509584517,
27.5565516378423));
#55025=CARTESIAN_POINT('Ctrl Pts',(-4.5937470694728,-4.96888084599642,27.565300843219));
#55026=CARTESIAN_POINT('Ctrl Pts',(-4.45717070231507,-5.09514615720741,
27.5740500181807));
#55027=CARTESIAN_POINT('Ctrl Pts',(-4.31538563497412,-5.2157772052054,27.5827991931424));
#55028=CARTESIAN_POINT('Ctrl Pts',(-4.16887340952143,-5.33036429293395,
27.5915483681041));
#55029=CARTESIAN_POINT('Ctrl Pts',(-4.0223616812264,-5.4449509918359,27.6002975133773));
#55030=CARTESIAN_POINT('Ctrl Pts',(-3.87112305263356,-5.55349359497806,
27.6090466586505));
#55031=CARTESIAN_POINT('Ctrl Pts',(-3.71567116929191,-5.65562346357083,
27.6177958039238));
#55032=CARTESIAN_POINT('Ctrl Pts',(-3.56021980053529,-5.75775299408792,
27.6265449202351));
#55033=CARTESIAN_POINT('Ctrl Pts',(-3.40055544442325,-5.85346967519738,
27.6352940365465));
#55034=CARTESIAN_POINT('Ctrl Pts',(-3.23722035887108,-5.94244843041239,
27.6440431528579));
#55035=CARTESIAN_POINT('Ctrl Pts',(-3.07388580043764,-6.03142689847311,
27.6527922409339));
#55036=CARTESIAN_POINT('Ctrl Pts',(-2.90688078789508,-6.11366734707766,
27.6615413290099));
#55037=CARTESIAN_POINT('Ctrl Pts',(-2.73677250610687,-6.18889047001298,
27.6702904170859));
#55038=CARTESIAN_POINT('Ctrl Pts',(-2.56666475917254,-6.26411335643203,
27.679039477653));
#55039=CARTESIAN_POINT('Ctrl Pts',(-2.39345402457436,-6.33231884545125,
27.6877885382202));
#55040=CARTESIAN_POINT('Ctrl Pts',(-2.21772855944434,-6.39327529804755,
27.6965375987873));
#55041=CARTESIAN_POINT('Ctrl Pts',(-2.04200363223982,-6.45423156404578,
27.7052866325721));
#55042=CARTESIAN_POINT('Ctrl Pts',(-1.86376426061447,-6.50793874412334,
27.714035666357));
#55043=CARTESIAN_POINT('Ctrl Pts',(-1.68361577622123,-6.55421443943201,
27.7227847001418));
#55044=CARTESIAN_POINT('Ctrl Pts',(-1.50346782833673,-6.60048999692483,
27.7315337078706));
#55045=CARTESIAN_POINT('Ctrl Pts',(-1.32141105657867,-6.63933404265066,
27.7402827155995));
#55046=CARTESIAN_POINT('Ctrl Pts',(-1.13806375347037,-6.67061465631443,
27.7490317233284));
#55047=CARTESIAN_POINT('Ctrl Pts',(-0.954716981174895,-6.70189517941702,
27.7577807057278));
#55048=CARTESIAN_POINT('Ctrl Pts',(-0.770079967447028,-6.7256122660895,
27.7665296881273));
#55049=CARTESIAN_POINT('Ctrl Pts',(-0.584779764077667,-6.74168536995945,
27.7752786705267));
#55050=CARTESIAN_POINT('Ctrl Pts',(-0.391489587597413,-6.75845153117847,
27.7844049009423));
#55051=CARTESIAN_POINT('Ctrl Pts',(-0.197478091809546,-6.76689985146382,
27.793531131358));
#55052=CARTESIAN_POINT('Ctrl Pts',(-0.00346214753518824,-6.76699911434415,
27.8026573617736));
#55053=CARTESIAN_POINT('Ctrl Pts',(0.184490798480555,-6.76709527525946,
27.8114983974887));
#55054=CARTESIAN_POINT('Ctrl Pts',(0.372447602150772,-6.75935633790785,
27.8203394332039));
#55055=CARTESIAN_POINT('Ctrl Pts',(0.55975644819029,-6.74380914014546,27.829180468919));
#55056=CARTESIAN_POINT('Ctrl Pts',(0.745136131039397,-6.72842206873198,
27.8379304475323));
#55057=CARTESIAN_POINT('Ctrl Pts',(0.929880851941056,-6.70538686355779,
27.8466804261456));
#55058=CARTESIAN_POINT('Ctrl Pts',(1.11336305057062,-6.67478177303379,27.8554304047589));
#55059=CARTESIAN_POINT('Ctrl Pts',(1.29684337089742,-6.64417699581335,27.8641802937989));
#55060=CARTESIAN_POINT('Ctrl Pts',(1.47906091204828,-6.60600253548141,27.8729301828389));
#55061=CARTESIAN_POINT('Ctrl Pts',(1.65939671094879,-6.56038806441298,27.8816800718789));
#55062=CARTESIAN_POINT('Ctrl Pts',(1.83973072368831,-6.51477404513943,27.8904298742544));
#55063=CARTESIAN_POINT('Ctrl Pts',(2.01818275356719,-6.4617202328876,27.8991796766299));
#55064=CARTESIAN_POINT('Ctrl Pts',(2.19414664033022,-6.40140683918212,27.9079294790054));
#55065=CARTESIAN_POINT('Ctrl Pts',(2.37010884270947,-6.34109402281614,27.9166791976249));
#55066=CARTESIAN_POINT('Ctrl Pts',(2.54358267847486,-6.27352185699921,27.9254289162444));
#55067=CARTESIAN_POINT('Ctrl Pts',(2.71397890841415,-6.19891986435404,27.934178634864));
#55068=CARTESIAN_POINT('Ctrl Pts',(2.88437356388614,-6.12431856103397,27.9429282726358));
#55069=CARTESIAN_POINT('Ctrl Pts',(3.05169040786844,-6.04268767582723,27.9516779104076));
#55070=CARTESIAN_POINT('Ctrl Pts',(3.21536112511726,-5.95430447954122,27.9604275481794));
#55071=CARTESIAN_POINT('Ctrl Pts',(3.3790303844251,-5.86592207055234,27.9691771080115));
#55072=CARTESIAN_POINT('Ctrl Pts',(3.53905332979635,-5.77078760703584,27.9779266678435));
#55073=CARTESIAN_POINT('Ctrl Pts',(3.6948864304155,-5.66922422085521,27.9866762276756));
#55074=CARTESIAN_POINT('Ctrl Pts',(3.85071819468408,-5.56766170563389,27.9954257124756));
#55075=CARTESIAN_POINT('Ctrl Pts',(4.00235994598897,-5.45967053456491,28.0041751972756));
#55076=CARTESIAN_POINT('Ctrl Pts',(4.14929662973982,-5.34561750206932,28.0129246820756));
#55077=CARTESIAN_POINT('Ctrl Pts',(4.29623210224728,-5.23156540974726,28.0216740947509));
#55078=CARTESIAN_POINT('Ctrl Pts',(4.43846235841804,-5.11145173172458,28.0304235074263));
#55079=CARTESIAN_POINT('Ctrl Pts',(4.57550431797119,-4.98568443006845,28.0391729201016));
#55080=CARTESIAN_POINT('Ctrl Pts',(4.71254519337202,-4.85991812336973,28.0479222635595));
#55081=CARTESIAN_POINT('Ctrl Pts',(4.84439764314707,-4.72849847631384,28.0566716070174));
#55082=CARTESIAN_POINT('Ctrl Pts',(4.97061384196426,-4.59187184425625,28.0654209504753));
#55083=CARTESIAN_POINT('Ctrl Pts',(5.09682908419953,-4.45524624768036,28.0741702276227));
#55084=CARTESIAN_POINT('Ctrl Pts',(5.21740796649926,-4.31341395557189,28.0829195047701));
#55085=CARTESIAN_POINT('Ctrl Pts',(5.33194095942014,-4.16685668163159,28.0916687819174));
#55086=CARTESIAN_POINT('Ctrl Pts',(5.44647312234907,-4.0203004697552,28.100417995661));
#55087=CARTESIAN_POINT('Ctrl Pts',(5.55495930712074,-3.86901957035854,28.1091672094045));
#55088=CARTESIAN_POINT('Ctrl Pts',(5.65703106079593,-3.71352778058683,28.117916423148));
#55089=CARTESIAN_POINT('Ctrl Pts',(5.75910210868538,-3.55803706597922,28.1266655763942));
#55090=CARTESIAN_POINT('Ctrl Pts',(5.85475865698357,-3.3983357588123,28.1354147296404));
#55091=CARTESIAN_POINT('Ctrl Pts',(5.94367583068877,-3.23496624707062,28.1441638828866));
#55092=CARTESIAN_POINT('Ctrl Pts',(6.03259241909898,-3.07159781070451,28.1529129785417));
#55093=CARTESIAN_POINT('Ctrl Pts',(6.11476958470796,-2.90456146976195,28.1616620741969));
#55094=CARTESIAN_POINT('Ctrl Pts',(6.18992823574222,-2.73442451648627,28.170411169852));
#55095=CARTESIAN_POINT('Ctrl Pts',(6.26508641700778,-2.56428862662798,28.1791602108221));
#55096=CARTESIAN_POINT('Ctrl Pts',(6.33322605570147,-2.39105242531672,28.1879092517922));
#55097=CARTESIAN_POINT('Ctrl Pts',(6.39411573747626,-2.21530425354136,28.1966582927623));
#55098=CARTESIAN_POINT('Ctrl Pts',(6.45500505888992,-2.03955712188982,28.2054072819533));
#55099=CARTESIAN_POINT('Ctrl Pts',(6.50864441544805,-1.86129832026005,28.2141562711443));
#55100=CARTESIAN_POINT('Ctrl Pts',(6.55485164049792,-1.68113324012754,28.2229052603353));
#55101=CARTESIAN_POINT('Ctrl Pts',(6.60199852639014,-1.49730435913325,28.2318321672122));
#55102=CARTESIAN_POINT('Ctrl Pts',(6.6414076744093,-1.31149113174059,28.2407590740891));
#55103=CARTESIAN_POINT('Ctrl Pts',(6.67293975269537,-1.12435050446819,28.249685980966));
#55104=CARTESIAN_POINT('Ctrl Pts',(6.70384664831451,-0.940920291567684,
28.25843589515));
#55105=CARTESIAN_POINT('Ctrl Pts',(6.72718585889621,-0.756215114281942,
28.267185809334));
#55106=CARTESIAN_POINT('Ctrl Pts',(6.7428781045183,-0.5708623893792,28.275935723518));
#55107=CARTESIAN_POINT('Ctrl Pts',(6.75857004154099,-0.38551330957232,28.2846854656285));
#55108=CARTESIAN_POINT('Ctrl Pts',(6.76661529035543,-0.199516993263584,
28.2934352077391));
#55109=CARTESIAN_POINT('Ctrl Pts',(6.76698652348895,-0.013505218209579,
28.3021849498497));
#55110=CARTESIAN_POINT('Ctrl Pts',(6.76735774981535,0.172503146033357,28.3109345315204));
#55111=CARTESIAN_POINT('Ctrl Pts',(6.76005524147509,0.358526681827927,28.319684113191));
#55112=CARTESIAN_POINT('Ctrl Pts',(6.74510380214926,0.543933542109321,28.3284336948616));
#55113=CARTESIAN_POINT('Ctrl Pts',(6.73015261711039,0.729337249079217,28.3371831277236));
#55114=CARTESIAN_POINT('Ctrl Pts',(6.7075527844468,0.914124015849204,28.3459325605855));
#55115=CARTESIAN_POINT('Ctrl Pts',(6.67738106408378,1.09766621748845,28.3546819934474));
#55116=CARTESIAN_POINT('Ctrl Pts',(6.64720981677356,1.28120554142793,28.3634312891298));
#55117=CARTESIAN_POINT('Ctrl Pts',(6.60946696581638,1.46350005650103,28.3721805848121));
#55118=CARTESIAN_POINT('Ctrl Pts',(6.56428070011121,1.64393062206029,28.3809298804945));
#55119=CARTESIAN_POINT('Ctrl Pts',(6.5190950828288,1.82435859844156,28.3896790506245));
#55120=CARTESIAN_POINT('Ctrl Pts',(6.46646633415812,2.00292240086077,28.3984282207545));
#55121=CARTESIAN_POINT('Ctrl Pts',(6.40657319597354,2.17901557695978,28.4071773908845));
#55122=CARTESIAN_POINT('Ctrl Pts',(6.34668083768468,2.35510646006967,28.4159264470875));
#55123=CARTESIAN_POINT('Ctrl Pts',(6.2795243714407,2.52872650996072,28.4246755032906));
#55124=CARTESIAN_POINT('Ctrl Pts',(6.20533187335331,2.69928607997475,28.4334245594937));
#55125=CARTESIAN_POINT('Ctrl Pts',(6.12831449784455,2.87633970114966,28.4425067357825));
#55126=CARTESIAN_POINT('Ctrl Pts',(6.04371489463361,3.05009490561937,28.4515889120714));
#55127=CARTESIAN_POINT('Ctrl Pts',(5.95184265120704,3.21991584599238,28.4606710883602));
#55128=CARTESIAN_POINT('Ctrl Pts',(5.86333281335717,3.38352155904912,28.4694208687146));
#55129=CARTESIAN_POINT('Ctrl Pts',(5.7680733723592,3.54347560903441,28.4781706490691));
#55130=CARTESIAN_POINT('Ctrl Pts',(5.66638790086602,3.69923467178269,28.4869204294235));
#55131=CARTESIAN_POINT('Ctrl Pts',(5.56470608502994,3.85498813489401,28.4956698952178));
#55132=CARTESIAN_POINT('Ctrl Pts',(5.45659885767208,4.00654667255914,28.504419361012));
#55133=CARTESIAN_POINT('Ctrl Pts',(5.34243340580766,4.15339551505878,28.5131688268063));
#55134=CARTESIAN_POINT('Ctrl Pts',(5.22827145140856,4.30023985883551,28.5219180245602));
#55135=CARTESIAN_POINT('Ctrl Pts',(5.10805181978355,4.44237456992737,28.530667222314));
#55136=CARTESIAN_POINT('Ctrl Pts',(4.9821828128282,4.57931691626157,28.5394164200679));
#55137=CARTESIAN_POINT('Ctrl Pts',(4.85631699296501,4.71625579511881,28.5481653962859));
#55138=CARTESIAN_POINT('Ctrl Pts',(4.72480227792113,4.84800236135502,28.5569143725039));
#55139=CARTESIAN_POINT('Ctrl Pts',(4.58808530848391,4.97410918678653,28.5656633487219));
#55140=CARTESIAN_POINT('Ctrl Pts',(4.4513594505726,5.10022421088756,28.5744128937431));
#55141=CARTESIAN_POINT('Ctrl Pts',(4.30943087208342,5.22069856611737,28.5831624387643));
#55142=CARTESIAN_POINT('Ctrl Pts',(4.16278164322782,5.33512305301438,28.5919119837855));
#55143=CARTESIAN_POINT('Ctrl Pts',(4.01614103534699,5.449540813312,28.6006610144528));
#55144=CARTESIAN_POINT('Ctrl Pts',(3.86478055833715,5.55790924068128,28.6094100451201));
#55145=CARTESIAN_POINT('Ctrl Pts',(3.70921425812245,5.65986029751098,28.6181590757873));
#55146=CARTESIAN_POINT('Ctrl Pts',(3.55364584530423,5.76181273884466,28.6269082252672));
#55147=CARTESIAN_POINT('Ctrl Pts',(3.39387173464657,5.85734747817882,28.635657374747));
#55148=CARTESIAN_POINT('Ctrl Pts',(3.23043456092727,5.94614005448632,28.6444065242269));
#55149=CARTESIAN_POINT('Ctrl Pts',(3.18690768806603,5.9697874481117,28.64673661296));
#55150=CARTESIAN_POINT('Ctrl Pts',(3.1431211498298,5.9929568849925,28.6490667016931));
#55151=CARTESIAN_POINT('Ctrl Pts',(3.09908550384705,6.0156427786102,28.6513967904262));
#55152=CARTESIAN_POINT('Origin',(0.,0.,-63.6971797838103));
#55153=CARTESIAN_POINT('',(3.09908550384736,6.01564277861005,31.0457633158951));
#55154=CARTESIAN_POINT('',(3.09908550384718,6.01564277861014,30.6513967904261));
#55155=CARTESIAN_POINT('',(3.09908550384721,6.01564277861012,-63.6971797838103));
#55156=CARTESIAN_POINT('',(-6.76829295411965,-0.00242009354003358,29.6949426053424));
#55157=CARTESIAN_POINT('Ctrl Pts',(-6.7669982393656,-0.00488143655476046,
29.6971797838099));
#55158=CARTESIAN_POINT('Ctrl Pts',(-6.76685599634114,-0.20206894176599,
29.7064249492294));
#55159=CARTESIAN_POINT('Ctrl Pts',(-6.75809085851693,-0.398938330293628,
29.715670114649));
#55160=CARTESIAN_POINT('Ctrl Pts',(-6.74080995914764,-0.59478575525652,
29.7249152800685));
#55161=CARTESIAN_POINT('Ctrl Pts',(-6.72341233013775,-0.791956097449425,
29.7342228950639));
#55162=CARTESIAN_POINT('Ctrl Pts',(-6.69738357825563,-0.988090451151311,
29.7435305100593));
#55163=CARTESIAN_POINT('Ctrl Pts',(-6.6628831636456,-1.18248760991732,29.7528381250547));
#55164=CARTESIAN_POINT('Ctrl Pts',(-6.62827458067607,-1.3774942576415,29.7621749220022));
#55165=CARTESIAN_POINT('Ctrl Pts',(-6.58514122922429,-1.57075264470449,
29.7715117189497));
#55166=CARTESIAN_POINT('Ctrl Pts',(-6.53369301835144,-1.76157444973117,
29.7808485158971));
#55167=CARTESIAN_POINT('Ctrl Pts',(-6.48202976119589,-1.95319386305431,
29.7902243393422));
#55168=CARTESIAN_POINT('Ctrl Pts',(-6.4219820771575,-2.14235612770112,29.7996001627872));
#55169=CARTESIAN_POINT('Ctrl Pts',(-6.35381039694746,-2.32838623077066,
29.8089759862322));
#55170=CARTESIAN_POINT('Ctrl Pts',(-6.29103291597426,-2.4996963880076,29.8176099318254));
#55171=CARTESIAN_POINT('Ctrl Pts',(-6.22136680736831,-2.66835060517495,
29.8262438774186));
#55172=CARTESIAN_POINT('Ctrl Pts',(-6.14505012808121,-2.83383978435076,
29.8348778230117));
#55173=CARTESIAN_POINT('Ctrl Pts',(-6.07370575265772,-2.98854675323271,
29.8429492362537));
#55174=CARTESIAN_POINT('Ctrl Pts',(-5.99638391577799,-3.14084231455015,
29.8510206494958));
#55175=CARTESIAN_POINT('Ctrl Pts',(-5.91326881104139,-3.29021898486487,
29.8590920627378));
#55176=CARTESIAN_POINT('Ctrl Pts',(-5.83025805043447,-3.43940812514268,
29.867153342989));
#55177=CARTESIAN_POINT('Ctrl Pts',(-5.74146867235082,-3.58568534391104,
29.8752146232402));
#55178=CARTESIAN_POINT('Ctrl Pts',(-5.64713329442595,-3.72856199559374,
29.8832759034915));
#55179=CARTESIAN_POINT('Ctrl Pts',(-5.55289565856978,-3.87129061098495,
29.8913288313491));
#55180=CARTESIAN_POINT('Ctrl Pts',(-5.45312366189551,-4.01062536229669,
29.8993817592067));
#55181=CARTESIAN_POINT('Ctrl Pts',(-5.34809625418465,-4.14610123561595,
29.9074346870644));
#55182=CARTESIAN_POINT('Ctrl Pts',(-5.24315466809728,-4.28146640678951,
29.9154810345887));
#55183=CARTESIAN_POINT('Ctrl Pts',(-5.13296644561109,-4.41297868270579,
29.9235273821131));
#55184=CARTESIAN_POINT('Ctrl Pts',(-5.01785429461257,-4.54020123761472,
29.9315737296375));
#55185=CARTESIAN_POINT('Ctrl Pts',(-4.90281102524929,-4.66734766417798,
29.9396152623306));
#55186=CARTESIAN_POINT('Ctrl Pts',(-4.78284994244122,-4.79020920385607,
29.9476567950239));
#55187=CARTESIAN_POINT('Ctrl Pts',(-4.65833448314634,-4.90838148916012,
29.9556983277171));
#55188=CARTESIAN_POINT('Ctrl Pts',(-4.53142524683287,-5.02882560562792,
29.9638944567653));
#55189=CARTESIAN_POINT('Ctrl Pts',(-4.39978498217611,-5.14439802142215,
29.9720905858135));
#55190=CARTESIAN_POINT('Ctrl Pts',(-4.263838812226,-5.25470908646284,29.9802867148617));
#55191=CARTESIAN_POINT('Ctrl Pts',(-4.13050291712297,-5.3629020911085,29.9883254716978));
#55192=CARTESIAN_POINT('Ctrl Pts',(-3.99302528617483,-5.46603373152687,
29.9963642285339));
#55193=CARTESIAN_POINT('Ctrl Pts',(-3.8518409479282,-5.56377662310985,30.00440298537));
#55194=CARTESIAN_POINT('Ctrl Pts',(-3.71064294452981,-5.66152897517168,
30.0124425202728));
#55195=CARTESIAN_POINT('Ctrl Pts',(-3.56573782647819,-5.75389132716835,
30.0204820551756));
#55196=CARTESIAN_POINT('Ctrl Pts',(-3.41758986525397,-5.84057946722013,
30.0285215900784));
#55197=CARTESIAN_POINT('Ctrl Pts',(-3.26939823152485,-5.92729316204965,
30.036563494954));
#55198=CARTESIAN_POINT('Ctrl Pts',(-3.11796217398246,-6.00832912695545,
30.0446053998295));
#55199=CARTESIAN_POINT('Ctrl Pts',(-2.96377068943838,-6.08344904642309,
30.052647304705));
#55200=CARTESIAN_POINT('Ctrl Pts',(-2.80437797421315,-6.16110293221873,
30.0609604813858));
#55201=CARTESIAN_POINT('Ctrl Pts',(-2.64204107909781,-6.23243447639111,
30.0692736580666));
#55202=CARTESIAN_POINT('Ctrl Pts',(-2.4773216746203,-6.29723481541355,30.0775868347474));
#55203=CARTESIAN_POINT('Ctrl Pts',(-2.31770065773291,-6.3600294572605,30.085642702358));
#55204=CARTESIAN_POINT('Ctrl Pts',(-2.15584279267876,-6.41669112472147,
30.0936985699685));
#55205=CARTESIAN_POINT('Ctrl Pts',(-1.9922732365107,-6.46708097607284,30.101754437579));
#55206=CARTESIAN_POINT('Ctrl Pts',(-1.82086692101523,-6.51988504891404,
30.110196268795));
#55207=CARTESIAN_POINT('Ctrl Pts',(-1.64758133181649,-6.56580141985971,
30.118638100011));
#55208=CARTESIAN_POINT('Ctrl Pts',(-1.47303040899556,-6.60473091156441,
30.1270799312269));
#55209=CARTESIAN_POINT('Ctrl Pts',(-1.29847948617462,-6.6436604032691,30.1355217624429));
#55210=CARTESIAN_POINT('Ctrl Pts',(-1.12266369870626,-6.67560301751157,
30.1439635936588));
#55211=CARTESIAN_POINT('Ctrl Pts',(-0.94619989704853,-6.70052197629598,
30.1524054248748));
#55212=CARTESIAN_POINT('Ctrl Pts',(-0.774154575396528,-6.72481698886525,
30.1606358809414));
#55213=CARTESIAN_POINT('Ctrl Pts',(-0.600921132677589,-6.742517045862,30.1688663370079));
#55214=CARTESIAN_POINT('Ctrl Pts',(-0.427046353577607,-6.7535117096142,
30.1770967930745));
#55215=CARTESIAN_POINT('Ctrl Pts',(-0.253377974086122,-6.76449332205266,
30.1853174791047));
#55216=CARTESIAN_POINT('Ctrl Pts',(-0.0790701284325291,-6.76878536837594,
30.1935381651349));
#55217=CARTESIAN_POINT('Ctrl Pts',(0.0953214214695674,-6.76632860764307,
30.2017588511652));
#55218=CARTESIAN_POINT('Ctrl Pts',(0.269540946664971,-6.76387427032776,
30.2099714280805));
#55219=CARTESIAN_POINT('Ctrl Pts',(0.443843655654126,-6.75468438873625,
30.2181840049959));
#55220=CARTESIAN_POINT('Ctrl Pts',(0.617669798945825,-6.73875159205845,
30.2263965819113));
#55221=CARTESIAN_POINT('Ctrl Pts',(0.791359337635991,-6.72283131647384,
30.234602704816));
#55222=CARTESIAN_POINT('Ctrl Pts',(0.96457270116618,-6.70017871290767,30.2428088277206));
#55223=CARTESIAN_POINT('Ctrl Pts',(1.13675118480139,-6.67083845883354,30.2510149506253));
#55224=CARTESIAN_POINT('Ctrl Pts',(1.30882888172884,-6.64151537942346,30.259216269979));
#55225=CARTESIAN_POINT('Ctrl Pts',(1.47987255306294,-6.60551250809738,30.2674175893327));
#55226=CARTESIAN_POINT('Ctrl Pts',(1.64932956449011,-6.56292625188634,30.2756189086865));
#55227=CARTESIAN_POINT('Ctrl Pts',(1.81873796271549,-6.52035221266325,30.283817875276));
#55228=CARTESIAN_POINT('Ctrl Pts',(1.98656025945274,-6.47119863388872,30.2920168418655));
#55229=CARTESIAN_POINT('Ctrl Pts',(2.15225470193199,-6.41561288561051,30.300215808455));
#55230=CARTESIAN_POINT('Ctrl Pts',(2.31792726371152,-6.3600344776815,30.308413692334));
#55231=CARTESIAN_POINT('Ctrl Pts',(2.48147219072227,-6.29802570518288,30.3166115762129));
#55232=CARTESIAN_POINT('Ctrl Pts',(2.64236356024418,-6.22978360904243,30.3248094600919));
#55233=CARTESIAN_POINT('Ctrl Pts',(2.80326290971407,-6.16153812820596,30.3330077505724));
#55234=CARTESIAN_POINT('Ctrl Pts',(2.96150810930629,-6.08705884780282,30.3412060410529));
#55235=CARTESIAN_POINT('Ctrl Pts',(3.11659381819117,-6.00659071124483,30.3494043315335));
#55236=CARTESIAN_POINT('Ctrl Pts',(3.27171539076207,-5.92610396637015,30.3576045178748));
#55237=CARTESIAN_POINT('Ctrl Pts',(3.42367569916727,-5.8396257721012,30.3658047042161));
#55238=CARTESIAN_POINT('Ctrl Pts',(3.57199453607082,-5.74744674044747,30.3740048905575));
#55239=CARTESIAN_POINT('Ctrl Pts',(3.7204535967971,-5.65518056075196,30.3822128295316));
#55240=CARTESIAN_POINT('Ctrl Pts',(3.8652640028644,-5.55720296520223,30.3904207685057));
#55241=CARTESIAN_POINT('Ctrl Pts',(4.0059742741666,-5.45384810154402,30.3986287074798));
#55242=CARTESIAN_POINT('Ctrl Pts',(4.14675280828444,-5.35044309731018,30.4068406283738));
#55243=CARTESIAN_POINT('Ctrl Pts',(4.28342696142729,-5.24165584706851,30.4150525492677));
#55244=CARTESIAN_POINT('Ctrl Pts',(4.41557891651402,-5.12786035613656,30.4232644701617));
#55245=CARTESIAN_POINT('Ctrl Pts',(4.54791209707177,-5.01390881271615,30.4314876524042));
#55246=CARTESIAN_POINT('Ctrl Pts',(4.67571042355632,-4.89493554747051,30.4397108346468));
#55247=CARTESIAN_POINT('Ctrl Pts',(4.79859261712912,-4.77135178904615,30.4479340168894));
#55248=CARTESIAN_POINT('Ctrl Pts',(4.90817252212099,-4.66114626526002,30.4552670201722));
#55249=CARTESIAN_POINT('Ctrl Pts',(5.01384347551547,-4.54727504101347,30.462600023455));
#55250=CARTESIAN_POINT('Ctrl Pts',(5.11536292965119,-4.43005091369732,30.4699330267378));
#55251=CARTESIAN_POINT('Ctrl Pts',(5.23906330857525,-4.28721455694677,30.4788682135201));
#55252=CARTESIAN_POINT('Ctrl Pts',(5.35685635282951,-4.13910351529673,30.4878034003024));
#55253=CARTESIAN_POINT('Ctrl Pts',(5.46831113383627,-3.98620901905084,30.4967385870846));
#55254=CARTESIAN_POINT('Ctrl Pts',(5.5795989900604,-3.83354351146136,30.5056603917213));
#55255=CARTESIAN_POINT('Ctrl Pts',(5.68456737255042,-3.67610905247899,30.5145821963579));
#55256=CARTESIAN_POINT('Ctrl Pts',(5.78282577957969,-3.51442954162244,30.5235040009946));
#55257=CARTESIAN_POINT('Ctrl Pts',(5.88084451105185,-3.35314440543581,30.5324040432338));
#55258=CARTESIAN_POINT('Ctrl Pts',(5.97218579932985,-3.18763510392477,30.5413040854731));
#55259=CARTESIAN_POINT('Ctrl Pts',(6.05650289291878,-3.01845352922096,30.5502041277124));
#55260=CARTESIAN_POINT('Ctrl Pts',(6.14069017910248,-2.84953241203875,30.5590904682058));
#55261=CARTESIAN_POINT('Ctrl Pts',(6.21787472676923,-2.67695052902459,30.5679768086992));
#55262=CARTESIAN_POINT('Ctrl Pts',(6.28775458985052,-2.50128591284838,30.5768631491926));
#55263=CARTESIAN_POINT('Ctrl Pts',(6.3574557823198,-2.32607044043254,30.5857267688646));
#55264=CARTESIAN_POINT('Ctrl Pts',(6.41988946340562,-2.14778820223259,30.5945903885365));
#55265=CARTESIAN_POINT('Ctrl Pts',(6.47480115604427,-1.96703812613985,30.6034540082084));
#55266=CARTESIAN_POINT('Ctrl Pts',(6.52692906747278,-1.79545128362051,30.6118682813621));
#55267=CARTESIAN_POINT('Ctrl Pts',(6.57227855714262,-1.62164082876767,30.6202825545158));
#55268=CARTESIAN_POINT('Ctrl Pts',(6.61067131476496,-1.4461375343112,30.6286968276695));
#55269=CARTESIAN_POINT('Ctrl Pts',(6.6481331446317,-1.27488975308507,30.6369070758741));
#55270=CARTESIAN_POINT('Ctrl Pts',(6.67893452146936,-1.10219459339382,30.6451173240786));
#55271=CARTESIAN_POINT('Ctrl Pts',(6.70298249497128,-0.928608998507214,
30.6533275722831));
#55272=CARTESIAN_POINT('Ctrl Pts',(6.72703618515591,-0.754982138864243,
30.6615397722274));
#55273=CARTESIAN_POINT('Ctrl Pts',(6.74433322470396,-0.580464774897712,
30.6697519721716));
#55274=CARTESIAN_POINT('Ctrl Pts',(6.75483246138537,-0.405619795639249,
30.6779641721158));
#55275=CARTESIAN_POINT('Ctrl Pts',(6.76533606356442,-0.230702117253558,
30.6861797866263));
#55276=CARTESIAN_POINT('Ctrl Pts',(6.76903621060775,-0.0554569072121219,
30.6943954011368));
#55277=CARTESIAN_POINT('Ctrl Pts',(6.76594385974772,0.119552025253029,30.7026110156472));
#55278=CARTESIAN_POINT('Ctrl Pts',(6.76284803631324,0.294757485077517,30.7108358559327));
#55279=CARTESIAN_POINT('Ctrl Pts',(6.75294448632581,0.469725781350313,30.7190606962181));
#55280=CARTESIAN_POINT('Ctrl Pts',(6.73629620173029,0.643896329042222,30.7272855365035));
#55281=CARTESIAN_POINT('Ctrl Pts',(6.71963725332978,0.818178439024317,30.7355156450851));
#55282=CARTESIAN_POINT('Ctrl Pts',(6.69622500562402,0.991661429965108,30.7437457536666));
#55283=CARTESIAN_POINT('Ctrl Pts',(6.66617374553966,1.1637940514875,30.7519758622481));
#55284=CARTESIAN_POINT('Ctrl Pts',(6.63608128471658,1.33616266947545,30.7602172544348));
#55285=CARTESIAN_POINT('Ctrl Pts',(6.59933170541764,1.50717687313839,30.7684586466215));
#55286=CARTESIAN_POINT('Ctrl Pts',(6.55608964980781,1.67629875132178,30.7767000388082));
#55287=CARTESIAN_POINT('Ctrl Pts',(6.53726960857914,1.74990488949431,30.7802869020724));
#55288=CARTESIAN_POINT('Ctrl Pts',(6.51722038263344,1.82315281110361,30.7838737653366));
#55289=CARTESIAN_POINT('Ctrl Pts',(6.49595839816831,1.89599933788665,30.7874606286008));
#55290=CARTESIAN_POINT('Ctrl Pts',(6.44587287868093,2.06759931919429,30.795909976789));
#55291=CARTESIAN_POINT('Ctrl Pts',(6.3889402599342,2.23736201625861,30.8043593249772));
#55292=CARTESIAN_POINT('Ctrl Pts',(6.32531449620336,2.40472150656156,30.8128086731654));
#55293=CARTESIAN_POINT('Ctrl Pts',(6.26174807036031,2.57192491608725,30.821250141425));
#55294=CARTESIAN_POINT('Ctrl Pts',(6.19150106064262,2.73672927628151,30.8296916096846));
#55295=CARTESIAN_POINT('Ctrl Pts',(6.11477715678058,2.89858402033034,30.8381330779442));
#55296=CARTESIAN_POINT('Ctrl Pts',(6.03614647150604,3.06446126065405,30.8467843378588));
#55297=CARTESIAN_POINT('Ctrl Pts',(5.95071286114916,3.22724002553104,30.8554355977734));
#55298=CARTESIAN_POINT('Ctrl Pts',(5.85874871527526,3.38634795779472,30.8640868576881));
#55299=CARTESIAN_POINT('Ctrl Pts',(5.76914969626247,3.5413639644407,30.8725156251627));
#55300=CARTESIAN_POINT('Ctrl Pts',(5.67335207946818,3.6928953121624,30.8809443926373));
#55301=CARTESIAN_POINT('Ctrl Pts',(5.57165496922936,3.84043616062835,30.8893731601119));
#55302=CARTESIAN_POINT('Ctrl Pts',(5.4699998891518,3.98791603228148,30.8977984440809));
#55303=CARTESIAN_POINT('Ctrl Pts',(5.36245036500796,4.13140841832292,30.90622372805));
#55304=CARTESIAN_POINT('Ctrl Pts',(5.24934929153977,4.27043569386204,30.914649012019));
#55305=CARTESIAN_POINT('Ctrl Pts',(5.13627918007783,4.40942490996244,30.9230719895227));
#55306=CARTESIAN_POINT('Ctrl Pts',(5.01766075978946,4.54395119445761,30.9314949670265));
#55307=CARTESIAN_POINT('Ctrl Pts',(4.89387797507892,4.67356901789601,30.9399179445303));
#55308=CARTESIAN_POINT('Ctrl Pts',(4.76425403063248,4.80930334948289,30.948738392144));
#55309=CARTESIAN_POINT('Ctrl Pts',(4.62896675170893,4.93965443927406,30.9575588397578));
#55310=CARTESIAN_POINT('Ctrl Pts',(4.48850180617996,5.06415249927559,30.9663792873715));
#55311=CARTESIAN_POINT('Ctrl Pts',(4.3543598826087,5.18304628581148,30.974802683011));
#55312=CARTESIAN_POINT('Ctrl Pts',(4.21549649140343,5.29660220907103,30.9832260786504));
#55313=CARTESIAN_POINT('Ctrl Pts',(4.07236987403007,5.40445118481908,30.9916494742899));
#55314=CARTESIAN_POINT('Ctrl Pts',(3.92922778921737,5.5123118156144,31.0000737802307));
#55315=CARTESIAN_POINT('Ctrl Pts',(3.78182182859266,5.6144640722578,31.0084980861716));
#55316=CARTESIAN_POINT('Ctrl Pts',(3.63064085309637,5.71058105588456,31.0169223921125));
#55317=CARTESIAN_POINT('Ctrl Pts',(3.47939478624575,5.80673942292362,31.0253503251598));
#55318=CARTESIAN_POINT('Ctrl Pts',(3.32437074210901,5.89685715225192,31.033778258207));
#55319=CARTESIAN_POINT('Ctrl Pts',(3.16608450050147,5.98065196577132,31.0422061912543));
#55320=CARTESIAN_POINT('Ctrl Pts',(3.14381554134836,5.99244088223402,31.0433918994679));
#55321=CARTESIAN_POINT('Ctrl Pts',(3.12148205153332,6.00410472377132,31.0445776076815));
#55322=CARTESIAN_POINT('Ctrl Pts',(3.09908550384736,6.01564277861005,31.0457633158951));
#55323=CARTESIAN_POINT('Ctrl Pts',(3.09908550384738,6.01564277861003,29.0457563580462));
#55324=CARTESIAN_POINT('Ctrl Pts',(2.9337323201834,6.10082796552475,29.0545058059455));
#55325=CARTESIAN_POINT('Ctrl Pts',(2.7648650214443,6.17919158180189,29.0632552538448));
#55326=CARTESIAN_POINT('Ctrl Pts',(2.59305716434349,6.2504674659138,29.0720047017441));
#55327=CARTESIAN_POINT('Ctrl Pts',(2.42125069459278,6.32174277447227,29.0807540789915));
#55328=CARTESIAN_POINT('Ctrl Pts',(2.24650397871052,6.38593035557828,29.089503456239));
#55329=CARTESIAN_POINT('Ctrl Pts',(2.06941053323763,6.44281220003541,29.0982528334864));
#55330=CARTESIAN_POINT('Ctrl Pts',(1.89231845896674,6.49969360406688,29.107002142989));
#55331=CARTESIAN_POINT('Ctrl Pts',(1.71287996431495,6.54926929700883,29.1157514524916));
#55332=CARTESIAN_POINT('Ctrl Pts',(1.53170449173493,6.59137090065481,29.1245007619942));
#55333=CARTESIAN_POINT('Ctrl Pts',(1.35053036178147,6.63347219230088,29.1332500066588));
#55334=CARTESIAN_POINT('Ctrl Pts',(1.16761955878808,6.66809944062461,29.1419992513234));
#55335=CARTESIAN_POINT('Ctrl Pts',(0.983593309309987,6.69513503985399,29.150748495988));
#55336=CARTESIAN_POINT('Ctrl Pts',(0.799568362459552,6.72217044771219,29.1594976787211));
#55337=CARTESIAN_POINT('Ctrl Pts',(0.614428268438235,6.7416142723598,29.1682468614543));
#55338=CARTESIAN_POINT('Ctrl Pts',(0.42880181632998,6.75340047696804,29.1769960441875));
#55339=CARTESIAN_POINT('Ctrl Pts',(0.243176616522413,6.76518660206243,29.1857451678956));
#55340=CARTESIAN_POINT('Ctrl Pts',(0.0570653511650086,6.76931519233997,
29.1944942916037));
#55341=CARTESIAN_POINT('Ctrl Pts',(-0.128899900800564,6.76577222610794,
29.2032434153119));
#55342=CARTESIAN_POINT('Ctrl Pts',(-0.314863959942571,6.76222928260131,
29.2119924829011));
#55343=CARTESIAN_POINT('Ctrl Pts',(-0.500681721081245,6.75101488651272,
29.2207415504904));
#55344=CARTESIAN_POINT('Ctrl Pts',(-0.685722110173877,6.73216712415985,
29.2294906180797));
#55345=CARTESIAN_POINT('Ctrl Pts',(-0.870761373828091,6.71331947644139,
29.238239632456));
#55346=CARTESIAN_POINT('Ctrl Pts',(-1.05502298984381,6.6868385843999,29.2469886468324));
#55347=CARTESIAN_POINT('Ctrl Pts',(-1.23788117676088,6.65281438131421,29.2557376612087));
#55348=CARTESIAN_POINT('Ctrl Pts',(-1.43009641451812,6.61704912302373,29.2649343720962));
#55349=CARTESIAN_POINT('Ctrl Pts',(-1.62076048992706,6.57294837083162,29.2741310829838));
#55350=CARTESIAN_POINT('Ctrl Pts',(-1.80915798961134,6.52067760042049,29.2833277938713));
#55351=CARTESIAN_POINT('Ctrl Pts',(-1.98840443003017,6.47094578577408,29.2920777915778));
#55352=CARTESIAN_POINT('Ctrl Pts',(-2.16559895952199,6.41381888474473,29.3008277892843));
#55353=CARTESIAN_POINT('Ctrl Pts',(-2.34013966242332,6.3494909528523,29.3095777869908));
#55354=CARTESIAN_POINT('Ctrl Pts',(-2.51467682554025,6.28516432556681,29.3183276072424));
#55355=CARTESIAN_POINT('Ctrl Pts',(-2.68656000078853,6.21363705879656,29.327077427494));
#55356=CARTESIAN_POINT('Ctrl Pts',(-2.855205338409,6.13515211510854,29.3358272477456));
#55357=CARTESIAN_POINT('Ctrl Pts',(-3.02384747998346,6.05666865881112,29.3445769021769));
#55358=CARTESIAN_POINT('Ctrl Pts',(-3.18925164684563,5.9712279103983,29.3533265566081));
#55359=CARTESIAN_POINT('Ctrl Pts',(-3.35085601829191,5.87912008251889,29.3620762110394));
#55360=CARTESIAN_POINT('Ctrl Pts',(-3.51245754191456,5.78701387778151,29.3708257112825));
#55361=CARTESIAN_POINT('Ctrl Pts',(-3.67025915510978,5.68824097060956,29.3795752115256));
#55362=CARTESIAN_POINT('Ctrl Pts',(-3.8237248792888,5.58313684656823,29.3883247117688));
#55363=CARTESIAN_POINT('Ctrl Pts',(-3.97718810300842,5.47803443501741,29.3970740694539));
#55364=CARTESIAN_POINT('Ctrl Pts',(-4.12631534263068,5.36660117496343,29.405823427139));
#55365=CARTESIAN_POINT('Ctrl Pts',(-4.27060009886266,5.24921554097317,29.4145727848241));
#55366=CARTESIAN_POINT('Ctrl Pts',(-4.41488269594253,5.13183166360257,29.4233220115793));
#55367=CARTESIAN_POINT('Ctrl Pts',(-4.55432273235127,5.00849577139435,29.4320712383345));
#55368=CARTESIAN_POINT('Ctrl Pts',(-4.68844662480245,4.87962675277306,29.4408204650897));
#55369=CARTESIAN_POINT('Ctrl Pts',(-4.82256868835186,4.75075949139853,29.4495695725412));
#55370=CARTESIAN_POINT('Ctrl Pts',(-4.95137454637881,4.61635945312505,29.4583186799927));
#55371=CARTESIAN_POINT('Ctrl Pts',(-5.07442674461088,4.47688309134579,29.4670677874442));
#55372=CARTESIAN_POINT('Ctrl Pts',(-5.19747742838547,4.33740844616341,29.4758167872165));
#55373=CARTESIAN_POINT('Ctrl Pts',(-5.31477440450934,4.1928578173602,29.4845657869889));
#55374=CARTESIAN_POINT('Ctrl Pts',(-5.42591931531158,4.04372211999399,29.4933147867613));
#55375=CARTESIAN_POINT('Ctrl Pts',(-5.5370763646299,3.8945701350079,29.5020647420418));
#55376=CARTESIAN_POINT('Ctrl Pts',(-5.64207983273481,3.74083230916404,29.5108146973224));
#55377=CARTESIAN_POINT('Ctrl Pts',(-5.7405730346876,3.58303087251806,29.519564652603));
#55378=CARTESIAN_POINT('Ctrl Pts',(-5.83906243363776,3.42523552887413,29.5283142700318));
#55379=CARTESIAN_POINT('Ctrl Pts',(-5.93104191768434,3.26337713156978,29.5370638874606));
#55380=CARTESIAN_POINT('Ctrl Pts',(-6.01619906699662,3.09800545291144,29.5458135048894));
#55381=CARTESIAN_POINT('Ctrl Pts',(-6.10135338095391,2.93263928039579,29.5545628309948));
#55382=CARTESIAN_POINT('Ctrl Pts',(-6.17968568352848,2.76376031540203,29.5633121571002));
#55383=CARTESIAN_POINT('Ctrl Pts',(-6.25092992694897,2.59194213831516,29.5720614832056));
#55384=CARTESIAN_POINT('Ctrl Pts',(-6.32217217691122,2.42012876880773,29.5808105644994));
#55385=CARTESIAN_POINT('Ctrl Pts',(-6.38632665483874,2.24537661647603,29.5895596457932));
#55386=CARTESIAN_POINT('Ctrl Pts',(-6.44317547869378,2.06827917621368,29.598308727087));
#55387=CARTESIAN_POINT('Ctrl Pts',(-6.50002944235958,1.89116572423345,29.607058599402));
#55388=CARTESIAN_POINT('Ctrl Pts',(-6.54957634250415,1.71170683289131,29.6158084717169));
#55389=CARTESIAN_POINT('Ctrl Pts',(-6.59164787708408,1.53051209225308,29.6245583440319));
#55390=CARTESIAN_POINT('Ctrl Pts',(-6.63371649075019,1.3493299314798,29.6333076088667));
#55391=CARTESIAN_POINT('Ctrl Pts',(-6.66831071257131,1.16641244173959,29.6420568737015));
#55392=CARTESIAN_POINT('Ctrl Pts',(-6.69531304840338,0.982380875159628,
29.6508061385363));
#55393=CARTESIAN_POINT('Ctrl Pts',(-6.72231677033048,0.798339861795456,
29.6595558524919));
#55394=CARTESIAN_POINT('Ctrl Pts',(-6.74172778477893,0.613184940729765,
29.6683055664476));
#55395=CARTESIAN_POINT('Ctrl Pts',(-6.7534801583552,0.427545027690162,29.6770552804032));
#55396=CARTESIAN_POINT('Ctrl Pts',(-6.76249038365213,0.285219953548068,
29.6837634482055));
#55397=CARTESIAN_POINT('Ctrl Pts',(-6.76699999999991,0.142609995760195,
29.6904716160077));
#55398=CARTESIAN_POINT('Ctrl Pts',(-6.767,4.44901934821046E-12,29.6971797838099));
#55399=CARTESIAN_POINT('',(-6.767,9.60786626183482E-10,29.3028202161448));
#55400=CARTESIAN_POINT('Ctrl Pts',(3.09908550384705,6.0156427786102,28.6513967904262));
#55401=CARTESIAN_POINT('Ctrl Pts',(2.93373232018317,6.10082796552485,28.6601462383254));
#55402=CARTESIAN_POINT('Ctrl Pts',(2.76486502144419,6.17919158180193,28.6688956862247));
#55403=CARTESIAN_POINT('Ctrl Pts',(2.5930571643435,6.2504674659138,28.677645134124));
#55404=CARTESIAN_POINT('Ctrl Pts',(2.4212506945929,6.32174277447221,28.6863945113714));
#55405=CARTESIAN_POINT('Ctrl Pts',(2.24650397871076,6.38593035557819,28.6951438886188));
#55406=CARTESIAN_POINT('Ctrl Pts',(2.06941053323799,6.4428122000353,28.7038932658663));
#55407=CARTESIAN_POINT('Ctrl Pts',(1.89231845896711,6.49969360406677,28.7126425753689));
#55408=CARTESIAN_POINT('Ctrl Pts',(1.71287996431532,6.54926929700874,28.7213918848714));
#55409=CARTESIAN_POINT('Ctrl Pts',(1.5317044917353,6.59137090065473,28.730141194374));
#55410=CARTESIAN_POINT('Ctrl Pts',(1.35053036178209,6.63347219230075,28.7388904390386));
#55411=CARTESIAN_POINT('Ctrl Pts',(1.16761955878895,6.66809944062445,28.7476396837032));
#55412=CARTESIAN_POINT('Ctrl Pts',(0.983593309311117,6.69513503985382,28.7563889283678));
#55413=CARTESIAN_POINT('Ctrl Pts',(0.799568362460557,6.72217044771208,28.765138111101));
#55414=CARTESIAN_POINT('Ctrl Pts',(0.614428268439116,6.74161427235972,28.7738872938342));
#55415=CARTESIAN_POINT('Ctrl Pts',(0.428801816330733,6.75340047696799,28.7826364765673));
#55416=CARTESIAN_POINT('Ctrl Pts',(0.243176616523421,6.76518660206239,28.7913856002755));
#55417=CARTESIAN_POINT('Ctrl Pts',(0.057065351166272,6.76931519233996,28.8001347239836));
#55418=CARTESIAN_POINT('Ctrl Pts',(-0.128899900799046,6.76577222610797,
28.8088838476917));
#55419=CARTESIAN_POINT('Ctrl Pts',(-0.314863959940799,6.76222928260138,
28.817632915281));
#55420=CARTESIAN_POINT('Ctrl Pts',(-0.500681721079224,6.75101488651287,
28.8263819828702));
#55421=CARTESIAN_POINT('Ctrl Pts',(-0.685722110171609,6.73216712416008,
28.8351310504595));
#55422=CARTESIAN_POINT('Ctrl Pts',(-0.870761373825832,6.71331947644168,
28.8438800648358));
#55423=CARTESIAN_POINT('Ctrl Pts',(-1.05502298984156,6.68683858440026,28.8526290792122));
#55424=CARTESIAN_POINT('Ctrl Pts',(-1.23788117675864,6.65281438131462,28.8613780935885));
#55425=CARTESIAN_POINT('Ctrl Pts',(-1.43009641449636,6.61704912302784,28.8705748044751));
#55426=CARTESIAN_POINT('Ctrl Pts',(-1.62076048988609,6.57294837084113,28.8797715153617));
#55427=CARTESIAN_POINT('Ctrl Pts',(-1.8091579895517,6.52067760043703,28.8889682262483));
#55428=CARTESIAN_POINT('Ctrl Pts',(-1.98840442997098,6.47094578579226,28.8977182239548));
#55429=CARTESIAN_POINT('Ctrl Pts',(-2.16559895946333,6.41381888476454,28.9064682216613));
#55430=CARTESIAN_POINT('Ctrl Pts',(-2.34013966236525,6.34949095287371,28.9152182193678));
#55431=CARTESIAN_POINT('Ctrl Pts',(-2.51467682548265,6.28516432558985,28.9239680396194));
#55432=CARTESIAN_POINT('Ctrl Pts',(-2.68656000073147,6.21363705882123,28.932717859871));
#55433=CARTESIAN_POINT('Ctrl Pts',(-2.85520533835254,6.13515211513481,28.9414676801226));
#55434=CARTESIAN_POINT('Ctrl Pts',(-3.02384747992761,6.056668658839,28.9502173345538));
#55435=CARTESIAN_POINT('Ctrl Pts',(-3.18925164679046,5.97122791042776,28.9589669889851));
#55436=CARTESIAN_POINT('Ctrl Pts',(-3.35085601823748,5.87912008254991,28.9677166434163));
#55437=CARTESIAN_POINT('Ctrl Pts',(-3.51245754186099,5.78701387781403,28.9764661436595));
#55438=CARTESIAN_POINT('Ctrl Pts',(-3.67025915505712,5.68824097064353,28.9852156439026));
#55439=CARTESIAN_POINT('Ctrl Pts',(-3.82372487923712,5.58313684660363,28.9939651441457));
#55440=CARTESIAN_POINT('Ctrl Pts',(-3.97718810295761,5.4780344350543,29.0027145018308));
#55441=CARTESIAN_POINT('Ctrl Pts',(-4.1263153425808,5.36660117500178,29.011463859516));
#55442=CARTESIAN_POINT('Ctrl Pts',(-4.27060009881377,5.24921554101295,29.0202132172011));
#55443=CARTESIAN_POINT('Ctrl Pts',(-4.41488269589484,5.1318316636436,29.0289624439563));
#55444=CARTESIAN_POINT('Ctrl Pts',(-4.55432273230482,5.0084957714366,29.0377116707114));
#55445=CARTESIAN_POINT('Ctrl Pts',(-4.68844662475729,4.87962675281645,29.0464608974666));
#55446=CARTESIAN_POINT('Ctrl Pts',(-4.82256868830816,4.75075949144289,29.0552100049181));
#55447=CARTESIAN_POINT('Ctrl Pts',(-4.95137454633662,4.61635945317032,29.0639591123696));
#55448=CARTESIAN_POINT('Ctrl Pts',(-5.07442674457021,4.47688309139189,29.0727082198212));
#55449=CARTESIAN_POINT('Ctrl Pts',(-5.19747742834581,4.33740844621092,29.0814572195935));
#55450=CARTESIAN_POINT('Ctrl Pts',(-5.31477440447077,4.19285781740908,29.0902062193659));
#55451=CARTESIAN_POINT('Ctrl Pts',(-5.42591931527416,4.0437221200442,29.0989552191382));
#55452=CARTESIAN_POINT('Ctrl Pts',(-5.53707636459378,3.89457013505924,29.1077051744188));
#55453=CARTESIAN_POINT('Ctrl Pts',(-5.64207983270005,3.74083230921646,29.1164551296994));
#55454=CARTESIAN_POINT('Ctrl Pts',(-5.74057303465425,3.58303087257151,29.1252050849799));
#55455=CARTESIAN_POINT('Ctrl Pts',(-5.83906243360593,3.42523552892838,29.1339547024088));
#55456=CARTESIAN_POINT('Ctrl Pts',(-5.93104191765408,3.26337713162477,29.1427043198376));
#55457=CARTESIAN_POINT('Ctrl Pts',(-6.01619906696795,3.09800545296711,29.1514539372664));
#55458=CARTESIAN_POINT('Ctrl Pts',(-6.10135338092672,2.93263928045236,29.1602032633718));
#55459=CARTESIAN_POINT('Ctrl Pts',(-6.1796856835028,2.76376031545944,29.1689525894771));
#55460=CARTESIAN_POINT('Ctrl Pts',(-6.25092992692484,2.59194213837335,29.1777019155825));
#55461=CARTESIAN_POINT('Ctrl Pts',(-6.32217217688859,2.42012876886682,29.1864509968763));
#55462=CARTESIAN_POINT('Ctrl Pts',(-6.38632665481767,2.24537661653596,29.1952000781701));
#55463=CARTESIAN_POINT('Ctrl Pts',(-6.4431754786743,2.06827917627438,29.2039491594639));
#55464=CARTESIAN_POINT('Ctrl Pts',(-6.50002944234177,1.89116572429469,29.2126990317789));
#55465=CARTESIAN_POINT('Ctrl Pts',(-6.54957634248803,1.71170683295301,29.2214489040938));
#55466=CARTESIAN_POINT('Ctrl Pts',(-6.59164787706967,1.53051209231518,29.2301987764088));
#55467=CARTESIAN_POINT('Ctrl Pts',(-6.63371649073748,1.34932993154229,29.2389480412436));
#55468=CARTESIAN_POINT('Ctrl Pts',(-6.66831071256033,1.16641244180241,29.2476973060784));
#55469=CARTESIAN_POINT('Ctrl Pts',(-6.69531304839413,0.982380875222698,
29.2564465709132));
#55470=CARTESIAN_POINT('Ctrl Pts',(-6.72231677032296,0.798339861858778,
29.2651962848688));
#55471=CARTESIAN_POINT('Ctrl Pts',(-6.74172778477316,0.613184940793268,
29.2739459988245));
#55472=CARTESIAN_POINT('Ctrl Pts',(-6.75348015835118,0.427545027753774,
29.2826957127801));
#55473=CARTESIAN_POINT('Ctrl Pts',(-6.76249038363065,0.285219953908639,
29.2894038805684));
#55474=CARTESIAN_POINT('Ctrl Pts',(-6.76699999997976,0.142609996418872,
29.2961120483566));
#55475=CARTESIAN_POINT('Ctrl Pts',(-6.767,9.60595125194256E-10,29.3028202161448));
#55476=CARTESIAN_POINT('Ctrl Pts',(-6.767,3.94550158016225E-12,29.3028202161898));
#55477=CARTESIAN_POINT('Ctrl Pts',(-6.76700000000011,-0.1860072495561,29.3115697280026));
#55478=CARTESIAN_POINT('Ctrl Pts',(-6.75932637294268,-0.372014355812326,
29.3203192398153));
#55479=CARTESIAN_POINT('Ctrl Pts',(-6.74400518263393,-0.557389537582745,
29.329068751628));
#55480=CARTESIAN_POINT('Ctrl Pts',(-6.72868405703768,-0.742763936379325,
29.3378182264853));
#55481=CARTESIAN_POINT('Ctrl Pts',(-6.70571545643609,-0.927506130401745,
29.3465677013425));
#55482=CARTESIAN_POINT('Ctrl Pts',(-6.67517739401626,-1.11098864009237,
29.3553171761997));
#55483=CARTESIAN_POINT('Ctrl Pts',(-6.64463945804446,-1.2944703900425,29.3640666148282));
#55484=CARTESIAN_POINT('Ctrl Pts',(-6.60653217002786,-1.47669218339003,
29.3728160534567));
#55485=CARTESIAN_POINT('Ctrl Pts',(-6.56098496085545,-1.65703510627524,
29.3815654920852));
#55486=CARTESIAN_POINT('Ctrl Pts',(-6.51543793649624,-1.83737729739771,
29.3903148952119));
#55487=CARTESIAN_POINT('Ctrl Pts',(-6.46245112156964,-2.01584035544735,
29.3990642983385));
#55488=CARTESIAN_POINT('Ctrl Pts',(-6.40220448361785,-2.19181813797212,
29.4078137014651));
#55489=CARTESIAN_POINT('Ctrl Pts',(-6.34195808512043,-2.36779522106115,
29.4165630698167));
#55490=CARTESIAN_POINT('Ctrl Pts',(-6.27445201416427,-2.54128677725564,
29.4253124381682));
#55491=CARTESIAN_POINT('Ctrl Pts',(-6.19991555052799,-2.71170355428486,
29.4340618065197));
#55492=CARTESIAN_POINT('Ctrl Pts',(-6.12537937695189,-2.88211966813372,
29.4428111408229));
#55493=CARTESIAN_POINT('Ctrl Pts',(-6.0438129802841,-3.04946076419752,29.4515604751261));
#55494=CARTESIAN_POINT('Ctrl Pts',(-5.95549339308928,-3.21315848424411,
29.4603098094293));
#55495=CARTESIAN_POINT('Ctrl Pts',(-5.86717414225757,-3.37685558085172,
29.4690591104109));
#55496=CARTESIAN_POINT('Ctrl Pts',(-5.77210188844016,-3.53690907700082,
29.4778084113924));
#55497=CARTESIAN_POINT('Ctrl Pts',(-5.67059953311324,-3.69277537024064,
29.486557712374));
#55498=CARTESIAN_POINT('Ctrl Pts',(-5.56909755592647,-3.84864108281114,
29.4953069807606));
#55499=CARTESIAN_POINT('Ctrl Pts',(-5.46116568154892,-4.0003193835493,29.5040562491472));
#55500=CARTESIAN_POINT('Ctrl Pts',(-5.34717048488289,-4.14729511918278,
29.5128055175338));
#55501=CARTESIAN_POINT('Ctrl Pts',(-5.2331757034321,-4.29427031947295,29.5215547540522));
#55502=CARTESIAN_POINT('Ctrl Pts',(-5.11311781951445,-4.43654276249674,
29.5303039905706));
#55503=CARTESIAN_POINT('Ctrl Pts',(-4.98740458929134,-4.57362924412503,
29.5390532270889));
#55504=CARTESIAN_POINT('Ctrl Pts',(-4.86169180652617,-4.71071523781395,
29.5478024324656));
#55505=CARTESIAN_POINT('Ctrl Pts',(-4.73032391141436,-4.84261509584623,
29.5565516378423));
#55506=CARTESIAN_POINT('Ctrl Pts',(-4.59374706947177,-4.96888084599737,
29.5653008432191));
#55507=CARTESIAN_POINT('Ctrl Pts',(-4.45717070231383,-5.0951461572085,29.5740500181808));
#55508=CARTESIAN_POINT('Ctrl Pts',(-4.31538563497265,-5.21577720520662,
29.5827991931425));
#55509=CARTESIAN_POINT('Ctrl Pts',(-4.16887340951972,-5.33036429293528,
29.5915483681042));
#55510=CARTESIAN_POINT('Ctrl Pts',(-4.02236168122446,-5.44495099183735,
29.6002975133774));
#55511=CARTESIAN_POINT('Ctrl Pts',(-3.87112305263137,-5.55349359497959,
29.6090466586507));
#55512=CARTESIAN_POINT('Ctrl Pts',(-3.71567116928946,-5.65562346357244,
29.6177958039239));
#55513=CARTESIAN_POINT('Ctrl Pts',(-3.56021980053269,-5.75775299408953,
29.6265449202353));
#55514=CARTESIAN_POINT('Ctrl Pts',(-3.40055544442049,-5.85346967519899,
29.6352940365466));
#55515=CARTESIAN_POINT('Ctrl Pts',(-3.23722035886816,-5.94244843041397,
29.644043152858));
#55516=CARTESIAN_POINT('Ctrl Pts',(-3.07388580043446,-6.03142689847474,
29.652792240934));
#55517=CARTESIAN_POINT('Ctrl Pts',(-2.90688078789162,-6.11366734707931,
29.6615413290101));
#55518=CARTESIAN_POINT('Ctrl Pts',(-2.73677250610313,-6.18889047001464,
29.6702904170861));
#55519=CARTESIAN_POINT('Ctrl Pts',(-2.56666475916852,-6.26411335643368,
29.6790394776532));
#55520=CARTESIAN_POINT('Ctrl Pts',(-2.39345402457006,-6.33231884545289,
29.6877885382204));
#55521=CARTESIAN_POINT('Ctrl Pts',(-2.21772855943975,-6.39327529804914,
29.6965375987876));
#55522=CARTESIAN_POINT('Ctrl Pts',(-2.04200363223531,-6.45423156404721,
29.7052866325724));
#55523=CARTESIAN_POINT('Ctrl Pts',(-1.86376426061004,-6.50793874412461,
29.7140356663572));
#55524=CARTESIAN_POINT('Ctrl Pts',(-1.68361577621689,-6.55421443943312,
29.722784700142));
#55525=CARTESIAN_POINT('Ctrl Pts',(-1.50346782833187,-6.60048999692595,
29.7315337078709));
#55526=CARTESIAN_POINT('Ctrl Pts',(-1.32141105657328,-6.63933404265174,
29.7402827155998));
#55527=CARTESIAN_POINT('Ctrl Pts',(-1.13806375346445,-6.67061465631544,
29.7490317233287));
#55528=CARTESIAN_POINT('Ctrl Pts',(-0.954716981169325,-6.7018951794178,
29.7577807057281));
#55529=CARTESIAN_POINT('Ctrl Pts',(-0.770079967441817,-6.72561226609009,
29.7665296881275));
#55530=CARTESIAN_POINT('Ctrl Pts',(-0.584779764072827,-6.74168536995987,
29.7752786705269));
#55531=CARTESIAN_POINT('Ctrl Pts',(-0.391489587592689,-6.75845153117874,
29.7844049009426));
#55532=CARTESIAN_POINT('Ctrl Pts',(-0.197478091804947,-6.76689985146395,
29.7935311313582));
#55533=CARTESIAN_POINT('Ctrl Pts',(-0.00346214753071807,-6.76699911434415,
29.8026573617738));
#55534=CARTESIAN_POINT('Ctrl Pts',(0.184490798485026,-6.76709527525934,
29.8114983974889));
#55535=CARTESIAN_POINT('Ctrl Pts',(0.372447602155239,-6.75935633790761,
29.8203394332041));
#55536=CARTESIAN_POINT('Ctrl Pts',(0.559756448194746,-6.74380914014509,
29.8291804689192));
#55537=CARTESIAN_POINT('Ctrl Pts',(0.745136131043843,-6.72842206873149,
29.8379304475325));
#55538=CARTESIAN_POINT('Ctrl Pts',(0.929880851945483,-6.70538686355717,
29.8466804261458));
#55539=CARTESIAN_POINT('Ctrl Pts',(1.11336305057502,-6.67478177303306,29.8554304047591));
#55540=CARTESIAN_POINT('Ctrl Pts',(1.29684337090168,-6.64417699581252,29.8641802937991));
#55541=CARTESIAN_POINT('Ctrl Pts',(1.47906091205239,-6.60600253548049,29.8729301828391));
#55542=CARTESIAN_POINT('Ctrl Pts',(1.65939671095275,-6.56038806441198,29.881680071879));
#55543=CARTESIAN_POINT('Ctrl Pts',(1.83973072369224,-6.51477404513832,29.8904298742545));
#55544=CARTESIAN_POINT('Ctrl Pts',(2.0181827535711,-6.46172023288638,29.89917967663));
#55545=CARTESIAN_POINT('Ctrl Pts',(2.19414664033409,-6.40140683918079,29.9079294790055));
#55546=CARTESIAN_POINT('Ctrl Pts',(2.37010884271342,-6.34109402281466,29.9166791976251));
#55547=CARTESIAN_POINT('Ctrl Pts',(2.54358267847889,-6.27352185699758,29.9254289162446));
#55548=CARTESIAN_POINT('Ctrl Pts',(2.71397890841824,-6.19891986435225,29.9341786348642));
#55549=CARTESIAN_POINT('Ctrl Pts',(2.88437356389031,-6.12431856103202,29.942928272636));
#55550=CARTESIAN_POINT('Ctrl Pts',(3.05169040787266,-6.0426876758251,29.9516779104078));
#55551=CARTESIAN_POINT('Ctrl Pts',(3.21536112512153,-5.95430447953892,29.9604275481796));
#55552=CARTESIAN_POINT('Ctrl Pts',(3.37903038442942,-5.86592207054986,29.9691771080117));
#55553=CARTESIAN_POINT('Ctrl Pts',(3.53905332980071,-5.77078760703317,29.9779266678438));
#55554=CARTESIAN_POINT('Ctrl Pts',(3.69488643041989,-5.66922422085235,29.9866762276758));
#55555=CARTESIAN_POINT('Ctrl Pts',(3.8507181946885,-5.56766170563084,29.9954257124758));
#55556=CARTESIAN_POINT('Ctrl Pts',(4.00235994599341,-5.45967053456166,30.0041751972758));
#55557=CARTESIAN_POINT('Ctrl Pts',(4.14929662974426,-5.34561750206587,30.0129246820758));
#55558=CARTESIAN_POINT('Ctrl Pts',(4.29623210225173,-5.23156540974361,30.0216740947512));
#55559=CARTESIAN_POINT('Ctrl Pts',(4.43846235842249,-5.11145173172073,30.0304235074266));
#55560=CARTESIAN_POINT('Ctrl Pts',(4.57550431797562,-4.98568443006439,30.0391729201019));
#55561=CARTESIAN_POINT('Ctrl Pts',(4.71254519337633,-4.85991812336555,30.0479222635598));
#55562=CARTESIAN_POINT('Ctrl Pts',(4.84439764315127,-4.72849847630954,30.0566716070177));
#55563=CARTESIAN_POINT('Ctrl Pts',(4.97061384196834,-4.59187184425184,30.0654209504756));
#55564=CARTESIAN_POINT('Ctrl Pts',(5.09682908420349,-4.45524624767584,30.074170227623));
#55565=CARTESIAN_POINT('Ctrl Pts',(5.21740796650309,-4.31341395556726,30.0829195047704));
#55566=CARTESIAN_POINT('Ctrl Pts',(5.33194095942384,-4.16685668162686,30.0916687819177));
#55567=CARTESIAN_POINT('Ctrl Pts',(5.44647312235257,-4.02030046975047,30.1004179956613));
#55568=CARTESIAN_POINT('Ctrl Pts',(5.55495930712403,-3.86901957035382,30.1091672094048));
#55569=CARTESIAN_POINT('Ctrl Pts',(5.65703106079901,-3.71352778058213,30.1179164231483));
#55570=CARTESIAN_POINT('Ctrl Pts',(5.75910210868834,-3.55803706597444,30.1266655763945));
#55571=CARTESIAN_POINT('Ctrl Pts',(5.85475865698639,-3.39833575880744,30.1354147296407));
#55572=CARTESIAN_POINT('Ctrl Pts',(5.94367583069146,-3.23496624706568,30.1441638828869));
#55573=CARTESIAN_POINT('Ctrl Pts',(6.03259241910153,-3.07159781069949,30.152912978542));
#55574=CARTESIAN_POINT('Ctrl Pts',(6.11476958471038,-2.90456146975686,30.1616620741971));
#55575=CARTESIAN_POINT('Ctrl Pts',(6.1899282357445,-2.73442451648112,30.1704111698523));
#55576=CARTESIAN_POINT('Ctrl Pts',(6.26508641701002,-2.56428862662254,30.1791602108224));
#55577=CARTESIAN_POINT('Ctrl Pts',(6.33322605570365,-2.39105242531098,30.1879092517925));
#55578=CARTESIAN_POINT('Ctrl Pts',(6.39411573747835,-2.21530425353532,30.1966582927626));
#55579=CARTESIAN_POINT('Ctrl Pts',(6.45500505889193,-2.03955712188347,30.2054072819536));
#55580=CARTESIAN_POINT('Ctrl Pts',(6.50864441544996,-1.86129832025341,30.2141562711446));
#55581=CARTESIAN_POINT('Ctrl Pts',(6.5548516404997,-1.68113324012061,30.2229052603357));
#55582=CARTESIAN_POINT('Ctrl Pts',(6.60199852639166,-1.49730435912651,30.2318321672125));
#55583=CARTESIAN_POINT('Ctrl Pts',(6.64140767441058,-1.31149113173406,30.2407590740894));
#55584=CARTESIAN_POINT('Ctrl Pts',(6.67293975269643,-1.12435050446188,30.2496859809663));
#55585=CARTESIAN_POINT('Ctrl Pts',(6.70384664831542,-0.940920291561225,
30.2584358951503));
#55586=CARTESIAN_POINT('Ctrl Pts',(6.72718585889695,-0.756215114275331,
30.2671858093343));
#55587=CARTESIAN_POINT('Ctrl Pts',(6.74287810451887,-0.570862389372445,
30.2759357235183));
#55588=CARTESIAN_POINT('Ctrl Pts',(6.75857004154139,-0.385513309565421,
30.2846854656289));
#55589=CARTESIAN_POINT('Ctrl Pts',(6.76661529035564,-0.199516993256552,
30.2934352077394));
#55590=CARTESIAN_POINT('Ctrl Pts',(6.76698652348897,-0.0135052182024178,
30.30218494985));
#55591=CARTESIAN_POINT('Ctrl Pts',(6.76735774981517,0.172503146040519,30.3109345315207));
#55592=CARTESIAN_POINT('Ctrl Pts',(6.76005524147471,0.358526681835083,30.3196841131913));
#55593=CARTESIAN_POINT('Ctrl Pts',(6.74510380214869,0.543933542116461,30.328433694862));
#55594=CARTESIAN_POINT('Ctrl Pts',(6.73015261710962,0.729337249086341,30.3371831277239));
#55595=CARTESIAN_POINT('Ctrl Pts',(6.70755278444583,0.914124015856304,30.3459325605858));
#55596=CARTESIAN_POINT('Ctrl Pts',(6.67738106408262,1.09766621749552,30.3546819934478));
#55597=CARTESIAN_POINT('Ctrl Pts',(6.64720981677221,1.28120554143496,30.3634312891301));
#55598=CARTESIAN_POINT('Ctrl Pts',(6.60946696581483,1.46350005650802,30.3721805848125));
#55599=CARTESIAN_POINT('Ctrl Pts',(6.56428070010947,1.64393062206724,30.3809298804948));
#55600=CARTESIAN_POINT('Ctrl Pts',(6.5190950828269,1.82435859844834,30.3896790506248));
#55601=CARTESIAN_POINT('Ctrl Pts',(6.46646633415607,2.00292240086737,30.3984282207548));
#55602=CARTESIAN_POINT('Ctrl Pts',(6.40657319597136,2.1790155769662,30.4071773908848));
#55603=CARTESIAN_POINT('Ctrl Pts',(6.34668083768237,2.3551064600759,30.4159264470878));
#55604=CARTESIAN_POINT('Ctrl Pts',(6.27952437143826,2.52872650996677,30.4246755032909));
#55605=CARTESIAN_POINT('Ctrl Pts',(6.20533187335076,2.69928607998062,30.433424559494));
#55606=CARTESIAN_POINT('Ctrl Pts',(6.12831449784194,2.87633970115522,30.4425067357828));
#55607=CARTESIAN_POINT('Ctrl Pts',(6.04371489463096,3.05009490562461,30.4515889120717));
#55608=CARTESIAN_POINT('Ctrl Pts',(5.95184265120436,3.21991584599732,30.4606710883605));
#55609=CARTESIAN_POINT('Ctrl Pts',(5.86333281335429,3.3835215590541,30.4694208687149));
#55610=CARTESIAN_POINT('Ctrl Pts',(5.76807337235613,3.54347560903942,30.4781706490694));
#55611=CARTESIAN_POINT('Ctrl Pts',(5.66638790086274,3.69923467178772,30.4869204294238));
#55612=CARTESIAN_POINT('Ctrl Pts',(5.56470608502659,3.85498813489885,30.4956698952181));
#55613=CARTESIAN_POINT('Ctrl Pts',(5.45659885766867,4.00654667256377,30.5044193610123));
#55614=CARTESIAN_POINT('Ctrl Pts',(5.34243340580421,4.15339551506322,30.5131688268066));
#55615=CARTESIAN_POINT('Ctrl Pts',(5.22827145140507,4.30023985883976,30.5219180245604));
#55616=CARTESIAN_POINT('Ctrl Pts',(5.10805181978003,4.44237456993142,30.5306672223143));
#55617=CARTESIAN_POINT('Ctrl Pts',(4.98218281282465,4.57931691626542,30.5394164200682));
#55618=CARTESIAN_POINT('Ctrl Pts',(4.85631699296145,4.71625579512248,30.5481653962862));
#55619=CARTESIAN_POINT('Ctrl Pts',(4.72480227791756,4.84800236135849,30.5569143725042));
#55620=CARTESIAN_POINT('Ctrl Pts',(4.58808530848034,4.97410918678982,30.5656633487222));
#55621=CARTESIAN_POINT('Ctrl Pts',(4.45135945056885,5.10022421089084,30.5744128937434));
#55622=CARTESIAN_POINT('Ctrl Pts',(4.30943087207948,5.22069856612062,30.5831624387646));
#55623=CARTESIAN_POINT('Ctrl Pts',(4.16278164322369,5.3351230530176,30.5919119837858));
#55624=CARTESIAN_POINT('Ctrl Pts',(4.01614103534287,5.44954081331503,30.600661014453));
#55625=CARTESIAN_POINT('Ctrl Pts',(3.86478055833306,5.55790924068413,30.6094100451203));
#55626=CARTESIAN_POINT('Ctrl Pts',(3.70921425811839,5.65986029751364,30.6181590757875));
#55627=CARTESIAN_POINT('Ctrl Pts',(3.55364584530021,5.76181273884714,30.6269082252674));
#55628=CARTESIAN_POINT('Ctrl Pts',(3.39387173464259,5.85734747818112,30.6356573747472));
#55629=CARTESIAN_POINT('Ctrl Pts',(3.23043456092335,5.94614005448846,30.6444065242271));
#55630=CARTESIAN_POINT('Ctrl Pts',(3.18690768806344,5.96978744811307,30.6467366129601));
#55631=CARTESIAN_POINT('Ctrl Pts',(3.14312114982856,5.99295688499313,30.6490667016931));
#55632=CARTESIAN_POINT('Ctrl Pts',(3.09908550384718,6.01564277861014,30.6513967904261));
#55633=CARTESIAN_POINT('Origin',(0.,0.,-63.6971797838103));
#55634=CARTESIAN_POINT('',(3.09908550384727,6.01564277861009,33.045773705108));
#55635=CARTESIAN_POINT('',(3.09908550384731,6.01564277861007,32.651275857025));
#55636=CARTESIAN_POINT('',(3.09908550384721,6.01564277861012,-63.6971797838103));
#55637=CARTESIAN_POINT('',(-6.76699962134934,-0.00226377072112061,31.6971797837756));
#55638=CARTESIAN_POINT('Ctrl Pts',(-6.7669996213491,-0.00226377144942592,
31.6971797838099));
#55639=CARTESIAN_POINT('Ctrl Pts',(-6.76692578390497,-0.222983030274878,
31.7075764721537));
#55640=CARTESIAN_POINT('Ctrl Pts',(-6.75604897537786,-0.443454407875999,
31.7179731604974));
#55641=CARTESIAN_POINT('Ctrl Pts',(-6.73446647616864,-0.662759595449747,
31.7283698488412));
#55642=CARTESIAN_POINT('Ctrl Pts',(-6.72638873903325,-0.74483950846053,
31.7322610439574));
#55643=CARTESIAN_POINT('Ctrl Pts',(-6.71681185948521,-0.826756188685703,
31.7361522390737));
#55644=CARTESIAN_POINT('Ctrl Pts',(-6.70574275848478,-0.908461918315195,
31.7400434341899));
#55645=CARTESIAN_POINT('Ctrl Pts',(-6.68208302226691,-1.08310446701431,
31.7483606995234));
#55646=CARTESIAN_POINT('Ctrl Pts',(-6.65157362820262,-1.25699086935697,
31.7566779648568));
#55647=CARTESIAN_POINT('Ctrl Pts',(-6.6142774749381,-1.42955324648175,31.7649952301902));
#55648=CARTESIAN_POINT('Ctrl Pts',(-6.57701277810894,-1.60197008052,31.7733054805503));
#55649=CARTESIAN_POINT('Ctrl Pts',(-6.53297279979114,-1.77306477598608,
31.7816157309104));
#55650=CARTESIAN_POINT('Ctrl Pts',(-6.48227194989753,-1.94227685142251,
31.7899259812705));
#55651=CARTESIAN_POINT('Ctrl Pts',(-6.43160457699367,-2.11137719873351,
31.7982307445004));
#55652=CARTESIAN_POINT('Ctrl Pts',(-6.37428519571406,-2.27859707089379,
31.8065355077303));
#55653=CARTESIAN_POINT('Ctrl Pts',(-6.31047883354035,-2.44338819908734,
31.8148402709601));
#55654=CARTESIAN_POINT('Ctrl Pts',(-6.24670292156264,-2.60810068430576,
31.8231410709227));
#55655=CARTESIAN_POINT('Ctrl Pts',(-6.17644632359794,-2.77038641176818,
31.8314418708853));
#55656=CARTESIAN_POINT('Ctrl Pts',(-6.09992333431186,-2.92971403306153,
31.8397426708479));
#55657=CARTESIAN_POINT('Ctrl Pts',(-6.02342286069177,-3.08899477474999,
31.8480410284328));
#55658=CARTESIAN_POINT('Ctrl Pts',(-5.9406598213746,-3.24531883201725,31.8563393860177));
#55659=CARTESIAN_POINT('Ctrl Pts',(-5.85189598370829,-3.39817633383831,
31.8646377436027));
#55660=CARTESIAN_POINT('Ctrl Pts',(-5.76312311452502,-3.55104938855971,
31.8729369455265));
#55661=CARTESIAN_POINT('Ctrl Pts',(-5.6683483951749,-3.70045487852671,31.8812361474502));
#55662=CARTESIAN_POINT('Ctrl Pts',(-5.56787904463112,-3.84590846801606,
31.889535349374));
#55663=CARTESIAN_POINT('Ctrl Pts',(-5.46739950839948,-3.99137680374247,
31.8978353926796));
#55664=CARTESIAN_POINT('Ctrl Pts',(-5.36122438758727,-4.13289215376013,
31.9061354359852));
#55665=CARTESIAN_POINT('Ctrl Pts',(-5.24970359036488,-4.27000014207378,
31.9144354792907));
#55666=CARTESIAN_POINT('Ctrl Pts',(-5.13815297435195,-4.40714479076368,
31.9227377418887));
#55667=CARTESIAN_POINT('Ctrl Pts',(-5.02125405265445,-4.53987945904959,
31.9310400044865));
#55668=CARTESIAN_POINT('Ctrl Pts',(-4.89939639549994,-4.66778362392284,
31.9393422670845));
#55669=CARTESIAN_POINT('Ctrl Pts',(-4.77748592458961,-4.79574322314046,
31.9476481279271));
#55670=CARTESIAN_POINT('Ctrl Pts',(-4.65061267477801,-4.91886789471148,
31.9559539887697));
#55671=CARTESIAN_POINT('Ctrl Pts',(-4.51920248849852,-5.0367745500418,31.9642598496123));
#55672=CARTESIAN_POINT('Ctrl Pts',(-4.38763696610762,-5.15482057935726,
31.9725755285685));
#55673=CARTESIAN_POINT('Ctrl Pts',(-4.25152405140372,-5.26763603625039,
31.9808912075246));
#55674=CARTESIAN_POINT('Ctrl Pts',(-4.11132294846449,-5.37487791614184,
31.9892068864807));
#55675=CARTESIAN_POINT('Ctrl Pts',(-3.97103316944413,-5.48218762566831,
31.9975278250376));
#55676=CARTESIAN_POINT('Ctrl Pts',(-3.82665032953597,-5.58391652786719,
32.0058487635944));
#55677=CARTESIAN_POINT('Ctrl Pts',(-3.67866203664944,-5.67976536664273,
32.0141697021512));
#55678=CARTESIAN_POINT('Ctrl Pts',(-3.53045378732077,-5.77575666648157,
32.0225030082002));
#55679=CARTESIAN_POINT('Ctrl Pts',(-3.378629674649,-5.86585025973974,32.0308363142491));
#55680=CARTESIAN_POINT('Ctrl Pts',(-3.22370246671382,-5.94979255151835,
32.039169620298));
#55681=CARTESIAN_POINT('Ctrl Pts',(-3.10966689474783,-6.01157903423296,
32.0453034255497));
#55682=CARTESIAN_POINT('Ctrl Pts',(-2.99395061897389,-6.07003381744407,
32.0514372308013));
#55683=CARTESIAN_POINT('Ctrl Pts',(-2.87676452165102,-6.1250726434035,32.057571036053));
#55684=CARTESIAN_POINT('Ctrl Pts',(-2.72256050327969,-6.19749768633331,
32.065642449295));
#55685=CARTESIAN_POINT('Ctrl Pts',(-2.56533592850153,-6.26422877010482,
32.073713862537));
#55686=CARTESIAN_POINT('Ctrl Pts',(-2.40555850139185,-6.32499622896184,
32.0817852757791));
#55687=CARTESIAN_POINT('Ctrl Pts',(-2.24598166160797,-6.38568739930746,
32.0898465560303));
#55688=CARTESIAN_POINT('Ctrl Pts',(-2.08385869058967,-6.44042971072414,
32.0979078362815));
#55689=CARTESIAN_POINT('Ctrl Pts',(-1.91968221119545,-6.48899909138688,
32.1059691165327));
#55690=CARTESIAN_POINT('Ctrl Pts',(-1.75567583711146,-6.53751814870492,
32.1140220443904));
#55691=CARTESIAN_POINT('Ctrl Pts',(-1.58962054337844,-6.57987689829311,
32.122074972248));
#55692=CARTESIAN_POINT('Ctrl Pts',(-1.42202918432237,-6.61589918294826,
32.1301279001056));
#55693=CARTESIAN_POINT('Ctrl Pts',(-1.2545747701153,-6.65189203251583,32.13817424763));
#55694=CARTESIAN_POINT('Ctrl Pts',(-1.0855871515895,-6.68155864466435,32.1462205951543));
#55695=CARTESIAN_POINT('Ctrl Pts',(-0.915594511135806,-6.70477260547873,
32.1542669426787));
#55696=CARTESIAN_POINT('Ctrl Pts',(-0.745703592099352,-6.72797267535649,
32.1623084753719));
#55697=CARTESIAN_POINT('Ctrl Pts',(-0.574809216937471,-6.74472773006746,
32.1703500080651));
#55698=CARTESIAN_POINT('Ctrl Pts',(-0.403449829011714,-6.75496241554832,
32.1783915407582));
#55699=CARTESIAN_POINT('Ctrl Pts',(-0.228796101835591,-6.76539386017091,
32.1865876698065));
#55700=CARTESIAN_POINT('Ctrl Pts',(-0.0536596877783217,-6.76905159753581,
32.1947837988547));
#55701=CARTESIAN_POINT('Ctrl Pts',(0.12138325107208,-6.76591125469136,32.202979927903));
#55702=CARTESIAN_POINT('Ctrl Pts',(0.293065225942237,-6.76283120893318,
32.2110186847391));
#55703=CARTESIAN_POINT('Ctrl Pts',(0.464656896194815,-6.75321180321184,
32.2190574415752));
#55704=CARTESIAN_POINT('Ctrl Pts',(0.635614615127708,-6.73708268177229,
32.2270961984113));
#55705=CARTESIAN_POINT('Ctrl Pts',(0.806588880960806,-6.72095199920426,
32.2351357333141));
#55706=CARTESIAN_POINT('Ctrl Pts',(0.976928701445892,-6.6983103813075,32.2431752682168));
#55707=CARTESIAN_POINT('Ctrl Pts',(1.14609585613162,-6.66923933357905,32.2512148031196));
#55708=CARTESIAN_POINT('Ctrl Pts',(1.31531287956567,-6.64015971600284,32.2592567079951));
#55709=CARTESIAN_POINT('Ctrl Pts',(1.48335618123837,-6.604646959209,32.2672986128707));
#55710=CARTESIAN_POINT('Ctrl Pts',(1.6496981771387,-6.56283360480405,32.2753405177462));
#55711=CARTESIAN_POINT('Ctrl Pts',(1.82165126819941,-6.51960979052532,32.283653694427));
#55712=CARTESIAN_POINT('Ctrl Pts',(1.99178584450771,-6.46965298263884,32.2919668711078));
#55713=CARTESIAN_POINT('Ctrl Pts',(2.15953768467293,-6.41316505233395,32.3002800477887));
#55714=CARTESIAN_POINT('Ctrl Pts',(2.32209727743496,-6.35842553390429,32.3083359153992));
#55715=CARTESIAN_POINT('Ctrl Pts',(2.48241911867582,-6.29755337063983,32.3163917830097));
#55716=CARTESIAN_POINT('Ctrl Pts',(2.6400120116576,-6.23078049511484,32.3244476506202));
#55717=CARTESIAN_POINT('Ctrl Pts',(2.8051553168492,-6.16080847320002,32.3328894818362));
#55718=CARTESIAN_POINT('Ctrl Pts',(2.9673013085468,-6.08435661958424,32.3413313130522));
#55719=CARTESIAN_POINT('Ctrl Pts',(3.12591640348562,-6.0017443829623,32.3497731442682));
#55720=CARTESIAN_POINT('Ctrl Pts',(3.28453149842456,-5.9191321463403,32.3582149754842));
#55721=CARTESIAN_POINT('Ctrl Pts',(3.43961533894103,-5.83035983005544,32.3666568067001));
#55722=CARTESIAN_POINT('Ctrl Pts',(3.59067229527634,-5.73579649812778,32.3750986379161));
#55723=CARTESIAN_POINT('Ctrl Pts',(3.73794693401972,-5.64360093900966,32.3833290939827));
#55724=CARTESIAN_POINT('Ctrl Pts',(3.88188396889984,-5.54559457348232,32.3915595500493));
#55725=CARTESIAN_POINT('Ctrl Pts',(4.02199394598704,-5.44204499232077,32.3997900061158));
#55726=CARTESIAN_POINT('Ctrl Pts',(4.16193760427525,-5.33861833061388,32.408010692146));
#55727=CARTESIAN_POINT('Ctrl Pts',(4.29806296529143,-5.22966176676282,32.4162313781762));
#55728=CARTESIAN_POINT('Ctrl Pts',(4.42990667331544,-5.11548784239737,32.4244520642064));
#55729=CARTESIAN_POINT('Ctrl Pts',(4.56162032701516,-5.00142654238699,32.4326646411218));
#55730=CARTESIAN_POINT('Ctrl Pts',(4.68906046970116,-4.88215836424707,32.4408772180372));
#55731=CARTESIAN_POINT('Ctrl Pts',(4.81179409502263,-4.75803810273787,32.4490897949526));
#55732=CARTESIAN_POINT('Ctrl Pts',(4.93443126777576,-4.6340153835116,32.4572959178573));
#55733=CARTESIAN_POINT('Ctrl Pts',(5.05236903921426,-4.50514842955538,32.465502040762));
#55734=CARTESIAN_POINT('Ctrl Pts',(5.16520871727372,-4.371831184641,32.4737081636666));
#55735=CARTESIAN_POINT('Ctrl Pts',(5.27798234329545,-4.23859197854988,32.4819094830203));
#55736=CARTESIAN_POINT('Ctrl Pts',(5.38566358986551,-4.10090794394812,32.4901108023741));
#55737=CARTESIAN_POINT('Ctrl Pts',(5.48789171907028,-3.95920869363562,32.4983121217278));
#55738=CARTESIAN_POINT('Ctrl Pts',(5.59009052144693,-3.81755009348067,32.5065110883173));
#55739=CARTESIAN_POINT('Ctrl Pts',(5.68683910978897,-3.67187886007352,32.5147100549069));
#55740=CARTESIAN_POINT('Ctrl Pts',(5.77781788769589,-3.5226565907879,32.5229090214964));
#55741=CARTESIAN_POINT('Ctrl Pts',(5.86878465144408,-3.37345402697724,32.5311069053753));
#55742=CARTESIAN_POINT('Ctrl Pts',(5.95398293492057,-3.22070166689604,32.5393047892543));
#55743=CARTESIAN_POINT('Ctrl Pts',(6.03313723726971,-3.06488891744376,32.5475026731332));
#55744=CARTESIAN_POINT('Ctrl Pts',(6.1122954655424,-2.90906843993472,32.5557009636137));
#55745=CARTESIAN_POINT('Ctrl Pts',(6.18540895299778,-2.75018759037932,32.5638992540943));
#55746=CARTESIAN_POINT('Ctrl Pts',(6.25224879121642,-2.58875917240922,32.5720975445748));
#55747=CARTESIAN_POINT('Ctrl Pts',(6.31910408619757,-2.42729342399688,32.5802977309161));
#55748=CARTESIAN_POINT('Ctrl Pts',(6.37968270524256,-2.26327926506783,32.5884979172574));
#55749=CARTESIAN_POINT('Ctrl Pts',(6.43380437632073,-2.097248255986,32.5966981035988));
#55750=CARTESIAN_POINT('Ctrl Pts',(6.4879772151923,-1.93106027761251,32.6049060425729));
#55751=CARTESIAN_POINT('Ctrl Pts',(6.53568079862508,-1.76285198096014,32.613113981547));
#55752=CARTESIAN_POINT('Ctrl Pts',(6.5767848671248,-1.5931697372089,32.6213219205211));
#55753=CARTESIAN_POINT('Ctrl Pts',(6.61790887645348,-1.42340517546032,32.629533841415));
#55754=CARTESIAN_POINT('Ctrl Pts',(6.65242691673485,-1.25216559228056,32.637745762309));
#55755=CARTESIAN_POINT('Ctrl Pts',(6.68026014890569,-1.08000617727054,32.645957683203));
#55756=CARTESIAN_POINT('Ctrl Pts',(6.70813154994514,-0.907610672896134,
32.6541808654455));
#55757=CARTESIAN_POINT('Ctrl Pts',(6.72929977907265,-0.734293171843731,
32.6624040476881));
#55758=CARTESIAN_POINT('Ctrl Pts',(6.74373792122086,-0.560613815284455,
32.6706272299306));
#55759=CARTESIAN_POINT('Ctrl Pts',(6.75661310027526,-0.405735660546783,
32.6779602332134));
#55760=CARTESIAN_POINT('Ctrl Pts',(6.76413715051455,-0.250569959535481,
32.6852932364962));
#55761=CARTESIAN_POINT('Ctrl Pts',(6.76632591716136,-0.0955122125724868,
32.6926262397789));
#55762=CARTESIAN_POINT('Ctrl Pts',(6.76899290612317,0.093424008744249,32.7015614265612));
#55763=CARTESIAN_POINT('Ctrl Pts',(6.7637437604845,0.282591998645421,32.7104966133435));
#55764=CARTESIAN_POINT('Ctrl Pts',(6.75056509323352,0.471338436812814,32.7194318001257));
#55765=CARTESIAN_POINT('Ctrl Pts',(6.73740616354918,0.659802191205731,32.7283536047623));
#55766=CARTESIAN_POINT('Ctrl Pts',(6.71634142687637,0.847845396523924,32.7372754093989));
#55767=CARTESIAN_POINT('Ctrl Pts',(6.68740946285743,1.03481576915162,32.7461972140355));
#55768=CARTESIAN_POINT('Ctrl Pts',(6.65854807076005,1.22133007669985,32.7550972562748));
#55769=CARTESIAN_POINT('Ctrl Pts',(6.6218577907849,1.40677651960491,32.763997298514));
#55770=CARTESIAN_POINT('Ctrl Pts',(6.57742870056266,1.59050956897928,32.7728973407533));
#55771=CARTESIAN_POINT('Ctrl Pts',(6.53306800957807,1.77395975862261,32.7817836812467));
#55772=CARTESIAN_POINT('Ctrl Pts',(6.480992334127,1.95570156660659,32.7906700217401));
#55773=CARTESIAN_POINT('Ctrl Pts',(6.42134286456127,2.13509831524173,32.7995563622334));
#55774=CARTESIAN_POINT('Ctrl Pts',(6.36184590827701,2.3140363777055,32.8084199819053));
#55775=CARTESIAN_POINT('Ctrl Pts',(6.29481388053628,2.49064110088217,32.8172836015772));
#55776=CARTESIAN_POINT('Ctrl Pts',(6.22043774472953,2.66429038656529,32.8261472212491));
#55777=CARTESIAN_POINT('Ctrl Pts',(6.14983215175829,2.8291364175092,32.834561494403));
#55778=CARTESIAN_POINT('Ctrl Pts',(6.07260860983294,2.99131895356997,32.8429757675569));
#55779=CARTESIAN_POINT('Ctrl Pts',(5.98897247047364,3.15031708688329,32.8513900407107));
#55780=CARTESIAN_POINT('Ctrl Pts',(5.90736429702192,3.30545991558551,32.8596002889153));
#55781=CARTESIAN_POINT('Ctrl Pts',(5.81972826442297,3.45742132116671,32.8678105371198));
#55782=CARTESIAN_POINT('Ctrl Pts',(5.72635188422313,3.60571533791206,32.8760207853244));
#55783=CARTESIAN_POINT('Ctrl Pts',(5.63295330659624,3.75404460710146,32.8842329852686));
#55784=CARTESIAN_POINT('Ctrl Pts',(5.53381185236988,3.89870444934127,32.8924451852128));
#55785=CARTESIAN_POINT('Ctrl Pts',(5.42925849200748,4.03923770369667,32.900657385157));
#55786=CARTESIAN_POINT('Ctrl Pts',(5.32466165920383,4.1798293906421,32.9088729996675));
#55787=CARTESIAN_POINT('Ctrl Pts',(5.21464864961048,4.31629078610236,32.917088614178));
#55788=CARTESIAN_POINT('Ctrl Pts',(5.09959089478538,4.44819757944969,32.9253042286885));
#55789=CARTESIAN_POINT('Ctrl Pts',(4.98440393514553,4.58025249834339,32.933529068974));
#55790=CARTESIAN_POINT('Ctrl Pts',(4.86416114944602,4.70774233123302,32.9417539092594));
#55791=CARTESIAN_POINT('Ctrl Pts',(4.73927170448295,4.83027874051667,32.9499787495448));
#55792=CARTESIAN_POINT('Ctrl Pts',(4.61430226348916,4.9528936386299,32.9582088581263));
#55793=CARTESIAN_POINT('Ctrl Pts',(4.48468049291367,5.07054854962502,32.9664389667079));
#55794=CARTESIAN_POINT('Ctrl Pts',(4.35084879418545,5.1828953076572,32.9746690752895));
#55795=CARTESIAN_POINT('Ctrl Pts',(4.21683361014447,5.29539609481873,32.9829104674762));
#55796=CARTESIAN_POINT('Ctrl Pts',(4.07859724970943,5.40257397540435,32.9911518596628));
#55797=CARTESIAN_POINT('Ctrl Pts',(3.93661205132688,5.50412341407313,32.9993932518496));
#55798=CARTESIAN_POINT('Ctrl Pts',(3.87481648565114,5.54832030979238,33.0029801151137));
#55799=CARTESIAN_POINT('Ctrl Pts',(3.81231114292086,5.59145163960211,33.0065669783779));
#55800=CARTESIAN_POINT('Ctrl Pts',(3.74913639406064,5.63349494530083,33.0101538416421));
#55801=CARTESIAN_POINT('Ctrl Pts',(3.60032663912576,5.7325290393108,33.0186027908339));
#55802=CARTESIAN_POINT('Ctrl Pts',(3.4474616679766,5.82574900357178,33.0270517400257));
#55803=CARTESIAN_POINT('Ctrl Pts',(3.29102360987895,5.91282103561569,33.0355006892175));
#55804=CARTESIAN_POINT('Ctrl Pts',(3.22761964408248,5.94811111917128,33.0389250278477));
#55805=CARTESIAN_POINT('Ctrl Pts',(3.16362910304274,5.98239177950754,33.0423493664778));
#55806=CARTESIAN_POINT('Ctrl Pts',(3.09908550384727,6.01564277861009,33.045773705108));
#55807=CARTESIAN_POINT('Ctrl Pts',(3.09908550384736,6.01564277861005,31.0457633158951));
#55808=CARTESIAN_POINT('Ctrl Pts',(2.93978214379508,6.09771127104242,31.0541970845775));
#55809=CARTESIAN_POINT('Ctrl Pts',(2.77728693821518,6.1734119192158,31.06263085326));
#55810=CARTESIAN_POINT('Ctrl Pts',(2.61214130867702,6.24251606193393,31.0710646219425));
#55811=CARTESIAN_POINT('Ctrl Pts',(2.44685001542714,6.31168115670966,31.0795058294778));
#55812=CARTESIAN_POINT('Ctrl Pts',(2.2789039384388,6.37423800109378,31.0879470370132));
#55813=CARTESIAN_POINT('Ctrl Pts',(2.10886249709093,6.43000684046008,31.0963882445486));
#55814=CARTESIAN_POINT('Ctrl Pts',(2.0511158617316,6.44894612258902,31.0992549065204));
#55815=CARTESIAN_POINT('Ctrl Pts',(1.99312768629269,6.46710296868331,31.1021215684921));
#55816=CARTESIAN_POINT('Ctrl Pts',(1.93492021400103,6.48447166432626,31.1049882304639));
#55817=CARTESIAN_POINT('Ctrl Pts',(1.76961003393245,6.5337990460395,31.1131295976818));
#55818=CARTESIAN_POINT('Ctrl Pts',(1.60220166882337,6.57686372138172,31.1212709648996));
#55819=CARTESIAN_POINT('Ctrl Pts',(1.43321504134359,6.61348498488252,31.1294123321175));
#55820=CARTESIAN_POINT('Ctrl Pts',(1.26437592633729,6.65007428080551,31.137546592541));
#55821=CARTESIAN_POINT('Ctrl Pts',(1.09396164660413,6.68023128374515,31.1456808529645));
#55822=CARTESIAN_POINT('Ctrl Pts',(0.922507776869986,6.70382490833512,31.1538151133879));
#55823=CARTESIAN_POINT('Ctrl Pts',(0.751170866772573,6.72740243820665,31.1619438249128));
#55824=CARTESIAN_POINT('Ctrl Pts',(0.578796139762534,6.74442545419302,31.1700725364376));
#55825=CARTESIAN_POINT('Ctrl Pts',(0.405929832819718,6.75481383687419,31.1782012479625));
#55826=CARTESIAN_POINT('Ctrl Pts',(0.233145962624057,6.76519726552763,31.186326083055));
#55827=CARTESIAN_POINT('Ctrl Pts',(0.0598713439351249,6.76895233946947,
31.1944509181475));
#55828=CARTESIAN_POINT('Ctrl Pts',(-0.113342202082167,6.76605073475119,
31.2025757532401));
#55829=CARTESIAN_POINT('Ctrl Pts',(-0.2865072564816,6.76314994234529,31.2106983137623));
#55830=CARTESIAN_POINT('Ctrl Pts',(-0.459610906599376,6.75359619007722,
31.2188208742844));
#55831=CARTESIAN_POINT('Ctrl Pts',(-0.632100897357243,6.73741326144984,
31.2269434348066));
#55832=CARTESIAN_POINT('Ctrl Pts',(-0.804600055510615,6.72122947274179,
31.2350664270218));
#55833=CARTESIAN_POINT('Ctrl Pts',(-0.976485124324183,6.69841583412734,
31.2431894192369));
#55834=CARTESIAN_POINT('Ctrl Pts',(-1.14720834676363,6.66904805868993,31.2513124114521));
#55835=CARTESIAN_POINT('Ctrl Pts',(-1.23435734910002,6.65405670429983,31.2554589514332));
#55836=CARTESIAN_POINT('Ctrl Pts',(-1.32120370627018,6.6373583099481,31.2596054914143));
#55837=CARTESIAN_POINT('Ctrl Pts',(-1.40767548398425,6.61896810173532,31.2637520313953));
#55838=CARTESIAN_POINT('Ctrl Pts',(-1.59502034743857,6.57912491662224,31.2727356904237));
#55839=CARTESIAN_POINT('Ctrl Pts',(-1.78051361467214,6.53135738162034,31.281719349452));
#55840=CARTESIAN_POINT('Ctrl Pts',(-1.9635166759737,6.47586992327465,31.2907030084804));
#55841=CARTESIAN_POINT('Ctrl Pts',(-2.14683413459578,6.42028713806337,31.2997021013398));
#55842=CARTESIAN_POINT('Ctrl Pts',(-2.32765260758264,6.3569579904057,31.3087011941992));
#55843=CARTESIAN_POINT('Ctrl Pts',(-2.5053511830219,6.28613589176457,31.3177002870585));
#55844=CARTESIAN_POINT('Ctrl Pts',(-2.68346641196309,6.21514773509321,31.3267204802759));
#55845=CARTESIAN_POINT('Ctrl Pts',(-2.8584468837172,6.13663156412673,31.3357406734933));
#55846=CARTESIAN_POINT('Ctrl Pts',(-3.02969160558259,6.05088900700239,31.3447608667106));
#55847=CARTESIAN_POINT('Ctrl Pts',(-3.20110975560926,5.96505961406868,31.3537901951323));
#55848=CARTESIAN_POINT('Ctrl Pts',(-3.36878438653771,5.87198932674126,31.362819523554));
#55849=CARTESIAN_POINT('Ctrl Pts',(-3.53214007237226,5.77202525194945,31.3718488519757));
#55850=CARTESIAN_POINT('Ctrl Pts',(-3.69572605679668,5.67192024796167,31.3808909099305));
#55851=CARTESIAN_POINT('Ctrl Pts',(-3.8549807173307,5.56490214844779,31.3899329678852));
#55852=CARTESIAN_POINT('Ctrl Pts',(-4.0093565897801,5.45136209914429,31.39897502584));
#55853=CARTESIAN_POINT('Ctrl Pts',(-4.14332802850144,5.35282906081172,31.4068219613356));
#55854=CARTESIAN_POINT('Ctrl Pts',(-4.27362554592084,5.2493849196875,31.4146688968313));
#55855=CARTESIAN_POINT('Ctrl Pts',(-4.39991149110694,5.14130993720716,31.422515832327));
#55856=CARTESIAN_POINT('Ctrl Pts',(-4.53917744008327,5.02212672189731,31.4311692966278));
#55857=CARTESIAN_POINT('Ctrl Pts',(-4.67368667760506,4.89720573293097,31.4398227609286));
#55858=CARTESIAN_POINT('Ctrl Pts',(-4.80297040682896,4.7669449620407,31.4484762252294));
#55859=CARTESIAN_POINT('Ctrl Pts',(-4.93213503929425,4.63680418796427,31.4571217179196));
#55860=CARTESIAN_POINT('Ctrl Pts',(-5.05608355122076,4.50133365812178,31.4657672106098));
#55861=CARTESIAN_POINT('Ctrl Pts',(-5.17438220667066,4.36096982095613,31.4744127033));
#55862=CARTESIAN_POINT('Ctrl Pts',(-5.29623967409301,4.21638337870418,31.4833182807965));
#55863=CARTESIAN_POINT('Ctrl Pts',(-5.41210179073021,4.06660482120568,31.492223858293));
#55864=CARTESIAN_POINT('Ctrl Pts',(-5.52153582322863,3.91215172926651,31.5011294357896));
#55865=CARTESIAN_POINT('Ctrl Pts',(-5.62757228362368,3.76249390534837,31.5097585239621));
#55866=CARTESIAN_POINT('Ctrl Pts',(-5.72757361259153,3.60844771641768,31.5183876121346));
#55867=CARTESIAN_POINT('Ctrl Pts',(-5.82118697962478,3.45051751890161,31.5270167003072));
#55868=CARTESIAN_POINT('Ctrl Pts',(-5.91929962214053,3.28499682989753,31.5360605224657));
#55869=CARTESIAN_POINT('Ctrl Pts',(-6.0103949046184,3.11520983685613,31.5451043446242));
#55870=CARTESIAN_POINT('Ctrl Pts',(-6.0941174845633,2.9417717593892,31.5541481667827));
#55871=CARTESIAN_POINT('Ctrl Pts',(-6.1778400645082,2.76833368192228,31.5631919889412));
#55872=CARTESIAN_POINT('Ctrl Pts',(-6.25418974322116,2.5912448519767,31.5722358110998));
#55873=CARTESIAN_POINT('Ctrl Pts',(-6.32286637598467,2.41115113409395,31.5812796332583));
#55874=CARTESIAN_POINT('Ctrl Pts',(-6.38454938399387,2.24939710225573,31.5894024857074));
#55875=CARTESIAN_POINT('Ctrl Pts',(-6.44003201479634,2.08524629932887,31.5975253381565));
#55876=CARTESIAN_POINT('Ctrl Pts',(-6.48913545647371,1.91922120338844,31.6056481906056));
#55877=CARTESIAN_POINT('Ctrl Pts',(-6.53825536735526,1.75314042293563,31.6137737674445));
#55878=CARTESIAN_POINT('Ctrl Pts',(-6.58099170619849,1.58518444405631,31.6218993442833));
#55879=CARTESIAN_POINT('Ctrl Pts',(-6.61721562648338,1.41589065701564,31.6300249211222));
#55880=CARTESIAN_POINT('Ctrl Pts',(-6.65344540730411,1.24656948055111,31.6381518125685));
#55881=CARTESIAN_POINT('Ctrl Pts',(-6.68316060146275,1.07591042487806,31.6462787040148));
#55882=CARTESIAN_POINT('Ctrl Pts',(-6.70628368056084,0.904460168190584,
31.6544055954611));
#55883=CARTESIAN_POINT('Ctrl Pts',(-6.72942557385929,0.732870410208039,
31.6625390993903));
#55884=CARTESIAN_POINT('Ctrl Pts',(-6.74596459569385,0.560488529650756,
31.6706726033194));
#55885=CARTESIAN_POINT('Ctrl Pts',(-6.75587513796982,0.387866111127572,
31.6788061072486));
#55886=CARTESIAN_POINT('Ctrl Pts',(-6.76333781332565,0.257880785127765,
31.6849306660909));
#55887=CARTESIAN_POINT('Ctrl Pts',(-6.76704311804857,0.127759179243045,
31.6910552249333));
#55888=CARTESIAN_POINT('Ctrl Pts',(-6.76699962134934,-0.00226377072111077,
31.6971797837756));
#55889=CARTESIAN_POINT('',(-6.767,4.09441144183509E-12,31.3028202161898));
#55890=CARTESIAN_POINT('Ctrl Pts',(3.09908550384718,6.01564277861014,30.6513967904261));
#55891=CARTESIAN_POINT('Ctrl Pts',(2.93373232018331,6.10082796552479,30.6601462383254));
#55892=CARTESIAN_POINT('Ctrl Pts',(2.76486502144433,6.17919158180187,30.6688956862247));
#55893=CARTESIAN_POINT('Ctrl Pts',(2.59305716434363,6.25046746591374,30.677645134124));
#55894=CARTESIAN_POINT('Ctrl Pts',(2.42125069459292,6.32174277447221,30.6863945113714));
#55895=CARTESIAN_POINT('Ctrl Pts',(2.24650397871066,6.38593035557823,30.6951438886189));
#55896=CARTESIAN_POINT('Ctrl Pts',(2.06941053323777,6.44281220003537,30.7038932658663));
#55897=CARTESIAN_POINT('Ctrl Pts',(1.892318458967,6.4996936040668,30.7126425753689));
#55898=CARTESIAN_POINT('Ctrl Pts',(1.71287996431534,6.54926929700873,30.7213918848714));
#55899=CARTESIAN_POINT('Ctrl Pts',(1.53170449173545,6.59137090065469,30.730141194374));
#55900=CARTESIAN_POINT('Ctrl Pts',(1.35053036178223,6.63347219230072,30.7388904390386));
#55901=CARTESIAN_POINT('Ctrl Pts',(1.1676195587891,6.66809944062442,30.7476396837032));
#55902=CARTESIAN_POINT('Ctrl Pts',(0.983593309311263,6.6951350398538,30.7563889283678));
#55903=CARTESIAN_POINT('Ctrl Pts',(0.799568362460831,6.72217044771204,30.765138111101));
#55904=CARTESIAN_POINT('Ctrl Pts',(0.614428268439518,6.74161427235968,30.7738872938341));
#55905=CARTESIAN_POINT('Ctrl Pts',(0.428801816331264,6.75340047696796,30.7826364765673));
#55906=CARTESIAN_POINT('Ctrl Pts',(0.243176616523825,6.76518660206238,30.7913856002754));
#55907=CARTESIAN_POINT('Ctrl Pts',(0.0570653511665475,6.76931519233996,
30.8001347239836));
#55908=CARTESIAN_POINT('Ctrl Pts',(-0.128899900798899,6.76577222610797,
30.8088838476917));
#55909=CARTESIAN_POINT('Ctrl Pts',(-0.31486395994078,6.76222928260138,30.817632915281));
#55910=CARTESIAN_POINT('Ctrl Pts',(-0.500681721079332,6.75101488651286,
30.8263819828702));
#55911=CARTESIAN_POINT('Ctrl Pts',(-0.685722110171844,6.73216712416006,
30.8351310504595));
#55912=CARTESIAN_POINT('Ctrl Pts',(-0.870761373826321,6.71331947644162,
30.8438800648358));
#55913=CARTESIAN_POINT('Ctrl Pts',(-1.0550229898423,6.68683858440015,30.8526290792122));
#55914=CARTESIAN_POINT('Ctrl Pts',(-1.23788117675963,6.65281438131444,30.8613780935886));
#55915=CARTESIAN_POINT('Ctrl Pts',(-1.43009641451701,6.61704912302397,30.8705748044761));
#55916=CARTESIAN_POINT('Ctrl Pts',(-1.62076048992608,6.57294837083187,30.8797715153636));
#55917=CARTESIAN_POINT('Ctrl Pts',(-1.80915798961049,6.52067760042072,30.8889682262512));
#55918=CARTESIAN_POINT('Ctrl Pts',(-1.98840443002933,6.47094578577433,30.8977182239577));
#55919=CARTESIAN_POINT('Ctrl Pts',(-2.16559895952116,6.41381888474501,30.9064682216642));
#55920=CARTESIAN_POINT('Ctrl Pts',(-2.3401396624225,6.34949095285261,30.9152182193707));
#55921=CARTESIAN_POINT('Ctrl Pts',(-2.51467682553944,6.28516432556713,30.9239680396223));
#55922=CARTESIAN_POINT('Ctrl Pts',(-2.68656000078773,6.21363705879691,30.9327178598739));
#55923=CARTESIAN_POINT('Ctrl Pts',(-2.85520533840821,6.13515211510891,30.9414676801255));
#55924=CARTESIAN_POINT('Ctrl Pts',(-3.02384747998257,6.05666865881156,30.9502173345567));
#55925=CARTESIAN_POINT('Ctrl Pts',(-3.18925164684464,5.97122791039883,30.958966988988));
#55926=CARTESIAN_POINT('Ctrl Pts',(-3.35085601829082,5.87912008251951,30.9677166434192));
#55927=CARTESIAN_POINT('Ctrl Pts',(-3.51245754191338,5.78701387778223,30.9764661436623));
#55928=CARTESIAN_POINT('Ctrl Pts',(-3.67025915510852,5.68824097061037,30.9852156439055));
#55929=CARTESIAN_POINT('Ctrl Pts',(-3.82372487928746,5.58313684656915,30.9939651441486));
#55930=CARTESIAN_POINT('Ctrl Pts',(-3.97718810300689,5.47803443501851,31.0027145018337));
#55931=CARTESIAN_POINT('Ctrl Pts',(-4.12631534262898,5.36660117496473,31.0114638595188));
#55932=CARTESIAN_POINT('Ctrl Pts',(-4.2706000988608,5.24921554097468,31.0202132172039));
#55933=CARTESIAN_POINT('Ctrl Pts',(-4.41488269594072,5.13183166360413,31.0289624439591));
#55934=CARTESIAN_POINT('Ctrl Pts',(-4.55432273234951,5.00849577139596,31.0377116707143));
#55935=CARTESIAN_POINT('Ctrl Pts',(-4.68844662480073,4.87962675277471,31.0464608974695));
#55936=CARTESIAN_POINT('Ctrl Pts',(-4.82256868835018,4.75075949140023,31.0552100049209));
#55937=CARTESIAN_POINT('Ctrl Pts',(-4.95137454637718,4.61635945312679,31.0639591123724));
#55938=CARTESIAN_POINT('Ctrl Pts',(-5.0744267446093,4.47688309134758,31.0727082198239));
#55939=CARTESIAN_POINT('Ctrl Pts',(-5.19747742838395,4.33740844616524,31.0814572195963));
#55940=CARTESIAN_POINT('Ctrl Pts',(-5.31477440450787,4.19285781736207,31.0902062193687));
#55941=CARTESIAN_POINT('Ctrl Pts',(-5.42591931531016,4.0437221199959,31.098955219141));
#55942=CARTESIAN_POINT('Ctrl Pts',(-5.53707636462853,3.89457013500984,31.1077051744216));
#55943=CARTESIAN_POINT('Ctrl Pts',(-5.6420798327335,3.74083230916602,31.1164551297022));
#55944=CARTESIAN_POINT('Ctrl Pts',(-5.74057303468635,3.58303087252008,31.1252050849828));
#55945=CARTESIAN_POINT('Ctrl Pts',(-5.83906243363655,3.42523552887618,31.1339547024116));
#55946=CARTESIAN_POINT('Ctrl Pts',(-5.93104191768319,3.26337713157186,31.1427043198404));
#55947=CARTESIAN_POINT('Ctrl Pts',(-6.01619906699553,3.09800545291355,31.1514539372692));
#55948=CARTESIAN_POINT('Ctrl Pts',(-6.10135338095288,2.93263928039793,31.1602032633746));
#55949=CARTESIAN_POINT('Ctrl Pts',(-6.17968568352752,2.76376031540419,31.16895258948));
#55950=CARTESIAN_POINT('Ctrl Pts',(-6.25092992694807,2.59194213831734,31.1777019155854));
#55951=CARTESIAN_POINT('Ctrl Pts',(-6.32217217691038,2.42012876880994,31.1864509968792));
#55952=CARTESIAN_POINT('Ctrl Pts',(-6.38632665483796,2.24537661647826,31.195200078173));
#55953=CARTESIAN_POINT('Ctrl Pts',(-6.44317547869306,2.06827917621592,31.2039491594668));
#55954=CARTESIAN_POINT('Ctrl Pts',(-6.50002944235893,1.89116572423572,31.2126990317817));
#55955=CARTESIAN_POINT('Ctrl Pts',(-6.54957634250356,1.71170683289359,31.2214489040967));
#55956=CARTESIAN_POINT('Ctrl Pts',(-6.59164787708355,1.53051209225537,31.2301987764117));
#55957=CARTESIAN_POINT('Ctrl Pts',(-6.63371649074972,1.3493299314821,31.2389480412465));
#55958=CARTESIAN_POINT('Ctrl Pts',(-6.66831071257091,1.16641244174191,31.2476973060813));
#55959=CARTESIAN_POINT('Ctrl Pts',(-6.69531304840304,0.982380875161951,
31.256446570916));
#55960=CARTESIAN_POINT('Ctrl Pts',(-6.72231677033021,0.798339861797786,
31.2651962848717));
#55961=CARTESIAN_POINT('Ctrl Pts',(-6.74172778477872,0.613184940732099,
31.2739459988273));
#55962=CARTESIAN_POINT('Ctrl Pts',(-6.75348015835506,0.427545027692498,
31.282695712783));
#55963=CARTESIAN_POINT('Ctrl Pts',(-6.76249038365209,0.285219953549511,
31.2894038805853));
#55964=CARTESIAN_POINT('Ctrl Pts',(-6.76699999999992,0.142609995760739,
31.2961120483875));
#55965=CARTESIAN_POINT('Ctrl Pts',(-6.767,4.09441144960993E-12,31.3028202161898));
#55966=CARTESIAN_POINT('Ctrl Pts',(-6.76699999999999,3.85398425696932E-7,
31.3028286423802));
#55967=CARTESIAN_POINT('Ctrl Pts',(-6.76700001009724,-0.177291765525944,
31.3111296342103));
#55968=CARTESIAN_POINT('Ctrl Pts',(-6.76002823219753,-0.35452500436781,
31.3194306260403));
#55969=CARTESIAN_POINT('Ctrl Pts',(-6.7461245034264,-0.531124452713244,
31.3277316178704));
#55970=CARTESIAN_POINT('Ctrl Pts',(-6.73221366727717,-0.707814176054133,
31.3360368530433));
#55971=CARTESIAN_POINT('Ctrl Pts',(-6.71136384379665,-0.883869119375745,
31.3443420882161));
#55972=CARTESIAN_POINT('Ctrl Pts',(-6.68366659620006,-1.05872084651222,
31.352647323389));
#55973=CARTESIAN_POINT('Ctrl Pts',(-6.65593315543186,-1.23380105983825,
31.3609634113659));
#55974=CARTESIAN_POINT('Ctrl Pts',(-6.62133446535324,-1.40767457409,31.3692794993429));
#55975=CARTESIAN_POINT('Ctrl Pts',(-6.58001323514508,-1.5797831576883,31.3775955873198));
#55976=CARTESIAN_POINT('Ctrl Pts',(-6.53866348691055,-1.75201052277253,
31.385917414681));
#55977=CARTESIAN_POINT('Ctrl Pts',(-6.49058203898741,-1.92247019636217,
31.3942392420421));
#55978=CARTESIAN_POINT('Ctrl Pts',(-6.43596117186355,-2.09062019369009,
31.4025610694033));
#55979=CARTESIAN_POINT('Ctrl Pts',(-6.38125239988589,-2.25904080555985,
31.4108962896133));
#55980=CARTESIAN_POINT('Ctrl Pts',(-6.31998329308616,-2.42514398813847,
31.4192315098233));
#55981=CARTESIAN_POINT('Ctrl Pts',(-6.25239444022301,-2.58840737981261,
31.4275667300333));
#55982=CARTESIAN_POINT('Ctrl Pts',(-6.19730143494457,-2.72148658619436,
31.4343609322068));
#55983=CARTESIAN_POINT('Ctrl Pts',(-6.13801039301637,-2.85267932733502,
31.4411551343802));
#55984=CARTESIAN_POINT('Ctrl Pts',(-6.07467368380669,-2.98171572006227,
31.4479493365537));
#55985=CARTESIAN_POINT('Ctrl Pts',(-5.99591537686446,-3.14217065925854,
31.4563978313822));
#55986=CARTESIAN_POINT('Ctrl Pts',(-5.91072768780452,-3.29964212496179,
31.4648463262106));
#55987=CARTESIAN_POINT('Ctrl Pts',(-5.81935924605262,-3.45359913212027,
31.473294821039));
#55988=CARTESIAN_POINT('Ctrl Pts',(-5.7280742640647,-3.60741550849602,31.4817355986582));
#55989=CARTESIAN_POINT('Ctrl Pts',(-5.63061995245565,-3.75772353995931,
31.4901763762773));
#55990=CARTESIAN_POINT('Ctrl Pts',(-5.52729130552716,-3.90401585855436,
31.4986171538965));
#55991=CARTESIAN_POINT('Ctrl Pts',(-5.42404115359031,-4.05019704422869,
31.5070515193658));
#55992=CARTESIAN_POINT('Ctrl Pts',(-5.31492575410719,-4.19236832701484,
31.5154858848351));
#55993=CARTESIAN_POINT('Ctrl Pts',(-5.20028415625305,-4.33005007987478,
31.5239202503044));
#55994=CARTESIAN_POINT('Ctrl Pts',(-5.08571204217955,-4.46764838441495,
31.532349503741));
#55995=CARTESIAN_POINT('Ctrl Pts',(-4.96562062041456,-4.60076232855225,
31.5407787571776));
#55996=CARTESIAN_POINT('Ctrl Pts',(-4.84039031513101,-4.72894391986053,
31.5492080106142));
#55997=CARTESIAN_POINT('Ctrl Pts',(-4.71521670143398,-4.8570674835392,31.5576334481394));
#55998=CARTESIAN_POINT('Ctrl Pts',(-4.58490907565386,-4.98026290865399,
31.5660588856645));
#55999=CARTESIAN_POINT('Ctrl Pts',(-4.44988621019408,-5.0981174678821,31.5744843231897));
#56000=CARTESIAN_POINT('Ctrl Pts',(-4.31489300562593,-5.21594613763365,
31.5829079098729));
#56001=CARTESIAN_POINT('Ctrl Pts',(-4.17518687582563,-5.32843605967748,
31.5913314965561));
#56002=CARTESIAN_POINT('Ctrl Pts',(-4.03122170360776,-5.43521302032972,
31.5997550832393));
#56003=CARTESIAN_POINT('Ctrl Pts',(-3.88727264033771,-5.54197803320001,
31.6081777273673));
#56004=CARTESIAN_POINT('Ctrl Pts',(-3.73906575244608,-5.64303116049174,
31.6166003714953));
#56005=CARTESIAN_POINT('Ctrl Pts',(-3.58708634329544,-5.73803978425937,
31.6250230156233));
#56006=CARTESIAN_POINT('Ctrl Pts',(-3.43510274693006,-5.83305102562837,
31.6334458918052));
#56007=CARTESIAN_POINT('Ctrl Pts',(-3.27934670499372,-5.9220172550498,31.6418687679872));
#56008=CARTESIAN_POINT('Ctrl Pts',(-3.12033102343843,-6.00465014003045,
31.6502916441691));
#56009=CARTESIAN_POINT('Ctrl Pts',(-2.96128878538232,-6.08729682516123,
31.6587159270181));
#56010=CARTESIAN_POINT('Ctrl Pts',(-2.7989861184597,-6.16360790392657,31.6671402098671));
#56011=CARTESIAN_POINT('Ctrl Pts',(-2.63395918026583,-6.23334164286648,
31.675564492716));
#56012=CARTESIAN_POINT('Ctrl Pts',(-2.46882078897949,-6.30312247739538,
31.6839944650142));
#56013=CARTESIAN_POINT('Ctrl Pts',(-2.30095475736142,-6.36631696590148,
31.6924244373123));
#56014=CARTESIAN_POINT('Ctrl Pts',(-2.13091686438916,-6.42273168652263,
31.7008544096105));
#56015=CARTESIAN_POINT('Ctrl Pts',(-1.96081818561475,-6.47916657449581,
31.7092873954877));
#56016=CARTESIAN_POINT('Ctrl Pts',(-1.78854641571458,-6.52881676278467,
31.7177203813648));
#56017=CARTESIAN_POINT('Ctrl Pts',(-1.61467169920262,-6.5715389600758,31.726153367242));
#56018=CARTESIAN_POINT('Ctrl Pts',(-1.44063701901058,-6.61430046152821,
31.7345941114148));
#56019=CARTESIAN_POINT('Ctrl Pts',(-1.26499677117063,-6.65012116395491,
31.7430348555876));
#56020=CARTESIAN_POINT('Ctrl Pts',(-1.08833156359738,-6.67890884858281,
31.7514755997604));
#56021=CARTESIAN_POINT('Ctrl Pts',(-0.99064865201976,-6.69482632826462,
31.7561427126459));
#56022=CARTESIAN_POINT('Ctrl Pts',(-0.892652510235858,-6.70859453374112,
31.7608098255314));
#56023=CARTESIAN_POINT('Ctrl Pts',(-0.794441887477484,-6.72020469088712,
31.7654769384169));
#56024=CARTESIAN_POINT('Ctrl Pts',(-0.623122109235702,-6.74045758707839,
31.7736183056347));
#56025=CARTESIAN_POINT('Ctrl Pts',(-0.450809018270542,-6.75418076647741,
31.7817596728526));
#56026=CARTESIAN_POINT('Ctrl Pts',(-0.27804582147657,-6.7612853453437,31.7899010400705));
#56027=CARTESIAN_POINT('Ctrl Pts',(-0.105433433813596,-6.76838372245299,
31.7980353004939));
#56028=CARTESIAN_POINT('Ctrl Pts',(0.0676279143409377,-6.7688749843508,
31.8061695609174));
#56029=CARTESIAN_POINT('Ctrl Pts',(0.24058810366446,-6.76272181627894,31.8143038213409));
#56030=CARTESIAN_POINT('Ctrl Pts',(0.413430305793929,-6.7565728456761,31.8224325328657));
#56031=CARTESIAN_POINT('Ctrl Pts',(0.586171122158248,-6.74378848230862,
31.8305612443905));
#56032=CARTESIAN_POINT('Ctrl Pts',(0.758258667673219,-6.72438345076323,
31.8386899559153));
#56033=CARTESIAN_POINT('Ctrl Pts',(0.930264147817969,-6.70498767311878,
31.8468147910079));
#56034=CARTESIAN_POINT('Ctrl Pts',(1.10161661451117,-6.6789775554696,31.8549396261004));
#56035=CARTESIAN_POINT('Ctrl Pts',(1.27176756200563,-6.64641980830509,31.8630644611929));
#56036=CARTESIAN_POINT('Ctrl Pts',(1.44187087526515,-6.61387117577321,31.871187021715));
#56037=CARTESIAN_POINT('Ctrl Pts',(1.61077298025001,-6.57477863431058,31.8793095822372));
#56038=CARTESIAN_POINT('Ctrl Pts',(1.77793387804411,-6.52926030460596,31.8874321427593));
#56039=CARTESIAN_POINT('Ctrl Pts',(1.94510366000662,-6.48373955572009,31.8955551349745));
#56040=CARTESIAN_POINT('Ctrl Pts',(2.11053169567993,-6.43179242874369,31.9036781271897));
#56041=CARTESIAN_POINT('Ctrl Pts',(2.27369132140218,-6.37358743369701,31.9118011194049));
#56042=CARTESIAN_POINT('Ctrl Pts',(2.35697933811328,-6.34387555749811,31.915947659386));
#56043=CARTESIAN_POINT('Ctrl Pts',(2.43967650322425,-6.31253381200568,31.9200941993671));
#56044=CARTESIAN_POINT('Ctrl Pts',(2.52171455836815,-6.27958953165843,31.9242407393482));
#56045=CARTESIAN_POINT('Ctrl Pts',(2.69945356923415,-6.20821431692009,31.9332243983766));
#56046=CARTESIAN_POINT('Ctrl Pts',(2.87400969861641,-6.12934957648348,31.9422080574049));
#56047=CARTESIAN_POINT('Ctrl Pts',(3.04478884474696,-6.04330620529065,31.9511917164333));
#56048=CARTESIAN_POINT('Ctrl Pts',(3.21586138764105,-5.9571150124978,31.9601908092926));
#56049=CARTESIAN_POINT('Ctrl Pts',(3.38314376436154,-5.86372064674218,31.969189902152));
#56050=CARTESIAN_POINT('Ctrl Pts',(3.54606770778625,-5.76347922801806,31.9781889950114));
#56051=CARTESIAN_POINT('Ctrl Pts',(3.70937366232987,-5.66300277117907,31.9872091882288));
#56052=CARTESIAN_POINT('Ctrl Pts',(3.86830053205349,-5.55564726513335,31.9962293814461));
#56053=CARTESIAN_POINT('Ctrl Pts',(4.02230794127331,-5.4418129171784,32.0052495746635));
#56054=CARTESIAN_POINT('Ctrl Pts',(4.17647132155895,-5.32786328344164,32.0142789030851));
#56055=CARTESIAN_POINT('Ctrl Pts',(4.32570509960904,-5.20742184651481,32.0233082315069));
#56056=CARTESIAN_POINT('Ctrl Pts',(4.46950188560458,-5.08092923534437,32.0323375599285));
#56057=CARTESIAN_POINT('Ctrl Pts',(4.61350139608383,-4.95425829508879,32.0413796178833));
#56058=CARTESIAN_POINT('Ctrl Pts',(4.75204840847654,-4.82151928092027,32.050421675838));
#56059=CARTESIAN_POINT('Ctrl Pts',(4.88467063155627,-4.68319141411193,32.0594637337928));
#56060=CARTESIAN_POINT('Ctrl Pts',(4.9997636817242,-4.56314685638631,32.0673106692885));
#56061=CARTESIAN_POINT('Ctrl Pts',(5.11039516174533,-4.43889385236908,32.0751576047843));
#56062=CARTESIAN_POINT('Ctrl Pts',(5.21628047439694,-4.31076640661788,32.08300454028));
#56063=CARTESIAN_POINT('Ctrl Pts',(5.33304895981509,-4.16946968277394,32.0916580045808));
#56064=CARTESIAN_POINT('Ctrl Pts',(5.44414737920278,-4.02333573848796,32.1003114688816));
#56065=CARTESIAN_POINT('Ctrl Pts',(5.5491821175239,-3.87283705138145,32.1089649331824));
#56066=CARTESIAN_POINT('Ctrl Pts',(5.6541200973669,-3.72247700434923,32.1176104258726));
#56067=CARTESIAN_POINT('Ctrl Pts',(5.75300536396091,-3.56776048255794,32.1262559185628));
#56068=CARTESIAN_POINT('Ctrl Pts',(5.84548543773335,-3.40919183931433,32.134901411253));
#56069=CARTESIAN_POINT('Ctrl Pts',(5.94074761576993,-3.24585293064452,32.1438069887495));
#56070=CARTESIAN_POINT('Ctrl Pts',(6.02921298958072,-3.07842675588515,32.152712566246));
#56071=CARTESIAN_POINT('Ctrl Pts',(6.11054397824642,-2.90749742732757,32.1616181437425));
#56072=CARTESIAN_POINT('Ctrl Pts',(6.18934990325549,-2.74187490054964,32.1702472319151));
#56073=CARTESIAN_POINT('Ctrl Pts',(6.26145764313278,-2.57296377608173,32.1788763200876));
#56074=CARTESIAN_POINT('Ctrl Pts',(6.32660606909151,-2.40132143757027,32.1875054082601));
#56075=CARTESIAN_POINT('Ctrl Pts',(6.39488567946284,-2.22142957027925,32.1965492304186));
#56076=CARTESIAN_POINT('Ctrl Pts',(6.45552035026923,-2.03853777114086,32.2055930525772));
#56077=CARTESIAN_POINT('Ctrl Pts',(6.50826548648449,-1.85331307593585,32.2146368747357));
#56078=CARTESIAN_POINT('Ctrl Pts',(6.56101062269975,-1.66808838073083,32.2236806968943));
#56079=CARTESIAN_POINT('Ctrl Pts',(6.60586608548287,-1.48053115055913,32.2327245190528));
#56080=CARTESIAN_POINT('Ctrl Pts',(6.64264691453548,-1.29132914813085,32.2417683412113));
#56081=CARTESIAN_POINT('Ctrl Pts',(6.67691423322725,-1.11505673988637,32.2501941310611));
#56082=CARTESIAN_POINT('Ctrl Pts',(6.70415801674973,-0.937433912934323,
32.2586199209109));
#56083=CARTESIAN_POINT('Ctrl Pts',(6.72429472379184,-0.759045102470971,
32.2670457107607));
#56084=CARTESIAN_POINT('Ctrl Pts',(6.74443610322751,-0.580614899801526,
32.2754734556772));
#56085=CARTESIAN_POINT('Ctrl Pts',(6.7574670809708,-0.401418688658511,32.2839012005938));
#56086=CARTESIAN_POINT('Ctrl Pts',(6.76335602080805,-0.222045796626584,
32.2923289455103));
#56087=CARTESIAN_POINT('Ctrl Pts',(6.7692471245352,-0.0426069940570784,
32.3007597872002));
#56088=CARTESIAN_POINT('Ctrl Pts',(6.76799094678658,0.137008287681627,32.3091906288901));
#56089=CARTESIAN_POINT('Ctrl Pts',(6.75960796831947,0.316210554270361,32.31762147058));
#56090=CARTESIAN_POINT('Ctrl Pts',(6.75121728696513,0.495577484869227,32.3260600591374));
#56091=CARTESIAN_POINT('Ctrl Pts',(6.73568673686856,0.674530310722837,32.3344986476947));
#56092=CARTESIAN_POINT('Ctrl Pts',(6.71308879052693,0.852483366700916,32.342937236252));
#56093=CARTESIAN_POINT('Ctrl Pts',(6.69047899482105,1.03052973339614,32.3513802496322));
#56094=CARTESIAN_POINT('Ctrl Pts',(6.66079446146052,1.20757495719898,32.3598232630124));
#56095=CARTESIAN_POINT('Ctrl Pts',(6.6241589308752,1.38304282598419,32.3682662763926));
#56096=CARTESIAN_POINT('Ctrl Pts',(6.58748491211128,1.55869503599674,32.3767181597469));
#56097=CARTESIAN_POINT('Ctrl Pts',(6.54384538413784,1.73276625823651,32.3851700431012));
#56098=CARTESIAN_POINT('Ctrl Pts',(6.49341443362765,1.9046936743624,32.3936219264555));
#56099=CARTESIAN_POINT('Ctrl Pts',(6.47967040637978,1.95154932685327,32.3959253316847));
#56100=CARTESIAN_POINT('Ctrl Pts',(6.46542223746913,1.99824585363452,32.3982287369138));
#56101=CARTESIAN_POINT('Ctrl Pts',(6.45067407628573,2.04477210503648,32.400532142143));
#56102=CARTESIAN_POINT('Ctrl Pts',(6.39741524044961,2.21278857533894,32.4088502422396));
#56103=CARTESIAN_POINT('Ctrl Pts',(6.33753650125075,2.37888527235834,32.4171683423362));
#56104=CARTESIAN_POINT('Ctrl Pts',(6.27119724463434,2.54251334684612,32.4254864424328));
#56105=CARTESIAN_POINT('Ctrl Pts',(6.20491570892634,2.70599905071382,32.4337973050607));
#56106=CARTESIAN_POINT('Ctrl Pts',(6.1321849867042,2.86702009110896,32.4421081676886));
#56107=CARTESIAN_POINT('Ctrl Pts',(6.05321394639003,3.02504378798543,32.4504190303165));
#56108=CARTESIAN_POINT('Ctrl Pts',(5.97369014889362,3.18417357049868,32.4587880647626));
#56109=CARTESIAN_POINT('Ctrl Pts',(5.88783843755256,3.34026354500124,32.4671570992088));
#56110=CARTESIAN_POINT('Ctrl Pts',(5.79592159995018,3.49278997468084,32.475526133655));
#56111=CARTESIAN_POINT('Ctrl Pts',(5.70475335629834,3.64407419057747,32.48382700857));
#56112=CARTESIAN_POINT('Ctrl Pts',(5.60761859757572,3.791852389679,32.492127883485));
#56113=CARTESIAN_POINT('Ctrl Pts',(5.50481991256358,3.93563803343798,32.5004287584001));
#56114=CARTESIAN_POINT('Ctrl Pts',(5.40204866565804,4.0793852992175,32.5087274177197));
#56115=CARTESIAN_POINT('Ctrl Pts',(5.29361670686519,4.21914185041018,32.5170260770393));
#56116=CARTESIAN_POINT('Ctrl Pts',(5.17986971979655,4.35445044591563,32.525324736359));
#56117=CARTESIAN_POINT('Ctrl Pts',(5.0661342121998,4.48974538592779,32.5336225581687));
#56118=CARTESIAN_POINT('Ctrl Pts',(4.94708496951385,4.62059299913685,32.5419203799785));
#56119=CARTESIAN_POINT('Ctrl Pts',(4.82310781680742,4.74656928606875,32.5502182017882));
#56120=CARTESIAN_POINT('Ctrl Pts',(4.69728322650426,4.87442280056793,32.558639673058));
#56121=CARTESIAN_POINT('Ctrl Pts',(4.56638293228499,4.9972583754097,32.5670611443277));
#56122=CARTESIAN_POINT('Ctrl Pts',(4.43084893714561,5.11467170952307,32.5754826155974));
#56123=CARTESIAN_POINT('Ctrl Pts',(4.29722719054381,5.23042845942507,32.5837852683663));
#56124=CARTESIAN_POINT('Ctrl Pts',(4.15910193248385,5.34091477065818,32.5920879211352));
#56125=CARTESIAN_POINT('Ctrl Pts',(4.01692982274302,5.44578403897527,32.600390573904));
#56126=CARTESIAN_POINT('Ctrl Pts',(3.87170579500402,5.55290446898655,32.6088714544242));
#56127=CARTESIAN_POINT('Ctrl Pts',(3.72225951820408,5.65416374958702,32.6173523349444));
#56128=CARTESIAN_POINT('Ctrl Pts',(3.56910845987579,5.74923941070844,32.6258332154645));
#56129=CARTESIAN_POINT('Ctrl Pts',(3.4159574015475,5.84431507182986,32.6343140959847));
#56130=CARTESIAN_POINT('Ctrl Pts',(3.25910190906719,5.93320694589108,32.6427949765049));
#56131=CARTESIAN_POINT('Ctrl Pts',(3.09908550384733,6.01564277861006,32.651275857025));
#56132=CARTESIAN_POINT('Origin',(0.,0.,-63.6971797838103));
#56133=CARTESIAN_POINT('',(3.09908550384718,6.01564277861013,35.0459194627137));
#56134=CARTESIAN_POINT('',(3.09908550384707,6.01564277861019,34.6514623413619));
#56135=CARTESIAN_POINT('',(3.09908550384721,6.01564277861012,-63.6971797838103));
#56136=CARTESIAN_POINT('',(-6.76699913328736,0.0034249216301115,33.6971797837708));
#56137=CARTESIAN_POINT('Ctrl Pts',(-6.76699913328778,0.00342492080084751,
33.6971797838099));
#56138=CARTESIAN_POINT('Ctrl Pts',(-6.76708965214103,-0.175423302883435,
33.7056048624315));
#56139=CARTESIAN_POINT('Ctrl Pts',(-6.76008560640622,-0.354407685060025,
33.7140299410532));
#56140=CARTESIAN_POINT('Ctrl Pts',(-6.74598121021841,-0.532941377057729,
33.7224550196748));
#56141=CARTESIAN_POINT('Ctrl Pts',(-6.73188987970641,-0.711309683504007,
33.730872293684));
#56142=CARTESIAN_POINT('Ctrl Pts',(-6.71071134395962,-0.889227800981069,
33.7392895676932));
#56143=CARTESIAN_POINT('Ctrl Pts',(-6.68249185780763,-1.06611048692654,
33.7477068417025));
#56144=CARTESIAN_POINT('Ctrl Pts',(-6.65428790377499,-1.24289581592602,
33.75611948281));
#56145=CARTESIAN_POINT('Ctrl Pts',(-6.61905077549059,-1.41864652062158,
33.7645321239175));
#56146=CARTESIAN_POINT('Ctrl Pts',(-6.57687846791906,-1.5927832929255,33.7729447650251));
#56147=CARTESIAN_POINT('Ctrl Pts',(-6.53472619505594,-1.7668373384436,33.7813534095571));
#56148=CARTESIAN_POINT('Ctrl Pts',(-6.48564539169211,-1.93927865689273,
33.7897620540891));
#56149=CARTESIAN_POINT('Ctrl Pts',(-6.4297850314648,-2.10953868159635,33.7981706986212));
#56150=CARTESIAN_POINT('Ctrl Pts',(-6.41693674348431,-2.14869972209187,
33.8001047478474));
#56151=CARTESIAN_POINT('Ctrl Pts',(-6.40373000543813,-2.18774541800157,
33.8020387970736));
#56152=CARTESIAN_POINT('Ctrl Pts',(-6.39016700662022,-2.2266689532803,33.8039728462998));
#56153=CARTESIAN_POINT('Ctrl Pts',(-6.33107907016831,-2.39624143573127,
33.8123986361496));
#56154=CARTESIAN_POINT('Ctrl Pts',(-6.26524208101887,-2.56344664873282,
33.8208244259994));
#56155=CARTESIAN_POINT('Ctrl Pts',(-6.19287793451735,-2.72773750353075,
33.8292502158492));
#56156=CARTESIAN_POINT('Ctrl Pts',(-6.12049699709923,-2.89206647933437,
33.8376779607657));
#56157=CARTESIAN_POINT('Ctrl Pts',(-6.04158601622402,-3.0534794452517,33.8461057056822));
#56158=CARTESIAN_POINT('Ctrl Pts',(-5.95641420385625,-3.21145120344363,
33.8545334505988));
#56159=CARTESIAN_POINT('Ctrl Pts',(-5.8712110951206,-3.36948100833108,33.8629642922887));
#56160=CARTESIAN_POINT('Ctrl Pts',(-5.77974272506954,-3.52406679259694,
33.8713951339787));
#56161=CARTESIAN_POINT('Ctrl Pts',(-5.6823234274213,-3.67470943969439,33.8798259756686));
#56162=CARTESIAN_POINT('Ctrl Pts',(-5.58481461387319,-3.82549050815637,
33.888264564226));
#56163=CARTESIAN_POINT('Ctrl Pts',(-5.48134412803832,-3.97232092199644,
33.8967031527833));
#56164=CARTESIAN_POINT('Ctrl Pts',(-5.37226930641004,-4.11473103609514,
33.9051417413406));
#56165=CARTESIAN_POINT('Ctrl Pts',(-5.26313729076524,-4.25721582376466,
33.9135847547209));
#56166=CARTESIAN_POINT('Ctrl Pts',(-5.14839528601612,-4.3952754309605,33.9220277681012));
#56167=CARTESIAN_POINT('Ctrl Pts',(-5.02844017602248,-4.52847417969485,
33.9304707814815));
#56168=CARTESIAN_POINT('Ctrl Pts',(-4.90835904482523,-4.66181286299838,
33.9389226648358));
#56169=CARTESIAN_POINT('Ctrl Pts',(-4.78305409559201,-4.79028024606345,
33.9473745481901));
#56170=CARTESIAN_POINT('Ctrl Pts',(-4.65295898004466,-4.91347755973524,
33.9558264315445));
#56171=CARTESIAN_POINT('Ctrl Pts',(-4.61750395104761,-4.94705271980343,
33.9581298367734));
#56172=CARTESIAN_POINT('Ctrl Pts',(-4.58169333105088,-4.98023668318396,
33.9604332420023));
#56173=CARTESIAN_POINT('Ctrl Pts',(-4.54553631636656,-5.01302190266437,
33.9627366472312));
#56174=CARTESIAN_POINT('Ctrl Pts',(-4.41497853130123,-5.13140461970047,
33.9710539125646));
#56175=CARTESIAN_POINT('Ctrl Pts',(-4.27966702246925,-5.24479818046762,
33.979371177898));
#56176=CARTESIAN_POINT('Ctrl Pts',(-4.14001558193193,-5.3528086068307,33.9876884432314));
#56177=CARTESIAN_POINT('Ctrl Pts',(-4.00048192663891,-5.46072793471025,
33.9959986935915));
#56178=CARTESIAN_POINT('Ctrl Pts',(-3.85661590630194,-5.56327296237675,
34.0043089439516));
#56179=CARTESIAN_POINT('Ctrl Pts',(-3.70886596052665,-5.66008854054835,
34.0126191943117));
#56180=CARTESIAN_POINT('Ctrl Pts',(-3.56121357176315,-5.75684019288599,
34.0209239575415));
#56181=CARTESIAN_POINT('Ctrl Pts',(-3.40968265759789,-5.84786974395474,
34.0292287207714));
#56182=CARTESIAN_POINT('Ctrl Pts',(-3.2547525207898,-5.93286398195783,34.0375334840013));
#56183=CARTESIAN_POINT('Ctrl Pts',(-3.09989632101333,-6.01781765831298,
34.0458342839639));
#56184=CARTESIAN_POINT('Ctrl Pts',(-2.94164443581863,-6.09674159465641,
34.0541350839265));
#56185=CARTESIAN_POINT('Ctrl Pts',(-2.78050296652484,-6.16936724900914,
34.0624358838891));
#56186=CARTESIAN_POINT('Ctrl Pts',(-2.61940891053195,-6.24197153442426,
34.070734241474));
#56187=CARTESIAN_POINT('Ctrl Pts',(-2.455427281904,-6.3082810890148,34.0790325990589));
#56188=CARTESIAN_POINT('Ctrl Pts',(-2.2890866732251,-6.36807437161841,34.0873309566438));
#56189=CARTESIAN_POINT('Ctrl Pts',(-2.12272913977065,-6.42787373805144,
34.0956301585676));
#56190=CARTESIAN_POINT('Ctrl Pts',(-1.95401247144154,-6.48115538299653,
34.1039293604914));
#56191=CARTESIAN_POINT('Ctrl Pts',(-1.7834835928178,-6.52774656938746,34.1122285624152));
#56192=CARTESIAN_POINT('Ctrl Pts',(-1.61293742579809,-6.57434247924156,
34.1205286057207));
#56193=CARTESIAN_POINT('Ctrl Pts',(-1.44057901785703,-6.61424648633407,
34.1288286490263));
#56194=CARTESIAN_POINT('Ctrl Pts',(-1.26696866307933,-6.64733626400643,
34.1371286923318));
#56195=CARTESIAN_POINT('Ctrl Pts',(-1.09331188780462,-6.68043488933036,
34.1454309549297));
#56196=CARTESIAN_POINT('Ctrl Pts',(-0.918402840289488,-6.70671558864302,
34.1537332175277));
#56197=CARTESIAN_POINT('Ctrl Pts',(-0.742810361132624,-6.72610747515932,
34.1620354801256));
#56198=CARTESIAN_POINT('Ctrl Pts',(-0.567141779263084,-6.74550776622218,
34.1703413409682));
#56199=CARTESIAN_POINT('Ctrl Pts',(-0.390789520997402,-6.75801325588428,
34.1786472018108));
#56200=CARTESIAN_POINT('Ctrl Pts',(-0.214326073743895,-6.76360505456325,
34.1869530626534));
#56201=CARTESIAN_POINT('Ctrl Pts',(-0.0376540342455185,-6.76920346314278,
34.1952687416095));
#56202=CARTESIAN_POINT('Ctrl Pts',(0.139129108747934,-6.7678718413669,34.2035844205656));
#56203=CARTESIAN_POINT('Ctrl Pts',(0.315451153998915,-6.75964344987521,
34.2119000995217));
#56204=CARTESIAN_POINT('Ctrl Pts',(0.491884721539005,-6.75140985399143,
34.2202210380786));
#56205=CARTESIAN_POINT('Ctrl Pts',(0.667856263612172,-6.73627081892348,
34.2285419766354));
#56206=CARTESIAN_POINT('Ctrl Pts',(0.842800017963015,-6.71431136675397,
34.2368629151922));
#56207=CARTESIAN_POINT('Ctrl Pts',(1.01800379292136,-6.69231927603664,34.2451962212412));
#56208=CARTESIAN_POINT('Ctrl Pts',(1.19217638426054,-6.6634865661243,34.2535295272901));
#56209=CARTESIAN_POINT('Ctrl Pts',(1.36476218204342,-6.6279493952854,34.261862833339));
#56210=CARTESIAN_POINT('Ctrl Pts',(1.49179551870497,-6.60179193942767,34.2679966385907));
#56211=CARTESIAN_POINT('Ctrl Pts',(1.61796939998943,-6.57200318582296,34.2741304438425));
#56212=CARTESIAN_POINT('Ctrl Pts',(1.74306822618047,-6.5386544608872,34.2802642490942));
#56213=CARTESIAN_POINT('Ctrl Pts',(1.90768452566187,-6.49477120587597,34.2883356623363));
#56214=CARTESIAN_POINT('Ctrl Pts',(2.07094537377384,-6.44458654756956,34.2964070755783));
#56215=CARTESIAN_POINT('Ctrl Pts',(2.23231929035817,-6.3881953309127,34.3044784888204));
#56216=CARTESIAN_POINT('Ctrl Pts',(2.39349061535627,-6.33187490875766,34.3125397690716));
#56217=CARTESIAN_POINT('Ctrl Pts',(2.55277937468498,-6.26936355344841,34.3206010493228));
#56218=CARTESIAN_POINT('Ctrl Pts',(2.70966438187405,-6.200807039217,34.328662329574));
#56219=CARTESIAN_POINT('Ctrl Pts',(2.86638683853874,-6.13232155725017,34.3367152574316));
#56220=CARTESIAN_POINT('Ctrl Pts',(3.0207101604859,-6.05780352891701,34.3447681852893));
#56221=CARTESIAN_POINT('Ctrl Pts',(3.17212853550339,-5.97744841502168,34.3528211131469));
#56222=CARTESIAN_POINT('Ctrl Pts',(3.32342318119117,-5.89715896214258,34.3608674606713));
#56223=CARTESIAN_POINT('Ctrl Pts',(3.47181727672117,-5.81104209095456,34.3689138081957));
#56224=CARTESIAN_POINT('Ctrl Pts',(3.61682531321139,-5.71934119053177,34.3769601557201));
#56225=CARTESIAN_POINT('Ctrl Pts',(3.76174657875115,-5.62769516275246,34.3850016884132));
#56226=CARTESIAN_POINT('Ctrl Pts',(3.90328550435128,-5.53047195636487,34.3930432211064));
#56227=CARTESIAN_POINT('Ctrl Pts',(4.04098160901787,-5.42796063320096,34.4010847537995));
#56228=CARTESIAN_POINT('Ctrl Pts',(4.18132488515081,-5.32347855675891,34.4092808828478));
#56229=CARTESIAN_POINT('Ctrl Pts',(4.31767573316271,-5.21350315579193,34.417477011896));
#56230=CARTESIAN_POINT('Ctrl Pts',(4.44957764152242,-5.0983867852551,34.4256731409443));
#56231=CARTESIAN_POINT('Ctrl Pts',(4.57894692808211,-4.98548074080972,34.4337118977804));
#56232=CARTESIAN_POINT('Ctrl Pts',(4.70403629602601,-4.86762963010654,34.4417506546165));
#56233=CARTESIAN_POINT('Ctrl Pts',(4.82444889387516,-4.74520619893243,34.4497894114526));
#56234=CARTESIAN_POINT('Ctrl Pts',(4.94487314639105,-4.62277091846417,34.4578289463554));
#56235=CARTESIAN_POINT('Ctrl Pts',(5.06061946550275,-4.49576270252504,34.4658684812581));
#56236=CARTESIAN_POINT('Ctrl Pts',(5.17132854583285,-4.36459048148327,34.4739080161609));
#56237=CARTESIAN_POINT('Ctrl Pts',(5.28207026206822,-4.2333795922115,34.4819499210365));
#56238=CARTESIAN_POINT('Ctrl Pts',(5.38777154306417,-4.09800253976918,34.489991825912));
#56239=CARTESIAN_POINT('Ctrl Pts',(5.48811408449555,-3.95890045284818,34.4980337307875));
#56240=CARTESIAN_POINT('Ctrl Pts',(5.59184140885884,-3.81510613506593,34.5063469074683));
#56241=CARTESIAN_POINT('Ctrl Pts',(5.68984188934675,-3.66733143312462,34.5146600841492));
#56242=CARTESIAN_POINT('Ctrl Pts',(5.78181383338206,-3.51609411081556,34.52297326083));
#56243=CARTESIAN_POINT('Ctrl Pts',(5.8709390659472,-3.36953787929622,34.5310291284405));
#56244=CARTESIAN_POINT('Ctrl Pts',(5.9544032765479,-3.21973054106396,34.5390849960511));
#56245=CARTESIAN_POINT('Ctrl Pts',(6.0319800003596,-3.06716583758716,34.5471408636616));
#56246=CARTESIAN_POINT('Ctrl Pts',(6.11327349230423,-2.90729162682223,34.5555826948775));
#56247=CARTESIAN_POINT('Ctrl Pts',(6.18810126641518,-2.74438977672137,34.5640245260935));
#56248=CARTESIAN_POINT('Ctrl Pts',(6.25626078166885,-2.57904828022903,34.5724663573094));
#56249=CARTESIAN_POINT('Ctrl Pts',(6.32442029692256,-2.41370678373658,34.5809081885254));
#56250=CARTESIAN_POINT('Ctrl Pts',(6.38591147500212,-2.2459261032453,34.5893500197414));
#56251=CARTESIAN_POINT('Ctrl Pts',(6.44059276114633,-2.07630775297631,34.5977918509573));
#56252=CARTESIAN_POINT('Ctrl Pts',(6.49390488167561,-1.91093647934403,34.6060223070239));
#56253=CARTESIAN_POINT('Ctrl Pts',(6.54092172979095,-1.74326855251469,34.6142527630904));
#56254=CARTESIAN_POINT('Ctrl Pts',(6.58144113511989,-1.57382387354869,34.622483219157));
#56255=CARTESIAN_POINT('Ctrl Pts',(6.6219124415271,-1.40458033540115,34.6307039051872));
#56256=CARTESIAN_POINT('Ctrl Pts',(6.65590158058441,-1.23356459009026,34.6389245912175));
#56257=CARTESIAN_POINT('Ctrl Pts',(6.68325529423569,-1.06131412506884,34.6471452772477));
#56258=CARTESIAN_POINT('Ctrl Pts',(6.71058202541813,-0.889233572727791,
34.6553578541631));
#56259=CARTESIAN_POINT('Ctrl Pts',(6.7312863103825,-0.715921077884259,34.6635704310785));
#56260=CARTESIAN_POINT('Ctrl Pts',(6.74526531879975,-0.541926912966403,
34.671783007994));
#56261=CARTESIAN_POINT('Ctrl Pts',(6.75923334154567,-0.368069484693473,
34.6799891308986));
#56262=CARTESIAN_POINT('Ctrl Pts',(6.76648658607982,-0.19353180911163,34.6881952538032));
#56263=CARTESIAN_POINT('Ctrl Pts',(6.76697368452304,-0.0188720155952667,
34.6964013767079));
#56264=CARTESIAN_POINT('Ctrl Pts',(6.76746049783745,0.155685538749563,34.7046026960616));
#56265=CARTESIAN_POINT('Ctrl Pts',(6.76118905412521,0.330364711065663,34.7128040154154));
#56266=CARTESIAN_POINT('Ctrl Pts',(6.74815999195772,0.504604521324516,34.7210053347691));
#56267=CARTESIAN_POINT('Ctrl Pts',(6.73513466751953,0.678794346309399,34.7292043013586));
#56268=CARTESIAN_POINT('Ctrl Pts',(6.71535560884039,0.852544702931206,34.7374032679482));
#56269=CARTESIAN_POINT('Ctrl Pts',(6.68887552707403,1.02529663186323,34.7456022345377));
#56270=CARTESIAN_POINT('Ctrl Pts',(6.6623989421221,1.19802574812267,34.7538001184166));
#56271=CARTESIAN_POINT('Ctrl Pts',(6.62922314998981,1.36975634479695,34.7619980022955));
#56272=CARTESIAN_POINT('Ctrl Pts',(6.58945250612212,1.53993657972039,34.7701958861745));
#56273=CARTESIAN_POINT('Ctrl Pts',(6.5496798896958,1.71012525530406,34.778394176655));
#56274=CARTESIAN_POINT('Ctrl Pts',(6.50331185145674,1.87876306670202,34.7865924671355));
#56275=CARTESIAN_POINT('Ctrl Pts',(6.45050346000626,2.04531027290415,34.794790757616));
#56276=CARTESIAN_POINT('Ctrl Pts',(6.39768285657577,2.21189599327224,34.8029909439574));
#56277=CARTESIAN_POINT('Ctrl Pts',(6.33841904198215,2.37638980377696,34.8111911302987));
#56278=CARTESIAN_POINT('Ctrl Pts',(6.27291637400521,2.53826893073554,34.81939131664));
#56279=CARTESIAN_POINT('Ctrl Pts',(6.2073517783952,2.70030110170723,34.8275992556141));
#56280=CARTESIAN_POINT('Ctrl Pts',(6.13553667985029,2.85971331753786,34.8358071945882));
#56281=CARTESIAN_POINT('Ctrl Pts',(6.05772323735311,3.01600367699247,34.8440151335623));
#56282=CARTESIAN_POINT('Ctrl Pts',(5.97987204519757,3.17236985763538,34.8522270544562));
#56283=CARTESIAN_POINT('Ctrl Pts',(5.89601687931091,3.32561084793011,34.8604389753502));
#56284=CARTESIAN_POINT('Ctrl Pts',(5.80645491842284,3.47525111039811,34.8686508962442));
#56285=CARTESIAN_POINT('Ctrl Pts',(5.71677013749364,3.62509658078034,34.8768740784867));
#56286=CARTESIAN_POINT('Ctrl Pts',(5.62136311756674,3.77133115481839,34.8850972607293));
#56287=CARTESIAN_POINT('Ctrl Pts',(5.52057395244849,3.91350894154431,34.8933204429718));
#56288=CARTESIAN_POINT('Ctrl Pts',(5.43069545323876,4.04029564601689,34.9006534462547));
#56289=CARTESIAN_POINT('Ctrl Pts',(5.33653768861316,4.16385664902198,34.9079864495375));
#56290=CARTESIAN_POINT('Ctrl Pts',(5.23836745235498,4.28389955929269,34.9153194528204));
#56291=CARTESIAN_POINT('Ctrl Pts',(5.11872529153638,4.43019841445657,34.9242563403282));
#56292=CARTESIAN_POINT('Ctrl Pts',(4.9928749510221,4.57157535941286,34.9331932278359));
#56293=CARTESIAN_POINT('Ctrl Pts',(4.86122711320063,4.70752163605044,34.9421301153437));
#56294=CARTESIAN_POINT('Ctrl Pts',(4.72987446156941,4.8431630883617,34.9510469641952));
#56295=CARTESIAN_POINT('Ctrl Pts',(4.59275043899065,4.97339799229441,34.9599638130466));
#56296=CARTESIAN_POINT('Ctrl Pts',(4.45030382908657,5.09775291955362,34.9688806618981));
#56297=CARTESIAN_POINT('Ctrl Pts',(4.30806194981394,5.22192911835591,34.977784695056));
#56298=CARTESIAN_POINT('Ctrl Pts',(4.16051293739821,5.34024202984869,34.9866887282139));
#56299=CARTESIAN_POINT('Ctrl Pts',(4.00814202564201,5.45225517582242,34.9955927613719));
#56300=CARTESIAN_POINT('Ctrl Pts',(3.85613176909673,5.56400319163239,35.004475719077));
#56301=CARTESIAN_POINT('Ctrl Pts',(3.69932259696003,5.6694810461941,35.0133586767822));
#56302=CARTESIAN_POINT('Ctrl Pts',(3.53823190768989,5.76829298557252,35.0222416344873));
#56303=CARTESIAN_POINT('Ctrl Pts',(3.39510098981263,5.85608852263642,35.0301342438961));
#56304=CARTESIAN_POINT('Ctrl Pts',(3.24859059684888,5.93862207051218,35.0380268533049));
#56305=CARTESIAN_POINT('Ctrl Pts',(3.0990855038472,6.01564277861013,35.0459194627137));
#56306=CARTESIAN_POINT('Ctrl Pts',(3.09908550384727,6.01564277861009,33.045773705108));
#56307=CARTESIAN_POINT('Ctrl Pts',(2.94004160920022,6.09757760195576,33.0542117246657));
#56308=CARTESIAN_POINT('Ctrl Pts',(2.77763778918707,6.17325722407048,33.0626497442234));
#56309=CARTESIAN_POINT('Ctrl Pts',(2.61239456112603,6.24241008401396,33.071087763781));
#56310=CARTESIAN_POINT('Ctrl Pts',(2.44726656488396,6.3115147204391,33.0795198991136));
#56311=CARTESIAN_POINT('Ctrl Pts',(2.27930341468169,6.37410154006354,33.0879520344462));
#56312=CARTESIAN_POINT('Ctrl Pts',(2.10904802773521,6.42994598863056,33.0963841697788));
#56313=CARTESIAN_POINT('Ctrl Pts',(1.93888523470524,6.48576006602225,33.1048117192687));
#56314=CARTESIAN_POINT('Ctrl Pts',(1.76643300670117,6.53483897979737,33.1132392687585));
#56315=CARTESIAN_POINT('Ctrl Pts',(1.59225231329541,6.57700703746054,33.1216668182484));
#56316=CARTESIAN_POINT('Ctrl Pts',(1.4148392827628,6.61995762374779,33.1302507609674));
#56317=CARTESIAN_POINT('Ctrl Pts',(1.23563333481011,6.65573821405969,33.1388347036864));
#56318=CARTESIAN_POINT('Ctrl Pts',(1.05524239882421,6.68421666911866,33.1474186464055));
#56319=CARTESIAN_POINT('Ctrl Pts',(0.878232759112823,6.71216131634816,33.155841689391));
#56320=CARTESIAN_POINT('Ctrl Pts',(0.700082505122222,6.73307510953281,33.1642647323764));
#56321=CARTESIAN_POINT('Ctrl Pts',(0.52137539127125,6.74688496280889,33.1726877753619));
#56322=CARTESIAN_POINT('Ctrl Pts',(0.342677693318895,6.76069408845766,33.1811103745457));
#56323=CARTESIAN_POINT('Ctrl Pts',(0.163423526398336,6.767399994887,33.1895329737295));
#56324=CARTESIAN_POINT('Ctrl Pts',(-0.0157991414938836,6.76698155658253,
33.1979555729133));
#56325=CARTESIAN_POINT('Ctrl Pts',(-0.195037358157048,6.76656308197572,
33.2063789028141));
#56326=CARTESIAN_POINT('Ctrl Pts',(-0.374243736950611,6.75901903164635,
33.214802232715));
#56327=CARTESIAN_POINT('Ctrl Pts',(-0.55283084576014,6.74438040563966,33.2232255626159));
#56328=CARTESIAN_POINT('Ctrl Pts',(-0.737382501555146,6.72925287103703,
33.2319302193566));
#56329=CARTESIAN_POINT('Ctrl Pts',(-0.921272425447512,6.70654868286527,
33.2406348760974));
#56330=CARTESIAN_POINT('Ctrl Pts',(-1.10385876102418,6.67636014874199,33.2493395328382));
#56331=CARTESIAN_POINT('Ctrl Pts',(-1.28070950995677,6.64711992738579,33.2577707500974));
#56332=CARTESIAN_POINT('Ctrl Pts',(-1.45633700072461,6.61085854578323,33.2662019673566));
#56333=CARTESIAN_POINT('Ctrl Pts',(-1.63016890437465,6.56771180421385,33.2746331846158));
#56334=CARTESIAN_POINT('Ctrl Pts',(-1.81245732814894,6.52246607344448,33.2834745610973));
#56335=CARTESIAN_POINT('Ctrl Pts',(-1.99277069739514,6.46964844903224,33.2923159375789));
#56336=CARTESIAN_POINT('Ctrl Pts',(-2.17046753907376,6.40947421102754,33.3011573140604));
#56337=CARTESIAN_POINT('Ctrl Pts',(-2.34816438075237,6.34929997302284,33.309998690542));
#56338=CARTESIAN_POINT('Ctrl Pts',(-2.52324431328163,6.28176930052493,33.3188400670235));
#56339=CARTESIAN_POINT('Ctrl Pts',(-2.69509059764972,6.20715519948229,33.3276814435051));
#56340=CARTESIAN_POINT('Ctrl Pts',(-2.85333108305194,6.13844861318482,33.335822810723));
#56341=CARTESIAN_POINT('Ctrl Pts',(-3.00914418974486,6.0635994130988,33.3439641779408));
#56342=CARTESIAN_POINT('Ctrl Pts',(-3.16201576885751,5.98280413163397,33.3521055451587));
#56343=CARTESIAN_POINT('Ctrl Pts',(-3.31475390270805,5.90207937830507,33.3602398055821));
#56344=CARTESIAN_POINT('Ctrl Pts',(-3.4645552986537,5.81541904518829,33.3683740660056));
#56345=CARTESIAN_POINT('Ctrl Pts',(-3.61092578394971,5.72306770734081,33.3765083264291));
#56346=CARTESIAN_POINT('Ctrl Pts',(-3.75719642058769,5.6307793682402,33.3846370379539));
#56347=CARTESIAN_POINT('Ctrl Pts',(-3.90004049800891,5.53280794827193,33.3927657494787));
#56348=CARTESIAN_POINT('Ctrl Pts',(-4.03898850387016,5.42944388179901,33.4008944610035));
#56349=CARTESIAN_POINT('Ctrl Pts',(-4.17787024799543,5.32612910773903,33.4090192960961));
#56350=CARTESIAN_POINT('Ctrl Pts',(-4.31285932734706,5.2174270262601,33.4171441311886));
#56351=CARTESIAN_POINT('Ctrl Pts',(-4.44351530932409,5.1036712958225,33.4252689662811));
#56352=CARTESIAN_POINT('Ctrl Pts',(-4.57413471379273,4.98994741162049,33.4333915268032));
#56353=CARTESIAN_POINT('Ctrl Pts',(-4.70042316178427,4.87117293721467,33.4415140873254));
#56354=CARTESIAN_POINT('Ctrl Pts',(-4.82197344176443,4.74772167749106,33.4496366478476));
#56355=CARTESIAN_POINT('Ctrl Pts',(-4.94353018182662,4.62426385665328,33.4577596400628));
#56356=CARTESIAN_POINT('Ctrl Pts',(-5.06034799119233,4.49612901204469,33.465882632278));
#56357=CARTESIAN_POINT('Ctrl Pts',(-5.17205653826282,4.3637277831016,33.4740056244932));
#56358=CARTESIAN_POINT('Ctrl Pts',(-5.22908034727287,4.29614099059608,33.4781521644744));
#56359=CARTESIAN_POINT('Ctrl Pts',(-5.28477340689579,4.22744303401794,33.4822987044556));
#56360=CARTESIAN_POINT('Ctrl Pts',(-5.33909048514278,4.1576918826986,33.4864452444368));
#56361=CARTESIAN_POINT('Ctrl Pts',(-5.45677079513745,4.00657298281193,33.4954289034652));
#56362=CARTESIAN_POINT('Ctrl Pts',(-5.56793181226996,3.85058350284633,33.5044125624936));
#56363=CARTESIAN_POINT('Ctrl Pts',(-5.67221657546274,3.69029106183317,33.5133962215221));
#56364=CARTESIAN_POINT('Ctrl Pts',(-5.77668049877385,3.52972324010454,33.5223953143816));
#56365=CARTESIAN_POINT('Ctrl Pts',(-5.87424442618288,3.36483788239926,33.531394407241));
#56366=CARTESIAN_POINT('Ctrl Pts',(-5.96459647945295,3.19622868976822,33.5403935001005));
#56367=CARTESIAN_POINT('Ctrl Pts',(-6.05516038303925,3.02722415569794,33.549413693318));
#56368=CARTESIAN_POINT('Ctrl Pts',(-6.13847846550649,2.85447852845012,33.5584338865355));
#56369=CARTESIAN_POINT('Ctrl Pts',(-6.21428513635634,2.67860957290544,33.5674540797529));
#56370=CARTESIAN_POINT('Ctrl Pts',(-6.29016858044267,2.50256250600508,33.5764834081747));
#56371=CARTESIAN_POINT('Ctrl Pts',(-6.35852532659879,2.3233860134179,33.5855127365965));
#56372=CARTESIAN_POINT('Ctrl Pts',(-6.41913862994282,2.14171619258383,33.5945420650183));
#56373=CARTESIAN_POINT('Ctrl Pts',(-6.47983738582691,1.95979025392109,33.6035841229731));
#56374=CARTESIAN_POINT('Ctrl Pts',(-6.53277079511993,1.77536418551779,33.6126261809279));
#56375=CARTESIAN_POINT('Ctrl Pts',(-6.57777186379046,1.58908977340066,33.6216682388828));
#56376=CARTESIAN_POINT('Ctrl Pts',(-6.61682497369461,1.42743594375495,33.6295151743779));
#56377=CARTESIAN_POINT('Ctrl Pts',(-6.64990483474276,1.26439037905654,33.6373621098731));
#56378=CARTESIAN_POINT('Ctrl Pts',(-6.67693357879417,1.10038492554693,33.6452090453682));
#56379=CARTESIAN_POINT('Ctrl Pts',(-6.70999996181544,0.899744187930262,
33.6548088171568));
#56380=CARTESIAN_POINT('Ctrl Pts',(-6.73402868125974,0.697549037419545,
33.6644085889453));
#56381=CARTESIAN_POINT('Ctrl Pts',(-6.74890395273286,0.494554786436053,
33.6740083607339));
#56382=CARTESIAN_POINT('Ctrl Pts',(-6.7608723347487,0.33122917942572,33.6817321684129));
#56383=CARTESIAN_POINT('Ctrl Pts',(-6.76691614885309,0.167386511247601,
33.6894559760919));
#56384=CARTESIAN_POINT('Ctrl Pts',(-6.76699913328736,0.003424921630116,
33.6971797837708));
#56385=CARTESIAN_POINT('',(-6.76699785065912,-0.00539343812502433,33.3028202162135));
#56386=CARTESIAN_POINT('Ctrl Pts',(3.09908550384733,6.01564277861006,32.651275857025));
#56387=CARTESIAN_POINT('Ctrl Pts',(2.94207978962374,6.09652759023844,32.6595971707146));
#56388=CARTESIAN_POINT('Ctrl Pts',(2.78203138935587,6.1711970514421,32.6679184844042));
#56389=CARTESIAN_POINT('Ctrl Pts',(2.61947314133681,6.23944304099453,32.6762397980938));
#56390=CARTESIAN_POINT('Ctrl Pts',(2.45667623468372,6.30778922536847,32.6845733286557));
#56391=CARTESIAN_POINT('Ctrl Pts',(2.2913624423339,6.36969297089404,32.6929068592175));
#56392=CARTESIAN_POINT('Ctrl Pts',(2.12408121548847,6.4249955634233,32.7012403897794));
#56393=CARTESIAN_POINT('Ctrl Pts',(2.0115413906263,6.46220083860589,32.7068468411883));
#56394=CARTESIAN_POINT('Ctrl Pts',(1.89811138804103,6.49641945309301,32.7124532925971));
#56395=CARTESIAN_POINT('Ctrl Pts',(1.78396096288937,6.52761612557654,32.7180597440059));
#56396=CARTESIAN_POINT('Ctrl Pts',(1.61962256307724,6.57252889071599,32.7261311572479));
#56397=CARTESIAN_POINT('Ctrl Pts',(1.45328462129516,6.61131411443873,32.73420257049));
#56398=CARTESIAN_POINT('Ctrl Pts',(1.28545415222779,6.64378631674141,32.742273983732));
#56399=CARTESIAN_POINT('Ctrl Pts',(1.11783438041326,6.6762177528837,32.7503352639832));
#56400=CARTESIAN_POINT('Ctrl Pts',(0.9487261711101,6.70235186732054,32.7583965442345));
#56401=CARTESIAN_POINT('Ctrl Pts',(0.778653271254402,6.72205237134945,32.7664578244857));
#56402=CARTESIAN_POINT('Ctrl Pts',(0.608756586064406,6.74173246343894,32.7745107523433));
#56403=CARTESIAN_POINT('Ctrl Pts',(0.437897566757396,6.75499216799324,32.7825636802009));
#56404=CARTESIAN_POINT('Ctrl Pts',(0.266611676714297,6.76174587024975,32.7906166080585));
#56405=CARTESIAN_POINT('Ctrl Pts',(0.0954657504538968,6.76849405381635,
32.7986629555829));
#56406=CARTESIAN_POINT('Ctrl Pts',(-0.0761059815110598,6.7687468016881,
32.8067093031072));
#56407=CARTESIAN_POINT('Ctrl Pts',(-0.247561483685967,6.76247013389303,
32.8147556506315));
#56408=CARTESIAN_POINT('Ctrl Pts',(-0.418914389086828,6.75619722197549,
32.8227971833247));
#56409=CARTESIAN_POINT('Ctrl Pts',(-0.590150831376489,6.74340268594741,
32.8308387160178));
#56410=CARTESIAN_POINT('Ctrl Pts',(-0.760727420740435,6.72410460889282,
32.8388802487109));
#56411=CARTESIAN_POINT('Ctrl Pts',(-0.934583300258403,6.70443553137261,
32.8470763777592));
#56412=CARTESIAN_POINT('Ctrl Pts',(-1.1077533020177,6.67801029604354,32.8552725068074));
#56413=CARTESIAN_POINT('Ctrl Pts',(-1.27966561724474,6.64490367936524,32.8634686358557));
#56414=CARTESIAN_POINT('Ctrl Pts',(-1.44827707896115,6.61243273612164,32.8715073926918));
#56415=CARTESIAN_POINT('Ctrl Pts',(-1.61567833783162,6.57353475680192,32.8795461495279));
#56416=CARTESIAN_POINT('Ctrl Pts',(-1.78133888071629,6.52833216005807,32.887584906364));
#56417=CARTESIAN_POINT('Ctrl Pts',(-1.9470154577899,6.4831251881808,32.8956244412668));
#56418=CARTESIAN_POINT('Ctrl Pts',(-2.11095062305154,6.4316124820358,32.9036639761696));
#56419=CARTESIAN_POINT('Ctrl Pts',(-2.27262810136108,6.37396662314009,32.9117035110723));
#56420=CARTESIAN_POINT('Ctrl Pts',(-2.43435324053951,6.31630377083411,32.9197454159479));
#56421=CARTESIAN_POINT('Ctrl Pts',(-2.59381901643189,6.25250429237782,32.9277873208234));
#56422=CARTESIAN_POINT('Ctrl Pts',(-2.75052838345207,6.18278922589348,32.9358292256989));
#56423=CARTESIAN_POINT('Ctrl Pts',(-2.91252391507618,6.11072251110747,32.9441424023798));
#56424=CARTESIAN_POINT('Ctrl Pts',(-3.07157342616548,6.03233431217328,32.9524555790606));
#56425=CARTESIAN_POINT('Ctrl Pts',(-3.22715566352832,5.9479202519332,32.9607687557414));
#56426=CARTESIAN_POINT('Ctrl Pts',(-3.3779223264858,5.86611897188471,32.968824623352));
#56427=CARTESIAN_POINT('Ctrl Pts',(-3.5254328760615,5.7786595481313,32.9768804909625));
#56428=CARTESIAN_POINT('Ctrl Pts',(-3.66924315661712,5.6858546989541,32.9849363585731));
#56429=CARTESIAN_POINT('Ctrl Pts',(-3.81994351246532,5.58860348894737,32.9933781897891));
#56430=CARTESIAN_POINT('Ctrl Pts',(-3.96657991269236,5.4854823239354,33.001820021005));
#56431=CARTESIAN_POINT('Ctrl Pts',(-4.10868144830041,5.37689740988165,33.010261852221));
#56432=CARTESIAN_POINT('Ctrl Pts',(-4.25078298390857,5.26831249582783,33.018703683437));
#56433=CARTESIAN_POINT('Ctrl Pts',(-4.38834935454169,5.15426419290825,33.027145514653));
#56434=CARTESIAN_POINT('Ctrl Pts',(-4.52095554968078,5.0352010801765,33.035587345869));
#56435=CARTESIAN_POINT('Ctrl Pts',(-4.64913029779636,4.92011683039282,33.0437470671294));
#56436=CARTESIAN_POINT('Ctrl Pts',(-4.77311108384849,4.79995272957011,33.0519067883899));
#56437=CARTESIAN_POINT('Ctrl Pts',(-4.89246522808437,4.67504791333579,33.0600665096504));
#56438=CARTESIAN_POINT('Ctrl Pts',(-5.01167597079469,4.55029316764418,33.0682164271752));
#56439=CARTESIAN_POINT('Ctrl Pts',(-5.1262708878455,4.42080930722444,33.0763663447));
#56440=CARTESIAN_POINT('Ctrl Pts',(-5.23585041703899,4.28697555514289,33.0845162622248));
#56441=CARTESIAN_POINT('Ctrl Pts',(-5.34532132898999,4.15327446153514,33.0926581014017));
#56442=CARTESIAN_POINT('Ctrl Pts',(-5.44978652130772,4.015232342053,33.1007999405785));
#56443=CARTESIAN_POINT('Ctrl Pts',(-5.54888336725751,3.8732650795644,33.1089417797553));
#56444=CARTESIAN_POINT('Ctrl Pts',(-5.64789321709116,3.73142244869587,33.1170764712941));
#56445=CARTESIAN_POINT('Ctrl Pts',(-5.74154390171591,3.585661838549,33.1252111628329));
#56446=CARTESIAN_POINT('Ctrl Pts',(-5.82951327604952,3.43643186522917,33.1333458543717));
#56447=CARTESIAN_POINT('Ctrl Pts',(-5.9174395202893,3.28727505717624,33.1414765575906));
#56448=CARTESIAN_POINT('Ctrl Pts',(-5.99968981356505,3.13465258587875,33.1496072608095));
#56449=CARTESIAN_POINT('Ctrl Pts',(-6.07598537388288,2.97904191584499,33.1577379640283));
#56450=CARTESIAN_POINT('Ctrl Pts',(-6.15225804036006,2.82347793956205,33.165866227485));
#56451=CARTESIAN_POINT('Ctrl Pts',(-6.22257937066534,2.66492787772565,33.1739944909416));
#56452=CARTESIAN_POINT('Ctrl Pts',(-6.28671661044567,2.50389361993405,33.1821227543983));
#56453=CARTESIAN_POINT('Ctrl Pts',(-6.35084680440882,2.34287705261287,33.1902501249219));
#56454=CARTESIAN_POINT('Ctrl Pts',(-6.40879412622396,2.17937717268235,33.1983774954456));
#56455=CARTESIAN_POINT('Ctrl Pts',(-6.46037404997259,2.013915622473,33.2065048659692));
#56456=CARTESIAN_POINT('Ctrl Pts',(-6.51197711765053,1.84837982960984,33.2146358832468));
#56457=CARTESIAN_POINT('Ctrl Pts',(-6.55720696619344,1.68088095613857,33.2227669005244));
#56458=CARTESIAN_POINT('Ctrl Pts',(-6.59592887245198,1.51195612024768,33.230897917802));
#56459=CARTESIAN_POINT('Ctrl Pts',(-6.63465877599399,1.34299639610026,33.2390306143886));
#56460=CARTESIAN_POINT('Ctrl Pts',(-6.66687798578942,1.17261048116098,33.2471633109753));
#56461=CARTESIAN_POINT('Ctrl Pts',(-6.69250301964037,1.00134526118841,33.255296007562));
#56462=CARTESIAN_POINT('Ctrl Pts',(-6.71815280979513,0.829914582163535,
33.2634365611337));
#56463=CARTESIAN_POINT('Ctrl Pts',(-6.7371956485091,0.657603263896057,33.2715771147054));
#56464=CARTESIAN_POINT('Ctrl Pts',(-6.74959992417062,0.484963775591544,
33.2797176682771));
#56465=CARTESIAN_POINT('Ctrl Pts',(-6.76133419466654,0.321649245237541,
33.2874185175813));
#56466=CARTESIAN_POINT('Ctrl Pts',(-6.76712811155804,0.158041329314807,
33.2951193668855));
#56467=CARTESIAN_POINT('Ctrl Pts',(-6.76699785065953,-0.00539343761909804,
33.3028202161897));
#56468=CARTESIAN_POINT('Ctrl Pts',(-6.76699785065912,-0.00539343812484117,
33.3028202162135));
#56469=CARTESIAN_POINT('Ctrl Pts',(-6.7668025852718,-0.250387526453958,
33.3143640424755));
#56470=CARTESIAN_POINT('Ctrl Pts',(-6.75329908010437,-0.494887213932031,
33.3259078687374));
#56471=CARTESIAN_POINT('Ctrl Pts',(-6.72666862041688,-0.737711509398421,
33.3374516949994));
#56472=CARTESIAN_POINT('Ctrl Pts',(-6.71462409806051,-0.847536975790543,
33.3426727792435));
#56473=CARTESIAN_POINT('Ctrl Pts',(-6.69989494559919,-0.95702010800004,
33.3478938634877));
#56474=CARTESIAN_POINT('Ctrl Pts',(-6.68250099372052,-1.06605322049339,
33.3531149477319));
#56475=CARTESIAN_POINT('Ctrl Pts',(-6.65273357345905,-1.25264879719985,
33.3620501345141));
#56476=CARTESIAN_POINT('Ctrl Pts',(-6.61512750839485,-1.4381154136122,33.3709853212964));
#56477=CARTESIAN_POINT('Ctrl Pts',(-6.5697816277517,-1.62180712899415,33.3799205080786));
#56478=CARTESIAN_POINT('Ctrl Pts',(-6.52450366120969,-1.80522373101277,
33.3888423127152));
#56479=CARTESIAN_POINT('Ctrl Pts',(-6.47150907061117,-1.98687048590991,
33.3977641173518));
#56480=CARTESIAN_POINT('Ctrl Pts',(-6.410947704516,-2.16611138447704,33.4066859219884));
#56481=CARTESIAN_POINT('Ctrl Pts',(-6.35053406195511,-2.34491507198488,
33.4155859642277));
#56482=CARTESIAN_POINT('Ctrl Pts',(-6.28259056378408,-2.52132437130597,
33.4244860064669));
#56483=CARTESIAN_POINT('Ctrl Pts',(-6.20731663576343,-2.6947187577509,33.4333860487062));
#56484=CARTESIAN_POINT('Ctrl Pts',(-6.13215859306182,-2.86784620098825,
33.4422723891995));
#56485=CARTESIAN_POINT('Ctrl Pts',(-6.04969273412608,-3.03796775415776,
33.4511587296929));
#56486=CARTESIAN_POINT('Ctrl Pts',(-5.9601673228959,-3.20448037645481,33.4600450701862));
#56487=CARTESIAN_POINT('Ctrl Pts',(-5.87087081251491,-3.37056725504265,
33.4689086898581));
#56488=CARTESIAN_POINT('Ctrl Pts',(-5.77455088954403,-3.53306338862778,
33.47777230953));
#56489=CARTESIAN_POINT('Ctrl Pts',(-5.67150235408961,-3.69138863404492,
33.4866359292019));
#56490=CARTESIAN_POINT('Ctrl Pts',(-5.5736779259755,-3.84168748614078,33.4950502023558));
#56491=CARTESIAN_POINT('Ctrl Pts',(-5.46979023457897,-3.98822757624349,
33.5034644755097));
#56492=CARTESIAN_POINT('Ctrl Pts',(-5.36013090501699,-4.13053092000069,
33.5118787486636));
#56493=CARTESIAN_POINT('Ctrl Pts',(-5.25313053823785,-4.26938376577987,
33.5200889968682));
#56494=CARTESIAN_POINT('Ctrl Pts',(-5.14073706316906,-4.40406876775802,
33.5282992450727));
#56495=CARTESIAN_POINT('Ctrl Pts',(-5.02331705709524,-4.53415645339859,
33.5365094932772));
#56496=CARTESIAN_POINT('Ctrl Pts',(-4.90586913794518,-4.66427506347535,
33.5447216932215));
#56497=CARTESIAN_POINT('Ctrl Pts',(-4.78339254569706,-4.78979391566198,
33.5529338931657));
#56498=CARTESIAN_POINT('Ctrl Pts',(-4.65629173412285,-4.91031936708187,
33.5611460931099));
#56499=CARTESIAN_POINT('Ctrl Pts',(-4.52913807505962,-5.03089493200921,
33.5693617076204));
#56500=CARTESIAN_POINT('Ctrl Pts',(-4.39735662427768,-5.14647271517083,
33.5775773221309));
#56501=CARTESIAN_POINT('Ctrl Pts',(-4.2613860649639,-5.25669837496232,33.5857929366414));
#56502=CARTESIAN_POINT('Ctrl Pts',(-4.12526281667301,-5.36704781333742,
33.5940177769268));
#56503=CARTESIAN_POINT('Ctrl Pts',(-3.98494134067954,-5.47203289979203,
33.6022426172123));
#56504=CARTESIAN_POINT('Ctrl Pts',(-3.84089132867578,-5.57134120309492,
33.6104674574977));
#56505=CARTESIAN_POINT('Ctrl Pts',(-3.69674904763208,-5.67071311681809,
33.6186975660792));
#56506=CARTESIAN_POINT('Ctrl Pts',(-3.54887376960743,-5.76440080884536,
33.6269276746607));
#56507=CARTESIAN_POINT('Ctrl Pts',(-3.39776104093056,-5.85213712319991,
33.6351577832422));
#56508=CARTESIAN_POINT('Ctrl Pts',(-3.24644113438345,-5.93999372538798,
33.6433991754289));
#56509=CARTESIAN_POINT('Ctrl Pts',(-3.09187522516354,-6.0218824861561,33.6516405676156));
#56510=CARTESIAN_POINT('Ctrl Pts',(-2.93458104387901,-6.09758338171,33.6598819598023));
#56511=CARTESIAN_POINT('Ctrl Pts',(-2.86612261989647,-6.13053033474645,
33.6634688230666));
#56512=CARTESIAN_POINT('Ctrl Pts',(-2.79714763125209,-6.16230580362811,
33.6670556863308));
#56513=CARTESIAN_POINT('Ctrl Pts',(-2.72769970169662,-6.19289458471272,
33.670642549595));
#56514=CARTESIAN_POINT('Ctrl Pts',(-2.56412210465004,-6.26494337491329,
33.6790910444234));
#56515=CARTESIAN_POINT('Ctrl Pts',(-2.39754655500624,-6.33056952167647,
33.6875395392518));
#56516=CARTESIAN_POINT('Ctrl Pts',(-2.228505189376,-6.38952686988045,33.6959880340803));
#56517=CARTESIAN_POINT('Ctrl Pts',(-2.05961823321371,-6.44843036397165,
33.7044288116994));
#56518=CARTESIAN_POINT('Ctrl Pts',(-1.88827026407826,-6.50067709254612,
33.7128695893186));
#56519=CARTESIAN_POINT('Ctrl Pts',(-1.71501368446944,-6.54606882503404,
33.7213103669378));
#56520=CARTESIAN_POINT('Ctrl Pts',(-1.54188872154352,-6.59142607508399,
33.7297447324071));
#56521=CARTESIAN_POINT('Ctrl Pts',(-1.36685835996665,-6.629938626022,33.7381790978764));
#56522=CARTESIAN_POINT('Ctrl Pts',(-1.19049084534923,-6.66145783947776,
33.7466134633457));
#56523=CARTESIAN_POINT('Ctrl Pts',(-1.0142302263253,-6.69295794927355,33.7550427167824));
#56524=CARTESIAN_POINT('Ctrl Pts',(-0.836634397506523,-6.71747311379963,
33.763471970219));
#56525=CARTESIAN_POINT('Ctrl Pts',(-0.658282890031881,-6.73490554029463,
33.7719012236556));
#56526=CARTESIAN_POINT('Ctrl Pts',(-0.480012122038219,-6.75233007515424,
33.7803266611808));
#56527=CARTESIAN_POINT('Ctrl Pts',(-0.30098668883616,-6.76267823310201,
33.7887520987061));
#56528=CARTESIAN_POINT('Ctrl Pts',(-0.121792753588958,-6.7659038956501,
33.7971775362313));
#56529=CARTESIAN_POINT('Ctrl Pts',(0.0573618175695597,-6.76912884960688,
33.8056011229145));
#56530=CARTESIAN_POINT('Ctrl Pts',(0.236684483945418,-6.76523441908685,
33.8140247095977));
#56531=CARTESIAN_POINT('Ctrl Pts',(0.415587019380714,-6.7542265604081,33.8224482962809));
#56532=CARTESIAN_POINT('Ctrl Pts',(0.594469536560332,-6.74321993345103,
33.8308709404089));
#56533=CARTESIAN_POINT('Ctrl Pts',(0.77293168381078,-6.7251014855954,33.8392935845369));
#56534=CARTESIAN_POINT('Ctrl Pts',(0.950387979692742,-6.69992923007815,
33.8477162286649));
#56535=CARTESIAN_POINT('Ctrl Pts',(1.12784916470806,-6.67475628103513,33.8561391048468));
#56536=CARTESIAN_POINT('Ctrl Pts',(1.30430411306229,-6.64252918407661,33.8645619810287));
#56537=CARTESIAN_POINT('Ctrl Pts',(1.47917481759715,-6.60335754438501,33.8729848572107));
#56538=CARTESIAN_POINT('Ctrl Pts',(1.65407472651038,-6.56417936281214,33.8814091400597));
#56539=CARTESIAN_POINT('Ctrl Pts',(1.82738953895219,-6.51805439971197,33.8898334229087));
#56540=CARTESIAN_POINT('Ctrl Pts',(1.99855338766498,-6.46514294943684,33.8982577057577));
#56541=CARTESIAN_POINT('Ctrl Pts',(2.16983283411233,-6.41219576472462,33.9066876780558));
#56542=CARTESIAN_POINT('Ctrl Pts',(2.33895809519942,-6.35245303285671,33.915117650354));
#56543=CARTESIAN_POINT('Ctrl Pts',(2.50537940031931,-6.28612464563468,33.9235476226521));
#56544=CARTESIAN_POINT('Ctrl Pts',(2.67186019836991,-6.21977254708468,33.9319806085293));
#56545=CARTESIAN_POINT('Ctrl Pts',(2.83563480565612,-6.14683022802284,33.9404135944065));
#56546=CARTESIAN_POINT('Ctrl Pts',(2.99617474068942,-6.06755518501931,33.9488465802837));
#56547=CARTESIAN_POINT('Ctrl Pts',(3.15686237148472,-5.98820720945927,33.9572873244566));
#56548=CARTESIAN_POINT('Ctrl Pts',(3.31430908801181,-5.90251502289283,33.9657280686294));
#56549=CARTESIAN_POINT('Ctrl Pts',(3.46801128996304,-5.81078193470456,33.9741688128022));
#56550=CARTESIAN_POINT('Ctrl Pts',(3.55299734244075,-5.76006026027348,33.9788359256875));
#56551=CARTESIAN_POINT('Ctrl Pts',(3.63683908351056,-5.70749249695703,33.9835030385727));
#56552=CARTESIAN_POINT('Ctrl Pts',(3.719455311038,-5.65313551838192,33.988170151458));
#56553=CARTESIAN_POINT('Ctrl Pts',(3.86357204079958,-5.55831455854855,33.9963115186759));
#56554=CARTESIAN_POINT('Ctrl Pts',(4.00424412887687,-5.4578581470722,34.0044528858937));
#56555=CARTESIAN_POINT('Ctrl Pts',(4.14099873769758,-5.3520480616664,34.0125942531116));
#56556=CARTESIAN_POINT('Ctrl Pts',(4.27763397014559,-5.24633034041782,34.020728513535));
#56557=CARTESIAN_POINT('Ctrl Pts',(4.41035824268065,-5.13526847007893,34.0288627739585));
#56558=CARTESIAN_POINT('Ctrl Pts',(4.53872663540292,-5.01918813445801,34.036997034382));
#56559=CARTESIAN_POINT('Ctrl Pts',(4.66700745984418,-4.90318698464938,34.0451257459068));
#56560=CARTESIAN_POINT('Ctrl Pts',(4.79093805008766,-4.78217442998399,34.0532544574315));
#56561=CARTESIAN_POINT('Ctrl Pts',(4.91010564445792,-4.65651710619241,34.0613831689563));
#56562=CARTESIAN_POINT('Ctrl Pts',(5.02921641000494,-4.53091970605607,34.0695080040488));
#56563=CARTESIAN_POINT('Ctrl Pts',(5.14356845145161,-4.40068221268763,34.0776328391413));
#56564=CARTESIAN_POINT('Ctrl Pts',(5.25278506741071,-4.2662088598177,34.0857576742338));
#56565=CARTESIAN_POINT('Ctrl Pts',(5.36197110787203,-4.13177315313985,34.093880234756));
#56566=CARTESIAN_POINT('Ctrl Pts',(5.46602435649172,-3.9931042333415,34.1020027952782));
#56567=CARTESIAN_POINT('Ctrl Pts',(5.56460772447092,-3.85064018998901,34.1101253558003));
#56568=CARTESIAN_POINT('Ctrl Pts',(5.66319633190043,-3.70816857504213,34.1182483480155));
#56569=CARTESIAN_POINT('Ctrl Pts',(5.75631426641379,-3.56190173238892,34.1263713402307));
#56570=CARTESIAN_POINT('Ctrl Pts',(5.8436670886332,-3.41230771725313,34.1344943324458));
#56571=CARTESIAN_POINT('Ctrl Pts',(5.88825804233793,-3.33594453133714,34.1386408724271));
#56572=CARTESIAN_POINT('Ctrl Pts',(5.9313474338422,-3.25871480604756,34.1427874124084));
#56573=CARTESIAN_POINT('Ctrl Pts',(5.9729006403841,-3.18068340771275,34.1469339523897));
#56574=CARTESIAN_POINT('Ctrl Pts',(6.06292746776206,-3.01162499290993,34.1559176114181));
#56575=CARTESIAN_POINT('Ctrl Pts',(6.14569643807502,-2.83888592048222,34.1649012704466));
#56576=CARTESIAN_POINT('Ctrl Pts',(6.22095320011086,-2.66308660806038,34.173884929475));
#56577=CARTESIAN_POINT('Ctrl Pts',(6.29633925246657,-2.48698527428227,34.1828840223345));
#56578=CARTESIAN_POINT('Ctrl Pts',(6.36418720716324,-2.30781341220419,34.1918831151939));
#56579=CARTESIAN_POINT('Ctrl Pts',(6.42429160021571,-2.12620940534979,34.2008822080534));
#56580=CARTESIAN_POINT('Ctrl Pts',(6.48453692127384,-1.94417958784817,34.2099024012709));
#56581=CARTESIAN_POINT('Ctrl Pts',(6.5370022773313,-1.75970644342602,34.2189225944883));
#56582=CARTESIAN_POINT('Ctrl Pts',(6.58153193264677,-1.57344412660599,34.2279427877058));
#56583=CARTESIAN_POINT('Ctrl Pts',(6.62610668538862,-1.38699317254946,34.2369721161276));
#56584=CARTESIAN_POINT('Ctrl Pts',(6.66272963199257,-1.19874965998421,34.2460014445494));
#56585=CARTESIAN_POINT('Ctrl Pts',(6.69129630227897,-1.00937742946224,34.2550307729711));
#56586=CARTESIAN_POINT('Ctrl Pts',(6.71990324581237,-0.819738222266482,
34.264072830926));
#56587=CARTESIAN_POINT('Ctrl Pts',(6.74043116743781,-0.628967351954016,
34.2731148888808));
#56588=CARTESIAN_POINT('Ctrl Pts',(6.75282730103158,-0.437735585076878,
34.2821569468356));
#56589=CARTESIAN_POINT('Ctrl Pts',(6.76358499150263,-0.271779632703956,
34.2900038823307));
#56590=CARTESIAN_POINT('Ctrl Pts',(6.76821926374527,-0.105476725647189,
34.2978508178259));
#56591=CARTESIAN_POINT('Ctrl Pts',(6.76672744690542,0.0607343337573115,
34.305697753321));
#56592=CARTESIAN_POINT('Ctrl Pts',(6.76508229718105,0.244029005904913,34.3143512176217));
#56593=CARTESIAN_POINT('Ctrl Pts',(6.75598423759691,0.427373527978166,34.3230046819225));
#56594=CARTESIAN_POINT('Ctrl Pts',(6.73943635421743,0.610152954145541,34.3316581462232));
#56595=CARTESIAN_POINT('Ctrl Pts',(6.72290371482327,0.792764003075407,34.3403036389133));
#56596=CARTESIAN_POINT('Ctrl Pts',(6.69893496700205,0.974810692669004,34.3489491316035));
#56597=CARTESIAN_POINT('Ctrl Pts',(6.66758519465642,1.15568017721104,34.3575946242936));
#56598=CARTESIAN_POINT('Ctrl Pts',(6.63529231822572,1.34199080970958,34.3665002017902));
#56599=CARTESIAN_POINT('Ctrl Pts',(6.59516738389635,1.52705197798527,34.3754057792868));
#56600=CARTESIAN_POINT('Ctrl Pts',(6.54732823285542,1.71019940686877,34.3843113567834));
#56601=CARTESIAN_POINT('Ctrl Pts',(6.50097433243883,1.88766070154679,34.3929404449559));
#56602=CARTESIAN_POINT('Ctrl Pts',(6.44737810572147,2.0633249796476,34.4015695331283));
#56603=CARTESIAN_POINT('Ctrl Pts',(6.38669867572393,2.23659764497467,34.4101986213008));
#56604=CARTESIAN_POINT('Ctrl Pts',(6.32310285162108,2.41819819637104,34.4192424434595));
#56605=CARTESIAN_POINT('Ctrl Pts',(6.25172622432653,2.59717124063413,34.4282862656181));
#56606=CARTESIAN_POINT('Ctrl Pts',(6.17281117396229,2.7728489339678,34.4373300877768));
#56607=CARTESIAN_POINT('Ctrl Pts',(6.09389612359799,2.94852662730158,34.4463739099354));
#56608=CARTESIAN_POINT('Ctrl Pts',(6.00744277645742,3.12090860402851,34.4554177320941));
#56609=CARTESIAN_POINT('Ctrl Pts',(5.91375248523791,3.28934956235157,34.4644615542527));
#56610=CARTESIAN_POINT('Ctrl Pts',(5.8264647554555,3.44627968459813,34.4728873441025));
#56611=CARTESIAN_POINT('Ctrl Pts',(5.73293380946965,3.59972040454659,34.4813131339524));
#56612=CARTESIAN_POINT('Ctrl Pts',(5.63347206019072,3.74917078125957,34.4897389238022));
#56613=CARTESIAN_POINT('Ctrl Pts',(5.5339872324399,3.89865583548771,34.4981666687187));
#56614=CARTESIAN_POINT('Ctrl Pts',(5.42856904122757,4.04414842440703,34.5065944136352));
#56615=CARTESIAN_POINT('Ctrl Pts',(5.31757276197332,4.18517728670118,34.5150221585518));
#56616=CARTESIAN_POINT('Ctrl Pts',(5.20653569715525,4.32625797002665,34.5234530002417));
#56617=CARTESIAN_POINT('Ctrl Pts',(5.08991666237077,4.46287139595117,34.5318838419316));
#56618=CARTESIAN_POINT('Ctrl Pts',(4.96811091470667,4.59457973477144,34.5403146836216));
#56619=CARTESIAN_POINT('Ctrl Pts',(4.84619324310758,4.72640909674403,34.548753272179));
#56620=CARTESIAN_POINT('Ctrl Pts',(4.71907956199458,4.85332412320422,34.5571918607363));
#56621=CARTESIAN_POINT('Ctrl Pts',(4.58720244125173,4.97492339267392,34.5656304492937));
#56622=CARTESIAN_POINT('Ctrl Pts',(4.4552561699748,5.0965864234267,34.574073462674));
#56623=CARTESIAN_POINT('Ctrl Pts',(4.31854172632411,5.21292791942066,34.5825164760543));
#56624=CARTESIAN_POINT('Ctrl Pts',(4.17752481791164,5.32358670406825,34.5909594894345));
#56625=CARTESIAN_POINT('Ctrl Pts',(4.03635976140795,5.43436174348208,34.5994113727888));
#56626=CARTESIAN_POINT('Ctrl Pts',(3.89088347633704,5.53944194759298,34.6078632561432));
#56627=CARTESIAN_POINT('Ctrl Pts',(3.74159156531282,5.63850880626961,34.6163151394975));
#56628=CARTESIAN_POINT('Ctrl Pts',(3.70090480307715,5.66550765501338,34.6186185447264));
#56629=CARTESIAN_POINT('Ctrl Pts',(3.65993479012726,5.69206013077368,34.6209219499552));
#56630=CARTESIAN_POINT('Ctrl Pts',(3.61869188063002,5.71816037489877,34.6232253551841));
#56631=CARTESIAN_POINT('Ctrl Pts',(3.46974835597489,5.81241808856974,34.6315438103483));
#56632=CARTESIAN_POINT('Ctrl Pts',(3.31697584700636,5.90094381771582,34.6398622655126));
#56633=CARTESIAN_POINT('Ctrl Pts',(3.16084977546522,5.98342023402514,34.6481807206768));
#56634=CARTESIAN_POINT('Ctrl Pts',(3.14031925885143,5.99426585012609,34.6492745942385));
#56635=CARTESIAN_POINT('Ctrl Pts',(3.11973079513912,6.00500692051147,34.6503684678002));
#56636=CARTESIAN_POINT('Ctrl Pts',(3.09908550384707,6.01564277861019,34.6514623413619));
#56637=CARTESIAN_POINT('Origin',(0.,0.,-63.6971797838103));
#56638=CARTESIAN_POINT('',(3.09908550384717,6.01564277861014,37.0457563580462));
#56639=CARTESIAN_POINT('',(3.09908550384717,6.01564277861014,36.651532120892));
#56640=CARTESIAN_POINT('',(3.09908550384721,6.01564277861012,-63.6971797838103));
#56641=CARTESIAN_POINT('',(-6.767,4.50145461541613E-12,35.6971797838099));
#56642=CARTESIAN_POINT('Ctrl Pts',(-6.767,4.88611405695858E-12,35.6971797838098));
#56643=CARTESIAN_POINT('Ctrl Pts',(-6.76700000000014,-0.186007249555188,
35.7059292956226));
#56644=CARTESIAN_POINT('Ctrl Pts',(-6.75932637294273,-0.372014355811442,
35.7146788074353));
#56645=CARTESIAN_POINT('Ctrl Pts',(-6.744005182634,-0.557389537581891,35.7234283192481));
#56646=CARTESIAN_POINT('Ctrl Pts',(-6.72868405703777,-0.742763936378502,
35.7321777941053));
#56647=CARTESIAN_POINT('Ctrl Pts',(-6.7057154564362,-0.927506130400955,
35.7409272689625));
#56648=CARTESIAN_POINT('Ctrl Pts',(-6.67517739401639,-1.11098864009162,
35.7496767438197));
#56649=CARTESIAN_POINT('Ctrl Pts',(-6.64463945804465,-1.29447039004152,
35.7584261824482));
#56650=CARTESIAN_POINT('Ctrl Pts',(-6.60653217002812,-1.47669218338883,
35.7671756210767));
#56651=CARTESIAN_POINT('Ctrl Pts',(-6.56098496085581,-1.65703510627383,
35.7759250597052));
#56652=CARTESIAN_POINT('Ctrl Pts',(-6.51543793649669,-1.83737729739609,
35.7846744628318));
#56653=CARTESIAN_POINT('Ctrl Pts',(-6.46245112157021,-2.01584035544553,
35.7934238659585));
#56654=CARTESIAN_POINT('Ctrl Pts',(-6.40220448361854,-2.1918181379701,35.8021732690851));
#56655=CARTESIAN_POINT('Ctrl Pts',(-6.34195808512117,-2.36779522105917,
35.8109226374366));
#56656=CARTESIAN_POINT('Ctrl Pts',(-6.27445201416505,-2.54128677725371,
35.8196720057882));
#56657=CARTESIAN_POINT('Ctrl Pts',(-6.19991555052882,-2.71170355428299,
35.8284213741397));
#56658=CARTESIAN_POINT('Ctrl Pts',(-6.1253793769528,-2.88211966813178,35.8371707084429));
#56659=CARTESIAN_POINT('Ctrl Pts',(-6.04381298028511,-3.04946076419551,
35.8459200427461));
#56660=CARTESIAN_POINT('Ctrl Pts',(-5.9554933930904,-3.21315848424205,35.8546693770492));
#56661=CARTESIAN_POINT('Ctrl Pts',(-5.86717414225866,-3.37685558084983,
35.8634186780308));
#56662=CARTESIAN_POINT('Ctrl Pts',(-5.77210188844123,-3.53690907699909,
35.8721679790124));
#56663=CARTESIAN_POINT('Ctrl Pts',(-5.67059953311426,-3.69277537023907,
35.8809172799939));
#56664=CARTESIAN_POINT('Ctrl Pts',(-5.56909755592753,-3.84864108280962,
35.8896665483805));
#56665=CARTESIAN_POINT('Ctrl Pts',(-5.46116568155,-4.00031938354783,35.8984158167672));
#56666=CARTESIAN_POINT('Ctrl Pts',(-5.34717048488399,-4.14729511918136,
35.9071650851538));
#56667=CARTESIAN_POINT('Ctrl Pts',(-5.23317570343298,-4.29427031947189,
35.9159143216722));
#56668=CARTESIAN_POINT('Ctrl Pts',(-5.11311781951509,-4.43654276249602,
35.9246635581906));
#56669=CARTESIAN_POINT('Ctrl Pts',(-4.98740458929172,-4.57362924412462,
35.9334127947089));
#56670=CARTESIAN_POINT('Ctrl Pts',(-4.86169180652671,-4.71071523781338,
35.9421620000856));
#56671=CARTESIAN_POINT('Ctrl Pts',(-4.73032391141508,-4.84261509584552,
35.9509112054623));
#56672=CARTESIAN_POINT('Ctrl Pts',(-4.59374706947268,-4.96888084599653,
35.959660410839));
#56673=CARTESIAN_POINT('Ctrl Pts',(-4.45717070231474,-5.09514615720771,
35.9684095858007));
#56674=CARTESIAN_POINT('Ctrl Pts',(-4.31538563497356,-5.21577720520587,
35.9771587607625));
#56675=CARTESIAN_POINT('Ctrl Pts',(-4.16887340952063,-5.33036429293457,
35.9859079357242));
#56676=CARTESIAN_POINT('Ctrl Pts',(-4.02236168122556,-5.44495099183652,
35.9946570809974));
#56677=CARTESIAN_POINT('Ctrl Pts',(-3.87112305263268,-5.55349359497867,
36.0034062262706));
#56678=CARTESIAN_POINT('Ctrl Pts',(-3.71567116929099,-5.65562346357143,
36.0121553715439));
#56679=CARTESIAN_POINT('Ctrl Pts',(-3.56021980053412,-5.75775299408865,
36.0209044878552));
#56680=CARTESIAN_POINT('Ctrl Pts',(-3.40055544442181,-5.85346967519823,
36.0296536041666));
#56681=CARTESIAN_POINT('Ctrl Pts',(-3.23722035886936,-5.94244843041332,
36.038402720478));
#56682=CARTESIAN_POINT('Ctrl Pts',(-3.07388580043576,-6.03142689847407,
36.047151808554));
#56683=CARTESIAN_POINT('Ctrl Pts',(-2.90688078789303,-6.11366734707864,
36.05590089663));
#56684=CARTESIAN_POINT('Ctrl Pts',(-2.73677250610466,-6.18889047001396,
36.064649984706));
#56685=CARTESIAN_POINT('Ctrl Pts',(-2.56666475917026,-6.26411335643296,
36.0733990452732));
#56686=CARTESIAN_POINT('Ctrl Pts',(-2.39345402457205,-6.33231884545213,
36.0821481058404));
#56687=CARTESIAN_POINT('Ctrl Pts',(-2.21772855944197,-6.39327529804837,
36.0908971664075));
#56688=CARTESIAN_POINT('Ctrl Pts',(-2.04200363223764,-6.45423156404647,
36.0996462001923));
#56689=CARTESIAN_POINT('Ctrl Pts',(-1.86376426061249,-6.5079387441239,36.1083952339771));
#56690=CARTESIAN_POINT('Ctrl Pts',(-1.68361577621946,-6.55421443943246,
36.1171442677619));
#56691=CARTESIAN_POINT('Ctrl Pts',(-1.50346782833442,-6.60048999692537,
36.1258932754908));
#56692=CARTESIAN_POINT('Ctrl Pts',(-1.32141105657582,-6.63933404265124,
36.1346422832197));
#56693=CARTESIAN_POINT('Ctrl Pts',(-1.13806375346697,-6.67061465631501,
36.1433912909486));
#56694=CARTESIAN_POINT('Ctrl Pts',(-0.954716981171831,-6.70189517941744,
36.152140273348));
#56695=CARTESIAN_POINT('Ctrl Pts',(-0.770079967444305,-6.7256122660898,
36.1608892557474));
#56696=CARTESIAN_POINT('Ctrl Pts',(-0.584779764075293,-6.74168536995966,
36.1696382381469));
#56697=CARTESIAN_POINT('Ctrl Pts',(-0.391489587595131,-6.7584515311786,
36.1787644685625));
#56698=CARTESIAN_POINT('Ctrl Pts',(-0.197478091807359,-6.76689985146388,
36.1878906989781));
#56699=CARTESIAN_POINT('Ctrl Pts',(-0.00346214753309966,-6.76699911434415,
36.1970169293937));
#56700=CARTESIAN_POINT('Ctrl Pts',(0.184490798482673,-6.7670952752594,36.2058579651089));
#56701=CARTESIAN_POINT('Ctrl Pts',(0.372447602152916,-6.75935633790774,
36.214699000824));
#56702=CARTESIAN_POINT('Ctrl Pts',(0.559756448192457,-6.74380914014528,
36.2235400365391));
#56703=CARTESIAN_POINT('Ctrl Pts',(0.745136131041587,-6.72842206873174,
36.2322900151524));
#56704=CARTESIAN_POINT('Ctrl Pts',(0.929880851943267,-6.70538686355748,
36.2410399937657));
#56705=CARTESIAN_POINT('Ctrl Pts',(1.11336305057284,-6.67478177303342,36.249789972379));
#56706=CARTESIAN_POINT('Ctrl Pts',(1.29684337089954,-6.64417699581294,36.258539861419));
#56707=CARTESIAN_POINT('Ctrl Pts',(1.47906091205029,-6.60600253548096,36.267289750459));
#56708=CARTESIAN_POINT('Ctrl Pts',(1.6593967109507,-6.5603880644125,36.276039639499));
#56709=CARTESIAN_POINT('Ctrl Pts',(1.8397307236901,-6.51477404513892,36.2847894418745));
#56710=CARTESIAN_POINT('Ctrl Pts',(2.01818275356888,-6.46172023288707,36.29353924425));
#56711=CARTESIAN_POINT('Ctrl Pts',(2.19414664033179,-6.40140683918158,36.3022890466255));
#56712=CARTESIAN_POINT('Ctrl Pts',(2.37010884271118,-6.3410940228155,36.311038765245));
#56713=CARTESIAN_POINT('Ctrl Pts',(2.54358267847669,-6.27352185699847,36.3197884838646));
#56714=CARTESIAN_POINT('Ctrl Pts',(2.7139789084161,-6.19891986435319,36.3285382024841));
#56715=CARTESIAN_POINT('Ctrl Pts',(2.8843735638881,-6.12431856103305,36.3372878402559));
#56716=CARTESIAN_POINT('Ctrl Pts',(3.0516904078704,-6.04268767582624,36.3460374780277));
#56717=CARTESIAN_POINT('Ctrl Pts',(3.21536112511921,-5.95430447954017,36.3547871157996));
#56718=CARTESIAN_POINT('Ctrl Pts',(3.37903038442716,-5.86592207055116,36.3635366756316));
#56719=CARTESIAN_POINT('Ctrl Pts',(3.53905332979852,-5.77078760703452,36.3722862354637));
#56720=CARTESIAN_POINT('Ctrl Pts',(3.69488643041776,-5.66922422085374,36.3810357952958));
#56721=CARTESIAN_POINT('Ctrl Pts',(3.85071819468642,-5.56766170563228,36.3897852800958));
#56722=CARTESIAN_POINT('Ctrl Pts',(4.0023599459914,-5.45967053456314,36.3985347648958));
#56723=CARTESIAN_POINT('Ctrl Pts',(4.14929662974232,-5.34561750206738,36.4072842496958));
#56724=CARTESIAN_POINT('Ctrl Pts',(4.29623210224975,-5.23156540974523,36.4160336623711));
#56725=CARTESIAN_POINT('Ctrl Pts',(4.43846235842047,-5.11145173172247,36.4247830750465));
#56726=CARTESIAN_POINT('Ctrl Pts',(4.57550431797358,-4.98568443006626,36.4335324877218));
#56727=CARTESIAN_POINT('Ctrl Pts',(4.71254519337427,-4.85991812336754,36.4422818311797));
#56728=CARTESIAN_POINT('Ctrl Pts',(4.8443976431492,-4.72849847631166,36.4510311746376));
#56729=CARTESIAN_POINT('Ctrl Pts',(4.97061384196626,-4.59187184425409,36.4597805180955));
#56730=CARTESIAN_POINT('Ctrl Pts',(5.0968290842015,-4.45524624767812,36.4685297952429));
#56731=CARTESIAN_POINT('Ctrl Pts',(5.21740796650117,-4.31341395556957,36.4772790723902));
#56732=CARTESIAN_POINT('Ctrl Pts',(5.33194095942201,-4.1668566816292,36.4860283495376));
#56733=CARTESIAN_POINT('Ctrl Pts',(5.44647312235089,-4.02030046975274,36.4947775632811));
#56734=CARTESIAN_POINT('Ctrl Pts',(5.55495930712251,-3.86901957035601,36.5035267770247));
#56735=CARTESIAN_POINT('Ctrl Pts',(5.65703106079764,-3.71352778058422,36.5122759907682));
#56736=CARTESIAN_POINT('Ctrl Pts',(5.75910210868711,-3.55803706597644,36.5210251440144));
#56737=CARTESIAN_POINT('Ctrl Pts',(5.8547586569853,-3.39833575880934,36.5297742972606));
#56738=CARTESIAN_POINT('Ctrl Pts',(5.94367583069048,-3.23496624706747,36.5385234505068));
#56739=CARTESIAN_POINT('Ctrl Pts',(6.03259241910056,-3.0715978107014,36.547272546162));
#56740=CARTESIAN_POINT('Ctrl Pts',(6.11476958470941,-2.90456146975888,36.5560216418171));
#56741=CARTESIAN_POINT('Ctrl Pts',(6.18992823574355,-2.73442451648326,36.5647707374722));
#56742=CARTESIAN_POINT('Ctrl Pts',(6.26508641700904,-2.56428862662491,36.5735197784423));
#56743=CARTESIAN_POINT('Ctrl Pts',(6.33322605570266,-2.39105242531359,36.5822688194124));
#56744=CARTESIAN_POINT('Ctrl Pts',(6.39411573747736,-2.21530425353817,36.5910178603825));
#56745=CARTESIAN_POINT('Ctrl Pts',(6.45500505889099,-2.03955712188645,36.5997668495735));
#56746=CARTESIAN_POINT('Ctrl Pts',(6.50864441544907,-1.86129832025651,36.6085158387645));
#56747=CARTESIAN_POINT('Ctrl Pts',(6.55485164049888,-1.68113324012382,36.6172648279555));
#56748=CARTESIAN_POINT('Ctrl Pts',(6.60199852639096,-1.4973043591296,36.6261917348324));
#56749=CARTESIAN_POINT('Ctrl Pts',(6.64140767441001,-1.31149113173701,36.6351186417093));
#56750=CARTESIAN_POINT('Ctrl Pts',(6.67293975269596,-1.12435050446469,36.6440455485862));
#56751=CARTESIAN_POINT('Ctrl Pts',(6.70384664831501,-0.940920291564142,
36.6527954627702));
#56752=CARTESIAN_POINT('Ctrl Pts',(6.72718585889661,-0.756215114278357,
36.6615453769542));
#56753=CARTESIAN_POINT('Ctrl Pts',(6.7428781045186,-0.570862389375578,36.6702952911382));
#56754=CARTESIAN_POINT('Ctrl Pts',(6.75857004154121,-0.385513309568533,
36.6790450332488));
#56755=CARTESIAN_POINT('Ctrl Pts',(6.76661529035555,-0.199516993259636,
36.6877947753593));
#56756=CARTESIAN_POINT('Ctrl Pts',(6.76698652348896,-0.013505218205474,
36.6965445174699));
#56757=CARTESIAN_POINT('Ctrl Pts',(6.76735774981525,0.172503146037491,36.7052940991406));
#56758=CARTESIAN_POINT('Ctrl Pts',(6.76005524147487,0.358526681832086,36.7140436808112));
#56759=CARTESIAN_POINT('Ctrl Pts',(6.74510380214892,0.543933542113499,36.7227932624819));
#56760=CARTESIAN_POINT('Ctrl Pts',(6.73015261710994,0.729337249083414,36.7315426953438));
#56761=CARTESIAN_POINT('Ctrl Pts',(6.70755278444622,0.914124015853416,36.7402921282057));
#56762=CARTESIAN_POINT('Ctrl Pts',(6.67738106408309,1.09766621749267,36.7490415610676));
#56763=CARTESIAN_POINT('Ctrl Pts',(6.64720981677277,1.28120554143203,36.75779085675));
#56764=CARTESIAN_POINT('Ctrl Pts',(6.60946696581549,1.46350005650501,36.7665401524323));
#56765=CARTESIAN_POINT('Ctrl Pts',(6.56428070011024,1.64393062206415,36.7752894481147));
#56766=CARTESIAN_POINT('Ctrl Pts',(6.51909508282775,1.8243585984453,36.7840386182447));
#56767=CARTESIAN_POINT('Ctrl Pts',(6.466466334157,2.00292240086438,36.7927877883747));
#56768=CARTESIAN_POINT('Ctrl Pts',(6.40657319597236,2.17901557696326,36.8015369585047));
#56769=CARTESIAN_POINT('Ctrl Pts',(6.34668083768339,2.35510646007314,36.8102860147077));
#56770=CARTESIAN_POINT('Ctrl Pts',(6.27952437143931,2.52872650996418,36.8190350709108));
#56771=CARTESIAN_POINT('Ctrl Pts',(6.20533187335181,2.69928607997821,36.8277841271139));
#56772=CARTESIAN_POINT('Ctrl Pts',(6.12831449784299,2.87633970115298,36.8368663034027));
#56773=CARTESIAN_POINT('Ctrl Pts',(6.043714894632,3.05009490562255,36.8459484796916));
#56774=CARTESIAN_POINT('Ctrl Pts',(5.95184265120539,3.21991584599543,36.8550306559804));
#56775=CARTESIAN_POINT('Ctrl Pts',(5.86333281335542,3.38352155905215,36.8637804363349));
#56776=CARTESIAN_POINT('Ctrl Pts',(5.76807337235736,3.54347560903741,36.8725302166893));
#56777=CARTESIAN_POINT('Ctrl Pts',(5.66638790086408,3.69923467178567,36.8812799970437));
#56778=CARTESIAN_POINT('Ctrl Pts',(5.56470608502797,3.85498813489685,36.890029462838));
#56779=CARTESIAN_POINT('Ctrl Pts',(5.45659885767009,4.00654667256184,36.8987789286322));
#56780=CARTESIAN_POINT('Ctrl Pts',(5.34243340580566,4.15339551506135,36.9075283944265));
#56781=CARTESIAN_POINT('Ctrl Pts',(5.22827145140647,4.30023985883805,36.9162775921804));
#56782=CARTESIAN_POINT('Ctrl Pts',(5.10805181978138,4.44237456992987,36.9250267899342));
#56783=CARTESIAN_POINT('Ctrl Pts',(4.98218281282593,4.57931691626403,36.9337759876881));
#56784=CARTESIAN_POINT('Ctrl Pts',(4.85631699296275,4.71625579512114,36.9425249639061));
#56785=CARTESIAN_POINT('Ctrl Pts',(4.72480227791888,4.84800236135721,36.9512739401241));
#56786=CARTESIAN_POINT('Ctrl Pts',(4.58808530848167,4.97410918678859,36.9600229163421));
#56787=CARTESIAN_POINT('Ctrl Pts',(4.45135945057028,5.10022421088958,36.9687724613633));
#56788=CARTESIAN_POINT('Ctrl Pts',(4.30943087208103,5.22069856611934,36.9775220063845));
#56789=CARTESIAN_POINT('Ctrl Pts',(4.16278164322535,5.33512305301631,36.9862715514057));
#56790=CARTESIAN_POINT('Ctrl Pts',(4.01614103534455,5.44954081331379,36.995020582073));
#56791=CARTESIAN_POINT('Ctrl Pts',(3.86478055833474,5.55790924068295,37.0037696127402));
#56792=CARTESIAN_POINT('Ctrl Pts',(3.70921425812008,5.65986029751254,37.0125186434075));
#56793=CARTESIAN_POINT('Ctrl Pts',(3.5536458453018,5.76181273884617,37.0212677928873));
#56794=CARTESIAN_POINT('Ctrl Pts',(3.39387173464407,5.85734747818027,37.0300169423672));
#56795=CARTESIAN_POINT('Ctrl Pts',(3.23043456092471,5.94614005448772,37.038766091847));
#56796=CARTESIAN_POINT('Ctrl Pts',(3.18690768806435,5.96978744811259,37.0410961805801));
#56797=CARTESIAN_POINT('Ctrl Pts',(3.14312114982902,5.9929568849929,37.0434262693131));
#56798=CARTESIAN_POINT('Ctrl Pts',(3.09908550384717,6.01564277861014,37.0457563580462));
#56799=CARTESIAN_POINT('Ctrl Pts',(3.0990855038472,6.01564277861013,35.0459194627137));
#56800=CARTESIAN_POINT('Ctrl Pts',(2.93136712737222,6.1020464445842,35.0547735800526));
#56801=CARTESIAN_POINT('Ctrl Pts',(2.75987960907094,6.18151138996883,35.0636276973915));
#56802=CARTESIAN_POINT('Ctrl Pts',(2.58519441278919,6.25372359863174,35.0724818147303));
#56803=CARTESIAN_POINT('Ctrl Pts',(2.57466267638231,6.25807725860514,35.0730156277375));
#56804=CARTESIAN_POINT('Ctrl Pts',(2.56411932536443,6.26240456914106,35.0735494407446));
#56805=CARTESIAN_POINT('Ctrl Pts',(2.55356448819932,6.26670546655955,35.0740832537517));
#56806=CARTESIAN_POINT('Ctrl Pts',(2.39122705594141,6.33285491371824,35.0822935019562));
#56807=CARTESIAN_POINT('Ctrl Pts',(2.2263263371004,6.39268881649299,35.0905037501607));
#56808=CARTESIAN_POINT('Ctrl Pts',(2.05939522783671,6.44602050070921,35.0987139983652));
#56809=CARTESIAN_POINT('Ctrl Pts',(1.89242443572067,6.49936486292991,35.1069261983094));
#56810=CARTESIAN_POINT('Ctrl Pts',(1.72342263064715,6.54620381877281,35.1151383982535));
#56811=CARTESIAN_POINT('Ctrl Pts',(1.55293741088268,6.5864007164673,35.1233505981977));
#56812=CARTESIAN_POINT('Ctrl Pts',(1.3823813047447,6.62661432770628,35.1315662127081));
#56813=CARTESIAN_POINT('Ctrl Pts',(1.21034090129479,6.66018029723885,35.1397818272185));
#56814=CARTESIAN_POINT('Ctrl Pts',(1.03737360229679,6.68701316054169,35.1479974417289));
#56815=CARTESIAN_POINT('Ctrl Pts',(0.86421206860269,6.71387615597401,35.1562222820143));
#56816=CARTESIAN_POINT('Ctrl Pts',(0.690121912293478,6.73399088885896,35.1644471222997));
#56817=CARTESIAN_POINT('Ctrl Pts',(0.515666242315641,6.74732371585476,35.1726719625851));
#56818=CARTESIAN_POINT('Ctrl Pts',(0.341098827417393,6.76066508298967,35.1809020711666));
#56819=CARTESIAN_POINT('Ctrl Pts',(0.166165786911986,6.76721587130811,35.1891321797481));
#56820=CARTESIAN_POINT('Ctrl Pts',(-0.00857021009941388,6.76699457303601,
35.1973622883296));
#56821=CARTESIAN_POINT('Ctrl Pts',(-0.183545772844242,6.76677297136059,
35.2056036805162));
#56822=CARTESIAN_POINT('Ctrl Pts',(-0.358323397887863,6.75976075224408,
35.2138450727029));
#56823=CARTESIAN_POINT('Ctrl Pts',(-0.532344962192309,6.74602830124722,
35.2220864648896));
#56824=CARTESIAN_POINT('Ctrl Pts',(-0.608083568257796,6.74005158967977,
35.2256733281542));
#56825=CARTESIAN_POINT('Ctrl Pts',(-0.683679079804085,6.73280258171049,
35.2292601914188));
#56826=CARTESIAN_POINT('Ctrl Pts',(-0.759086148045756,6.72429009039951,
35.2328470546835));
#56827=CARTESIAN_POINT('Ctrl Pts',(-0.936699895508152,6.70423977526012,
35.2412955495119));
#56828=CARTESIAN_POINT('Ctrl Pts',(-1.11367249075454,6.67713063639898,35.2497440443403));
#56829=CARTESIAN_POINT('Ctrl Pts',(-1.28942021218734,6.6430177266362,35.2581925391687));
#56830=CARTESIAN_POINT('Ctrl Pts',(-1.46500739828611,6.6089359770348,35.2666333167879));
#56831=CARTESIAN_POINT('Ctrl Pts',(-1.63937161501225,6.56786327199708,35.2750740944071));
#56832=CARTESIAN_POINT('Ctrl Pts',(-1.81193574336636,6.51990627708033,35.2835148720262));
#56833=CARTESIAN_POINT('Ctrl Pts',(-1.98436878106708,6.47198571333764,35.2919492374956));
#56834=CARTESIAN_POINT('Ctrl Pts',(-2.1550041363007,6.41719137423499,35.3003836029649));
#56835=CARTESIAN_POINT('Ctrl Pts',(-2.32327595385652,6.35568075364332,35.3088179684342));
#56836=CARTESIAN_POINT('Ctrl Pts',(-2.49144578258572,6.29420741437486,35.3172472218708));
#56837=CARTESIAN_POINT('Ctrl Pts',(-2.65725461732566,6.22602602375008,35.3256764753074));
#56838=CARTESIAN_POINT('Ctrl Pts',(-2.82015243589234,6.15134369372502,35.3341057287439));
#56839=CARTESIAN_POINT('Ctrl Pts',(-2.98297651084329,6.07669517228681,35.3425311662692));
#56840=CARTESIAN_POINT('Ctrl Pts',(-3.14289189476114,5.99555171849709,35.3509566037945));
#56841=CARTESIAN_POINT('Ctrl Pts',(-3.29936883688705,5.90816843684898,35.3593820413198));
#56842=CARTESIAN_POINT('Ctrl Pts',(-3.45581140523587,5.82080435095844,35.367805628003));
#56843=CARTESIAN_POINT('Ctrl Pts',(-3.60881674564846,5.72720333028828,35.3762292146862));
#56844=CARTESIAN_POINT('Ctrl Pts',(-3.75787952875216,5.62766651885002,35.3846528013694));
#56845=CARTESIAN_POINT('Ctrl Pts',(-3.9069256325118,5.52814084505919,35.3930754454974));
#56846=CARTESIAN_POINT('Ctrl Pts',(-4.05202978121308,5.42268088970375,35.4014980896254));
#56847=CARTESIAN_POINT('Ctrl Pts',(-4.19271521254371,5.31163140160389,35.4099207337534));
#56848=CARTESIAN_POINT('Ctrl Pts',(-4.33340451992718,5.20057885395709,35.4183436099354));
#56849=CARTESIAN_POINT('Ctrl Pts',(-4.46967460576564,5.08393667340918,35.4267664861174));
#56850=CARTESIAN_POINT('Ctrl Pts',(-4.60108112797115,4.96209043184702,35.4351893622993));
#56851=CARTESIAN_POINT('Ctrl Pts',(-4.73250959579531,4.84022384128615,35.4436136451484));
#56852=CARTESIAN_POINT('Ctrl Pts',(-4.85907263658495,4.71315168407173,35.4520379279974));
#56853=CARTESIAN_POINT('Ctrl Pts',(-4.98036190608001,4.58129722725639,35.4604622108465));
#56854=CARTESIAN_POINT('Ctrl Pts',(-5.10173308986262,4.44935372081668,35.4688921831446));
#56855=CARTESIAN_POINT('Ctrl Pts',(-5.21782315931491,4.31262170655697,35.4773221554428));
#56856=CARTESIAN_POINT('Ctrl Pts',(-5.32826263794759,4.17155921221932,35.485752127741));
#56857=CARTESIAN_POINT('Ctrl Pts',(-5.43874159691134,4.03044629031673,35.4941851136182));
#56858=CARTESIAN_POINT('Ctrl Pts',(-5.54356573661601,3.88500006782507,35.5026180994954));
#56859=CARTESIAN_POINT('Ctrl Pts',(-5.6424079327895,3.73570899830195,35.5110510853726));
#56860=CARTESIAN_POINT('Ctrl Pts',(-5.74134106318118,3.58628058190456,35.5194918295454));
#56861=CARTESIAN_POINT('Ctrl Pts',(-5.8342810755705,3.43300053271089,35.5279325737182));
#56862=CARTESIAN_POINT('Ctrl Pts',(-5.92094540033487,3.27638437400945,35.536373317891));
#56863=CARTESIAN_POINT('Ctrl Pts',(-5.96886442009193,3.18978711702404,35.5410404307761));
#56864=CARTESIAN_POINT('Ctrl Pts',(-6.01486560565325,3.10217034801432,35.5457075436612));
#56865=CARTESIAN_POINT('Ctrl Pts',(-6.05890740361888,3.01362407648538,35.5503746565462));
#56866=CARTESIAN_POINT('Ctrl Pts',(-6.13625931929622,2.85810763425941,35.5585716452936));
#56867=CARTESIAN_POINT('Ctrl Pts',(-6.20771484785789,2.69942007259873,35.5667686340411));
#56868=CARTESIAN_POINT('Ctrl Pts',(-6.27300523970475,2.53804930264105,35.5749656227885));
#56869=CARTESIAN_POINT('Ctrl Pts',(-6.33823577321284,2.37682647767103,35.5831550965232));
#56870=CARTESIAN_POINT('Ctrl Pts',(-6.39731228980008,2.21292567422031,35.5913445702578));
#56871=CARTESIAN_POINT('Ctrl Pts',(-6.45001232168374,2.04685858088142,35.5995340439925));
#56872=CARTESIAN_POINT('Ctrl Pts',(-6.50266850996351,1.88092964646957,35.6077167045236));
#56873=CARTESIAN_POINT('Ctrl Pts',(-6.5489586750115,1.71283835509394,35.6158993650547));
#56874=CARTESIAN_POINT('Ctrl Pts',(-6.58870881764961,1.54311539303654,35.6240820255859));
#56875=CARTESIAN_POINT('Ctrl Pts',(-6.62843926318373,1.37347653258509,35.6322606314217));
#56876=CARTESIAN_POINT('Ctrl Pts',(-6.66163605740798,1.20220796131236,35.6404392372576));
#56877=CARTESIAN_POINT('Ctrl Pts',(-6.68817524503397,1.02985479156765,35.6486178430935));
#56878=CARTESIAN_POINT('Ctrl Pts',(-6.7147089798616,0.857537033874542,35.6567947685355));
#56879=CARTESIAN_POINT('Ctrl Pts',(-6.73458777152393,0.684135476315733,
35.6649716939774));
#56880=CARTESIAN_POINT('Ctrl Pts',(-6.74773887873612,0.510204884720826,
35.6731486194194));
#56881=CARTESIAN_POINT('Ctrl Pts',(-6.76057309465491,0.340465353942477,
35.6811285122894));
#56882=CARTESIAN_POINT('Ctrl Pts',(-6.76700010762539,0.17022232465388,35.6891084051592));
#56883=CARTESIAN_POINT('Ctrl Pts',(-6.76699999999865,-4.27847436253801E-6,
35.6970882980292));
#56884=CARTESIAN_POINT('',(-6.76699909143212,0.00350664467830086,35.3028202162169));
#56885=CARTESIAN_POINT('Ctrl Pts',(3.09908550384707,6.01564277861019,34.6514623413619));
#56886=CARTESIAN_POINT('Ctrl Pts',(2.94225676158109,6.09643641939472,34.6597717816335));
#56887=CARTESIAN_POINT('Ctrl Pts',(2.78214665864428,6.17115516241344,34.668081221905));
#56888=CARTESIAN_POINT('Ctrl Pts',(2.61926119430939,6.239532017386,34.6763906621765));
#56889=CARTESIAN_POINT('Ctrl Pts',(2.45647935227009,6.30786537328572,34.6846948162595));
#56890=CARTESIAN_POINT('Ctrl Pts',(2.29092598676088,6.3698647463026,34.6929989703425));
#56891=CARTESIAN_POINT('Ctrl Pts',(2.12312973459856,6.42531004155157,34.7013031244254));
#56892=CARTESIAN_POINT('Ctrl Pts',(1.95540951419974,6.48073021345291,34.7096035157338));
#56893=CARTESIAN_POINT('Ctrl Pts',(1.78544876220221,6.52960211728033,34.7179039070422));
#56894=CARTESIAN_POINT('Ctrl Pts',(1.61379425525372,6.57175449189257,34.7262042983505));
#56895=CARTESIAN_POINT('Ctrl Pts',(1.44218611769813,6.61389547979521,34.7345024474567));
#56896=CARTESIAN_POINT('Ctrl Pts',(1.26888547465544,6.64932047391046,34.7428005965629));
#56897=CARTESIAN_POINT('Ctrl Pts',(1.09445258014889,6.67790854607979,34.7510987456691));
#56898=CARTESIAN_POINT('Ctrl Pts',(0.919996881133932,6.70650035571466,34.7593979796349));
#56899=CARTESIAN_POINT('Ctrl Pts',(0.744408977038477,6.72825339445515,34.7676972136008));
#56900=CARTESIAN_POINT('Ctrl Pts',(0.568258187685816,6.74309807374385,34.7759964475667));
#56901=CARTESIAN_POINT('Ctrl Pts',(0.392085688931662,6.75794458253955,34.7842967043574));
#56902=CARTESIAN_POINT('Ctrl Pts',(0.215350513402237,6.76588100520434,34.7925969611481));
#56903=CARTESIAN_POINT('Ctrl Pts',(0.0386258614192862,6.76688976139183,
34.8008972179388));
#56904=CARTESIAN_POINT('Ctrl Pts',(-0.138149907699033,6.76789880935937,
34.8091998755567));
#56905=CARTESIAN_POINT('Ctrl Pts',(-0.314914799295381,6.76197619512784,
34.8175025331745));
#56906=CARTESIAN_POINT('Ctrl Pts',(-0.491096662607798,6.74915647084697,
34.8258051907924));
#56907=CARTESIAN_POINT('Ctrl Pts',(-0.667358736770107,6.73633091009143,
34.8341116283864));
#56908=CARTESIAN_POINT('Ctrl Pts',(-0.843036906908127,6.71660200630864,
34.8424180659803));
#56909=CARTESIAN_POINT('Ctrl Pts',(-1.01756499031653,6.69005609023438,34.8507245035742));
#56910=CARTESIAN_POINT('Ctrl Pts',(-1.19230029145033,6.66347865611306,34.8590408034269));
#56911=CARTESIAN_POINT('Ctrl Pts',(-1.36588243360027,6.63006809193622,34.8673571032795));
#56912=CARTESIAN_POINT('Ctrl Pts',(-1.53775512353514,6.58996192553807,34.8756734031321));
#56913=CARTESIAN_POINT('Ctrl Pts',(-1.70973991161785,6.54982960124961,34.88399512701));
#56914=CARTESIAN_POINT('Ctrl Pts',(-1.88001268926494,6.50299305821419,34.8923168508878));
#56915=CARTESIAN_POINT('Ctrl Pts',(-2.04803300333657,6.44963951064276,34.9006385747657));
#56916=CARTESIAN_POINT('Ctrl Pts',(-2.21629673150151,6.39620866881391,34.9089723544767));
#56917=CARTESIAN_POINT('Ctrl Pts',(-2.38230114892681,6.33624207514864,34.9173061341877));
#56918=CARTESIAN_POINT('Ctrl Pts',(-2.54552526514105,6.26997528898867,34.9256399138987));
#56919=CARTESIAN_POINT('Ctrl Pts',(-2.64419250444711,6.22991772274334,34.9306775949482));
#56920=CARTESIAN_POINT('Ctrl Pts',(-2.74184424504694,6.18755892995849,34.9357152759977));
#56921=CARTESIAN_POINT('Ctrl Pts',(-2.83836998641614,6.14295896292756,34.9407529570472));
#56922=CARTESIAN_POINT('Ctrl Pts',(-2.9930243084011,6.07150053573624,34.9488243702892));
#56923=CARTESIAN_POINT('Ctrl Pts',(-3.14526281607396,5.99406642673338,34.9568957835312));
#56924=CARTESIAN_POINT('Ctrl Pts',(-3.29457816194719,5.91084120365458,34.9649671967732));
#56925=CARTESIAN_POINT('Ctrl Pts',(-3.44370605477106,5.82772046295003,34.9730284770245));
#56926=CARTESIAN_POINT('Ctrl Pts',(-3.58991776608896,5.73882325340684,34.9810897572757));
#56927=CARTESIAN_POINT('Ctrl Pts',(-3.73272482197509,5.64438255289372,34.989151037527));
#56928=CARTESIAN_POINT('Ctrl Pts',(-3.87538391367902,5.55003970357521,34.9972039653846));
#56929=CARTESIAN_POINT('Ctrl Pts',(-4.01464506153743,5.45016499736433,35.0052568932422));
#56930=CARTESIAN_POINT('Ctrl Pts',(-4.15004345744367,5.3450377268387,35.0133098210999));
#56931=CARTESIAN_POINT('Ctrl Pts',(-4.28533121451376,5.239996359538,35.0213561686242));
#56932=CARTESIAN_POINT('Ctrl Pts',(-4.41676220883512,5.12971119814665,35.0294025161487));
#56933=CARTESIAN_POINT('Ctrl Pts',(-4.54389985272087,5.01450527255115,35.037448863673));
#56934=CARTESIAN_POINT('Ctrl Pts',(-4.67096141906987,4.8993682847051,35.0454903963662));
#56935=CARTESIAN_POINT('Ctrl Pts',(-4.79373447361304,4.77931664415647,35.0535319290593));
#56936=CARTESIAN_POINT('Ctrl Pts',(-4.91181491694693,4.65471408591953,35.0615734617525));
#56937=CARTESIAN_POINT('Ctrl Pts',(-5.03216542580734,4.52771607620914,35.0697695908007));
#56938=CARTESIAN_POINT('Ctrl Pts',(-5.14764074695656,4.39599063152631,35.077965719849));
#56939=CARTESIAN_POINT('Ctrl Pts',(-5.25785154387946,4.25996316210885,35.0861618488972));
#56940=CARTESIAN_POINT('Ctrl Pts',(-5.3659462056352,4.12654752855294,35.0942006057333));
#56941=CARTESIAN_POINT('Ctrl Pts',(-5.46897645068472,3.98899389220856,35.1022393625694));
#56942=CARTESIAN_POINT('Ctrl Pts',(-5.56661521527149,3.8477375228968,35.1102781194055));
#56943=CARTESIAN_POINT('Ctrl Pts',(-5.66426343025872,3.70646748146143,35.1183176543083));
#56944=CARTESIAN_POINT('Ctrl Pts',(-5.75651891325343,3.56149430062665,35.1263571892111));
#56945=CARTESIAN_POINT('Ctrl Pts',(-5.84309779477765,3.4132824613068,35.1343967241139));
#56946=CARTESIAN_POINT('Ctrl Pts',(-5.92970219887138,3.26502693065132,35.1424386289894));
#56947=CARTESIAN_POINT('Ctrl Pts',(-6.01062648235128,3.11353116346445,35.1504805338649));
#56948=CARTESIAN_POINT('Ctrl Pts',(-6.08563269032308,2.95928433214369,35.1585224387404));
#56949=CARTESIAN_POINT('Ctrl Pts',(-6.16316902887444,2.79983440316903,35.1668356154213));
#56950=CARTESIAN_POINT('Ctrl Pts',(-6.23438085666861,2.63744495680056,35.1751487921021));
#56951=CARTESIAN_POINT('Ctrl Pts',(-6.29905972437611,2.47267781741632,35.1834619687829));
#56952=CARTESIAN_POINT('Ctrl Pts',(-6.36173665468294,2.31301054311053,35.1915178363935));
#56953=CARTESIAN_POINT('Ctrl Pts',(-6.41827896296015,2.15111094331454,35.199573704004));
#56954=CARTESIAN_POINT('Ctrl Pts',(-6.46854819473955,1.98750427731154,35.2076295716145));
#56955=CARTESIAN_POINT('Ctrl Pts',(-6.52122586902032,1.81605907401727,35.2160714028305));
#56956=CARTESIAN_POINT('Ctrl Pts',(-6.56701445761997,1.64273967608754,35.2245132340464));
#56957=CARTESIAN_POINT('Ctrl Pts',(-6.60581523590073,1.46816009656367,35.2329550652623));
#56958=CARTESIAN_POINT('Ctrl Pts',(-6.64461601418148,1.2935805170398,35.2413968964783));
#56959=CARTESIAN_POINT('Ctrl Pts',(-6.67642898426788,1.11774122489512,35.2498387276942));
#56960=CARTESIAN_POINT('Ctrl Pts',(-6.70121782300071,0.941259097537779,
35.2582805589102));
#56961=CARTESIAN_POINT('Ctrl Pts',(-6.74481367139252,0.630881989878215,
35.2731271113367));
#56962=CARTESIAN_POINT('Ctrl Pts',(-6.76683634641136,0.317566188239821,
35.2879736637632));
#56963=CARTESIAN_POINT('Ctrl Pts',(-6.76699909143182,0.00350664525299999,
35.3028202161897));
#56964=CARTESIAN_POINT('Ctrl Pts',(-6.76699909143212,0.00350664467849019,
35.3028202162169));
#56965=CARTESIAN_POINT('Ctrl Pts',(-6.76708746338061,-0.167030421380243,
35.3108820234392));
#56966=CARTESIAN_POINT('Ctrl Pts',(-6.7607250453901,-0.337839588124926,
35.3189438306615));
#56967=CARTESIAN_POINT('Ctrl Pts',(-6.74787647786183,-0.508381785195997,
35.3270056378839));
#56968=CARTESIAN_POINT('Ctrl Pts',(-6.73504143045245,-0.678744526403567,
35.3350589619355));
#56969=CARTESIAN_POINT('Ctrl Pts',(-6.71573384360594,-0.848840487435429,
35.3431122859871));
#56970=CARTESIAN_POINT('Ctrl Pts',(-6.68997033672216,-1.01812862339572,
35.3511656100387));
#56971=CARTESIAN_POINT('Ctrl Pts',(-6.66422827530273,-1.18727584442923,
35.359212230528));
#56972=CARTESIAN_POINT('Ctrl Pts',(-6.63204104580464,-1.35561621114065,
35.3672588510172));
#56973=CARTESIAN_POINT('Ctrl Pts',(-6.5934772201377,-1.52261194909446,35.3753054715065));
#56974=CARTESIAN_POINT('Ctrl Pts',(-6.55343892722467,-1.6959926797608,35.383659750226));
#56975=CARTESIAN_POINT('Ctrl Pts',(-6.50652679565116,-1.86792351633893,
35.3920140289454));
#56976=CARTESIAN_POINT('Ctrl Pts',(-6.45287643485501,-2.03781125634661,
35.4003683076649));
#56977=CARTESIAN_POINT('Ctrl Pts',(-6.40124942677632,-2.20129190392644,
35.4084075157623));
#56978=CARTESIAN_POINT('Ctrl Pts',(-6.34338328244956,-2.36288035711749,
35.4164467238596));
#56979=CARTESIAN_POINT('Ctrl Pts',(-6.27945022569185,-2.52206143126186,
35.424485931957));
#56980=CARTESIAN_POINT('Ctrl Pts',(-6.21552446196669,-2.68122434715111,
35.4325242229982));
#56981=CARTESIAN_POINT('Ctrl Pts',(-6.1455333021718,-2.83798008325793,35.4405625140394));
#56982=CARTESIAN_POINT('Ctrl Pts',(-6.06969761707096,-2.99183218735997,
35.4486008050806));
#56983=CARTESIAN_POINT('Ctrl Pts',(-5.99385551476963,-3.14569731039626,
35.4566397763204));
#56984=CARTESIAN_POINT('Ctrl Pts',(-5.91216806867525,-3.29665797700334,
35.4646787475601));
#56985=CARTESIAN_POINT('Ctrl Pts',(-5.82490265043725,-3.44424129714065,
35.4727177187999));
#56986=CARTESIAN_POINT('Ctrl Pts',(-5.73761250544533,-3.59186643517689,
35.4807589678912));
#56987=CARTESIAN_POINT('Ctrl Pts',(-5.64474143370571,-3.73611200072254,
35.4888002169825));
#56988=CARTESIAN_POINT('Ctrl Pts',(-5.54660067049607,-3.87653324531759,
35.4968414660737));
#56989=CARTESIAN_POINT('Ctrl Pts',(-5.44836692289814,-4.01708753334031,
35.504890333922));
#56990=CARTESIAN_POINT('Ctrl Pts',(-5.34485373119514,-4.15380996054235,
35.5129392017703));
#56991=CARTESIAN_POINT('Ctrl Pts',(-5.2364135956204,-4.2862876309928,35.5209880696185));
#56992=CARTESIAN_POINT('Ctrl Pts',(-5.12791246737458,-4.41883981414038,
35.5290414645909));
#56993=CARTESIAN_POINT('Ctrl Pts',(-5.01447912353585,-4.54714220666268,
35.5370948595632));
#56994=CARTESIAN_POINT('Ctrl Pts',(-4.89650322992137,-4.67081846354251,
35.5451482545356));
#56995=CARTESIAN_POINT('Ctrl Pts',(-4.77838336477845,-4.79464564837203,
35.5532114774444));
#56996=CARTESIAN_POINT('Ctrl Pts',(-4.65571015313716,-4.91383517099587,
35.5612747003532));
#56997=CARTESIAN_POINT('Ctrl Pts',(-4.52890706630093,-5.0280502965672,35.569337923262));
#56998=CARTESIAN_POINT('Ctrl Pts',(-4.49498985568179,-5.05860048715442,
35.5714946690991));
#56999=CARTESIAN_POINT('Ctrl Pts',(-4.46077733722195,-5.08879502042966,
35.5736514149362));
#57000=CARTESIAN_POINT('Ctrl Pts',(-4.42627796346472,-5.11862797926813,
35.5758081607733));
#57001=CARTESIAN_POINT('Ctrl Pts',(-4.28335043668362,-5.24222300604602,
35.5847433475556));
#57002=CARTESIAN_POINT('Ctrl Pts',(-4.13515258213284,-5.3599068105399,35.5936785343379));
#57003=CARTESIAN_POINT('Ctrl Pts',(-3.98217594772205,-5.47124882649145,
35.6026137211202));
#57004=CARTESIAN_POINT('Ctrl Pts',(-3.82942842498542,-5.58242408654738,
35.6115355257568));
#57005=CARTESIAN_POINT('Ctrl Pts',(-3.67191661173363,-5.68727635826303,
35.6204573303934));
#57006=CARTESIAN_POINT('Ctrl Pts',(-3.51016469527428,-5.78541552630838,
35.6293791350301));
#57007=CARTESIAN_POINT('Ctrl Pts',(-3.34880733009906,-5.88331530964891,
35.6382791772694));
#57008=CARTESIAN_POINT('Ctrl Pts',(-3.18323072427315,-5.97453453697728,
35.6471792195087));
#57009=CARTESIAN_POINT('Ctrl Pts',(-3.01398702545083,-6.05872686382329,
35.656079261748));
#57010=CARTESIAN_POINT('Ctrl Pts',(-2.84500387979123,-6.14278957534426,
35.6649656022415));
#57011=CARTESIAN_POINT('Ctrl Pts',(-2.67236513267249,-6.21984685103397,
35.6738519427349));
#57012=CARTESIAN_POINT('Ctrl Pts',(-2.49664903924339,-6.28959717111081,
35.6827382832283));
#57013=CARTESIAN_POINT('Ctrl Pts',(-2.32138222119325,-6.35916915179441,
35.6916019029003));
#57014=CARTESIAN_POINT('Ctrl Pts',(-2.14305399679716,-6.42147136183039,
35.7004655225722));
#57015=CARTESIAN_POINT('Ctrl Pts',(-1.96226348141899,-6.47624976583589,
35.7093291422441));
#57016=CARTESIAN_POINT('Ctrl Pts',(-1.79063824971273,-6.52825114577708,
35.7177434153976));
#57017=CARTESIAN_POINT('Ctrl Pts',(-1.61679440425823,-6.57347246625104,
35.7261576885511));
#57018=CARTESIAN_POINT('Ctrl Pts',(-1.44126284911579,-6.61173580837579,
35.7345719617046));
#57019=CARTESIAN_POINT('Ctrl Pts',(-1.26998749245017,-6.64907136074594,
35.7427822099092));
#57020=CARTESIAN_POINT('Ctrl Pts',(-1.09726966871086,-6.67974539469198,
35.7509924581137));
#57021=CARTESIAN_POINT('Ctrl Pts',(-0.923666389551918,-6.70366537058736,
35.7592027063182));
#57022=CARTESIAN_POINT('Ctrl Pts',(-0.750021841432833,-6.72759103273784,
35.7674149062624));
#57023=CARTESIAN_POINT('Ctrl Pts',(-0.575491771160288,-6.74475938948673,
35.7756271062066));
#57024=CARTESIAN_POINT('Ctrl Pts',(-0.400639097955959,-6.75512970365404,
35.7838393061508));
#57025=CARTESIAN_POINT('Ctrl Pts',(-0.225713722424808,-6.76550432971406,
35.7920549206613));
#57026=CARTESIAN_POINT('Ctrl Pts',(-0.0504658317656606,-6.76907526098659,
35.8002705351718));
#57027=CARTESIAN_POINT('Ctrl Pts',(0.124540773021885,-6.76585387041836,
35.8084861496823));
#57028=CARTESIAN_POINT('Ctrl Pts',(0.299743902554118,-6.76262886236976,
35.8167109899677));
#57029=CARTESIAN_POINT('Ctrl Pts',(0.474704849010942,-6.75259630448826,
35.8249358302531));
#57030=CARTESIAN_POINT('Ctrl Pts',(0.648863073961833,-6.73581960204167,
35.8331606705385));
#57031=CARTESIAN_POINT('Ctrl Pts',(0.823132853310406,-6.71903215353392,
35.8413907791201));
#57032=CARTESIAN_POINT('Ctrl Pts',(0.996598534377933,-6.69549199677668,
35.8496208877016));
#57033=CARTESIAN_POINT('Ctrl Pts',(1.16870895120514,-6.66531382512279,35.8578509962831));
#57034=CARTESIAN_POINT('Ctrl Pts',(1.34105533405454,-6.63509427873253,35.8660923884698));
#57035=CARTESIAN_POINT('Ctrl Pts',(1.51204239440781,-6.59821861433577,35.8743337806565));
#57036=CARTESIAN_POINT('Ctrl Pts',(1.6811323426534,-6.55485187067448,35.8825751728432));
#57037=CARTESIAN_POINT('Ctrl Pts',(1.75472458411031,-6.53597756203677,35.8861620361076));
#57038=CARTESIAN_POINT('Ctrl Pts',(1.82795770277806,-6.51587433314231,35.889748899372));
#57039=CARTESIAN_POINT('Ctrl Pts',(1.90078853251695,-6.49455864202119,35.8933357626364));
#57040=CARTESIAN_POINT('Ctrl Pts',(2.07233420990709,-6.44435168041547,35.9017842574648));
#57041=CARTESIAN_POINT('Ctrl Pts',(2.24203792725608,-6.38730035969397,35.9102327522933));
#57042=CARTESIAN_POINT('Ctrl Pts',(2.40933404653316,-6.32355900203486,35.9186812471217));
#57043=CARTESIAN_POINT('Ctrl Pts',(2.57647735052358,-6.25987586840322,35.9271220247409));
#57044=CARTESIAN_POINT('Ctrl Pts',(2.74121713001409,-6.18951499698267,35.9355628023601));
#57045=CARTESIAN_POINT('Ctrl Pts',(2.9030031012906,-6.11268042628577,35.9440035799792));
#57046=CARTESIAN_POINT('Ctrl Pts',(3.06466616968524,-6.03590422400049,35.9524379454486));
#57047=CARTESIAN_POINT('Ctrl Pts',(3.22337960295659,-5.95266426873485,35.9608723109179));
#57048=CARTESIAN_POINT('Ctrl Pts',(3.37861292937405,-5.86321274332311,35.9693066763872));
#57049=CARTESIAN_POINT('Ctrl Pts',(3.53375216953899,-5.7738154340968,35.9777359298238));
#57050=CARTESIAN_POINT('Ctrl Pts',(3.68541522000411,-5.67821422683876,35.9861651832604));
#57051=CARTESIAN_POINT('Ctrl Pts',(3.83309571509002,-5.57670747295916,35.994594436697));
#57052=CARTESIAN_POINT('Ctrl Pts',(3.98070935542008,-5.47524667104664,36.0030198742223));
#57053=CARTESIAN_POINT('Ctrl Pts',(4.12434376104425,-5.36788584193663,36.0114453117475));
#57054=CARTESIAN_POINT('Ctrl Pts',(4.2635207662896,-5.25496714313395,36.0198707492728));
#57055=CARTESIAN_POINT('Ctrl Pts',(4.40266719808954,-5.14207324953286,36.0282943359559));
#57056=CARTESIAN_POINT('Ctrl Pts',(4.53735792143644,-5.02362412834757,36.0367179226392));
#57057=CARTESIAN_POINT('Ctrl Pts',(4.66714672430506,-4.9000031075305,36.0451415093223));
#57058=CARTESIAN_POINT('Ctrl Pts',(4.79692100448706,-4.77639591925757,36.0535641534504));
#57059=CARTESIAN_POINT('Ctrl Pts',(4.92179421629,-4.64761821494519,36.0619867975784));
#57060=CARTESIAN_POINT('Ctrl Pts',(5.04135576816381,-4.51409138352354,36.0704094417064));
#57061=CARTESIAN_POINT('Ctrl Pts',(5.16092061410174,-4.38056087327758,36.0788323178883));
#57062=CARTESIAN_POINT('Ctrl Pts',(5.27517328622964,-4.24228122369439,36.0872551940703));
#57063=CARTESIAN_POINT('Ctrl Pts',(5.38374213261956,-4.09970848347257,36.0956780702522));
#57064=CARTESIAN_POINT('Ctrl Pts',(5.49232911060918,-3.95711193281213,36.1041023531012));
#57065=CARTESIAN_POINT('Ctrl Pts',(5.5952301688979,-3.81022112766847,36.1125266359502));
#57066=CARTESIAN_POINT('Ctrl Pts',(5.69211558349487,-3.65952308151415,36.1209509187992));
#57067=CARTESIAN_POINT('Ctrl Pts',(5.78906643091869,-3.50872325947127,36.1293808910974));
#57068=CARTESIAN_POINT('Ctrl Pts',(5.8799933358985,-3.35411133916849,36.1378108633956));
#57069=CARTESIAN_POINT('Ctrl Pts',(5.96461082667901,-3.19620191575306,36.1462408356937));
#57070=CARTESIAN_POINT('Ctrl Pts',(6.04925856684666,-3.03823604226759,36.1546738215709));
#57071=CARTESIAN_POINT('Ctrl Pts',(6.12759224339033,-2.87697061193304,36.1631068074481));
#57072=CARTESIAN_POINT('Ctrl Pts',(6.19937332638077,-2.71294293345043,36.1715397933253));
#57073=CARTESIAN_POINT('Ctrl Pts',(6.27122044753022,-2.54876435050299,36.1799805374981));
#57074=CARTESIAN_POINT('Ctrl Pts',(6.33650280265216,-2.3818187501014,36.1884212816709));
#57075=CARTESIAN_POINT('Ctrl Pts',(6.39503039802752,-2.21266247048754,36.1968620258438));
#57076=CARTESIAN_POINT('Ctrl Pts',(6.42739186864194,-2.11913144573141,36.2015291387289));
#57077=CARTESIAN_POINT('Ctrl Pts',(6.45768910090555,-2.02492483767073,36.2061962516141));
#57078=CARTESIAN_POINT('Ctrl Pts',(6.48589658976253,-1.9301384476008,36.2108633644992));
#57079=CARTESIAN_POINT('Ctrl Pts',(6.53510206876611,-1.76479194156975,36.219004731717));
#57080=CARTESIAN_POINT('Ctrl Pts',(6.57804329603186,-1.59735186879326,36.2271460989349));
#57081=CARTESIAN_POINT('Ctrl Pts',(6.61453994949666,-1.42833828504062,36.2352874661527));
#57082=CARTESIAN_POINT('Ctrl Pts',(6.65100474415887,-1.25947223729159,36.2434217265761));
#57083=CARTESIAN_POINT('Ctrl Pts',(6.68103608615913,-1.08903576801106,36.2515559869996));
#57084=CARTESIAN_POINT('Ctrl Pts',(6.70450328506581,-0.91756454843337,36.2596902474231));
#57085=CARTESIAN_POINT('Ctrl Pts',(6.72795447549683,-0.746210300329624,
36.2678189589478));
#57086=CARTESIAN_POINT('Ctrl Pts',(6.74485038860386,-0.573823068480533,
36.2759476704725));
#57087=CARTESIAN_POINT('Ctrl Pts',(6.75511130774931,-0.400949148792437,
36.2840763819973));
#57088=CARTESIAN_POINT('Ctrl Pts',(6.76536733365211,-0.228157669480848,
36.2922012170898));
#57089=CARTESIAN_POINT('Ctrl Pts',(6.76899464479822,-0.054880329140094,
36.3003260521822));
#57090=CARTESIAN_POINT('Ctrl Pts',(6.76596532412493,0.118331030330624,36.3084508872747));
#57091=CARTESIAN_POINT('Ctrl Pts',(6.76293685151845,0.291493898795741,36.3165734477968));
#57092=CARTESIAN_POINT('Ctrl Pts',(6.75325546613401,0.464590457522918,36.324696008319));
#57093=CARTESIAN_POINT('Ctrl Pts',(6.73694535866609,0.637068469120464,36.3328185688411));
#57094=CARTESIAN_POINT('Ctrl Pts',(6.72063438435824,0.80955564747711,36.3409415610562));
#57095=CARTESIAN_POINT('Ctrl Pts',(6.697694014737,0.981423848227725,36.3490645532714));
#57096=CARTESIAN_POINT('Ctrl Pts',(6.66820036674673,1.15212537031294,36.3571875454865));
#57097=CARTESIAN_POINT('Ctrl Pts',(6.65314475825274,1.23926329528894,36.361334085468));
#57098=CARTESIAN_POINT('Ctrl Pts',(6.63638233341226,1.32609731651731,36.3654806254495));
#57099=CARTESIAN_POINT('Ctrl Pts',(6.61792837136154,1.41255551095451,36.369627165431));
#57100=CARTESIAN_POINT('Ctrl Pts',(6.5779470607922,1.59987094563239,36.3786108244594));
#57101=CARTESIAN_POINT('Ctrl Pts',(6.53004276773826,1.78532894167697,36.3875944834879));
#57102=CARTESIAN_POINT('Ctrl Pts',(6.4744203895597,1.96829104028181,36.3965781425163));
#57103=CARTESIAN_POINT('Ctrl Pts',(6.41870245272483,2.15156746583332,36.4055772353757));
#57104=CARTESIAN_POINT('Ctrl Pts',(6.35523999814356,2.33233919474975,36.4145763282352));
#57105=CARTESIAN_POINT('Ctrl Pts',(6.28428689503124,2.50998550213713,36.4235754210947));
#57106=CARTESIAN_POINT('Ctrl Pts',(6.21316742671953,2.68804834047318,36.4325956143121));
#57107=CARTESIAN_POINT('Ctrl Pts',(6.13452225753113,2.86297087179123,36.4416158075296));
#57108=CARTESIAN_POINT('Ctrl Pts',(6.04865345865544,3.03415232595458,36.4506360007471));
#57109=CARTESIAN_POINT('Ctrl Pts',(5.96269769611887,3.20550714420504,36.4596653291689));
#57110=CARTESIAN_POINT('Ctrl Pts',(5.86950380139162,3.37311310539593,36.4686946575907));
#57111=CARTESIAN_POINT('Ctrl Pts',(5.76941930559148,3.53639503962275,36.4777239860125));
#57112=CARTESIAN_POINT('Ctrl Pts',(5.66919371082616,3.6999071684643,36.4867660439674));
#57113=CARTESIAN_POINT('Ctrl Pts',(5.56205821605885,3.8590828773121,36.4958081019222));
#57114=CARTESIAN_POINT('Ctrl Pts',(5.44840437058529,4.01337499052694,36.504850159877));
#57115=CARTESIAN_POINT('Ctrl Pts',(5.34977257695484,4.14727374077163,36.5126970953721));
#57116=CARTESIAN_POINT('Ctrl Pts',(5.24623239078634,4.27749494957618,36.5205440308672));
#57117=CARTESIAN_POINT('Ctrl Pts',(5.13806432240161,4.40370117274819,36.5283909663623));
#57118=CARTESIAN_POINT('Ctrl Pts',(5.01876243282036,4.54289789804959,36.5370455928705));
#57119=CARTESIAN_POINT('Ctrl Pts',(4.89372473713899,4.67733240286398,36.5457002193786));
#57120=CARTESIAN_POINT('Ctrl Pts',(4.76334973590017,4.80653599731654,36.5543548458869));
#57121=CARTESIAN_POINT('Ctrl Pts',(4.6331375630723,4.93557822635569,36.5629986634281));
#57122=CARTESIAN_POINT('Ctrl Pts',(4.49760160300558,5.05940236966045,36.5716424809694));
#57123=CARTESIAN_POINT('Ctrl Pts',(4.35717837145664,5.17757526640709,36.5802862985107));
#57124=CARTESIAN_POINT('Ctrl Pts',(4.21686407093436,5.29565649246061,36.5889234107517));
#57125=CARTESIAN_POINT('Ctrl Pts',(4.07167029085023,5.40809501883335,36.5975605229928));
#57126=CARTESIAN_POINT('Ctrl Pts',(3.92206895355486,5.51449581771182,36.6061976352339));
#57127=CARTESIAN_POINT('Ctrl Pts',(3.7726101150563,5.62079526732366,36.6148265204221));
#57128=CARTESIAN_POINT('Ctrl Pts',(3.61875234417994,5.72106829015106,36.6234554056104));
#57129=CARTESIAN_POINT('Ctrl Pts',(3.46099924771643,5.81496115269108,36.6320842907986));
#57130=CARTESIAN_POINT('Ctrl Pts',(3.34248430827023,5.88549990703454,36.6385669008298));
#57131=CARTESIAN_POINT('Ctrl Pts',(3.2217715316867,5.95243847868828,36.6450495108609));
#57132=CARTESIAN_POINT('Ctrl Pts',(3.09908550384717,6.01564277861014,36.651532120892));
#57133=CARTESIAN_POINT('Origin',(0.,0.,-63.6971797838103));
#57134=CARTESIAN_POINT('',(3.09908550384713,6.01564277861016,39.0456530966623));
#57135=CARTESIAN_POINT('',(3.09908550384735,6.01564277861005,38.6513967904261));
#57136=CARTESIAN_POINT('',(3.09908550384721,6.01564277861012,-63.6971797838103));
#57137=CARTESIAN_POINT('',(-6.76700535807815,-1.06911827047406E-5,37.6971705070289));
#57138=CARTESIAN_POINT('Ctrl Pts',(-6.76699974905361,-0.00184290760892239,
37.6971797838099));
#57139=CARTESIAN_POINT('Ctrl Pts',(-6.76693552975974,-0.237650684080379,
37.7082773287428));
#57140=CARTESIAN_POINT('Ctrl Pts',(-6.75454167359002,-0.473079103425044,
37.7193748736757));
#57141=CARTESIAN_POINT('Ctrl Pts',(-6.72996025036087,-0.707053059227286,
37.7304724186087));
#57142=CARTESIAN_POINT('Ctrl Pts',(-6.70499092345331,-0.944719208002343,
37.7417450867825));
#57143=CARTESIAN_POINT('Ctrl Pts',(-6.66744627003892,-1.18088516299746,
37.7530177549562));
#57144=CARTESIAN_POINT('Ctrl Pts',(-6.61752558591685,-1.4144412747569,37.76429042313));
#57145=CARTESIAN_POINT('Ctrl Pts',(-6.6045686968806,-1.47506064881043,37.7672162386159));
#57146=CARTESIAN_POINT('Ctrl Pts',(-6.59077834990439,-1.53550427290328,
37.7701420541018));
#57147=CARTESIAN_POINT('Ctrl Pts',(-6.57615859055703,-1.59575286051536,
37.7730678695877));
#57148=CARTESIAN_POINT('Ctrl Pts',(-6.53547768294063,-1.76340043722524,
37.7812092368056));
#57149=CARTESIAN_POINT('Ctrl Pts',(-6.48832991777303,-1.92970502288278,
37.7893506040235));
#57150=CARTESIAN_POINT('Ctrl Pts',(-6.4348211596328,-2.09412646312059,37.7974919712414));
#57151=CARTESIAN_POINT('Ctrl Pts',(-6.38135911056881,-2.25840437594618,
37.8056262316649));
#57152=CARTESIAN_POINT('Ctrl Pts',(-6.32154723368755,-2.42080206973341,
37.8137604920884));
#57153=CARTESIAN_POINT('Ctrl Pts',(-6.25554214140539,-2.58079087046999,
37.8218947525119));
#57154=CARTESIAN_POINT('Ctrl Pts',(-6.18958207541336,-2.74067053262482,
37.8300234640367));
#57155=CARTESIAN_POINT('Ctrl Pts',(-6.11743734447345,-2.89814423640583,
37.8381521755615));
#57156=CARTESIAN_POINT('Ctrl Pts',(-6.03931395731611,-3.05269977642199,
37.8462808870864));
#57157=CARTESIAN_POINT('Ctrl Pts',(-5.96122782575807,-3.20718161175793,
37.8544057221789));
#57158=CARTESIAN_POINT('Ctrl Pts',(-5.87716888032726,-3.35874772853615,
37.8625305572714));
#57159=CARTESIAN_POINT('Ctrl Pts',(-5.7873906840792,-3.50690719435706,37.870655392364));
#57160=CARTESIAN_POINT('Ctrl Pts',(-5.6976376214887,-3.65502518252044,37.8787779528862));
#57161=CARTESIAN_POINT('Ctrl Pts',(-5.60216868744704,-3.79973810695931,
37.8869005134084));
#57162=CARTESIAN_POINT('Ctrl Pts',(-5.50128267391272,-3.94058091424447,
37.8950230739306));
#57163=CARTESIAN_POINT('Ctrl Pts',(-5.40039129854866,-4.08143120695922,
37.9031460661458));
#57164=CARTESIAN_POINT('Ctrl Pts',(-5.29408247852451,-4.21841067174524,
37.911269058361));
#57165=CARTESIAN_POINT('Ctrl Pts',(-5.18269759614329,-4.35108430473722,
37.9193920505762));
#57166=CARTESIAN_POINT('Ctrl Pts',(-5.12583900809701,-4.41881015120421,
37.9235385905571));
#57167=CARTESIAN_POINT('Ctrl Pts',(-5.06765836793178,-4.48541449969006,
37.9276851305381));
#57168=CARTESIAN_POINT('Ctrl Pts',(-5.00820507123816,-4.55084288505156,
37.931831670519));
#57169=CARTESIAN_POINT('Ctrl Pts',(-4.87939692081389,-4.69259632468153,
37.9408153295474));
#57170=CARTESIAN_POINT('Ctrl Pts',(-4.74467664467028,-4.82875776116382,
37.9497989885758));
#57171=CARTESIAN_POINT('Ctrl Pts',(-4.60454258261437,-4.95887856323292,
37.9587826476041));
#57172=CARTESIAN_POINT('Ctrl Pts',(-4.46416777172448,-5.08922291146144,
37.9677817404635));
#57173=CARTESIAN_POINT('Ctrl Pts',(-4.31836076045437,-5.21350572033224,
37.9767808333229));
#57174=CARTESIAN_POINT('Ctrl Pts',(-4.16765328480797,-5.33131832642072,
37.9857799261823));
#57175=CARTESIAN_POINT('Ctrl Pts',(-4.01659244224615,-5.44940717014791,
37.9948001193997));
#57176=CARTESIAN_POINT('Ctrl Pts',(-3.8606083345819,-5.56099530909942,38.003820312617));
#57177=CARTESIAN_POINT('Ctrl Pts',(-3.70026431117455,-5.6657155794699,38.0128405058344));
#57178=CARTESIAN_POINT('Ctrl Pts',(-3.5397578992929,-5.77054190533639,38.021869834256));
#57179=CARTESIAN_POINT('Ctrl Pts',(-3.3748829539253,-5.86848634177909,38.0308991626777));
#57180=CARTESIAN_POINT('Ctrl Pts',(-3.20622922738068,-5.95922672345078,
38.0399284910994));
#57181=CARTESIAN_POINT('Ctrl Pts',(-3.03733773307671,-6.05009503077033,
38.0489705490541));
#57182=CARTESIAN_POINT('Ctrl Pts',(-2.86465701626704,-6.13373886238583,
38.0580126070089));
#57183=CARTESIAN_POINT('Ctrl Pts',(-2.68880078161175,-6.20988239476434,
38.0670546649636));
#57184=CARTESIAN_POINT('Ctrl Pts',(-2.53618812011712,-6.27596175302345,
38.0749016004593));
#57185=CARTESIAN_POINT('Ctrl Pts',(-2.38118432692681,-6.33639318090253,
38.082748535955));
#57186=CARTESIAN_POINT('Ctrl Pts',(-2.22420161295688,-6.39102622314445,
38.0905954714507));
#57187=CARTESIAN_POINT('Ctrl Pts',(-2.05108380003152,-6.45127459410962,
38.0992489357516));
#57188=CARTESIAN_POINT('Ctrl Pts',(-1.87540633154713,-6.50452321409249,
38.1079024000524));
#57189=CARTESIAN_POINT('Ctrl Pts',(-1.6977491900116,-6.5505676614943,38.1165558643532));
#57190=CARTESIAN_POINT('Ctrl Pts',(-1.52025570704185,-6.59656969254202,
38.1252013570434));
#57191=CARTESIAN_POINT('Ctrl Pts',(-1.34078648166763,-6.63538071170318,
38.1338468497336));
#57192=CARTESIAN_POINT('Ctrl Pts',(-1.15993705013949,-6.66684595890093,
38.1424923424238));
#57193=CARTESIAN_POINT('Ctrl Pts',(-0.973647073918563,-6.69925778404589,
38.1513979199203));
#57194=CARTESIAN_POINT('Ctrl Pts',(-0.785892855662658,-6.72387484896148,
38.1603034974169));
#57195=CARTESIAN_POINT('Ctrl Pts',(-0.597339508404085,-6.7405841372762,
38.1692090749134));
#57196=CARTESIAN_POINT('Ctrl Pts',(-0.41464013159659,-6.75677465633291,
38.1778381630859));
#57197=CARTESIAN_POINT('Ctrl Pts',(-0.231190833158081,-6.76554101372821,
38.1864672512585));
#57198=CARTESIAN_POINT('Ctrl Pts',(-0.0476050447402823,-6.76683254999821,
38.1950963394311));
#57199=CARTESIAN_POINT('Ctrl Pts',(0.144804302351395,-6.76818616049604,
38.2041401615896));
#57200=CARTESIAN_POINT('Ctrl Pts',(0.337363249713542,-6.76132866194586,
38.2131839837481));
#57201=CARTESIAN_POINT('Ctrl Pts',(0.529361336727085,-6.74626308226847,
38.2222278059066));
#57202=CARTESIAN_POINT('Ctrl Pts',(0.721359423740628,-6.73119750259109,
38.2312716280651));
#57203=CARTESIAN_POINT('Ctrl Pts',(0.912796263558366,-6.70792383739874,
38.2403154502236));
#57204=CARTESIAN_POINT('Ctrl Pts',(1.10296273536256,-6.67650823442925,38.2493592723821));
#57205=CARTESIAN_POINT('Ctrl Pts',(1.28013370354561,-6.6472394956166,38.2577850622319));
#57206=CARTESIAN_POINT('Ctrl Pts',(1.45612444654051,-6.61091662712941,38.2662108520816));
#57207=CARTESIAN_POINT('Ctrl Pts',(1.63035802345081,-6.56766486015917,38.2746366419314));
#57208=CARTESIAN_POINT('Ctrl Pts',(1.80463202841247,-6.52440305732393,38.2830643868479));
#57209=CARTESIAN_POINT('Ctrl Pts',(1.97714773261153,-6.47420923027956,38.2914921317644));
#57210=CARTESIAN_POINT('Ctrl Pts',(2.14734168613832,-6.41725896960475,38.2999198766809));
#57211=CARTESIAN_POINT('Ctrl Pts',(2.31759817740396,-6.36028778256648,38.3083507183708));
#57212=CARTESIAN_POINT('Ctrl Pts',(2.48553090271921,-6.29655531686225,38.3167815600607));
#57213=CARTESIAN_POINT('Ctrl Pts',(2.65059440674841,-6.22628607525498,38.3252124017506));
#57214=CARTESIAN_POINT('Ctrl Pts',(2.81580958306958,-6.15595226518363,38.333650990308));
#57215=CARTESIAN_POINT('Ctrl Pts',(2.97814996550125,-6.07906980880263,38.3420895788653));
#57216=CARTESIAN_POINT('Ctrl Pts',(3.13709179542038,-5.995910612001,38.3505281674226));
#57217=CARTESIAN_POINT('Ctrl Pts',(3.29611696741091,-5.91270781019166,38.3589711808028));
#57218=CARTESIAN_POINT('Ctrl Pts',(3.4517397430259,-5.82322186435422,38.3674141941831));
#57219=CARTESIAN_POINT('Ctrl Pts',(3.60346308000267,-5.72776944639514,38.3758572075634));
#57220=CARTESIAN_POINT('Ctrl Pts',(3.7553458129201,-5.63221674901792,38.3843090909176));
#57221=CARTESIAN_POINT('Ctrl Pts',(3.90332064776322,-5.53068524126354,38.3927609742719));
#57222=CARTESIAN_POINT('Ctrl Pts',(4.04692063169226,-5.42353412460764,38.4012128576262));
#57223=CARTESIAN_POINT('Ctrl Pts',(4.08605616397931,-5.39433206015927,38.4035162628554));
#57224=CARTESIAN_POINT('Ctrl Pts',(4.12486695453269,-5.36471283553297,38.4058196680846));
#57225=CARTESIAN_POINT('Ctrl Pts',(4.16334399683875,-5.33468422345566,38.4081230733138));
#57226=CARTESIAN_POINT('Ctrl Pts',(4.30227906829076,-5.2262552197038,38.4164403386472));
#57227=CARTESIAN_POINT('Ctrl Pts',(4.43710985544817,-5.11229047568035,38.4247576039807));
#57228=CARTESIAN_POINT('Ctrl Pts',(4.56737751684648,-4.99313044277889,38.4330748693141));
#57229=CARTESIAN_POINT('Ctrl Pts',(4.69753530749622,-4.87407091219607,38.4413851196742));
#57230=CARTESIAN_POINT('Ctrl Pts',(4.82313738498907,-4.7498250565862,38.4496953700342));
#57231=CARTESIAN_POINT('Ctrl Pts',(4.94375725112098,-4.62077409553732,38.4580056203943));
#57232=CARTESIAN_POINT('Ctrl Pts',(5.0642974738146,-4.49180834484874,38.4663103836242));
#57233=CARTESIAN_POINT('Ctrl Pts',(5.1798618035169,-4.35804406405578,38.4746151468541));
#57234=CARTESIAN_POINT('Ctrl Pts',(5.29005979439378,-4.21990004286102,38.482919910084));
#57235=CARTESIAN_POINT('Ctrl Pts',(5.4002051956809,-4.08182194789,38.4912207100466));
#57236=CARTESIAN_POINT('Ctrl Pts',(5.50498914544803,-3.93936854931038,38.4995215100092));
#57237=CARTESIAN_POINT('Ctrl Pts',(5.60406063640611,-3.7929926685249,38.5078223099718));
#57238=CARTESIAN_POINT('Ctrl Pts',(5.70310297716192,-3.64665985650209,38.5161206675567));
#57239=CARTESIAN_POINT('Ctrl Pts',(5.79643601471079,-3.49640715050521,38.5244190251416));
#57240=CARTESIAN_POINT('Ctrl Pts',(5.88375121247998,-3.34271755756306,38.5327173827266));
#57241=CARTESIAN_POINT('Ctrl Pts',(5.97107529437035,-3.18901232705722,38.5410165846503));
#57242=CARTESIAN_POINT('Ctrl Pts',(6.05238013469612,-3.03186980957788,38.5493157865741));
#57243=CARTESIAN_POINT('Ctrl Pts',(6.12740215452806,-2.87179940745953,38.5576149884979));
#57244=CARTESIAN_POINT('Ctrl Pts',(6.20243178017074,-2.71171277723661,38.5659150318034));
#57245=CARTESIAN_POINT('Ctrl Pts',(6.271177167546,-2.54869798562367,38.574215075109));
#57246=CARTESIAN_POINT('Ctrl Pts',(6.33342212535606,-2.38328621488279,38.5825151184145));
#57247=CARTESIAN_POINT('Ctrl Pts',(6.39568372642389,-2.21783021580864,38.5908173810124));
#57248=CARTESIAN_POINT('Ctrl Pts',(6.45144131116843,-2.04997628585027,38.5991196436104));
#57249=CARTESIAN_POINT('Ctrl Pts',(6.50052791371773,-1.88027281078482,38.6074219062083));
#57250=CARTESIAN_POINT('Ctrl Pts',(6.54963579066124,-1.71049578533208,38.6157277670509));
#57251=CARTESIAN_POINT('Ctrl Pts',(6.59206682652152,-1.53886795115879,38.6240336278935));
#57252=CARTESIAN_POINT('Ctrl Pts',(6.62770466654014,-1.36595016494823,38.6323394887361));
#57253=CARTESIAN_POINT('Ctrl Pts',(6.663384633,-1.19282797771456,38.6406551676923));
#57254=CARTESIAN_POINT('Ctrl Pts',(6.69225528955528,-1.01841313301012,38.6489708466484));
#57255=CARTESIAN_POINT('Ctrl Pts',(6.71425171482333,-0.84327510931606,38.6572865256045));
#57256=CARTESIAN_POINT('Ctrl Pts',(6.7362620526552,-0.66802631221671,38.6656074641614));
#57257=CARTESIAN_POINT('Ctrl Pts',(6.75138945862924,-0.492053770065858,
38.6739284027182));
#57258=CARTESIAN_POINT('Ctrl Pts',(6.75962111215635,-0.31592945429344,38.682249341275));
#57259=CARTESIAN_POINT('Ctrl Pts',(6.76786500047033,-0.13954336323383,38.690582647324));
#57260=CARTESIAN_POINT('Ctrl Pts',(6.76919265107294,0.0369946045765517,
38.6989159533729));
#57261=CARTESIAN_POINT('Ctrl Pts',(6.76364336208099,0.213113750325444,38.7072492594219));
#57262=CARTESIAN_POINT('Ctrl Pts',(6.7595587577521,0.342747839696261,38.7133830646735));
#57263=CARTESIAN_POINT('Ctrl Pts',(6.75174943541119,0.472155075365261,38.719516869925));
#57264=CARTESIAN_POINT('Ctrl Pts',(6.7402488642125,0.601110845420475,38.7256506751766));
#57265=CARTESIAN_POINT('Ctrl Pts',(6.72511537711008,0.770802458923698,38.7337220884187));
#57266=CARTESIAN_POINT('Ctrl Pts',(6.70354158783764,0.940234380567401,38.7417935016607));
#57267=CARTESIAN_POINT('Ctrl Pts',(6.6755302075295,1.10886674057852,38.7498649149027));
#57268=CARTESIAN_POINT('Ctrl Pts',(6.64755399318921,1.27728739662912,38.7579261951539));
#57269=CARTESIAN_POINT('Ctrl Pts',(6.61315632898602,1.44491012506535,38.7659874754051));
#57270=CARTESIAN_POINT('Ctrl Pts',(6.57239186503604,1.61119650335027,38.7740487556564));
#57271=CARTESIAN_POINT('Ctrl Pts',(6.53166963765862,1.77731059023224,38.782101683514));
#57272=CARTESIAN_POINT('Ctrl Pts',(6.48459382625072,1.94209072320865,38.7901546113716));
#57273=CARTESIAN_POINT('Ctrl Pts',(6.43127066286263,2.10500514512495,38.7982075392292));
#57274=CARTESIAN_POINT('Ctrl Pts',(6.37799107172432,2.26778644388363,38.8062538867536));
#57275=CARTESIAN_POINT('Ctrl Pts',(6.31847440459218,2.42870471327798,38.814300234278));
#57276=CARTESIAN_POINT('Ctrl Pts',(6.25287758452075,2.58724001843625,38.8223465818024));
#57277=CARTESIAN_POINT('Ctrl Pts',(6.18732001674569,2.74568045809988,38.8303881144955));
#57278=CARTESIAN_POINT('Ctrl Pts',(6.11568968104562,2.90174042839282,38.8384296471887));
#57279=CARTESIAN_POINT('Ctrl Pts',(6.03819277572227,3.05491685700534,38.8464711798819));
#57280=CARTESIAN_POINT('Ctrl Pts',(5.95920601273738,3.21103806224841,38.8546673089301));
#57281=CARTESIAN_POINT('Ctrl Pts',(5.87412494248754,3.36416335100427,38.8628634379783));
#57282=CARTESIAN_POINT('Ctrl Pts',(5.78321880480353,3.51378275591518,38.8710595670266));
#57283=CARTESIAN_POINT('Ctrl Pts',(5.69405813743866,3.66052934896659,38.8790983238627));
#57284=CARTESIAN_POINT('Ctrl Pts',(5.5992942870446,3.80390315035634,38.8871370806988));
#57285=CARTESIAN_POINT('Ctrl Pts',(5.499226770835,3.94344949542043,38.8951758375349));
#57286=CARTESIAN_POINT('Ctrl Pts',(5.39914956914746,4.08300934709585,38.9032153724377));
#57287=CARTESIAN_POINT('Ctrl Pts',(5.29376789705891,4.21874070121749,38.9112549073404));
#57288=CARTESIAN_POINT('Ctrl Pts',(5.18342333543849,4.35021971004129,38.9192944422432));
#57289=CARTESIAN_POINT('Ctrl Pts',(5.07304624536894,4.48173747753329,38.9273363471187));
#57290=CARTESIAN_POINT('Ctrl Pts',(4.9577035936448,4.60900011865569,38.9353782519943));
#57291=CARTESIAN_POINT('Ctrl Pts',(4.83777568693623,4.73161868739322,38.9434201568698));
#57292=CARTESIAN_POINT('Ctrl Pts',(4.71380233822566,4.85837346030382,38.9517333335506));
#57293=CARTESIAN_POINT('Ctrl Pts',(4.58492928649313,4.98016505790788,38.9600465102315));
#57294=CARTESIAN_POINT('Ctrl Pts',(4.45161518447419,5.09660781788818,38.9683596869123));
#57295=CARTESIAN_POINT('Ctrl Pts',(4.32242741453802,5.20944644680479,38.9764155545228));
#57296=CARTESIAN_POINT('Ctrl Pts',(4.18906974925552,5.31726224411553,38.9844714221333));
#57297=CARTESIAN_POINT('Ctrl Pts',(4.05199001561559,5.41974777211556,38.9925272897439));
#57298=CARTESIAN_POINT('Ctrl Pts',(3.90834267302436,5.52714347066523,39.0009691209599));
#57299=CARTESIAN_POINT('Ctrl Pts',(3.76060823317765,5.62868530356234,39.0094109521758));
#57300=CARTESIAN_POINT('Ctrl Pts',(3.60933147526002,5.72407331379476,39.0178527833918));
#57301=CARTESIAN_POINT('Ctrl Pts',(3.45805471734239,5.81946132402718,39.0262946146078));
#57302=CARTESIAN_POINT('Ctrl Pts',(3.30323608358605,5.90869535548226,39.0347364458238));
#57303=CARTESIAN_POINT('Ctrl Pts',(3.14544408829463,5.9915332334397,39.0431782770398));
#57304=CARTESIAN_POINT('Ctrl Pts',(3.13002457736035,5.99962819137834,39.0440032169139));
#57305=CARTESIAN_POINT('Ctrl Pts',(3.114571560116,6.00766480946192,39.0448281567881));
#57306=CARTESIAN_POINT('Ctrl Pts',(3.09908550384713,6.01564277861016,39.0456530966623));
#57307=CARTESIAN_POINT('Ctrl Pts',(3.09908550384717,6.01564277861014,37.0457563580462));
#57308=CARTESIAN_POINT('Ctrl Pts',(2.93373232018327,6.10082796552481,37.0545058059455));
#57309=CARTESIAN_POINT('Ctrl Pts',(2.76486502144427,6.1791915818019,37.0632552538448));
#57310=CARTESIAN_POINT('Ctrl Pts',(2.59305716434354,6.25046746591378,37.072004701744));
#57311=CARTESIAN_POINT('Ctrl Pts',(2.42125069459281,6.32174277447226,37.0807540789915));
#57312=CARTESIAN_POINT('Ctrl Pts',(2.24650397871051,6.38593035557828,37.0895034562389));
#57313=CARTESIAN_POINT('Ctrl Pts',(2.06941053323759,6.44281220003542,37.0982528334863));
#57314=CARTESIAN_POINT('Ctrl Pts',(1.8923184589668,6.49969360406686,37.1070021429889));
#57315=CARTESIAN_POINT('Ctrl Pts',(1.71287996431511,6.54926929700879,37.1157514524915));
#57316=CARTESIAN_POINT('Ctrl Pts',(1.53170449173519,6.59137090065475,37.1245007619941));
#57317=CARTESIAN_POINT('Ctrl Pts',(1.35053036178182,6.63347219230081,37.1332500066587));
#57318=CARTESIAN_POINT('Ctrl Pts',(1.16761955878853,6.66809944062453,37.1419992513233));
#57319=CARTESIAN_POINT('Ctrl Pts',(0.983593309310534,6.69513503985391,37.1507484959879));
#57320=CARTESIAN_POINT('Ctrl Pts',(0.799568362460071,6.72217044771213,37.159497678721));
#57321=CARTESIAN_POINT('Ctrl Pts',(0.614428268438726,6.74161427235976,37.1682468614542));
#57322=CARTESIAN_POINT('Ctrl Pts',(0.428801816330442,6.75340047696801,37.1769960441874));
#57323=CARTESIAN_POINT('Ctrl Pts',(0.243176616522973,6.76518660206241,37.1857451678955));
#57324=CARTESIAN_POINT('Ctrl Pts',(0.0570653511656652,6.76931519233997,
37.1944942916036));
#57325=CARTESIAN_POINT('Ctrl Pts',(-0.12889990079981,6.76577222610796,37.2032434153118));
#57326=CARTESIAN_POINT('Ctrl Pts',(-0.314863959941719,6.76222928260134,
37.211992482901));
#57327=CARTESIAN_POINT('Ctrl Pts',(-0.500681721080297,6.75101488651279,
37.2207415504903));
#57328=CARTESIAN_POINT('Ctrl Pts',(-0.685722110172835,6.73216712415996,
37.2294906180796));
#57329=CARTESIAN_POINT('Ctrl Pts',(-0.870761373827337,6.71331947644149,
37.2382396324559));
#57330=CARTESIAN_POINT('Ctrl Pts',(-1.05502298984334,6.68683858439998,37.2469886468323));
#57331=CARTESIAN_POINT('Ctrl Pts',(-1.23788117676069,6.65281438131424,37.2557376612086));
#57332=CARTESIAN_POINT('Ctrl Pts',(-1.43009641451797,6.61704912302376,37.2649343720962));
#57333=CARTESIAN_POINT('Ctrl Pts',(-1.62076048992694,6.57294837083165,37.2741310829837));
#57334=CARTESIAN_POINT('Ctrl Pts',(-1.80915798961124,6.52067760042051,37.2833277938712));
#57335=CARTESIAN_POINT('Ctrl Pts',(-1.98840443003011,6.4709457857741,37.2920777915777));
#57336=CARTESIAN_POINT('Ctrl Pts',(-2.16559895952196,6.41381888474474,37.3008277892843));
#57337=CARTESIAN_POINT('Ctrl Pts',(-2.34013966242332,6.34949095285231,37.3095777869908));
#57338=CARTESIAN_POINT('Ctrl Pts',(-2.51467682554016,6.28516432556684,37.3183276072424));
#57339=CARTESIAN_POINT('Ctrl Pts',(-2.68656000078835,6.21363705879664,37.3270774274939));
#57340=CARTESIAN_POINT('Ctrl Pts',(-2.85520533840873,6.13515211510866,37.3358272477455));
#57341=CARTESIAN_POINT('Ctrl Pts',(-3.02384747998311,6.05666865881129,37.3445769021768));
#57342=CARTESIAN_POINT('Ctrl Pts',(-3.1892516468452,5.97122791039853,37.353326556608));
#57343=CARTESIAN_POINT('Ctrl Pts',(-3.3508560182914,5.87912008251918,37.3620762110393));
#57344=CARTESIAN_POINT('Ctrl Pts',(-3.51245754191397,5.78701387778187,37.3708257112824));
#57345=CARTESIAN_POINT('Ctrl Pts',(-3.67025915510912,5.68824097060998,37.3795752115256));
#57346=CARTESIAN_POINT('Ctrl Pts',(-3.82372487928807,5.58313684656873,37.3883247117687));
#57347=CARTESIAN_POINT('Ctrl Pts',(-3.97718810300773,5.47803443501791,37.3970740694538));
#57348=CARTESIAN_POINT('Ctrl Pts',(-4.12631534263003,5.36660117496393,37.4058234271389));
#57349=CARTESIAN_POINT('Ctrl Pts',(-4.27060009886204,5.24921554097367,37.414572784824));
#57350=CARTESIAN_POINT('Ctrl Pts',(-4.41488269594185,5.13183166360315,37.4233220115792));
#57351=CARTESIAN_POINT('Ctrl Pts',(-4.55432273235054,5.00849577139502,37.4320712383344));
#57352=CARTESIAN_POINT('Ctrl Pts',(-4.68844662480167,4.87962675277381,37.4408204650896));
#57353=CARTESIAN_POINT('Ctrl Pts',(-4.82256868835112,4.75075949139928,37.4495695725411));
#57354=CARTESIAN_POINT('Ctrl Pts',(-4.95137454637811,4.6163594531258,37.4583186799926));
#57355=CARTESIAN_POINT('Ctrl Pts',(-5.07442674461022,4.47688309134654,37.467067787444));
#57356=CARTESIAN_POINT('Ctrl Pts',(-5.19747742838477,4.33740844616425,37.4758167872164));
#57357=CARTESIAN_POINT('Ctrl Pts',(-5.3147744045086,4.19285781736114,37.4845657869888));
#57358=CARTESIAN_POINT('Ctrl Pts',(-5.42591931531081,4.04372211999502,37.4933147867611));
#57359=CARTESIAN_POINT('Ctrl Pts',(-5.53707636462918,3.89457013500892,37.5020647420417));
#57360=CARTESIAN_POINT('Ctrl Pts',(-5.64207983273414,3.74083230916506,37.5108146973223));
#57361=CARTESIAN_POINT('Ctrl Pts',(-5.74057303468697,3.58303087251908,37.5195646526029));
#57362=CARTESIAN_POINT('Ctrl Pts',(-5.83906243363723,3.42523552887503,37.5283142700317));
#57363=CARTESIAN_POINT('Ctrl Pts',(-5.93104191768392,3.26337713157055,37.5370638874605));
#57364=CARTESIAN_POINT('Ctrl Pts',(-6.01619906699629,3.09800545291209,37.5458135048893));
#57365=CARTESIAN_POINT('Ctrl Pts',(-6.10135338095361,2.93263928039642,37.5545628309947));
#57366=CARTESIAN_POINT('Ctrl Pts',(-6.17968568352821,2.76376031540264,37.5633121571001));
#57367=CARTESIAN_POINT('Ctrl Pts',(-6.25092992694873,2.59194213831574,37.5720614832055));
#57368=CARTESIAN_POINT('Ctrl Pts',(-6.32217217691096,2.42012876880842,37.5808105644993));
#57369=CARTESIAN_POINT('Ctrl Pts',(-6.38632665483847,2.24537661647681,37.5895596457931));
#57370=CARTESIAN_POINT('Ctrl Pts',(-6.4431754786935,2.06827917621456,37.5983087270869));
#57371=CARTESIAN_POINT('Ctrl Pts',(-6.50002944235933,1.89116572423431,37.6070585994019));
#57372=CARTESIAN_POINT('Ctrl Pts',(-6.54957634250394,1.71170683289215,37.6158084717168));
#57373=CARTESIAN_POINT('Ctrl Pts',(-6.59164787708389,1.5305120922539,37.6245583440318));
#57374=CARTESIAN_POINT('Ctrl Pts',(-6.63371649075,1.34932993148071,37.6333076088666));
#57375=CARTESIAN_POINT('Ctrl Pts',(-6.66831071257113,1.16641244174061,37.6420568737014));
#57376=CARTESIAN_POINT('Ctrl Pts',(-6.69531304840322,0.982380875160746,
37.6508061385361));
#57377=CARTESIAN_POINT('Ctrl Pts',(-6.72231677033035,0.798339861796548,
37.6595558524918));
#57378=CARTESIAN_POINT('Ctrl Pts',(-6.74172778477884,0.613184940730828,
37.6683055664475));
#57379=CARTESIAN_POINT('Ctrl Pts',(-6.75348015835514,0.427545027691196,
37.6770552804031));
#57380=CARTESIAN_POINT('Ctrl Pts',(-6.76249038365209,0.285219953548953,
37.6837634482053));
#57381=CARTESIAN_POINT('Ctrl Pts',(-6.7669999999999,0.142609995760929,37.6904716160076));
#57382=CARTESIAN_POINT('Ctrl Pts',(-6.767,5.0320187747232E-12,37.6971797838098));
#57383=CARTESIAN_POINT('',(-6.76702302174747,7.20323096178367E-5,37.3028600550208));
#57384=CARTESIAN_POINT('Ctrl Pts',(3.09908550384717,6.01564277861014,36.651532120892));
#57385=CARTESIAN_POINT('Ctrl Pts',(2.9359801966848,6.09966992444147,36.6601504462137));
#57386=CARTESIAN_POINT('Ctrl Pts',(2.76938649977694,6.17709521451719,36.6687687715353));
#57387=CARTESIAN_POINT('Ctrl Pts',(2.59985511119712,6.2476429476069,36.6773870968569));
#57388=CARTESIAN_POINT('Ctrl Pts',(2.53580837858245,6.27429495485829,36.6806429870026));
#57389=CARTESIAN_POINT('Ctrl Pts',(2.47134262033588,6.29996584594057,36.6838988771483));
#57390=CARTESIAN_POINT('Ctrl Pts',(2.40648839577786,6.32464248799776,36.687154767294));
#57391=CARTESIAN_POINT('Ctrl Pts',(2.2386547028249,6.38850219789888,36.6955805571438));
#57392=CARTESIAN_POINT('Ctrl Pts',(2.06829126929335,6.44567205805835,36.7040063469937));
#57393=CARTESIAN_POINT('Ctrl Pts',(1.89595968604162,6.49596997136725,36.7124321368435));
#57394=CARTESIAN_POINT('Ctrl Pts',(1.72358811606418,6.54627955548439,36.7208598817601));
#57395=CARTESIAN_POINT('Ctrl Pts',(1.54924780404718,6.58971392062384,36.7292876266766));
#57396=CARTESIAN_POINT('Ctrl Pts',(1.37351402332003,6.62614127737579,36.7377153715932));
#57397=CARTESIAN_POINT('Ctrl Pts',(1.19771566924371,6.66258201935405,36.7461462132833));
#57398=CARTESIAN_POINT('Ctrl Pts',(1.02052314996444,6.69201055192431,36.7545770549733));
#57399=CARTESIAN_POINT('Ctrl Pts',(0.842520801187833,6.71434640896386,36.7630078966634));
#57400=CARTESIAN_POINT('Ctrl Pts',(0.66435489097534,6.73670278980476,36.7714464852207));
#57401=CARTESIAN_POINT('Ctrl Pts',(0.485377993719001,6.75195343293511,36.7798850737781));
#57402=CARTESIAN_POINT('Ctrl Pts',(0.306179548867013,6.76006975436316,36.7883236623354));
#57403=CARTESIAN_POINT('Ctrl Pts',(0.126887140270615,6.76819033163145,36.7967666757157));
#57404=CARTESIAN_POINT('Ctrl Pts',(-0.0526267164854606,6.76916911916001,
36.8052096890959));
#57405=CARTESIAN_POINT('Ctrl Pts',(-0.231773143031693,6.76302966207965,
36.8136527024761));
#57406=CARTESIAN_POINT('Ctrl Pts',(-0.411107775386743,6.75688375507167,
36.8221045858305));
#57407=CARTESIAN_POINT('Ctrl Pts',(-0.590073875790865,6.74360468431347,
36.8305564691848));
#57408=CARTESIAN_POINT('Ctrl Pts',(-0.768087167234132,6.72326788872274,
36.8390083525391));
#57409=CARTESIAN_POINT('Ctrl Pts',(-0.816601413007557,6.71772546943745,
36.8413117577678));
#57410=CARTESIAN_POINT('Ctrl Pts',(-0.865044943110747,6.71165914262081,
36.8436151629966));
#57411=CARTESIAN_POINT('Ctrl Pts',(-0.913406063142955,6.70507109312151,
36.8459185682254));
#57412=CARTESIAN_POINT('Ctrl Pts',(-1.0880311191712,6.68128259293446,36.8542358335588));
#57413=CARTESIAN_POINT('Ctrl Pts',(-1.26189497854287,6.65064499429759,36.8625530988922));
#57414=CARTESIAN_POINT('Ctrl Pts',(-1.43442980892838,6.61322161455804,36.8708703642256));
#57415=CARTESIAN_POINT('Ctrl Pts',(-1.60681911946091,6.5758297985596,36.8791806145857));
#57416=CARTESIAN_POINT('Ctrl Pts',(-1.77788129611543,6.53166367777585,36.8874908649458));
#57417=CARTESIAN_POINT('Ctrl Pts',(-1.94705594194545,6.48083807535221,36.895801115306));
#57418=CARTESIAN_POINT('Ctrl Pts',(-2.11611888436437,6.43004603229046,36.9041058785358));
#57419=CARTESIAN_POINT('Ctrl Pts',(-2.28329644737229,6.37260336920495,36.9124106417657));
#57420=CARTESIAN_POINT('Ctrl Pts',(-2.44804048398312,6.30867551779133,36.9207154049956));
#57421=CARTESIAN_POINT('Ctrl Pts',(-2.61270590009155,6.24477817455208,36.9290162049581));
#57422=CARTESIAN_POINT('Ctrl Pts',(-2.77493978065457,6.17440193642565,36.9373170049207));
#57423=CARTESIAN_POINT('Ctrl Pts',(-2.9342109354109,6.09776148980223,36.9456178048833));
#57424=CARTESIAN_POINT('Ctrl Pts',(-3.09343522717903,6.02114359340362,36.9539161624683));
#57425=CARTESIAN_POINT('Ctrl Pts',(-3.24969821770864,5.93826531308279,36.9622145200533));
#57426=CARTESIAN_POINT('Ctrl Pts',(-3.40249022912408,5.84938879206325,36.9705128776383));
#57427=CARTESIAN_POINT('Ctrl Pts',(-3.55529778677459,5.76050322806251,36.9788120795621));
#57428=CARTESIAN_POINT('Ctrl Pts',(-3.70463335522753,5.66561837228997,36.9871112814859));
#57429=CARTESIAN_POINT('Ctrl Pts',(-3.85001282541519,5.56504180075394,36.9954104834097));
#57430=CARTESIAN_POINT('Ctrl Pts',(-3.99540703432518,5.46445503266016,37.0037105267152));
#57431=CARTESIAN_POINT('Ctrl Pts',(-4.13684405903616,5.35817559621645,37.0120105700207));
#57432=CARTESIAN_POINT('Ctrl Pts',(-4.2738697816766,5.24655373452628,37.0203106133263));
#57433=CARTESIAN_POINT('Ctrl Pts',(-4.41093214269751,5.13490202702205,37.0286128759242));
#57434=CARTESIAN_POINT('Ctrl Pts',(-4.54358058100991,5.01790526692851,37.0369151385221));
#57435=CARTESIAN_POINT('Ctrl Pts',(-4.67139486096394,4.89595333443444,37.04521740112));
#57436=CARTESIAN_POINT('Ctrl Pts',(-4.79926453630584,4.77394854732503,37.0535232619627));
#57437=CARTESIAN_POINT('Ctrl Pts',(-4.92229562607523,4.64698454763409,37.0618291228053));
#57438=CARTESIAN_POINT('Ctrl Pts',(-5.04010535577153,4.51548746014461,37.0701349836479));
#57439=CARTESIAN_POINT('Ctrl Pts',(-5.15805434487977,4.38383493382063,37.0784506626041));
#57440=CARTESIAN_POINT('Ctrl Pts',(-5.27076941002723,4.24763887311402,37.0867663415602));
#57441=CARTESIAN_POINT('Ctrl Pts',(-5.37790788531592,4.10735873488752,37.0950820205163));
#57442=CARTESIAN_POINT('Ctrl Pts',(-5.48511412483643,3.96698987059153,37.1034029590731));
#57443=CARTESIAN_POINT('Ctrl Pts',(-5.5867365405815,3.82253206145575,37.1117238976299));
#57444=CARTESIAN_POINT('Ctrl Pts',(-5.68247623606807,3.67447313590965,37.1200448361867));
#57445=CARTESIAN_POINT('Ctrl Pts',(-5.77835823039775,3.52619414893853,37.1283781422357));
#57446=CARTESIAN_POINT('Ctrl Pts',(-5.86833985364039,3.37430364820411,37.1367114482846));
#57447=CARTESIAN_POINT('Ctrl Pts',(-5.95216788904884,3.21931458863154,37.1450447543335));
#57448=CARTESIAN_POINT('Ctrl Pts',(-6.01387027232919,3.10523349020892,37.1511785595852));
#57449=CARTESIAN_POINT('Ctrl Pts',(-6.07223971776672,2.98947414502033,37.1573123648368));
#57450=CARTESIAN_POINT('Ctrl Pts',(-6.12719212312746,2.87224749739378,37.1634461700884));
#57451=CARTESIAN_POINT('Ctrl Pts',(-6.20505480737424,2.70614773543547,37.1721372280759));
#57452=CARTESIAN_POINT('Ctrl Pts',(-6.27626917716232,2.53664610066104,37.1808282860633));
#57453=CARTESIAN_POINT('Ctrl Pts',(-6.34053998751404,2.36428459935251,37.1895193440508));
#57454=CARTESIAN_POINT('Ctrl Pts',(-6.40466935798327,2.19230241161351,37.1981912757472));
#57455=CARTESIAN_POINT('Ctrl Pts',(-6.46188552719803,2.01747317717048,37.2068632074437));
#57456=CARTESIAN_POINT('Ctrl Pts',(-6.51193941222511,1.84036248916058,37.2155351391402));
#57457=CARTESIAN_POINT('Ctrl Pts',(-6.56184040138734,1.66379280794372,37.2241805813345));
#57458=CARTESIAN_POINT('Ctrl Pts',(-6.60462265583713,1.48495585292723,37.2328260235288));
#57459=CARTESIAN_POINT('Ctrl Pts',(-6.64008566687456,1.30443525579736,37.2414714657231));
#57460=CARTESIAN_POINT('Ctrl Pts',(-6.67548350019386,1.12424643874622,37.2501010183981));
#57461=CARTESIAN_POINT('Ctrl Pts',(-6.70358884369664,0.942380433296196,
37.2587305710732));
#57462=CARTESIAN_POINT('Ctrl Pts',(-6.72425049383304,0.759436828305091,
37.2673601237483));
#57463=CARTESIAN_POINT('Ctrl Pts',(-6.74486050175704,0.576950476846289,
37.2759681075173));
#57464=CARTESIAN_POINT('Ctrl Pts',(-6.75806388383551,0.393392188113838,
37.2845760912862));
#57465=CARTESIAN_POINT('Ctrl Pts',(-6.76376022331584,0.209372016971024,
37.2931840750552));
#57466=CARTESIAN_POINT('Ctrl Pts',(-6.76588579776919,0.14070536252861,37.2963961221));
#57467=CARTESIAN_POINT('Ctrl Pts',(-6.76696660310004,0.0719745239661936,
37.2996081691449));
#57468=CARTESIAN_POINT('Ctrl Pts',(-6.76699923788744,0.00321160876916168,
37.3028202161897));
#57469=CARTESIAN_POINT('Ctrl Pts',(-6.767,4.91316042210608E-12,37.3028202161897));
#57470=CARTESIAN_POINT('Ctrl Pts',(-6.76700000000014,-0.186007249555132,
37.3115697280025));
#57471=CARTESIAN_POINT('Ctrl Pts',(-6.75932637294273,-0.372014355811356,
37.3203192398152));
#57472=CARTESIAN_POINT('Ctrl Pts',(-6.74400518263401,-0.557389537581778,
37.3290687516279));
#57473=CARTESIAN_POINT('Ctrl Pts',(-6.7286840570378,-0.742763936378232,
37.3378182264851));
#57474=CARTESIAN_POINT('Ctrl Pts',(-6.70571545643626,-0.927506130400532,
37.3465677013423));
#57475=CARTESIAN_POINT('Ctrl Pts',(-6.67517739401648,-1.11098864009104,
37.3553171761995));
#57476=CARTESIAN_POINT('Ctrl Pts',(-6.64463945804472,-1.29447039004117,
37.3640666148281));
#57477=CARTESIAN_POINT('Ctrl Pts',(-6.60653217002815,-1.47669218338871,
37.3728160534566));
#57478=CARTESIAN_POINT('Ctrl Pts',(-6.56098496085578,-1.65703510627393,
37.3815654920851));
#57479=CARTESIAN_POINT('Ctrl Pts',(-6.5154379364966,-1.83737729739641,37.3903148952118));
#57480=CARTESIAN_POINT('Ctrl Pts',(-6.46245112157005,-2.01584035544606,
37.3990642983384));
#57481=CARTESIAN_POINT('Ctrl Pts',(-6.40220448361828,-2.19181813797084,
37.407813701465));
#57482=CARTESIAN_POINT('Ctrl Pts',(-6.34195808512091,-2.36779522105988,
37.4165630698166));
#57483=CARTESIAN_POINT('Ctrl Pts',(-6.27445201416478,-2.54128677725439,
37.4253124381681));
#57484=CARTESIAN_POINT('Ctrl Pts',(-6.19991555052854,-2.71170355428363,
37.4340618065196));
#57485=CARTESIAN_POINT('Ctrl Pts',(-6.12537937695241,-2.88211966813262,
37.4428111408228));
#57486=CARTESIAN_POINT('Ctrl Pts',(-6.0438129802846,-3.04946076419655,37.451560475126));
#57487=CARTESIAN_POINT('Ctrl Pts',(-5.95549339308974,-3.21315848424326,
37.4603098094292));
#57488=CARTESIAN_POINT('Ctrl Pts',(-5.86717414225799,-3.376855580851,37.4690591104108));
#57489=CARTESIAN_POINT('Ctrl Pts',(-5.77210188844054,-3.53690907700021,
37.4778084113923));
#57490=CARTESIAN_POINT('Ctrl Pts',(-5.67059953311356,-3.69277537024016,
37.4865577123739));
#57491=CARTESIAN_POINT('Ctrl Pts',(-5.56909755592688,-3.84864108281055,
37.4953069807605));
#57492=CARTESIAN_POINT('Ctrl Pts',(-5.46116568154942,-4.00031938354862,
37.5040562491471));
#57493=CARTESIAN_POINT('Ctrl Pts',(-5.34717048488348,-4.14729511918202,
37.5128055175337));
#57494=CARTESIAN_POINT('Ctrl Pts',(-5.23317570343271,-4.2942703194722,37.5215547540521));
#57495=CARTESIAN_POINT('Ctrl Pts',(-5.11311781951508,-4.43654276249601,
37.5303039905704));
#57496=CARTESIAN_POINT('Ctrl Pts',(-4.987404589292,-4.57362924412431,37.5390532270888));
#57497=CARTESIAN_POINT('Ctrl Pts',(-4.86169180652702,-4.71071523781306,
37.5478024324655));
#57498=CARTESIAN_POINT('Ctrl Pts',(-4.73032391141542,-4.84261509584519,
37.5565516378422));
#57499=CARTESIAN_POINT('Ctrl Pts',(-4.59374706947305,-4.96888084599619,
37.5653008432189));
#57500=CARTESIAN_POINT('Ctrl Pts',(-4.45717070231523,-5.09514615720727,
37.5740500181806));
#57501=CARTESIAN_POINT('Ctrl Pts',(-4.31538563497419,-5.21577720520535,
37.5827991931423));
#57502=CARTESIAN_POINT('Ctrl Pts',(-4.16887340952139,-5.33036429293397,
37.591548368104));
#57503=CARTESIAN_POINT('Ctrl Pts',(-4.02236168122617,-5.44495099183609,
37.6002975133773));
#57504=CARTESIAN_POINT('Ctrl Pts',(-3.87112305263311,-5.55349359497838,
37.6090466586505));
#57505=CARTESIAN_POINT('Ctrl Pts',(-3.71567116929123,-5.65562346357127,
37.6177958039237));
#57506=CARTESIAN_POINT('Ctrl Pts',(-3.5602198005346,-5.75775299408835,37.6265449202351));
#57507=CARTESIAN_POINT('Ctrl Pts',(-3.40055544442255,-5.85346967519779,
37.6352940365465));
#57508=CARTESIAN_POINT('Ctrl Pts',(-3.23722035887036,-5.94244843041277,
37.6440431528578));
#57509=CARTESIAN_POINT('Ctrl Pts',(-3.07388580043715,-6.03142689847335,
37.6527922409338));
#57510=CARTESIAN_POINT('Ctrl Pts',(-2.9068807878948,-6.11366734707778,37.6615413290098));
#57511=CARTESIAN_POINT('Ctrl Pts',(-2.73677250610683,-6.188890470013,37.6702904170858));
#57512=CARTESIAN_POINT('Ctrl Pts',(-2.56666475917226,-6.26411335643215,
37.679039477653));
#57513=CARTESIAN_POINT('Ctrl Pts',(-2.39345402457385,-6.33231884545146,
37.6877885382202));
#57514=CARTESIAN_POINT('Ctrl Pts',(-2.21772855944357,-6.39327529804781,
37.6965375987873));
#57515=CARTESIAN_POINT('Ctrl Pts',(-2.04200363223892,-6.45423156404607,
37.7052866325721));
#57516=CARTESIAN_POINT('Ctrl Pts',(-1.86376426061344,-6.50793874412364,
37.7140356663569));
#57517=CARTESIAN_POINT('Ctrl Pts',(-1.68361577622007,-6.5542144394323,37.7227847001417));
#57518=CARTESIAN_POINT('Ctrl Pts',(-1.50346782833494,-6.60048999692525,
37.7315337078706));
#57519=CARTESIAN_POINT('Ctrl Pts',(-1.32141105657625,-6.63933404265116,
37.7402827155996));
#57520=CARTESIAN_POINT('Ctrl Pts',(-1.1380637534673,-6.67061465631496,37.7490317233285));
#57521=CARTESIAN_POINT('Ctrl Pts',(-0.954716981172442,-6.70189517941735,
37.7577807057279));
#57522=CARTESIAN_POINT('Ctrl Pts',(-0.770079967445198,-6.72561226608969,
37.7665296881273));
#57523=CARTESIAN_POINT('Ctrl Pts',(-0.584779764076472,-6.74168536995955,
37.7752786705267));
#57524=CARTESIAN_POINT('Ctrl Pts',(-0.391489587596343,-6.75845153117853,
37.7844049009423));
#57525=CARTESIAN_POINT('Ctrl Pts',(-0.197478091808605,-6.76689985146384,
37.793531131358));
#57526=CARTESIAN_POINT('Ctrl Pts',(-0.00346214753437534,-6.76699911434415,
37.8026573617736));
#57527=CARTESIAN_POINT('Ctrl Pts',(0.184490798481368,-6.76709527525944,
37.8114983974887));
#57528=CARTESIAN_POINT('Ctrl Pts',(0.372447602151582,-6.75935633790781,
37.8203394332038));
#57529=CARTESIAN_POINT('Ctrl Pts',(0.559756448191097,-6.74380914014539,
37.8291804689189));
#57530=CARTESIAN_POINT('Ctrl Pts',(0.745136131040202,-6.72842206873189,
37.8379304475323));
#57531=CARTESIAN_POINT('Ctrl Pts',(0.929880851941859,-6.70538686355767,
37.8466804261456));
#57532=CARTESIAN_POINT('Ctrl Pts',(1.11336305057141,-6.67478177303366,37.8554304047589));
#57533=CARTESIAN_POINT('Ctrl Pts',(1.29684337089809,-6.64417699581322,37.8641802937988));
#57534=CARTESIAN_POINT('Ctrl Pts',(1.47906091204882,-6.60600253548129,37.8729301828389));
#57535=CARTESIAN_POINT('Ctrl Pts',(1.6593967109492,-6.56038806441288,37.8816800718788));
#57536=CARTESIAN_POINT('Ctrl Pts',(1.83973072368859,-6.51477404513934,37.8904298742543));
#57537=CARTESIAN_POINT('Ctrl Pts',(2.01818275356735,-6.46172023288755,37.8991796766298));
#57538=CARTESIAN_POINT('Ctrl Pts',(2.19414664033026,-6.40140683918211,37.9079294790053));
#57539=CARTESIAN_POINT('Ctrl Pts',(2.37010884270963,-6.34109402281608,37.9166791976248));
#57540=CARTESIAN_POINT('Ctrl Pts',(2.54358267847514,-6.2735218569991,37.9254289162444));
#57541=CARTESIAN_POINT('Ctrl Pts',(2.71397890841454,-6.19891986435387,37.9341786348639));
#57542=CARTESIAN_POINT('Ctrl Pts',(2.88437356388664,-6.12431856103374,37.9429282726357));
#57543=CARTESIAN_POINT('Ctrl Pts',(3.05169040786905,-6.04268767582692,37.9516779104076));
#57544=CARTESIAN_POINT('Ctrl Pts',(3.21536112511797,-5.95430447954084,37.9604275481794));
#57545=CARTESIAN_POINT('Ctrl Pts',(3.37903038442591,-5.86592207055188,37.9691771080115));
#57546=CARTESIAN_POINT('Ctrl Pts',(3.53905332979726,-5.77078760703528,37.9779266678435));
#57547=CARTESIAN_POINT('Ctrl Pts',(3.6948864304165,-5.66922422085456,37.9866762276756));
#57548=CARTESIAN_POINT('Ctrl Pts',(3.85071819468506,-5.56766170563322,37.9954257124756));
#57549=CARTESIAN_POINT('Ctrl Pts',(4.00235994598994,-5.4596705345642,38.0041751972756));
#57550=CARTESIAN_POINT('Ctrl Pts',(4.14929662974076,-5.34561750206858,38.0129246820756));
#57551=CARTESIAN_POINT('Ctrl Pts',(4.29623210224831,-5.23156540974642,38.0216740947509));
#57552=CARTESIAN_POINT('Ctrl Pts',(4.43846235841914,-5.11145173172363,38.0304235074263));
#57553=CARTESIAN_POINT('Ctrl Pts',(4.57550431797236,-4.98568443006738,38.0391729201016));
#57554=CARTESIAN_POINT('Ctrl Pts',(4.71254519337315,-4.85991812336863,38.0479222635595));
#57555=CARTESIAN_POINT('Ctrl Pts',(4.84439764314818,-4.72849847631271,38.0566716070175));
#57556=CARTESIAN_POINT('Ctrl Pts',(4.97061384196533,-4.59187184425509,38.0654209504754));
#57557=CARTESIAN_POINT('Ctrl Pts',(5.09682908420066,-4.45524624767908,38.0741702276227));
#57558=CARTESIAN_POINT('Ctrl Pts',(5.21740796650043,-4.31341395557047,38.0829195047701));
#57559=CARTESIAN_POINT('Ctrl Pts',(5.33194095942135,-4.16685668163004,38.0916687819174));
#57560=CARTESIAN_POINT('Ctrl Pts',(5.44647312235024,-4.02030046975362,38.100417995661));
#57561=CARTESIAN_POINT('Ctrl Pts',(5.55495930712187,-3.86901957035693,38.1091672094045));
#57562=CARTESIAN_POINT('Ctrl Pts',(5.657031060797,-3.71352778058519,38.1179164231481));
#57563=CARTESIAN_POINT('Ctrl Pts',(5.75910210868641,-3.55803706597755,38.1266655763943));
#57564=CARTESIAN_POINT('Ctrl Pts',(5.85475865698456,-3.3983357588106,38.1354147296405));
#57565=CARTESIAN_POINT('Ctrl Pts',(5.94367583068971,-3.2349662470689,38.1441638828866));
#57566=CARTESIAN_POINT('Ctrl Pts',(6.03259241909987,-3.07159781070276,38.1529129785418));
#57567=CARTESIAN_POINT('Ctrl Pts',(6.1147695847088,-2.90456146976017,38.1616620741969));
#57568=CARTESIAN_POINT('Ctrl Pts',(6.18992823574302,-2.73442451648447,38.170411169852));
#57569=CARTESIAN_POINT('Ctrl Pts',(6.26508641700858,-2.56428862662605,38.1791602108221));
#57570=CARTESIAN_POINT('Ctrl Pts',(6.33322605570226,-2.39105242531465,38.1879092517923));
#57571=CARTESIAN_POINT('Ctrl Pts',(6.39411573747703,-2.21530425353914,38.1966582927624));
#57572=CARTESIAN_POINT('Ctrl Pts',(6.45500505889067,-2.03955712188745,38.2054072819534));
#57573=CARTESIAN_POINT('Ctrl Pts',(6.50864441544877,-1.86129832025755,38.2141562711444));
#57574=CARTESIAN_POINT('Ctrl Pts',(6.5548516404986,-1.6811332401249,38.2229052603354));
#57575=CARTESIAN_POINT('Ctrl Pts',(6.60199852639071,-1.49730435913071,38.2318321672123));
#57576=CARTESIAN_POINT('Ctrl Pts',(6.64140767440978,-1.31149113173816,38.2407590740892));
#57577=CARTESIAN_POINT('Ctrl Pts',(6.67293975269576,-1.12435050446587,38.249685980966));
#57578=CARTESIAN_POINT('Ctrl Pts',(6.70384664831484,-0.940920291565358,
38.25843589515));
#57579=CARTESIAN_POINT('Ctrl Pts',(6.72718585889647,-0.756215114279608,
38.267185809334));
#57580=CARTESIAN_POINT('Ctrl Pts',(6.7428781045185,-0.57086238937686,38.275935723518));
#57581=CARTESIAN_POINT('Ctrl Pts',(6.75857004154112,-0.385513309569975,
38.2846854656286));
#57582=CARTESIAN_POINT('Ctrl Pts',(6.7666152903555,-0.199516993261237,38.2934352077392));
#57583=CARTESIAN_POINT('Ctrl Pts',(6.76698652348896,-0.0135052182072312,
38.3021849498497));
#57584=CARTESIAN_POINT('Ctrl Pts',(6.76735774981529,0.172503146035705,38.3109345315204));
#57585=CARTESIAN_POINT('Ctrl Pts',(6.76005524147496,0.358526681830274,38.319684113191));
#57586=CARTESIAN_POINT('Ctrl Pts',(6.74510380214907,0.543933542111663,38.3284336948617));
#57587=CARTESIAN_POINT('Ctrl Pts',(6.73015261711013,0.729337249081553,38.3371831277236));
#57588=CARTESIAN_POINT('Ctrl Pts',(6.70755278444648,0.914124015851531,38.3459325605855));
#57589=CARTESIAN_POINT('Ctrl Pts',(6.6773810640834,1.09766621749077,38.3546819934475));
#57590=CARTESIAN_POINT('Ctrl Pts',(6.64720981677314,1.2812055414301,38.3634312891298));
#57591=CARTESIAN_POINT('Ctrl Pts',(6.60946696581592,1.46350005650307,38.3721805848122));
#57592=CARTESIAN_POINT('Ctrl Pts',(6.56428070011073,1.64393062206219,38.3809298804945));
#57593=CARTESIAN_POINT('Ctrl Pts',(6.5190950828283,1.82435859844333,38.3896790506245));
#57594=CARTESIAN_POINT('Ctrl Pts',(6.46646633415761,2.0029224008624,38.3984282207545));
#57595=CARTESIAN_POINT('Ctrl Pts',(6.40657319597303,2.17901557696127,38.4071773908845));
#57596=CARTESIAN_POINT('Ctrl Pts',(6.34668083768422,2.3551064600709,38.4159264470875));
#57597=CARTESIAN_POINT('Ctrl Pts',(6.2795243714403,2.5287265099617,38.4246755032906));
#57598=CARTESIAN_POINT('Ctrl Pts',(6.20533187335299,2.6992860799755,38.4334245594937));
#57599=CARTESIAN_POINT('Ctrl Pts',(6.12831449784421,2.87633970115039,38.4425067357825));
#57600=CARTESIAN_POINT('Ctrl Pts',(6.04371489463325,3.05009490562009,38.4515889120714));
#57601=CARTESIAN_POINT('Ctrl Pts',(5.95184265120665,3.21991584599309,38.4606710883602));
#57602=CARTESIAN_POINT('Ctrl Pts',(5.8633328133567,3.38352155904993,38.4694208687146));
#57603=CARTESIAN_POINT('Ctrl Pts',(5.76807337235865,3.54347560903532,38.4781706490691));
#57604=CARTESIAN_POINT('Ctrl Pts',(5.66638790086537,3.69923467178369,38.4869204294235));
#57605=CARTESIAN_POINT('Ctrl Pts',(5.56470608502933,3.85498813489489,38.4956698952177));
#57606=CARTESIAN_POINT('Ctrl Pts',(5.45659885767152,4.00654667255989,38.504419361012));
#57607=CARTESIAN_POINT('Ctrl Pts',(5.34243340580716,4.15339551505942,38.5131688268063));
#57608=CARTESIAN_POINT('Ctrl Pts',(5.22827145140797,4.30023985883624,38.5219180245601));
#57609=CARTESIAN_POINT('Ctrl Pts',(5.10805181978285,4.44237456992818,38.530667222314));
#57610=CARTESIAN_POINT('Ctrl Pts',(4.98218281282739,4.57931691626244,38.5394164200679));
#57611=CARTESIAN_POINT('Ctrl Pts',(4.85631699296418,4.71625579511967,38.5481653962859));
#57612=CARTESIAN_POINT('Ctrl Pts',(4.72480227792028,4.84800236135585,38.5569143725039));
#57613=CARTESIAN_POINT('Ctrl Pts',(4.58808530848303,4.97410918678734,38.5656633487219));
#57614=CARTESIAN_POINT('Ctrl Pts',(4.45135945057161,5.10022421088843,38.5744128937431));
#57615=CARTESIAN_POINT('Ctrl Pts',(4.3094308720823,5.22069856611829,38.5831624387643));
#57616=CARTESIAN_POINT('Ctrl Pts',(4.16278164322658,5.33512305301535,38.5919119837855));
#57617=CARTESIAN_POINT('Ctrl Pts',(4.01614103534572,5.44954081331294,38.6006610144528));
#57618=CARTESIAN_POINT('Ctrl Pts',(3.86478055833585,5.55790924068218,38.6094100451201));
#57619=CARTESIAN_POINT('Ctrl Pts',(3.70921425812113,5.65986029751185,38.6181590757873));
#57620=CARTESIAN_POINT('Ctrl Pts',(3.55364584530289,5.76181273884549,38.6269082252672));
#57621=CARTESIAN_POINT('Ctrl Pts',(3.39387173464521,5.85734747817961,38.635657374747));
#57622=CARTESIAN_POINT('Ctrl Pts',(3.23043456092589,5.94614005448708,38.6444065242269));
#57623=CARTESIAN_POINT('Ctrl Pts',(3.1869076880652,5.96978744811214,38.6467366129599));
#57624=CARTESIAN_POINT('Ctrl Pts',(3.14312114982954,5.99295688499263,38.649066701693));
#57625=CARTESIAN_POINT('Ctrl Pts',(3.09908550384735,6.01564277861005,38.6513967904261));
#57626=CARTESIAN_POINT('Origin',(0.,0.,-63.6971797838103));
#57627=CARTESIAN_POINT('',(3.09908550384737,6.01564277861004,41.0460412338187));
#57628=CARTESIAN_POINT('',(3.0990855038471,6.01564277861018,40.6514943894097));
#57629=CARTESIAN_POINT('',(3.09908550384721,6.01564277861012,-63.6971797838103));
#57630=CARTESIAN_POINT('',(-6.76699998768905,-0.000408186690650814,39.6971797838371));
#57631=CARTESIAN_POINT('Ctrl Pts',(-6.76699998768905,-0.000408186690462319,
39.6971797838371));
#57632=CARTESIAN_POINT('Ctrl Pts',(-6.7669893069887,-0.177474957546841,
39.7055509473628));
#57633=CARTESIAN_POINT('Ctrl Pts',(-6.76002454313562,-0.354721736622949,
39.7139221108885));
#57634=CARTESIAN_POINT('Ctrl Pts',(-6.74608922499918,-0.531572354764644,
39.7222932744142));
#57635=CARTESIAN_POINT('Ctrl Pts',(-6.73216752127865,-0.708250194800711,
39.7306562595474));
#57636=CARTESIAN_POINT('Ctrl Pts',(-6.71128886035345,-0.884532305404253,
39.7390192446805));
#57637=CARTESIAN_POINT('Ctrl Pts',(-6.68348879857372,-1.05984266725754,
39.7473822298137));
#57638=CARTESIAN_POINT('Ctrl Pts',(-6.65571106829061,-1.23501220414491,
39.7557384970491));
#57639=CARTESIAN_POINT('Ctrl Pts',(-6.62102307112024,-1.40921121080189,
39.7640947642845));
#57640=CARTESIAN_POINT('Ctrl Pts',(-6.57951218369061,-1.58186864962514,
39.7724510315198));
#57641=CARTESIAN_POINT('Ctrl Pts',(-6.53802743766386,-1.75441735775269,
39.7808020364117));
#57642=CARTESIAN_POINT('Ctrl Pts',(-6.48972844551703,-1.92542610070345,
39.7891530413036));
#57643=CARTESIAN_POINT('Ctrl Pts',(-6.43475374173362,-2.09433361316798,
39.7975040461954));
#57644=CARTESIAN_POINT('Ctrl Pts',(-6.3798024647024,-2.26316914790154,39.8058514924156));
#57645=CARTESIAN_POINT('Ctrl Pts',(-6.31818125176635,-2.42990491138873,
39.8141989386358));
#57646=CARTESIAN_POINT('Ctrl Pts',(-6.25007870163198,-2.59399406772768,
39.822546384856));
#57647=CARTESIAN_POINT('Ctrl Pts',(-6.18199193246221,-2.75804520074498,
39.8308918967763));
#57648=CARTESIAN_POINT('Ctrl Pts',(-6.10742695007066,-2.91945063234419,
39.8392374086966));
#57649=CARTESIAN_POINT('Ctrl Pts',(-6.02662089271538,-3.07768250725875,
39.8475829206169));
#57650=CARTESIAN_POINT('Ctrl Pts',(-5.94582084388802,-3.23590261646329,
39.8559278119867));
#57651=CARTESIAN_POINT('Ctrl Pts',(-5.85878080098072,-3.3909493341977,39.8642727033565));
#57652=CARTESIAN_POINT('Ctrl Pts',(-5.76578446894041,-3.54231823213635,
39.8726175947263));
#57653=CARTESIAN_POINT('Ctrl Pts',(-5.67278041850855,-3.69369969319868,
39.8809631786948));
#57654=CARTESIAN_POINT('Ctrl Pts',(-5.57381927358222,-3.84140243443189,
39.8893087626633));
#57655=CARTESIAN_POINT('Ctrl Pts',(-5.46922891738796,-3.98494969218023,
39.8976543466318));
#57656=CARTESIAN_POINT('Ctrl Pts',(-5.36457065941219,-4.12859014317207,
39.9060053486908));
#57657=CARTESIAN_POINT('Ctrl Pts',(-5.25427608820586,-4.26806944150156,
39.9143563507499));
#57658=CARTESIAN_POINT('Ctrl Pts',(-5.13871494445318,-4.40294193916449,
39.9227073528089));
#57659=CARTESIAN_POINT('Ctrl Pts',(-5.02311737044658,-4.53785695491938,
39.9310609874927));
#57660=CARTESIAN_POINT('Ctrl Pts',(-4.90225014228802,-4.66816201893523,
39.9394146221764));
#57661=CARTESIAN_POINT('Ctrl Pts',(-4.77652120601833,-4.79344700277965,
39.9477682568602));
#57662=CARTESIAN_POINT('Ctrl Pts',(-4.65066169959826,-4.91886209572755,
39.9561305668368));
#57663=CARTESIAN_POINT('Ctrl Pts',(-4.51993064258537,-5.03924645202986,
39.9644928768133));
#57664=CARTESIAN_POINT('Ctrl Pts',(-4.38477143172748,-5.15422821492283,
39.9728551867899));
#57665=CARTESIAN_POINT('Ctrl Pts',(-4.26136283552805,-5.25921357150409,
39.9804904854029));
#57666=CARTESIAN_POINT('Ctrl Pts',(-4.1342631326172,-5.35969524653657,39.9881257840159));
#57667=CARTESIAN_POINT('Ctrl Pts',(-4.00383178889481,-5.4554211575492,39.9957610826289));
#57668=CARTESIAN_POINT('Ctrl Pts',(-3.8647554384088,-5.55749179464177,40.0039024498467));
#57669=CARTESIAN_POINT('Ctrl Pts',(-3.72159612305646,-5.65437077790788,
40.0120438170646));
#57670=CARTESIAN_POINT('Ctrl Pts',(-3.57478265544449,-5.74571300765477,
40.0201851842825));
#57671=CARTESIAN_POINT('Ctrl Pts',(-3.42809734482381,-5.83697550258215,
40.0283194447059));
#57672=CARTESIAN_POINT('Ctrl Pts',(-3.27776453996345,-5.92271067241397,
40.0364537051294));
#57673=CARTESIAN_POINT('Ctrl Pts',(-3.1242444878253,-6.00261487855861,40.0445879655529));
#57674=CARTESIAN_POINT('Ctrl Pts',(-2.970829161522,-6.08246457693975,40.0527166770777));
#57675=CARTESIAN_POINT('Ctrl Pts',(-2.81423124013008,-6.15649106274397,
40.0608453886025));
#57676=CARTESIAN_POINT('Ctrl Pts',(-2.65493815887967,-6.2244351046922,40.0689741001273));
#57677=CARTESIAN_POINT('Ctrl Pts',(-2.49572104155544,-6.29234674538266,
40.0770989352198));
#57678=CARTESIAN_POINT('Ctrl Pts',(-2.33381165978804,-6.3541815750316,40.0852237703124));
#57679=CARTESIAN_POINT('Ctrl Pts',(-2.16972013415191,-6.40972725936571,
40.0933486054049));
#57680=CARTESIAN_POINT('Ctrl Pts',(-2.00567454639833,-6.46525739352979,
40.1014711659271));
#57681=CARTESIAN_POINT('Ctrl Pts',(-1.83944837825209,-6.51450177280169,
40.1095937264492));
#57682=CARTESIAN_POINT('Ctrl Pts',(-1.67156969058518,-6.55729698652707,
40.1177162869714));
#57683=CARTESIAN_POINT('Ctrl Pts',(-1.50368208060156,-6.60009447470703,
40.1258392791865));
#57684=CARTESIAN_POINT('Ctrl Pts',(-1.33414212939293,-6.63644201839307,
40.1339622714017));
#57685=CARTESIAN_POINT('Ctrl Pts',(-1.16349113385735,-6.66622662241806,
40.1420852636169));
#57686=CARTESIAN_POINT('Ctrl Pts',(-1.07637900115297,-6.68143075509968,
40.146231803598));
#57687=CARTESIAN_POINT('Ctrl Pts',(-0.988977531711366,-6.69492554177188,
40.1503783435792));
#57688=CARTESIAN_POINT('Ctrl Pts',(-0.901359588944638,-6.70670111839029,
40.1545248835603));
#57689=CARTESIAN_POINT('Ctrl Pts',(-0.711531509107533,-6.73221341676049,
40.1635085425886));
#57690=CARTESIAN_POINT('Ctrl Pts',(-0.520780911100196,-6.74964037716923,
40.172492201617));
#57691=CARTESIAN_POINT('Ctrl Pts',(-0.329777953790215,-6.75895964636526,
40.1814758606454));
#57692=CARTESIAN_POINT('Ctrl Pts',(-0.138446855423123,-6.76829492596703,
40.1904749535048));
#57693=CARTESIAN_POINT('Ctrl Pts',(0.0531372298977748,-6.76949466268849,
40.1994740463642));
#57694=CARTESIAN_POINT('Ctrl Pts',(0.244304328232994,-6.76258858686573,
40.2084731392236));
#57695=CARTESIAN_POINT('Ctrl Pts',(0.435919659992452,-6.75566631822506,
40.2174933324409));
#57696=CARTESIAN_POINT('Ctrl Pts',(0.627115808575196,-6.7406002183414,40.2265135256583));
#57697=CARTESIAN_POINT('Ctrl Pts',(0.817225335351815,-6.71747212508241,
40.2355337188757));
#57698=CARTESIAN_POINT('Ctrl Pts',(1.00752739562876,-6.69432060883759,40.2445630472974));
#57699=CARTESIAN_POINT('Ctrl Pts',(1.19674039916342,-6.66309082283544,40.2535923757191));
#57700=CARTESIAN_POINT('Ctrl Pts',(1.38420568205252,-6.62391603432392,40.2626217041408));
#57701=CARTESIAN_POINT('Ctrl Pts',(1.57193525320336,-6.58468601725702,40.2716637620956));
#57702=CARTESIAN_POINT('Ctrl Pts',(1.75791194283566,-6.53748865039368,40.2807058200503));
#57703=CARTESIAN_POINT('Ctrl Pts',(1.94148860172122,-6.48250808016362,40.2897478780051));
#57704=CARTESIAN_POINT('Ctrl Pts',(2.10080125023388,-6.4347944965672,40.2975948135007));
#57705=CARTESIAN_POINT('Ctrl Pts',(2.25830651812223,-6.38122002535534,40.3054417489963));
#57706=CARTESIAN_POINT('Ctrl Pts',(2.4135921446991,-6.32193498535431,40.3132886844919));
#57707=CARTESIAN_POINT('Ctrl Pts',(2.58483843909759,-6.25655647198356,40.3219421487927));
#57708=CARTESIAN_POINT('Ctrl Pts',(2.75353582436312,-6.18417428724513,40.3305956130935));
#57709=CARTESIAN_POINT('Ctrl Pts',(2.91910892899455,-6.10500549227143,40.3392490773943));
#57710=CARTESIAN_POINT('Ctrl Pts',(3.0845295069299,-6.02590962795127,40.3478945700845));
#57711=CARTESIAN_POINT('Ctrl Pts',(3.24683127136244,-5.94003975356798,40.3565400627747));
#57712=CARTESIAN_POINT('Ctrl Pts',(3.4054589288059,-5.84766094128381,40.3651855554648));
#57713=CARTESIAN_POINT('Ctrl Pts',(3.56885862701655,-5.75250307101346,40.3740911329614));
#57714=CARTESIAN_POINT('Ctrl Pts',(3.72835940075996,-5.6504386328712,40.382996710458));
#57715=CARTESIAN_POINT('Ctrl Pts',(3.88337960349927,-5.54180943872359,40.3919022879545));
#57716=CARTESIAN_POINT('Ctrl Pts',(4.03358693126474,-5.43655282905661,40.4005313761271));
#57717=CARTESIAN_POINT('Ctrl Pts',(4.17958744935665,-5.32513315917595,40.4091604642996));
#57718=CARTESIAN_POINT('Ctrl Pts',(4.32087920515903,-5.20790667105549,40.4177895524722));
#57719=CARTESIAN_POINT('Ctrl Pts',(4.46896177036093,-5.08504600610086,40.4268333746307));
#57720=CARTESIAN_POINT('Ctrl Pts',(4.61187149305091,-4.9558067525573,40.4358771967892));
#57721=CARTESIAN_POINT('Ctrl Pts',(4.74906675487989,-4.82064870714457,40.4449210189478));
#57722=CARTESIAN_POINT('Ctrl Pts',(4.88626201670897,-4.68549066173174,40.4539648411063));
#57723=CARTESIAN_POINT('Ctrl Pts',(5.01774251887779,-4.54441407019152,40.4630086632648));
#57724=CARTESIAN_POINT('Ctrl Pts',(5.14300831224654,-4.39792615901666,40.4720524854234));
#57725=CARTESIAN_POINT('Ctrl Pts',(5.25971375290996,-4.26144886728546,40.4804782752732));
#57726=CARTESIAN_POINT('Ctrl Pts',(5.37097391419248,-4.12033448493361,40.488904065123));
#57727=CARTESIAN_POINT('Ctrl Pts',(5.47642802186094,-3.97505032941425,40.4973298549728));
#57728=CARTESIAN_POINT('Ctrl Pts',(5.58190659843003,-3.8297324630832,40.5057575998893));
#57729=CARTESIAN_POINT('Ctrl Pts',(5.6815762405327,-3.68024316275739,40.5141853448058));
#57730=CARTESIAN_POINT('Ctrl Pts',(5.77511892322488,-3.52707958835775,40.5226130897223));
#57731=CARTESIAN_POINT('Ctrl Pts',(5.86869597815981,-3.37385973402892,40.5310439314122));
#57732=CARTESIAN_POINT('Ctrl Pts',(5.95614141199291,-3.21696319640461,40.5394747731021));
#57733=CARTESIAN_POINT('Ctrl Pts',(6.03718246284654,-3.05691297067781,40.5479056147921));
#57734=CARTESIAN_POINT('Ctrl Pts',(6.11829798008194,-2.89671567922214,40.5563442033494));
#57735=CARTESIAN_POINT('Ctrl Pts',(6.19299720718392,-2.73335920601794,40.5647827919068));
#57736=CARTESIAN_POINT('Ctrl Pts',(6.26105450610643,-2.5673888430786,40.5732213804641));
#57737=CARTESIAN_POINT('Ctrl Pts',(6.32914749126888,-2.40133145261552,40.5816643938444));
#57738=CARTESIAN_POINT('Ctrl Pts',(6.39059148392767,-2.23265774820703,40.5901074072246));
#57739=CARTESIAN_POINT('Ctrl Pts',(6.44521011227507,-2.06193006880136,40.5985504206049));
#57740=CARTESIAN_POINT('Ctrl Pts',(6.49988612129841,-1.89102302806892,40.6070023039592));
#57741=CARTESIAN_POINT('Ctrl Pts',(6.54772234890497,-1.71805801963597,40.6154541873135));
#57742=CARTESIAN_POINT('Ctrl Pts',(6.58859283013561,-1.54361054631202,40.6239060706678));
#57743=CARTESIAN_POINT('Ctrl Pts',(6.59973132746635,-1.49606809862198,40.6262094758968));
#57744=CARTESIAN_POINT('Ctrl Pts',(6.61035274938802,-1.44841559263421,40.6285128811259));
#57745=CARTESIAN_POINT('Ctrl Pts',(6.62045521010196,-1.40066477468157,40.630816286355));
#57746=CARTESIAN_POINT('Ctrl Pts',(6.65693374423811,-1.22824343179927,40.6391335516884));
#57747=CARTESIAN_POINT('Ctrl Pts',(6.68670754520988,-1.05422956792178,40.6474508170218));
#57748=CARTESIAN_POINT('Ctrl Pts',(6.7096447804503,-0.879179117231563,40.6557680823552));
#57749=CARTESIAN_POINT('Ctrl Pts',(6.73256266989776,-0.70427630812673,40.6640783327153));
#57750=CARTESIAN_POINT('Ctrl Pts',(6.74865543694662,-0.52833899725857,40.6723885830754));
#57751=CARTESIAN_POINT('Ctrl Pts',(6.75784224608755,-0.351933483764263,
40.6806988334355));
#57752=CARTESIAN_POINT('Ctrl Pts',(6.76702298932,-0.175644448111405,40.6890035966654));
#57753=CARTESIAN_POINT('Ctrl Pts',(6.76930684277377,0.00111182795543882,
40.6973083598952));
#57754=CARTESIAN_POINT('Ctrl Pts',(6.76466474650015,0.17776351554252,40.7056131231251));
#57755=CARTESIAN_POINT('Ctrl Pts',(6.76002486556583,0.354330899961088,40.7139139230877));
#57756=CARTESIAN_POINT('Ctrl Pts',(6.74846563108645,0.530793448378331,40.7222147230503));
#57757=CARTESIAN_POINT('Ctrl Pts',(6.73001007095392,0.706578689785423,40.7305155230129));
#57758=CARTESIAN_POINT('Ctrl Pts',(6.71155994107486,0.88231220919593,40.7388138805979));
#57759=CARTESIAN_POINT('Ctrl Pts',(6.68621756648536,1.0573684733161,40.7471122381828));
#57760=CARTESIAN_POINT('Ctrl Pts',(6.65405790624388,1.23117926410141,40.7554105957677));
#57761=CARTESIAN_POINT('Ctrl Pts',(6.62189497383071,1.40500773973616,40.7637097976915));
#57762=CARTESIAN_POINT('Ctrl Pts',(6.58291342568409,1.57759014545674,40.7720089996153));
#57763=CARTESIAN_POINT('Ctrl Pts',(6.5372396140938,1.74836701751169,40.7803082015391));
#57764=CARTESIAN_POINT('Ctrl Pts',(6.49156117204478,1.91916120310433,40.7886082448446));
#57765=CARTESIAN_POINT('Ctrl Pts',(6.43918920361854,2.08814915383814,40.7969082881502));
#57766=CARTESIAN_POINT('Ctrl Pts',(6.38030034156562,2.2547852561647,40.8052083314557));
#57767=CARTESIAN_POINT('Ctrl Pts',(6.32139573361864,2.42146591419026,40.8135105940537));
#57768=CARTESIAN_POINT('Ctrl Pts',(6.25597087498801,2.5857931424035,40.8218128566516));
#57769=CARTESIAN_POINT('Ctrl Pts',(6.18425113812239,2.74723986223118,40.8301151192496));
#57770=CARTESIAN_POINT('Ctrl Pts',(6.11250031754195,2.90875655392457,40.8384209800922));
#57771=CARTESIAN_POINT('Ctrl Pts',(6.03444932246879,3.06738993135616,40.8467268409348));
#57772=CARTESIAN_POINT('Ctrl Pts',(5.95037027780558,3.22263596408405,40.8550327017774));
#57773=CARTESIAN_POINT('Ctrl Pts',(5.86619184577965,3.37806550857552,40.8633483807335));
#57774=CARTESIAN_POINT('Ctrl Pts',(5.77597129333123,3.53009940209645,40.8716640596897));
#57775=CARTESIAN_POINT('Ctrl Pts',(5.68002564840435,3.6782601367316,40.8799797386458));
#57776=CARTESIAN_POINT('Ctrl Pts',(5.58401931862118,3.82651458185144,40.8883006772027));
#57777=CARTESIAN_POINT('Ctrl Pts',(5.4822808751195,3.97089069870037,40.8966216157595));
#57778=CARTESIAN_POINT('Ctrl Pts',(5.37516881303009,4.11094262079012,40.9049425543164));
#57779=CARTESIAN_POINT('Ctrl Pts',(5.26789754923871,4.25120270341684,40.9132758603653));
#57780=CARTESIAN_POINT('Ctrl Pts',(5.1552369273305,4.38712547930825,40.9216091664143));
#57781=CARTESIAN_POINT('Ctrl Pts',(5.03758449860262,4.51829961594388,40.9299424724632));
#57782=CARTESIAN_POINT('Ctrl Pts',(4.95098536484261,4.61485152504757,40.9360762777148));
#57783=CARTESIAN_POINT('Ctrl Pts',(4.861682553003,4.70883144820397,40.9422100829664));
#57784=CARTESIAN_POINT('Ctrl Pts',(4.76984630227297,4.80008908799544,40.948343888218));
#57785=CARTESIAN_POINT('Ctrl Pts',(4.6479513616092,4.9212160340442,40.9564853336847));
#57786=CARTESIAN_POINT('Ctrl Pts',(4.52121319054477,5.03792146431372,40.9646267791515));
#57787=CARTESIAN_POINT('Ctrl Pts',(4.3899908637469,5.14978341449607,40.9727682246182));
#57788=CARTESIAN_POINT('Ctrl Pts',(4.26006191464205,5.26054281029919,40.9808294248689));
#57789=CARTESIAN_POINT('Ctrl Pts',(4.12573706105073,5.36655348541563,40.9888906251197));
#57790=CARTESIAN_POINT('Ctrl Pts',(3.98740513822656,5.46743900410827,40.9969518253704));
#57791=CARTESIAN_POINT('Ctrl Pts',(3.84700767776288,5.56983092010883,41.0051333934452));
#57792=CARTESIAN_POINT('Ctrl Pts',(3.70248276567876,5.66694309843023,41.0133149615198));
#57793=CARTESIAN_POINT('Ctrl Pts',(3.55427531661674,5.75842130915141,41.0214965295946));
#57794=CARTESIAN_POINT('Ctrl Pts',(3.40606786755482,5.84989951987252,41.0296780976693));
#57795=CARTESIAN_POINT('Ctrl Pts',(3.25417819184764,5.9357435028679,41.037859665744));
#57796=CARTESIAN_POINT('Ctrl Pts',(3.09908550384737,6.01564277861004,41.0460412338188));
#57797=CARTESIAN_POINT('Ctrl Pts',(3.09908550384713,6.01564277861016,39.0456530966623));
#57798=CARTESIAN_POINT('Ctrl Pts',(2.9446003203866,6.09522908555046,39.0538824990093));
#57799=CARTESIAN_POINT('Ctrl Pts',(2.78682478641158,6.16897536872828,39.0621119013562));
#57800=CARTESIAN_POINT('Ctrl Pts',(2.62623941930812,6.23659807206398,39.0703413037032));
#57801=CARTESIAN_POINT('Ctrl Pts',(2.46584144851121,6.30414186257548,39.078561102687));
#57802=CARTESIAN_POINT('Ctrl Pts',(2.30264050108509,6.36557616480819,39.0867809016708));
#57803=CARTESIAN_POINT('Ctrl Pts',(2.13714233615255,6.42066286570354,39.0950007006546));
#57804=CARTESIAN_POINT('Ctrl Pts',(1.97180409788713,6.47569633439248,39.103212556559));
#57805=CARTESIAN_POINT('Ctrl Pts',(1.80417340096941,6.52439430504693,39.1114244124634));
#57806=CARTESIAN_POINT('Ctrl Pts',(1.63477675133519,6.56656637621931,39.1196362683678));
#57807=CARTESIAN_POINT('Ctrl Pts',(1.46550982262301,6.60870615277448,39.12784183578));
#57808=CARTESIAN_POINT('Ctrl Pts',(1.29447998119713,6.6443298975055,39.1360474031922));
#57809=CARTESIAN_POINT('Ctrl Pts',(1.12222978257994,6.67329673512954,39.1442529706043));
#57810=CARTESIAN_POINT('Ctrl Pts',(0.950076953392023,6.70224719840702,39.1524538995811));
#57811=CARTESIAN_POINT('Ctrl Pts',(0.776705493949861,6.7245481917699,39.1606548285579));
#57812=CARTESIAN_POINT('Ctrl Pts',(0.602669155930628,6.74010970893574,39.1688557575347));
#57813=CARTESIAN_POINT('Ctrl Pts',(0.428678188946208,6.75566716923539,39.1770545485406));
#57814=CARTESIAN_POINT('Ctrl Pts',(0.254023044948438,6.76448861684865,39.1852533395464));
#57815=CARTESIAN_POINT('Ctrl Pts',(0.0792638848705898,6.7665357633397,39.1934521305523));
#57816=CARTESIAN_POINT('Ctrl Pts',(-0.0954753772327584,6.76858267674387,
39.2016499880486));
#57817=CARTESIAN_POINT('Ctrl Pts',(-0.270318273336021,6.76385682026826,
39.209847845545));
#57818=CARTESIAN_POINT('Ctrl Pts',(-0.444703345564633,6.75237202281122,
39.2180457030413));
#57819=CARTESIAN_POINT('Ctrl Pts',(-0.619100239948408,6.74088644676082,
39.2262441162982));
#57820=CARTESIAN_POINT('Ctrl Pts',(-0.793038890761985,6.7226410404945,39.2344425295551));
#57821=CARTESIAN_POINT('Ctrl Pts',(-0.965961612094605,6.69770163294541,
39.242640942812));
#57822=CARTESIAN_POINT('Ctrl Pts',(-1.1389274682706,6.67275600436631,39.2508414011285));
#57823=CARTESIAN_POINT('Ctrl Pts',(-1.31087653538488,6.64111309994968,39.2590418594451));
#57824=CARTESIAN_POINT('Ctrl Pts',(-1.48125993131168,6.60289012598957,39.2672423177616));
#57825=CARTESIAN_POINT('Ctrl Pts',(-1.6518057834008,6.56463070741214,39.275450595003));
#57826=CARTESIAN_POINT('Ctrl Pts',(-1.82078263170728,6.51977876420005,39.2836588722445));
#57827=CARTESIAN_POINT('Ctrl Pts',(-1.98765450752797,6.46850203360127,39.2918671494859));
#57828=CARTESIAN_POINT('Ctrl Pts',(-2.15461006186638,6.41719959009677,39.3000795427983));
#57829=CARTESIAN_POINT('Ctrl Pts',(-2.31945820115124,6.35946605453715,39.3082919361107));
#57830=CARTESIAN_POINT('Ctrl Pts',(-2.48168172307127,6.29551783615725,39.3165043294231));
#57831=CARTESIAN_POINT('Ctrl Pts',(-2.64412359806743,6.2314835433904,39.3247277766278));
#57832=CARTESIAN_POINT('Ctrl Pts',(-2.80393346830925,6.16121799693371,39.3329512238325));
#57833=CARTESIAN_POINT('Ctrl Pts',(-2.96061653670768,6.0849846937008,39.3411746710371));
#57834=CARTESIAN_POINT('Ctrl Pts',(-3.08466060653792,6.02463171946898,39.347685073659));
#57835=CARTESIAN_POINT('Ctrl Pts',(-3.20674532188333,5.96053928021444,39.3541954762809));
#57836=CARTESIAN_POINT('Ctrl Pts',(-3.32663794447513,5.89285745512127,39.3607058789027));
#57837=CARTESIAN_POINT('Ctrl Pts',(-3.49118429266487,5.79996769328983,39.369641065685));
#57838=CARTESIAN_POINT('Ctrl Pts',(-3.65194238196678,5.70012322094762,39.3785762524673));
#57839=CARTESIAN_POINT('Ctrl Pts',(-3.80834113109411,5.59364164290284,39.3875114392495));
#57840=CARTESIAN_POINT('Ctrl Pts',(-3.9645056432784,5.48731954132109,39.3964332438862));
#57841=CARTESIAN_POINT('Ctrl Pts',(-4.11632362974265,5.37438031348778,39.4053550485228));
#57842=CARTESIAN_POINT('Ctrl Pts',(-4.2632510875454,5.25518593053975,39.4142768531594));
#57843=CARTESIAN_POINT('Ctrl Pts',(-4.40982015443415,5.13628229095915,39.4231768953987));
#57844=CARTESIAN_POINT('Ctrl Pts',(-4.55152230097991,5.01115411069876,39.432076937638));
#57845=CARTESIAN_POINT('Ctrl Pts',(-4.68784530566999,4.88020444142536,39.4409769798773));
#57846=CARTESIAN_POINT('Ctrl Pts',(-4.82395843909019,4.74945637109297,39.4498633203707));
#57847=CARTESIAN_POINT('Ctrl Pts',(-4.95470876426148,4.61290486721666,39.4587496608641));
#57848=CARTESIAN_POINT('Ctrl Pts',(-5.07961745791228,4.47099267291648,39.4676360013575));
#57849=CARTESIAN_POINT('Ctrl Pts',(-5.20420678183671,4.32944332332579,39.4764996210295));
#57850=CARTESIAN_POINT('Ctrl Pts',(-5.3229841079977,4.18256082681411,39.4853632407014));
#57851=CARTESIAN_POINT('Ctrl Pts',(-5.43550828445764,4.03082357460512,39.4942268603733));
#57852=CARTESIAN_POINT('Ctrl Pts',(-5.54232798026772,3.88677873345232,39.502641133527));
#57853=CARTESIAN_POINT('Ctrl Pts',(-5.64351257316431,3.73835929877524,39.5110554066807));
#57854=CARTESIAN_POINT('Ctrl Pts',(-5.73871556846863,3.58600510655183,39.5194696798344));
#57855=CARTESIAN_POINT('Ctrl Pts',(-5.83161013071872,3.4373451200848,39.527679928039));
#57856=CARTESIAN_POINT('Ctrl Pts',(-5.91871951545199,3.28508121074497,39.5358901762436));
#57857=CARTESIAN_POINT('Ctrl Pts',(-5.99976880637994,3.12970657889686,39.5441004244481));
#57858=CARTESIAN_POINT('Ctrl Pts',(-6.08083736434019,2.9742950114011,39.5523126243924));
#57859=CARTESIAN_POINT('Ctrl Pts',(-6.15584279376882,2.81577156373658,39.5605248243366));
#57860=CARTESIAN_POINT('Ctrl Pts',(-6.22455695618284,2.65465246298565,39.5687370242809));
#57861=CARTESIAN_POINT('Ctrl Pts',(-6.29329968938915,2.49346637021739,39.5769526387914));
#57862=CARTESIAN_POINT('Ctrl Pts',(-6.35574580469699,2.32968280140303,39.5851682533019));
#57863=CARTESIAN_POINT('Ctrl Pts',(-6.4117159255237,2.16383638253583,39.5933838678123));
#57864=CARTESIAN_POINT('Ctrl Pts',(-6.46774889834276,1.9978037254098,39.6016087080978));
#57865=CARTESIAN_POINT('Ctrl Pts',(-6.51729123776591,1.82970392883746,39.6098335483833));
#57866=CARTESIAN_POINT('Ctrl Pts',(-6.56021365311348,1.66008608978676,39.6180583886687));
#57867=CARTESIAN_POINT('Ctrl Pts',(-6.60316356176015,1.49035960461389,39.6262884972503));
#57868=CARTESIAN_POINT('Ctrl Pts',(-6.6394850198573,1.31911348591226,39.6345186058319));
#57869=CARTESIAN_POINT('Ctrl Pts',(-6.66910018189931,1.14690529852754,39.6427487144135));
#57870=CARTESIAN_POINT('Ctrl Pts',(-6.69875594678292,0.974461011075437,
39.6509901066002));
#57871=CARTESIAN_POINT('Ctrl Pts',(-6.72168700417267,0.801052372189292,
39.659231498787));
#57872=CARTESIAN_POINT('Ctrl Pts',(-6.73786741612785,0.627241327307671,
39.6674728909737));
#57873=CARTESIAN_POINT('Ctrl Pts',(-6.74490954249729,0.551594344656564,
39.6710597542378));
#57874=CARTESIAN_POINT('Ctrl Pts',(-6.75067362222021,0.475871132458775,
39.6746466175018));
#57875=CARTESIAN_POINT('Ctrl Pts',(-6.75516059642061,0.400117878338753,
39.6782334807659));
#57876=CARTESIAN_POINT('Ctrl Pts',(-6.7630608671859,0.266738190342119,39.6845489151139));
#57877=CARTESIAN_POINT('Ctrl Pts',(-6.76700804548976,0.133175820827996,
39.6908643494619));
#57878=CARTESIAN_POINT('Ctrl Pts',(-6.76699998768909,-0.00040818611676218,
39.6971797838099));
#57879=CARTESIAN_POINT('',(-6.76699837066092,-0.00360871217654551,39.3028202161897));
#57880=CARTESIAN_POINT('Ctrl Pts',(3.09908550384735,6.01564277861005,38.6513967904261));
#57881=CARTESIAN_POINT('Ctrl Pts',(2.93373232018349,6.1008279655247,38.6601462383254));
#57882=CARTESIAN_POINT('Ctrl Pts',(2.76486502144451,6.17919158180179,38.6688956862246));
#57883=CARTESIAN_POINT('Ctrl Pts',(2.59305716434381,6.25046746591367,38.6776451341239));
#57884=CARTESIAN_POINT('Ctrl Pts',(2.42125069459311,6.32174277447214,38.6863945113713));
#57885=CARTESIAN_POINT('Ctrl Pts',(2.24650397871084,6.38593035557817,38.6951438886188));
#57886=CARTESIAN_POINT('Ctrl Pts',(2.06941053323796,6.44281220003531,38.7038932658662));
#57887=CARTESIAN_POINT('Ctrl Pts',(1.89231845896707,6.49969360406678,38.7126425753688));
#57888=CARTESIAN_POINT('Ctrl Pts',(1.71287996431528,6.54926929700875,38.7213918848714));
#57889=CARTESIAN_POINT('Ctrl Pts',(1.53170449173527,6.59137090065474,38.730141194374));
#57890=CARTESIAN_POINT('Ctrl Pts',(1.35053036178192,6.63347219230079,38.7388904390386));
#57891=CARTESIAN_POINT('Ctrl Pts',(1.16761955878866,6.6680994406245,38.7476396837031));
#57892=CARTESIAN_POINT('Ctrl Pts',(0.983593309310698,6.69513503985388,38.7563889283677));
#57893=CARTESIAN_POINT('Ctrl Pts',(0.79956836246001,6.72217044771214,38.7651381111009));
#57894=CARTESIAN_POINT('Ctrl Pts',(0.614428268438438,6.74161427235979,38.7738872938341));
#57895=CARTESIAN_POINT('Ctrl Pts',(0.428801816329926,6.75340047696804,38.7826364765673));
#57896=CARTESIAN_POINT('Ctrl Pts',(0.243176616522485,6.76518660206243,38.7913856002754));
#57897=CARTESIAN_POINT('Ctrl Pts',(0.0570653511652053,6.76931519233997,
38.8001347239836));
#57898=CARTESIAN_POINT('Ctrl Pts',(-0.128899900800241,6.76577222610795,
38.8088838476917));
#57899=CARTESIAN_POINT('Ctrl Pts',(-0.314863959942378,6.76222928260132,
38.817632915281));
#57900=CARTESIAN_POINT('Ctrl Pts',(-0.500681721081183,6.75101488651273,
38.8263819828702));
#57901=CARTESIAN_POINT('Ctrl Pts',(-0.685722110173944,6.73216712415984,
38.8351310504595));
#57902=CARTESIAN_POINT('Ctrl Pts',(-0.870761373828287,6.71331947644136,
38.8438800648359));
#57903=CARTESIAN_POINT('Ctrl Pts',(-1.05502298984414,6.68683858439985,38.8526290792122));
#57904=CARTESIAN_POINT('Ctrl Pts',(-1.23788117676133,6.65281438131412,38.8613780935886));
#57905=CARTESIAN_POINT('Ctrl Pts',(-1.43009641451857,6.61704912302363,38.8705748044761));
#57906=CARTESIAN_POINT('Ctrl Pts',(-1.62076048992751,6.57294837083151,38.8797715153636));
#57907=CARTESIAN_POINT('Ctrl Pts',(-1.80915798961178,6.52067760042036,38.8889682262511));
#57908=CARTESIAN_POINT('Ctrl Pts',(-1.98840443003049,6.47094578577397,38.8977182239576));
#57909=CARTESIAN_POINT('Ctrl Pts',(-2.16559895952219,6.41381888474466,38.9064682216642));
#57910=CARTESIAN_POINT('Ctrl Pts',(-2.3401396624234,6.34949095285228,38.9152182193707));
#57911=CARTESIAN_POINT('Ctrl Pts',(-2.51467682554033,6.28516432556678,38.9239680396223));
#57912=CARTESIAN_POINT('Ctrl Pts',(-2.68656000078861,6.21363705879653,38.9327178598738));
#57913=CARTESIAN_POINT('Ctrl Pts',(-2.85520533840908,6.1351521151085,38.9414676801254));
#57914=CARTESIAN_POINT('Ctrl Pts',(-3.02384747998342,6.05666865881114,38.9502173345567));
#57915=CARTESIAN_POINT('Ctrl Pts',(-3.18925164684548,5.97122791039838,38.9589669889879));
#57916=CARTESIAN_POINT('Ctrl Pts',(-3.35085601829165,5.87912008251904,38.9677166434192));
#57917=CARTESIAN_POINT('Ctrl Pts',(-3.5124575419142,5.78701387778173,38.9764661436623));
#57918=CARTESIAN_POINT('Ctrl Pts',(-3.67025915510932,5.68824097060985,38.9852156439055));
#57919=CARTESIAN_POINT('Ctrl Pts',(-3.82372487928825,5.58313684656861,38.9939651441486));
#57920=CARTESIAN_POINT('Ctrl Pts',(-3.97718810300799,5.47803443501773,39.0027145018337));
#57921=CARTESIAN_POINT('Ctrl Pts',(-4.12631534263035,5.36660117496369,39.0114638595188));
#57922=CARTESIAN_POINT('Ctrl Pts',(-4.27060009886244,5.24921554097335,39.020213217204));
#57923=CARTESIAN_POINT('Ctrl Pts',(-4.41488269594222,5.13183166360283,39.0289624439591));
#57924=CARTESIAN_POINT('Ctrl Pts',(-4.55432273235087,5.00849577139471,39.0377116707143));
#57925=CARTESIAN_POINT('Ctrl Pts',(-4.68844662480197,4.87962675277352,39.0464608974695));
#57926=CARTESIAN_POINT('Ctrl Pts',(-4.82256868835139,4.750759491399,39.055210004921));
#57927=CARTESIAN_POINT('Ctrl Pts',(-4.95137454637836,4.61635945312553,39.0639591123725));
#57928=CARTESIAN_POINT('Ctrl Pts',(-5.07442674461044,4.47688309134629,39.0727082198239));
#57929=CARTESIAN_POINT('Ctrl Pts',(-5.19747742838505,4.33740844616392,39.0814572195963));
#57930=CARTESIAN_POINT('Ctrl Pts',(-5.31477440450893,4.19285781736072,39.0902062193687));
#57931=CARTESIAN_POINT('Ctrl Pts',(-5.42591931531119,4.04372211999451,39.0989552191411));
#57932=CARTESIAN_POINT('Ctrl Pts',(-5.53707636462952,3.89457013500843,39.1077051744216));
#57933=CARTESIAN_POINT('Ctrl Pts',(-5.64207983273445,3.74083230916458,39.1164551297022));
#57934=CARTESIAN_POINT('Ctrl Pts',(-5.74057303468726,3.58303087251862,39.1252050849828));
#57935=CARTESIAN_POINT('Ctrl Pts',(-5.83906243363743,3.42523552887469,39.1339547024116));
#57936=CARTESIAN_POINT('Ctrl Pts',(-5.93104191768403,3.26337713157034,39.1427043198404));
#57937=CARTESIAN_POINT('Ctrl Pts',(-6.01619906699632,3.09800545291201,39.1514539372692));
#57938=CARTESIAN_POINT('Ctrl Pts',(-6.10135338095369,2.93263928039626,39.1602032633746));
#57939=CARTESIAN_POINT('Ctrl Pts',(-6.17968568352833,2.76376031540238,39.16895258948));
#57940=CARTESIAN_POINT('Ctrl Pts',(-6.25092992694887,2.5919421383154,39.1777019155854));
#57941=CARTESIAN_POINT('Ctrl Pts',(-6.32217217691103,2.42012876880821,39.1864509968792));
#57942=CARTESIAN_POINT('Ctrl Pts',(-6.38632665483849,2.24537661647675,39.195200078173));
#57943=CARTESIAN_POINT('Ctrl Pts',(-6.44317547869347,2.06827917621465,39.2039491594668));
#57944=CARTESIAN_POINT('Ctrl Pts',(-6.50002944235934,1.89116572423431,39.2126990317818));
#57945=CARTESIAN_POINT('Ctrl Pts',(-6.54957634250397,1.71170683289204,39.2214489040967));
#57946=CARTESIAN_POINT('Ctrl Pts',(-6.59164787708394,1.53051209225369,39.2301987764117));
#57947=CARTESIAN_POINT('Ctrl Pts',(-6.63371649075009,1.34932993148028,39.2389480412465));
#57948=CARTESIAN_POINT('Ctrl Pts',(-6.66831071257125,1.16641244173996,39.2476973060813));
#57949=CARTESIAN_POINT('Ctrl Pts',(-6.69531304840335,0.982380875159863,
39.2564465709161));
#57950=CARTESIAN_POINT('Ctrl Pts',(-6.72231677033045,0.79833986179569,39.2651962848717));
#57951=CARTESIAN_POINT('Ctrl Pts',(-6.74172778477891,0.613184940729997,
39.2739459988274));
#57952=CARTESIAN_POINT('Ctrl Pts',(-6.75348015835519,0.427545027690393,
39.282695712783));
#57953=CARTESIAN_POINT('Ctrl Pts',(-6.76249038365212,0.285219953548298,
39.2894038805853));
#57954=CARTESIAN_POINT('Ctrl Pts',(-6.7669999999999,0.142609995760424,39.2961120483875));
#57955=CARTESIAN_POINT('Ctrl Pts',(-6.767,4.67741087612267E-12,39.3028202161897));
#57956=CARTESIAN_POINT('Ctrl Pts',(-6.76699724104549,-0.00611062049019318,
39.3028202161897));
#57957=CARTESIAN_POINT('Ctrl Pts',(-6.76678101224438,-0.245565795769802,
39.3141020673561));
#57958=CARTESIAN_POINT('Ctrl Pts',(-6.75385175166444,-0.484454529984376,
39.3253839185225));
#57959=CARTESIAN_POINT('Ctrl Pts',(-6.72840805681548,-0.721674456372541,
39.3366657696888));
#57960=CARTESIAN_POINT('Ctrl Pts',(-6.70195509449772,-0.968304114958578,
39.3483951346868));
#57961=CARTESIAN_POINT('Ctrl Pts',(-6.66197504121415,-1.21313061101869,
39.3601244996846));
#57962=CARTESIAN_POINT('Ctrl Pts',(-6.6087384623976,-1.45494499402095,39.3718538646825));
#57963=CARTESIAN_POINT('Ctrl Pts',(-6.58712569453163,-1.55311580519366,
39.3766157041649));
#57964=CARTESIAN_POINT('Ctrl Pts',(-6.56332857647657,-1.65079044562883,
39.3813775436472));
#57965=CARTESIAN_POINT('Ctrl Pts',(-6.53736745489185,-1.7478889437607,39.3861393831296));
#57966=CARTESIAN_POINT('Ctrl Pts',(-6.4933628341328,-1.91247284174916,39.3942107963716));
#57967=CARTESIAN_POINT('Ctrl Pts',(-6.44305781121587,-2.0756966424793,39.4022822096136));
#57968=CARTESIAN_POINT('Ctrl Pts',(-6.38654762293997,-2.23702893587005,
39.4103536228556));
#57969=CARTESIAN_POINT('Ctrl Pts',(-6.33010837852473,-2.39815868992951,
39.4184149031069));
#57970=CARTESIAN_POINT('Ctrl Pts',(-6.26747959072336,-2.55740131402768,
39.4264761833581));
#57971=CARTESIAN_POINT('Ctrl Pts',(-6.19880741801831,-2.71423572932072,
39.4345374636094));
#57972=CARTESIAN_POINT('Ctrl Pts',(-6.13020639741324,-2.87090764650779,
39.442590391467));
#57973=CARTESIAN_POINT('Ctrl Pts',(-6.05557460105233,-3.0251759816103,39.4506433193246));
#57974=CARTESIAN_POINT('Ctrl Pts',(-5.97510786264064,-3.17653506667407,
39.4586962471822));
#57975=CARTESIAN_POINT('Ctrl Pts',(-5.89470687645742,-3.32777047085628,
39.4667425947065));
#57976=CARTESIAN_POINT('Ctrl Pts',(-5.80848061223211,-3.47610102889844,
39.4747889422309));
#57977=CARTESIAN_POINT('Ctrl Pts',(-5.71667281695634,-3.6210414115103,39.4828352897553));
#57978=CARTESIAN_POINT('Ctrl Pts',(-5.62491995828841,-3.76589506365514,
39.4908768224485));
#57979=CARTESIAN_POINT('Ctrl Pts',(-5.52759241645241,-3.90736226452003,
39.4989183551416));
#57980=CARTESIAN_POINT('Ctrl Pts',(-5.42497959273133,-4.04498274637218,
39.5069598878348));
#57981=CARTESIAN_POINT('Ctrl Pts',(-5.32039406441056,-4.18524894586192,
39.515156016883));
#57982=CARTESIAN_POINT('Ctrl Pts',(-5.21031815682281,-4.32151866788484,
39.5233521459313));
#57983=CARTESIAN_POINT('Ctrl Pts',(-5.09510456143018,-4.45333566083822,
39.5315482749795));
#57984=CARTESIAN_POINT('Ctrl Pts',(-4.98210315892401,-4.58262166243479,
39.5395870318156));
#57985=CARTESIAN_POINT('Ctrl Pts',(-4.86415984724632,-4.70762410039903,
39.5476257886517));
#57986=CARTESIAN_POINT('Ctrl Pts',(-4.74164766469593,-4.8279463981991,39.5556645454878));
#57987=CARTESIAN_POINT('Ctrl Pts',(-4.61912362426101,-4.948280341926,39.5637040803906));
#57988=CARTESIAN_POINT('Ctrl Pts',(-4.49203009881134,-5.06393298172611,
39.5717436152934));
#57989=CARTESIAN_POINT('Ctrl Pts',(-4.36077628353313,-5.17454531383918,
39.5797831501962));
#57990=CARTESIAN_POINT('Ctrl Pts',(-4.22948377597157,-5.2851902533373,39.5878250550717));
#57991=CARTESIAN_POINT('Ctrl Pts',(-4.094028822871,-5.39079168710017,39.5958669599473));
#57992=CARTESIAN_POINT('Ctrl Pts',(-3.9548527875009,-5.49103163614965,39.6039088648228));
#57993=CARTESIAN_POINT('Ctrl Pts',(-3.8109820268197,-5.59465290745577,39.6122220415036));
#57994=CARTESIAN_POINT('Ctrl Pts',(-3.66313510567491,-5.69254440155902,
39.6205352181844));
#57995=CARTESIAN_POINT('Ctrl Pts',(-3.51183001016619,-5.78440480773054,
39.6288483948653));
#57996=CARTESIAN_POINT('Ctrl Pts',(-3.36520810316052,-5.87342195474662,
39.6369042624758));
#57997=CARTESIAN_POINT('Ctrl Pts',(-3.21533926440627,-5.9567756841761,39.6449601300863));
#57998=CARTESIAN_POINT('Ctrl Pts',(-3.06271740221846,-6.03423989530978,
39.6530159976969));
#57999=CARTESIAN_POINT('Ctrl Pts',(-2.90278329421852,-6.11541548399668,
39.6614578289128));
#58000=CARTESIAN_POINT('Ctrl Pts',(-2.73982631511816,-6.19012312421717,
39.6698996601288));
#58001=CARTESIAN_POINT('Ctrl Pts',(-2.57443460704302,-6.25816070855161,
39.6783414913447));
#58002=CARTESIAN_POINT('Ctrl Pts',(-2.40904289896788,-6.32619829288606,
39.6867833225607));
#58003=CARTESIAN_POINT('Ctrl Pts',(-2.24121692436823,-6.38756574335857,
39.6952251537767));
#58004=CARTESIAN_POINT('Ctrl Pts',(-2.07155830167522,-6.44212194876506,
39.7036669849926));
#58005=CARTESIAN_POINT('Ctrl Pts',(-1.90614776400091,-6.49531212045522,
39.7118974410592));
#58006=CARTESIAN_POINT('Ctrl Pts',(-1.73844521549067,-6.54220532803548,
39.7201278971258));
#58007=CARTESIAN_POINT('Ctrl Pts',(-1.56897070613128,-6.58259978453057,
39.7283583531923));
#58008=CARTESIAN_POINT('Ctrl Pts',(-1.39969737300103,-6.62294629042551,
39.7365790392226));
#58009=CARTESIAN_POINT('Ctrl Pts',(-1.22865661273056,-6.65680932401883,
39.7447997252528));
#58010=CARTESIAN_POINT('Ctrl Pts',(-1.05638602562939,-6.68403602360542,
39.753020411283));
#58011=CARTESIAN_POINT('Ctrl Pts',(-0.884285371057839,-6.71123586601336,
39.7612329881984));
#58012=CARTESIAN_POINT('Ctrl Pts',(-0.710957657292857,-6.73181235564676,
39.7694455651138));
#58013=CARTESIAN_POINT('Ctrl Pts',(-0.53695323243361,-6.7456630679407,39.7776581420292));
#58014=CARTESIAN_POINT('Ctrl Pts',(-0.363085552281877,-6.7595028953873,
39.7858642649339));
#58015=CARTESIAN_POINT('Ctrl Pts',(-0.188542576060101,-6.76662744487597,
39.7940703878385));
#58016=CARTESIAN_POINT('Ctrl Pts',(-0.0138824708663815,-6.76698576007092,
39.8022765107431));
#58017=CARTESIAN_POINT('Ctrl Pts',(0.160675394972847,-6.76734386552185,
39.8104778300969));
#58018=CARTESIAN_POINT('Ctrl Pts',(0.335349895637805,-6.76094362610986,
39.8186791494506));
#58019=CARTESIAN_POINT('Ctrl Pts',(0.509580051723304,-6.74778609403749,
39.8268804688043));
#58020=CARTESIAN_POINT('Ctrl Pts',(0.683760225305153,-6.73463233654932,
39.8350794353939));
#58021=CARTESIAN_POINT('Ctrl Pts',(0.857495950865726,-6.71472517069232,
39.8432784019833));
#58022=CARTESIAN_POINT('Ctrl Pts',(1.03022830809612,-6.68811771974727,39.8514773685729));
#58023=CARTESIAN_POINT('Ctrl Pts',(1.20293785523847,-6.6615137824363,39.8596752524518));
#58024=CARTESIAN_POINT('Ctrl Pts',(1.37464394349423,-6.6282113760114,39.8678731363308));
#58025=CARTESIAN_POINT('Ctrl Pts',(1.54479480779287,-6.58831526278276,39.8760710202097));
#58026=CARTESIAN_POINT('Ctrl Pts',(1.71495411129512,-6.54841717077237,39.8842693106903));
#58027=CARTESIAN_POINT('Ctrl Pts',(1.88355768798516,-6.50192480225152,39.8924676011708));
#58028=CARTESIAN_POINT('Ctrl Pts',(2.05006591133739,-6.44899362375033,39.9006658916513));
#58029=CARTESIAN_POINT('Ctrl Pts',(2.21661263984078,-6.39605020487453,39.9088660779927));
#58030=CARTESIAN_POINT('Ctrl Pts',(2.38106270823189,-6.33666511902945,39.917066264334));
#58031=CARTESIAN_POINT('Ctrl Pts',(2.54289349365061,-6.2710431093997,39.9252664506754));
#58032=CARTESIAN_POINT('Ctrl Pts',(2.70487727737897,-6.20535905930884,39.9334743896495));
#58033=CARTESIAN_POINT('Ctrl Pts',(2.86423649795181,-6.13342643977186,39.9416823286236));
#58034=CARTESIAN_POINT('Ctrl Pts',(3.02046944019675,-6.05549777977315,39.9498902675977));
#58035=CARTESIAN_POINT('Ctrl Pts',(3.17677817577527,-5.97753131422052,39.9581021884916));
#58036=CARTESIAN_POINT('Ctrl Pts',(3.32995729490357,-5.89356318088711,39.9663141093856));
#58037=CARTESIAN_POINT('Ctrl Pts',(3.47953147935324,-5.80389090905316,39.9745260302796));
#58038=CARTESIAN_POINT('Ctrl Pts',(3.6293107811016,-5.71409566590411,39.9827492125221));
#58039=CARTESIAN_POINT('Ctrl Pts',(3.77547496826922,-5.61858084776005,39.9909723947647));
#58040=CARTESIAN_POINT('Ctrl Pts',(3.91757840077306,-5.51768687710678,39.9991955770072));
#58041=CARTESIAN_POINT('Ctrl Pts',(4.04429880004363,-5.42771491780995,40.0065285802901));
#58042=CARTESIAN_POINT('Ctrl Pts',(4.16779034346317,-5.33346607268934,40.0138615835729));
#58043=CARTESIAN_POINT('Ctrl Pts',(4.28776083656118,-5.23520735104658,40.0211945868557));
#58044=CARTESIAN_POINT('Ctrl Pts',(4.43394361090994,-5.11548014010676,40.030129773638));
#58045=CARTESIAN_POINT('Ctrl Pts',(4.57520177472949,-4.98955074287292,40.0390649604202));
#58046=CARTESIAN_POINT('Ctrl Pts',(4.71102716015007,-4.85782997812073,40.0480001472025));
#58047=CARTESIAN_POINT('Ctrl Pts',(4.84664912116181,-4.7263064903254,40.0569219518391));
#58048=CARTESIAN_POINT('Ctrl Pts',(4.97685435412913,-4.5890091214301,40.0658437564758));
#58049=CARTESIAN_POINT('Ctrl Pts',(5.10116897555833,-4.44638775668533,40.0747655611124));
#58050=CARTESIAN_POINT('Ctrl Pts',(5.22518036414416,-4.3041142792724,40.0836656033517));
#58051=CARTESIAN_POINT('Ctrl Pts',(5.34332964903508,-4.15654291920981,40.092565645591));
#58052=CARTESIAN_POINT('Ctrl Pts',(5.45518130116827,-4.00415858469467,40.1014656878302));
#58053=CARTESIAN_POINT('Ctrl Pts',(5.56686075603846,-3.85200884810301,40.1103520283236));
#58054=CARTESIAN_POINT('Ctrl Pts',(5.67226176565813,-3.69506112459502,40.1192383688171));
#58055=CARTESIAN_POINT('Ctrl Pts',(5.77098851009418,-3.53383369959043,40.1281247093105));
#58056=CARTESIAN_POINT('Ctrl Pts',(5.86946282747804,-3.37301850496838,40.1369883289824));
#58057=CARTESIAN_POINT('Ctrl Pts',(5.96129679718971,-3.20794566347558,40.1458519486543));
#58058=CARTESIAN_POINT('Ctrl Pts',(6.04613782496832,-3.03916212161961,40.1547155683262));
#58059=CARTESIAN_POINT('Ctrl Pts',(6.1266777859317,-2.87893516270284,40.1631298414799));
#58060=CARTESIAN_POINT('Ctrl Pts',(6.20091602757362,-2.71536458494684,40.1715441146336));
#58061=CARTESIAN_POINT('Ctrl Pts',(6.26858660046434,-2.54894312068333,40.1799583877873));
#58062=CARTESIAN_POINT('Ctrl Pts',(6.3346163322578,-2.38655695812284,40.1881686359919));
#58063=CARTESIAN_POINT('Ctrl Pts',(6.39432863137815,-2.22161216636013,40.1963788841964));
#58064=CARTESIAN_POINT('Ctrl Pts',(6.44753721662558,-2.05464177905252,40.204589132401));
#58065=CARTESIAN_POINT('Ctrl Pts',(6.50075845061444,-1.88763169955526,40.2128013323452));
#58066=CARTESIAN_POINT('Ctrl Pts',(6.54747278245295,-1.71859540432895,40.2210135322894));
#58067=CARTESIAN_POINT('Ctrl Pts',(6.58754396417207,-1.54808059224971,40.2292257322336));
#58068=CARTESIAN_POINT('Ctrl Pts',(6.62763180716421,-1.37749488149171,40.2374413467441));
#58069=CARTESIAN_POINT('Ctrl Pts',(6.66107091582961,-1.20542977537698,40.2456569612546));
#58070=CARTESIAN_POINT('Ctrl Pts',(6.68777623666107,-1.03244273853398,40.2538725757651));
#58071=CARTESIAN_POINT('Ctrl Pts',(6.71451154639715,-0.859261444831786,
40.2620974160506));
#58072=CARTESIAN_POINT('Ctrl Pts',(6.73449791071248,-0.685156504510114,
40.270322256336));
#58073=CARTESIAN_POINT('Ctrl Pts',(6.74770210147544,-0.510691051168863,
40.2785470966214));
#58074=CARTESIAN_POINT('Ctrl Pts',(6.76091474998158,-0.336113846640106,
40.286777205203));
#58075=CARTESIAN_POINT('Ctrl Pts',(6.7673365519278,-0.161176023548126,40.2950073137846));
#58076=CARTESIAN_POINT('Ctrl Pts',(6.76698641441174,0.0135597627938511,
40.3032374223661));
#58077=CARTESIAN_POINT('Ctrl Pts',(6.76663579685176,0.188535114580424,40.3114788145528));
#58078=CARTESIAN_POINT('Ctrl Pts',(6.75949470964332,0.363307521746561,40.3197202067395));
#58079=CARTESIAN_POINT('Ctrl Pts',(6.74563394985275,0.537318913303875,40.3279615989262));
#58080=CARTESIAN_POINT('Ctrl Pts',(6.73960139503915,0.613053091921744,40.3315484621904));
#58081=CARTESIAN_POINT('Ctrl Pts',(6.73229664967877,0.688643237948223,40.3351353254546));
#58082=CARTESIAN_POINT('Ctrl Pts',(6.72372856026666,0.764044009108428,40.3387221887188));
#58083=CARTESIAN_POINT('Ctrl Pts',(6.70354713635535,0.941644271294464,40.3471707476174));
#58084=CARTESIAN_POINT('Ctrl Pts',(6.67630725626448,1.11859816690005,40.355619306516));
#58085=CARTESIAN_POINT('Ctrl Pts',(6.64206440465825,1.29432200181096,40.3640678654146));
#58086=CARTESIAN_POINT('Ctrl Pts',(6.6078528846049,1.46988505278098,40.3725086940437));
#58087=CARTESIAN_POINT('Ctrl Pts',(6.56665122883549,1.64421996076122,40.3809495226729));
#58088=CARTESIAN_POINT('Ctrl Pts',(6.51856653089795,1.81674967517736,40.389390351302));
#58089=CARTESIAN_POINT('Ctrl Pts',(6.47051843501161,1.98914806004979,40.397824754776));
#58090=CARTESIAN_POINT('Ctrl Pts',(6.41559783096888,2.15974367059655,40.4062591582501));
#58091=CARTESIAN_POINT('Ctrl Pts',(6.35396263276272,2.32797076043817,40.4146935617241));
#58092=CARTESIAN_POINT('Ctrl Pts',(6.29236488592939,2.49609563051501,40.4231228402047));
#58093=CARTESIAN_POINT('Ctrl Pts',(6.22406079385863,2.66185453694141,40.4315521186853));
#58094=CARTESIAN_POINT('Ctrl Pts',(6.14925787681769,2.82469760583246,40.4399813971658));
#58095=CARTESIAN_POINT('Ctrl Pts',(6.07104937984889,2.99495449103902,40.4487944385093));
#58096=CARTESIAN_POINT('Ctrl Pts',(5.98573656891452,3.16202346297437,40.4576074798528));
#58097=CARTESIAN_POINT('Ctrl Pts',(5.89361308808811,3.32529904939639,40.4664205211963));
#58098=CARTESIAN_POINT('Ctrl Pts',(5.80556200177603,3.48135690374288,40.4748439747723));
#58099=CARTESIAN_POINT('Ctrl Pts',(5.71128960475681,3.63394921250901,40.4832674283484));
#58100=CARTESIAN_POINT('Ctrl Pts',(5.61109946859779,3.78257210816946,40.4916908819245));
#58101=CARTESIAN_POINT('Ctrl Pts',(5.51092010916819,3.93117901753833,40.5001134294505));
#58102=CARTESIAN_POINT('Ctrl Pts',(5.40482446599098,4.07581708866082,40.5085359769765));
#58103=CARTESIAN_POINT('Ctrl Pts',(5.29315957063137,4.2160112381057,40.5169585245025));
#58104=CARTESIAN_POINT('Ctrl Pts',(5.18149111520029,4.35620985718439,40.525381340554));
#58105=CARTESIAN_POINT('Ctrl Pts',(5.06425326169615,4.49196401166464,40.5338041566055));
#58106=CARTESIAN_POINT('Ctrl Pts',(4.94183370014266,4.6228312407154,40.542226972657));
#58107=CARTESIAN_POINT('Ctrl Pts',(4.81939316380426,4.75372089193421,40.5506512318337));
#58108=CARTESIAN_POINT('Ctrl Pts',(4.69176937762932,4.87972170546081,40.5590754910104));
#58109=CARTESIAN_POINT('Ctrl Pts',(4.55938754390115,5.00042740418447,40.5674997501871));
#58110=CARTESIAN_POINT('Ctrl Pts',(4.42692011906221,5.1212111448459,40.5759294560455));
#58111=CARTESIAN_POINT('Ctrl Pts',(4.28968874691289,5.23669270582208,40.5843591619038));
#58112=CARTESIAN_POINT('Ctrl Pts',(4.14815314656469,5.34650488381386,40.5927888677621));
#58113=CARTESIAN_POINT('Ctrl Pts',(4.00656615436389,5.4563569348217,40.6012216344631));
#58114=CARTESIAN_POINT('Ctrl Pts',(3.86067208477238,5.56053529876295,40.6096544011641));
#58115=CARTESIAN_POINT('Ctrl Pts',(3.7109608657171,5.65871526524495,40.618087167865));
#58116=CARTESIAN_POINT('Ctrl Pts',(3.56112336055373,5.75697804960752,40.6265270478692));
#58117=CARTESIAN_POINT('Ctrl Pts',(3.40746255645117,5.84923215213074,40.6349669278733));
#58118=CARTESIAN_POINT('Ctrl Pts',(3.25049509572416,5.93519760687656,40.6434068078774));
#58119=CARTESIAN_POINT('Ctrl Pts',(3.20035666026769,5.96265663172346,40.6461026683882));
#58120=CARTESIAN_POINT('Ctrl Pts',(3.1498810270518,5.9894743913875,40.6487985288989));
#58121=CARTESIAN_POINT('Ctrl Pts',(3.0990855038471,6.01564277861018,40.6514943894097));
#58122=CARTESIAN_POINT('Origin',(0.,0.,-63.6971797838103));
#58123=CARTESIAN_POINT('',(3.09908550384712,6.01564277861017,43.045630740225));
#58124=CARTESIAN_POINT('',(3.09908550384717,6.01564277861014,42.6514898562653));
#58125=CARTESIAN_POINT('',(3.09908550384721,6.01564277861012,-63.6971797838103));
#58126=CARTESIAN_POINT('',(-6.76699843322197,0.00460486387876293,41.6971797837852));
#58127=CARTESIAN_POINT('Ctrl Pts',(-6.76699843322233,0.00460486335559169,
41.6971797838098));
#58128=CARTESIAN_POINT('Ctrl Pts',(-6.7671159111045,-0.168032755431752,
41.7052849047448));
#58129=CARTESIAN_POINT('Ctrl Pts',(-6.76062274111126,-0.340827023646455,
41.7133900256798));
#58130=CARTESIAN_POINT('Ctrl Pts',(-6.74750964751565,-0.513227587609325,
41.7214951466149));
#58131=CARTESIAN_POINT('Ctrl Pts',(-6.73636368628527,-0.659765853962388,
41.7283843953685));
#58132=CARTESIAN_POINT('Ctrl Pts',(-6.72043584051447,-0.80601946530117,
41.7352736441221));
#58133=CARTESIAN_POINT('Ctrl Pts',(-6.69975003711939,-0.951650377039166,
41.7421628928757));
#58134=CARTESIAN_POINT('Ctrl Pts',(-6.6750977729527,-1.12520572021015,41.7503731410802));
#58135=CARTESIAN_POINT('Ctrl Pts',(-6.64369867344581,-1.29779320395664,
41.7585833892847));
#58136=CARTESIAN_POINT('Ctrl Pts',(-6.60565998398111,-1.46885846017602,
41.7667936374892));
#58137=CARTESIAN_POINT('Ctrl Pts',(-6.56761225196154,-1.6399643820174,41.7750058374335));
#58138=CARTESIAN_POINT('Ctrl Pts',(-6.52292186269664,-1.80954700792686,
41.7832180373777));
#58139=CARTESIAN_POINT('Ctrl Pts',(-6.47174667829002,-1.97706447341561,
41.7914302373219));
#58140=CARTESIAN_POINT('Ctrl Pts',(-6.42055021565599,-2.14465159131042,
41.7996458518324));
#58141=CARTESIAN_POINT('Ctrl Pts',(-6.36286369011821,-2.31017149797406,
41.8078614663428));
#58142=CARTESIAN_POINT('Ctrl Pts',(-6.29889411857824,-2.47309965083101,
41.8160770808533));
#58143=CARTESIAN_POINT('Ctrl Pts',(-6.23485271201375,-2.63621076486114,
41.8243019211387));
#58144=CARTESIAN_POINT('Ctrl Pts',(-6.16451429729534,-2.79672398057163,
41.8325267614242));
#58145=CARTESIAN_POINT('Ctrl Pts',(-6.08813352982892,-2.95413593508708,
41.8407516017096));
#58146=CARTESIAN_POINT('Ctrl Pts',(-6.01170383782557,-3.11164871743182,
41.8489817102912));
#58147=CARTESIAN_POINT('Ctrl Pts',(-5.92922424502312,-3.26605596551176,
41.8572118188727));
#58148=CARTESIAN_POINT('Ctrl Pts',(-5.84099421978324,-3.41688096433849,
41.8654419274543));
#58149=CARTESIAN_POINT('Ctrl Pts',(-5.75264322982504,-3.56791274655275,
41.873683319641));
#58150=CARTESIAN_POINT('Ctrl Pts',(-5.65852625106592,-3.71535217052858,
41.8819247118277));
#58151=CARTESIAN_POINT('Ctrl Pts',(-5.55898528670911,-3.8587525940583,41.8901661040144));
#58152=CARTESIAN_POINT('Ctrl Pts',(-5.5156625300379,-3.92116410167497,41.8937529672786));
#58153=CARTESIAN_POINT('Ctrl Pts',(-5.47131286370705,-3.98281097164823,
41.8973398305428));
#58154=CARTESIAN_POINT('Ctrl Pts',(-5.4259667489167,-4.04365847218213,41.900926693807));
#58155=CARTESIAN_POINT('Ctrl Pts',(-5.31915854685407,-4.18697862567439,
41.9093751886355));
#58156=CARTESIAN_POINT('Ctrl Pts',(-5.20657598901216,-4.32618844051475,
41.9178236834639));
#58157=CARTESIAN_POINT('Ctrl Pts',(-5.08856073177413,-4.46081143728877,
41.9262721782923));
#58158=CARTESIAN_POINT('Ctrl Pts',(-4.97065327461787,-4.59531146377573,
41.9347129559115));
#58159=CARTESIAN_POINT('Ctrl Pts',(-4.84732322849867,-4.72523277418302,
41.9431537335307));
#58160=CARTESIAN_POINT('Ctrl Pts',(-4.71895350609851,-4.85013059693042,
41.9515945111499));
#58161=CARTESIAN_POINT('Ctrl Pts',(-4.59068130147954,-4.97493353937175,
41.9600288766192));
#58162=CARTESIAN_POINT('Ctrl Pts',(-4.45737729080423,-5.09472036999594,
41.9684632420884));
#58163=CARTESIAN_POINT('Ctrl Pts',(-4.31946261697925,-5.20908165615772,
41.9768976075577));
#58164=CARTESIAN_POINT('Ctrl Pts',(-4.18163153264475,-5.32337362843594,
41.9853268609944));
#58165=CARTESIAN_POINT('Ctrl Pts',(-4.03919561271726,-5.43224640014772,
41.993756114431));
#58166=CARTESIAN_POINT('Ctrl Pts',(-3.89261088277409,-5.53532921471783,
42.0021853678677));
#58167=CARTESIAN_POINT('Ctrl Pts',(-3.74609251153582,-5.63836536384008,
42.0106108053929));
#58168=CARTESIAN_POINT('Ctrl Pts',(-3.59542934765794,-5.73561659085825,
42.0190362429182));
#58169=CARTESIAN_POINT('Ctrl Pts',(-3.4411086590045,-5.82675383012911,42.0274616804434));
#58170=CARTESIAN_POINT('Ctrl Pts',(-3.2868218704568,-5.91787104899911,42.0358852671266));
#58171=CARTESIAN_POINT('Ctrl Pts',(-3.12887944457916,-6.00287678629404,
42.0443088538097));
#58172=CARTESIAN_POINT('Ctrl Pts',(-2.96779611359637,-6.08148626802053,
42.0527324404929));
#58173=CARTESIAN_POINT('Ctrl Pts',(-2.80673080699336,-6.16008695375836,
42.0611550846209));
#58174=CARTESIAN_POINT('Ctrl Pts',(-2.64252559549371,-6.23229266454623,
42.0695777287489));
#58175=CARTESIAN_POINT('Ctrl Pts',(-2.47571848383332,-6.29786527236063,
42.078000372877));
#58176=CARTESIAN_POINT('Ctrl Pts',(-2.3089067764376,-6.36343968677877,42.0864232490589));
#58177=CARTESIAN_POINT('Ctrl Pts',(-2.13949333638898,-6.42238051225617,
42.0948461252408));
#58178=CARTESIAN_POINT('Ctrl Pts',(-1.96803509669743,-6.47449819354111,
42.1032690014228));
#58179=CARTESIAN_POINT('Ctrl Pts',(-1.79654822252821,-6.5266245787681,42.1116932842718));
#58180=CARTESIAN_POINT('Ctrl Pts',(-1.62301618700375,-6.57192545160094,
42.1201175671208));
#58181=CARTESIAN_POINT('Ctrl Pts',(-1.44801034699811,-6.61026134392479,
42.1285418499698));
#58182=CARTESIAN_POINT('Ctrl Pts',(-1.27288631451881,-6.64862312689289,
42.1369718222679));
#58183=CARTESIAN_POINT('Ctrl Pts',(-1.09628681462513,-6.6800104585119,42.1454017945661));
#58184=CARTESIAN_POINT('Ctrl Pts',(-0.918793647272057,-6.70433495834841,
42.1538317668642));
#58185=CARTESIAN_POINT('Ctrl Pts',(-0.741237028976705,-6.72866815380096,
42.1622647527414));
#58186=CARTESIAN_POINT('Ctrl Pts',(-0.562786437325949,-6.74593344387162,
42.1706977386186));
#58187=CARTESIAN_POINT('Ctrl Pts',(-0.384028615301828,-6.75609436158417,
42.1791307244958));
#58188=CARTESIAN_POINT('Ctrl Pts',(-0.205106337170434,-6.76626462727912,
42.1875714686686));
#58189=CARTESIAN_POINT('Ctrl Pts',(-0.0258765972778607,-6.76931744920169,
42.1960122128414));
#58190=CARTESIAN_POINT('Ctrl Pts',(0.15307292701594,-6.76526848536071,42.2044529570142));
#58191=CARTESIAN_POINT('Ctrl Pts',(0.252018898312637,-6.76302970511487,
42.2091200698995));
#58192=CARTESIAN_POINT('Ctrl Pts',(0.350879241127732,-6.75862063444282,
42.2137871827848));
#58193=CARTESIAN_POINT('Ctrl Pts',(0.449555269248574,-6.75205072995537,
42.21845429567));
#58194=CARTESIAN_POINT('Ctrl Pts',(0.621686906146081,-6.74059011043894,
42.2265956628879));
#58195=CARTESIAN_POINT('Ctrl Pts',(0.793599377061357,-6.72252829119632,
42.2347370301057));
#58196=CARTESIAN_POINT('Ctrl Pts',(0.964742383957024,-6.69787736022368,
42.2428783973235));
#58197=CARTESIAN_POINT('Ctrl Pts',(1.1357359960245,-6.67324794763887,42.251012657747));
#58198=CARTESIAN_POINT('Ctrl Pts',(1.30596112122551,-6.642040924175,42.2591469181704));
#58199=CARTESIAN_POINT('Ctrl Pts',(1.47487010898186,-6.60432034062793,42.2672811785939));
#58200=CARTESIAN_POINT('Ctrl Pts',(1.64366387312816,-6.56662548870041,42.2754098901187));
#58201=CARTESIAN_POINT('Ctrl Pts',(1.81114293157273,-6.5224260026454,42.2835386016436));
#58202=CARTESIAN_POINT('Ctrl Pts',(1.9767674269714,-6.47183741604074,42.2916673131684));
#58203=CARTESIAN_POINT('Ctrl Pts',(2.14231293910877,-6.42127295419821,42.2997921482609));
#58204=CARTESIAN_POINT('Ctrl Pts',(2.30600530002384,-6.36432556584715,42.3079169833535));
#58205=CARTESIAN_POINT('Ctrl Pts',(2.46731749392409,-6.30116127266841,42.316041818446));
#58206=CARTESIAN_POINT('Ctrl Pts',(2.62858452802384,-6.23801466251046,42.3241643789682));
#58207=CARTESIAN_POINT('Ctrl Pts',(2.78747238206722,-6.16865474826588,42.3322869394903));
#58208=CARTESIAN_POINT('Ctrl Pts',(2.94347181719057,-6.09329653483275,42.3404095000125));
#58209=CARTESIAN_POINT('Ctrl Pts',(3.09947954327883,-6.01793431630626,42.3485324922277));
#58210=CARTESIAN_POINT('Ctrl Pts',(3.25259821245427,-5.93657331743266,42.3566554844428));
#58211=CARTESIAN_POINT('Ctrl Pts',(3.40234092262927,-5.84947563856814,42.364778476658));
#58212=CARTESIAN_POINT('Ctrl Pts',(3.47878001283058,-5.80501492777115,42.3689250166392));
#58213=CARTESIAN_POINT('Ctrl Pts',(3.55433978964625,-5.75906009934237,42.3730715566205));
#58214=CARTESIAN_POINT('Ctrl Pts',(3.62895815416705,-5.71165052461235,42.3772180966017));
#58215=CARTESIAN_POINT('Ctrl Pts',(3.79062208292333,-5.60893562110648,42.3862017556301));
#58216=CARTESIAN_POINT('Ctrl Pts',(3.94778550942087,-5.49944065792936,42.3951854146585));
#58217=CARTESIAN_POINT('Ctrl Pts',(4.099921306424,-5.38358006173685,42.404169073687));
#58218=CARTESIAN_POINT('Ctrl Pts',(4.25231847111563,-5.26752041826676,42.4131681665465));
#58219=CARTESIAN_POINT('Ctrl Pts',(4.39967055226727,-5.14507342852191,42.4221672594059));
#58220=CARTESIAN_POINT('Ctrl Pts',(4.54148410181434,-5.01669324884108,42.4311663522654));
#58221=CARTESIAN_POINT('Ctrl Pts',(4.68363016450503,-4.88801205351497,42.4401865454829));
#58222=CARTESIAN_POINT('Ctrl Pts',(4.8202115342865,-4.75336999460394,42.4492067387004));
#58223=CARTESIAN_POINT('Ctrl Pts',(4.95077025594302,-4.61325946299034,42.4582269319178));
#58224=CARTESIAN_POINT('Ctrl Pts',(5.08146120099783,-4.47300703437904,42.4672562603396));
#58225=CARTESIAN_POINT('Ctrl Pts',(5.20611715428203,-4.32727524803248,42.4762855887614));
#58226=CARTESIAN_POINT('Ctrl Pts',(5.32431999048377,-4.17659019284092,42.4853149171832));
#58227=CARTESIAN_POINT('Ctrl Pts',(5.44268946885848,-4.02569270209503,42.494356975138));
#58228=CARTESIAN_POINT('Ctrl Pts',(5.55458749173169,-3.86982816795383,42.5033990330928));
#58229=CARTESIAN_POINT('Ctrl Pts',(5.65963750572569,-3.70955419205369,42.5124410910476));
#58230=CARTESIAN_POINT('Ctrl Pts',(5.7508026683128,-3.57046422418131,42.5202880265428));
#58231=CARTESIAN_POINT('Ctrl Pts',(5.83681107249541,-3.42805394440939,42.5281349620379));
#58232=CARTESIAN_POINT('Ctrl Pts',(5.91744409407256,-3.28270382360727,42.535981897533));
#58233=CARTESIAN_POINT('Ctrl Pts',(6.00636479109011,-3.12241423256244,42.5446353618338));
#58234=CARTESIAN_POINT('Ctrl Pts',(6.08882553004275,-2.95840747967115,42.5532888261345));
#58235=CARTESIAN_POINT('Ctrl Pts',(6.16452586860145,-2.79122013021967,42.5619422904353));
#58236=CARTESIAN_POINT('Ctrl Pts',(6.24015647166431,-2.62418679451417,42.5705877831254));
#58237=CARTESIAN_POINT('Ctrl Pts',(6.30903897070218,-2.45397898214835,42.5792332758155));
#58238=CARTESIAN_POINT('Ctrl Pts',(6.37091920020569,-2.28115706264398,42.5878787685056));
#58239=CARTESIAN_POINT('Ctrl Pts',(6.43466099018841,-2.10313609236246,42.5967843460022));
#58240=CARTESIAN_POINT('Ctrl Pts',(6.4909724624241,-1.9223415557936,42.6056899234988));
#58241=CARTESIAN_POINT('Ctrl Pts',(6.53962870314262,-1.73940950469785,42.6145955009954));
#58242=CARTESIAN_POINT('Ctrl Pts',(6.58677432525006,-1.5621569010248,42.6232245891679));
#58243=CARTESIAN_POINT('Ctrl Pts',(6.62673282869204,-1.38289783675792,42.6318536773404));
#58244=CARTESIAN_POINT('Ctrl Pts',(6.65934956475971,-1.20222808748369,42.6404827655129));
#58245=CARTESIAN_POINT('Ctrl Pts',(6.69353393679229,-1.01287493113444,42.6495265876715));
#58246=CARTESIAN_POINT('Ctrl Pts',(6.71965330256688,-0.821972463292397,
42.6585704098301));
#58247=CARTESIAN_POINT('Ctrl Pts',(6.73758934643241,-0.630221230077622,
42.6676142319888));
#58248=CARTESIAN_POINT('Ctrl Pts',(6.75552539029795,-0.43846999686272,42.6766580541474));
#58249=CARTESIAN_POINT('Ctrl Pts',(6.76527804188348,-0.245870378693191,
42.685701876306));
#58250=CARTESIAN_POINT('Ctrl Pts',(6.76679140733531,-0.053132378198996,
42.6947456984647));
#58251=CARTESIAN_POINT('Ctrl Pts',(6.76820135315682,0.126434386798115,42.7031714883145));
#58252=CARTESIAN_POINT('Ctrl Pts',(6.76245923937044,0.306042628603557,42.7115972781643));
#58253=CARTESIAN_POINT('Ctrl Pts',(6.7495899555549,0.485102496254617,42.7200230680141));
#58254=CARTESIAN_POINT('Ctrl Pts',(6.73671768563253,0.66420391181936,42.7284508129306));
#58255=CARTESIAN_POINT('Ctrl Pts',(6.71671497212188,0.842756368876598,42.7368785578472));
#58256=CARTESIAN_POINT('Ctrl Pts',(6.68965862793557,1.02017471135446,42.7453063027637));
#58257=CARTESIAN_POINT('Ctrl Pts',(6.66259234190026,1.19765824617164,42.7537371444536));
#58258=CARTESIAN_POINT('Ctrl Pts',(6.62846730721728,1.37400650792871,42.7621679861436));
#58259=CARTESIAN_POINT('Ctrl Pts',(6.58741160309024,1.54864371999245,42.7705988278335));
#58260=CARTESIAN_POINT('Ctrl Pts',(6.54631817401137,1.72344140136376,42.7790374163909));
#58261=CARTESIAN_POINT('Ctrl Pts',(6.49828142794358,1.89652456892985,42.7874760049483));
#58262=CARTESIAN_POINT('Ctrl Pts',(6.44347985555778,2.0673307309236,42.7959145935056));
#58263=CARTESIAN_POINT('Ctrl Pts',(6.3886495476493,2.23822645612015,42.8043576068859));
#58264=CARTESIAN_POINT('Ctrl Pts',(6.32704744756299,2.40684248162703,42.8128006202662));
#58265=CARTESIAN_POINT('Ctrl Pts',(6.25890071606799,2.5726349967307,42.8212436336465));
#58266=CARTESIAN_POINT('Ctrl Pts',(6.19068239168181,2.73860168842704,42.8296955170008));
#58267=CARTESIAN_POINT('Ctrl Pts',(6.11590583448472,2.90173864103937,42.8381474003551));
#58268=CARTESIAN_POINT('Ctrl Pts',(6.03484524762624,3.06152443028029,42.8465992837094));
#58269=CARTESIAN_POINT('Ctrl Pts',(6.01275367681282,3.10507110585712,42.8489026889383));
#58270=CARTESIAN_POINT('Ctrl Pts',(5.99019562670143,3.14836903081173,42.8512060941672));
#58271=CARTESIAN_POINT('Ctrl Pts',(5.96717721818493,3.19140800380879,42.8535094993961));
#58272=CARTESIAN_POINT('Ctrl Pts',(5.88406764621074,3.34680322244131,42.8618261048869));
#58273=CARTESIAN_POINT('Ctrl Pts',(5.79480385367624,3.49910004449492,42.8701427103777));
#58274=CARTESIAN_POINT('Ctrl Pts',(5.69964289076411,3.64778835978216,42.8784593158685));
#58275=CARTESIAN_POINT('Ctrl Pts',(5.60455801142871,3.79635779503183,42.8867692720246));
#58276=CARTESIAN_POINT('Ctrl Pts',(5.50358554028747,3.94132417917203,42.8950792281806));
#58277=CARTESIAN_POINT('Ctrl Pts',(5.3970282457195,4.08220223836423,42.9033891843367));
#58278=CARTESIAN_POINT('Ctrl Pts',(5.2905384442719,4.22299106575071,42.9116938769877));
#58279=CARTESIAN_POINT('Ctrl Pts',(5.17847107612982,4.35969645089914,42.9199985696386));
#58280=CARTESIAN_POINT('Ctrl Pts',(5.06117210616261,4.49186218753443,42.9283032622896));
#58281=CARTESIAN_POINT('Ctrl Pts',(4.94392795336888,4.6239661593297,42.9366040739194));
#58282=CARTESIAN_POINT('Ctrl Pts',(4.82145730117771,4.75153445063336,42.9449048855492));
#58283=CARTESIAN_POINT('Ctrl Pts',(4.69414639063808,4.87414389029084,42.953205697179));
#58284=CARTESIAN_POINT('Ctrl Pts',(4.56686135994001,4.9967284058247,42.9615048214147));
#58285=CARTESIAN_POINT('Ctrl Pts',(4.43473827917861,5.11435583460496,42.9698039456503));
#58286=CARTESIAN_POINT('Ctrl Pts',(4.29820050075553,5.22663959493143,42.978103069886));
#58287=CARTESIAN_POINT('Ctrl Pts',(4.16168176791428,5.33890769285611,42.9864010364812));
#58288=CARTESIAN_POINT('Ctrl Pts',(4.02074983493964,5.44583338904462,42.9946990030764));
#58289=CARTESIAN_POINT('Ctrl Pts',(3.87586141588145,5.54707015323237,43.0029969696717));
#58290=CARTESIAN_POINT('Ctrl Pts',(3.73093540160447,5.64833318603651,43.0112970893988));
#58291=CARTESIAN_POINT('Ctrl Pts',(3.58205113465018,5.74390413726842,43.0195972091258));
#58292=CARTESIAN_POINT('Ctrl Pts',(3.42969509580122,5.8334792833983,43.0278973288529));
#58293=CARTESIAN_POINT('Ctrl Pts',(3.32119094562956,5.89727245615832,43.0338084659769));
#58294=CARTESIAN_POINT('Ctrl Pts',(3.21092656187111,5.95802549407168,43.039719603101));
#58295=CARTESIAN_POINT('Ctrl Pts',(3.09908550384712,6.01564277861017,43.045630740225));
#58296=CARTESIAN_POINT('Ctrl Pts',(3.09908550384737,6.01564277861004,41.0460412338188));
#58297=CARTESIAN_POINT('Ctrl Pts',(2.94665044189545,6.0941729221307,41.0540826047719));
#58298=CARTESIAN_POINT('Ctrl Pts',(2.79112159957602,6.16696026658,41.0621239757251));
#58299=CARTESIAN_POINT('Ctrl Pts',(2.63298169230085,6.23375459959795,41.0701653466782));
#58300=CARTESIAN_POINT('Ctrl Pts',(2.47261853433126,6.30148797798289,41.07831976932));
#58301=CARTESIAN_POINT('Ctrl Pts',(2.30957067502836,6.36305836293058,41.0864741919618));
#58302=CARTESIAN_POINT('Ctrl Pts',(2.14436518815934,6.41825419719493,41.0946286146036));
#58303=CARTESIAN_POINT('Ctrl Pts',(1.98150303802598,6.4726671129949,41.1026673718489));
#58304=CARTESIAN_POINT('Ctrl Pts',(1.81654443640663,6.52088502335897,41.1107061290943));
#58305=CARTESIAN_POINT('Ctrl Pts',(1.65001184703235,6.56275474969566,41.1187448863396));
#58306=CARTESIAN_POINT('Ctrl Pts',(1.48346194172913,6.60462882961388,41.1267844794487));
#58307=CARTESIAN_POINT('Ctrl Pts',(1.31533808499582,6.64015332005647,41.1348240725577));
#58308=CARTESIAN_POINT('Ctrl Pts',(1.14617489316087,6.66922575073656,41.1428636656668));
#58309=CARTESIAN_POINT('Ctrl Pts',(0.976960617147773,6.69830696075696,41.1509056865853));
#58310=CARTESIAN_POINT('Ctrl Pts',(0.806706749164652,6.72093216955925,41.1589477075039));
#58311=CARTESIAN_POINT('Ctrl Pts',(0.635954870452851,6.73705057148507,41.1669897284225));
#58312=CARTESIAN_POINT('Ctrl Pts',(0.460996292000625,6.75356607169003,41.1752298752273));
#58313=CARTESIAN_POINT('Ctrl Pts',(0.285515264690243,6.76324998340181,41.1834700220322));
#58314=CARTESIAN_POINT('Ctrl Pts',(0.110095320071505,6.76610434596588,41.1917101688371));
#58315=CARTESIAN_POINT('Ctrl Pts',(-0.0614046923037506,6.76889492497402,
41.1997661814079));
#58316=CARTESIAN_POINT('Ctrl Pts',(-0.232845954937012,6.76515801909524,
41.2078221939787));
#58317=CARTESIAN_POINT('Ctrl Pts',(-0.403688049607549,6.75494818326566,
41.2158782065494));
#58318=CARTESIAN_POINT('Ctrl Pts',(-0.580387485856322,6.74438830199777,
41.2242104204714));
#58319=CARTESIAN_POINT('Ctrl Pts',(-0.756445492117974,6.726903815481,41.2325426343933));
#58320=CARTESIAN_POINT('Ctrl Pts',(-0.931275858727255,6.70261249625486,
41.2408748483153));
#58321=CARTESIAN_POINT('Ctrl Pts',(-1.10610622533641,6.67832117702874,41.2492070622372));
#58322=CARTESIAN_POINT('Ctrl Pts',(-1.27970854145619,6.64722318059881,41.2575392761591));
#58323=CARTESIAN_POINT('Ctrl Pts',(-1.45151475646483,6.60949271213494,41.2658714900811));
#58324=CARTESIAN_POINT('Ctrl Pts',(-1.62122277378632,6.57222303015461,41.2741019461476));
#58325=CARTESIAN_POINT('Ctrl Pts',(-1.78974282827711,6.5283583640965,41.2823324022142));
#58326=CARTESIAN_POINT('Ctrl Pts',(-1.95652396937399,6.47798602632524,41.2905628582808));
#58327=CARTESIAN_POINT('Ctrl Pts',(-2.12310713142855,6.42767348348718,41.298783544311));
#58328=CARTESIAN_POINT('Ctrl Pts',(-2.2879551505189,6.37086875375443,41.3070042303412));
#58329=CARTESIAN_POINT('Ctrl Pts',(-2.45052652895091,6.30771026053891,41.3152249163714));
#58330=CARTESIAN_POINT('Ctrl Pts',(-2.61293754242438,6.24461406862908,41.3234374932868));
#58331=CARTESIAN_POINT('Ctrl Pts',(-2.77307605571986,6.17517672389178,41.3316500702022));
#58332=CARTESIAN_POINT('Ctrl Pts',(-2.9304149349874,6.09958665065124,41.3398626471176));
#58333=CARTESIAN_POINT('Ctrl Pts',(-3.08763016648538,6.02405598131646,41.3480687700223));
#58334=CARTESIAN_POINT('Ctrl Pts',(-3.24204982444864,5.94238236875823,41.3562748929269));
#58335=CARTESIAN_POINT('Ctrl Pts',(-3.39316591702405,5.85480264906908,41.3644810158316));
#58336=CARTESIAN_POINT('Ctrl Pts',(-3.54419355201104,5.76727419520257,41.3726823351853));
#58337=CARTESIAN_POINT('Ctrl Pts',(-3.69192116456413,5.67384670065939,41.3808836545391));
#58338=CARTESIAN_POINT('Ctrl Pts',(-3.83586450333802,5.57480336083986,41.3890849738928));
#58339=CARTESIAN_POINT('Ctrl Pts',(-3.97976654817822,5.47578843420806,41.3972839404823));
#58340=CARTESIAN_POINT('Ctrl Pts',(-4.11988618443246,5.37116107103508,41.4054829070719));
#58341=CARTESIAN_POINT('Ctrl Pts',(-4.25576714244758,5.26124842877274,41.4136818736614));
#58342=CARTESIAN_POINT('Ctrl Pts',(-4.39163015676819,5.15135030097146,41.4218797575403));
#58343=CARTESIAN_POINT('Ctrl Pts',(-4.52325532839601,5.03616850895693,41.4300776414193));
#58344=CARTESIAN_POINT('Ctrl Pts',(-4.65021855588829,4.91607123447904,41.4382755252982));
#58345=CARTESIAN_POINT('Ctrl Pts',(-4.77718808054846,4.79596800337327,41.4464738157788));
#58346=CARTESIAN_POINT('Ctrl Pts',(-4.89949493984377,4.67094905051927,41.4546721062593));
#58347=CARTESIAN_POINT('Ctrl Pts',(-5.01675103656091,4.54142026652072,41.4628703967399));
#58348=CARTESIAN_POINT('Ctrl Pts',(-5.13403424883809,4.41186152889402,41.4710705830812));
#58349=CARTESIAN_POINT('Ctrl Pts',(-5.2462641316202,4.27779114877439,41.4792707694225));
#58350=CARTESIAN_POINT('Ctrl Pts',(-5.35309207785388,4.1396490438222,41.4874709557639));
#58351=CARTESIAN_POINT('Ctrl Pts',(-5.46002102152844,4.00137633634913,41.495678894738));
#58352=CARTESIAN_POINT('Ctrl Pts',(-5.56153760556237,3.85902449722819,41.5038868337121));
#58353=CARTESIAN_POINT('Ctrl Pts',(-5.65733533659436,3.7130642183136,41.5120947726862));
#58354=CARTESIAN_POINT('Ctrl Pts',(-5.753179542008,3.56703312964564,41.5203066935801));
#58355=CARTESIAN_POINT('Ctrl Pts',(-5.84329917803921,3.4173904179821,41.5285186144741));
#58356=CARTESIAN_POINT('Ctrl Pts',(-5.92743320698998,3.2646323800196,41.5367305353681));
#58357=CARTESIAN_POINT('Ctrl Pts',(-6.0116826124331,3.11166485860769,41.5449537176106));
#58358=CARTESIAN_POINT('Ctrl Pts',(-6.08992984596416,2.95557379371224,41.5531768998532));
#58359=CARTESIAN_POINT('Ctrl Pts',(-6.16196110076714,2.79687761488281,41.5614000820957));
#58360=CARTESIAN_POINT('Ctrl Pts',(-6.22619480158398,2.65536067338867,41.5687330853785));
#58361=CARTESIAN_POINT('Ctrl Pts',(-6.28548608766533,2.51177254889014,41.5760660886612));
#58362=CARTESIAN_POINT('Ctrl Pts',(-6.33971681340106,2.36649101538121,41.583399091944));
#58363=CARTESIAN_POINT('Ctrl Pts',(-6.41039570506891,2.177145628077,41.5929561933397));
#58364=CARTESIAN_POINT('Ctrl Pts',(-6.47261128120862,1.98456975275513,41.6025132947355));
#58365=CARTESIAN_POINT('Ctrl Pts',(-6.52610743942796,1.78947218169021,41.6120703961312));
#58366=CARTESIAN_POINT('Ctrl Pts',(-6.57946562461814,1.59487779073682,41.6216028486125));
#58367=CARTESIAN_POINT('Ctrl Pts',(-6.62414924673454,1.39777480200119,41.6311353010937));
#58368=CARTESIAN_POINT('Ctrl Pts',(-6.65995207290432,1.19888589391044,41.640667753575));
#58369=CARTESIAN_POINT('Ctrl Pts',(-6.6955405052461,1.00118796873682,41.6501431239989));
#58370=CARTESIAN_POINT('Ctrl Pts',(-6.7223541321133,0.801725566272196,41.6596184944227));
#58371=CARTESIAN_POINT('Ctrl Pts',(-6.7402386003398,0.601225923001824,41.6690938648466));
#58372=CARTESIAN_POINT('Ctrl Pts',(-6.75790903440202,0.403125779288352,
41.6784558378261));
#58373=CARTESIAN_POINT('Ctrl Pts',(-6.76686273816051,0.204013205259285,
41.6878178108057));
#58374=CARTESIAN_POINT('Ctrl Pts',(-6.76699843322198,0.00460486387857811,
41.6971797837852));
#58375=CARTESIAN_POINT('',(-6.76699994849255,0.000834926224110294,41.302820216214));
#58376=CARTESIAN_POINT('Ctrl Pts',(3.0990855038471,6.01564277861018,40.6514943894097));
#58377=CARTESIAN_POINT('Ctrl Pts',(3.069218343977,6.03102947718936,40.6530795231337));
#58378=CARTESIAN_POINT('Ctrl Pts',(3.0392405925958,6.04619167767068,40.6546646568578));
#58379=CARTESIAN_POINT('Ctrl Pts',(3.00915580109585,6.06112781293475,40.6562497905818));
#58380=CARTESIAN_POINT('Ctrl Pts',(2.85463802662748,6.13784093824151,40.6643911577997));
#58381=CARTESIAN_POINT('Ctrl Pts',(2.69698790972868,6.20873922885997,40.6725325250175));
#58382=CARTESIAN_POINT('Ctrl Pts',(2.53668708341959,6.27355621962633,40.6806738922354));
#58383=CARTESIAN_POINT('Ctrl Pts',(2.37652618754003,6.33831663008947,40.6888081526589));
#58384=CARTESIAN_POINT('Ctrl Pts',(2.21371952507958,6.39700617108109,40.6969424130824));
#58385=CARTESIAN_POINT('Ctrl Pts',(2.04877258900682,6.44940461426745,40.7050766735058));
#58386=CARTESIAN_POINT('Ctrl Pts',(1.88393817377604,6.50176731312848,40.7132053850307));
#58387=CARTESIAN_POINT('Ctrl Pts',(1.71696673922693,6.5478473481717,40.7213340965555));
#58388=CARTESIAN_POINT('Ctrl Pts',(1.54838294991314,6.58747290244281,40.7294628080803));
#58389=CARTESIAN_POINT('Ctrl Pts',(1.37987955509287,6.62707956001941,40.7375876431729));
#58390=CARTESIAN_POINT('Ctrl Pts',(1.20976569224582,6.66023778266953,40.7457124782654));
#58391=CARTESIAN_POINT('Ctrl Pts',(1.03858033438825,6.68682584557292,40.7538373133579));
#58392=CARTESIAN_POINT('Ctrl Pts',(0.867442900351693,6.71340646507353,40.7619598738801));
#58393=CARTESIAN_POINT('Ctrl Pts',(0.695234930307182,6.73342053311475,40.7700824344022));
#58394=CARTESIAN_POINT('Ctrl Pts',(0.522504683473259,6.74679760002837,40.7782049949244));
#58395=CARTESIAN_POINT('Ctrl Pts',(0.349765256474587,6.76017537789841,40.7863279871396));
#58396=CARTESIAN_POINT('Ctrl Pts',(0.176503861899764,6.76691541779922,40.7944509793548));
#58397=CARTESIAN_POINT('Ctrl Pts',(0.00327315476795207,6.76699920839791,
40.80257397157));
#58398=CARTESIAN_POINT('Ctrl Pts',(-0.0851558420898549,6.76704198094505,
40.806720511551));
#58399=CARTESIAN_POINT('Ctrl Pts',(-0.173576807295014,6.76535111136654,
40.8108670515321));
#58400=CARTESIAN_POINT('Ctrl Pts',(-0.26191626517331,6.76192937481882,40.8150135915132));
#58401=CARTESIAN_POINT('Ctrl Pts',(-0.453307538849495,6.75451603392019,
40.8239972505416));
#58402=CARTESIAN_POINT('Ctrl Pts',(-0.644221361093534,6.73897891496851,
40.8329809095699));
#58403=CARTESIAN_POINT('Ctrl Pts',(-0.833993664631919,6.71541090085736,
40.8419645685983));
#58404=CARTESIAN_POINT('Ctrl Pts',(-1.02409199497715,6.69180239714766,40.8509636614577));
#58405=CARTESIAN_POINT('Ctrl Pts',(-1.21304464953948,6.66013545144486,40.859962754317));
#58406=CARTESIAN_POINT('Ctrl Pts',(-1.40019667346197,6.62055422722494,40.8689618471764));
#58407=CARTESIAN_POINT('Ctrl Pts',(-1.58778751658146,6.58088019609508,40.8779820403938));
#58408=CARTESIAN_POINT('Ctrl Pts',(-1.77356904672516,6.53325480731981,40.8870022336112));
#58409=CARTESIAN_POINT('Ctrl Pts',(-1.95689774113366,6.47787312555178,40.8960224268285));
#58410=CARTESIAN_POINT('Ctrl Pts',(-2.14041210175138,6.4224353559632,40.9050517552502));
#58411=CARTESIAN_POINT('Ctrl Pts',(-2.32146843701564,6.35922567552714,40.9140810836719));
#58412=CARTESIAN_POINT('Ctrl Pts',(-2.49944068700665,6.28848831215704,40.9231104120936));
#58413=CARTESIAN_POINT('Ctrl Pts',(-2.67766384199675,6.21765122336294,40.9321524700483));
#58414=CARTESIAN_POINT('Ctrl Pts',(-2.85279399561198,6.1392653201658,40.9411945280031));
#58415=CARTESIAN_POINT('Ctrl Pts',(-3.0242251558089,6.05362298189875,40.9502365859578));
#58416=CARTESIAN_POINT('Ctrl Pts',(-3.17299762140804,5.97930031028507,40.9580835214535));
#58417=CARTESIAN_POINT('Ctrl Pts',(-3.31898456659371,5.89951343658971,40.9659304569492));
#58418=CARTESIAN_POINT('Ctrl Pts',(-3.4618056093732,5.81448113961274,40.9737773924449));
#58419=CARTESIAN_POINT('Ctrl Pts',(-3.61930617705035,5.72070899802823,40.9824308567457));
#58420=CARTESIAN_POINT('Ctrl Pts',(-3.77309473582241,5.62047393602927,40.9910843210465));
#58421=CARTESIAN_POINT('Ctrl Pts',(-3.92264165196769,5.51408845324848,40.9997377853474));
#58422=CARTESIAN_POINT('Ctrl Pts',(-4.07205080481473,5.40780097325753,41.0083832780376));
#58423=CARTESIAN_POINT('Ctrl Pts',(-4.21722586162392,5.29537454867129,41.0170287707278));
#58424=CARTESIAN_POINT('Ctrl Pts',(-4.35766520130469,5.17716553659801,41.025674263418));
#58425=CARTESIAN_POINT('Ctrl Pts',(-4.50232941743482,5.05540040931979,41.0345798409145));
#58426=CARTESIAN_POINT('Ctrl Pts',(-4.64196825079845,4.92749950011744,41.043485418411));
#58427=CARTESIAN_POINT('Ctrl Pts',(-4.77606727526543,4.79389928785938,41.0523909959076));
#58428=CARTESIAN_POINT('Ctrl Pts',(-4.90600295955243,4.66444692927855,41.0610200840801));
#58429=CARTESIAN_POINT('Ctrl Pts',(-5.03073741675548,4.52964407580015,41.0696491722527));
#58430=CARTESIAN_POINT('Ctrl Pts',(-5.14983720867053,4.38992775842525,41.0782782604253));
#58431=CARTESIAN_POINT('Ctrl Pts',(-5.27466121274285,4.24349635087574,41.0873220825838));
#58432=CARTESIAN_POINT('Ctrl Pts',(-5.3932953083213,4.09166774730639,41.0963659047423));
#58433=CARTESIAN_POINT('Ctrl Pts',(-5.50528473431925,3.93498780100669,41.1054097269008));
#58434=CARTESIAN_POINT('Ctrl Pts',(-5.6172741603172,3.778307854707,41.1144535490593));
#58435=CARTESIAN_POINT('Ctrl Pts',(-5.72261866449503,3.61677685901155,41.1234973712178));
#58436=CARTESIAN_POINT('Ctrl Pts',(-5.82091267018917,3.45098025002046,41.1325411933763));
#58437=CARTESIAN_POINT('Ctrl Pts',(-5.91248950805211,3.29651376884917,41.1409669832261));
#58438=CARTESIAN_POINT('Ctrl Pts',(-5.99790663143424,3.13841251196621,41.1493927730758));
#58439=CARTESIAN_POINT('Ctrl Pts',(-6.07688873477558,2.97719873457545,41.1578185629256));
#58440=CARTESIAN_POINT('Ctrl Pts',(-6.15588916462177,2.81594755016529,41.166246307842));
#58441=CARTESIAN_POINT('Ctrl Pts',(-6.22845145147225,2.65158270296457,41.1746740527584));
#58442=CARTESIAN_POINT('Ctrl Pts',(-6.29434752276427,2.48464851894011,41.1831017976749));
#58443=CARTESIAN_POINT('Ctrl Pts',(-6.36026780755679,2.31765299497734,41.1915326393648));
#58444=CARTESIAN_POINT('Ctrl Pts',(-6.41951687104965,2.14808655993829,41.1999634810547));
#58445=CARTESIAN_POINT('Ctrl Pts',(-6.47191566315663,1.97651123168777,41.2083943227446));
#58446=CARTESIAN_POINT('Ctrl Pts',(-6.52436260306527,1.80477824761083,41.2168329113019));
#58447=CARTESIAN_POINT('Ctrl Pts',(-6.56994659882727,1.63103299962583,41.2252714998592));
#58448=CARTESIAN_POINT('Ctrl Pts',(-6.60853884934117,1.45585139239845,41.2337100884165));
#58449=CARTESIAN_POINT('Ctrl Pts',(-6.6471513359257,1.28057792767814,41.2421531017967));
#58450=CARTESIAN_POINT('Ctrl Pts',(-6.67876470189843,1.10386692665057,41.2505961151769));
#58451=CARTESIAN_POINT('Ctrl Pts',(-6.70330160567991,0.926302641305302,
41.2590391285571));
#58452=CARTESIAN_POINT('Ctrl Pts',(-6.72786428718906,0.748551812301852,
41.2674910119114));
#58453=CARTESIAN_POINT('Ctrl Pts',(-6.74533561831508,0.569946237354676,
41.2759428952657));
#58454=CARTESIAN_POINT('Ctrl Pts',(-6.75569017492979,0.391074494639017,
41.2843947786199));
#58455=CARTESIAN_POINT('Ctrl Pts',(-6.75851211873265,0.342326293760333,
41.2866981838493));
#58456=CARTESIAN_POINT('Ctrl Pts',(-6.7608057738674,0.293558321921608,41.2890015890787));
#58457=CARTESIAN_POINT('Ctrl Pts',(-6.76257129648251,0.244782474844337,
41.291304994308));
#58458=CARTESIAN_POINT('Ctrl Pts',(-6.7655133731944,0.163502131810913,41.2951434016019));
#58459=CARTESIAN_POINT('Ctrl Pts',(-6.76698991274409,0.0821736906038927,
41.2989818088958));
#58460=CARTESIAN_POINT('Ctrl Pts',(-6.76699994849249,0.000834926739618518,
41.3028202161897));
#58461=CARTESIAN_POINT('Ctrl Pts',(-6.76699994849255,0.000834926224295111,
41.302820216214));
#58462=CARTESIAN_POINT('Ctrl Pts',(-6.76702159771241,-0.174630001529597,
41.311100473087));
#58463=CARTESIAN_POINT('Ctrl Pts',(-6.76021436775829,-0.350273550115445,
41.3193807299599));
#58464=CARTESIAN_POINT('Ctrl Pts',(-6.74656269657631,-0.52552904883085,
41.3276609868328));
#58465=CARTESIAN_POINT('Ctrl Pts',(-6.73292255833172,-0.700636491629351,
41.3359342485414));
#58466=CARTESIAN_POINT('Ctrl Pts',(-6.71244952477012,-0.875356188557083,
41.3442075102499));
#58467=CARTESIAN_POINT('Ctrl Pts',(-6.68518007513384,-1.04912171030509,
41.3524807719585));
#58468=CARTESIAN_POINT('Ctrl Pts',(-6.65792847524227,-1.2227734904762,41.3607486182439));
#58469=CARTESIAN_POINT('Ctrl Pts',(-6.62388937715619,-1.39547199333365,
41.3690164645292));
#58470=CARTESIAN_POINT('Ctrl Pts',(-6.58315107345072,-1.56665597503876,
41.3772843108146));
#58471=CARTESIAN_POINT('Ctrl Pts',(-6.54243168849149,-1.73776045941543,
41.3855483175369));
#58472=CARTESIAN_POINT('Ctrl Pts',(-6.49501937864736,-1.90735148248255,
41.3938123242592));
#58473=CARTESIAN_POINT('Ctrl Pts',(-6.44105354449972,-2.07487788481336,
41.4020763309816));
#58474=CARTESIAN_POINT('Ctrl Pts',(-6.3847966610295,-2.24951640273799,41.4106911753644));
#58475=CARTESIAN_POINT('Ctrl Pts',(-6.32141771498079,-2.42191077070381,
41.4193060197474));
#58476=CARTESIAN_POINT('Ctrl Pts',(-6.25113255705074,-2.59145340575136,
41.4279208641303));
#58477=CARTESIAN_POINT('Ctrl Pts',(-6.18371954334532,-2.75406782274516,
41.4361836700989));
#58478=CARTESIAN_POINT('Ctrl Pts',(-6.10995370878172,-2.91405860628642,
41.4444464760676));
#58479=CARTESIAN_POINT('Ctrl Pts',(-6.03007486180251,-3.07090966344785,
41.4527092820363));
#58480=CARTESIAN_POINT('Ctrl Pts',(-5.95018477644512,-3.22778278842283,
41.4609732505222));
#58481=CARTESIAN_POINT('Ctrl Pts',(-5.8641801242536,-3.38151499281869,41.4692372190082));
#58482=CARTESIAN_POINT('Ctrl Pts',(-5.77234689493559,-3.53161440767922,
41.4775011874941));
#58483=CARTESIAN_POINT('Ctrl Pts',(-5.68048491395558,-3.68176081650563,
41.4857677433096));
#58484=CARTESIAN_POINT('Ctrl Pts',(-5.58279090321834,-3.82827186915964,
41.4940342991251));
#58485=CARTESIAN_POINT('Ctrl Pts',(-5.47959449987094,-3.97068421269989,
41.5023008549406));
#58486=CARTESIAN_POINT('Ctrl Pts',(-5.37634799565992,-4.11316569606644,
41.5105714240896));
#58487=CARTESIAN_POINT('Ctrl Pts',(-5.26759398206475,-4.25154422045178,
41.5188419932387));
#58488=CARTESIAN_POINT('Ctrl Pts',(-5.15370280173387,-4.38538897150531,
41.5271125623877));
#58489=CARTESIAN_POINT('Ctrl Pts',(-5.03967715035149,-4.51939175274485,
41.5353928965785));
#58490=CARTESIAN_POINT('Ctrl Pts',(-4.92050244578517,-4.64884980091141,
41.5436732307692));
#58491=CARTESIAN_POINT('Ctrl Pts',(-4.79658706322744,-4.77336794568355,
41.55195356496));
#58492=CARTESIAN_POINT('Ctrl Pts',(-4.67258598133548,-4.89797220665761,
41.5602396257935));
#58493=CARTESIAN_POINT('Ctrl Pts',(-4.5438379418359,-5.01762951397747,41.5685256866271));
#58494=CARTESIAN_POINT('Ctrl Pts',(-4.41078491776607,-5.13198454880833,
41.5768117474606));
#58495=CARTESIAN_POINT('Ctrl Pts',(-4.27755089760805,-5.24649514428211,
41.5851090800755));
#58496=CARTESIAN_POINT('Ctrl Pts',(-4.1400004714568,-5.35568884362025,41.5934064126903));
#58497=CARTESIAN_POINT('Ctrl Pts',(-3.99860590072931,-5.45925268243308,
41.6017037453052));
#58498=CARTESIAN_POINT('Ctrl Pts',(-3.95811173010324,-5.48891246171598,
41.6040800289271));
#58499=CARTESIAN_POINT('Ctrl Pts',(-3.91730242562021,-5.51811076410782,
41.6064563125491));
#58500=CARTESIAN_POINT('Ctrl Pts',(-3.87618945569539,-5.54684093007505,
41.608832596171));
#58501=CARTESIAN_POINT('Ctrl Pts',(-3.73654292242446,-5.64442736289563,
41.616904009413));
#58502=CARTESIAN_POINT('Ctrl Pts',(-3.59295179309453,-5.73691623808197,
41.6249754226551));
#58503=CARTESIAN_POINT('Ctrl Pts',(-3.44583111845353,-5.82396230268511,
41.6330468358971));
#58504=CARTESIAN_POINT('Ctrl Pts',(-3.29889514163395,-5.91089908816394,
41.6411081161483));
#58505=CARTESIAN_POINT('Ctrl Pts',(-3.14843875307453,-5.9924064714656,41.6491693963995));
#58506=CARTESIAN_POINT('Ctrl Pts',(-2.9949093108269,-6.06817989350368,41.6572306766507));
#58507=CARTESIAN_POINT('Ctrl Pts',(-2.84153894236072,-6.14387480574846,
41.6652836045084));
#58508=CARTESIAN_POINT('Ctrl Pts',(-2.685102188131,-6.21384741588624,41.673336532366));
#58509=CARTESIAN_POINT('Ctrl Pts',(-2.52607448894336,-6.27783694247545,
41.6813894602236));
#58510=CARTESIAN_POINT('Ctrl Pts',(-2.36717673693423,-6.34177418095085,
41.689435807748));
#58511=CARTESIAN_POINT('Ctrl Pts',(-2.20569259806756,-6.3997379281198,41.6974821552723));
#58512=CARTESIAN_POINT('Ctrl Pts',(-2.04212107476457,-6.45151381584217,
41.7055285027967));
#58513=CARTESIAN_POINT('Ctrl Pts',(-1.87864743056523,-6.50325872153675,
41.7135700354899));
#58514=CARTESIAN_POINT('Ctrl Pts',(-1.71308924313668,-6.54882302659542,
41.721611568183));
#58515=CARTESIAN_POINT('Ctrl Pts',(-1.54596430700804,-6.58804093501681,
41.7296531008761));
#58516=CARTESIAN_POINT('Ctrl Pts',(-1.37562643785263,-6.6280127974329,41.7378492299244));
#58517=CARTESIAN_POINT('Ctrl Pts',(-1.20366133405153,-6.66139161775555,
41.7460453589726));
#58518=CARTESIAN_POINT('Ctrl Pts',(-1.03063262690695,-6.68805542653131,
41.7542414880209));
#58519=CARTESIAN_POINT('Ctrl Pts',(-0.860926208888125,-6.71420726892063,
41.7622802448569));
#58520=CARTESIAN_POINT('Ctrl Pts',(-0.690197047214644,-6.73389959282415,
41.770319001693));
#58521=CARTESIAN_POINT('Ctrl Pts',(-0.518985914405807,-6.74706918748047,
41.7783577585291));
#58522=CARTESIAN_POINT('Ctrl Pts',(-0.347758210168852,-6.76024005681436,
41.7863972934319));
#58523=CARTESIAN_POINT('Ctrl Pts',(-0.17604881429155,-6.76688691105645,
41.7944368283347));
#58524=CARTESIAN_POINT('Ctrl Pts',(-0.00440196878264766,-6.76699856824803,
41.8024763632375));
#58525=CARTESIAN_POINT('Ctrl Pts',(0.167295476462347,-6.76711025835501,
41.810518268113));
#58526=CARTESIAN_POINT('Ctrl Pts',(0.338929961368386,-6.76068291650286,
41.8185601729886));
#58527=CARTESIAN_POINT('Ctrl Pts',(0.509959049061346,-6.74775746217071,
41.8266020778641));
#58528=CARTESIAN_POINT('Ctrl Pts',(0.686757338217968,-6.73439600276446,
41.8349152545449));
#58529=CARTESIAN_POINT('Ctrl Pts',(0.862908237529732,-6.71409040300712,
41.8432284312257));
#58530=CARTESIAN_POINT('Ctrl Pts',(1.03782141959566,-6.68694367413308,41.8515416079066));
#58531=CARTESIAN_POINT('Ctrl Pts',(1.20732069672647,-6.66063718958876,41.8595974755171));
#58532=CARTESIAN_POINT('Ctrl Pts',(1.37565738690412,-6.62790690117781,41.8676533431277));
#58533=CARTESIAN_POINT('Ctrl Pts',(1.54230801372537,-6.58889785857988,41.8757092107382));
#58534=CARTESIAN_POINT('Ctrl Pts',(1.71694301664174,-6.54801985891198,41.8841510419542));
#58535=CARTESIAN_POINT('Ctrl Pts',(1.88972595164476,-6.50024679205816,41.8925928731701));
#58536=CARTESIAN_POINT('Ctrl Pts',(2.06007669451811,-6.44580274385614,41.9010347043861));
#58537=CARTESIAN_POINT('Ctrl Pts',(2.23042743739158,-6.39135869565408,41.9094765356021));
#58538=CARTESIAN_POINT('Ctrl Pts',(2.39834558410787,-6.33024390422619,41.9179183668181));
#58539=CARTESIAN_POINT('Ctrl Pts',(2.56327997653748,-6.26273780082497,41.9263601980341));
#58540=CARTESIAN_POINT('Ctrl Pts',(2.72408457402659,-6.19692198384718,41.9345906541006));
#58541=CARTESIAN_POINT('Ctrl Pts',(2.88258802821156,-6.12481253435969,41.9428211101672));
#58542=CARTESIAN_POINT('Ctrl Pts',(3.03826251800127,-6.04658993745306,41.9510515662337));
#58543=CARTESIAN_POINT('Ctrl Pts',(3.19375221299813,-5.9684601953784,41.959272252264));
#58544=CARTESIAN_POINT('Ctrl Pts',(3.34641931321335,-5.88423191491491,41.9674929382942));
#58545=CARTESIAN_POINT('Ctrl Pts',(3.49575407391469,-5.79413431452092,41.9757136243244));
#58546=CARTESIAN_POINT('Ctrl Pts',(3.64494152662763,-5.70412558892214,41.9839262012398));
#58547=CARTESIAN_POINT('Ctrl Pts',(3.79080288120831,-5.60825925737429,41.9921387781551));
#58548=CARTESIAN_POINT('Ctrl Pts',(3.93285111718936,-5.50681133597497,42.0003513550705));
#58549=CARTESIAN_POINT('Ctrl Pts',(4.07478772184563,-5.4054431393662,42.0085574779751));
#58550=CARTESIAN_POINT('Ctrl Pts',(4.21291688604373,-5.29850229706694,42.0167636008798));
#58551=CARTESIAN_POINT('Ctrl Pts',(4.34677874850116,-5.18630923794356,42.0249697237844));
#58552=CARTESIAN_POINT('Ctrl Pts',(4.4805622533377,-5.07418185235132,42.0331710431382));
#58553=CARTESIAN_POINT('Ctrl Pts',(4.61008315853134,-4.95680860427007,42.041372362492));
#58554=CARTESIAN_POINT('Ctrl Pts',(4.7349129404829,-4.83455152481051,42.0495736818457));
#58555=CARTESIAN_POINT('Ctrl Pts',(4.85970691172722,-4.71232951801079,42.0577726484352));
#58556=CARTESIAN_POINT('Ctrl Pts',(4.97981218176148,-4.58522671828342,42.0659716150247));
#58557=CARTESIAN_POINT('Ctrl Pts',(5.09483533201472,-4.45364367003631,42.0741705816143));
#58558=CARTESIAN_POINT('Ctrl Pts',(5.2098432929413,-4.3220779979252,42.0823684654932));
#58559=CARTESIAN_POINT('Ctrl Pts',(5.31977023414561,-4.18603352499365,42.0905663493722));
#58560=CARTESIAN_POINT('Ctrl Pts',(5.42426146289995,-4.0459456968796,42.0987642332511));
#58561=CARTESIAN_POINT('Ctrl Pts',(5.52875787424774,-3.90585092063919,42.1069625237317));
#58562=CARTESIAN_POINT('Ctrl Pts',(5.62781782156914,-3.7617126771366,42.1151608142122));
#58563=CARTESIAN_POINT('Ctrl Pts',(5.72112854872728,-3.6139973891714,42.1233591046927));
#58564=CARTESIAN_POINT('Ctrl Pts',(5.81446085406098,-3.46624794193519,42.131559291034));
#58565=CARTESIAN_POINT('Ctrl Pts',(5.90204109975462,-3.31492010583429,42.1397594773754));
#58566=CARTESIAN_POINT('Ctrl Pts',(5.98360126929088,-3.16050705585996,42.1479596637167));
#58567=CARTESIAN_POINT('Ctrl Pts',(6.06523854756767,-3.00594802046318,42.1561676026908));
#58568=CARTESIAN_POINT('Ctrl Pts',(6.14084421097973,-2.84829826120235,42.1643755416649));
#58569=CARTESIAN_POINT('Ctrl Pts',(6.21019700957568,-2.68807405073917,42.172583480639));
#58570=CARTESIAN_POINT('Ctrl Pts',(6.27958345331552,-2.52777211065692,42.180795401533));
#58571=CARTESIAN_POINT('Ctrl Pts',(6.34271085472138,-2.36489356343775,42.189007322427));
#58572=CARTESIAN_POINT('Ctrl Pts',(6.39940713655381,-2.1999721136015,42.1972192433209));
#58573=CARTESIAN_POINT('Ctrl Pts',(6.45618116835496,-2.03482450012359,42.2054424255635));
#58574=CARTESIAN_POINT('Ctrl Pts',(6.5065063521424,-1.86762872872908,42.213665607806));
#58575=CARTESIAN_POINT('Ctrl Pts',(6.55026093701272,-1.69893221084457,42.2218887900486));
#58576=CARTESIAN_POINT('Ctrl Pts',(6.58927898440913,-1.54849749069047,42.2292217933313));
#58577=CARTESIAN_POINT('Ctrl Pts',(6.62307268442447,-1.39686968340749,42.2365547966141));
#58578=CARTESIAN_POINT('Ctrl Pts',(6.6515904139959,-1.24444122578685,42.2438877998968));
#58579=CARTESIAN_POINT('Ctrl Pts',(6.68633896523764,-1.05870876566714,42.252822986679));
#58580=CARTESIAN_POINT('Ctrl Pts',(6.71332601968396,-0.871402116491395,
42.2617581734613));
#58581=CARTESIAN_POINT('Ctrl Pts',(6.73242731649758,-0.683162812276314,
42.2706933602435));
#58582=CARTESIAN_POINT('Ctrl Pts',(6.75150000547755,-0.495205432307076,
42.2796151648801));
#58583=CARTESIAN_POINT('Ctrl Pts',(6.76271047669215,-0.306318440875435,
42.2885369695166));
#58584=CARTESIAN_POINT('Ctrl Pts',(6.76598585572273,-0.117151185056005,
42.2974587741532));
#58585=CARTESIAN_POINT('Ctrl Pts',(6.76925324532711,0.0715546469659966,
42.3063588163924));
#58586=CARTESIAN_POINT('Ctrl Pts',(6.76462416870618,0.260539121144108,42.3152588586317));
#58587=CARTESIAN_POINT('Ctrl Pts',(6.75207764811812,0.449150791810227,42.3241589008709));
#58588=CARTESIAN_POINT('Ctrl Pts',(6.73955044308297,0.637472092036088,42.3330452413643));
#58589=CARTESIAN_POINT('Ctrl Pts',(6.7191301250787,0.825421477125606,42.3419315818577));
#58590=CARTESIAN_POINT('Ctrl Pts',(6.69084758979494,1.0123475342664,42.350817922351));
#58591=CARTESIAN_POINT('Ctrl Pts',(6.66263736801696,1.19879565410852,42.3596815420229));
#58592=CARTESIAN_POINT('Ctrl Pts',(6.62660508041631,1.38422541235042,42.3685451616948));
#58593=CARTESIAN_POINT('Ctrl Pts',(6.58283314977905,1.56799130168828,42.3774087813667));
#58594=CARTESIAN_POINT('Ctrl Pts',(6.54128026343128,1.74244106899538,42.3858230545206));
#58595=CARTESIAN_POINT('Ctrl Pts',(6.49275295455914,1.91539120841361,42.3942373276746));
#58596=CARTESIAN_POINT('Ctrl Pts',(6.43736502764553,2.08629348387188,42.4026516008285));
#58597=CARTESIAN_POINT('Ctrl Pts',(6.3833201185753,2.2530518092276,42.4108618490331));
#58598=CARTESIAN_POINT('Ctrl Pts',(6.32279423564831,2.41769979886549,42.4190720972376));
#58599=CARTESIAN_POINT('Ctrl Pts',(6.25598808775781,2.57970968247056,42.4272823454422));
#58600=CARTESIAN_POINT('Ctrl Pts',(6.18916605871436,2.74175807905419,42.4354945453863));
#58601=CARTESIAN_POINT('Ctrl Pts',(6.11606092603107,2.9011667911064,42.4437067453305));
#58602=CARTESIAN_POINT('Ctrl Pts',(6.03692112188408,3.05742904548085,42.4519189452747));
#58603=CARTESIAN_POINT('Ctrl Pts',(5.95774841204665,3.21375627243673,42.4601345597852));
#58604=CARTESIAN_POINT('Ctrl Pts',(5.87253619262379,3.3669341180665,42.4683501742958));
#58605=CARTESIAN_POINT('Ctrl Pts',(5.78157835265737,3.51648130267796,42.4765657888063));
#58606=CARTESIAN_POINT('Ctrl Pts',(5.6905183710241,3.66619642222185,42.4847906290917));
#58607=CARTESIAN_POINT('Ctrl Pts',(5.593700066994,3.81227243328368,42.4930154693771));
#58608=CARTESIAN_POINT('Ctrl Pts',(5.49146063118123,3.95425709029986,42.5012403096626));
#58609=CARTESIAN_POINT('Ctrl Pts',(5.38915570745532,4.09633269342515,42.5094704182442));
#58610=CARTESIAN_POINT('Ctrl Pts',(5.281422948332,4.23431143852898,42.5177005268258));
#58611=CARTESIAN_POINT('Ctrl Pts',(5.1686391247196,4.36777501691855,42.5259306354074));
#58612=CARTESIAN_POINT('Ctrl Pts',(5.0557006727549,4.50142157592145,42.5341720275941));
#58613=CARTESIAN_POINT('Ctrl Pts',(4.93769756359107,4.63054034164055,42.5424134197808));
#58614=CARTESIAN_POINT('Ctrl Pts',(4.81504331682191,4.75474992582456,42.5506548119675));
#58615=CARTESIAN_POINT('Ctrl Pts',(4.76166107241942,4.80880909258559,42.5542416752316));
#58616=CARTESIAN_POINT('Ctrl Pts',(4.70739823009763,4.86193887165618,42.5578285384958));
#58617=CARTESIAN_POINT('Ctrl Pts',(4.65229075505896,4.91411026844056,42.5614154017599));
#58618=CARTESIAN_POINT('Ctrl Pts',(4.52249896975261,5.03698686051487,42.5698633552613));
#58619=CARTESIAN_POINT('Ctrl Pts',(4.38772373593038,5.15482456114658,42.5783113087626));
#58620=CARTESIAN_POINT('Ctrl Pts',(4.24838326576361,5.26721260508628,42.586759262264));
#58621=CARTESIAN_POINT('Ctrl Pts',(4.10915498731491,5.37951015839015,42.5952004137902));
#58622=CARTESIAN_POINT('Ctrl Pts',(3.96536905461369,5.48636658937178,42.6036415653164));
#58623=CARTESIAN_POINT('Ctrl Pts',(3.81747902898346,5.58740931588796,42.6120827168425));
#58624=CARTESIAN_POINT('Ctrl Pts',(3.66971391030278,5.68836670237739,42.6205167390273));
#58625=CARTESIAN_POINT('Ctrl Pts',(3.51785188528157,5.78351998852695,42.628950761212));
#58626=CARTESIAN_POINT('Ctrl Pts',(3.36237800086015,5.87253805260823,42.6373847833968));
#58627=CARTESIAN_POINT('Ctrl Pts',(3.27570640570748,5.92216270590637,42.6420864743529));
#58628=CARTESIAN_POINT('Ctrl Pts',(3.18791291542018,5.96988146038011,42.6467881653091));
#58629=CARTESIAN_POINT('Ctrl Pts',(3.09908550384717,6.01564277861014,42.6514898562653));
#58630=CARTESIAN_POINT('Origin',(0.,0.,-63.6971797838103));
#58631=CARTESIAN_POINT('',(3.09908550384733,6.01564277861006,45.0456868593144));
#58632=CARTESIAN_POINT('',(3.09908550384713,6.01564277861016,44.6513967904261));
#58633=CARTESIAN_POINT('',(3.09908550384721,6.01564277861012,-63.6971797838103));
#58634=CARTESIAN_POINT('',(-6.76699891035573,-0.00384021409550919,43.6971797838495));
#58635=CARTESIAN_POINT('Ctrl Pts',(-6.76699891035574,-0.00384021409532003,
43.6971797838495));
#58636=CARTESIAN_POINT('Ctrl Pts',(-6.76688889412393,-0.197704332677314,
43.7062639835883));
#58637=CARTESIAN_POINT('Ctrl Pts',(-6.75844393087704,-0.391285946385338,
43.7153481833271));
#58638=CARTESIAN_POINT('Ctrl Pts',(-6.74176126980812,-0.583904085372994,
43.7244323830658));
#58639=CARTESIAN_POINT('Ctrl Pts',(-6.72503138903265,-0.777067423472387,
43.7335422953239));
#58640=CARTESIAN_POINT('Ctrl Pts',(-6.70001720613928,-0.969261620986978,
43.7426522075821));
#58641=CARTESIAN_POINT('Ctrl Pts',(-6.66686713123509,-1.1598153536047,43.7517621198402));
#58642=CARTESIAN_POINT('Ctrl Pts',(-6.63357584368091,-1.35118080678795,
43.7609108384918));
#58643=CARTESIAN_POINT('Ctrl Pts',(-6.59207929180269,-1.54089158702463,
43.7700595571434));
#58644=CARTESIAN_POINT('Ctrl Pts',(-6.54257710767204,-1.72828637388765,
43.779208275795));
#58645=CARTESIAN_POINT('Ctrl Pts',(-6.49408878146193,-1.91184311416213,
43.7881696188585));
#58646=CARTESIAN_POINT('Ctrl Pts',(-6.43791966665236,-2.09317765977988,
43.7971309619219));
#58647=CARTESIAN_POINT('Ctrl Pts',(-6.37430158871318,-2.2716884152825,43.8060923049854));
#58648=CARTESIAN_POINT('Ctrl Pts',(-6.31086919860206,-2.44967813532555,
43.8150274917677));
#58649=CARTESIAN_POINT('Ctrl Pts',(-6.23993743073889,-2.62512261726111,
43.82396267855));
#58650=CARTESIAN_POINT('Ctrl Pts',(-6.16172172418814,-2.79740493916558,
43.8328978653323));
#58651=CARTESIAN_POINT('Ctrl Pts',(-6.08362316056912,-2.96942923544882,
43.841819669969));
#58652=CARTESIAN_POINT('Ctrl Pts',(-5.99826253221266,-3.13830058685223,
43.8507414746057));
#58653=CARTESIAN_POINT('Ctrl Pts',(-5.90590361626398,-3.30342117741593,
43.8596632792425));
#58654=CARTESIAN_POINT('Ctrl Pts',(-5.81376998561476,-3.46813899969992,
43.8685633214818));
#58655=CARTESIAN_POINT('Ctrl Pts',(-5.71467226302677,-3.62912409593327,
43.8774633637211));
#58656=CARTESIAN_POINT('Ctrl Pts',(-5.60892012914344,-3.78580295114386,
43.8863634059605));
#58657=CARTESIAN_POINT('Ctrl Pts',(-5.50333080222544,-3.94224059695269,
43.8952497464539));
#58658=CARTESIAN_POINT('Ctrl Pts',(-5.39110764306521,-4.09438501285902,
43.9041360869474));
#58659=CARTESIAN_POINT('Ctrl Pts',(-5.27260514316644,-4.24168881511302,
43.9130224274408));
#58660=CARTESIAN_POINT('Ctrl Pts',(-5.15440563347442,-4.3886159872576,43.9218860471127));
#58661=CARTESIAN_POINT('Ctrl Pts',(-5.02995898159621,-4.53072704181745,
43.9307496667846));
#58662=CARTESIAN_POINT('Ctrl Pts',(-4.89966123547151,-4.66750562695085,
43.9396132864566));
#58663=CARTESIAN_POINT('Ctrl Pts',(-4.77596901178222,-4.79735013962594,
43.94802755961));
#58664=CARTESIAN_POINT('Ctrl Pts',(-4.64700432697074,-4.92238917552397,
43.9564418327634));
#58665=CARTESIAN_POINT('Ctrl Pts',(-4.51314140094846,-5.04220623289498,
43.9648561059167));
#58666=CARTESIAN_POINT('Ctrl Pts',(-4.38252431400659,-5.15911802815295,
43.9730663541212));
#58667=CARTESIAN_POINT('Ctrl Pts',(-4.24736849838787,-5.27094489657062,
43.9812766023257));
#58668=CARTESIAN_POINT('Ctrl Pts',(-4.10811297565561,-5.37733175276085,
43.9894868505303));
#58669=CARTESIAN_POINT('Ctrl Pts',(-3.96882434910982,-5.48374389922739,
43.9976990504744));
#58670=CARTESIAN_POINT('Ctrl Pts',(-3.8254343566595,-5.58471324094904,44.0059112504186));
#58671=CARTESIAN_POINT('Ctrl Pts',(-3.67841269500965,-5.6799268520987,44.0141234503628));
#58672=CARTESIAN_POINT('Ctrl Pts',(-3.53132990294273,-5.77518005229731,
44.0223390648732));
#58673=CARTESIAN_POINT('Ctrl Pts',(-3.38061273190973,-5.86467256084481,
44.0305546793837));
#58674=CARTESIAN_POINT('Ctrl Pts',(-3.22675733264959,-5.94813635655674,
44.0387702938941));
#58675=CARTESIAN_POINT('Ctrl Pts',(-3.07272916052049,-6.03169387845254,
44.0469951341795));
#58676=CARTESIAN_POINT('Ctrl Pts',(-2.91555603440391,-6.10920899587778,
44.0552199744649));
#58677=CARTESIAN_POINT('Ctrl Pts',(-2.75575691486018,-6.18046056748203,
44.0634448147503));
#58678=CARTESIAN_POINT('Ctrl Pts',(-2.59585543842534,-6.25175777819479,
44.0716749233318));
#58679=CARTESIAN_POINT('Ctrl Pts',(-2.43332494512286,-6.31678331344898,
44.0799050319133));
#58680=CARTESIAN_POINT('Ctrl Pts',(-2.26870152245154,-6.37536527596859,
44.0881351404949));
#58681=CARTESIAN_POINT('Ctrl Pts',(-2.10385239854164,-6.43402755525774,
44.0963765326815));
#58682=CARTESIAN_POINT('Ctrl Pts',(-1.93690495258762,-6.48622851044388,
44.1046179248682));
#58683=CARTESIAN_POINT('Ctrl Pts',(-1.76840845069959,-6.53184664176175,
44.1128593170549));
#58684=CARTESIAN_POINT('Ctrl Pts',(-1.69507449217272,-6.55170081150803,
44.1164461803194));
#58685=CARTESIAN_POINT('Ctrl Pts',(-1.62144721854119,-6.57030871465975,
44.1200330435839));
#58686=CARTESIAN_POINT('Ctrl Pts',(-1.54757229995239,-6.58766339276834,
44.1236199068484));
#58687=CARTESIAN_POINT('Ctrl Pts',(-1.37356737653549,-6.62854058753074,
44.1320684016769));
#58688=CARTESIAN_POINT('Ctrl Pts',(-1.19779126771295,-6.66255476759419,
44.1405168965053));
#58689=CARTESIAN_POINT('Ctrl Pts',(-1.02081218703135,-6.68956138164591,
44.1489653913337));
#58690=CARTESIAN_POINT('Ctrl Pts',(-0.843994766459049,-6.71654332672453,
44.1574061689529));
#58691=CARTESIAN_POINT('Ctrl Pts',(-0.665976892409825,-6.73653041487473,
44.1658469465721));
#58692=CARTESIAN_POINT('Ctrl Pts',(-0.487337925993888,-6.7494289199819,
44.1742877241913));
#58693=CARTESIAN_POINT('Ctrl Pts',(-0.30883466506351,-6.76231762656675,
44.1827220896606));
#58694=CARTESIAN_POINT('Ctrl Pts',(-0.129711583760677,-6.76812846110855,
44.1911564551299));
#58695=CARTESIAN_POINT('Ctrl Pts',(0.0494454626071732,-6.76681935226792,
44.1995908205993));
#58696=CARTESIAN_POINT('Ctrl Pts',(0.22849392265844,-6.76551103687253,44.2080200740359));
#58697=CARTESIAN_POINT('Ctrl Pts',(0.407575974118805,-6.75709138424464,
44.2164493274725));
#58698=CARTESIAN_POINT('Ctrl Pts',(0.58610397752143,-6.74157037547882,44.2248785809091));
#58699=CARTESIAN_POINT('Ctrl Pts',(0.76455116154374,-6.7260563930522,44.2333040184344));
#58700=CARTESIAN_POINT('Ctrl Pts',(0.942444466007396,-6.70344749362747,
44.2417294559597));
#58701=CARTESIAN_POINT('Ctrl Pts',(1.11919919384768,-6.673805673264,44.2501548934849));
#58702=CARTESIAN_POINT('Ctrl Pts',(1.29591509342742,-6.64417036441135,44.2585784801681));
#58703=CARTESIAN_POINT('Ctrl Pts',(1.47149258608872,-6.60750526743822,44.2670020668513));
#58704=CARTESIAN_POINT('Ctrl Pts',(1.64535448228701,-6.5639239504749,44.2754256535345));
#58705=CARTESIAN_POINT('Ctrl Pts',(1.81919692425085,-6.52034751003241,44.2838482976625));
#58706=CARTESIAN_POINT('Ctrl Pts',(1.99132382911603,-6.46985647344597,44.2922709417905));
#58707=CARTESIAN_POINT('Ctrl Pts',(2.16117023800555,-6.41261508297193,44.3006935859185));
#58708=CARTESIAN_POINT('Ctrl Pts',(2.33102132636682,-6.3553721154291,44.3091164621004));
#58709=CARTESIAN_POINT('Ctrl Pts',(2.49859147766921,-6.29137853005043,44.3175393382824));
#58710=CARTESIAN_POINT('Ctrl Pts',(2.66333252815353,-6.22084792005715,44.3259622144643));
#58711=CARTESIAN_POINT('Ctrl Pts',(2.82810109130764,-6.15030553106053,44.3343864973133));
#58712=CARTESIAN_POINT('Ctrl Pts',(2.99003930545369,-6.07322407264201,44.3428107801623));
#58713=CARTESIAN_POINT('Ctrl Pts',(3.1486202233711,-5.98986474713566,44.3512350630113));
#58714=CARTESIAN_POINT('Ctrl Pts',(3.30730824097709,-5.90644912382299,44.3596650353095));
#58715=CARTESIAN_POINT('Ctrl Pts',(3.46263413618509,-5.81674731655718,44.3680950076077));
#58716=CARTESIAN_POINT('Ctrl Pts',(3.61409586825149,-5.72106633898678,44.3765249799058));
#58717=CARTESIAN_POINT('Ctrl Pts',(3.76561174544246,-5.62535115701121,44.384957965783));
#58718=CARTESIAN_POINT('Ctrl Pts',(3.91326042653645,-5.52365272598554,44.3933909516602));
#58719=CARTESIAN_POINT('Ctrl Pts',(4.05656951705068,-5.41632096107083,44.4018239375374));
#58720=CARTESIAN_POINT('Ctrl Pts',(4.20001045105504,-5.30889045158634,44.4102646817103));
#58721=CARTESIAN_POINT('Ctrl Pts',(4.33910355456252,-5.19581645837651,44.4187054258831));
#58722=CARTESIAN_POINT('Ctrl Pts',(4.47340928254556,-5.07748937870235,44.4271461700559));
#58723=CARTESIAN_POINT('Ctrl Pts',(4.54767050652973,-5.01206317611936,44.431813282941));
#58724=CARTESIAN_POINT('Ctrl Pts',(4.62046872254336,-4.94503163854069,44.4364803958261));
#58725=CARTESIAN_POINT('Ctrl Pts',(4.69173451581017,-4.87646554721301,44.4411475087112));
#58726=CARTESIAN_POINT('Ctrl Pts',(4.81605141307395,-4.75685804211657,44.449288875929));
#58727=CARTESIAN_POINT('Ctrl Pts',(4.93594998097428,-4.63234113408405,44.4574302431468));
#58728=CARTESIAN_POINT('Ctrl Pts',(5.05101697431889,-4.50327841967855,44.4655716103647));
#58729=CARTESIAN_POINT('Ctrl Pts',(5.16598352292975,-4.37432836720682,44.4737058707881));
#58730=CARTESIAN_POINT('Ctrl Pts',(5.27612665022993,-4.24084067836807,44.4818401312116));
#58731=CARTESIAN_POINT('Ctrl Pts',(5.38106859648469,-4.10321700132059,44.489974391635));
#58732=CARTESIAN_POINT('Ctrl Pts',(5.48593895513416,-3.96568720617469,44.4981031031598));
#58733=CARTESIAN_POINT('Ctrl Pts',(5.58561497575892,-3.82402733007337,44.5062318146846));
#58734=CARTESIAN_POINT('Ctrl Pts',(5.67975801198224,-3.67867339204279,44.5143605262093));
#58735=CARTESIAN_POINT('Ctrl Pts',(5.77385615313152,-3.53338877061884,44.5224853613018));
#58736=CARTESIAN_POINT('Ctrl Pts',(5.86242636564597,-3.38441390187614,44.5306101963943));
#58737=CARTESIAN_POINT('Ctrl Pts',(5.94517233844275,-3.23221516397272,44.5387350314868));
#58738=CARTESIAN_POINT('Ctrl Pts',(6.0278951462725,-3.0800590345326,44.5468575920089));
#58739=CARTESIAN_POINT('Ctrl Pts',(6.10479678808972,-2.92468115530904,44.5549801525311));
#58740=CARTESIAN_POINT('Ctrl Pts',(6.1756260950989,-2.76657393422506,44.5631027130532));
#58741=CARTESIAN_POINT('Ctrl Pts',(6.246459166502,-2.60845831015246,44.5712257052683));
#58742=CARTESIAN_POINT('Ctrl Pts',(6.31121910514574,-2.44761338690518,44.5793486974835));
#58743=CARTESIAN_POINT('Ctrl Pts',(6.36970215766022,-2.28455322168226,44.5874716896986));
#58744=CARTESIAN_POINT('Ctrl Pts',(6.39955597372514,-2.20131597651837,44.5916182296801));
#58745=CARTESIAN_POINT('Ctrl Pts',(6.42777494090506,-2.11750180098473,44.5957647696615));
#58746=CARTESIAN_POINT('Ctrl Pts',(6.45433689979305,-2.03318080454491,44.5999113096429));
#58747=CARTESIAN_POINT('Ctrl Pts',(6.5118845377867,-1.85049570218309,44.6088949686714));
#58748=CARTESIAN_POINT('Ctrl Pts',(6.56162305658886,-1.66552119221636,44.6178786276999));
#58749=CARTESIAN_POINT('Ctrl Pts',(6.60341601288126,-1.47891377734583,44.6268622867283));
#58750=CARTESIAN_POINT('Ctrl Pts',(6.64528076902984,-1.29198577291342,44.6358613795878));
#58751=CARTESIAN_POINT('Ctrl Pts',(6.67917262709894,-1.10341948994128,44.6448604724474));
#58752=CARTESIAN_POINT('Ctrl Pts',(6.70500649420441,-0.913880141307793,
44.6538595653069));
#58753=CARTESIAN_POINT('Ctrl Pts',(6.730900934509,-0.72389637586825,44.6628797585243));
#58754=CARTESIAN_POINT('Ctrl Pts',(6.74869954840513,-0.532935217663735,
44.6718999517418));
#58755=CARTESIAN_POINT('Ctrl Pts',(6.75836901832327,-0.341668277965887,
44.6809201449593));
#58756=CARTESIAN_POINT('Ctrl Pts',(6.76804828100098,-0.150207632597564,
44.6899494733811));
#58757=CARTESIAN_POINT('Ctrl Pts',(6.76958194657552,0.0415591739957861,
44.6989788018029));
#58758=CARTESIAN_POINT('Ctrl Pts',(6.76298886987241,0.232960395736803,44.7080081302247));
#58759=CARTESIAN_POINT('Ctrl Pts',(6.75638649826011,0.42463145462011,44.7170501881796));
#58760=CARTESIAN_POINT('Ctrl Pts',(6.74163448406952,0.615935658974207,44.7260922461344));
#58761=CARTESIAN_POINT('Ctrl Pts',(6.71880378020087,0.806203921572273,44.7351343040893));
#58762=CARTESIAN_POINT('Ctrl Pts',(6.69899069545212,0.971323719610178,44.7429812395843));
#58763=CARTESIAN_POINT('Ctrl Pts',(6.67309419700013,1.13566332147699,44.7508281750793));
#58764=CARTESIAN_POINT('Ctrl Pts',(6.6411920100604,1.29879085518415,44.7586751105743));
#58765=CARTESIAN_POINT('Ctrl Pts',(6.60601083188276,1.47868506870226,44.767328574875));
#58766=CARTESIAN_POINT('Ctrl Pts',(6.56349363194616,1.65726355612998,44.7759820391758));
#58767=CARTESIAN_POINT('Ctrl Pts',(6.51375604940836,1.83392233445042,44.7846355034765));
#58768=CARTESIAN_POINT('Ctrl Pts',(6.46406428535748,2.01041837390193,44.7932809961666));
#58769=CARTESIAN_POINT('Ctrl Pts',(6.40716548729329,2.18499793983939,44.8019264888567));
#58770=CARTESIAN_POINT('Ctrl Pts',(6.34322602845369,2.35706863539178,44.8105719815468));
#58771=CARTESIAN_POINT('Ctrl Pts',(6.27736306075519,2.53431578243841,44.8194775590434));
#58772=CARTESIAN_POINT('Ctrl Pts',(6.20402925680783,2.70890043112542,44.82838313654));
#58773=CARTESIAN_POINT('Ctrl Pts',(6.12346210347251,2.88019111646017,44.8372887140366));
#58774=CARTESIAN_POINT('Ctrl Pts',(6.04539629918276,3.04616378105642,44.8459178022091));
#58775=CARTESIAN_POINT('Ctrl Pts',(5.96053968343559,3.20904364133053,44.8545468903816));
#58776=CARTESIAN_POINT('Ctrl Pts',(5.86915756771335,3.36827529239419,44.8631759785541));
#58777=CARTESIAN_POINT('Ctrl Pts',(5.77338341561825,3.53515998582456,44.8722198007128));
#58778=CARTESIAN_POINT('Ctrl Pts',(5.67044115448376,3.6980368238629,44.8812636228714));
#58779=CARTESIAN_POINT('Ctrl Pts',(5.56069135782519,3.85629363806859,44.8903074450301));
#58780=CARTESIAN_POINT('Ctrl Pts',(5.45094156116662,4.01455045227428,44.8993512671887));
#58781=CARTESIAN_POINT('Ctrl Pts',(5.33438442010266,4.16818690627899,44.9083950893474));
#58782=CARTESIAN_POINT('Ctrl Pts',(5.21143435583699,4.31662379120557,44.9174389115061));
#58783=CARTESIAN_POINT('Ctrl Pts',(5.09689635502667,4.45490484170802,44.9258639685886));
#58784=CARTESIAN_POINT('Ctrl Pts',(4.97686061622874,4.58861306477576,44.9342890256711));
#58785=CARTESIAN_POINT('Ctrl Pts',(4.85172589363782,4.71731330876001,44.9427140827536));
#58786=CARTESIAN_POINT('Ctrl Pts',(4.72427403878008,4.84839670812998,44.951295147467));
#58787=CARTESIAN_POINT('Ctrl Pts',(4.59153275331571,4.97428458065801,44.9598762121804));
#58788=CARTESIAN_POINT('Ctrl Pts',(4.45396213209447,5.09455693126188,44.9684572768938));
#58789=CARTESIAN_POINT('Ctrl Pts',(4.31877156467922,5.21274849845961,44.9768898840692));
#58790=CARTESIAN_POINT('Ctrl Pts',(4.17891768344854,5.32551707867113,44.9853224912446));
#58791=CARTESIAN_POINT('Ctrl Pts',(4.03487008848478,5.43250516511958,44.99375509842));
#58792=CARTESIAN_POINT('Ctrl Pts',(3.88701851851171,5.54231856779246,45.0024103919024));
#58793=CARTESIAN_POINT('Ctrl Pts',(3.73474899182892,5.64604174992405,45.0110656853848));
#58794=CARTESIAN_POINT('Ctrl Pts',(3.57860057541301,5.74333587052452,45.0197209788672));
#58795=CARTESIAN_POINT('Ctrl Pts',(3.4224521589971,5.84062999112499,45.0283762723496));
#58796=CARTESIAN_POINT('Ctrl Pts',(3.26242519189843,5.93149488651081,45.037031565832));
#58797=CARTESIAN_POINT('Ctrl Pts',(3.09908550384733,6.01564277861006,45.0456868593144));
#58798=CARTESIAN_POINT('Ctrl Pts',(3.09908550384712,6.01564277861017,43.045630740225));
#58799=CARTESIAN_POINT('Ctrl Pts',(2.9419576178338,6.09659052961784,43.0539354227508));
#58800=CARTESIAN_POINT('Ctrl Pts',(2.78171701424298,6.17134687375159,43.0622401052765));
#58801=CARTESIAN_POINT('Ctrl Pts',(2.61889088468052,6.23968745484398,43.0705447878023));
#58802=CARTESIAN_POINT('Ctrl Pts',(2.4546986312921,6.30860141869969,43.078919147257));
#58803=CARTESIAN_POINT('Ctrl Pts',(2.28787760231696,6.37099133390253,43.0872935067117));
#58804=CARTESIAN_POINT('Ctrl Pts',(2.11898561054603,6.42667791182185,43.0956678661665));
#58805=CARTESIAN_POINT('Ctrl Pts',(1.95120332122819,6.4819986018653,43.1039872020104));
#58806=CARTESIAN_POINT('Ctrl Pts',(1.7813775537115,6.5307037424505,43.1123065378543));
#58807=CARTESIAN_POINT('Ctrl Pts',(1.61006699785046,6.57266865606603,43.1206258736982));
#58808=CARTESIAN_POINT('Ctrl Pts',(1.43705688468038,6.61504989998473,43.1290277449583));
#58809=CARTESIAN_POINT('Ctrl Pts',(1.26253272416397,6.65055639756547,43.1374296162185));
#58810=CARTESIAN_POINT('Ctrl Pts',(1.08707678624679,6.67911319419003,43.1458314874786));
#58811=CARTESIAN_POINT('Ctrl Pts',(0.911620848329616,6.70766999081459,43.1542333587388));
#58812=CARTESIAN_POINT('Ctrl Pts',(0.735233496888212,6.72927709584685,43.162635229999));
#58813=CARTESIAN_POINT('Ctrl Pts',(0.558498370545718,6.74391344621932,43.1710371012591));
#58814=CARTESIAN_POINT('Ctrl Pts',(0.388714498010424,6.75797412729302,43.1791085145012));
#58815=CARTESIAN_POINT('Ctrl Pts',(0.21808693188033,6.76564472910105,43.1871799277432));
#58816=CARTESIAN_POINT('Ctrl Pts',(0.0471480780741471,6.7668357493539,43.1952513409852));
#58817=CARTESIAN_POINT('Ctrl Pts',(-0.123576176159475,6.76802527437947,
43.2033126212365));
#58818=CARTESIAN_POINT('Ctrl Pts',(-0.294610572263851,6.76275140100793,
43.2113739014877));
#58819=CARTESIAN_POINT('Ctrl Pts',(-0.465415262605885,6.75097605041919,
43.2194351817389));
#58820=CARTESIAN_POINT('Ctrl Pts',(-0.636042980065169,6.73921290041894,
43.2274881095966));
#58821=CARTESIAN_POINT('Ctrl Pts',(-0.806441096464912,6.72096170399405,
43.2355410374542));
#58822=CARTESIAN_POINT('Ctrl Pts',(-0.976067524947408,6.69623634489876,
43.2435939653119));
#58823=CARTESIAN_POINT('Ctrl Pts',(-1.1455553456542,6.67153118977202,43.2516403128363));
#58824=CARTESIAN_POINT('Ctrl Pts',(-1.31427236631446,6.6403624549363,43.2596866603607));
#58825=CARTESIAN_POINT('Ctrl Pts',(-1.48167949414037,6.60279598932482,43.2677330078851));
#58826=CARTESIAN_POINT('Ctrl Pts',(-1.64898644768527,6.56525200300518,43.2757745405783));
#58827=CARTESIAN_POINT('Ctrl Pts',(-1.81498470576385,6.52131798844838,43.2838160732714));
#58828=CARTESIAN_POINT('Ctrl Pts',(-1.97914337764906,6.47111122533896,43.2918576059646));
#58829=CARTESIAN_POINT('Ctrl Pts',(-2.14645795690911,6.41993925038819,43.3000537350128));
#58830=CARTESIAN_POINT('Ctrl Pts',(-2.31186110747613,6.36225094694745,43.3082498640611));
#58831=CARTESIAN_POINT('Ctrl Pts',(-2.47480438153987,6.29822453339916,43.3164459931093));
#58832=CARTESIAN_POINT('Ctrl Pts',(-2.63461901483382,6.23542747803655,43.3244847499454));
#58833=CARTESIAN_POINT('Ctrl Pts',(-2.79206702665504,6.16653366234927,43.3325235067815));
#58834=CARTESIAN_POINT('Ctrl Pts',(-2.94664929054513,6.09176057954758,43.3405622636176));
#58835=CARTESIAN_POINT('Ctrl Pts',(-3.10124651636469,6.0169802595017,43.3486017985203));
#58836=CARTESIAN_POINT('Ctrl Pts',(-3.25297710568235,5.93631970179732,43.3566413334231));
#58837=CARTESIAN_POINT('Ctrl Pts',(-3.4013651148282,5.85004310715996,43.3646808683259));
#58838=CARTESIAN_POINT('Ctrl Pts',(-3.54979686724296,5.76374107906406,43.3727227732014));
#58839=CARTESIAN_POINT('Ctrl Pts',(-3.69488375546739,5.67181990632548,43.380764678077));
#58840=CARTESIAN_POINT('Ctrl Pts',(-3.83617761333508,5.57458790575113,43.3888065829525));
#58841=CARTESIAN_POINT('Ctrl Pts',(-3.98223763549984,5.47407604788741,43.3971197596333));
#58842=CARTESIAN_POINT('Ctrl Pts',(-4.12424389634693,5.3678890496725,43.4054329363142));
#58843=CARTESIAN_POINT('Ctrl Pts',(-4.26173808893117,5.25641298428437,43.413746112995));
#58844=CARTESIAN_POINT('Ctrl Pts',(-4.39497656745786,5.14838732105241,43.4218019806055));
#58845=CARTESIAN_POINT('Ctrl Pts',(-4.52397790198581,5.03539542431061,43.429857848216));
#58846=CARTESIAN_POINT('Ctrl Pts',(-4.6483627099482,4.91782605596854,43.4379137158265));
#58847=CARTESIAN_POINT('Ctrl Pts',(-4.77870690195993,4.7946238372015,43.4463555470425));
#58848=CARTESIAN_POINT('Ctrl Pts',(-4.90398098136119,4.66639508233387,43.4547973782585));
#58849=CARTESIAN_POINT('Ctrl Pts',(-5.02379638349647,4.5336253591544,43.4632392094745));
#58850=CARTESIAN_POINT('Ctrl Pts',(-5.14361178563174,4.40085563597493,43.4716810406904));
#58851=CARTESIAN_POINT('Ctrl Pts',(-5.25796828117685,4.26354535356909,43.4801228719063));
#58852=CARTESIAN_POINT('Ctrl Pts',(-5.36653018699977,4.12221333169697,43.4885647031223));
#58853=CARTESIAN_POINT('Ctrl Pts',(-5.47831305615991,3.97668807779401,43.497256998151));
#58854=CARTESIAN_POINT('Ctrl Pts',(-5.58432744583572,3.82641131247741,43.5059492931796));
#58855=CARTESIAN_POINT('Ctrl Pts',(-5.68415610484355,3.67187395967915,43.5146415882083));
#58856=CARTESIAN_POINT('Ctrl Pts',(-5.78007555539817,3.52338816293602,43.522993500089));
#58857=CARTESIAN_POINT('Ctrl Pts',(-5.87028426080624,3.37096942442776,43.5313454119698));
#58858=CARTESIAN_POINT('Ctrl Pts',(-5.9544518841414,3.21508814178476,43.5396973238505));
#58859=CARTESIAN_POINT('Ctrl Pts',(-6.03853035496607,3.05937197260385,43.5480403891715));
#58860=CARTESIAN_POINT('Ctrl Pts',(-6.11658032902696,2.90020086545064,43.5563834544924));
#58861=CARTESIAN_POINT('Ctrl Pts',(-6.18831481050102,2.73807392269341,43.5647265198134));
#58862=CARTESIAN_POINT('Ctrl Pts',(-6.25998471771382,2.5760929240811,43.5730620748371));
#58863=CARTESIAN_POINT('Ctrl Pts',(-6.32535032107552,2.41116170357753,43.5813976298608));
#58864=CARTESIAN_POINT('Ctrl Pts',(-6.38417050338549,2.24380390936968,43.5897331848846));
#58865=CARTESIAN_POINT('Ctrl Pts',(-6.44294708442541,2.07657017143119,43.5980625610633));
#58866=CARTESIAN_POINT('Ctrl Pts',(-6.4951877993785,1.90691376699399,43.6063919372421));
#58867=CARTESIAN_POINT('Ctrl Pts',(-6.54069953748574,1.73537850635929,43.6147213134209));
#58868=CARTESIAN_POINT('Ctrl Pts',(-6.58618145098423,1.56395565567086,43.6230452312191));
#58869=CARTESIAN_POINT('Ctrl Pts',(-6.62494309208294,1.39065673491937,43.6313691490173));
#58870=CARTESIAN_POINT('Ctrl Pts',(-6.65684108440876,1.21604102600513,43.6396930668155));
#58871=CARTESIAN_POINT('Ctrl Pts',(-6.68872682337062,1.04149239434806,43.6480137870459));
#58872=CARTESIAN_POINT('Ctrl Pts',(-6.71375410681703,0.865628319988322,
43.6563345072763));
#58873=CARTESIAN_POINT('Ctrl Pts',(-6.73183049171232,0.689019035188684,
43.6646552275067));
#58874=CARTESIAN_POINT('Ctrl Pts',(-6.74990324280198,0.512445253273955,
43.6729742750641));
#58875=CARTESIAN_POINT('Ctrl Pts',(-6.76102784515868,0.335126900850402,
43.6812933226216));
#58876=CARTESIAN_POINT('Ctrl Pts',(-6.76516359776396,0.157640399293324,
43.689612370179));
#58877=CARTESIAN_POINT('Ctrl Pts',(-6.76641762556073,0.103823590662527,
43.6921348413893));
#58878=CARTESIAN_POINT('Ctrl Pts',(-6.76702945930099,0.0499913483530002,
43.6946573125995));
#58879=CARTESIAN_POINT('Ctrl Pts',(-6.76699891035622,-0.00384021324774086,
43.6971797838098));
#58880=CARTESIAN_POINT('',(-6.76699984387958,0.000602726414096441,43.3028202161897));
#58881=CARTESIAN_POINT('Ctrl Pts',(3.09908550384717,6.01564277861014,42.6514898562653));
#58882=CARTESIAN_POINT('Ctrl Pts',(2.93987777019309,6.09766200708263,42.6599168220883));
#58883=CARTESIAN_POINT('Ctrl Pts',(2.77734729302395,6.17339041892882,42.6683437879113));
#58884=CARTESIAN_POINT('Ctrl Pts',(2.61202061225415,6.24256656521654,42.6767707537343));
#58885=CARTESIAN_POINT('Ctrl Pts',(2.44674469261368,6.31172147198447,42.6851951321813));
#58886=CARTESIAN_POINT('Ctrl Pts',(2.27867458764138,6.37432799404581,42.6936195106282));
#58887=CARTESIAN_POINT('Ctrl Pts',(2.10835819139115,6.43017221672902,42.7020438890751));
#58888=CARTESIAN_POINT('Ctrl Pts',(1.93807135869421,6.48600674596116,42.7104668052168));
#58889=CARTESIAN_POINT('Ctrl Pts',(1.76553932864102,6.5350812117948,42.7188897213584));
#58890=CARTESIAN_POINT('Ctrl Pts',(1.59132692617963,6.57723099898549,42.7273126375001));
#58891=CARTESIAN_POINT('Ctrl Pts',(1.4171204692445,6.61937934768694,42.7357352661842));
#58892=CARTESIAN_POINT('Ctrl Pts',(1.24123407831885,6.65460341070326,42.7441578948684));
#58893=CARTESIAN_POINT('Ctrl Pts',(1.06424495043908,6.68278921450205,42.7525805235525));
#58894=CARTESIAN_POINT('Ctrl Pts',(0.88723718228041,6.7109779867953,42.7610040392976));
#58895=CARTESIAN_POINT('Ctrl Pts',(0.709126774946567,6.73212697011826,42.7694275550427));
#58896=CARTESIAN_POINT('Ctrl Pts',(0.530498633683403,6.74617374514325,42.7778510707878));
#58897=CARTESIAN_POINT('Ctrl Pts',(0.35175453806,6.76022963846729,42.7862800545592));
#58898=CARTESIAN_POINT('Ctrl Pts',(0.17249236956393,6.76717408219812,42.7947090383307));
#58899=CARTESIAN_POINT('Ctrl Pts',(-0.00669927327009474,6.766996683887,
42.8031380221021));
#58900=CARTESIAN_POINT('Ctrl Pts',(-0.185944842087931,6.76681923218958,
42.8115695424943));
#58901=CARTESIAN_POINT('Ctrl Pts',(-0.365119509352608,6.75951567108584,
42.8200010628864));
#58902=CARTESIAN_POINT('Ctrl Pts',(-0.543636598857979,6.74512774144287,
42.8284325832786));
#58903=CARTESIAN_POINT('Ctrl Pts',(-0.722332975389522,6.73072536181572,
42.836872571556));
#58904=CARTESIAN_POINT('Ctrl Pts',(-0.90037012165086,6.70922442470045,42.8453125598334));
#58905=CARTESIAN_POINT('Ctrl Pts',(-1.07716704268992,6.68071853636588,42.8537525481108));
#58906=CARTESIAN_POINT('Ctrl Pts',(-1.25305966353853,6.6523584530606,42.8621493666148));
#58907=CARTESIAN_POINT('Ctrl Pts',(-1.42772440839463,6.61706502585254,42.8705461851189));
#58908=CARTESIAN_POINT('Ctrl Pts',(-1.60060127131946,6.57498019542649,42.8789430036229));
#58909=CARTESIAN_POINT('Ctrl Pts',(-1.76821880692063,6.53417568611933,42.8870843708408));
#58910=CARTESIAN_POINT('Ctrl Pts',(-1.93448858358166,6.48690531125586,42.8952257380586));
#58911=CARTESIAN_POINT('Ctrl Pts',(-2.09887052513986,6.43327533366163,42.9033671052764));
#58912=CARTESIAN_POINT('Ctrl Pts',(-2.26310897376519,6.379692170959,42.9115013656999));
#58913=CARTESIAN_POINT('Ctrl Pts',(-2.42546252190072,6.31976056852021,42.9196356261233));
#58914=CARTESIAN_POINT('Ctrl Pts',(-2.58540261115405,6.25363752852992,42.9277698865468));
#58915=CARTESIAN_POINT('Ctrl Pts',(-2.74523359505533,6.18755959528923,42.9358985980716));
#58916=CARTESIAN_POINT('Ctrl Pts',(-2.90265406105496,6.11529877278384,42.9440273095964));
#58917=CARTESIAN_POINT('Ctrl Pts',(-3.05715195579901,6.03706144735618,42.9521560211212));
#58918=CARTESIAN_POINT('Ctrl Pts',(-3.21157617335267,5.95886143186294,42.9602808562137));
#58919=CARTESIAN_POINT('Ctrl Pts',(-3.36308026916501,5.87469075398754,42.9684056913062));
#58920=CARTESIAN_POINT('Ctrl Pts',(-3.51117349793127,5.78480333869917,42.9765305263987));
#58921=CARTESIAN_POINT('Ctrl Pts',(-3.65922526758303,5.69494108764467,42.9846530869209));
#58922=CARTESIAN_POINT('Ctrl Pts',(-3.80386775991283,5.59936547737208,42.992775647443));
#58923=CARTESIAN_POINT('Ctrl Pts',(-3.94463614192823,5.49837564265971,43.0008982079652));
#58924=CARTESIAN_POINT('Ctrl Pts',(-4.08541200541813,5.39738044059949,43.0090212001803));
#58925=CARTESIAN_POINT('Ctrl Pts',(-4.22231304754953,5.29097064945622,43.0171441923955));
#58926=CARTESIAN_POINT('Ctrl Pts',(-4.35490451628916,5.17948797218454,43.0252671846107));
#58927=CARTESIAN_POINT('Ctrl Pts',(-4.42258842041516,5.12257946282197,43.029413724592));
#58928=CARTESIAN_POINT('Ctrl Pts',(-4.48914985206684,5.06434972862147,43.0335602645733));
#58929=CARTESIAN_POINT('Ctrl Pts',(-4.55453438253697,5.00484820531937,43.0377068045546));
#58930=CARTESIAN_POINT('Ctrl Pts',(-4.69619280862793,4.8759355698629,43.046690463583));
#58931=CARTESIAN_POINT('Ctrl Pts',(-4.83225487386259,4.74111493348462,43.0556741226114));
#58932=CARTESIAN_POINT('Ctrl Pts',(-4.96227231454179,4.60088496664849,43.0646577816398));
#58933=CARTESIAN_POINT('Ctrl Pts',(-5.09251312380689,4.4604140862147,43.0736568744992));
#58934=CARTESIAN_POINT('Ctrl Pts',(-5.21668838999999,4.31451547627411,43.0826559673587));
#58935=CARTESIAN_POINT('Ctrl Pts',(-5.33438984187612,4.16372117400876,43.0916550602181));
#58936=CARTESIAN_POINT('Ctrl Pts',(-5.45236727076581,4.01257330124332,43.1006752534355));
#58937=CARTESIAN_POINT('Ctrl Pts',(-5.56384036654162,3.8565069579234,43.109695446653));
#58938=CARTESIAN_POINT('Ctrl Pts',(-5.66844238087631,3.69608576397861,43.1187156398704));
#58939=CARTESIAN_POINT('Ctrl Pts',(-5.77315033094328,3.53550210340483,43.1277449682922));
#58940=CARTESIAN_POINT('Ctrl Pts',(-5.87097317237599,3.37055498480376,43.1367742967139));
#58941=CARTESIAN_POINT('Ctrl Pts',(-5.96158917476093,3.20183439786841,43.1458036251357));
#58942=CARTESIAN_POINT('Ctrl Pts',(-6.05233292744388,3.03287594891427,43.1548456830905));
#58943=CARTESIAN_POINT('Ctrl Pts',(-6.13584941245282,2.86013360535714,43.1638877410453));
#58944=CARTESIAN_POINT('Ctrl Pts',(-6.21186325883687,2.68422127506519,43.1729297990001));
#58945=CARTESIAN_POINT('Ctrl Pts',(-6.27783007217801,2.53155993231266,43.1807767344954));
#58946=CARTESIAN_POINT('Ctrl Pts',(-6.33814719360531,2.37651162294236,43.1886236699907));
#58947=CARTESIAN_POINT('Ctrl Pts',(-6.39266447184091,2.21948866869443,43.196470605486));
#58948=CARTESIAN_POINT('Ctrl Pts',(-6.45445102698719,2.04152843781232,43.2053638431604));
#58949=CARTESIAN_POINT('Ctrl Pts',(-6.50883338074033,1.8608973894608,43.2142570808348));
#58950=CARTESIAN_POINT('Ctrl Pts',(-6.55560081224318,1.67820945966723,43.2231503185091));
#58951=CARTESIAN_POINT('Ctrl Pts',(-6.6023193763613,1.49571242086473,43.2320342636213));
#58952=CARTESIAN_POINT('Ctrl Pts',(-6.64143882873939,1.31116304398865,43.2409182087335));
#58953=CARTESIAN_POINT('Ctrl Pts',(-6.67279818559416,1.12519037248425,43.2498021538456));
#58954=CARTESIAN_POINT('Ctrl Pts',(-6.70410369344196,0.939537045656859,
43.25867084381));
#58955=CARTESIAN_POINT('Ctrl Pts',(-6.72767566198704,0.752465562753678,
43.2675395337744));
#58956=CARTESIAN_POINT('Ctrl Pts',(-6.74340410743541,0.564614951824003,
43.2764082237388));
#58957=CARTESIAN_POINT('Ctrl Pts',(-6.75901782205446,0.37813461340171,43.2852122212224));
#58958=CARTESIAN_POINT('Ctrl Pts',(-6.76690201965948,0.190886734716022,
43.2940162187061));
#58959=CARTESIAN_POINT('Ctrl Pts',(-6.76699909195969,0.00350562643901177,
43.3028202161897));
#58960=CARTESIAN_POINT('Ctrl Pts',(-6.767,5.35191256783216E-12,43.3028202161897));
#58961=CARTESIAN_POINT('Ctrl Pts',(-6.76700000000015,-0.18600724955472,
43.3115697280024));
#58962=CARTESIAN_POINT('Ctrl Pts',(-6.75932637294276,-0.372014355810972,
43.3203192398152));
#58963=CARTESIAN_POINT('Ctrl Pts',(-6.74400518263404,-0.557389537581421,
43.3290687516279));
#58964=CARTESIAN_POINT('Ctrl Pts',(-6.72868405703783,-0.742763936377903,
43.3378182264851));
#58965=CARTESIAN_POINT('Ctrl Pts',(-6.7057154564363,-0.927506130400228,
43.3465677013423));
#58966=CARTESIAN_POINT('Ctrl Pts',(-6.67517739401653,-1.11098864009077,
43.3553171761995));
#58967=CARTESIAN_POINT('Ctrl Pts',(-6.64463945804479,-1.2944703900408,43.364066614828));
#58968=CARTESIAN_POINT('Ctrl Pts',(-6.60653217002826,-1.47669218338824,
43.3728160534566));
#58969=CARTESIAN_POINT('Ctrl Pts',(-6.56098496085593,-1.65703510627337,
43.3815654920851));
#58970=CARTESIAN_POINT('Ctrl Pts',(-6.51543793649679,-1.83737729739575,
43.3903148952117));
#58971=CARTESIAN_POINT('Ctrl Pts',(-6.46245112157028,-2.01584035544531,
43.3990642983383));
#58972=CARTESIAN_POINT('Ctrl Pts',(-6.40220448361857,-2.19181813797001,
43.407813701465));
#58973=CARTESIAN_POINT('Ctrl Pts',(-6.34195808512125,-2.36779522105895,
43.4165630698165));
#58974=CARTESIAN_POINT('Ctrl Pts',(-6.27445201416518,-2.54128677725338,
43.425312438168));
#58975=CARTESIAN_POINT('Ctrl Pts',(-6.19991555052901,-2.71170355428254,
43.4340618065196));
#58976=CARTESIAN_POINT('Ctrl Pts',(-6.12537937695296,-2.88211966813145,
43.4428111408228));
#58977=CARTESIAN_POINT('Ctrl Pts',(-6.04381298028522,-3.0494607641953,43.4515604751259));
#58978=CARTESIAN_POINT('Ctrl Pts',(-5.95549339309045,-3.21315848424195,
43.4603098094291));
#58979=CARTESIAN_POINT('Ctrl Pts',(-5.86717414225866,-3.37685558084984,
43.4690591104107));
#58980=CARTESIAN_POINT('Ctrl Pts',(-5.77210188844116,-3.53690907699921,
43.4778084113923));
#58981=CARTESIAN_POINT('Ctrl Pts',(-5.67059953311412,-3.6927753702393,43.4865577123738));
#58982=CARTESIAN_POINT('Ctrl Pts',(-5.56909755592737,-3.84864108280984,
43.4953069807604));
#58983=CARTESIAN_POINT('Ctrl Pts',(-5.46116568154984,-4.00031938354804,
43.5040562491471));
#58984=CARTESIAN_POINT('Ctrl Pts',(-5.34717048488383,-4.14729511918157,
43.5128055175337));
#58985=CARTESIAN_POINT('Ctrl Pts',(-5.23317570343297,-4.29427031947189,
43.5215547540521));
#58986=CARTESIAN_POINT('Ctrl Pts',(-5.11311781951525,-4.43654276249582,
43.5303039905704));
#58987=CARTESIAN_POINT('Ctrl Pts',(-4.98740458929206,-4.57362924412424,
43.5390532270888));
#58988=CARTESIAN_POINT('Ctrl Pts',(-4.86169180652698,-4.71071523781311,
43.5478024324655));
#58989=CARTESIAN_POINT('Ctrl Pts',(-4.73032391141527,-4.84261509584534,
43.5565516378422));
#58990=CARTESIAN_POINT('Ctrl Pts',(-4.59374706947278,-4.96888084599644,
43.5653008432189));
#58991=CARTESIAN_POINT('Ctrl Pts',(-4.45717070231475,-5.09514615720771,
43.5740500181806));
#58992=CARTESIAN_POINT('Ctrl Pts',(-4.31538563497346,-5.21577720520596,
43.5827991931423));
#58993=CARTESIAN_POINT('Ctrl Pts',(-4.16887340952043,-5.33036429293473,
43.591548368104));
#58994=CARTESIAN_POINT('Ctrl Pts',(-4.02236168122516,-5.44495099183683,
43.6002975133773));
#58995=CARTESIAN_POINT('Ctrl Pts',(-3.87112305263206,-5.55349359497911,
43.6090466586506));
#58996=CARTESIAN_POINT('Ctrl Pts',(-3.71567116929015,-5.65562346357199,
43.6177958039238));
#58997=CARTESIAN_POINT('Ctrl Pts',(-3.56021980053348,-5.75775299408904,
43.6265449202352));
#58998=CARTESIAN_POINT('Ctrl Pts',(-3.40055544442138,-5.85346967519847,
43.6352940365465));
#58999=CARTESIAN_POINT('Ctrl Pts',(-3.23722035886915,-5.94244843041343,
43.6440431528579));
#59000=CARTESIAN_POINT('Ctrl Pts',(-3.07388580043589,-6.03142689847399,
43.6527922409339));
#59001=CARTESIAN_POINT('Ctrl Pts',(-2.90688078789351,-6.1136673470784,43.6615413290099));
#59002=CARTESIAN_POINT('Ctrl Pts',(-2.7367725061055,-6.18889047001359,43.6702904170859));
#59003=CARTESIAN_POINT('Ctrl Pts',(-2.56666475917112,-6.26411335643261,
43.6790394776531));
#59004=CARTESIAN_POINT('Ctrl Pts',(-2.39345402457291,-6.33231884545181,
43.6877885382202));
#59005=CARTESIAN_POINT('Ctrl Pts',(-2.21772855944284,-6.39327529804807,
43.6965375987874));
#59006=CARTESIAN_POINT('Ctrl Pts',(-2.04200363223816,-6.45423156404631,
43.7052866325722));
#59007=CARTESIAN_POINT('Ctrl Pts',(-1.86376426061265,-6.50793874412387,
43.714035666357));
#59008=CARTESIAN_POINT('Ctrl Pts',(-1.68361577621924,-6.55421443943252,
43.7227847001418));
#59009=CARTESIAN_POINT('Ctrl Pts',(-1.5034678283347,-6.60048999692529,43.7315337078707));
#59010=CARTESIAN_POINT('Ctrl Pts',(-1.32141105657661,-6.63933404265107,
43.7402827155996));
#59011=CARTESIAN_POINT('Ctrl Pts',(-1.13806375346827,-6.67061465631479,
43.7490317233284));
#59012=CARTESIAN_POINT('Ctrl Pts',(-0.954716981172886,-6.7018951794173,
43.7577807057279));
#59013=CARTESIAN_POINT('Ctrl Pts',(-0.770079967445112,-6.72561226608972,
43.7665296881273));
#59014=CARTESIAN_POINT('Ctrl Pts',(-0.584779764075847,-6.74168536995961,
43.7752786705267));
#59015=CARTESIAN_POINT('Ctrl Pts',(-0.391489587595688,-6.75845153117857,
43.7844049009424));
#59016=CARTESIAN_POINT('Ctrl Pts',(-0.197478091807917,-6.76689985146386,
43.793531131358));
#59017=CARTESIAN_POINT('Ctrl Pts',(-0.00346214753366012,-6.76699911434415,
43.8026573617736));
#59018=CARTESIAN_POINT('Ctrl Pts',(0.184490798482111,-6.76709527525942,
43.8114983974887));
#59019=CARTESIAN_POINT('Ctrl Pts',(0.372447602152351,-6.75935633790777,
43.8203394332039));
#59020=CARTESIAN_POINT('Ctrl Pts',(0.559756448191892,-6.74380914014532,
43.829180468919));
#59021=CARTESIAN_POINT('Ctrl Pts',(0.745136131041022,-6.7284220687318,43.8379304475323));
#59022=CARTESIAN_POINT('Ctrl Pts',(0.929880851942699,-6.70538686355756,
43.8466804261456));
#59023=CARTESIAN_POINT('Ctrl Pts',(1.11336305057228,-6.67478177303351,43.8554304047589));
#59024=CARTESIAN_POINT('Ctrl Pts',(1.29684337089884,-6.64417699581307,43.8641802937989));
#59025=CARTESIAN_POINT('Ctrl Pts',(1.47906091204948,-6.60600253548114,43.8729301828389));
#59026=CARTESIAN_POINT('Ctrl Pts',(1.65939671094976,-6.56038806441274,43.8816800718788));
#59027=CARTESIAN_POINT('Ctrl Pts',(1.8397307236893,-6.51477404513915,43.8904298742543));
#59028=CARTESIAN_POINT('Ctrl Pts',(2.0181827535682,-6.46172023288729,43.8991796766298));
#59029=CARTESIAN_POINT('Ctrl Pts',(2.19414664033124,-6.40140683918177,43.9079294790053));
#59030=CARTESIAN_POINT('Ctrl Pts',(2.37010884271063,-6.34109402281571,43.9166791976249));
#59031=CARTESIAN_POINT('Ctrl Pts',(2.54358267847615,-6.27352185699869,43.9254289162444));
#59032=CARTESIAN_POINT('Ctrl Pts',(2.71397890841557,-6.19891986435342,43.934178634864));
#59033=CARTESIAN_POINT('Ctrl Pts',(2.88437356388768,-6.12431856103325,43.9429282726358));
#59034=CARTESIAN_POINT('Ctrl Pts',(3.0516904078701,-6.04268767582639,43.9516779104076));
#59035=CARTESIAN_POINT('Ctrl Pts',(3.21536112511903,-5.95430447954027,43.9604275481794));
#59036=CARTESIAN_POINT('Ctrl Pts',(3.37903038442686,-5.86592207055133,43.9691771080115));
#59037=CARTESIAN_POINT('Ctrl Pts',(3.53905332979811,-5.77078760703476,43.9779266678436));
#59038=CARTESIAN_POINT('Ctrl Pts',(3.69488643041726,-5.66922422085407,43.9866762276756));
#59039=CARTESIAN_POINT('Ctrl Pts',(3.85071819468582,-5.56766170563269,43.9954257124756));
#59040=CARTESIAN_POINT('Ctrl Pts',(4.00235994599071,-5.45967053456364,44.0041751972756));
#59041=CARTESIAN_POINT('Ctrl Pts',(4.14929662974154,-5.34561750206798,44.0129246820756));
#59042=CARTESIAN_POINT('Ctrl Pts',(4.29623210224898,-5.23156540974586,44.021674094751));
#59043=CARTESIAN_POINT('Ctrl Pts',(4.43846235841972,-5.11145173172312,44.0304235074263));
#59044=CARTESIAN_POINT('Ctrl Pts',(4.57550431797285,-4.98568443006693,44.0391729201017));
#59045=CARTESIAN_POINT('Ctrl Pts',(4.71254519337365,-4.85991812336815,44.0479222635596));
#59046=CARTESIAN_POINT('Ctrl Pts',(4.84439764314869,-4.72849847631219,44.0566716070175));
#59047=CARTESIAN_POINT('Ctrl Pts',(4.97061384196585,-4.59187184425454,44.0654209504754));
#59048=CARTESIAN_POINT('Ctrl Pts',(5.09682908420118,-4.45524624767849,44.0741702276228));
#59049=CARTESIAN_POINT('Ctrl Pts',(5.21740796650095,-4.31341395556985,44.0829195047701));
#59050=CARTESIAN_POINT('Ctrl Pts',(5.33194095942187,-4.16685668162939,44.0916687819175));
#59051=CARTESIAN_POINT('Ctrl Pts',(5.44647312235076,-4.02030046975292,44.100417995661));
#59052=CARTESIAN_POINT('Ctrl Pts',(5.55495930712237,-3.8690195703562,44.1091672094046));
#59053=CARTESIAN_POINT('Ctrl Pts',(5.65703106079751,-3.71352778058442,44.1179164231481));
#59054=CARTESIAN_POINT('Ctrl Pts',(5.75910210868684,-3.55803706597686,44.1266655763943));
#59055=CARTESIAN_POINT('Ctrl Pts',(5.85475865698491,-3.39833575880998,44.1354147296405));
#59056=CARTESIAN_POINT('Ctrl Pts',(5.94367583069,-3.23496624706836,44.1441638828867));
#59057=CARTESIAN_POINT('Ctrl Pts',(6.03259241910016,-3.07159781070219,44.1529129785418));
#59058=CARTESIAN_POINT('Ctrl Pts',(6.11476958470909,-2.90456146975957,44.1616620741969));
#59059=CARTESIAN_POINT('Ctrl Pts',(6.1899282357433,-2.73442451648384,44.170411169852));
#59060=CARTESIAN_POINT('Ctrl Pts',(6.26508641700885,-2.56428862662538,44.1791602108222));
#59061=CARTESIAN_POINT('Ctrl Pts',(6.33322605570253,-2.39105242531395,44.1879092517923));
#59062=CARTESIAN_POINT('Ctrl Pts',(6.39411573747728,-2.21530425353841,44.1966582927624));
#59063=CARTESIAN_POINT('Ctrl Pts',(6.45500505889096,-2.03955712188657,44.2054072819534));
#59064=CARTESIAN_POINT('Ctrl Pts',(6.50864441544907,-1.86129832025651,44.2141562711444));
#59065=CARTESIAN_POINT('Ctrl Pts',(6.55485164049891,-1.6811332401237,44.2229052603354));
#59066=CARTESIAN_POINT('Ctrl Pts',(6.60199852639099,-1.49730435912947,44.2318321672123));
#59067=CARTESIAN_POINT('Ctrl Pts',(6.64140767441003,-1.31149113173689,44.2407590740892));
#59068=CARTESIAN_POINT('Ctrl Pts',(6.67293975269598,-1.12435050446457,44.2496859809661));
#59069=CARTESIAN_POINT('Ctrl Pts',(6.70384664831503,-0.940920291564023,
44.2584358951501));
#59070=CARTESIAN_POINT('Ctrl Pts',(6.72718585889662,-0.756215114278239,
44.2671858093341));
#59071=CARTESIAN_POINT('Ctrl Pts',(6.74287810451862,-0.570862389375461,
44.2759357235181));
#59072=CARTESIAN_POINT('Ctrl Pts',(6.75857004154122,-0.385513309568418,
44.2846854656287));
#59073=CARTESIAN_POINT('Ctrl Pts',(6.76661529035555,-0.199516993259524,
44.2934352077393));
#59074=CARTESIAN_POINT('Ctrl Pts',(6.76698652348896,-0.0135052182053635,
44.3021849498498));
#59075=CARTESIAN_POINT('Ctrl Pts',(6.76735774981525,0.1725031460376,44.3109345315205));
#59076=CARTESIAN_POINT('Ctrl Pts',(6.76005524147486,0.358526681832194,44.3196841131911));
#59077=CARTESIAN_POINT('Ctrl Pts',(6.74510380214892,0.543933542113605,44.3284336948618));
#59078=CARTESIAN_POINT('Ctrl Pts',(6.73015261710993,0.72933724908339,44.3371831277237));
#59079=CARTESIAN_POINT('Ctrl Pts',(6.70755278444624,0.914124015853262,44.3459325605856));
#59080=CARTESIAN_POINT('Ctrl Pts',(6.67738106408313,1.09766621749239,44.3546819934475));
#59081=CARTESIAN_POINT('Ctrl Pts',(6.64720981677282,1.28120554143175,44.3634312891299));
#59082=CARTESIAN_POINT('Ctrl Pts',(6.60946696581555,1.46350005650473,44.3721805848122));
#59083=CARTESIAN_POINT('Ctrl Pts',(6.56428070011031,1.64393062206387,44.3809298804946));
#59084=CARTESIAN_POINT('Ctrl Pts',(6.51909508282779,1.82435859844514,44.3896790506246));
#59085=CARTESIAN_POINT('Ctrl Pts',(6.46646633415702,2.00292240086435,44.3984282207546));
#59086=CARTESIAN_POINT('Ctrl Pts',(6.40657319597233,2.17901557696335,44.4071773908846));
#59087=CARTESIAN_POINT('Ctrl Pts',(6.34668083768341,2.35510646007311,44.4159264470876));
#59088=CARTESIAN_POINT('Ctrl Pts',(6.27952437143936,2.52872650996403,44.4246755032907));
#59089=CARTESIAN_POINT('Ctrl Pts',(6.20533187335193,2.69928607997793,44.4334245594938));
#59090=CARTESIAN_POINT('Ctrl Pts',(6.12831449784312,2.87633970115271,44.4425067357826));
#59091=CARTESIAN_POINT('Ctrl Pts',(6.04371489463214,3.05009490562228,44.4515889120715));
#59092=CARTESIAN_POINT('Ctrl Pts',(5.95184265120553,3.21991584599516,44.4606710883603));
#59093=CARTESIAN_POINT('Ctrl Pts',(5.86333281335551,3.383521559052,44.4694208687147));
#59094=CARTESIAN_POINT('Ctrl Pts',(5.76807337235739,3.54347560903737,44.4781706490692));
#59095=CARTESIAN_POINT('Ctrl Pts',(5.66638790086404,3.69923467178573,44.4869204294236));
#59096=CARTESIAN_POINT('Ctrl Pts',(5.56470608502793,3.85498813489691,44.4956698952178));
#59097=CARTESIAN_POINT('Ctrl Pts',(5.45659885767004,4.0065466725619,44.5044193610121));
#59098=CARTESIAN_POINT('Ctrl Pts',(5.34243340580562,4.15339551506141,44.5131688268064));
#59099=CARTESIAN_POINT('Ctrl Pts',(5.22827145140643,4.30023985883811,44.5219180245603));
#59100=CARTESIAN_POINT('Ctrl Pts',(5.10805181978133,4.44237456992993,44.5306672223142));
#59101=CARTESIAN_POINT('Ctrl Pts',(4.98218281282589,4.57931691626407,44.539416420068));
#59102=CARTESIAN_POINT('Ctrl Pts',(4.85631699296262,4.71625579512128,44.548165396286));
#59103=CARTESIAN_POINT('Ctrl Pts',(4.72480227791865,4.84800236135743,44.556914372504));
#59104=CARTESIAN_POINT('Ctrl Pts',(4.58808530848134,4.97410918678889,44.565663348722));
#59105=CARTESIAN_POINT('Ctrl Pts',(4.45135945056995,5.10022421088987,44.5744128937432));
#59106=CARTESIAN_POINT('Ctrl Pts',(4.30943087208069,5.22069856611962,44.5831624387644));
#59107=CARTESIAN_POINT('Ctrl Pts',(4.16278164322501,5.33512305301658,44.5919119837856));
#59108=CARTESIAN_POINT('Ctrl Pts',(4.0161410353442,5.44954081331405,44.6006610144529));
#59109=CARTESIAN_POINT('Ctrl Pts',(3.86478055833438,5.5579092406832,44.6094100451201));
#59110=CARTESIAN_POINT('Ctrl Pts',(3.70921425811972,5.65986029751278,44.6181590757874));
#59111=CARTESIAN_POINT('Ctrl Pts',(3.55364584530143,5.76181273884639,44.6269082252673));
#59112=CARTESIAN_POINT('Ctrl Pts',(3.3938717346437,5.85734747818048,44.6356573747471));
#59113=CARTESIAN_POINT('Ctrl Pts',(3.23043456092433,5.94614005448792,44.644406524227));
#59114=CARTESIAN_POINT('Ctrl Pts',(3.18690768806409,5.96978744811273,44.64673661296));
#59115=CARTESIAN_POINT('Ctrl Pts',(3.14312114982886,5.99295688499298,44.649066701693));
#59116=CARTESIAN_POINT('Ctrl Pts',(3.09908550384713,6.01564277861016,44.6513967904261));
#59117=CARTESIAN_POINT('Origin',(0.,0.,-63.6971797838103));
#59118=CARTESIAN_POINT('',(3.09908550384709,6.01564277861018,47.0459139429101));
#59119=CARTESIAN_POINT('',(3.09908550384732,6.01564277861007,46.6512066495886));
#59120=CARTESIAN_POINT('',(3.09908550384721,6.01564277861012,-63.6971797838103));
#59121=CARTESIAN_POINT('',(-6.76699846313023,-0.00456070095142003,45.6971797837712));
#59122=CARTESIAN_POINT('Ctrl Pts',(-6.76699846312968,-0.00456070176632315,
45.6971797838098));
#59123=CARTESIAN_POINT('Ctrl Pts',(-6.76693165203006,-0.103692509023912,
45.7018724945944));
#59124=CARTESIAN_POINT('Ctrl Pts',(-6.76468666223142,-0.202774974724137,
45.7065652053789));
#59125=CARTESIAN_POINT('Ctrl Pts',(-6.76026920478145,-0.301743730479347,
45.7112579161634));
#59126=CARTESIAN_POINT('Ctrl Pts',(-6.7525215102958,-0.475323146217892,
45.7194883722299));
#59127=CARTESIAN_POINT('Ctrl Pts',(-6.73807283924028,-0.648858023399886,
45.7277188282965));
#59128=CARTESIAN_POINT('Ctrl Pts',(-6.71691515652579,-0.821790593785403,
45.735949284363));
#59129=CARTESIAN_POINT('Ctrl Pts',(-6.69578258922741,-0.994517883019688,
45.7441699703932));
#59130=CARTESIAN_POINT('Ctrl Pts',(-6.66795691146689,-1.16664393675678,
45.7523906564234));
#59131=CARTESIAN_POINT('Ctrl Pts',(-6.63348206267254,-1.33761157448703,
45.7606113424536));
#59132=CARTESIAN_POINT('Ctrl Pts',(-6.59904122083407,-1.50841056495365,
45.768823919369));
#59133=CARTESIAN_POINT('Ctrl Pts',(-6.55796434037573,-1.67805306604469,
45.7770364962844));
#59134=CARTESIAN_POINT('Ctrl Pts',(-6.51034707987385,-1.84598751338629,
45.7852490731998));
#59135=CARTESIAN_POINT('Ctrl Pts',(-6.4627672403075,-2.01378998622826,45.7934551961044));
#59136=CARTESIAN_POINT('Ctrl Pts',(-6.40865735556372,-2.17988673552435,
45.8016613190091));
#59137=CARTESIAN_POINT('Ctrl Pts',(-6.34816405334433,-2.34373679235253,
45.8098674419137));
#59138=CARTESIAN_POINT('Ctrl Pts',(-6.28770616159362,-2.5074909376154,45.8180687612674));
#59139=CARTESIAN_POINT('Ctrl Pts',(-6.22087241996648,-2.66900067486691,
45.8262700806211));
#59140=CARTESIAN_POINT('Ctrl Pts',(-6.14785918808317,-2.82774051205223,
45.8344713999748));
#59141=CARTESIAN_POINT('Ctrl Pts',(-6.07486690196608,-2.98643481053948,
45.8426703665643));
#59142=CARTESIAN_POINT('Ctrl Pts',(-5.99569880272875,-3.14236046478394,
45.8508693331539));
#59143=CARTESIAN_POINT('Ctrl Pts',(-5.91059934396207,-3.29501204780121,
45.8590682997434));
#59144=CARTESIAN_POINT('Ctrl Pts',(-5.82551112296334,-3.44764347248739,
45.8672661836223));
#59145=CARTESIAN_POINT('Ctrl Pts',(-5.73449327625604,-3.59700137351191,
45.8754640675012));
#59146=CARTESIAN_POINT('Ctrl Pts',(-5.63783617155951,-3.74260501558143,
45.8836619513802));
#59147=CARTESIAN_POINT('Ctrl Pts',(-5.54117427282915,-3.88821587935274,
45.8918602418607));
#59148=CARTESIAN_POINT('Ctrl Pts',(-5.43887275720035,-4.03007181438313,
45.9000585323412));
#59149=CARTESIAN_POINT('Ctrl Pts',(-5.33126529469141,-4.16772112282227,
45.9082568228217));
#59150=CARTESIAN_POINT('Ctrl Pts',(-5.22363294787663,-4.3054022627665,45.916457009163));
#59151=CARTESIAN_POINT('Ctrl Pts',(-5.11069243117124,-4.43887455614888,
45.9246571955044));
#59152=CARTESIAN_POINT('Ctrl Pts',(-4.99281768431763,-4.5677194059142,45.9328573818457));
#59153=CARTESIAN_POINT('Ctrl Pts',(-4.87483149613951,-4.6966860683756,45.9410653208198));
#59154=CARTESIAN_POINT('Ctrl Pts',(-4.75190200018331,-4.82101628175486,
45.9492732597938));
#59155=CARTESIAN_POINT('Ctrl Pts',(-4.6244406487371,-4.94032769017481,45.9574811987679));
#59156=CARTESIAN_POINT('Ctrl Pts',(-4.4969174619275,-5.05969698017386,45.9656931196619));
#59157=CARTESIAN_POINT('Ctrl Pts',(-4.36485830718876,-5.17404237624267,
45.9739050405559));
#59158=CARTESIAN_POINT('Ctrl Pts',(-4.22870762648803,-5.28302193916342,
45.9821169614498));
#59159=CARTESIAN_POINT('Ctrl Pts',(-4.09237023669766,-5.3921509502902,45.9903401436924));
#59160=CARTESIAN_POINT('Ctrl Pts',(-3.95193039624666,-5.49589920959848,
45.9985633259349));
#59161=CARTESIAN_POINT('Ctrl Pts',(-3.80786241885848,-5.59396753646687,
46.0067865081775));
#59162=CARTESIAN_POINT('Ctrl Pts',(-3.67939014133803,-5.68141973461536,
46.0141195114605));
#59163=CARTESIAN_POINT('Ctrl Pts',(-3.54803325774793,-5.76435570532466,
46.0214525147435));
#59164=CARTESIAN_POINT('Ctrl Pts',(-3.41414382398665,-5.84259453916955,
46.0287855180265));
#59165=CARTESIAN_POINT('Ctrl Pts',(-3.25100096796157,-5.93792772900352,
46.0377207048088));
#59166=CARTESIAN_POINT('Ctrl Pts',(-3.08375932500652,-6.02648457399728,
46.0466558915912));
#59167=CARTESIAN_POINT('Ctrl Pts',(-2.91298097454007,-6.10793179742273,
46.0555910783735));
#59168=CARTESIAN_POINT('Ctrl Pts',(-2.74245839721137,-6.18925703810364,
46.0645128830101));
#59169=CARTESIAN_POINT('Ctrl Pts',(-2.56840991414264,-6.26349379274193,
46.0734346876467));
#59170=CARTESIAN_POINT('Ctrl Pts',(-2.3914222851357,-6.33035452831485,46.0823564922834));
#59171=CARTESIAN_POINT('Ctrl Pts',(-2.21486637092911,-6.39705217469747,
46.0912565345227));
#59172=CARTESIAN_POINT('Ctrl Pts',(-2.03538586065373,-6.45640961957508,
46.100156576762));
#59173=CARTESIAN_POINT('Ctrl Pts',(-1.85358698663192,-6.50818748062691,
46.1090566190013));
#59174=CARTESIAN_POINT('Ctrl Pts',(-1.67206799464952,-6.5598856289004,46.1179429594947));
#59175=CARTESIAN_POINT('Ctrl Pts',(-1.48823800567415,-6.60402739933049,
46.1268292999881));
#59176=CARTESIAN_POINT('Ctrl Pts',(-1.30272071005423,-6.64042225702521,
46.1357156404815));
#59177=CARTESIAN_POINT('Ctrl Pts',(-1.11767774977619,-6.67672405942173,
46.1445792601535));
#59178=CARTESIAN_POINT('Ctrl Pts',(-0.930956344206983,-6.70531842414489,
46.1534428798254));
#59179=CARTESIAN_POINT('Ctrl Pts',(-0.743191996133971,-6.72606531761939,
46.1623064994974));
#59180=CARTESIAN_POINT('Ctrl Pts',(-0.564946474366039,-6.74576043487875,
46.1707207726509));
#59181=CARTESIAN_POINT('Ctrl Pts',(-0.385761376642811,-6.75838387267933,
46.1791350458044));
#59182=CARTESIAN_POINT('Ctrl Pts',(-0.206191209780811,-6.76385793648929,
46.1875493189579));
#59183=CARTESIAN_POINT('Ctrl Pts',(-0.0309751675667889,-6.76919926802764,
46.1957595671624));
#59184=CARTESIAN_POINT('Ctrl Pts',(0.144439133819563,-6.76772758024457,
46.203969815367));
#59185=CARTESIAN_POINT('Ctrl Pts',(0.31948715555248,-6.7594538949117,46.2121800635715));
#59186=CARTESIAN_POINT('Ctrl Pts',(0.494576789690166,-6.75117824275887,
46.2203922635157));
#59187=CARTESIAN_POINT('Ctrl Pts',(0.669299615144041,-6.73609738839269,
46.22860446346));
#59188=CARTESIAN_POINT('Ctrl Pts',(0.843094771168033,-6.71427436189713,
46.2368166634042));
#59189=CARTESIAN_POINT('Ctrl Pts',(1.01696218981099,-6.69244226156381,46.2450322779147));
#59190=CARTESIAN_POINT('Ctrl Pts',(1.18990081770612,-6.66386244854279,46.2532478924251));
#59191=CARTESIAN_POINT('Ctrl Pts',(1.36135846933956,-6.6286493434151,46.2614635069356));
#59192=CARTESIAN_POINT('Ctrl Pts',(1.53300866039976,-6.59339669551396,46.2696883472211));
#59193=CARTESIAN_POINT('Ctrl Pts',(1.70317420470409,-6.5514959492847,46.2779131875065));
#59194=CARTESIAN_POINT('Ctrl Pts',(1.87131565199657,-6.50311208042678,46.2861380277919));
#59195=CARTESIAN_POINT('Ctrl Pts',(2.03956479973073,-6.45469722001899,46.2943681363734));
#59196=CARTESIAN_POINT('Ctrl Pts',(2.20578692882527,-6.39979107020287,46.302598244955));
#59197=CARTESIAN_POINT('Ctrl Pts',(2.36946119459583,-6.33860731133461,46.3108283535366));
#59198=CARTESIAN_POINT('Ctrl Pts',(2.53335986029653,-6.277339668594,46.3190697457233));
#59199=CARTESIAN_POINT('Ctrl Pts',(2.69470335810053,-6.20977736290887,46.32731113791));
#59200=CARTESIAN_POINT('Ctrl Pts',(2.85299321245167,-6.13618111936933,46.3355525300967));
#59201=CARTESIAN_POINT('Ctrl Pts',(2.92188497865142,-6.10415016436032,46.339139393361));
#59202=CARTESIAN_POINT('Ctrl Pts',(2.99019866156302,-6.07097682855361,46.3427262566253));
#59203=CARTESIAN_POINT('Ctrl Pts',(3.05789483861246,-6.03668519603162,46.3463131198896));
#59204=CARTESIAN_POINT('Ctrl Pts',(3.21734635921982,-5.9559147125559,46.3547616147181));
#59205=CARTESIAN_POINT('Ctrl Pts',(3.37373376537696,-5.86875288562713,46.3632101095465));
#59206=CARTESIAN_POINT('Ctrl Pts',(3.52652924162476,-5.77545500441008,46.3716586043749));
#59207=CARTESIAN_POINT('Ctrl Pts',(3.67918514808085,-5.68224234538789,46.3800993819941));
#59208=CARTESIAN_POINT('Ctrl Pts',(3.82825538147023,-5.58290497733933,46.3885401596133));
#59209=CARTESIAN_POINT('Ctrl Pts',(3.97323632479801,-5.47774425355051,46.3969809372325));
#59210=CARTESIAN_POINT('Ctrl Pts',(4.11810713140899,-5.372663416515,46.4054153027018));
#59211=CARTESIAN_POINT('Ctrl Pts',(4.2588945717964,-5.26176823770797,46.413849668171));
#59212=CARTESIAN_POINT('Ctrl Pts',(4.39512332186689,-5.14540377284249,46.4222840336404));
#59213=CARTESIAN_POINT('Ctrl Pts',(4.53126950427668,-5.02910983597972,46.430713287077));
#59214=CARTESIAN_POINT('Ctrl Pts',(4.66286225216365,-4.90735343816392,46.4391425405136));
#59215=CARTESIAN_POINT('Ctrl Pts',(4.78945839401117,-4.78052060889146,46.4475717939502));
#59216=CARTESIAN_POINT('Ctrl Pts',(4.9159972259603,-4.65374519666545,46.4559972314755));
#59217=CARTESIAN_POINT('Ctrl Pts',(5.0375437270808,-4.52189817102035,46.4644226690007));
#59218=CARTESIAN_POINT('Ctrl Pts',(5.15369047056232,-4.38540346303908,46.4728481065259));
#59219=CARTESIAN_POINT('Ctrl Pts',(5.26981169972771,-4.24893873927454,46.4812716932091));
#59220=CARTESIAN_POINT('Ctrl Pts',(5.38053531837965,-4.10782862079312,46.4896952798923));
#59221=CARTESIAN_POINT('Ctrl Pts',(5.48549285196325,-3.96253166183693,46.4981188665755));
#59222=CARTESIAN_POINT('Ctrl Pts',(5.59043864134923,-3.81725096084852,46.5065415107035));
#59223=CARTESIAN_POINT('Ctrl Pts',(5.6896194367138,-3.66778462355201,46.5149641548315));
#59224=CARTESIAN_POINT('Ctrl Pts',(5.78270875119717,-3.5146220990069,46.5233867989595));
#59225=CARTESIAN_POINT('Ctrl Pts',(5.87580063040251,-3.36145535465102,46.5318096751414));
#59226=CARTESIAN_POINT('Ctrl Pts',(5.96280052129554,-3.20459250512422,46.5402325513233));
#59227=CARTESIAN_POINT('Ctrl Pts',(6.04342656492772,-3.04454994282011,46.5486554275053));
#59228=CARTESIAN_POINT('Ctrl Pts',(6.12406607355669,-2.88448065251981,46.5570797103543));
#59229=CARTESIAN_POINT('Ctrl Pts',(6.19832946325092,-2.72123088871047,46.5655039932032));
#59230=CARTESIAN_POINT('Ctrl Pts',(6.26598176415498,-2.55533980739887,46.5739282760522));
#59231=CARTESIAN_POINT('Ctrl Pts',(6.33367975492169,-2.38933668938462,46.5823582483504));
#59232=CARTESIAN_POINT('Ctrl Pts',(6.3947576090331,-2.22068899836572,46.5907882206486));
#59233=CARTESIAN_POINT('Ctrl Pts',(6.44902891123204,-2.04995490245353,46.5992181929467));
#59234=CARTESIAN_POINT('Ctrl Pts',(6.5033196145456,-1.87915977185763,46.6076511788239));
#59235=CARTESIAN_POINT('Ctrl Pts',(6.55079881906786,-1.70627706873265,46.6160841647011));
#59236=CARTESIAN_POINT('Ctrl Pts',(6.5913304168321,-1.5318786949834,46.6245171505783));
#59237=CARTESIAN_POINT('Ctrl Pts',(6.6318993034193,-1.35731987579298,46.6329578947512));
#59238=CARTESIAN_POINT('Ctrl Pts',(6.66550774326317,-1.18124292626535,46.641398638924));
#59239=CARTESIAN_POINT('Ctrl Pts',(6.69207082851838,-1.00422956842213,46.6498393830968));
#59240=CARTESIAN_POINT('Ctrl Pts',(6.70675826779258,-0.906354155266412,
46.6545064959821));
#59241=CARTESIAN_POINT('Ctrl Pts',(6.71929266270581,-0.808192573016185,
46.6591736088674));
#59242=CARTESIAN_POINT('Ctrl Pts',(6.72966648202166,-0.709843673462194,
46.6638407217526));
#59243=CARTESIAN_POINT('Ctrl Pts',(6.74776269580049,-0.538282683526237,
46.6719820889705));
#59244=CARTESIAN_POINT('Ctrl Pts',(6.7593172142716,-0.365810598614877,46.6801234561884));
#59245=CARTESIAN_POINT('Ctrl Pts',(6.76424799388039,-0.192971700736592,
46.6882648234062));
#59246=CARTESIAN_POINT('Ctrl Pts',(6.76917446929359,-0.0202836780708488,
46.6963990838297));
#59247=CARTESIAN_POINT('Ctrl Pts',(6.76748870466451,0.152770156792283,46.7045333442532));
#59248=CARTESIAN_POINT('Ctrl Pts',(6.75916030829398,0.325639258664043,46.7126676046766));
#59249=CARTESIAN_POINT('Ctrl Pts',(6.75083759325464,0.49839043547832,46.7207963162014));
#59250=CARTESIAN_POINT('Ctrl Pts',(6.73588128581851,0.670956766066609,46.7289250277262));
#59251=CARTESIAN_POINT('Ctrl Pts',(6.71431305172587,0.842786594235866,46.7370537392511));
#59252=CARTESIAN_POINT('Ctrl Pts',(6.69275510312545,1.0145344799358,46.7451785743436));
#59253=CARTESIAN_POINT('Ctrl Pts',(6.66459155230309,1.18554620019801,46.7533034094361));
#59254=CARTESIAN_POINT('Ctrl Pts',(6.62989600427889,1.35527413184449,46.7614282445286));
#59255=CARTESIAN_POINT('Ctrl Pts',(6.59521016937061,1.52495454768074,46.7695508050508));
#59256=CARTESIAN_POINT('Ctrl Pts',(6.55399605363946,1.693351532603,46.777673365573));
#59257=CARTESIAN_POINT('Ctrl Pts',(6.50637856122733,1.8599266162947,46.7857959260951));
#59258=CARTESIAN_POINT('Ctrl Pts',(6.45875853806897,2.02651055302006,46.7939189183103));
#59259=CARTESIAN_POINT('Ctrl Pts',(6.40473455520926,2.1912720420392,46.8020419105255));
#59260=CARTESIAN_POINT('Ctrl Pts',(6.34448173438675,2.35368658109632,46.8101649027407));
#59261=CARTESIAN_POINT('Ctrl Pts',(6.31372450553582,2.43659425377132,46.8143114427218));
#59262=CARTESIAN_POINT('Ctrl Pts',(6.28134496883979,2.51889061900879,46.8184579827029));
#59263=CARTESIAN_POINT('Ctrl Pts',(6.24737131521594,2.6005077676902,46.822604522684));
#59264=CARTESIAN_POINT('Ctrl Pts',(6.17376591854954,2.7773348664176,46.8315881817124));
#59265=CARTESIAN_POINT('Ctrl Pts',(6.09271162714002,2.95088512263563,46.8405718407408));
#59266=CARTESIAN_POINT('Ctrl Pts',(6.00452678470492,3.12056839241848,46.8495554997691));
#59267=CARTESIAN_POINT('Ctrl Pts',(5.91619044164476,3.29054317626114,46.8585545926285));
#59268=CARTESIAN_POINT('Ctrl Pts',(5.82069917312599,3.4566374830664,46.867553685488));
#59269=CARTESIAN_POINT('Ctrl Pts',(5.71841621935872,3.61828757040884,46.8765527783473));
#59270=CARTESIAN_POINT('Ctrl Pts',(5.61589344064769,3.78031668203322,46.8855729715647));
#59271=CARTESIAN_POINT('Ctrl Pts',(5.50654724276295,3.93788052181485,46.894593164782));
#59272=CARTESIAN_POINT('Ctrl Pts',(5.39078459887529,4.0904437911465,46.9036133579994));
#59273=CARTESIAN_POINT('Ctrl Pts',(5.27490471632333,4.24316156899073,46.9126426864211));
#59274=CARTESIAN_POINT('Ctrl Pts',(5.15259555508884,4.39086847241206,46.9216720148428));
#59275=CARTESIAN_POINT('Ctrl Pts',(5.02430409185478,4.53306269453351,46.9307013432645));
#59276=CARTESIAN_POINT('Ctrl Pts',(4.89583176351692,4.67545738184644,46.9397434012193));
#59277=CARTESIAN_POINT('Ctrl Pts',(4.76136042990209,4.81232367046866,46.948785459174));
#59278=CARTESIAN_POINT('Ctrl Pts',(4.62137521545124,4.94319533480248,46.9578275171288));
#59279=CARTESIAN_POINT('Ctrl Pts',(4.49989236789182,5.0567692040892,46.9656744526244));
#59280=CARTESIAN_POINT('Ctrl Pts',(4.37425753037591,5.16582891700249,46.97352138812));
#59281=CARTESIAN_POINT('Ctrl Pts',(4.24480826106292,5.27009410037544,46.9813683236157));
#59282=CARTESIAN_POINT('Ctrl Pts',(4.10203802238213,5.38508868624877,46.9900227475423));
#59283=CARTESIAN_POINT('Ctrl Pts',(3.95450121372337,5.49435153419774,46.9986771714689));
#59284=CARTESIAN_POINT('Ctrl Pts',(3.8026753874517,5.59749487696675,47.0073315953956));
#59285=CARTESIAN_POINT('Ctrl Pts',(3.65101725419665,5.70052429696837,47.0159764604316));
#59286=CARTESIAN_POINT('Ctrl Pts',(3.4950798062013,5.7974475277724,47.0246213254677));
#59287=CARTESIAN_POINT('Ctrl Pts',(3.33537168233416,5.88791854059509,47.0332661905038));
#59288=CARTESIAN_POINT('Ctrl Pts',(3.25748541499414,5.9320393362103,47.0374821079726));
#59289=CARTESIAN_POINT('Ctrl Pts',(3.17870283742253,5.97462622669391,47.0416980254413));
#59290=CARTESIAN_POINT('Ctrl Pts',(3.09908550384709,6.01564277861018,47.0459139429101));
#59291=CARTESIAN_POINT('Ctrl Pts',(3.09908550384733,6.01564277861006,45.0456868593144));
#59292=CARTESIAN_POINT('Ctrl Pts',(2.93958034937513,6.0978152297023,45.0541389626605));
#59293=CARTESIAN_POINT('Ctrl Pts',(2.77691659048998,6.17358242935526,45.0625910660065));
#59294=CARTESIAN_POINT('Ctrl Pts',(2.61164101840684,6.24272538167225,45.0710431693525));
#59295=CARTESIAN_POINT('Ctrl Pts',(2.57801047698548,6.25679470173318,45.0727630170475));
#59296=CARTESIAN_POINT('Ctrl Pts',(2.54427184984424,6.27058990954399,45.0744828647424));
#59297=CARTESIAN_POINT('Ctrl Pts',(2.51042982486944,6.28410941139682,45.0762027124373));
#59298=CARTESIAN_POINT('Ctrl Pts',(2.34676818089706,6.34949036601073,45.0845199777707));
#59299=CARTESIAN_POINT('Ctrl Pts',(2.18039267880978,6.40853692688432,45.0928372431041));
#59300=CARTESIAN_POINT('Ctrl Pts',(2.01182858200964,6.461024280763,45.1011545084375));
#59301=CARTESIAN_POINT('Ctrl Pts',(1.84340665605461,6.51346736559745,45.1094647587976));
#59302=CARTESIAN_POINT('Ctrl Pts',(1.67280014357719,6.5593621627641,45.1177750091577));
#59303=CARTESIAN_POINT('Ctrl Pts',(1.50055322763242,6.59853233765221,45.1260852595178));
#59304=CARTESIAN_POINT('Ctrl Pts',(1.32842004367123,6.63767664907761,45.1343900227476));
#59305=CARTESIAN_POINT('Ctrl Pts',(1.15464895255644,6.67010510892785,45.1426947859775));
#59306=CARTESIAN_POINT('Ctrl Pts',(0.979798425707771,6.69569145383661,45.1509995492073));
#59307=CARTESIAN_POINT('Ctrl Pts',(0.805031342462777,6.72126558821983,45.1593003491699));
#59308=CARTESIAN_POINT('Ctrl Pts',(0.629186193557567,6.74000406473415,45.1676011491325));
#59309=CARTESIAN_POINT('Ctrl Pts',(0.452830976215294,6.75183183343453,45.1759019490951));
#59310=CARTESIAN_POINT('Ctrl Pts',(0.276527648575783,6.7636561220031,45.18420030668));
#59311=CARTESIAN_POINT('Ctrl Pts',(0.0997148982905996,6.76857373261156,
45.192498664265));
#59312=CARTESIAN_POINT('Ctrl Pts',(-0.0770346015696344,6.76656151011435,
45.2007970218499));
#59313=CARTESIAN_POINT('Ctrl Pts',(-0.253802085286102,6.76454908287813,
45.2090962237737));
#59314=CARTESIAN_POINT('Ctrl Pts',(-0.430505957846561,6.75560541012814,
45.2173954256975));
#59315=CARTESIAN_POINT('Ctrl Pts',(-0.606573397413491,6.73975947000709,
45.2256946276213));
#59316=CARTESIAN_POINT('Ctrl Pts',(-0.782658686881366,6.72391192340808,
45.2339946709268));
#59317=CARTESIAN_POINT('Ctrl Pts',(-0.958107068082406,6.70116074533084,
45.2422947142323));
#59318=CARTESIAN_POINT('Ctrl Pts',(-1.1323507814872,6.67158682081447,45.2505947575379));
#59319=CARTESIAN_POINT('Ctrl Pts',(-1.30664108473885,6.64200498872665,45.2588970201358));
#59320=CARTESIAN_POINT('Ctrl Pts',(-1.47972573516905,6.60559683243518,45.2671992827337));
#59321=CARTESIAN_POINT('Ctrl Pts',(-1.65104691460278,6.56249442558092,45.2755015453317));
#59322=CARTESIAN_POINT('Ctrl Pts',(-1.82244234554509,6.51937333791474,45.2838074061743));
#59323=CARTESIAN_POINT('Ctrl Pts',(-1.99207244505875,6.4695523021355,45.2921132670169));
#59324=CARTESIAN_POINT('Ctrl Pts',(-2.15939412250235,6.41321339296474,45.3004191278595));
#59325=CARTESIAN_POINT('Ctrl Pts',(-2.32691358597379,6.35680788722844,45.3087348068156));
#59326=CARTESIAN_POINT('Ctrl Pts',(-2.49211884542283,6.29386922571135,45.3170504857718));
#59327=CARTESIAN_POINT('Ctrl Pts',(-2.65448527687942,6.2246282551515,45.3253661647279));
#59328=CARTESIAN_POINT('Ctrl Pts',(-2.8169544038108,6.15534349022921,45.3336871032847));
#59329=CARTESIAN_POINT('Ctrl Pts',(-2.9765808080228,6.07974861552979,45.3420080418416));
#59330=CARTESIAN_POINT('Ctrl Pts',(-3.13286396257183,5.9981207383662,45.3503289803984));
#59331=CARTESIAN_POINT('Ctrl Pts',(-3.28937940229686,5.91637153689312,45.3586622864473));
#59332=CARTESIAN_POINT('Ctrl Pts',(-3.44254136015966,5.82857158587743,45.3669955924963));
#59333=CARTESIAN_POINT('Ctrl Pts',(-3.59187666795456,5.73504237143926,45.3753288985452));
#59334=CARTESIAN_POINT('Ctrl Pts',(-3.70179627127209,5.66619934763298,45.3814627037969));
#59335=CARTESIAN_POINT('Ctrl Pts',(-3.80964325951199,5.59425321995921,45.3875965090487));
#59336=CARTESIAN_POINT('Ctrl Pts',(-3.91524047656804,5.51934606730211,45.3937303143004));
#59337=CARTESIAN_POINT('Ctrl Pts',(-4.0532153760656,5.42147126389677,45.4017448357692));
#59338=CARTESIAN_POINT('Ctrl Pts',(-4.18778596920639,5.31822896559392,45.4097593572381));
#59339=CARTESIAN_POINT('Ctrl Pts',(-4.31849079120842,5.2098873583071,45.4177738787069));
#59340=CARTESIAN_POINT('Ctrl Pts',(-4.44903199527607,5.10168137440218,45.4257783674973));
#59341=CARTESIAN_POINT('Ctrl Pts',(-4.57571676755245,4.98838901765393,45.4337828562878));
#59342=CARTESIAN_POINT('Ctrl Pts',(-4.69811078084983,4.87032279123906,45.4417873450782));
#59343=CARTESIAN_POINT('Ctrl Pts',(-4.82037907632526,4.75237783733117,45.4497836120049));
#59344=CARTESIAN_POINT('Ctrl Pts',(-4.93836511173299,4.62966902965933,45.4577798789316));
#59345=CARTESIAN_POINT('Ctrl Pts',(-5.05166609793072,4.50255023681218,45.4657761458583));
#59346=CARTESIAN_POINT('Ctrl Pts',(-5.16487609682491,4.37553352777365,45.473765991316));
#59347=CARTESIAN_POINT('Ctrl Pts',(-5.27340828304388,4.24411416140957,45.4817558367738));
#59348=CARTESIAN_POINT('Ctrl Pts',(-5.3768954784377,4.10868397591689,45.4897456822315));
#59349=CARTESIAN_POINT('Ctrl Pts',(-5.48032271791807,3.97333225269628,45.4977308987254));
#59350=CARTESIAN_POINT('Ctrl Pts',(-5.57871055502915,3.83397463479472,45.5057161152193));
#59351=CARTESIAN_POINT('Ctrl Pts',(-5.67173112246984,3.69103712720518,45.5137013317132));
#59352=CARTESIAN_POINT('Ctrl Pts',(-5.76473112548316,3.54813121937979,45.5216847828836));
#59353=CARTESIAN_POINT('Ctrl Pts',(-5.85236600804091,3.40164730950946,45.5296682340538));
#59354=CARTESIAN_POINT('Ctrl Pts',(-5.93435038671638,3.25204158763063,45.5376516852241));
#59355=CARTESIAN_POINT('Ctrl Pts',(-6.01632816088129,3.10244791771323,45.5456344932623));
#59356=CARTESIAN_POINT('Ctrl Pts',(-6.09265615419054,2.94973326750943,45.5536173013006));
#59357=CARTESIAN_POINT('Ctrl Pts',(-6.1630944028326,2.79437942695215,45.5616001093388));
#59358=CARTESIAN_POINT('Ctrl Pts',(-6.23354122773228,2.63900667118072,45.5695838893293));
#59359=CARTESIAN_POINT('Ctrl Pts',(-6.2980967247161,2.4809944302798,45.5775676693197));
#59360=CARTESIAN_POINT('Ctrl Pts',(-6.35656873276757,2.32084530841711,45.5855514493102));
#59361=CARTESIAN_POINT('Ctrl Pts',(-6.41505969468335,2.16064427377041,45.5935378172653));
#59362=CARTESIAN_POINT('Ctrl Pts',(-6.46746311446471,1.99830533514858,45.6015241852202));
#59363=CARTESIAN_POINT('Ctrl Pts',(-6.51363649930655,1.83434690146154,45.6095105531753));
#59364=CARTESIAN_POINT('Ctrl Pts',(-6.5598607569089,1.67020782218919,45.6175057203246));
#59365=CARTESIAN_POINT('Ctrl Pts',(-6.59984117190231,1.50444604950245,45.6255008874739));
#59366=CARTESIAN_POINT('Ctrl Pts',(-6.63348610337766,1.33759153566978,45.6334960546232));
#59367=CARTESIAN_POINT('Ctrl Pts',(-6.66715123024904,1.17063686728674,45.6414960208777));
#59368=CARTESIAN_POINT('Ctrl Pts',(-6.69447324239003,1.00258852399637,45.6494959871323));
#59369=CARTESIAN_POINT('Ctrl Pts',(-6.71541239859187,0.833981604616404,
45.6574959533868));
#59370=CARTESIAN_POINT('Ctrl Pts',(-6.73638267762508,0.665124077013908,
45.6655078103593));
#59371=CARTESIAN_POINT('Ctrl Pts',(-6.75095112627625,0.495706690858887,
45.6735196673318));
#59372=CARTESIAN_POINT('Ctrl Pts',(-6.75913011130805,0.326265441640491,
45.6815315243043));
#59373=CARTESIAN_POINT('Ctrl Pts',(-6.76445500583179,0.215951414099029,
45.6867476107933));
#59374=CARTESIAN_POINT('Ctrl Pts',(-6.76707272562536,0.105627227563015,
45.6919636972822));
#59375=CARTESIAN_POINT('Ctrl Pts',(-6.76699846313023,-0.00456070095141469,
45.6971797837712));
#59376=CARTESIAN_POINT('',(-6.7669992409897,-0.00233727624500557,45.3028202161897));
#59377=CARTESIAN_POINT('Ctrl Pts',(3.09908550384713,6.01564277861016,44.6513967904261));
#59378=CARTESIAN_POINT('Ctrl Pts',(2.93373232018324,6.10082796552483,44.6601462383254));
#59379=CARTESIAN_POINT('Ctrl Pts',(2.76486502144423,6.17919158180192,44.6688956862247));
#59380=CARTESIAN_POINT('Ctrl Pts',(2.59305716434351,6.2504674659138,44.677645134124));
#59381=CARTESIAN_POINT('Ctrl Pts',(2.42125069459277,6.32174277447227,44.6863945113714));
#59382=CARTESIAN_POINT('Ctrl Pts',(2.24650397871048,6.38593035557829,44.6951438886188));
#59383=CARTESIAN_POINT('Ctrl Pts',(2.06941053323756,6.44281220003544,44.7038932658662));
#59384=CARTESIAN_POINT('Ctrl Pts',(1.89231845896665,6.49969360406691,44.7126425753688));
#59385=CARTESIAN_POINT('Ctrl Pts',(1.71287996431483,6.54926929700887,44.7213918848714));
#59386=CARTESIAN_POINT('Ctrl Pts',(1.53170449173479,6.59137090065485,44.730141194374));
#59387=CARTESIAN_POINT('Ctrl Pts',(1.35053036178141,6.63347219230089,44.7388904390386));
#59388=CARTESIAN_POINT('Ctrl Pts',(1.16761955878812,6.6680994406246,44.7476396837032));
#59389=CARTESIAN_POINT('Ctrl Pts',(0.98359330931013,6.69513503985397,44.7563889283678));
#59390=CARTESIAN_POINT('Ctrl Pts',(0.799568362459666,6.72217044771218,44.7651381111009));
#59391=CARTESIAN_POINT('Ctrl Pts',(0.614428268438323,6.74161427235979,44.7738872938341));
#59392=CARTESIAN_POINT('Ctrl Pts',(0.42880181633004,6.75340047696803,44.7826364765673));
#59393=CARTESIAN_POINT('Ctrl Pts',(0.243176616522572,6.76518660206243,44.7913856002754));
#59394=CARTESIAN_POINT('Ctrl Pts',(0.0570653511652667,6.76931519233997,
44.8001347239836));
#59395=CARTESIAN_POINT('Ctrl Pts',(-0.128899900800206,6.76577222610795,
44.8088838476917));
#59396=CARTESIAN_POINT('Ctrl Pts',(-0.314863959942114,6.76222928260132,
44.8176329152809));
#59397=CARTESIAN_POINT('Ctrl Pts',(-0.500681721080689,6.75101488651276,
44.8263819828702));
#59398=CARTESIAN_POINT('Ctrl Pts',(-0.685722110173223,6.73216712415992,
44.8351310504595));
#59399=CARTESIAN_POINT('Ctrl Pts',(-0.870761373827468,6.71331947644147,
44.8438800648358));
#59400=CARTESIAN_POINT('Ctrl Pts',(-1.05502298984322,6.68683858439999,44.8526290792122));
#59401=CARTESIAN_POINT('Ctrl Pts',(-1.23788117676032,6.65281438131431,44.8613780935885));
#59402=CARTESIAN_POINT('Ctrl Pts',(-1.43009641451759,6.61704912302384,44.8705748044761));
#59403=CARTESIAN_POINT('Ctrl Pts',(-1.62076048992657,6.57294837083175,44.8797715153636));
#59404=CARTESIAN_POINT('Ctrl Pts',(-1.80915798961087,6.52067760042062,44.8889682262511));
#59405=CARTESIAN_POINT('Ctrl Pts',(-1.98840443002961,6.47094578577424,44.8977182239576));
#59406=CARTESIAN_POINT('Ctrl Pts',(-2.16559895952135,6.41381888474494,44.9064682216641));
#59407=CARTESIAN_POINT('Ctrl Pts',(-2.34013966242259,6.34949095285257,44.9152182193706));
#59408=CARTESIAN_POINT('Ctrl Pts',(-2.51467682553956,6.28516432556709,44.9239680396222));
#59409=CARTESIAN_POINT('Ctrl Pts',(-2.68656000078787,6.21363705879685,44.9327178598738));
#59410=CARTESIAN_POINT('Ctrl Pts',(-2.85520533840837,6.13515211510883,44.9414676801254));
#59411=CARTESIAN_POINT('Ctrl Pts',(-3.02384747998275,6.05666865881147,44.9502173345567));
#59412=CARTESIAN_POINT('Ctrl Pts',(-3.18925164684484,5.97122791039872,44.9589669889879));
#59413=CARTESIAN_POINT('Ctrl Pts',(-3.35085601829104,5.87912008251938,44.9677166434192));
#59414=CARTESIAN_POINT('Ctrl Pts',(-3.51245754191351,5.78701387778214,44.9764661436623));
#59415=CARTESIAN_POINT('Ctrl Pts',(-3.67025915510856,5.68824097061034,44.9852156439054));
#59416=CARTESIAN_POINT('Ctrl Pts',(-3.82372487928742,5.58313684656918,44.9939651441486));
#59417=CARTESIAN_POINT('Ctrl Pts',(-3.97718810300709,5.47803443501838,45.0027145018337));
#59418=CARTESIAN_POINT('Ctrl Pts',(-4.1263153426294,5.36660117496442,45.0114638595188));
#59419=CARTESIAN_POINT('Ctrl Pts',(-4.27060009886142,5.24921554097418,45.0202132172039));
#59420=CARTESIAN_POINT('Ctrl Pts',(-4.41488269594124,5.13183166360367,45.0289624439591));
#59421=CARTESIAN_POINT('Ctrl Pts',(-4.55432273234995,5.00849577139556,45.0377116707143));
#59422=CARTESIAN_POINT('Ctrl Pts',(-4.68844662480109,4.87962675277437,45.0464608974695));
#59423=CARTESIAN_POINT('Ctrl Pts',(-4.82256868835036,4.75075949140003,45.0552100049209));
#59424=CARTESIAN_POINT('Ctrl Pts',(-4.95137454637721,4.61635945312676,45.0639591123724));
#59425=CARTESIAN_POINT('Ctrl Pts',(-5.07442674460918,4.47688309134772,45.0727082198239));
#59426=CARTESIAN_POINT('Ctrl Pts',(-5.19747742838393,4.33740844616527,45.0814572195962));
#59427=CARTESIAN_POINT('Ctrl Pts',(-5.31477440450794,4.19285781736198,45.0902062193686));
#59428=CARTESIAN_POINT('Ctrl Pts',(-5.42591931531033,4.04372211999568,45.098955219141));
#59429=CARTESIAN_POINT('Ctrl Pts',(-5.53707636462871,3.89457013500959,45.1077051744216));
#59430=CARTESIAN_POINT('Ctrl Pts',(-5.64207983273368,3.74083230916574,45.1164551297022));
#59431=CARTESIAN_POINT('Ctrl Pts',(-5.74057303468654,3.58303087251978,45.1252050849828));
#59432=CARTESIAN_POINT('Ctrl Pts',(-5.83906243363682,3.42523552887573,45.1339547024116));
#59433=CARTESIAN_POINT('Ctrl Pts',(-5.93104191768352,3.26337713157127,45.1427043198404));
#59434=CARTESIAN_POINT('Ctrl Pts',(-6.01619906699591,3.09800545291282,45.1514539372692));
#59435=CARTESIAN_POINT('Ctrl Pts',(-6.10135338095319,2.93263928039728,45.1602032633746));
#59436=CARTESIAN_POINT('Ctrl Pts',(-6.17968568352777,2.76376031540362,45.1689525894799));
#59437=CARTESIAN_POINT('Ctrl Pts',(-6.25092992694826,2.59194213831687,45.1777019155853));
#59438=CARTESIAN_POINT('Ctrl Pts',(-6.32217217691047,2.42012876880967,45.1864509968791));
#59439=CARTESIAN_POINT('Ctrl Pts',(-6.38632665483798,2.2453766164782,45.1952000781729));
#59440=CARTESIAN_POINT('Ctrl Pts',(-6.44317547869301,2.06827917621609,45.2039491594667));
#59441=CARTESIAN_POINT('Ctrl Pts',(-6.50002944235889,1.89116572423585,45.2126990317817));
#59442=CARTESIAN_POINT('Ctrl Pts',(-6.54957634250353,1.7117068328937,45.2214489040967));
#59443=CARTESIAN_POINT('Ctrl Pts',(-6.59164787708353,1.53051209225546,45.2301987764116));
#59444=CARTESIAN_POINT('Ctrl Pts',(-6.63371649074977,1.34932993148191,45.2389480412464));
#59445=CARTESIAN_POINT('Ctrl Pts',(-6.668310712571,1.16641244174144,45.2476973060812));
#59446=CARTESIAN_POINT('Ctrl Pts',(-6.69531304840315,0.982380875161198,
45.256446570916));
#59447=CARTESIAN_POINT('Ctrl Pts',(-6.7223167703303,0.798339861797004,45.2651962848717));
#59448=CARTESIAN_POINT('Ctrl Pts',(-6.7417277847788,0.61318494073129,45.2739459988274));
#59449=CARTESIAN_POINT('Ctrl Pts',(-6.75348015835511,0.427545027691661,
45.282695712783));
#59450=CARTESIAN_POINT('Ctrl Pts',(-6.76249038365207,0.28521995354942,45.2894038805852));
#59451=CARTESIAN_POINT('Ctrl Pts',(-6.76699999999988,0.142609995761396,
45.2961120483875));
#59452=CARTESIAN_POINT('Ctrl Pts',(-6.767,5.50082243727984E-12,45.3028202161897));
#59453=CARTESIAN_POINT('Ctrl Pts',(-6.76699857274565,-0.0043950492956634,
45.3028202161897));
#59454=CARTESIAN_POINT('Ctrl Pts',(-6.76686460262846,-0.210667045539541,
45.3125155163845));
#59455=CARTESIAN_POINT('Ctrl Pts',(-6.75729411431099,-0.416736582006849,
45.3222108165793));
#59456=CARTESIAN_POINT('Ctrl Pts',(-6.73837284507612,-0.621788067383695,
45.3319061167741));
#59457=CARTESIAN_POINT('Ctrl Pts',(-6.72034007666234,-0.817210789971848,
45.3411461471835));
#59458=CARTESIAN_POINT('Ctrl Pts',(-6.69381460588411,-1.01170871981791,
45.3503861775929));
#59459=CARTESIAN_POINT('Ctrl Pts',(-6.65892323893038,-1.20458718988415,
45.3596262080024));
#59460=CARTESIAN_POINT('Ctrl Pts',(-6.62398604063929,-1.39771901426128,
45.3688783755961));
#59461=CARTESIAN_POINT('Ctrl Pts',(-6.58066101984478,-1.58922693698234,
45.3781305431897));
#59462=CARTESIAN_POINT('Ctrl Pts',(-6.52912587635335,-1.77842747693941,
45.3873827107835));
#59463=CARTESIAN_POINT('Ctrl Pts',(-6.4775270261816,-1.96786190269752,45.3966463157157));
#59464=CARTESIAN_POINT('Ctrl Pts',(-6.41769781049481,-2.15498305559458,
45.405909920648));
#59465=CARTESIAN_POINT('Ctrl Pts',(-6.34986606512067,-2.33912162040134,
45.4151735255802));
#59466=CARTESIAN_POINT('Ctrl Pts',(-6.34012656891899,-2.36556081701386,
45.4165036232293));
#59467=CARTESIAN_POINT('Ctrl Pts',(-6.33022217370865,-2.39193855499759,
45.4178337208783));
#59468=CARTESIAN_POINT('Ctrl Pts',(-6.32015363622328,-2.41825288473594,
45.4191638185273));
#59469=CARTESIAN_POINT('Ctrl Pts',(-6.25464887440804,-2.58945092659074,
45.427817282828));
#59470=CARTESIAN_POINT('Ctrl Pts',(-6.18214232253387,-2.75809489593996,
45.4364707471288));
#59471=CARTESIAN_POINT('Ctrl Pts',(-6.10285146591681,-2.92360958148606,
45.4451242114295));
#59472=CARTESIAN_POINT('Ctrl Pts',(-6.02363365239697,-3.08897179415212,
45.4537697041196));
#59473=CARTESIAN_POINT('Ctrl Pts',(-5.93764413027185,-3.25121019943543,
45.4624151968098));
#59474=CARTESIAN_POINT('Ctrl Pts',(-5.84514838106999,-3.40976969944817,
45.4710606895));
#59475=CARTESIAN_POINT('Ctrl Pts',(-5.74987005603456,-3.57309918983049,
45.4799662669965));
#59476=CARTESIAN_POINT('Ctrl Pts',(-5.64768803982555,-3.73252466433785,
45.4888718444931));
#59477=CARTESIAN_POINT('Ctrl Pts',(-5.5389445730861,-3.88746472862199,45.4977774219897));
#59478=CARTESIAN_POINT('Ctrl Pts',(-5.4335772386222,-4.0375944059699,45.5064065101622));
#59479=CARTESIAN_POINT('Ctrl Pts',(-5.32204994745615,-4.18351273053596,
45.5150355983347));
#59480=CARTESIAN_POINT('Ctrl Pts',(-5.20471931157317,-4.32471801251102,
45.5236646865071));
#59481=CARTESIAN_POINT('Ctrl Pts',(-5.08174949327091,-4.47270994775557,
45.5327085086658));
#59482=CARTESIAN_POINT('Ctrl Pts',(-4.95240490224127,-4.6155243387253,45.5417523308244));
#59483=CARTESIAN_POINT('Ctrl Pts',(-4.81714573443428,-4.75261990624347,
45.5507961529831));
#59484=CARTESIAN_POINT('Ctrl Pts',(-4.68188656662729,-4.88971547376163,
45.5598399751417));
#59485=CARTESIAN_POINT('Ctrl Pts',(-4.54071306800496,-5.02109191921025,
45.5688837973004));
#59486=CARTESIAN_POINT('Ctrl Pts',(-4.39413283355317,-5.14624966758221,
45.577927619459));
#59487=CARTESIAN_POINT('Ctrl Pts',(-4.25756952768939,-5.26285444677407,
45.5863534093088));
#59488=CARTESIAN_POINT('Ctrl Pts',(-4.11637314747104,-5.37401052896704,
45.5947791991586));
#59489=CARTESIAN_POINT('Ctrl Pts',(-3.9710112762364,-5.47935748459648,45.6032049890084));
#59490=CARTESIAN_POINT('Ctrl Pts',(-3.82561567615772,-5.58472888426344,
45.6116327339249));
#59491=CARTESIAN_POINT('Ctrl Pts',(-3.67605292636013,-5.68428827529069,
45.6200604788414));
#59492=CARTESIAN_POINT('Ctrl Pts',(-3.52282042112096,-5.77771799939502,
45.6284882237579));
#59493=CARTESIAN_POINT('Ctrl Pts',(-3.36953161062352,-5.87118205423574,
45.6369190654479));
#59494=CARTESIAN_POINT('Ctrl Pts',(-3.21257063890073,-5.95851177868701,
45.6453499071378));
#59495=CARTESIAN_POINT('Ctrl Pts',(-3.05246070212078,-6.03943479656899,
45.6537807488278));
#59496=CARTESIAN_POINT('Ctrl Pts',(-2.89220364474537,-6.12043217237539,
45.6622193373851));
#59497=CARTESIAN_POINT('Ctrl Pts',(-2.72879213744786,-6.19501093041115,
45.6706579259424));
#59498=CARTESIAN_POINT('Ctrl Pts',(-2.56277163846469,-6.26294583475548,
45.6790965144998));
#59499=CARTESIAN_POINT('Ctrl Pts',(-2.39666408566866,-6.33091636116146,
45.6875395278801));
#59500=CARTESIAN_POINT('Ctrl Pts',(-2.22794512218614,-6.39223596776628,
45.6959825412603));
#59501=CARTESIAN_POINT('Ctrl Pts',(-2.05717721685793,-6.44672869744343,
45.7044255546406));
#59502=CARTESIAN_POINT('Ctrl Pts',(-1.88622990794259,-6.50127867553127,
45.7128774379949));
#59503=CARTESIAN_POINT('Ctrl Pts',(-1.7132296751096,-6.548987356646,45.7213293213492));
#59504=CARTESIAN_POINT('Ctrl Pts',(-1.53875211389063,-6.58972920020217,
45.7297812047035));
#59505=CARTESIAN_POINT('Ctrl Pts',(-1.49120146630198,-6.60083263970188,
45.7320846099324));
#59506=CARTESIAN_POINT('Ctrl Pts',(-1.44354114170434,-6.61141892278309,
45.7343880151614));
#59507=CARTESIAN_POINT('Ctrl Pts',(-1.39578288781783,-6.62148617230867,
45.7366914203903));
#59508=CARTESIAN_POINT('Ctrl Pts',(-1.22333469483533,-6.65783756390512,
45.7450086857237));
#59509=CARTESIAN_POINT('Ctrl Pts',(-1.0492989249379,-6.68748304993526,45.753325951057));
#59510=CARTESIAN_POINT('Ctrl Pts',(-0.874231609361912,-6.71029120777873,
45.7616432163904));
#59511=CARTESIAN_POINT('Ctrl Pts',(-0.699311949595541,-6.7330801286961,
45.7699534667505));
#59512=CARTESIAN_POINT('Ctrl Pts',(-0.523362820761848,-6.74904316629383,
45.7782637171106));
#59513=CARTESIAN_POINT('Ctrl Pts',(-0.346950581447075,-6.75809990263784,
45.7865739674707));
#59514=CARTESIAN_POINT('Ctrl Pts',(-0.170654824414324,-6.76715065895846,
45.7948787307005));
#59515=CARTESIAN_POINT('Ctrl Pts',(0.00610308757387329,-6.76930418286158,
45.8031834939304));
#59516=CARTESIAN_POINT('Ctrl Pts',(0.182751304352238,-6.76453183603696,
45.8114882571603));
#59517=CARTESIAN_POINT('Ctrl Pts',(0.359315219618329,-6.75976176671087,
45.8197890571229));
#59518=CARTESIAN_POINT('Ctrl Pts',(0.535769197016702,-6.7480724230201,45.8280898570855));
#59519=CARTESIAN_POINT('Ctrl Pts',(0.711540782673459,-6.72948725495431,
45.8363906570481));
#59520=CARTESIAN_POINT('Ctrl Pts',(0.887260650351361,-6.71090755527708,
45.844689014633));
#59521=CARTESIAN_POINT('Ctrl Pts',(1.06229818101648,-6.68543611212831,45.852987372218));
#59522=CARTESIAN_POINT('Ctrl Pts',(1.23608521204884,-6.65314830351422,45.8612857298029));
#59523=CARTESIAN_POINT('Ctrl Pts',(1.40988992551327,-6.62085720968962,45.8695849317267));
#59524=CARTESIAN_POINT('Ctrl Pts',(1.58244354178506,-6.58174842075848,45.8778841336504));
#59525=CARTESIAN_POINT('Ctrl Pts',(1.75318669042906,-6.53594870148951,45.8861833355742));
#59526=CARTESIAN_POINT('Ctrl Pts',(1.92394714919171,-6.49014433899719,45.8944833788797));
#59527=CARTESIAN_POINT('Ctrl Pts',(2.09289643820234,-6.43764778375086,45.9027834221853));
#59528=CARTESIAN_POINT('Ctrl Pts',(2.25948907429872,-6.37863607075406,45.9110834654909));
#59529=CARTESIAN_POINT('Ctrl Pts',(2.42612625447195,-6.31960857901492,45.9193857280888));
#59530=CARTESIAN_POINT('Ctrl Pts',(2.590405197851,-6.25406257363528,45.9276879906866));
#59531=CARTESIAN_POINT('Ctrl Pts',(2.75179899218133,-6.18222381563704,45.9359902532846));
#59532=CARTESIAN_POINT('Ctrl Pts',(2.91326273543907,-6.11035392233964,45.9442961141272));
#59533=CARTESIAN_POINT('Ctrl Pts',(3.07183851986749,-6.03218598223624,45.9526019749698));
#59534=CARTESIAN_POINT('Ctrl Pts',(3.22702251580944,-5.94799249179578,45.9609078358124));
#59535=CARTESIAN_POINT('Ctrl Pts',(3.38238995018334,-5.86369947870948,45.9692235147685));
#59536=CARTESIAN_POINT('Ctrl Pts',(3.53435727943124,-5.77336685058202,45.9775391937246));
#59537=CARTESIAN_POINT('Ctrl Pts',(3.68244722952413,-5.67731198735547,45.9858548726807));
#59538=CARTESIAN_POINT('Ctrl Pts',(3.83063084533104,-5.58119637019292,45.9941758112376));
#59539=CARTESIAN_POINT('Ctrl Pts',(3.97493190742218,-5.4793515005047,46.0024967497944));
#59540=CARTESIAN_POINT('Ctrl Pts',(4.11490481376219,-5.37213620207798,46.0108176883513));
#59541=CARTESIAN_POINT('Ctrl Pts',(4.25508576319729,-5.26476154850811,46.0191509944002));
#59542=CARTESIAN_POINT('Ctrl Pts',(4.39092543330336,-5.15200073634286,46.0274843004491));
#59543=CARTESIAN_POINT('Ctrl Pts',(4.52201278480097,-5.03425162006197,46.035817606498));
#59544=CARTESIAN_POINT('Ctrl Pts',(4.61850081492207,-4.94758131855199,46.0419514117498));
#59545=CARTESIAN_POINT('Ctrl Pts',(4.71241486627321,-4.85820923611743,46.0480852170016));
#59546=CARTESIAN_POINT('Ctrl Pts',(4.8036047670012,-4.76630572272104,46.0542190222533));
#59547=CARTESIAN_POINT('Ctrl Pts',(4.92360064917607,-4.64537080474297,46.0622904354954));
#59548=CARTESIAN_POINT('Ctrl Pts',(5.03924729246588,-4.51967888634194,46.0703618487374));
#59549=CARTESIAN_POINT('Ctrl Pts',(5.15013365027661,-4.38957997811733,46.0784332619794));
#59550=CARTESIAN_POINT('Ctrl Pts',(5.26088079944952,-4.25964439829626,46.0864945422307));
#59551=CARTESIAN_POINT('Ctrl Pts',(5.36687931527553,-4.12531311737569,46.0945558224819));
#59552=CARTESIAN_POINT('Ctrl Pts',(5.46775273160348,-3.9869749266885,46.1026171027331));
#59553=CARTESIAN_POINT('Ctrl Pts',(5.5685216317191,-3.8487800699364,46.1106700305908));
#59554=CARTESIAN_POINT('Ctrl Pts',(5.66417578187042,-3.70658686404281,46.1187229584484));
#59555=CARTESIAN_POINT('Ctrl Pts',(5.75437705612355,-3.56081924505567,46.126775886306));
#59556=CARTESIAN_POINT('Ctrl Pts',(5.84450462371335,-3.41517073796477,46.1348222338304));
#59557=CARTESIAN_POINT('Ctrl Pts',(5.92918798858885,-3.26595394666839,46.1428685813548));
#59558=CARTESIAN_POINT('Ctrl Pts',(6.00813073389935,-3.11362394716736,46.1509149288792));
#59559=CARTESIAN_POINT('Ctrl Pts',(6.08702624088287,-2.96138509998561,46.1589564615723));
#59560=CARTESIAN_POINT('Ctrl Pts',(6.16018779544525,-2.80603708340868,46.1669979942655));
#59561=CARTESIAN_POINT('Ctrl Pts',(6.22736363127136,-2.64806178249655,46.1750395269586));
#59562=CARTESIAN_POINT('Ctrl Pts',(6.29583090490721,-2.48704944789376,46.1832356560069));
#59563=CARTESIAN_POINT('Ctrl Pts',(6.3580797627172,-2.32330812057301,46.1914317850551));
#59564=CARTESIAN_POINT('Ctrl Pts',(6.41389379559058,-2.15737233200129,46.1996279141033));
#59565=CARTESIAN_POINT('Ctrl Pts',(6.4686361545347,-1.99462264286348,46.2076666709394));
#59566=CARTESIAN_POINT('Ctrl Pts',(6.51718845418104,-1.82976237334537,46.2157054277755));
#59567=CARTESIAN_POINT('Ctrl Pts',(6.55939608412578,-1.66331356381034,46.2237441846116));
#59568=CARTESIAN_POINT('Ctrl Pts',(6.60160779932296,-1.49684864378987,46.2317837195144));
#59569=CARTESIAN_POINT('Ctrl Pts',(6.63747353013455,-1.32879523960759,46.2398232544172));
#59570=CARTESIAN_POINT('Ctrl Pts',(6.66688933868066,-1.1596876932115,46.24786278932));
#59571=CARTESIAN_POINT('Ctrl Pts',(6.6963138187065,-0.990530295639011,46.2559046941956));
#59572=CARTESIAN_POINT('Ctrl Pts',(6.71928452786946,-0.820318505058142,
46.2639465990711));
#59573=CARTESIAN_POINT('Ctrl Pts',(6.73574917293496,-0.649593780224284,
46.2719885039466));
#59574=CARTESIAN_POINT('Ctrl Pts',(6.75276920805537,-0.473110120780893,
46.2803016806274));
#59575=CARTESIAN_POINT('Ctrl Pts',(6.76283653056089,-0.29607875144971,46.2886148573082));
#59576=CARTESIAN_POINT('Ctrl Pts',(6.7659518508028,-0.119098919466973,46.296928033989));
#59577=CARTESIAN_POINT('Ctrl Pts',(6.76897074579287,0.0524030407257231,
46.3049839015996));
#59578=CARTESIAN_POINT('Ctrl Pts',(6.76546166354127,0.223856239532683,46.3130397692101));
#59579=CARTESIAN_POINT('Ctrl Pts',(6.75547814928279,0.39472012181132,46.3210956368206));
#59580=CARTESIAN_POINT('Ctrl Pts',(6.74501631619583,0.573770240908646,46.3295374680366));
#59581=CARTESIAN_POINT('Ctrl Pts',(6.72744444476342,0.752172701315157,46.3379792992525));
#59582=CARTESIAN_POINT('Ctrl Pts',(6.70288428426154,0.929317637731945,46.3464211304685));
#59583=CARTESIAN_POINT('Ctrl Pts',(6.67832412375965,1.10646257414873,46.3548629616844));
#59584=CARTESIAN_POINT('Ctrl Pts',(6.64677583983355,1.28234954782513,46.3633047929004));
#59585=CARTESIAN_POINT('Ctrl Pts',(6.60842066002361,1.4563877849574,46.3717466241164));
#59586=CARTESIAN_POINT('Ctrl Pts',(6.57102255228109,1.62608326744095,46.37997780736));
#59587=CARTESIAN_POINT('Ctrl Pts',(6.52702917216304,1.79458571382543,46.3882089906037));
#59588=CARTESIAN_POINT('Ctrl Pts',(6.47652826378856,1.96134409228671,46.3964401738473));
#59589=CARTESIAN_POINT('Ctrl Pts',(6.42608815898527,2.12790169208354,46.4046614466685));
#59590=CARTESIAN_POINT('Ctrl Pts',(6.36915623117908,2.2927190655902,46.4128827194897));
#59591=CARTESIAN_POINT('Ctrl Pts',(6.30587133907991,2.45525470266743,46.4211039923109));
#59592=CARTESIAN_POINT('Ctrl Pts',(6.24264994472732,2.6176272574299,46.4293170162076));
#59593=CARTESIAN_POINT('Ctrl Pts',(6.17308841055718,2.77772230349296,46.4375300401042));
#59594=CARTESIAN_POINT('Ctrl Pts',(6.09737558966443,2.93501276293041,46.4457430640009));
#59595=CARTESIAN_POINT('Ctrl Pts',(6.01845506532761,3.09896710230928,46.4543040467337));
#59596=CARTESIAN_POINT('Ctrl Pts',(5.9328507410126,3.25987364252657,46.4628650294665));
#59597=CARTESIAN_POINT('Ctrl Pts',(5.84083313343287,3.41715631884067,46.4714260121993));
#59598=CARTESIAN_POINT('Ctrl Pts',(5.75268393266127,3.56782685437153,46.4796270924661));
#59599=CARTESIAN_POINT('Ctrl Pts',(5.65864985070985,3.71517164022411,46.4878281727329));
#59600=CARTESIAN_POINT('Ctrl Pts',(5.55901639374952,3.85870778033581,46.4960292529997));
#59601=CARTESIAN_POINT('Ctrl Pts',(5.45941581825502,4.00219655002767,46.5042276267103));
#59602=CARTESIAN_POINT('Ctrl Pts',(5.35421975207708,4.14187888304339,46.5124260004211));
#59603=CARTESIAN_POINT('Ctrl Pts',(5.24375747124643,4.2773001511172,46.5206243741317));
#59604=CARTESIAN_POINT('Ctrl Pts',(5.13331158006555,4.41270132629472,46.5288215314229));
#59605=CARTESIAN_POINT('Ctrl Pts',(5.01760125753553,4.5438424184666,46.537018688714));
#59606=CARTESIAN_POINT('Ctrl Pts',(4.8969966066966,4.67030119307117,46.5452158460052));
#59607=CARTESIAN_POINT('Ctrl Pts',(4.77638794301987,4.79676417529583,46.5534132760376));
#59608=CARTESIAN_POINT('Ctrl Pts',(4.65088487507611,4.91854427121403,46.56161070607));
#59609=CARTESIAN_POINT('Ctrl Pts',(4.52089499289623,5.03525545163359,46.5698081361024));
#59610=CARTESIAN_POINT('Ctrl Pts',(4.3908347845312,5.1520297742912,46.5780100010491));
#59611=CARTESIAN_POINT('Ctrl Pts',(4.25628318015729,5.26372946396891,46.5862118659958));
#59612=CARTESIAN_POINT('Ctrl Pts',(4.11768199038142,5.37000782365245,46.5944137309424));
#59613=CARTESIAN_POINT('Ctrl Pts',(3.97903649457181,5.47632015687256,46.6026182177433));
#59614=CARTESIAN_POINT('Ctrl Pts',(3.83633912354135,5.57720749587675,46.6108227045441));
#59615=CARTESIAN_POINT('Ctrl Pts',(3.69006137002425,5.67236600418685,46.6190271913449));
#59616=CARTESIAN_POINT('Ctrl Pts',(3.54365877316924,5.76760572721022,46.6272386804102));
#59617=CARTESIAN_POINT('Ctrl Pts',(3.39366999761389,5.85710666947437,46.6354501694755));
#59618=CARTESIAN_POINT('Ctrl Pts',(3.24059241283144,5.94061022235084,46.6436616585408));
#59619=CARTESIAN_POINT('Ctrl Pts',(3.193708143015,5.96618550895636,46.6461766555567));
#59620=CARTESIAN_POINT('Ctrl Pts',(3.14653428003767,5.99119853883744,46.6486916525726));
#59621=CARTESIAN_POINT('Ctrl Pts',(3.09908550384732,6.01564277861007,46.6512066495885));
#59622=CARTESIAN_POINT('Origin',(0.,0.,-63.6971797838103));
#59623=CARTESIAN_POINT('',(3.09908550384708,6.01564277861019,49.0457563580462));
#59624=CARTESIAN_POINT('',(3.09908550384732,6.01564277861007,48.6513967904261));
#59625=CARTESIAN_POINT('',(3.09908550384721,6.01564277861012,-63.6971797838103));
#59626=CARTESIAN_POINT('',(-6.76699762275617,0.00351474313282491,47.6971797838098));
#59627=CARTESIAN_POINT('Ctrl Pts',(-6.767,5.76061319672769E-12,47.6971797838098));
#59628=CARTESIAN_POINT('Ctrl Pts',(-6.76700000000016,-0.186007249554285,
47.7059292956226));
#59629=CARTESIAN_POINT('Ctrl Pts',(-6.75932637294278,-0.37201435581051,
47.7146788074353));
#59630=CARTESIAN_POINT('Ctrl Pts',(-6.74400518263408,-0.557389537580933,
47.7234283192481));
#59631=CARTESIAN_POINT('Ctrl Pts',(-6.72868405703788,-0.742763936377517,
47.7321777941053));
#59632=CARTESIAN_POINT('Ctrl Pts',(-6.70571545643634,-0.927506130399944,
47.7409272689625));
#59633=CARTESIAN_POINT('Ctrl Pts',(-6.67517739401656,-1.11098864009058,
47.7496767438197));
#59634=CARTESIAN_POINT('Ctrl Pts',(-6.64463945804483,-1.29447039004059,
47.7584261824482));
#59635=CARTESIAN_POINT('Ctrl Pts',(-6.60653217002831,-1.476692183388,47.7671756210767));
#59636=CARTESIAN_POINT('Ctrl Pts',(-6.56098496085599,-1.65703510627311,
47.7759250597052));
#59637=CARTESIAN_POINT('Ctrl Pts',(-6.5154379364968,-1.83737729739572,47.7846744628319));
#59638=CARTESIAN_POINT('Ctrl Pts',(-6.46245112157023,-2.0158403554455,47.7934238659585));
#59639=CARTESIAN_POINT('Ctrl Pts',(-6.40220448361843,-2.19181813797041,
47.8021732690852));
#59640=CARTESIAN_POINT('Ctrl Pts',(-6.34195808512111,-2.36779522105933,
47.8109226374367));
#59641=CARTESIAN_POINT('Ctrl Pts',(-6.27445201416505,-2.54128677725372,
47.8196720057882));
#59642=CARTESIAN_POINT('Ctrl Pts',(-6.19991555052887,-2.71170355428285,
47.8284213741397));
#59643=CARTESIAN_POINT('Ctrl Pts',(-6.12537937695282,-2.88211966813174,
47.8371707084429));
#59644=CARTESIAN_POINT('Ctrl Pts',(-6.04381298028509,-3.04946076419556,
47.8459200427461));
#59645=CARTESIAN_POINT('Ctrl Pts',(-5.95549339309033,-3.21315848424218,
47.8546693770493));
#59646=CARTESIAN_POINT('Ctrl Pts',(-5.8671741422586,-3.37685558084993,47.8634186780308));
#59647=CARTESIAN_POINT('Ctrl Pts',(-5.77210188844118,-3.53690907699916,
47.8721679790124));
#59648=CARTESIAN_POINT('Ctrl Pts',(-5.67059953311423,-3.69277537023913,
47.880917279994));
#59649=CARTESIAN_POINT('Ctrl Pts',(-5.56909755592743,-3.84864108280976,
47.8896665483806));
#59650=CARTESIAN_POINT('Ctrl Pts',(-5.46116568154985,-4.00031938354804,
47.8984158167672));
#59651=CARTESIAN_POINT('Ctrl Pts',(-5.34717048488377,-4.14729511918165,
47.9071650851539));
#59652=CARTESIAN_POINT('Ctrl Pts',(-5.23317570343316,-4.29427031947164,
47.9159143216722));
#59653=CARTESIAN_POINT('Ctrl Pts',(-5.11311781951571,-4.43654276249527,
47.9246635581906));
#59654=CARTESIAN_POINT('Ctrl Pts',(-4.98740458929283,-4.57362924412341,
47.9334127947089));
#59655=CARTESIAN_POINT('Ctrl Pts',(-4.86169180652779,-4.71071523781227,
47.9421620000856));
#59656=CARTESIAN_POINT('Ctrl Pts',(-4.73032391141612,-4.84261509584451,
47.9509112054623));
#59657=CARTESIAN_POINT('Ctrl Pts',(-4.59374706947367,-4.96888084599561,
47.959660410839));
#59658=CARTESIAN_POINT('Ctrl Pts',(-4.45717070231578,-5.0951461572068,47.9684095858007));
#59659=CARTESIAN_POINT('Ctrl Pts',(-4.31538563497464,-5.21577720520498,
47.9771587607624));
#59660=CARTESIAN_POINT('Ctrl Pts',(-4.16887340952175,-5.33036429293369,
47.9859079357241));
#59661=CARTESIAN_POINT('Ctrl Pts',(-4.02236168122654,-5.44495099183581,
47.9946570809974));
#59662=CARTESIAN_POINT('Ctrl Pts',(-3.87112305263349,-5.55349359497811,
48.0034062262706));
#59663=CARTESIAN_POINT('Ctrl Pts',(-3.71567116929162,-5.65562346357102,
48.0121553715439));
#59664=CARTESIAN_POINT('Ctrl Pts',(-3.56021980053478,-5.75775299408824,
48.0209044878552));
#59665=CARTESIAN_POINT('Ctrl Pts',(-3.40055544442251,-5.85346967519782,
48.0296536041666));
#59666=CARTESIAN_POINT('Ctrl Pts',(-3.23722035887009,-5.94244843041292,
48.038402720478));
#59667=CARTESIAN_POINT('Ctrl Pts',(-3.07388580043665,-6.03142689847362,
48.047151808554));
#59668=CARTESIAN_POINT('Ctrl Pts',(-2.90688078789406,-6.11366734707814,
48.05590089663));
#59669=CARTESIAN_POINT('Ctrl Pts',(-2.73677250610585,-6.18889047001344,
48.064649984706));
#59670=CARTESIAN_POINT('Ctrl Pts',(-2.56666475917162,-6.2641133564324,48.0733990452732));
#59671=CARTESIAN_POINT('Ctrl Pts',(-2.39345402457356,-6.33231884545155,
48.0821481058403));
#59672=CARTESIAN_POINT('Ctrl Pts',(-2.21772855944364,-6.39327529804779,
48.0908971664075));
#59673=CARTESIAN_POINT('Ctrl Pts',(-2.04200363223899,-6.45423156404605,
48.0996462001923));
#59674=CARTESIAN_POINT('Ctrl Pts',(-1.86376426061351,-6.50793874412362,
48.1083952339771));
#59675=CARTESIAN_POINT('Ctrl Pts',(-1.68361577622014,-6.55421443943229,
48.1171442677619));
#59676=CARTESIAN_POINT('Ctrl Pts',(-1.50346782833576,-6.60048999692505,
48.1258932754908));
#59677=CARTESIAN_POINT('Ctrl Pts',(-1.32141105657782,-6.63933404265082,
48.1346422832196));
#59678=CARTESIAN_POINT('Ctrl Pts',(-1.13806375346965,-6.67061465631456,
48.1433912909485));
#59679=CARTESIAN_POINT('Ctrl Pts',(-0.954716981174169,-6.70189517941712,
48.152140273348));
#59680=CARTESIAN_POINT('Ctrl Pts',(-0.7700799674463,-6.72561226608958,48.1608892557474));
#59681=CARTESIAN_POINT('Ctrl Pts',(-0.584779764076936,-6.74168536995951,
48.1696382381468));
#59682=CARTESIAN_POINT('Ctrl Pts',(-0.39148958759668,-6.75845153117851,
48.1787644685625));
#59683=CARTESIAN_POINT('Ctrl Pts',(-0.197478091808809,-6.76689985146384,
48.1878906989781));
#59684=CARTESIAN_POINT('Ctrl Pts',(-0.00346214753445197,-6.76699911434415,
48.1970169293937));
#59685=CARTESIAN_POINT('Ctrl Pts',(0.184490798481292,-6.76709527525944,
48.2058579651088));
#59686=CARTESIAN_POINT('Ctrl Pts',(0.372447602151505,-6.75935633790781,
48.214699000824));
#59687=CARTESIAN_POINT('Ctrl Pts',(0.559756448191021,-6.7438091401454,48.2235400365391));
#59688=CARTESIAN_POINT('Ctrl Pts',(0.745136131040126,-6.7284220687319,48.2322900151524));
#59689=CARTESIAN_POINT('Ctrl Pts',(0.929880851941783,-6.70538686355768,
48.2410399937657));
#59690=CARTESIAN_POINT('Ctrl Pts',(1.11336305057134,-6.67478177303367,48.249789972379));
#59691=CARTESIAN_POINT('Ctrl Pts',(1.29684337089801,-6.64417699581324,48.258539861419));
#59692=CARTESIAN_POINT('Ctrl Pts',(1.47906091204875,-6.60600253548131,48.267289750459));
#59693=CARTESIAN_POINT('Ctrl Pts',(1.65939671094913,-6.5603880644129,48.276039639499));
#59694=CARTESIAN_POINT('Ctrl Pts',(1.83973072368852,-6.51477404513937,48.2847894418745));
#59695=CARTESIAN_POINT('Ctrl Pts',(2.01818275356728,-6.46172023288757,48.2935392442499));
#59696=CARTESIAN_POINT('Ctrl Pts',(2.19414664033019,-6.40140683918213,48.3022890466254));
#59697=CARTESIAN_POINT('Ctrl Pts',(2.37010884270956,-6.34109402281611,48.311038765245));
#59698=CARTESIAN_POINT('Ctrl Pts',(2.54358267847507,-6.27352185699913,48.3197884838645));
#59699=CARTESIAN_POINT('Ctrl Pts',(2.71397890841447,-6.1989198643539,48.3285382024841));
#59700=CARTESIAN_POINT('Ctrl Pts',(2.88437356388658,-6.12431856103377,48.3372878402559));
#59701=CARTESIAN_POINT('Ctrl Pts',(3.05169040786899,-6.04268767582695,48.3460374780277));
#59702=CARTESIAN_POINT('Ctrl Pts',(3.21536112511791,-5.95430447954088,48.3547871157995));
#59703=CARTESIAN_POINT('Ctrl Pts',(3.37903038442584,-5.86592207055191,48.3635366756316));
#59704=CARTESIAN_POINT('Ctrl Pts',(3.5390533297972,-5.77078760703532,48.3722862354637));
#59705=CARTESIAN_POINT('Ctrl Pts',(3.69488643041644,-5.6692242208546,48.3810357952957));
#59706=CARTESIAN_POINT('Ctrl Pts',(3.850718194685,-5.56766170563326,48.3897852800957));
#59707=CARTESIAN_POINT('Ctrl Pts',(4.00235994598988,-5.45967053456425,48.3985347648957));
#59708=CARTESIAN_POINT('Ctrl Pts',(4.1492966297407,-5.34561750206863,48.4072842496957));
#59709=CARTESIAN_POINT('Ctrl Pts',(4.29623210224804,-5.23156540974662,48.4160336623711));
#59710=CARTESIAN_POINT('Ctrl Pts',(4.43846235841869,-5.11145173172401,48.4247830750464));
#59711=CARTESIAN_POINT('Ctrl Pts',(4.57550431797173,-4.98568443006796,48.4335324877218));
#59712=CARTESIAN_POINT('Ctrl Pts',(4.71254519337245,-4.85991812336931,48.4422818311797));
#59713=CARTESIAN_POINT('Ctrl Pts',(4.84439764314741,-4.7284984763135,48.4510311746375));
#59714=CARTESIAN_POINT('Ctrl Pts',(4.9706138419645,-4.59187184425599,48.4597805180954));
#59715=CARTESIAN_POINT('Ctrl Pts',(5.09682908419994,-4.45524624767991,48.4685297952428));
#59716=CARTESIAN_POINT('Ctrl Pts',(5.21740796649981,-4.31341395557123,48.4772790723902));
#59717=CARTESIAN_POINT('Ctrl Pts',(5.33194095942083,-4.16685668163071,48.4860283495376));
#59718=CARTESIAN_POINT('Ctrl Pts',(5.44647312234966,-4.0203004697544,48.4947775632811));
#59719=CARTESIAN_POINT('Ctrl Pts',(5.55495930712123,-3.86901957035783,48.5035267770246));
#59720=CARTESIAN_POINT('Ctrl Pts',(5.65703106079633,-3.71352778058622,48.5122759907682));
#59721=CARTESIAN_POINT('Ctrl Pts',(5.75910210868577,-3.5580370659786,48.5210251440144));
#59722=CARTESIAN_POINT('Ctrl Pts',(5.85475865698394,-3.39833575881167,48.5297742972606));
#59723=CARTESIAN_POINT('Ctrl Pts',(5.94367583068912,-3.23496624706998,48.5385234505067));
#59724=CARTESIAN_POINT('Ctrl Pts',(6.03259241909938,-3.07159781070374,48.5472725461619));
#59725=CARTESIAN_POINT('Ctrl Pts',(6.11476958470839,-2.90456146976105,48.556021641817));
#59726=CARTESIAN_POINT('Ctrl Pts',(6.18992823574268,-2.73442451648525,48.5647707374721));
#59727=CARTESIAN_POINT('Ctrl Pts',(6.26508641700826,-2.56428862662683,48.5735197784422));
#59728=CARTESIAN_POINT('Ctrl Pts',(6.33322605570196,-2.39105242531544,48.5822688194124));
#59729=CARTESIAN_POINT('Ctrl Pts',(6.39411573747675,-2.21530425353994,48.5910178603825));
#59730=CARTESIAN_POINT('Ctrl Pts',(6.45500505889042,-2.03955712188826,48.5997668495735));
#59731=CARTESIAN_POINT('Ctrl Pts',(6.50864441544854,-1.86129832025836,48.6085158387645));
#59732=CARTESIAN_POINT('Ctrl Pts',(6.55485164049839,-1.68113324012572,48.6172648279555));
#59733=CARTESIAN_POINT('Ctrl Pts',(6.60199852639052,-1.49730435913154,48.6261917348324));
#59734=CARTESIAN_POINT('Ctrl Pts',(6.64140767440961,-1.31149113173899,48.6351186417092));
#59735=CARTESIAN_POINT('Ctrl Pts',(6.67293975269562,-1.1243505044667,48.6440455485861));
#59736=CARTESIAN_POINT('Ctrl Pts',(6.70384664831472,-0.940920291566195,
48.6527954627701));
#59737=CARTESIAN_POINT('Ctrl Pts',(6.72718585889637,-0.756215114280447,
48.6615453769542));
#59738=CARTESIAN_POINT('Ctrl Pts',(6.74287810451843,-0.570862389377701,
48.6702952911381));
#59739=CARTESIAN_POINT('Ctrl Pts',(6.75857004154109,-0.38551330957069,48.6790450332487));
#59740=CARTESIAN_POINT('Ctrl Pts',(6.76661529035548,-0.199516993261825,
48.6877947753593));
#59741=CARTESIAN_POINT('Ctrl Pts',(6.76698652348896,-0.013505218207691,
48.6965445174699));
#59742=CARTESIAN_POINT('Ctrl Pts',(6.76735774981531,0.172503146035245,48.7052940991405));
#59743=CARTESIAN_POINT('Ctrl Pts',(6.76005524147499,0.358526681829814,48.7140436808112));
#59744=CARTESIAN_POINT('Ctrl Pts',(6.74510380214911,0.543933542111204,48.7227932624818));
#59745=CARTESIAN_POINT('Ctrl Pts',(6.7301526171102,0.729337249080968,48.7315426953437));
#59746=CARTESIAN_POINT('Ctrl Pts',(6.70755278444657,0.914124015850821,48.7402921282056));
#59747=CARTESIAN_POINT('Ctrl Pts',(6.67738106408353,1.09766621748993,48.7490415610676));
#59748=CARTESIAN_POINT('Ctrl Pts',(6.6472098167733,1.28120554142928,48.7577908567499));
#59749=CARTESIAN_POINT('Ctrl Pts',(6.6094669658161,1.46350005650224,48.7665401524323));
#59750=CARTESIAN_POINT('Ctrl Pts',(6.56428070011094,1.64393062206138,48.7752894481146));
#59751=CARTESIAN_POINT('Ctrl Pts',(6.51909508282852,1.82435859844252,48.7840386182446));
#59752=CARTESIAN_POINT('Ctrl Pts',(6.46646633415786,2.00292240086159,48.7927877883746));
#59753=CARTESIAN_POINT('Ctrl Pts',(6.40657319597331,2.17901557696048,48.8015369585046));
#59754=CARTESIAN_POINT('Ctrl Pts',(6.34668083768443,2.35510646007035,48.8102860147076));
#59755=CARTESIAN_POINT('Ctrl Pts',(6.27952437144043,2.5287265099614,48.8190350709107));
#59756=CARTESIAN_POINT('Ctrl Pts',(6.20533187335302,2.69928607997543,48.8277841271138));
#59757=CARTESIAN_POINT('Ctrl Pts',(6.12831449784424,2.87633970115033,48.8368663034027));
#59758=CARTESIAN_POINT('Ctrl Pts',(6.04371489463328,3.05009490562002,48.8459484796915));
#59759=CARTESIAN_POINT('Ctrl Pts',(5.95184265120669,3.21991584599302,48.8550306559803));
#59760=CARTESIAN_POINT('Ctrl Pts',(5.86333281335674,3.38352155904987,48.8637804363348));
#59761=CARTESIAN_POINT('Ctrl Pts',(5.76807337235869,3.54347560903525,48.8725302166892));
#59762=CARTESIAN_POINT('Ctrl Pts',(5.66638790086541,3.69923467178363,48.8812799970436));
#59763=CARTESIAN_POINT('Ctrl Pts',(5.56470608502931,3.85498813489493,48.8900294628379));
#59764=CARTESIAN_POINT('Ctrl Pts',(5.45659885767141,4.00654667256004,48.8987789286322));
#59765=CARTESIAN_POINT('Ctrl Pts',(5.34243340580697,4.15339551505966,48.9075283944264));
#59766=CARTESIAN_POINT('Ctrl Pts',(5.22827145140793,4.30023985883628,48.9162775921803));
#59767=CARTESIAN_POINT('Ctrl Pts',(5.10805181978298,4.44237456992802,48.9250267899341));
#59768=CARTESIAN_POINT('Ctrl Pts',(4.9821828128277,4.57931691626211,48.933775987688));
#59769=CARTESIAN_POINT('Ctrl Pts',(4.8563169929645,4.71625579511934,48.942524963906));
#59770=CARTESIAN_POINT('Ctrl Pts',(4.7248022779206,4.84800236135553,48.951273940124));
#59771=CARTESIAN_POINT('Ctrl Pts',(4.58808530848337,4.97410918678703,48.9600229163421));
#59772=CARTESIAN_POINT('Ctrl Pts',(4.45135945057195,5.10022421088813,48.9687724613633));
#59773=CARTESIAN_POINT('Ctrl Pts',(4.30943087208266,5.220698566118,48.9775220063844));
#59774=CARTESIAN_POINT('Ctrl Pts',(4.16278164322694,5.33512305301507,48.9862715514057));
#59775=CARTESIAN_POINT('Ctrl Pts',(4.01614103534619,5.44954081331258,48.9950205820729));
#59776=CARTESIAN_POINT('Ctrl Pts',(3.86478055833644,5.55790924068177,49.0037696127402));
#59777=CARTESIAN_POINT('Ctrl Pts',(3.70921425812184,5.65986029751139,49.0125186434074));
#59778=CARTESIAN_POINT('Ctrl Pts',(3.55364584530371,5.76181273884498,49.0212677928873));
#59779=CARTESIAN_POINT('Ctrl Pts',(3.39387173464616,5.85734747817905,49.0300169423671));
#59780=CARTESIAN_POINT('Ctrl Pts',(3.23043456092697,5.94614005448649,49.0387660918469));
#59781=CARTESIAN_POINT('Ctrl Pts',(3.18690768806583,5.9697874481118,49.04109618058));
#59782=CARTESIAN_POINT('Ctrl Pts',(3.14312114982972,5.99295688499254,49.0434262693131));
#59783=CARTESIAN_POINT('Ctrl Pts',(3.09908550384708,6.01564277861019,49.0457563580462));
#59784=CARTESIAN_POINT('Ctrl Pts',(3.09908550384709,6.01564277861018,47.0459139429101));
#59785=CARTESIAN_POINT('Ctrl Pts',(2.93606339535898,6.09962706288626,47.0545463314129));
#59786=CARTESIAN_POINT('Ctrl Pts',(2.76953995568906,6.17702472520362,47.0631787199156));
#59787=CARTESIAN_POINT('Ctrl Pts',(2.60006334833904,6.24755628903206,47.0718111084183));
#59788=CARTESIAN_POINT('Ctrl Pts',(2.43070337527171,6.31803931283788,47.0804375560867));
#59789=CARTESIAN_POINT('Ctrl Pts',(2.25839456749121,6.3816655451314,47.0890640037551));
#59790=CARTESIAN_POINT('Ctrl Pts',(2.08370711628746,6.4382026726046,47.0976904514235));
#59791=CARTESIAN_POINT('Ctrl Pts',(1.90916134328403,6.4946939463063,47.1063099027131));
#59792=CARTESIAN_POINT('Ctrl Pts',(1.73224106521693,6.54410749540541,47.1149293540028));
#59793=CARTESIAN_POINT('Ctrl Pts',(1.55353408329108,6.58626000489299,47.1235488052924));
#59794=CARTESIAN_POINT('Ctrl Pts',(1.43892682911922,6.61329299105146,47.1290765783773));
#59795=CARTESIAN_POINT('Ctrl Pts',(1.32358510542547,6.63734061643636,47.1346043514622));
#59796=CARTESIAN_POINT('Ctrl Pts',(1.20766724045767,6.65836532764051,47.140132124547));
#59797=CARTESIAN_POINT('Ctrl Pts',(1.0309777209973,6.69041255453248,47.1485579143968));
#59798=CARTESIAN_POINT('Ctrl Pts',(0.853026240713427,6.71541981467453,47.1569837042466));
#59799=CARTESIAN_POINT('Ctrl Pts',(0.674398239450259,6.73331092514124,47.1654094940964));
#59800=CARTESIAN_POINT('Ctrl Pts',(0.495728790481579,6.75120618694745,47.1738372390129));
#59801=CARTESIAN_POINT('Ctrl Pts',(0.316382837402103,6.76198197381547,47.1822649839294));
#59802=CARTESIAN_POINT('Ctrl Pts',(0.136950059128389,6.76561406535318,47.1906927288458));
#59803=CARTESIAN_POINT('Ctrl Pts',(-0.0425486516889925,6.7692474915023,
47.1991235705357));
#59804=CARTESIAN_POINT('Ctrl Pts',(-0.222133920036509,6.76573198170366,
47.2075544122257));
#59805=CARTESIAN_POINT('Ctrl Pts',(-0.401216555870379,6.75509543050989,
47.2159852539156));
#59806=CARTESIAN_POINT('Ctrl Pts',(-0.580463745788857,6.74444910568319,
47.2244238424729));
#59807=CARTESIAN_POINT('Ctrl Pts',(-0.759207049298254,6.72666868617792,
47.2328624310302));
#59808=CARTESIAN_POINT('Ctrl Pts',(-0.936861759259506,6.70183400600442,
47.2413010195876));
#59809=CARTESIAN_POINT('Ctrl Pts',(-1.11460962349945,6.67698630362216,47.2497440329678));
#59810=CARTESIAN_POINT('Ctrl Pts',(-1.29126742893335,6.64507701701444,47.258187046348));
#59811=CARTESIAN_POINT('Ctrl Pts',(-1.46626056559307,6.6062371251558,47.2666300597283));
#59812=CARTESIAN_POINT('Ctrl Pts',(-1.64143754473994,6.5673564292836,47.2750819430825));
#59813=CARTESIAN_POINT('Ctrl Pts',(-1.81494604009456,6.52153066302154,47.2835338264368));
#59814=CARTESIAN_POINT('Ctrl Pts',(-1.98622546773283,6.46894097911934,47.2919857097911));
#59815=CARTESIAN_POINT('Ctrl Pts',(-2.03290452289036,6.45460862882231,47.2942891150203));
#59816=CARTESIAN_POINT('Ctrl Pts',(-2.07941812318807,6.43977417843863,47.2965925202495));
#59817=CARTESIAN_POINT('Ctrl Pts',(-2.12575517203482,6.42444191728489,47.2988959254787));
#59818=CARTESIAN_POINT('Ctrl Pts',(-2.29307159779326,6.36907932517157,47.3072131908121));
#59819=CARTESIAN_POINT('Ctrl Pts',(-2.45838553073322,6.30712282735392,47.3155304561456));
#59820=CARTESIAN_POINT('Ctrl Pts',(-2.6211503339279,6.23873864871335,47.323847721479));
#59821=CARTESIAN_POINT('Ctrl Pts',(-2.7837778575355,6.17041214686544,47.3321579718391));
#59822=CARTESIAN_POINT('Ctrl Pts',(-2.94386021593875,6.09566889944545,47.3404682221992));
#59823=CARTESIAN_POINT('Ctrl Pts',(-3.10086751331362,6.01472440473179,47.3487784725593));
#59824=CARTESIAN_POINT('Ctrl Pts',(-3.25777114119002,5.93383335642038,47.3570832357891));
#59825=CARTESIAN_POINT('Ctrl Pts',(-3.4116034457619,5.84674937864201,47.365387999019));
#59826=CARTESIAN_POINT('Ctrl Pts',(-3.56185584117991,5.75373547937795,47.3736927622489));
#59827=CARTESIAN_POINT('Ctrl Pts',(-3.71203653191623,5.66076596897052,47.3819935622115));
#59828=CARTESIAN_POINT('Ctrl Pts',(-3.85864042310634,5.56187235955357,47.3902943621741));
#59829=CARTESIAN_POINT('Ctrl Pts',(-4.0011846181465,5.4573629759718,47.3985951621367));
#59830=CARTESIAN_POINT('Ctrl Pts',(-4.14368687183637,5.35288434260519,47.4068935197216));
#59831=CARTESIAN_POINT('Ctrl Pts',(-4.28213153019121,5.24279343412293,47.4151918773066));
#59832=CARTESIAN_POINT('Ctrl Pts',(-4.4160655352711,5.12744129056499,47.4234902348915));
#59833=CARTESIAN_POINT('Ctrl Pts',(-4.55001316782912,5.01207741019077,47.4317894368153));
#59834=CARTESIAN_POINT('Ctrl Pts',(-4.67944896164117,4.89145144640008,47.440088638739));
#59835=CARTESIAN_POINT('Ctrl Pts',(-4.80395331463428,4.76595442181462,47.4483878406628));
#59836=CARTESIAN_POINT('Ctrl Pts',(-4.92847029000877,4.6404446742097,47.4566878839684));
#59837=CARTESIAN_POINT('Ctrl Pts',(-5.04805458255985,4.51006312818003,47.4649879272739));
#59838=CARTESIAN_POINT('Ctrl Pts',(-5.1623238872576,4.37523726020082,47.4732879705795));
#59839=CARTESIAN_POINT('Ctrl Pts',(-5.27662374565087,4.24037534204586,47.4815902331774));
#59840=CARTESIAN_POINT('Ctrl Pts',(-5.3856055587599,4.10106699889841,47.4898924957753));
#59841=CARTESIAN_POINT('Ctrl Pts',(-5.48892758899494,3.95777246980802,47.4981947583733));
#59842=CARTESIAN_POINT('Ctrl Pts',(-5.59229439954663,3.81441583610767,47.5065006192159));
#59843=CARTESIAN_POINT('Ctrl Pts',(-5.68999633505279,3.66706985528161,47.5148064800585));
#59844=CARTESIAN_POINT('Ctrl Pts',(-5.78173512256456,3.51622353847183,47.5231123409011));
#59845=CARTESIAN_POINT('Ctrl Pts',(-5.87358235179552,3.36519891067309,47.5314280198573));
#59846=CARTESIAN_POINT('Ctrl Pts',(-5.95945216866167,3.21066597756631,47.5397436988134));
#59847=CARTESIAN_POINT('Ctrl Pts',(-6.03909183422184,3.05313917433108,47.5480593777695));
#59848=CARTESIAN_POINT('Ctrl Pts',(-6.11878187123628,2.89551273664727,47.5563803163264));
#59849=CARTESIAN_POINT('Ctrl Pts',(-6.19223375406644,2.73488896844577,47.5647012548833));
#59850=CARTESIAN_POINT('Ctrl Pts',(-6.25924296835286,2.57180218195826,47.5730221934401));
#59851=CARTESIAN_POINT('Ctrl Pts',(-6.32635177908765,2.4084729979903,47.5813554994891));
#59852=CARTESIAN_POINT('Ctrl Pts',(-6.38699866499412,2.24267380630154,47.5896888055379));
#59853=CARTESIAN_POINT('Ctrl Pts',(-6.44102862009678,2.0749552561668,47.5980221115869));
#59854=CARTESIAN_POINT('Ctrl Pts',(-6.48079785698841,1.95150450114106,47.6041559168385));
#59855=CARTESIAN_POINT('Ctrl Pts',(-6.51698319977678,1.82701418374228,47.6102897220901));
#59856=CARTESIAN_POINT('Ctrl Pts',(-6.54954059514499,1.70170708188803,47.6164235273416));
#59857=CARTESIAN_POINT('Ctrl Pts',(-6.60381077106686,1.49283169781688,47.6266480150904));
#59858=CARTESIAN_POINT('Ctrl Pts',(-6.64813743337064,1.2811567617572,47.6368725028391));
#59859=CARTESIAN_POINT('Ctrl Pts',(-6.68226665206471,1.06752114297744,47.6470969905879));
#59860=CARTESIAN_POINT('Ctrl Pts',(-6.71580609236908,0.857577307251926,
47.6571447915518));
#59861=CARTESIAN_POINT('Ctrl Pts',(-6.73949747235133,0.645739900102742,
47.6671925925157));
#59862=CARTESIAN_POINT('Ctrl Pts',(-6.75314355816964,0.432829161161674,
47.6772403934795));
#59863=CARTESIAN_POINT('Ctrl Pts',(-6.76217023085786,0.291992031906009,
47.683886856923));
#59864=CARTESIAN_POINT('Ctrl Pts',(-6.76680235460557,0.150685748618224,
47.6905333203664));
#59865=CARTESIAN_POINT('Ctrl Pts',(-6.76699380863722,0.00915389892568289,
47.6971797838098));
#59866=CARTESIAN_POINT('',(-6.767,5.25875296000095E-12,47.3028202161897));
#59867=CARTESIAN_POINT('Ctrl Pts',(3.09908550384732,6.01564277861007,46.6512066495885));
#59868=CARTESIAN_POINT('Ctrl Pts',(2.94392541256584,6.09557677857692,46.6594308272786));
#59869=CARTESIAN_POINT('Ctrl Pts',(2.78582439819486,6.16942480198856,46.6676550049686));
#59870=CARTESIAN_POINT('Ctrl Pts',(2.62530703088028,6.23699061997135,46.6758791826586));
#59871=CARTESIAN_POINT('Ctrl Pts',(2.53816003698039,6.27367299288897,46.6803441970989));
#59872=CARTESIAN_POINT('Ctrl Pts',(2.45030109831904,6.30850451592851,46.6848092115392));
#59873=CARTESIAN_POINT('Ctrl Pts',(2.36181586475785,6.34145999127789,46.6892742259795));
#59874=CARTESIAN_POINT('Ctrl Pts',(2.18474318113969,6.40740901152872,46.6982094127618));
#59875=CARTESIAN_POINT('Ctrl Pts',(2.00479427769777,6.46597926066129,46.7071445995441));
#59876=CARTESIAN_POINT('Ctrl Pts',(1.82258005357805,6.51693877125598,46.7160797863264));
#59877=CARTESIAN_POINT('Ctrl Pts',(1.64063872999669,6.56782196026852,46.725001590963));
#59878=CARTESIAN_POINT('Ctrl Pts',(1.4564391036601,6.61111708534289,46.7339233955997));
#59879=CARTESIAN_POINT('Ctrl Pts',(1.27060854541588,6.64664147704058,46.7428452002363));
#59880=CARTESIAN_POINT('Ctrl Pts',(1.0852312719738,6.68207921632214,46.7517452424756));
#59881=CARTESIAN_POINT('Ctrl Pts',(0.898231259765142,6.70978400408473,46.7606452847149));
#59882=CARTESIAN_POINT('Ctrl Pts',(0.710246807896361,6.7296239472851,46.7695453269542));
#59883=CARTESIAN_POINT('Ctrl Pts',(0.522551760855276,6.74943334660119,46.7784316674476));
#59884=CARTESIAN_POINT('Ctrl Pts',(0.333875552927846,6.76140202678392,46.7873180079409));
#59885=CARTESIAN_POINT('Ctrl Pts',(0.144865307356764,6.76544921219016,46.7962043484343));
#59886=CARTESIAN_POINT('Ctrl Pts',(-0.0436616720093867,6.76948604964978,
46.8050679681062));
#59887=CARTESIAN_POINT('Ctrl Pts',(-0.232520727267387,6.76564180217864,
46.8139315877782));
#59888=CARTESIAN_POINT('Ctrl Pts',(-0.421061756595683,6.75388747293976,
46.8227952074501));
#59889=CARTESIAN_POINT('Ctrl Pts',(-0.600044585298222,6.74272903647544,
46.8312094806037));
#59890=CARTESIAN_POINT('Ctrl Pts',(-0.778740569150256,6.72444254463978,
46.8396237537572));
#59891=CARTESIAN_POINT('Ctrl Pts',(-0.956590091467695,6.69904652894021,
46.8480380269108));
#59892=CARTESIAN_POINT('Ctrl Pts',(-1.13012721043577,6.67426630271106,46.8562482751153));
#59893=CARTESIAN_POINT('Ctrl Pts',(-1.30269149555158,6.64273995661422,46.8644585233199));
#59894=CARTESIAN_POINT('Ctrl Pts',(-1.47372865793921,6.60457514475903,46.8726687715244));
#59895=CARTESIAN_POINT('Ctrl Pts',(-1.64480647927,6.56640126036723,46.8808809714686));
#59896=CARTESIAN_POINT('Ctrl Pts',(-1.81435610720646,6.52158584371817,46.8890931714128));
#59897=CARTESIAN_POINT('Ctrl Pts',(-1.98183579380467,6.47028715640926,46.897305371357));
#59898=CARTESIAN_POINT('Ctrl Pts',(-2.14938511710104,6.41896713952136,46.9055209858674));
#59899=CARTESIAN_POINT('Ctrl Pts',(-2.31486244436512,6.36115858572511,46.9137366003779));
#59900=CARTESIAN_POINT('Ctrl Pts',(-2.4777433858052,6.29706889863043,46.9219522148883));
#59901=CARTESIAN_POINT('Ctrl Pts',(-2.64080723540247,6.23290724162657,46.9301770551738));
#59902=CARTESIAN_POINT('Ctrl Pts',(-2.80126854436963,6.1624504937069,46.9384018954592));
#59903=CARTESIAN_POINT('Ctrl Pts',(-2.95862413773496,6.08595368135612,46.9466267357446));
#59904=CARTESIAN_POINT('Ctrl Pts',(-3.1160805228276,6.00940787013795,46.9548568443262));
#59905=CARTESIAN_POINT('Ctrl Pts',(-3.2704269136844,5.92681444959039,46.9630869529077));
#59906=CARTESIAN_POINT('Ctrl Pts',(-3.42118681625558,5.83847323949327,46.9713170614892));
#59907=CARTESIAN_POINT('Ctrl Pts',(-3.57215341296688,5.75001091224135,46.9795584536759));
#59908=CARTESIAN_POINT('Ctrl Pts',(-3.71952340093979,5.65578524653429,46.9877998458626));
#59909=CARTESIAN_POINT('Ctrl Pts',(-3.86285039025964,5.55613857480813,46.9960412380493));
#59910=CARTESIAN_POINT('Ctrl Pts',(-3.92522993744552,5.51276981160202,46.9996281013137));
#59911=CARTESIAN_POINT('Ctrl Pts',(-3.98684409001736,5.46837470281088,47.0032149645781));
#59912=CARTESIAN_POINT('Ctrl Pts',(-4.0476581386488,5.42298373523563,47.0068018278425));
#59913=CARTESIAN_POINT('Ctrl Pts',(-4.18954903877564,5.31707785671216,47.0151706713691));
#59914=CARTESIAN_POINT('Ctrl Pts',(-4.32742197024226,5.20549438136416,47.0235395148958));
#59915=CARTESIAN_POINT('Ctrl Pts',(-4.4608059996976,5.0885654985528,47.0319083584224));
#59916=CARTESIAN_POINT('Ctrl Pts',(-4.59406364738814,4.97174740620583,47.0402692724448));
#59917=CARTESIAN_POINT('Ctrl Pts',(-4.7228406120741,4.84959422392152,47.0486301864673));
#59918=CARTESIAN_POINT('Ctrl Pts',(-4.846697292323,4.72247968302553,47.0569911004898));
#59919=CARTESIAN_POINT('Ctrl Pts',(-4.97045817713752,4.59546345731638,47.0653455478655));
#59920=CARTESIAN_POINT('Ctrl Pts',(-5.08930612336192,4.46349376528868,47.0736999952414));
#59921=CARTESIAN_POINT('Ctrl Pts',(-5.20283660433539,4.32698281353044,47.0820544426171));
#59922=CARTESIAN_POINT('Ctrl Pts',(-5.31629902297498,4.19055370106239,47.0904038814421));
#59923=CARTESIAN_POINT('Ctrl Pts',(-5.42445011179671,4.04958901851922,47.0987533202671));
#59924=CARTESIAN_POINT('Ctrl Pts',(-5.52692385525375,3.90453604135331,47.107102759092));
#59925=CARTESIAN_POINT('Ctrl Pts',(-5.62935841990309,3.75953852232242,47.1154490056743));
#59926=CARTESIAN_POINT('Ctrl Pts',(-5.7261197672751,3.61045610331053,47.1237952522565));
#59927=CARTESIAN_POINT('Ctrl Pts',(-5.81688345084336,3.4577674761766,47.1321414988388));
#59928=CARTESIAN_POINT('Ctrl Pts',(-5.90762870315803,3.30510985530745,47.1404860505605));
#59929=CARTESIAN_POINT('Ctrl Pts',(-5.99237854344952,3.14884778015148,47.1488306022822));
#59930=CARTESIAN_POINT('Ctrl Pts',(-6.07085283775845,2.98948738453271,47.1571751540039));
#59931=CARTESIAN_POINT('Ctrl Pts',(-6.14932357433846,2.83013421371402,47.1655193274151));
#59932=CARTESIAN_POINT('Ctrl Pts',(-6.2215191806665,2.66768331008425,47.1738635008262));
#59933=CARTESIAN_POINT('Ctrl Pts',(-6.28720620812607,2.50266399992108,47.1822076742373));
#59934=CARTESIAN_POINT('Ctrl Pts',(-6.35290061801783,2.33762614357133,47.1905527854333));
#59935=CARTESIAN_POINT('Ctrl Pts',(-6.41208486491018,2.1700196241852,47.1988978966292));
#59936=CARTESIAN_POINT('Ctrl Pts',(-6.46457414151185,2.00039250370931,47.2072430078251));
#59937=CARTESIAN_POINT('Ctrl Pts',(-6.51709907580486,1.83065014995345,47.2155937881295));
#59938=CARTESIAN_POINT('Ctrl Pts',(-6.56291984934629,1.65888477997448,47.2239445684338));
#59939=CARTESIAN_POINT('Ctrl Pts',(-6.60190166241576,1.48565926099896,47.2322953487382));
#59940=CARTESIAN_POINT('Ctrl Pts',(-6.64089680252307,1.31237451996926,47.2406489839935));
#59941=CARTESIAN_POINT('Ctrl Pts',(-6.67304825266115,1.1376289709083,47.2490026192488));
#59942=CARTESIAN_POINT('Ctrl Pts',(-6.69827255134879,0.96199471300386,47.2573562545041));
#59943=CARTESIAN_POINT('Ctrl Pts',(-6.72352306873745,0.786177896917976,
47.265718572715));
#59944=CARTESIAN_POINT('Ctrl Pts',(-6.74183200456947,0.609470866823461,
47.2740808909259));
#59945=CARTESIAN_POINT('Ctrl Pts',(-6.75316778180667,0.432451050141371,
47.2824432091368));
#59946=CARTESIAN_POINT('Ctrl Pts',(-6.76237532477453,0.288665799764858,
47.2892355448211));
#59947=CARTESIAN_POINT('Ctrl Pts',(-6.7669832534489,0.144674329426934,47.2960278805054));
#59948=CARTESIAN_POINT('Ctrl Pts',(-6.76699995441783,0.00078543557435644,
47.3028202161897));
#59949=CARTESIAN_POINT('Ctrl Pts',(-6.767,5.64341228108853E-12,47.3028202161897));
#59950=CARTESIAN_POINT('Ctrl Pts',(-6.76700000000016,-0.186007249554274,
47.3115697280025));
#59951=CARTESIAN_POINT('Ctrl Pts',(-6.75932637294278,-0.37201435581037,
47.3203192398152));
#59952=CARTESIAN_POINT('Ctrl Pts',(-6.7440051826341,-0.557389537580667,
47.3290687516279));
#59953=CARTESIAN_POINT('Ctrl Pts',(-6.72868405703791,-0.742763936377251,
47.3378182264851));
#59954=CARTESIAN_POINT('Ctrl Pts',(-6.70571545643638,-0.927506130399682,
47.3465677013423));
#59955=CARTESIAN_POINT('Ctrl Pts',(-6.6751773940166,-1.11098864009032,47.3553171761995));
#59956=CARTESIAN_POINT('Ctrl Pts',(-6.64463945804486,-1.29447039004045,
47.3640666148281));
#59957=CARTESIAN_POINT('Ctrl Pts',(-6.60653217002831,-1.476692183388,47.3728160534566));
#59958=CARTESIAN_POINT('Ctrl Pts',(-6.56098496085596,-1.65703510627323,
47.3815654920851));
#59959=CARTESIAN_POINT('Ctrl Pts',(-6.51543793649677,-1.83737729739583,
47.3903148952117));
#59960=CARTESIAN_POINT('Ctrl Pts',(-6.46245112157019,-2.01584035544561,
47.3990642983384));
#59961=CARTESIAN_POINT('Ctrl Pts',(-6.40220448361839,-2.19181813797052,
47.407813701465));
#59962=CARTESIAN_POINT('Ctrl Pts',(-6.34195808512107,-2.36779522105944,
47.4165630698166));
#59963=CARTESIAN_POINT('Ctrl Pts',(-6.274452014165,-2.54128677725383,47.4253124381681));
#59964=CARTESIAN_POINT('Ctrl Pts',(-6.19991555052883,-2.71170355428296,
47.4340618065196));
#59965=CARTESIAN_POINT('Ctrl Pts',(-6.12537937695283,-2.88211966813172,
47.4428111408228));
#59966=CARTESIAN_POINT('Ctrl Pts',(-6.04381298028515,-3.04946076419543,
47.451560475126));
#59967=CARTESIAN_POINT('Ctrl Pts',(-5.95549339309045,-3.21315848424194,
47.4603098094292));
#59968=CARTESIAN_POINT('Ctrl Pts',(-5.86717414225874,-3.3768555808497,47.4690591104107));
#59969=CARTESIAN_POINT('Ctrl Pts',(-5.77210188844132,-3.53690907699893,
47.4778084113923));
#59970=CARTESIAN_POINT('Ctrl Pts',(-5.67059953311438,-3.6927753702389,47.4865577123739));
#59971=CARTESIAN_POINT('Ctrl Pts',(-5.56909755592773,-3.84864108280932,
47.4953069807605));
#59972=CARTESIAN_POINT('Ctrl Pts',(-5.4611656815503,-4.00031938354741,47.5040562491471));
#59973=CARTESIAN_POINT('Ctrl Pts',(-5.3471704848844,-4.14729511918083,47.5128055175337));
#59974=CARTESIAN_POINT('Ctrl Pts',(-5.23317570343366,-4.29427031947104,
47.5215547540521));
#59975=CARTESIAN_POINT('Ctrl Pts',(-5.11311781951606,-4.43654276249488,
47.5303039905704));
#59976=CARTESIAN_POINT('Ctrl Pts',(-4.98740458929301,-4.57362924412321,
47.5390532270888));
#59977=CARTESIAN_POINT('Ctrl Pts',(-4.86169180652789,-4.71071523781218,
47.5478024324655));
#59978=CARTESIAN_POINT('Ctrl Pts',(-4.73032391141613,-4.8426150958445,47.5565516378422));
#59979=CARTESIAN_POINT('Ctrl Pts',(-4.59374706947358,-4.96888084599569,
47.5653008432189));
#59980=CARTESIAN_POINT('Ctrl Pts',(-4.45717070231569,-5.09514615720688,
47.5740500181806));
#59981=CARTESIAN_POINT('Ctrl Pts',(-4.31538563497455,-5.21577720520505,
47.5827991931423));
#59982=CARTESIAN_POINT('Ctrl Pts',(-4.16887340952167,-5.33036429293376,
47.591548368104));
#59983=CARTESIAN_POINT('Ctrl Pts',(-4.02236168122665,-5.44495099183572,
47.6002975133772));
#59984=CARTESIAN_POINT('Ctrl Pts',(-3.87112305263381,-5.55349359497788,
47.6090466586505));
#59985=CARTESIAN_POINT('Ctrl Pts',(-3.71567116929217,-5.65562346357066,
47.6177958039237));
#59986=CARTESIAN_POINT('Ctrl Pts',(-3.56021980053566,-5.75775299408769,
47.6265449202351));
#59987=CARTESIAN_POINT('Ctrl Pts',(-3.40055544442373,-5.8534696751971,47.6352940365465));
#59988=CARTESIAN_POINT('Ctrl Pts',(-3.23722035887168,-5.94244843041206,
47.6440431528578));
#59989=CARTESIAN_POINT('Ctrl Pts',(-3.07388580043826,-6.03142689847279,
47.6527922409338));
#59990=CARTESIAN_POINT('Ctrl Pts',(-2.9068807878957,-6.11366734707737,47.6615413290098));
#59991=CARTESIAN_POINT('Ctrl Pts',(-2.7367725061075,-6.18889047001271,47.6702904170858));
#59992=CARTESIAN_POINT('Ctrl Pts',(-2.5666647591727,-6.26411335643197,47.679039477653));
#59993=CARTESIAN_POINT('Ctrl Pts',(-2.39345402457405,-6.33231884545138,
47.6877885382202));
#59994=CARTESIAN_POINT('Ctrl Pts',(-2.21772855944354,-6.39327529804783,
47.6965375987874));
#59995=CARTESIAN_POINT('Ctrl Pts',(-2.04200363223889,-6.45423156404608,
47.7052866325722));
#59996=CARTESIAN_POINT('Ctrl Pts',(-1.8637642606134,-6.50793874412365,47.714035666357));
#59997=CARTESIAN_POINT('Ctrl Pts',(-1.68361577622003,-6.55421443943231,
47.7227847001418));
#59998=CARTESIAN_POINT('Ctrl Pts',(-1.50346782833515,-6.6004899969252,47.7315337078707));
#59999=CARTESIAN_POINT('Ctrl Pts',(-1.32141105657671,-6.63933404265106,
47.7402827155996));
#60000=CARTESIAN_POINT('Ctrl Pts',(-1.13806375346802,-6.67061465631484,
47.7490317233285));
#60001=CARTESIAN_POINT('Ctrl Pts',(-0.954716981172404,-6.70189517941738,
47.7577807057279));
#60002=CARTESIAN_POINT('Ctrl Pts',(-0.770079967444401,-6.7256122660898,
47.7665296881274));
#60003=CARTESIAN_POINT('Ctrl Pts',(-0.584779764074905,-6.74168536995969,
47.7752786705268));
#60004=CARTESIAN_POINT('Ctrl Pts',(-0.391489587594772,-6.75845153117862,
47.7844049009424));
#60005=CARTESIAN_POINT('Ctrl Pts',(-0.197478091807028,-6.76689985146389,
47.7935311313581));
#60006=CARTESIAN_POINT('Ctrl Pts',(-0.00346214753279914,-6.76699911434415,
47.8026573617737));
#60007=CARTESIAN_POINT('Ctrl Pts',(0.184490798482945,-6.7670952752594,47.8114983974888));
#60008=CARTESIAN_POINT('Ctrl Pts',(0.37244760215316,-6.75935633790772,47.8203394332039));
#60009=CARTESIAN_POINT('Ctrl Pts',(0.559756448192672,-6.74380914014526,
47.8291804689191));
#60010=CARTESIAN_POINT('Ctrl Pts',(0.745136131041901,-6.72842206873171,
47.8379304475324));
#60011=CARTESIAN_POINT('Ctrl Pts',(0.929880851943675,-6.70538686355743,
47.8466804261457));
#60012=CARTESIAN_POINT('Ctrl Pts',(1.11336305057335,-6.67478177303334,47.855430404759));
#60013=CARTESIAN_POINT('Ctrl Pts',(1.29684337090001,-6.64417699581285,47.864180293799));
#60014=CARTESIAN_POINT('Ctrl Pts',(1.47906091205074,-6.60600253548086,47.8729301828389));
#60015=CARTESIAN_POINT('Ctrl Pts',(1.65939671095111,-6.5603880644124,47.8816800718789));
#60016=CARTESIAN_POINT('Ctrl Pts',(1.83973072369048,-6.51477404513881,47.8904298742544));
#60017=CARTESIAN_POINT('Ctrl Pts',(2.01818275356923,-6.46172023288696,47.8991796766299));
#60018=CARTESIAN_POINT('Ctrl Pts',(2.19414664033212,-6.40140683918147,47.9079294790054));
#60019=CARTESIAN_POINT('Ctrl Pts',(2.37010884271147,-6.34109402281539,47.9166791976249));
#60020=CARTESIAN_POINT('Ctrl Pts',(2.54358267847696,-6.27352185699836,47.9254289162445));
#60021=CARTESIAN_POINT('Ctrl Pts',(2.71397890841634,-6.19891986435309,47.934178634864));
#60022=CARTESIAN_POINT('Ctrl Pts',(2.88437356388842,-6.1243185610329,47.9429282726358));
#60023=CARTESIAN_POINT('Ctrl Pts',(3.0516904078708,-6.04268767582604,47.9516779104077));
#60024=CARTESIAN_POINT('Ctrl Pts',(3.2153611251197,-5.95430447953991,47.9604275481795));
#60025=CARTESIAN_POINT('Ctrl Pts',(3.37903038442761,-5.8659220705509,47.9691771080116));
#60026=CARTESIAN_POINT('Ctrl Pts',(3.53905332979894,-5.77078760703426,47.9779266678436));
#60027=CARTESIAN_POINT('Ctrl Pts',(3.69488643041815,-5.66922422085349,47.9866762276757));
#60028=CARTESIAN_POINT('Ctrl Pts',(3.85071819468668,-5.5676617056321,47.9954257124757));
#60029=CARTESIAN_POINT('Ctrl Pts',(4.00235994599152,-5.45967053456304,48.0041751972757));
#60030=CARTESIAN_POINT('Ctrl Pts',(4.14929662974231,-5.34561750206738,48.0129246820757));
#60031=CARTESIAN_POINT('Ctrl Pts',(4.29623210224982,-5.23156540974517,48.0216740947511));
#60032=CARTESIAN_POINT('Ctrl Pts',(4.43846235842062,-5.11145173172234,48.0304235074264));
#60033=CARTESIAN_POINT('Ctrl Pts',(4.5755043179738,-4.98568443006606,48.0391729201018));
#60034=CARTESIAN_POINT('Ctrl Pts',(4.71254519337456,-4.85991812336727,48.0479222635597));
#60035=CARTESIAN_POINT('Ctrl Pts',(4.84439764314955,-4.72849847631131,48.0566716070176));
#60036=CARTESIAN_POINT('Ctrl Pts',(4.97061384196666,-4.59187184425365,48.0654209504755));
#60037=CARTESIAN_POINT('Ctrl Pts',(5.09682908420178,-4.45524624767779,48.0741702276228));
#60038=CARTESIAN_POINT('Ctrl Pts',(5.21740796650135,-4.31341395556935,48.0829195047702));
#60039=CARTESIAN_POINT('Ctrl Pts',(5.33194095942208,-4.16685668162911,48.0916687819175));
#60040=CARTESIAN_POINT('Ctrl Pts',(5.44647312235095,-4.02030046975266,48.1004179956611));
#60041=CARTESIAN_POINT('Ctrl Pts',(5.55495930712255,-3.86901957035595,48.1091672094046));
#60042=CARTESIAN_POINT('Ctrl Pts',(5.65703106079766,-3.71352778058419,48.1179164231482));
#60043=CARTESIAN_POINT('Ctrl Pts',(5.75910210868704,-3.55803706597654,48.1266655763944));
#60044=CARTESIAN_POINT('Ctrl Pts',(5.85475865698516,-3.39833575880957,48.1354147296405));
#60045=CARTESIAN_POINT('Ctrl Pts',(5.94367583069028,-3.23496624706785,48.1441638828867));
#60046=CARTESIAN_POINT('Ctrl Pts',(6.03259241910048,-3.07159781070158,48.1529129785419));
#60047=CARTESIAN_POINT('Ctrl Pts',(6.11476958470943,-2.90456146975886,48.161662074197));
#60048=CARTESIAN_POINT('Ctrl Pts',(6.18992823574365,-2.73442451648303,48.1704111698521));
#60049=CARTESIAN_POINT('Ctrl Pts',(6.26508641700917,-2.56428862662459,48.1791602108222));
#60050=CARTESIAN_POINT('Ctrl Pts',(6.33322605570282,-2.39105242531317,48.1879092517924));
#60051=CARTESIAN_POINT('Ctrl Pts',(6.39411573747755,-2.21530425353765,48.1966582927625));
#60052=CARTESIAN_POINT('Ctrl Pts',(6.45500505889119,-2.03955712188583,48.2054072819535));
#60053=CARTESIAN_POINT('Ctrl Pts',(6.50864441544928,-1.86129832025579,48.2141562711445));
#60054=CARTESIAN_POINT('Ctrl Pts',(6.55485164049909,-1.681133240123,48.2229052603355));
#60055=CARTESIAN_POINT('Ctrl Pts',(6.60199852639114,-1.4973043591288,48.2318321672124));
#60056=CARTESIAN_POINT('Ctrl Pts',(6.64140767441016,-1.31149113173623,48.2407590740893));
#60057=CARTESIAN_POINT('Ctrl Pts',(6.67293975269609,-1.12435050446393,48.2496859809661));
#60058=CARTESIAN_POINT('Ctrl Pts',(6.70384664831511,-0.940920291563414,
48.2584358951501));
#60059=CARTESIAN_POINT('Ctrl Pts',(6.72718585889669,-0.756215114277657,
48.2671858093341));
#60060=CARTESIAN_POINT('Ctrl Pts',(6.74287810451866,-0.570862389374904,
48.2759357235181));
#60061=CARTESIAN_POINT('Ctrl Pts',(6.75857004154125,-0.385513309567886,
48.2846854656287));
#60062=CARTESIAN_POINT('Ctrl Pts',(6.76661529035556,-0.199516993259019,
48.2934352077393));
#60063=CARTESIAN_POINT('Ctrl Pts',(6.76698652348896,-0.013505218204885,
48.3021849498499));
#60064=CARTESIAN_POINT('Ctrl Pts',(6.76735774981523,0.172503146038051,48.3109345315205));
#60065=CARTESIAN_POINT('Ctrl Pts',(6.76005524147484,0.358526681832619,48.3196841131912));
#60066=CARTESIAN_POINT('Ctrl Pts',(6.74510380214888,0.543933542114002,48.3284336948618));
#60067=CARTESIAN_POINT('Ctrl Pts',(6.73015261710988,0.729337249083888,48.3371831277237));
#60068=CARTESIAN_POINT('Ctrl Pts',(6.70755278444616,0.914124015853858,48.3459325605857));
#60069=CARTESIAN_POINT('Ctrl Pts',(6.67738106408302,1.09766621749308,48.3546819934476));
#60070=CARTESIAN_POINT('Ctrl Pts',(6.64720981677269,1.28120554143241,48.36343128913));
#60071=CARTESIAN_POINT('Ctrl Pts',(6.60946696581541,1.46350005650536,48.3721805848123));
#60072=CARTESIAN_POINT('Ctrl Pts',(6.56428070011016,1.64393062206447,48.3809298804946));
#60073=CARTESIAN_POINT('Ctrl Pts',(6.51909508282766,1.82435859844559,48.3896790506246));
#60074=CARTESIAN_POINT('Ctrl Pts',(6.46646633415692,2.00292240086464,48.3984282207546));
#60075=CARTESIAN_POINT('Ctrl Pts',(6.40657319597228,2.1790155769635,48.4071773908846));
#60076=CARTESIAN_POINT('Ctrl Pts',(6.34668083768332,2.35510646007335,48.4159264470877));
#60077=CARTESIAN_POINT('Ctrl Pts',(6.27952437143923,2.52872650996436,48.4246755032908));
#60078=CARTESIAN_POINT('Ctrl Pts',(6.20533187335175,2.69928607997835,48.4334245594938));
#60079=CARTESIAN_POINT('Ctrl Pts',(6.12831449784293,2.8763397011531,48.4425067357827));
#60080=CARTESIAN_POINT('Ctrl Pts',(6.04371489463196,3.05009490562264,48.4515889120715));
#60081=CARTESIAN_POINT('Ctrl Pts',(5.95184265120535,3.21991584599549,48.4606710883604));
#60082=CARTESIAN_POINT('Ctrl Pts',(5.86333281335533,3.3835215590523,48.4694208687148));
#60083=CARTESIAN_POINT('Ctrl Pts',(5.76807337235722,3.54347560903765,48.4781706490692));
#60084=CARTESIAN_POINT('Ctrl Pts',(5.66638790086387,3.69923467178598,48.4869204294236));
#60085=CARTESIAN_POINT('Ctrl Pts',(5.56470608502771,3.85498813489724,48.4956698952179));
#60086=CARTESIAN_POINT('Ctrl Pts',(5.45659885766975,4.0065466725623,48.5044193610122));
#60087=CARTESIAN_POINT('Ctrl Pts',(5.34243340580525,4.15339551506188,48.5131688268064));
#60088=CARTESIAN_POINT('Ctrl Pts',(5.22827145140607,4.30023985883855,48.5219180245603));
#60089=CARTESIAN_POINT('Ctrl Pts',(5.10805181978097,4.44237456993034,48.5306672223142));
#60090=CARTESIAN_POINT('Ctrl Pts',(4.98218281282554,4.57931691626446,48.5394164200681));
#60091=CARTESIAN_POINT('Ctrl Pts',(4.8563169929621,4.71625579512182,48.5481653962861));
#60092=CARTESIAN_POINT('Ctrl Pts',(4.72480227791796,4.84800236135812,48.5569143725041));
#60093=CARTESIAN_POINT('Ctrl Pts',(4.58808530848046,4.97410918678971,48.5656633487221));
#60094=CARTESIAN_POINT('Ctrl Pts',(4.45135945056897,5.10022421089073,48.5744128937433));
#60095=CARTESIAN_POINT('Ctrl Pts',(4.3094308720796,5.22069856612052,48.5831624387645));
#60096=CARTESIAN_POINT('Ctrl Pts',(4.16278164322382,5.33512305301751,48.5919119837857));
#60097=CARTESIAN_POINT('Ctrl Pts',(4.0161410353432,5.44954081331478,48.600661014453));
#60098=CARTESIAN_POINT('Ctrl Pts',(3.8647805583336,5.55790924068374,48.6094100451202));
#60099=CARTESIAN_POINT('Ctrl Pts',(3.70921425811917,5.65986029751314,48.6181590757875));
#60100=CARTESIAN_POINT('Ctrl Pts',(3.55364584530089,5.76181273884673,48.6269082252673));
#60101=CARTESIAN_POINT('Ctrl Pts',(3.39387173464318,5.85734747818079,48.6356573747471));
#60102=CARTESIAN_POINT('Ctrl Pts',(3.23043456092383,5.9461400544882,48.644406524227));
#60103=CARTESIAN_POINT('Ctrl Pts',(3.18690768806381,5.96978744811287,48.64673661296));
#60104=CARTESIAN_POINT('Ctrl Pts',(3.14312114982882,5.992956884993,48.6490667016931));
#60105=CARTESIAN_POINT('Ctrl Pts',(3.09908550384732,6.01564277861007,48.6513967904261));
#60106=CARTESIAN_POINT('Origin',(0.,0.,-63.6971797838103));
#60107=CARTESIAN_POINT('',(3.0990855038473,6.01564277861008,51.0457613895064));
#60108=CARTESIAN_POINT('',(3.09908550384729,6.01564277861008,50.6513967904261));
#60109=CARTESIAN_POINT('',(3.09908550384721,6.01564277861012,-63.6971797838103));
#60110=CARTESIAN_POINT('',(-6.76800097367046,-0.00217352041212573,49.6954478291652));
#60111=CARTESIAN_POINT('Ctrl Pts',(-6.76699845293094,-0.00457580925307041,
49.6971797838098));
#60112=CARTESIAN_POINT('Ctrl Pts',(-6.7668662394862,-0.200101480569433,
49.7063448954362));
#60113=CARTESIAN_POINT('Ctrl Pts',(-6.75825574679544,-0.39532739586738,
49.7155100070625));
#60114=CARTESIAN_POINT('Ctrl Pts',(-6.74126887845904,-0.589561623852473,
49.7246751186889));
#60115=CARTESIAN_POINT('Ctrl Pts',(-6.72359310938338,-0.791673001445151,
49.7342119204967));
#60116=CARTESIAN_POINT('Ctrl Pts',(-6.69684755273203,-0.992710310089097,
49.7437487223045));
#60117=CARTESIAN_POINT('Ctrl Pts',(-6.66120365726185,-1.19191226039562,
49.7532855241123));
#60118=CARTESIAN_POINT('Ctrl Pts',(-6.62664155718862,-1.3850684137974,49.7625328831373));
#60119=CARTESIAN_POINT('Ctrl Pts',(-6.58371344390243,-1.57649885085553,
49.7717802421623));
#60120=CARTESIAN_POINT('Ctrl Pts',(-6.53262555518545,-1.76552891670967,
49.7810276011872));
#60121=CARTESIAN_POINT('Ctrl Pts',(-6.47913908640227,-1.96343395781248,
49.7907091243865));
#60122=CARTESIAN_POINT('Ctrl Pts',(-6.41670838137096,-2.15870756645148,
49.8003906475858));
#60123=CARTESIAN_POINT('Ctrl Pts',(-6.34562561425132,-2.35060089418804,
49.810072170785));
#60124=CARTESIAN_POINT('Ctrl Pts',(-6.27454284713163,-2.54249422192472,
49.8197536939843));
#60125=CARTESIAN_POINT('Ctrl Pts',(-6.19480817045469,-2.73100707998284,
49.8294352171836));
#60126=CARTESIAN_POINT('Ctrl Pts',(-6.10676825880042,-2.91541942665334,
49.8391167403829));
#60127=CARTESIAN_POINT('Ctrl Pts',(-6.03337004509734,-3.0691626162599,49.8471881536249));
#60128=CARTESIAN_POINT('Ctrl Pts',(-5.95402701160415,-3.22041501290717,
49.8552595668669));
#60129=CARTESIAN_POINT('Ctrl Pts',(-5.86893009352057,-3.36867163097988,
49.8633309801089));
#60130=CARTESIAN_POINT('Ctrl Pts',(-5.7839400075693,-3.51674212514829,49.8713922603602));
#60131=CARTESIAN_POINT('Ctrl Pts',(-5.69321059329911,-3.66182400471009,
49.8794535406114));
#60132=CARTESIAN_POINT('Ctrl Pts',(-5.59698095479664,-3.80343176508317,
49.8875148208626));
#60133=CARTESIAN_POINT('Ctrl Pts',(-5.50085102103002,-3.94489280387898,
49.8955677487202));
#60134=CARTESIAN_POINT('Ctrl Pts',(-5.39923241176125,-4.08288658088965,
49.9036206765778));
#60135=CARTESIAN_POINT('Ctrl Pts',(-5.29241024442235,-4.21695183808558,
49.9116736044354));
#60136=CARTESIAN_POINT('Ctrl Pts',(-5.18567536526842,-4.35090754580073,
49.9197199519598));
#60137=CARTESIAN_POINT('Ctrl Pts',(-5.07374562223461,-4.4809408327538,49.9277662994843));
#60138=CARTESIAN_POINT('Ctrl Pts',(-4.95694951160859,-4.60661920928607,
49.9358126470086));
#60139=CARTESIAN_POINT('Ctrl Pts',(-4.84022329027853,-4.73222238148827,
49.9438541797018));
#60140=CARTESIAN_POINT('Ctrl Pts',(-4.7186367515078,-4.85347555839493,49.9518957123949));
#60141=CARTESIAN_POINT('Ctrl Pts',(-4.5925586848118,-4.96997924810152,49.959937245088));
#60142=CARTESIAN_POINT('Ctrl Pts',(-4.46405680037926,-5.08872269066031,
49.9681333741363));
#60143=CARTESIAN_POINT('Ctrl Pts',(-4.33088918138524,-5.20253186350212,
49.9763295031845));
#60144=CARTESIAN_POINT('Ctrl Pts',(-4.19348610198228,-5.31102281227274,
49.9845256322328));
#60145=CARTESIAN_POINT('Ctrl Pts',(-4.05872127124951,-5.41743064833173,
49.9925643890689));
#60146=CARTESIAN_POINT('Ctrl Pts',(-3.91988247186705,-5.51872241528514,
50.000603145905));
#60147=CARTESIAN_POINT('Ctrl Pts',(-3.77740905344398,-5.6145765506367,50.0086419027411));
#60148=CARTESIAN_POINT('Ctrl Pts',(-3.63492184509992,-5.7104399636554,50.0166814376439));
#60149=CARTESIAN_POINT('Ctrl Pts',(-3.48879962705872,-5.80086448852888,
50.0247209725467));
#60150=CARTESIAN_POINT('Ctrl Pts',(-3.33951041435837,-5.88557212107642,
50.0327605074495));
#60151=CARTESIAN_POINT('Ctrl Pts',(-3.19017719272408,-5.9703047245682,50.040802412325));
#60152=CARTESIAN_POINT('Ctrl Pts',(-3.03767544277751,-6.04931689701847,
50.0488443172005));
#60153=CARTESIAN_POINT('Ctrl Pts',(-2.88249729151362,-6.12237685579846,
50.056886222076));
#60154=CARTESIAN_POINT('Ctrl Pts',(-2.72208462704745,-6.19790129373147,
50.0651993987568));
#60155=CARTESIAN_POINT('Ctrl Pts',(-2.55881223557885,-6.26706474429625,
50.0735125754377));
#60156=CARTESIAN_POINT('Ctrl Pts',(-2.39324451917611,-6.3296658420041,50.0818257521185));
#60157=CARTESIAN_POINT('Ctrl Pts',(-2.23280144727658,-6.3903293133544,50.089881619729));
#60158=CARTESIAN_POINT('Ctrl Pts',(-2.07020339565959,-6.44483056700669,
50.0979374873396));
#60159=CARTESIAN_POINT('Ctrl Pts',(-1.90597732370652,-6.49303776683276,
50.1059933549501));
#60160=CARTESIAN_POINT('Ctrl Pts',(-1.73388303818443,-6.54355461542096,
50.1144351861661));
#60161=CARTESIAN_POINT('Ctrl Pts',(-1.56000136607515,-6.58715934738382,
50.1228770173821));
#60162=CARTESIAN_POINT('Ctrl Pts',(-1.38494751372303,-6.6237609697386,50.1313188485981));
#60163=CARTESIAN_POINT('Ctrl Pts',(-1.20989366137104,-6.66036259209335,
50.1397606798141));
#60164=CARTESIAN_POINT('Ctrl Pts',(-1.0336680976857,-6.68996111286377,50.1482025110301));
#60165=CARTESIAN_POINT('Ctrl Pts',(-0.856888108185714,-6.71252797164004,
50.1566443422461));
#60166=CARTESIAN_POINT('Ctrl Pts',(-0.68453451572473,-6.73452977847151,
50.1648747983126));
#60167=CARTESIAN_POINT('Ctrl Pts',(-0.511080729655507,-6.74992139281732,
50.1731052543792));
#60168=CARTESIAN_POINT('Ctrl Pts',(-0.337074956830591,-6.75859966808788,
50.1813357104457));
#60169=CARTESIAN_POINT('Ctrl Pts',(-0.163275739111443,-6.76726764173433,
50.1895563964759));
#60170=CARTESIAN_POINT('Ctrl Pts',(0.011073806073178,-6.76923812693641,
50.1977770825062));
#60171=CARTESIAN_POINT('Ctrl Pts',(0.185417177203249,-6.76445928884179,
50.2059977685364));
#60172=CARTESIAN_POINT('Ctrl Pts',(0.359588571151644,-6.75968516472684,
50.2142103454518));
#60173=CARTESIAN_POINT('Ctrl Pts',(0.533753447251468,-6.74817498584979,
50.2224229223672));
#60174=CARTESIAN_POINT('Ctrl Pts',(0.707352007490277,-6.72992883599073,
50.2306354992826));
#60175=CARTESIAN_POINT('Ctrl Pts',(0.880814141978052,-6.71169702521774,
50.2388416221872));
#60176=CARTESIAN_POINT('Ctrl Pts',(1.05371049209146,-6.68673982442808,50.2470477450919));
#60177=CARTESIAN_POINT('Ctrl Pts',(1.22548299758562,-6.65510934715791,50.2552538679965));
#60178=CARTESIAN_POINT('Ctrl Pts',(1.39715495401562,-6.62349738516106,50.2634551873502));
#60179=CARTESIAN_POINT('Ctrl Pts',(1.56770402470165,-6.58521999320251,50.2716565067039));
#60180=CARTESIAN_POINT('Ctrl Pts',(1.73657890814165,-6.54038092895189,50.2798578260577));
#60181=CARTESIAN_POINT('Ctrl Pts',(1.90540534537897,-6.49555472796637,50.2880567926472));
#60182=CARTESIAN_POINT('Ctrl Pts',(2.07255820494615,-6.44417069224509,50.2962557592367));
#60183=CARTESIAN_POINT('Ctrl Pts',(2.23749774457196,-6.38638339305083,50.3044547258262));
#60184=CARTESIAN_POINT('Ctrl Pts',(2.40241550318638,-6.32860372493051,50.3126526097052));
#60185=CARTESIAN_POINT('Ctrl Pts',(2.56512018536469,-6.26442259518839,50.320850493584));
#60186=CARTESIAN_POINT('Ctrl Pts',(2.72508853892699,-6.19404403076123,50.329048377463));
#60187=CARTESIAN_POINT('Ctrl Pts',(2.8850648266572,-6.12366197567272,50.3372466679435));
#60188=CARTESIAN_POINT('Ctrl Pts',(3.04230418709739,-6.04708201790509,50.3454449584241));
#60189=CARTESIAN_POINT('Ctrl Pts',(3.1963045860293,-5.96455580855172,50.3536432489046));
#60190=CARTESIAN_POINT('Ctrl Pts',(3.35034059766838,-5.88201051495085,50.3618434352459));
#60191=CARTESIAN_POINT('Ctrl Pts',(3.50113583996505,-5.79351640037113,50.3700436215872));
#60192=CARTESIAN_POINT('Ctrl Pts',(3.64821401811469,-5.69937044576254,50.3782438079286));
#60193=CARTESIAN_POINT('Ctrl Pts',(3.79543124714156,-5.60513548354085,50.3864517469027));
#60194=CARTESIAN_POINT('Ctrl Pts',(3.93892408863219,-5.50523819941379,50.3946596858767));
#60195=CARTESIAN_POINT('Ctrl Pts',(4.07824555221077,-5.40001872365949,50.4028676248508));
#60196=CARTESIAN_POINT('Ctrl Pts',(4.21763460485237,-5.29474820274966,50.4110795457448));
#60197=CARTESIAN_POINT('Ctrl Pts',(4.35284796746005,-5.18415056929953,50.4192914666388));
#60198=CARTESIAN_POINT('Ctrl Pts',(4.48347284046371,-5.06860535934929,50.4275033875327));
#60199=CARTESIAN_POINT('Ctrl Pts',(4.61427684478724,-4.95290169744814,50.4357265697753));
#60200=CARTESIAN_POINT('Ctrl Pts',(4.74047952508958,-4.83223714764187,50.4439497520178));
#60201=CARTESIAN_POINT('Ctrl Pts',(4.86170511249005,-4.70702797943545,50.4521729342604));
#60202=CARTESIAN_POINT('Ctrl Pts',(4.96980774285222,-4.59537300032729,50.4595059375432));
#60203=CARTESIAN_POINT('Ctrl Pts',(5.07395295370794,-4.48010469957471,50.466838940826));
#60204=CARTESIAN_POINT('Ctrl Pts',(5.17390238428699,-4.36153907673305,50.4741719441088));
#60205=CARTESIAN_POINT('Ctrl Pts',(5.29568970614727,-4.21706812190195,50.4831071308911));
#60206=CARTESIAN_POINT('Ctrl Pts',(5.41149997648915,-4.06740161523908,50.4920423176734));
#60207=CARTESIAN_POINT('Ctrl Pts',(5.52090884644196,-3.91303648197649,50.5009775044556));
#60208=CARTESIAN_POINT('Ctrl Pts',(5.63015385575383,-3.7589025399298,50.5098993090923));
#60209=CARTESIAN_POINT('Ctrl Pts',(5.73301644565672,-3.60008422298872,50.5188211137288));
#60210=CARTESIAN_POINT('Ctrl Pts',(5.82911312558786,-3.43711058435707,50.5277429183655));
#60211=CARTESIAN_POINT('Ctrl Pts',(5.92497540292707,-3.27453447707966,50.5366429606048));
#60212=CARTESIAN_POINT('Ctrl Pts',(6.01410457781343,-3.10782349959165,50.5455430028441));
#60213=CARTESIAN_POINT('Ctrl Pts',(6.09616127880189,-2.93753411262517,50.5544430450834));
#60214=CARTESIAN_POINT('Ctrl Pts',(6.17809165229264,-2.7675068886738,50.5633293855768));
#60215=CARTESIAN_POINT('Ctrl Pts',(6.25297115939355,-2.59391247586209,50.5722157260702));
#60216=CARTESIAN_POINT('Ctrl Pts',(6.32050557821505,-2.41733287648855,50.5811020665635));
#60217=CARTESIAN_POINT('Ctrl Pts',(6.38786732331621,-2.24120476032747,50.5899656862355));
#60218=CARTESIAN_POINT('Ctrl Pts',(6.44792136267434,-2.06210692854757,50.5988293059074));
#60219=CARTESIAN_POINT('Ctrl Pts',(6.50042121744808,-1.88064164469226,50.6076929255793));
#60220=CARTESIAN_POINT('Ctrl Pts',(6.55025956057991,-1.70837585229585,50.6161071987331));
#60221=CARTESIAN_POINT('Ctrl Pts',(6.59329047212807,-1.53397690997897,50.6245214718868));
#60222=CARTESIAN_POINT('Ctrl Pts',(6.62934272568025,-1.35797791788763,50.6329357450406));
#60223=CARTESIAN_POINT('Ctrl Pts',(6.66452080281028,-1.18624645844818,50.6411459932451));
#60224=CARTESIAN_POINT('Ctrl Pts',(6.69301974338952,-1.01315644319117,50.6493562414497));
#60225=CARTESIAN_POINT('Ctrl Pts',(6.71475402192053,-0.839266003780745,
50.6575664896542));
#60226=CARTESIAN_POINT('Ctrl Pts',(6.73649346712284,-0.665334227146208,
50.6657786895984));
#60227=CARTESIAN_POINT('Ctrl Pts',(6.75146500234347,-0.490602000479054,
50.6739908895426));
#60228=CARTESIAN_POINT('Ctrl Pts',(6.75963497474576,-0.315632710906001,
50.6822030894868));
#60229=CARTESIAN_POINT('Ctrl Pts',(6.76780834415645,-0.140590670518497,
50.6904187039973));
#60230=CARTESIAN_POINT('Ctrl Pts',(6.76917450009466,0.0346882738773664,
50.6986343185078));
#60231=CARTESIAN_POINT('Ctrl Pts',(6.76375190681956,0.209640508954743,50.7068499330183));
#60232=CARTESIAN_POINT('Ctrl Pts',(6.75832322420992,0.384789207722648,50.7150747733037));
#60233=CARTESIAN_POINT('Ctrl Pts',(6.74609057688584,0.559610108482023,50.7232996135891));
#60234=CARTESIAN_POINT('Ctrl Pts',(6.72712441626983,0.733543514746242,50.7315244538745));
#60235=CARTESIAN_POINT('Ctrl Pts',(6.70814610716865,0.907588331403449,50.7397545624561));
#60236=CARTESIAN_POINT('Ctrl Pts',(6.6824257390876,1.08074416917431,50.7479846710376));
#60237=CARTESIAN_POINT('Ctrl Pts',(6.65008492957727,1.25246134846922,50.7562147796191));
#60238=CARTESIAN_POINT('Ctrl Pts',(6.61769978032081,1.424413954652,50.7644561718058));
#60239=CARTESIAN_POINT('Ctrl Pts',(6.57867613900747,1.59492361669999,50.7726975639925));
#60240=CARTESIAN_POINT('Ctrl Pts',(6.53318579632867,1.76345466362177,50.7809389561792));
#60241=CARTESIAN_POINT('Ctrl Pts',(6.5133872434463,1.83680365701936,50.7845258194435));
#60242=CARTESIAN_POINT('Ctrl Pts',(6.49236438504947,1.90977809710686,50.7881126827077));
#60243=CARTESIAN_POINT('Ctrl Pts',(6.47013422086513,1.98233502819023,50.791699545972));
#60244=CARTESIAN_POINT('Ctrl Pts',(6.4177676139473,2.15325415670859,50.8001489598886));
#60245=CARTESIAN_POINT('Ctrl Pts',(6.35857887499528,2.32224495408212,50.8085983738051));
#60246=CARTESIAN_POINT('Ctrl Pts',(6.29272948473869,2.48874358500435,50.8170477877217));
#60247=CARTESIAN_POINT('Ctrl Pts',(6.22694159651133,2.65508670949554,50.8254893100526));
#60248=CARTESIAN_POINT('Ctrl Pts',(6.15450558008233,2.81894199877421,50.8339308323836));
#60249=CARTESIAN_POINT('Ctrl Pts',(6.07563244337218,2.97976163695074,50.8423723547145));
#60250=CARTESIAN_POINT('Ctrl Pts',(5.99645077784254,3.14121035487719,50.8508468978308));
#60251=CARTESIAN_POINT('Ctrl Pts',(5.91078161542371,3.29959929415626,50.8593214409472));
#60252=CARTESIAN_POINT('Ctrl Pts',(5.81888763225979,3.4543936838661,50.8677959840635));
#60253=CARTESIAN_POINT('Ctrl Pts',(5.72748898892862,3.60835367915241,50.8762248465093));
#60254=CARTESIAN_POINT('Ctrl Pts',(5.62993263870237,3.7587574908774,50.8846537089551));
#60255=CARTESIAN_POINT('Ctrl Pts',(5.52652345996922,3.90510274466753,50.8930825714009));
#60256=CARTESIAN_POINT('Ctrl Pts',(5.4231575139961,4.05138681521149,50.9015079099526));
#60257=CARTESIAN_POINT('Ctrl Pts',(5.31394380953577,4.19361543853159,50.9099332485044));
#60258=CARTESIAN_POINT('Ctrl Pts',(5.19923068858017,4.33131495586804,50.9183585870561));
#60259=CARTESIAN_POINT('Ctrl Pts',(5.08454951973867,4.4689761184753,50.9267815788198));
#60260=CARTESIAN_POINT('Ctrl Pts',(4.96437220194532,4.60211043464504,50.9352045705836));
#60261=CARTESIAN_POINT('Ctrl Pts',(4.83908775559834,4.73027680940748,50.9436275623473));
#60262=CARTESIAN_POINT('Ctrl Pts',(4.71249200090834,4.85978465664652,50.9521387146105));
#60263=CARTESIAN_POINT('Ctrl Pts',(4.58068181891687,4.98421970695032,50.9606498668738));
#60264=CARTESIAN_POINT('Ctrl Pts',(4.44409769073168,5.10316418658398,50.9691610191371));
#60265=CARTESIAN_POINT('Ctrl Pts',(4.30892535712618,5.22087920292743,50.9775841963274));
#60266=CARTESIAN_POINT('Ctrl Pts',(4.16907757488618,5.33321641597437,50.9860073735178));
#60267=CARTESIAN_POINT('Ctrl Pts',(4.02501557564025,5.43981053124586,50.9944305507081));
#60268=CARTESIAN_POINT('Ctrl Pts',(3.87869661362397,5.54807461466279,51.0029856905079));
#60269=CARTESIAN_POINT('Ctrl Pts',(3.72803056266511,5.65041392478799,51.0115408303076));
#60270=CARTESIAN_POINT('Ctrl Pts',(3.57353246629222,5.74649064319742,51.0200959701073));
#60271=CARTESIAN_POINT('Ctrl Pts',(3.41903436991944,5.84256736160677,51.028651109907));
#60272=CARTESIAN_POINT('Ctrl Pts',(3.26070454339456,5.93238131494943,51.0372062497067));
#60273=CARTESIAN_POINT('Ctrl Pts',(3.0990855038473,6.01564277861008,51.0457613895064));
#60274=CARTESIAN_POINT('Ctrl Pts',(3.09908550384708,6.01564277861019,49.0457563580462));
#60275=CARTESIAN_POINT('Ctrl Pts',(2.93373232018321,6.10082796552484,49.0545058059455));
#60276=CARTESIAN_POINT('Ctrl Pts',(2.76486502144422,6.17919158180192,49.0632552538448));
#60277=CARTESIAN_POINT('Ctrl Pts',(2.59305716434353,6.25046746591379,49.0720047017441));
#60278=CARTESIAN_POINT('Ctrl Pts',(2.42125069459282,6.32174277447225,49.0807540789915));
#60279=CARTESIAN_POINT('Ctrl Pts',(2.24650397871055,6.38593035557827,49.0895034562389));
#60280=CARTESIAN_POINT('Ctrl Pts',(2.06941053323766,6.4428122000354,49.0982528334864));
#60281=CARTESIAN_POINT('Ctrl Pts',(1.89231845896677,6.49969360406687,49.107002142989));
#60282=CARTESIAN_POINT('Ctrl Pts',(1.71287996431498,6.54926929700883,49.1157514524915));
#60283=CARTESIAN_POINT('Ctrl Pts',(1.53170449173496,6.59137090065481,49.1245007619941));
#60284=CARTESIAN_POINT('Ctrl Pts',(1.35053036178162,6.63347219230085,49.1332500066587));
#60285=CARTESIAN_POINT('Ctrl Pts',(1.16761955878835,6.66809944062456,49.1419992513233));
#60286=CARTESIAN_POINT('Ctrl Pts',(0.98359330931039,6.69513503985393,49.1507484959879));
#60287=CARTESIAN_POINT('Ctrl Pts',(0.799568362459827,6.72217044771216,49.1594976787211));
#60288=CARTESIAN_POINT('Ctrl Pts',(0.614428268438384,6.74161427235979,49.1682468614543));
#60289=CARTESIAN_POINT('Ctrl Pts',(0.42880181633,6.75340047696804,49.1769960441874));
#60290=CARTESIAN_POINT('Ctrl Pts',(0.243176616522559,6.76518660206243,49.1857451678956));
#60291=CARTESIAN_POINT('Ctrl Pts',(0.0570653511652789,6.76931519233997,
49.1944942916037));
#60292=CARTESIAN_POINT('Ctrl Pts',(-0.128899900800167,6.76577222610795,
49.2032434153118));
#60293=CARTESIAN_POINT('Ctrl Pts',(-0.314863959942176,6.76222928260132,
49.2119924829011));
#60294=CARTESIAN_POINT('Ctrl Pts',(-0.500681721080852,6.75101488651275,
49.2207415504904));
#60295=CARTESIAN_POINT('Ctrl Pts',(-0.685722110173486,6.73216712415989,
49.2294906180796));
#60296=CARTESIAN_POINT('Ctrl Pts',(-0.870761373827704,6.71331947644144,
49.238239632456));
#60297=CARTESIAN_POINT('Ctrl Pts',(-1.05502298984343,6.68683858439996,49.2469886468323));
#60298=CARTESIAN_POINT('Ctrl Pts',(-1.2378811767605,6.65281438131428,49.2557376612087));
#60299=CARTESIAN_POINT('Ctrl Pts',(-1.43009641451775,6.61704912302381,49.2649343720962));
#60300=CARTESIAN_POINT('Ctrl Pts',(-1.62076048992669,6.57294837083171,49.2741310829837));
#60301=CARTESIAN_POINT('Ctrl Pts',(-1.80915798961097,6.52067760042059,49.2833277938713));
#60302=CARTESIAN_POINT('Ctrl Pts',(-1.9884044300298,6.47094578577419,49.2920777915778));
#60303=CARTESIAN_POINT('Ctrl Pts',(-2.16559895952163,6.41381888474485,49.3008277892843));
#60304=CARTESIAN_POINT('Ctrl Pts',(-2.34013966242297,6.34949095285244,49.3095777869908));
#60305=CARTESIAN_POINT('Ctrl Pts',(-2.51467682553978,6.28516432556699,49.3183276072424));
#60306=CARTESIAN_POINT('Ctrl Pts',(-2.68656000078795,6.21363705879681,49.327077427494));
#60307=CARTESIAN_POINT('Ctrl Pts',(-2.85520533840831,6.13515211510886,49.3358272477455));
#60308=CARTESIAN_POINT('Ctrl Pts',(-3.02384747998279,6.05666865881146,49.3445769021768));
#60309=CARTESIAN_POINT('Ctrl Pts',(-3.18925164684496,5.97122791039866,49.3533265566081));
#60310=CARTESIAN_POINT('Ctrl Pts',(-3.35085601829125,5.87912008251926,49.3620762110393));
#60311=CARTESIAN_POINT('Ctrl Pts',(-3.5124575419138,5.78701387778197,49.3708257112825));
#60312=CARTESIAN_POINT('Ctrl Pts',(-3.67025915510894,5.6882409706101,49.3795752115256));
#60313=CARTESIAN_POINT('Ctrl Pts',(-3.82372487928787,5.58313684656887,49.3883247117687));
#60314=CARTESIAN_POINT('Ctrl Pts',(-3.97718810300761,5.478034435018,49.3970740694538));
#60315=CARTESIAN_POINT('Ctrl Pts',(-4.12631534262999,5.36660117496397,49.4058234271389));
#60316=CARTESIAN_POINT('Ctrl Pts',(-4.27060009886208,5.24921554097364,49.4145727848241));
#60317=CARTESIAN_POINT('Ctrl Pts',(-4.41488269594197,5.13183166360305,49.4233220115793));
#60318=CARTESIAN_POINT('Ctrl Pts',(-4.55432273235073,5.00849577139485,49.4320712383344));
#60319=CARTESIAN_POINT('Ctrl Pts',(-4.68844662480192,4.87962675277357,49.4408204650896));
#60320=CARTESIAN_POINT('Ctrl Pts',(-4.82256868835143,4.75075949139896,49.4495695725411));
#60321=CARTESIAN_POINT('Ctrl Pts',(-4.95137454637849,4.6163594531254,49.4583186799926));
#60322=CARTESIAN_POINT('Ctrl Pts',(-5.07442674461065,4.47688309134605,49.4670677874441));
#60323=CARTESIAN_POINT('Ctrl Pts',(-5.19747742838542,4.33740844616348,49.4758167872165));
#60324=CARTESIAN_POINT('Ctrl Pts',(-5.31477440450945,4.19285781736007,49.4845657869889));
#60325=CARTESIAN_POINT('Ctrl Pts',(-5.42591931531184,4.04372211999365,49.4933147867613));
#60326=CARTESIAN_POINT('Ctrl Pts',(-5.53707636463015,3.89457013500754,49.5020647420418));
#60327=CARTESIAN_POINT('Ctrl Pts',(-5.64207983273505,3.74083230916368,49.5108146973224));
#60328=CARTESIAN_POINT('Ctrl Pts',(-5.74057303468783,3.5830308725177,49.519564652603));
#60329=CARTESIAN_POINT('Ctrl Pts',(-5.83906243363804,3.42523552887364,49.5283142700318));
#60330=CARTESIAN_POINT('Ctrl Pts',(-5.93104191768467,3.26337713156918,49.5370638874606));
#60331=CARTESIAN_POINT('Ctrl Pts',(-6.01619906699699,3.09800545291071,49.5458135048894));
#60332=CARTESIAN_POINT('Ctrl Pts',(-6.10135338095426,2.93263928039505,49.5545628309948));
#60333=CARTESIAN_POINT('Ctrl Pts',(-6.17968568352882,2.76376031540128,49.5633121571002));
#60334=CARTESIAN_POINT('Ctrl Pts',(-6.25092992694929,2.5919421383144,49.5720614832056));
#60335=CARTESIAN_POINT('Ctrl Pts',(-6.32217217691152,2.42012876880696,49.5808105644994));
#60336=CARTESIAN_POINT('Ctrl Pts',(-6.38632665483902,2.24537661647525,49.5895596457932));
#60337=CARTESIAN_POINT('Ctrl Pts',(-6.44317547869404,2.06827917621289,49.598308727087));
#60338=CARTESIAN_POINT('Ctrl Pts',(-6.50002944235986,1.89116572423253,49.607058599402));
#60339=CARTESIAN_POINT('Ctrl Pts',(-6.54957634250443,1.71170683289025,49.6158084717169));
#60340=CARTESIAN_POINT('Ctrl Pts',(-6.59164787708436,1.53051209225189,49.6245583440319));
#60341=CARTESIAN_POINT('Ctrl Pts',(-6.63371649075043,1.3493299314786,49.6333076088667));
#60342=CARTESIAN_POINT('Ctrl Pts',(-6.66831071257153,1.16641244173839,49.6420568737015));
#60343=CARTESIAN_POINT('Ctrl Pts',(-6.69531304840356,0.982380875158415,
49.6508061385363));
#60344=CARTESIAN_POINT('Ctrl Pts',(-6.72231677033063,0.798339861794236,
49.6595558524919));
#60345=CARTESIAN_POINT('Ctrl Pts',(-6.74172778477905,0.613184940728539,
49.6683055664476));
#60346=CARTESIAN_POINT('Ctrl Pts',(-6.75348015835528,0.427545027688932,
49.6770552804032));
#60347=CARTESIAN_POINT('Ctrl Pts',(-6.76249038365213,0.285219953547603,
49.6837634482054));
#60348=CARTESIAN_POINT('Ctrl Pts',(-6.76699999999988,0.142609995760499,
49.6904716160076));
#60349=CARTESIAN_POINT('Ctrl Pts',(-6.767,5.52185849906123E-12,49.6971797838098));
#60350=CARTESIAN_POINT('',(-6.767,7.5280007819922E-10,49.3028202161545));
#60351=CARTESIAN_POINT('Ctrl Pts',(3.09908550384732,6.01564277861007,48.6513967904261));
#60352=CARTESIAN_POINT('Ctrl Pts',(2.93373232018345,6.10082796552472,48.6601462383254));
#60353=CARTESIAN_POINT('Ctrl Pts',(2.76486502144447,6.17919158180181,48.6688956862247));
#60354=CARTESIAN_POINT('Ctrl Pts',(2.59305716434378,6.25046746591368,48.677645134124));
#60355=CARTESIAN_POINT('Ctrl Pts',(2.42125069459307,6.32174277447215,48.6863945113714));
#60356=CARTESIAN_POINT('Ctrl Pts',(2.24650397871081,6.38593035557818,48.6951438886188));
#60357=CARTESIAN_POINT('Ctrl Pts',(2.06941053323792,6.44281220003532,48.7038932658662));
#60358=CARTESIAN_POINT('Ctrl Pts',(1.89231845896703,6.49969360406679,48.7126425753688));
#60359=CARTESIAN_POINT('Ctrl Pts',(1.71287996431524,6.54926929700876,48.7213918848714));
#60360=CARTESIAN_POINT('Ctrl Pts',(1.53170449173523,6.59137090065474,48.730141194374));
#60361=CARTESIAN_POINT('Ctrl Pts',(1.35053036178189,6.6334721923008,48.7388904390386));
#60362=CARTESIAN_POINT('Ctrl Pts',(1.16761955878862,6.66809944062451,48.7476396837032));
#60363=CARTESIAN_POINT('Ctrl Pts',(0.983593309310659,6.69513503985389,48.7563889283678));
#60364=CARTESIAN_POINT('Ctrl Pts',(0.799568362460224,6.72217044771211,48.765138111101));
#60365=CARTESIAN_POINT('Ctrl Pts',(0.61442826843891,6.74161427235974,48.7738872938341));
#60366=CARTESIAN_POINT('Ctrl Pts',(0.428801816330655,6.75340047696799,48.7826364765673));
#60367=CARTESIAN_POINT('Ctrl Pts',(0.243176616523087,6.76518660206241,48.7913856002754));
#60368=CARTESIAN_POINT('Ctrl Pts',(0.0570653511656807,6.76931519233997,
48.8001347239836));
#60369=CARTESIAN_POINT('Ctrl Pts',(-0.128899900799894,6.76577222610795,
48.8088838476917));
#60370=CARTESIAN_POINT('Ctrl Pts',(-0.314863959941646,6.76222928260134,
48.817632915281));
#60371=CARTESIAN_POINT('Ctrl Pts',(-0.500681721080068,6.7510148865128,48.8263819828702));
#60372=CARTESIAN_POINT('Ctrl Pts',(-0.685722110172451,6.73216712416,48.8351310504594));
#60373=CARTESIAN_POINT('Ctrl Pts',(-0.870761373826543,6.71331947644158,
48.8438800648358));
#60374=CARTESIAN_POINT('Ctrl Pts',(-1.05502298984215,6.68683858440016,48.8526290792122));
#60375=CARTESIAN_POINT('Ctrl Pts',(-1.2378811767591,6.65281438131454,48.8613780935885));
#60376=CARTESIAN_POINT('Ctrl Pts',(-1.4300964145011,6.61704912302695,48.8705748044753));
#60377=CARTESIAN_POINT('Ctrl Pts',(-1.62076048989504,6.57294837083906,48.8797715153621));
#60378=CARTESIAN_POINT('Ctrl Pts',(-1.80915798956474,6.52067760043342,48.8889682262489));
#60379=CARTESIAN_POINT('Ctrl Pts',(-1.98840442998381,6.47094578578832,48.8977182239554));
#60380=CARTESIAN_POINT('Ctrl Pts',(-2.16559895947592,6.41381888476028,48.9064682216619));
#60381=CARTESIAN_POINT('Ctrl Pts',(-2.3401396623776,6.34949095286916,48.9152182193684));
#60382=CARTESIAN_POINT('Ctrl Pts',(-2.51467682549499,6.28516432558492,48.92396803962));
#60383=CARTESIAN_POINT('Ctrl Pts',(-2.68656000074379,6.21363705881591,48.9327178598716));
#60384=CARTESIAN_POINT('Ctrl Pts',(-2.85520533836482,6.1351521151291,48.9414676801232));
#60385=CARTESIAN_POINT('Ctrl Pts',(-3.02384747993973,6.05666865883295,48.9502173345544));
#60386=CARTESIAN_POINT('Ctrl Pts',(-3.18925164680241,5.97122791042138,48.9589669889857));
#60387=CARTESIAN_POINT('Ctrl Pts',(-3.35085601824925,5.8791200825432,48.9677166434169));
#60388=CARTESIAN_POINT('Ctrl Pts',(-3.51245754187268,5.78701387780694,48.9764661436601));
#60389=CARTESIAN_POINT('Ctrl Pts',(-3.67025915506873,5.68824097063605,48.9852156439032));
#60390=CARTESIAN_POINT('Ctrl Pts',(-3.82372487924861,5.58313684659576,48.9939651441464));
#60391=CARTESIAN_POINT('Ctrl Pts',(-3.97718810296909,5.47803443504597,49.0027145018315));
#60392=CARTESIAN_POINT('Ctrl Pts',(-4.12631534259225,5.36660117499298,49.0114638595166));
#60393=CARTESIAN_POINT('Ctrl Pts',(-4.27060009882517,5.24921554100367,49.0202132172017));
#60394=CARTESIAN_POINT('Ctrl Pts',(-4.41488269590598,5.13183166363402,49.0289624439569));
#60395=CARTESIAN_POINT('Ctrl Pts',(-4.5543227323157,5.0084957714267,49.0377116707121));
#60396=CARTESIAN_POINT('Ctrl Pts',(-4.68844662476788,4.87962675280627,49.0464608974673));
#60397=CARTESIAN_POINT('Ctrl Pts',(-4.82256868831839,4.75075949143251,49.0552100049188));
#60398=CARTESIAN_POINT('Ctrl Pts',(-4.95137454634646,4.61635945315975,49.0639591123703));
#60399=CARTESIAN_POINT('Ctrl Pts',(-5.07442674457968,4.47688309138116,49.0727082198218));
#60400=CARTESIAN_POINT('Ctrl Pts',(-5.19747742835516,4.33740844619973,49.0814572195941));
#60401=CARTESIAN_POINT('Ctrl Pts',(-5.31477440447996,4.19285781739744,49.0902062193665));
#60402=CARTESIAN_POINT('Ctrl Pts',(-5.42591931528317,4.04372212003211,49.0989552191389));
#60403=CARTESIAN_POINT('Ctrl Pts',(-5.53707636460246,3.8945701350469,49.1077051744195));
#60404=CARTESIAN_POINT('Ctrl Pts',(-5.64207983270839,3.74083230920389,49.1164551297));
#60405=CARTESIAN_POINT('Ctrl Pts',(-5.74057303466223,3.58303087255872,49.1252050849806));
#60406=CARTESIAN_POINT('Ctrl Pts',(-5.83906243361357,3.42523552891537,49.1339547024094));
#60407=CARTESIAN_POINT('Ctrl Pts',(-5.93104191766135,3.26337713161155,49.1427043198382));
#60408=CARTESIAN_POINT('Ctrl Pts',(-6.01619906697486,3.0980054529537,49.151453937267));
#60409=CARTESIAN_POINT('Ctrl Pts',(-6.10135338093331,2.93263928043865,49.1602032633724));
#60410=CARTESIAN_POINT('Ctrl Pts',(-6.17968568350907,2.76376031544544,49.1689525894778));
#60411=CARTESIAN_POINT('Ctrl Pts',(-6.25092992693076,2.59194213835907,49.1777019155832));
#60412=CARTESIAN_POINT('Ctrl Pts',(-6.32217217689402,2.42012876885261,49.186450996877));
#60413=CARTESIAN_POINT('Ctrl Pts',(-6.38632665482262,2.24537661652185,49.1952000781708));
#60414=CARTESIAN_POINT('Ctrl Pts',(-6.44317547867879,2.06827917626039,49.2039491594646));
#60415=CARTESIAN_POINT('Ctrl Pts',(-6.50002944234587,1.89116572428058,49.2126990317795));
#60416=CARTESIAN_POINT('Ctrl Pts',(-6.54957634249174,1.71170683293879,49.2214489040945));
#60417=CARTESIAN_POINT('Ctrl Pts',(-6.59164787707299,1.53051209230087,49.2301987764094));
#60418=CARTESIAN_POINT('Ctrl Pts',(-6.63371649074038,1.34932993152801,49.2389480412442));
#60419=CARTESIAN_POINT('Ctrl Pts',(-6.66831071256281,1.16641244178818,49.247697306079));
#60420=CARTESIAN_POINT('Ctrl Pts',(-6.69531304839621,0.982380875208539,
49.2564465709138));
#60421=CARTESIAN_POINT('Ctrl Pts',(-6.72231677032465,0.798339861844562,
49.2651962848694));
#60422=CARTESIAN_POINT('Ctrl Pts',(-6.74172778477446,0.613184940779011,
49.2739459988251));
#60423=CARTESIAN_POINT('Ctrl Pts',(-6.75348015835208,0.427545027739492,
49.2826957127808));
#60424=CARTESIAN_POINT('Ctrl Pts',(-6.76249038363532,0.285219953829973,
49.289403880572));
#60425=CARTESIAN_POINT('Ctrl Pts',(-6.76699999998414,0.142609996275572,
49.2961120483633));
#60426=CARTESIAN_POINT('Ctrl Pts',(-6.767,7.52800906917709E-10,49.3028202161545));
#60427=CARTESIAN_POINT('Ctrl Pts',(-6.767,5.40600529812716E-12,49.3028202161897));
#60428=CARTESIAN_POINT('Ctrl Pts',(-6.76700000000015,-0.186007249554668,
49.3115697280025));
#60429=CARTESIAN_POINT('Ctrl Pts',(-6.75932637294276,-0.372014355810922,
49.3203192398152));
#60430=CARTESIAN_POINT('Ctrl Pts',(-6.74400518263404,-0.557389537581373,
49.3290687516279));
#60431=CARTESIAN_POINT('Ctrl Pts',(-6.72868405703783,-0.742763936377985,
49.3378182264852));
#60432=CARTESIAN_POINT('Ctrl Pts',(-6.70571545643628,-0.927506130400437,
49.3465677013423));
#60433=CARTESIAN_POINT('Ctrl Pts',(-6.67517739401647,-1.1109886400911,49.3553171761995));
#60434=CARTESIAN_POINT('Ctrl Pts',(-6.64463945804475,-1.29447039004101,
49.3640666148281));
#60435=CARTESIAN_POINT('Ctrl Pts',(-6.60653217002823,-1.47669218338832,
49.3728160534566));
#60436=CARTESIAN_POINT('Ctrl Pts',(-6.56098496085594,-1.65703510627333,
49.3815654920851));
#60437=CARTESIAN_POINT('Ctrl Pts',(-6.5154379364968,-1.83737729739571,49.3903148952117));
#60438=CARTESIAN_POINT('Ctrl Pts',(-6.46245112157029,-2.01584035544528,
49.3990642983384));
#60439=CARTESIAN_POINT('Ctrl Pts',(-6.40220448361858,-2.19181813796997,
49.407813701465));
#60440=CARTESIAN_POINT('Ctrl Pts',(-6.34195808512122,-2.36779522105905,
49.4165630698165));
#60441=CARTESIAN_POINT('Ctrl Pts',(-6.2744520141651,-2.54128677725359,49.4253124381681));
#60442=CARTESIAN_POINT('Ctrl Pts',(-6.19991555052887,-2.71170355428286,
49.4340618065196));
#60443=CARTESIAN_POINT('Ctrl Pts',(-6.12537937695291,-2.88211966813154,
49.4428111408228));
#60444=CARTESIAN_POINT('Ctrl Pts',(-6.04381298028529,-3.04946076419516,
49.451560475126));
#60445=CARTESIAN_POINT('Ctrl Pts',(-5.95549339309064,-3.21315848424159,
49.4603098094291));
#60446=CARTESIAN_POINT('Ctrl Pts',(-5.86717414225886,-3.37685558084949,
49.4690591104107));
#60447=CARTESIAN_POINT('Ctrl Pts',(-5.77210188844137,-3.53690907699886,
49.4778084113923));
#60448=CARTESIAN_POINT('Ctrl Pts',(-5.67059953311434,-3.69277537023896,
49.4865577123738));
#60449=CARTESIAN_POINT('Ctrl Pts',(-5.5690975559276,-3.84864108280951,49.4953069807604));
#60450=CARTESIAN_POINT('Ctrl Pts',(-5.46116568155008,-4.00031938354772,
49.5040562491471));
#60451=CARTESIAN_POINT('Ctrl Pts',(-5.34717048488407,-4.14729511918126,
49.5128055175337));
#60452=CARTESIAN_POINT('Ctrl Pts',(-5.23317570343322,-4.29427031947159,
49.5215547540521));
#60453=CARTESIAN_POINT('Ctrl Pts',(-5.11311781951551,-4.43654276249552,
49.5303039905704));
#60454=CARTESIAN_POINT('Ctrl Pts',(-4.98740458929233,-4.57362924412395,
49.5390532270888));
#60455=CARTESIAN_POINT('Ctrl Pts',(-4.86169180652717,-4.71071523781292,
49.5478024324655));
#60456=CARTESIAN_POINT('Ctrl Pts',(-4.73032391141537,-4.84261509584525,
49.5565516378422));
#60457=CARTESIAN_POINT('Ctrl Pts',(-4.59374706947278,-4.96888084599644,
49.565300843219));
#60458=CARTESIAN_POINT('Ctrl Pts',(-4.45717070231484,-5.09514615720762,
49.5740500181807));
#60459=CARTESIAN_POINT('Ctrl Pts',(-4.31538563497366,-5.21577720520579,
49.5827991931423));
#60460=CARTESIAN_POINT('Ctrl Pts',(-4.16887340952073,-5.33036429293449,
49.591548368104));
#60461=CARTESIAN_POINT('Ctrl Pts',(-4.02236168122547,-5.4449509918366,49.6002975133773));
#60462=CARTESIAN_POINT('Ctrl Pts',(-3.87112305263238,-5.55349359497889,
49.6090466586506));
#60463=CARTESIAN_POINT('Ctrl Pts',(-3.71567116929046,-5.65562346357178,
49.6177958039238));
#60464=CARTESIAN_POINT('Ctrl Pts',(-3.5602198005338,-5.75775299408884,49.6265449202352));
#60465=CARTESIAN_POINT('Ctrl Pts',(-3.4005554444217,-5.85346967519828,49.6352940365465));
#60466=CARTESIAN_POINT('Ctrl Pts',(-3.23722035886948,-5.94244843041326,
49.6440431528579));
#60467=CARTESIAN_POINT('Ctrl Pts',(-3.07388580043611,-6.03142689847388,
49.6527922409339));
#60468=CARTESIAN_POINT('Ctrl Pts',(-2.90688078789361,-6.11366734707835,
49.6615413290099));
#60469=CARTESIAN_POINT('Ctrl Pts',(-2.73677250610548,-6.1888904700136,49.6702904170859));
#60470=CARTESIAN_POINT('Ctrl Pts',(-2.56666475917063,-6.26411335643282,
49.6790394776531));
#60471=CARTESIAN_POINT('Ctrl Pts',(-2.39345402457194,-6.33231884545219,
49.6877885382203));
#60472=CARTESIAN_POINT('Ctrl Pts',(-2.21772855944137,-6.39327529804858,
49.6965375987875));
#60473=CARTESIAN_POINT('Ctrl Pts',(-2.04200363223679,-6.45423156404674,
49.7052866325723));
#60474=CARTESIAN_POINT('Ctrl Pts',(-1.86376426061139,-6.50793874412422,
49.7140356663571));
#60475=CARTESIAN_POINT('Ctrl Pts',(-1.6836157762181,-6.55421443943281,49.7227847001419));
#60476=CARTESIAN_POINT('Ctrl Pts',(-1.50346782833343,-6.60048999692559,
49.7315337078708));
#60477=CARTESIAN_POINT('Ctrl Pts',(-1.3214110565752,-6.63933404265135,49.7402827155996));
#60478=CARTESIAN_POINT('Ctrl Pts',(-1.13806375346673,-6.67061465631506,
49.7490317233285));
#60479=CARTESIAN_POINT('Ctrl Pts',(-0.954716981171458,-6.7018951794175,
49.757780705728));
#60480=CARTESIAN_POINT('Ctrl Pts',(-0.770079967443803,-6.72561226608986,
49.7665296881274));
#60481=CARTESIAN_POINT('Ctrl Pts',(-0.584779764074661,-6.74168536995971,
49.7752786705268));
#60482=CARTESIAN_POINT('Ctrl Pts',(-0.391489587594497,-6.75845153117864,
49.7844049009424));
#60483=CARTESIAN_POINT('Ctrl Pts',(-0.197478091806726,-6.7668998514639,
49.7935311313581));
#60484=CARTESIAN_POINT('Ctrl Pts',(-0.00346214753246707,-6.76699911434415,
49.8026573617737));
#60485=CARTESIAN_POINT('Ctrl Pts',(0.184490798483177,-6.76709527525939,
49.8114983974888));
#60486=CARTESIAN_POINT('Ctrl Pts',(0.372447602153291,-6.75935633790771,
49.8203394332039));
#60487=CARTESIAN_POINT('Ctrl Pts',(0.559756448192704,-6.74380914014526,
49.829180468919));
#60488=CARTESIAN_POINT('Ctrl Pts',(0.745136131041834,-6.72842206873171,
49.8379304475324));
#60489=CARTESIAN_POINT('Ctrl Pts',(0.929880851943513,-6.70538686355745,
49.8466804261457));
#60490=CARTESIAN_POINT('Ctrl Pts',(1.11336305057309,-6.67478177303338,49.855430404759));
#60491=CARTESIAN_POINT('Ctrl Pts',(1.29684337089978,-6.64417699581289,49.864180293799));
#60492=CARTESIAN_POINT('Ctrl Pts',(1.47906091205053,-6.60600253548091,49.8729301828389));
#60493=CARTESIAN_POINT('Ctrl Pts',(1.65939671095094,-6.56038806441244,49.8816800718789));
#60494=CARTESIAN_POINT('Ctrl Pts',(1.83973072369034,-6.51477404513885,49.8904298742544));
#60495=CARTESIAN_POINT('Ctrl Pts',(2.01818275356911,-6.461720232887,49.8991796766299));
#60496=CARTESIAN_POINT('Ctrl Pts',(2.19414664033203,-6.4014068391815,49.9079294790054));
#60497=CARTESIAN_POINT('Ctrl Pts',(2.37010884271141,-6.34109402281542,49.9166791976249));
#60498=CARTESIAN_POINT('Ctrl Pts',(2.54358267847693,-6.27352185699838,49.9254289162445));
#60499=CARTESIAN_POINT('Ctrl Pts',(2.71397890841633,-6.19891986435309,49.934178634864));
#60500=CARTESIAN_POINT('Ctrl Pts',(2.88437356388832,-6.12431856103295,49.9429282726358));
#60501=CARTESIAN_POINT('Ctrl Pts',(3.05169040787062,-6.04268767582613,49.9516779104077));
#60502=CARTESIAN_POINT('Ctrl Pts',(3.21536112511943,-5.95430447954005,49.9604275481795));
#60503=CARTESIAN_POINT('Ctrl Pts',(3.37903038442726,-5.8659220705511,49.9691771080115));
#60504=CARTESIAN_POINT('Ctrl Pts',(3.5390533297985,-5.77078760703452,49.9779266678436));
#60505=CARTESIAN_POINT('Ctrl Pts',(3.69488643041764,-5.66922422085382,49.9866762276757));
#60506=CARTESIAN_POINT('Ctrl Pts',(3.8507181946862,-5.56766170563243,49.9954257124757));
#60507=CARTESIAN_POINT('Ctrl Pts',(4.00235994599108,-5.45967053456337,50.0041751972757));
#60508=CARTESIAN_POINT('Ctrl Pts',(4.1492966297419,-5.3456175020677,50.0129246820756));
#60509=CARTESIAN_POINT('Ctrl Pts',(4.29623210224934,-5.23156540974556,50.021674094751));
#60510=CARTESIAN_POINT('Ctrl Pts',(4.43846235842008,-5.11145173172281,50.0304235074264));
#60511=CARTESIAN_POINT('Ctrl Pts',(4.5755043179732,-4.98568443006661,50.0391729201017));
#60512=CARTESIAN_POINT('Ctrl Pts',(4.7125451933739,-4.85991812336791,50.0479222635596));
#60513=CARTESIAN_POINT('Ctrl Pts',(4.84439764314884,-4.72849847631203,50.0566716070175));
#60514=CARTESIAN_POINT('Ctrl Pts',(4.97061384196591,-4.59187184425447,50.0654209504754));
#60515=CARTESIAN_POINT('Ctrl Pts',(5.09682908420106,-4.45524624767861,50.0741702276228));
#60516=CARTESIAN_POINT('Ctrl Pts',(5.21740796650067,-4.31341395557017,50.0829195047701));
#60517=CARTESIAN_POINT('Ctrl Pts',(5.33194095942145,-4.16685668162992,50.0916687819175));
#60518=CARTESIAN_POINT('Ctrl Pts',(5.44647312235028,-4.02030046975357,50.100417995661));
#60519=CARTESIAN_POINT('Ctrl Pts',(5.55495930712184,-3.86901957035696,50.1091672094046));
#60520=CARTESIAN_POINT('Ctrl Pts',(5.65703106079693,-3.7135277805853,50.1179164231481));
#60521=CARTESIAN_POINT('Ctrl Pts',(5.75910210868636,-3.55803706597764,50.1266655763943));
#60522=CARTESIAN_POINT('Ctrl Pts',(5.85475865698452,-3.39833575881067,50.1354147296405));
#60523=CARTESIAN_POINT('Ctrl Pts',(5.94367583068968,-3.23496624706894,50.1441638828867));
#60524=CARTESIAN_POINT('Ctrl Pts',(6.03259241909992,-3.07159781070267,50.1529129785418));
#60525=CARTESIAN_POINT('Ctrl Pts',(6.11476958470892,-2.90456146975993,50.1616620741969));
#60526=CARTESIAN_POINT('Ctrl Pts',(6.18992823574319,-2.73442451648409,50.1704111698521));
#60527=CARTESIAN_POINT('Ctrl Pts',(6.26508641700875,-2.56428862662563,50.1791602108222));
#60528=CARTESIAN_POINT('Ctrl Pts',(6.33322605570243,-2.3910524253142,50.1879092517923));
#60529=CARTESIAN_POINT('Ctrl Pts',(6.39411573747719,-2.21530425353867,50.1966582927624));
#60530=CARTESIAN_POINT('Ctrl Pts',(6.45500505889075,-2.03955712188719,50.2054072819534));
#60531=CARTESIAN_POINT('Ctrl Pts',(6.50864441544878,-1.8612983202575,50.2141562711444));
#60532=CARTESIAN_POINT('Ctrl Pts',(6.55485164049856,-1.68113324012507,50.2229052603354));
#60533=CARTESIAN_POINT('Ctrl Pts',(6.60199852639068,-1.49730435913086,50.2318321672123));
#60534=CARTESIAN_POINT('Ctrl Pts',(6.64140767440975,-1.31149113173827,50.2407590740892));
#60535=CARTESIAN_POINT('Ctrl Pts',(6.67293975269575,-1.12435050446596,50.249685980966));
#60536=CARTESIAN_POINT('Ctrl Pts',(6.70384664831483,-0.94092029156542,50.25843589515));
#60537=CARTESIAN_POINT('Ctrl Pts',(6.72718585889647,-0.756215114279639,
50.267185809334));
#60538=CARTESIAN_POINT('Ctrl Pts',(6.7428781045185,-0.570862389376862,50.275935723518));
#60539=CARTESIAN_POINT('Ctrl Pts',(6.75857004154113,-0.385513309569948,
50.2846854656286));
#60540=CARTESIAN_POINT('Ctrl Pts',(6.7666152903555,-0.199516993261185,50.2934352077392));
#60541=CARTESIAN_POINT('Ctrl Pts',(6.76698652348896,-0.0135052182071509,
50.3021849498498));
#60542=CARTESIAN_POINT('Ctrl Pts',(6.76735774981529,0.172503146035686,50.3109345315204));
#60543=CARTESIAN_POINT('Ctrl Pts',(6.76005524147496,0.358526681830155,50.3196841131911));
#60544=CARTESIAN_POINT('Ctrl Pts',(6.74510380214909,0.543933542111445,50.3284336948617));
#60545=CARTESIAN_POINT('Ctrl Pts',(6.73015261711016,0.729337249081364,50.3371831277236));
#60546=CARTESIAN_POINT('Ctrl Pts',(6.7075527844465,0.914124015851373,50.3459325605855));
#60547=CARTESIAN_POINT('Ctrl Pts',(6.67738106408342,1.09766621749064,50.3546819934475));
#60548=CARTESIAN_POINT('Ctrl Pts',(6.64720981677314,1.28120554143013,50.3634312891298));
#60549=CARTESIAN_POINT('Ctrl Pts',(6.60946696581589,1.46350005650325,50.3721805848122));
#60550=CARTESIAN_POINT('Ctrl Pts',(6.56428070011065,1.64393062206252,50.3809298804945));
#60551=CARTESIAN_POINT('Ctrl Pts',(6.5190950828282,1.82435859844368,50.3896790506245));
#60552=CARTESIAN_POINT('Ctrl Pts',(6.4664663341575,2.00292240086278,50.3984282207545));
#60553=CARTESIAN_POINT('Ctrl Pts',(6.4065731959729,2.17901557696168,50.4071773908845));
#60554=CARTESIAN_POINT('Ctrl Pts',(6.34668083768402,2.35510646007145,50.4159264470876));
#60555=CARTESIAN_POINT('Ctrl Pts',(6.27952437144002,2.52872650996239,50.4246755032906));
#60556=CARTESIAN_POINT('Ctrl Pts',(6.20533187335263,2.69928607997632,50.4334245594937));
#60557=CARTESIAN_POINT('Ctrl Pts',(6.12831449784381,2.87633970115123,50.4425067357826));
#60558=CARTESIAN_POINT('Ctrl Pts',(6.04371489463282,3.05009490562094,50.4515889120714));
#60559=CARTESIAN_POINT('Ctrl Pts',(5.95184265120618,3.21991584599395,50.4606710883603));
#60560=CARTESIAN_POINT('Ctrl Pts',(5.86333281335626,3.3835215590507,50.4694208687147));
#60561=CARTESIAN_POINT('Ctrl Pts',(5.76807337235824,3.54347560903599,50.4781706490691));
#60562=CARTESIAN_POINT('Ctrl Pts',(5.66638790086499,3.69923467178427,50.4869204294235));
#60563=CARTESIAN_POINT('Ctrl Pts',(5.56470608502893,3.85498813489548,50.4956698952178));
#60564=CARTESIAN_POINT('Ctrl Pts',(5.45659885767108,4.00654667256049,50.5044193610121));
#60565=CARTESIAN_POINT('Ctrl Pts',(5.34243340580669,4.15339551506003,50.5131688268063));
#60566=CARTESIAN_POINT('Ctrl Pts',(5.22827145140762,4.30023985883666,50.5219180245602));
#60567=CARTESIAN_POINT('Ctrl Pts',(5.10805181978264,4.44237456992841,50.5306672223141));
#60568=CARTESIAN_POINT('Ctrl Pts',(4.98218281282733,4.57931691626251,50.5394164200679));
#60569=CARTESIAN_POINT('Ctrl Pts',(4.8563169929641,4.71625579511976,50.5481653962859));
#60570=CARTESIAN_POINT('Ctrl Pts',(4.72480227792017,4.84800236135595,50.5569143725039));
#60571=CARTESIAN_POINT('Ctrl Pts',(4.5880853084829,4.97410918678746,50.5656633487219));
#60572=CARTESIAN_POINT('Ctrl Pts',(4.45135945057145,5.10022421088856,50.5744128937431));
#60573=CARTESIAN_POINT('Ctrl Pts',(4.30943087208213,5.22069856611844,50.5831624387643));
#60574=CARTESIAN_POINT('Ctrl Pts',(4.16278164322637,5.33512305301551,50.5919119837856));
#60575=CARTESIAN_POINT('Ctrl Pts',(4.01614103534579,5.44954081331287,50.6006610144528));
#60576=CARTESIAN_POINT('Ctrl Pts',(3.86478055833622,5.55790924068192,50.6094100451201));
#60577=CARTESIAN_POINT('Ctrl Pts',(3.70921425812181,5.65986029751141,50.6181590757873));
#60578=CARTESIAN_POINT('Ctrl Pts',(3.55364584530355,5.76181273884508,50.6269082252672));
#60579=CARTESIAN_POINT('Ctrl Pts',(3.39387173464586,5.85734747817923,50.635657374747));
#60580=CARTESIAN_POINT('Ctrl Pts',(3.23043456092652,5.94614005448673,50.6444065242269));
#60581=CARTESIAN_POINT('Ctrl Pts',(3.18690768806561,5.96978744811192,50.6467366129599));
#60582=CARTESIAN_POINT('Ctrl Pts',(3.14312114982971,5.99295688499254,50.649066701693));
#60583=CARTESIAN_POINT('Ctrl Pts',(3.09908550384729,6.01564277861008,50.6513967904261));
#60584=CARTESIAN_POINT('Origin',(0.,0.,-63.6971797838103));
#60585=CARTESIAN_POINT('',(3.09908550384738,6.01564277861003,53.0457619208681));
#60586=CARTESIAN_POINT('',(3.09908550384726,6.0156427786101,52.6512695067322));
#60587=CARTESIAN_POINT('',(3.09908550384721,6.01564277861012,-63.6971797838103));
#60588=CARTESIAN_POINT('',(-6.76699958286891,-0.00237601598699733,51.6971797837748));
#60589=CARTESIAN_POINT('Ctrl Pts',(-6.76699958286865,-0.00237601672971834,
51.6971797838098));
#60590=CARTESIAN_POINT('Ctrl Pts',(-6.76692339209237,-0.219370680476571,
51.7073982192068));
#60591=CARTESIAN_POINT('Ctrl Pts',(-6.75640560764649,-0.436117771244051,
51.7176166546039));
#60592=CARTESIAN_POINT('Ctrl Pts',(-6.73554224636009,-0.651735872496242,
51.7278350900009));
#60593=CARTESIAN_POINT('Ctrl Pts',(-6.72434858357413,-0.767419835537226,
51.733317510521));
#60594=CARTESIAN_POINT('Ctrl Pts',(-6.71017775251439,-0.882779033068135,
51.7387999310411));
#60595=CARTESIAN_POINT('Ctrl Pts',(-6.69305057914311,-0.997678778481391,
51.7442823515612));
#60596=CARTESIAN_POINT('Ctrl Pts',(-6.66706730317644,-1.17199077549657,
51.7525996168945));
#60597=CARTESIAN_POINT('Ctrl Pts',(-6.63424504598464,-1.34545547933586,
51.7609168822278));
#60598=CARTESIAN_POINT('Ctrl Pts',(-6.59465426282857,-1.51750589908473,
51.7692341475611));
#60599=CARTESIAN_POINT('Ctrl Pts',(-6.55509687145169,-1.68941120754333,
51.7775443979211));
#60600=CARTESIAN_POINT('Ctrl Pts',(-6.5087824056808,-1.85990427123355,51.7858546482811));
#60601=CARTESIAN_POINT('Ctrl Pts',(-6.45583272896794,-2.02842618194166,
51.7941648986411));
#60602=CARTESIAN_POINT('Ctrl Pts',(-6.40291801411033,-2.19683682023008,
51.8024696618709));
#60603=CARTESIAN_POINT('Ctrl Pts',(-6.34337692216246,-2.36327856825245,
51.8107744251008));
#60604=CARTESIAN_POINT('Ctrl Pts',(-6.27738176702665,-2.52720540340538,
51.8190791883306));
#60605=CARTESIAN_POINT('Ctrl Pts',(-6.21141810664073,-2.69105400804786,
51.8273799882931));
#60606=CARTESIAN_POINT('Ctrl Pts',(-6.13900665096635,-2.85238976968202,
51.8356807882556));
#60607=CARTESIAN_POINT('Ctrl Pts',(-6.06036875139973,-3.01068424067648,
51.8439815882181));
#60608=CARTESIAN_POINT('Ctrl Pts',(-5.98175398977785,-3.16893213605354,
51.8522799458029));
#60609=CARTESIAN_POINT('Ctrl Pts',(-5.89691659061609,-3.32414021335686,
51.8605783033877));
#60610=CARTESIAN_POINT('Ctrl Pts',(-5.80612508777875,-3.47580213261144,
51.8688766609725));
#60611=CARTESIAN_POINT('Ctrl Pts',(-5.71532434711396,-3.62747948311891,
51.8771758628962));
#60612=CARTESIAN_POINT('Ctrl Pts',(-5.61856846448963,-3.77560965235233,
51.8854750648199));
#60613=CARTESIAN_POINT('Ctrl Pts',(-5.51617108132283,-3.91971243863344,
51.8937742667436));
#60614=CARTESIAN_POINT('Ctrl Pts',(-5.41376331700229,-4.06382983420566,
51.9020743100491));
#60615=CARTESIAN_POINT('Ctrl Pts',(-5.30571311328846,-4.20391874899488,
51.9103743533545));
#60616=CARTESIAN_POINT('Ctrl Pts',(-5.19237639804994,-4.33952950686753,
51.91867439666));
#60617=CARTESIAN_POINT('Ctrl Pts',(-5.07900937847468,-4.47517652478232,
51.9269766592578));
#60618=CARTESIAN_POINT('Ctrl Pts',(-4.96035325320555,-4.60634273229985,
51.9352789218557));
#60619=CARTESIAN_POINT('Ctrl Pts',(-4.83680315784621,-4.73261283143349,
51.9435811844535));
#60620=CARTESIAN_POINT('Ctrl Pts',(-4.71319951521926,-4.85893765669883,
51.951887045296));
#60621=CARTESIAN_POINT('Ctrl Pts',(-4.58469791833195,-4.98036189589384,
51.9601929061386));
#60622=CARTESIAN_POINT('Ctrl Pts',(-4.45172927328002,-5.09650816514815,
51.9684987669812));
#60623=CARTESIAN_POINT('Ctrl Pts',(-4.31860344990854,-5.21279172748697,
51.9768144459372));
#60624=CARTESIAN_POINT('Ctrl Pts',(-4.18100029065957,-5.32378462558094,
51.9851301248932));
#60625=CARTESIAN_POINT('Ctrl Pts',(-4.03938352653386,-5.42915000028245,
51.9934458038493));
#60626=CARTESIAN_POINT('Ctrl Pts',(-3.8976771909327,-5.5345820177443,52.001766742406));
#60627=CARTESIAN_POINT('Ctrl Pts',(-3.75195247451745,-5.63437921724193,
52.0100876809628));
#60628=CARTESIAN_POINT('Ctrl Pts',(-3.60270092702286,-5.72824886247347,
52.0184086195196));
#60629=CARTESIAN_POINT('Ctrl Pts',(-3.45322754549838,-5.82225802707373,
52.0267419255684));
#60630=CARTESIAN_POINT('Ctrl Pts',(-3.30021715839903,-5.91032185718474,
52.0350752316172));
#60631=CARTESIAN_POINT('Ctrl Pts',(-3.14418586534891,-5.99219360869958,
52.0434085376661));
#60632=CARTESIAN_POINT('Ctrl Pts',(-3.02933762153226,-6.05245605154592,
52.0495423429188));
#60633=CARTESIAN_POINT('Ctrl Pts',(-2.91285318970383,-6.1093647091172,52.0556761481715));
#60634=CARTESIAN_POINT('Ctrl Pts',(-2.79494455544713,-6.16283813936213,
52.0618099534242));
#60635=CARTESIAN_POINT('Ctrl Pts',(-2.6397897579363,-6.23320329365438,52.0698813666668));
#60636=CARTESIAN_POINT('Ctrl Pts',(-2.48169049578681,-6.297834770252,52.0779527799093));
#60637=CARTESIAN_POINT('Ctrl Pts',(-2.32111802262275,-6.35646915551833,
52.0860241931519));
#60638=CARTESIAN_POINT('Ctrl Pts',(-2.16074713489885,-6.41502993017053,
52.0940854734037));
#60639=CARTESIAN_POINT('Ctrl Pts',(-1.99790956002941,-6.46760846766957,
52.1021467536555));
#60640=CARTESIAN_POINT('Ctrl Pts',(-1.83310086105797,-6.51398727609968,
52.1102080339073));
#60641=CARTESIAN_POINT('Ctrl Pts',(-1.66846292244738,-6.56031803086446,
52.1182609617655));
#60642=CARTESIAN_POINT('Ctrl Pts',(-1.50185827995957,-6.60046173957115,
52.1263138896236));
#60643=CARTESIAN_POINT('Ctrl Pts',(-1.33380208825379,-6.63424909009074,
52.1343668174818));
#60644=CARTESIAN_POINT('Ctrl Pts',(-1.16588322122824,-6.66800883176677,
52.1424131650067));
#60645=CARTESIAN_POINT('Ctrl Pts',(-0.996515529540075,-6.69542247996154,
52.1504595125317));
#60646=CARTESIAN_POINT('Ctrl Pts',(-0.826228832144859,-6.71637066554047,
52.1585058600566));
#60647=CARTESIAN_POINT('Ctrl Pts',(-0.65604403212678,-6.73730631599365,
52.1665473927504));
#60648=CARTESIAN_POINT('Ctrl Pts',(-0.484941690377815,-6.75178416017236,
52.174588925444));
#60649=CARTESIAN_POINT('Ctrl Pts',(-0.313461205972948,-6.75973602090718,
52.1826304581378));
#60650=CARTESIAN_POINT('Ctrl Pts',(-0.138684054289472,-6.76784075407631,
52.1908265871856));
#60651=CARTESIAN_POINT('Ctrl Pts',(0.0364855390093745,-6.76916595288036,
52.1990227162336));
#60652=CARTESIAN_POINT('Ctrl Pts',(0.21147113835977,-6.76369491902472,52.2072188452814));
#60653=CARTESIAN_POINT('Ctrl Pts',(0.383096874713335,-6.75832893338033,
52.2152576021181));
#60654=CARTESIAN_POINT('Ctrl Pts',(0.554545232689751,-6.74642537015907,
52.2232963589547));
#60655=CARTESIAN_POINT('Ctrl Pts',(0.725273008550923,-6.72802111048022,
52.2313351157914));
#60656=CARTESIAN_POINT('Ctrl Pts',(0.896017309056241,-6.70961506946357,
52.2393746506947));
#60657=CARTESIAN_POINT('Ctrl Pts',(1.06604051722078,-6.68470711906572,52.2474141855981));
#60658=CARTESIAN_POINT('Ctrl Pts',(1.23480554568945,-6.65338592480059,52.2554537205014));
#60659=CARTESIAN_POINT('Ctrl Pts',(1.40362032436361,-6.62205549736752,52.2634956253775));
#60660=CARTESIAN_POINT('Ctrl Pts',(1.5711758180773,-6.58430813107191,52.2715375302536));
#60661=CARTESIAN_POINT('Ctrl Pts',(1.73694625459791,-6.54028338137105,52.2795794351296));
#60662=CARTESIAN_POINT('Ctrl Pts',(1.90830850624375,-6.49477357639478,52.2878926118094));
#60663=CARTESIAN_POINT('Ctrl Pts',(2.07776274408362,-6.44255559117958,52.2962057884892));
#60664=CARTESIAN_POINT('Ctrl Pts',(2.24474748498567,-6.38383879250178,52.304518965169));
#60665=CARTESIAN_POINT('Ctrl Pts',(2.40656372173722,-6.32693939352188,52.3125748327801));
#60666=CARTESIAN_POINT('Ctrl Pts',(2.56606073966611,-6.26393769263172,52.3206307003911));
#60667=CARTESIAN_POINT('Ctrl Pts',(2.72275047413203,-6.19507214289017,52.3286865680022));
#60668=CARTESIAN_POINT('Ctrl Pts',(2.88694734965355,-6.12290718494205,52.3371283992164));
#60669=CARTESIAN_POINT('Ctrl Pts',(3.04806088839697,-6.04430288375702,52.3455702304305));
#60670=CARTESIAN_POINT('Ctrl Pts',(3.20556180836742,-5.95958576519679,52.3540120616447));
#60671=CARTESIAN_POINT('Ctrl Pts',(3.36306272833788,-5.87486864663656,52.3624538928589));
#60672=CARTESIAN_POINT('Ctrl Pts',(3.51695067594288,-5.78403901878042,52.370895724073));
#60673=CARTESIAN_POINT('Ctrl Pts',(3.66673498003363,-5.68747251300591,52.3793375552872));
#60674=CARTESIAN_POINT('Ctrl Pts',(3.81276883251153,-5.59332393753143,52.3875680113531));
#60675=CARTESIAN_POINT('Ctrl Pts',(3.95538799712883,-5.49340951628428,52.3957984674189));
#60676=CARTESIAN_POINT('Ctrl Pts',(4.09410662674354,-5.388003334154,52.4040289234848));
#60677=CARTESIAN_POINT('Ctrl Pts',(4.23266058917079,-5.28272227537306,52.4122496095143));
#60678=CARTESIAN_POINT('Ctrl Pts',(4.3673229536294,-5.17196265135855,52.4204702955438));
#60679=CARTESIAN_POINT('Ctrl Pts',(4.4976345674635,-5.05604314633068,52.4286909815733));
#60680=CARTESIAN_POINT('Ctrl Pts',(4.62781763827388,-4.94023798754752,52.436903558488));
#60681=CARTESIAN_POINT('Ctrl Pts',(4.75365823930553,-4.81928332078326,52.4451161354027));
#60682=CARTESIAN_POINT('Ctrl Pts',(4.87472812724708,-4.69353967549292,52.4533287123174));
#60683=CARTESIAN_POINT('Ctrl Pts',(4.99570287010013,-4.56789484825274,52.4615348352213));
#60684=CARTESIAN_POINT('Ctrl Pts',(5.11191411979888,-4.43746879566858,52.4697409581252));
#60685=CARTESIAN_POINT('Ctrl Pts',(5.2229684656058,-4.3026607357875,52.4779470810292));
#60686=CARTESIAN_POINT('Ctrl Pts',(5.33395780444062,-4.16793158739542,52.4861484003822));
#60687=CARTESIAN_POINT('Ctrl Pts',(5.43979602554531,-4.02882581757971,52.4943497197353));
#60688=CARTESIAN_POINT('Ctrl Pts',(5.54012814395647,-3.88577780483412,52.5025510390883));
#60689=CARTESIAN_POINT('Ctrl Pts',(5.64043147946015,-3.74277082917397,52.5107500056772));
#60690=CARTESIAN_POINT('Ctrl Pts',(5.73523164973299,-3.59582415415112,52.518948972266));
#60691=CARTESIAN_POINT('Ctrl Pts',(5.82421523360115,-3.44540359213377,52.5271479388549));
#60692=CARTESIAN_POINT('Ctrl Pts',(5.9131870667851,-3.29500289383112,52.5353458227331));
#60693=CARTESIAN_POINT('Ctrl Pts',(5.99634366011715,-3.14112953031877,52.5435437066114));
#60694=CARTESIAN_POINT('Ctrl Pts',(6.07341605438554,-2.98427653382389,52.5517415904897));
#60695=CARTESIAN_POINT('Ctrl Pts',(6.15049227131832,-2.82741575767759,52.5599398809695));
#60696=CARTESIAN_POINT('Ctrl Pts',(6.22148352979553,-2.66757537598841,52.5681381714494));
#60697=CARTESIAN_POINT('Ctrl Pts',(6.28616777047431,-2.50527119519027,52.5763364619293));
#60698=CARTESIAN_POINT('Ctrl Pts',(6.35086696943216,-2.34292948142884,52.58453664827));
#60699=CARTESIAN_POINT('Ctrl Pts',(6.40925611294659,-2.17812316683632,52.5927368346107));
#60700=CARTESIAN_POINT('Ctrl Pts',(6.46116202352605,-2.01138616524645,52.6009370209514));
#60701=CARTESIAN_POINT('Ctrl Pts',(6.51311700707134,-1.84449152690403,52.6091449599248));
#60702=CARTESIAN_POINT('Ctrl Pts',(6.55857640511746,-1.67566289763885,52.6173528988982));
#60703=CARTESIAN_POINT('Ctrl Pts',(6.59741724550374,-1.5054483347926,52.6255608378717));
#60704=CARTESIAN_POINT('Ctrl Pts',(6.63627692875847,-1.33515119570491,52.6337727587651));
#60705=CARTESIAN_POINT('Ctrl Pts',(6.66851158650499,-1.16346713474569,52.6419846796584));
#60706=CARTESIAN_POINT('Ctrl Pts',(6.6940497798853,-0.990952342152505,52.6501966005517));
#60707=CARTESIAN_POINT('Ctrl Pts',(6.71962299485218,-0.818200972850359,
52.6584197827937));
#60708=CARTESIAN_POINT('Ctrl Pts',(6.73848135445139,-0.644616951801082,
52.6666429650357));
#60709=CARTESIAN_POINT('Ctrl Pts',(6.7506054051546,-0.470760728924464,52.6748661472776));
#60710=CARTESIAN_POINT('Ctrl Pts',(6.76141699865814,-0.315724853884322,
52.6821991505685));
#60711=CARTESIAN_POINT('Ctrl Pts',(6.76687410868896,-0.160472716684156,
52.6895321538594));
#60712=CARTESIAN_POINT('Ctrl Pts',(6.76699784576786,-0.00539957157468165,
52.6968651571503));
#60713=CARTESIAN_POINT('Ctrl Pts',(6.76714861808691,0.183555412008736,52.7058003439324));
#60714=CARTESIAN_POINT('Ctrl Pts',(6.75938087136423,0.372636727960242,52.7147355307145));
#60715=CARTESIAN_POINT('Ctrl Pts',(6.7436899197528,0.561190935622188,52.7236707174967));
#60716=CARTESIAN_POINT('Ctrl Pts',(6.72802246833288,0.749462747410466,52.7325925221331));
#60717=CARTESIAN_POINT('Ctrl Pts',(6.70445551119342,0.937208769276504,52.7415143267696));
#60718=CARTESIAN_POINT('Ctrl Pts',(6.67303631072846,1.12377728919014,52.750436131406));
#60719=CARTESIAN_POINT('Ctrl Pts',(6.64169374914481,1.3098907242371,52.7593361736451));
#60720=CARTESIAN_POINT('Ctrl Pts',(6.6025372141473,1.49483213548823,52.7682362158841));
#60721=CARTESIAN_POINT('Ctrl Pts',(6.55566537160227,1.67795725081864,52.7771362581231));
#60722=CARTESIAN_POINT('Ctrl Pts',(6.50886568894818,1.86080044234077,52.7860225986163));
#60723=CARTESIAN_POINT('Ctrl Pts',(6.45437445567373,2.04183266664652,52.7949089391094));
#60724=CARTESIAN_POINT('Ctrl Pts',(6.39234132796682,2.22041918266967,52.8037952796025));
#60725=CARTESIAN_POINT('Ctrl Pts',(6.33046680813958,2.39854908414358,52.8126588992741));
#60726=CARTESIAN_POINT('Ctrl Pts',(6.26108895703377,2.57424551200998,52.8215225189456));
#60727=CARTESIAN_POINT('Ctrl Pts',(6.184407005314,2.74688896619852,52.8303861386172));
#60728=CARTESIAN_POINT('Ctrl Pts',(6.11161249114023,2.91078015690351,52.838800411772));
#60729=CARTESIAN_POINT('Ctrl Pts',(6.0322360834037,3.07191996059379,52.8472146849269));
#60730=CARTESIAN_POINT('Ctrl Pts',(5.94649005211601,3.22979025016879,52.8556289580817));
#60731=CARTESIAN_POINT('Ctrl Pts',(5.86282314627675,3.38383258255816,52.86383920629));
#60732=CARTESIAN_POINT('Ctrl Pts',(5.77317128137702,3.53461350358046,52.8720494544983));
#60733=CARTESIAN_POINT('Ctrl Pts',(5.67782841486083,3.68165091927507,52.8802597027066));
#60734=CARTESIAN_POINT('Ctrl Pts',(5.58246288344398,3.82872328869556,52.8884719026546));
#60735=CARTESIAN_POINT('Ctrl Pts',(5.48140384877693,3.97205008117772,52.8966841026027));
#60736=CARTESIAN_POINT('Ctrl Pts',(5.3749883397868,4.11117858371002,52.9048963025507));
#60737=CARTESIAN_POINT('Ctrl Pts',(5.2685285840888,4.2503649347483,52.9131119170651));
#60738=CARTESIAN_POINT('Ctrl Pts',(5.15670813311193,4.38534923569393,52.9213275315794));
#60739=CARTESIAN_POINT('Ctrl Pts',(5.03990403583711,4.51571215973215,52.9295431460938));
#60740=CARTESIAN_POINT('Ctrl Pts',(4.92296877268048,4.64622147562037,52.9377679863831));
#60741=CARTESIAN_POINT('Ctrl Pts',(4.80103892298979,4.77209878408107,52.9459928266725));
#60742=CARTESIAN_POINT('Ctrl Pts',(4.67452878860127,4.89296123063917,52.9542176669618));
#60743=CARTESIAN_POINT('Ctrl Pts',(4.5479376200735,5.01390109379612,52.9624477755473));
#60744=CARTESIAN_POINT('Ctrl Pts',(4.4167605844359,5.12981945661114,52.9706778841329));
#60745=CARTESIAN_POINT('Ctrl Pts',(4.28144468026112,5.24037407537513,52.9789079927184));
#60746=CARTESIAN_POINT('Ctrl Pts',(4.14594325590463,5.35108026621845,52.9871493849091));
#60747=CARTESIAN_POINT('Ctrl Pts',(4.00629191223432,5.45640781091807,52.9953907770998));
#60748=CARTESIAN_POINT('Ctrl Pts',(3.86296701449437,5.5560574911468,53.0036321692905));
#60749=CARTESIAN_POINT('Ctrl Pts',(3.80058837805495,5.59942756342531,53.0072190325314));
#60750=CARTESIAN_POINT('Ctrl Pts',(3.73751421717592,5.64172271250377,53.0108058957724));
#60751=CARTESIAN_POINT('Ctrl Pts',(3.67378519826734,5.68292101977424,53.0143927590134));
#60752=CARTESIAN_POINT('Ctrl Pts',(3.52366072521857,5.77997059429149,53.0228422214901));
#60753=CARTESIAN_POINT('Ctrl Pts',(3.36955833612814,5.87115183969503,53.0312916839669));
#60754=CARTESIAN_POINT('Ctrl Pts',(3.21196465222055,5.95613734503208,53.0397411464436));
#60755=CARTESIAN_POINT('Ctrl Pts',(3.17453284224266,5.97632318755934,53.0417480712518));
#60756=CARTESIAN_POINT('Ctrl Pts',(3.13690420305201,5.9961596765056,53.04375499606));
#60757=CARTESIAN_POINT('Ctrl Pts',(3.09908550384738,6.01564277861003,53.0457619208681));
#60758=CARTESIAN_POINT('Ctrl Pts',(3.0990855038473,6.01564277861008,51.0457613895064));
#60759=CARTESIAN_POINT('Ctrl Pts',(2.93977103845707,6.09771699219197,51.0541945390125));
#60760=CARTESIAN_POINT('Ctrl Pts',(2.77726086164494,6.17342423470136,51.0626276885186));
#60761=CARTESIAN_POINT('Ctrl Pts',(2.61209614700951,6.2425349593557,51.0710608380246));
#60762=CARTESIAN_POINT('Ctrl Pts',(2.44678085035074,6.31170869282385,51.0795016761022));
#60763=CARTESIAN_POINT('Ctrl Pts',(2.27880649072714,6.37427377006968,51.0879425141797));
#60764=CARTESIAN_POINT('Ctrl Pts',(2.10873242976109,6.43004949745132,51.0963833522573));
#60765=CARTESIAN_POINT('Ctrl Pts',(2.02246941290357,6.45833942293456,51.1006646174499));
#60766=CARTESIAN_POINT('Ctrl Pts',(1.93566646209994,6.48488351458044,51.1049458826424));
#60767=CARTESIAN_POINT('Ctrl Pts',(1.84839780253877,6.50966316821154,51.109227147835));
#60768=CARTESIAN_POINT('Ctrl Pts',(1.68244540946173,6.55678481348922,51.117368515053));
#60769=CARTESIAN_POINT('Ctrl Pts',(1.51447841508181,6.59761636710254,51.1255098822709));
#60770=CARTESIAN_POINT('Ctrl Pts',(1.34501910234251,6.63198406318454,51.1336512494888));
#60771=CARTESIAN_POINT('Ctrl Pts',(1.17570771469497,6.6663217588817,51.1417855099124));
#60772=CARTESIAN_POINT('Ctrl Pts',(1.00490695799231,6.69420675616965,51.149919770336));
#60773=CARTESIAN_POINT('Ctrl Pts',(0.833154105077299,6.71551511331729,51.1580540307596));
#60774=CARTESIAN_POINT('Ctrl Pts',(0.661518415754918,6.73680893467332,51.1661827422845));
#60775=CARTESIAN_POINT('Ctrl Pts',(0.488932285107155,6.751535003179,51.1743114538094));
#60776=CARTESIAN_POINT('Ctrl Pts',(0.315942968594335,6.75962048051485,51.1824401653343));
#60777=CARTESIAN_POINT('Ctrl Pts',(0.143036147489403,6.767702102036,51.190565000427));
#60778=CARTESIAN_POINT('Ctrl Pts',(-0.0302731117240618,6.7691494214961,
51.1986898355196));
#60779=CARTESIAN_POINT('Ctrl Pts',(-0.203432659633227,6.7639414658167,51.2068146706122));
#60780=CARTESIAN_POINT('Ctrl Pts',(-0.376543731041455,6.75873496811909,
51.2149372311345));
#60781=CARTESIAN_POINT('Ctrl Pts',(-0.549504809086361,6.74687691816608,
51.2230597916567));
#60782=CARTESIAN_POINT('Ctrl Pts',(-0.721764004372139,6.72839845148849,
51.231182352179));
#60783=CARTESIAN_POINT('Ctrl Pts',(-0.894032354787369,6.70991900272832,
51.2393053443943));
#60784=CARTESIAN_POINT('Ctrl Pts',(-1.06559838353237,6.68481846948204,51.2474283366096));
#60785=CARTESIAN_POINT('Ctrl Pts',(-1.23591539037973,6.65317985235801,51.2555513288248));
#60786=CARTESIAN_POINT('Ctrl Pts',(-1.32285703202534,6.63702930249175,51.2596978688055));
#60787=CARTESIAN_POINT('Ctrl Pts',(-1.40947332344334,6.61917589421818,51.263844408786));
#60788=CARTESIAN_POINT('Ctrl Pts',(-1.49569253948153,6.59963581020493,51.2679909487667));
#60789=CARTESIAN_POINT('Ctrl Pts',(-1.68249021710502,6.55730136920716,51.2769746077947));
#60790=CARTESIAN_POINT('Ctrl Pts',(-1.86733093762222,6.50706793785618,51.2859582668227));
#60791=CARTESIAN_POINT('Ctrl Pts',(-2.04957887020492,6.44914842865394,51.2949419258508));
#60792=CARTESIAN_POINT('Ctrl Pts',(-2.23213990280502,6.3911294143485,51.3039410187098));
#60793=CARTESIAN_POINT('Ctrl Pts',(-2.41209901646806,6.32539800234898,51.3129401115689));
#60794=CARTESIAN_POINT('Ctrl Pts',(-2.58883872890599,6.25221585005799,51.321939204428));
#60795=CARTESIAN_POINT('Ctrl Pts',(-2.76599284657973,6.17886210607062,51.330959397645));
#60796=CARTESIAN_POINT('Ctrl Pts',(-2.93991223778385,6.09802275946844,51.3399795908621));
#60797=CARTESIAN_POINT('Ctrl Pts',(-3.10999997975497,6.01000741479776,51.3489997840791));
#60798=CARTESIAN_POINT('Ctrl Pts',(-3.28025997815563,5.92190293255114,51.3580291125004));
#60799=CARTESIAN_POINT('Ctrl Pts',(-3.4466803656029,5.82660804874572,51.3670584409218));
#60800=CARTESIAN_POINT('Ctrl Pts',(-3.60869038939335,5.72447750222674,51.3760877693431));
#60801=CARTESIAN_POINT('Ctrl Pts',(-3.77092881466131,5.62220297222342,51.3851298272976));
#60802=CARTESIAN_POINT('Ctrl Pts',(-3.92874424145666,5.51307363799984,51.394171885252));
#60803=CARTESIAN_POINT('Ctrl Pts',(-4.08159446284338,5.39748790094858,51.4032139432064));
#60804=CARTESIAN_POINT('Ctrl Pts',(-4.2142419015127,5.29717956100994,51.4110608787036));
#60805=CARTESIAN_POINT('Ctrl Pts',(-4.34315034565717,5.19200947772809,51.4189078142008));
#60806=CARTESIAN_POINT('Ctrl Pts',(-4.46798590640216,5.08226238403643,51.426754749698));
#60807=CARTESIAN_POINT('Ctrl Pts',(-4.60565239656515,4.96123519351512,51.4354082139992));
#60808=CARTESIAN_POINT('Ctrl Pts',(-4.73848618965122,4.8345340811254,51.4440616783005));
#60809=CARTESIAN_POINT('Ctrl Pts',(-4.86602383026489,4.70256324607062,51.4527151426017));
#60810=CARTESIAN_POINT('Ctrl Pts',(-4.99344398262479,4.57071398314846,51.4613606352924));
#60811=CARTESIAN_POINT('Ctrl Pts',(-5.11557750295289,4.43360489781744,51.470006127983));
#60812=CARTESIAN_POINT('Ctrl Pts',(-5.23199650576142,4.29167817569075,51.4786516206737));
#60813=CARTESIAN_POINT('Ctrl Pts',(-5.35191777441042,4.14548183177755,51.48755719817));
#60814=CARTESIAN_POINT('Ctrl Pts',(-5.46577508277386,3.99417367043613,51.4964627756663));
#60815=CARTESIAN_POINT('Ctrl Pts',(-5.57314262826314,3.83827698909761,51.5053683531627));
#60816=CARTESIAN_POINT('Ctrl Pts',(-5.67717675938209,3.68722039454225,51.5139974413356));
#60817=CARTESIAN_POINT('Ctrl Pts',(-5.77511785628655,3.53185619126521,51.5226265295086));
#60818=CARTESIAN_POINT('Ctrl Pts',(-5.86661983604594,3.37269338946076,51.5312556176816));
#60819=CARTESIAN_POINT('Ctrl Pts',(-5.96251961310948,3.20588085436599,51.5402994398396));
#60820=CARTESIAN_POINT('Ctrl Pts',(-6.05134583987484,3.03489584060695,51.5493432619976));
#60821=CARTESIAN_POINT('Ctrl Pts',(-6.13275139796263,2.86035824518319,51.5583870841557));
#60822=CARTESIAN_POINT('Ctrl Pts',(-6.21415695605036,2.68582064975955,51.5674309063137));
#60823=CARTESIAN_POINT('Ctrl Pts',(-6.28814165119957,2.50773080723462,51.5764747284717));
#60824=CARTESIAN_POINT('Ctrl Pts',(-6.35441396599907,2.32673852177592,51.5855185506297));
#60825=CARTESIAN_POINT('Ctrl Pts',(-6.41379649453772,2.16456251224549,51.5936221611497));
#60826=CARTESIAN_POINT('Ctrl Pts',(-6.46697760690456,2.00008111175776,51.6017257716698));
#60827=CARTESIAN_POINT('Ctrl Pts',(-6.51378575904546,1.83381680798725,51.6098293821898));
#60828=CARTESIAN_POINT('Ctrl Pts',(-6.56060798484162,1.66750251406791,51.6179354291961));
#60829=CARTESIAN_POINT('Ctrl Pts',(-6.60105331856789,1.499404599782,51.6260414762025));
#60830=CARTESIAN_POINT('Ctrl Pts',(-6.63500037413545,1.33005978633387,51.6341475232088));
#60831=CARTESIAN_POINT('Ctrl Pts',(-6.6689527451573,1.16068845675348,51.6422548394658));
#60832=CARTESIAN_POINT('Ctrl Pts',(-6.69640474652884,0.990070201969377,
51.6503621557227));
#60833=CARTESIAN_POINT('Ctrl Pts',(-6.71728642054541,0.818750355331961,
51.6584694719797));
#60834=CARTESIAN_POINT('Ctrl Pts',(-6.7381836852255,0.647302597968643,51.6665828413165));
#60835=CARTESIAN_POINT('Ctrl Pts',(-6.75250078859449,0.475152569323373,
51.6746962106534));
#60836=CARTESIAN_POINT('Ctrl Pts',(-6.76021974971399,0.302849691393129,
51.6828095799902));
#60837=CARTESIAN_POINT('Ctrl Pts',(-6.76477696220644,0.201123459633057,
51.6875996479184));
#60838=CARTESIAN_POINT('Ctrl Pts',(-6.76703529859893,0.0993439772433435,
51.6923897158466));
#60839=CARTESIAN_POINT('Ctrl Pts',(-6.76699958286891,-0.00237601598698748,
51.6971797837748));
#60840=CARTESIAN_POINT('',(-6.767,5.55191004660612E-12,51.3028202161897));
#60841=CARTESIAN_POINT('Ctrl Pts',(3.09908550384729,6.01564277861008,50.6513967904261));
#60842=CARTESIAN_POINT('Ctrl Pts',(2.9337323201834,6.10082796552475,50.6601462383254));
#60843=CARTESIAN_POINT('Ctrl Pts',(2.76486502144439,6.17919158180185,50.6688956862247));
#60844=CARTESIAN_POINT('Ctrl Pts',(2.59305716434367,6.25046746591373,50.677645134124));
#60845=CARTESIAN_POINT('Ctrl Pts',(2.42125069459293,6.32174277447221,50.6863945113714));
#60846=CARTESIAN_POINT('Ctrl Pts',(2.24650397871065,6.38593035557824,50.6951438886188));
#60847=CARTESIAN_POINT('Ctrl Pts',(2.06941053323773,6.44281220003538,50.7038932658662));
#60848=CARTESIAN_POINT('Ctrl Pts',(1.89231845896681,6.49969360406686,50.7126425753688));
#60849=CARTESIAN_POINT('Ctrl Pts',(1.71287996431499,6.54926929700882,50.7213918848714));
#60850=CARTESIAN_POINT('Ctrl Pts',(1.53170449173495,6.59137090065481,50.730141194374));
#60851=CARTESIAN_POINT('Ctrl Pts',(1.35053036178145,6.63347219230089,50.7388904390386));
#60852=CARTESIAN_POINT('Ctrl Pts',(1.16761955878803,6.66809944062462,50.7476396837032));
#60853=CARTESIAN_POINT('Ctrl Pts',(0.98359330930991,6.695135039854,50.7563889283678));
#60854=CARTESIAN_POINT('Ctrl Pts',(0.799568362459444,6.72217044771221,50.765138111101));
#60855=CARTESIAN_POINT('Ctrl Pts',(0.614428268438097,6.74161427235981,50.7738872938341));
#60856=CARTESIAN_POINT('Ctrl Pts',(0.428801816329812,6.75340047696805,50.7826364765673));
#60857=CARTESIAN_POINT('Ctrl Pts',(0.243176616522342,6.76518660206243,50.7913856002755));
#60858=CARTESIAN_POINT('Ctrl Pts',(0.057065351165034,6.76931519233997,50.8001347239836));
#60859=CARTESIAN_POINT('Ctrl Pts',(-0.128899900800441,6.76577222610794,
50.8088838476917));
#60860=CARTESIAN_POINT('Ctrl Pts',(-0.31486395994235,6.76222928260131,50.817632915281));
#60861=CARTESIAN_POINT('Ctrl Pts',(-0.500681721080927,6.75101488651275,
50.8263819828702));
#60862=CARTESIAN_POINT('Ctrl Pts',(-0.685722110173463,6.73216712415989,
50.8351310504595));
#60863=CARTESIAN_POINT('Ctrl Pts',(-0.870761373827964,6.71331947644141,
50.8438800648359));
#60864=CARTESIAN_POINT('Ctrl Pts',(-1.05502298984397,6.68683858439988,50.8526290792122));
#60865=CARTESIAN_POINT('Ctrl Pts',(-1.23788117676131,6.65281438131413,50.8613780935886));
#60866=CARTESIAN_POINT('Ctrl Pts',(-1.43009641451859,6.61704912302363,50.8705748044761));
#60867=CARTESIAN_POINT('Ctrl Pts',(-1.62076048992755,6.5729483708315,50.8797715153637));
#60868=CARTESIAN_POINT('Ctrl Pts',(-1.80915798961185,6.52067760042034,50.8889682262512));
#60869=CARTESIAN_POINT('Ctrl Pts',(-1.98840443003071,6.47094578577391,50.8977182239577));
#60870=CARTESIAN_POINT('Ctrl Pts',(-2.16559895952256,6.41381888474454,50.9064682216642));
#60871=CARTESIAN_POINT('Ctrl Pts',(-2.34013966242391,6.34949095285209,50.9152182193707));
#60872=CARTESIAN_POINT('Ctrl Pts',(-2.51467682554086,6.28516432556656,50.9239680396223));
#60873=CARTESIAN_POINT('Ctrl Pts',(-2.68656000078916,6.21363705879629,50.9327178598739));
#60874=CARTESIAN_POINT('Ctrl Pts',(-2.85520533840965,6.13515211510823,50.9414676801255));
#60875=CARTESIAN_POINT('Ctrl Pts',(-3.02384747998402,6.05666865881084,50.9502173345567));
#60876=CARTESIAN_POINT('Ctrl Pts',(-3.18925164684609,5.97122791039805,50.958966988988));
#60877=CARTESIAN_POINT('Ctrl Pts',(-3.35085601829228,5.87912008251868,50.9677166434192));
#60878=CARTESIAN_POINT('Ctrl Pts',(-3.51245754191484,5.78701387778134,50.9764661436624));
#60879=CARTESIAN_POINT('Ctrl Pts',(-3.67025915510997,5.68824097060943,50.9852156439055));
#60880=CARTESIAN_POINT('Ctrl Pts',(-3.82372487928891,5.58313684656816,50.9939651441487));
#60881=CARTESIAN_POINT('Ctrl Pts',(-3.97718810300834,5.47803443501746,51.0027145018338));
#60882=CARTESIAN_POINT('Ctrl Pts',(-4.12631534263042,5.36660117496362,51.0114638595189));
#60883=CARTESIAN_POINT('Ctrl Pts',(-4.27060009886224,5.24921554097352,51.020213217204));
#60884=CARTESIAN_POINT('Ctrl Pts',(-4.41488269594234,5.13183166360274,51.0289624439592));
#60885=CARTESIAN_POINT('Ctrl Pts',(-4.5543227323513,5.00849577139434,51.0377116707144));
#60886=CARTESIAN_POINT('Ctrl Pts',(-4.68844662480268,4.87962675277284,51.0464608974696));
#60887=CARTESIAN_POINT('Ctrl Pts',(-4.8225686883521,4.75075949139828,51.055210004921));
#60888=CARTESIAN_POINT('Ctrl Pts',(-4.95137454637907,4.61635945312477,51.0639591123725));
#60889=CARTESIAN_POINT('Ctrl Pts',(-5.07442674461115,4.47688309134549,51.072708219824));
#60890=CARTESIAN_POINT('Ctrl Pts',(-5.19747742838558,4.33740844616327,51.0814572195964));
#60891=CARTESIAN_POINT('Ctrl Pts',(-5.31477440450931,4.19285781736023,51.0902062193687));
#60892=CARTESIAN_POINT('Ctrl Pts',(-5.42591931531142,4.04372211999421,51.0989552191411));
#60893=CARTESIAN_POINT('Ctrl Pts',(-5.53707636462976,3.89457013500809,51.1077051744217));
#60894=CARTESIAN_POINT('Ctrl Pts',(-5.6420798327347,3.74083230916422,51.1164551297023));
#60895=CARTESIAN_POINT('Ctrl Pts',(-5.74057303468751,3.58303087251822,51.1252050849829));
#60896=CARTESIAN_POINT('Ctrl Pts',(-5.83906243363768,3.42523552887426,51.1339547024117));
#60897=CARTESIAN_POINT('Ctrl Pts',(-5.93104191768428,3.26337713156988,51.1427043198405));
#60898=CARTESIAN_POINT('Ctrl Pts',(-6.01619906699658,3.09800545291152,51.1514539372693));
#60899=CARTESIAN_POINT('Ctrl Pts',(-6.10135338095388,2.93263928039585,51.1602032633747));
#60900=CARTESIAN_POINT('Ctrl Pts',(-6.17968568352847,2.76376031540206,51.1689525894801));
#60901=CARTESIAN_POINT('Ctrl Pts',(-6.25092992694897,2.59194213831516,51.1777019155855));
#60902=CARTESIAN_POINT('Ctrl Pts',(-6.32217217691108,2.42012876880806,51.1864509968793));
#60903=CARTESIAN_POINT('Ctrl Pts',(-6.3863266548385,2.24537661647669,51.195200078173));
#60904=CARTESIAN_POINT('Ctrl Pts',(-6.44317547869346,2.06827917621469,51.2039491594668));
#60905=CARTESIAN_POINT('Ctrl Pts',(-6.50002944235934,1.89116572423432,51.2126990317818));
#60906=CARTESIAN_POINT('Ctrl Pts',(-6.54957634250397,1.71170683289203,51.2214489040967));
#60907=CARTESIAN_POINT('Ctrl Pts',(-6.59164787708395,1.53051209225365,51.2301987764117));
#60908=CARTESIAN_POINT('Ctrl Pts',(-6.63371649075014,1.34932993148009,51.2389480412465));
#60909=CARTESIAN_POINT('Ctrl Pts',(-6.66831071257132,1.16641244173961,51.2476973060813));
#60910=CARTESIAN_POINT('Ctrl Pts',(-6.69531304840342,0.982380875159358,
51.2564465709161));
#60911=CARTESIAN_POINT('Ctrl Pts',(-6.72231677033052,0.798339861795154,
51.2651962848718));
#60912=CARTESIAN_POINT('Ctrl Pts',(-6.74172778477897,0.61318494072943,51.2739459988274));
#60913=CARTESIAN_POINT('Ctrl Pts',(-6.75348015835523,0.427545027689796,
51.2826957127831));
#60914=CARTESIAN_POINT('Ctrl Pts',(-6.76249038365211,0.28521995354819,51.2894038805853));
#60915=CARTESIAN_POINT('Ctrl Pts',(-6.76699999999988,0.142609995760808,
51.2961120483875));
#60916=CARTESIAN_POINT('Ctrl Pts',(-6.767,5.55191001589178E-12,51.3028202161897));
#60917=CARTESIAN_POINT('Ctrl Pts',(-6.76699999999988,1.30184050356826E-6,
51.3028480745936));
#60918=CARTESIAN_POINT('Ctrl Pts',(-6.7670000339791,-0.176623542518988,
51.3111183913113));
#60919=CARTESIAN_POINT('Ctrl Pts',(-6.76008062728606,-0.353204966336715,
51.319388708029));
#60920=CARTESIAN_POINT('Ctrl Pts',(-6.74627795308297,-0.529171786612536,
51.3276590247467));
#60921=CARTESIAN_POINT('Ctrl Pts',(-6.73246948759393,-0.705212438535618,
51.3359328114998));
#60922=CARTESIAN_POINT('Ctrl Pts',(-6.71177202596096,-0.880637625385335,
51.3442065982531));
#60923=CARTESIAN_POINT('Ctrl Pts',(-6.68427351682208,-1.05488224570849,
51.3524803850062));
#60924=CARTESIAN_POINT('Ctrl Pts',(-6.65665801029845,-1.22986822130954,
51.3607893740828));
#60925=CARTESIAN_POINT('Ctrl Pts',(-6.62218351491507,-1.40366321268522,
51.3690983631594));
#60926=CARTESIAN_POINT('Ctrl Pts',(-6.58099054131082,-1.57570698265177,
51.3774073522359));
#60927=CARTESIAN_POINT('Ctrl Pts',(-6.53989629136811,-1.74733843009267,
51.3856964278721));
#60928=CARTESIAN_POINT('Ctrl Pts',(-6.49211587419647,-1.91722671861169,
51.3939855035082));
#60929=CARTESIAN_POINT('Ctrl Pts',(-6.43783827923141,-2.0848326768503,51.4022745791444));
#60930=CARTESIAN_POINT('Ctrl Pts',(-6.38336509183233,-2.25304261279556,
51.4105935249411));
#60931=CARTESIAN_POINT('Ctrl Pts',(-6.32234795000335,-2.41895341249869,
51.4189124707379));
#60932=CARTESIAN_POINT('Ctrl Pts',(-6.25502576616589,-2.58204215004341,
51.4272314165347));
#60933=CARTESIAN_POINT('Ctrl Pts',(-6.18770358232849,-2.74513088758802,
51.4355503623314));
#60934=CARTESIAN_POINT('Ctrl Pts',(-6.11407655201758,-2.90539726828797,
51.4438693081282));
#60935=CARTESIAN_POINT('Ctrl Pts',(-6.0344288562706,-3.06234507830334,51.452188253925));
#60936=CARTESIAN_POINT('Ctrl Pts',(-5.95354082525634,-3.22173700050624,
51.4606367487534));
#60937=CARTESIAN_POINT('Ctrl Pts',(-5.86626371181114,-3.37806009651829,
51.4690852435818));
#60938=CARTESIAN_POINT('Ctrl Pts',(-5.77285319420822,-3.53078673925798,
51.4775337384102));
#60939=CARTESIAN_POINT('Ctrl Pts',(-5.679528001687,-3.68337387508126,51.4859745160294));
#60940=CARTESIAN_POINT('Ctrl Pts',(-5.5800807456535,-3.8323708228384,51.4944152936486));
#60941=CARTESIAN_POINT('Ctrl Pts',(-5.4748131506473,-3.9772741878703,51.5028560712677));
#60942=CARTESIAN_POINT('Ctrl Pts',(-5.3696255235808,-4.12206747511848,51.511290436737));
#60943=CARTESIAN_POINT('Ctrl Pts',(-5.25862656714004,-4.26277311012421,
51.5197248022063));
#60944=CARTESIAN_POINT('Ctrl Pts',(-5.14216168741832,-4.39891602334566,
51.5281591676756));
#60945=CARTESIAN_POINT('Ctrl Pts',(-5.02576739655974,-4.53497642093242,
51.5365884211122));
#60946=CARTESIAN_POINT('Ctrl Pts',(-4.90391400364841,-4.66647935755995,
51.5450176745489));
#60947=CARTESIAN_POINT('Ctrl Pts',(-4.77698786484249,-4.79298194646585,
51.5534469279855));
#60948=CARTESIAN_POINT('Ctrl Pts',(-4.65011918532413,-4.91942726782465,
51.5618723655108));
#60949=CARTESIAN_POINT('Ctrl Pts',(-4.51818257479515,-5.04087652022402,
51.570297803036));
#60950=CARTESIAN_POINT('Ctrl Pts',(-4.38160226463412,-5.15692258954439,
51.5787232405613));
#60951=CARTESIAN_POINT('Ctrl Pts',(-4.24505195749479,-5.27294316666362,
51.5871468272445));
#60952=CARTESIAN_POINT('Ctrl Pts',(-4.10386023675893,-5.38356270951558,
51.5955704139276));
#60953=CARTESIAN_POINT('Ctrl Pts',(-3.9584859282339,-5.48841308175453,51.6039940006108));
#60954=CARTESIAN_POINT('Ctrl Pts',(-3.81312788633164,-5.59325172178666,
51.6124166447388));
#60955=CARTESIAN_POINT('Ctrl Pts',(-3.6635884600021,-5.69232228314028,51.6208392888668));
#60956=CARTESIAN_POINT('Ctrl Pts',(-3.51035733890251,-5.78529863993323,
51.6292619329948));
#60957=CARTESIAN_POINT('Ctrl Pts',(-3.35712199610203,-5.87827755833616,
51.6376848091767));
#60958=CARTESIAN_POINT('Ctrl Pts',(-3.20019504098331,-5.96516176480793,
51.6461076853586));
#60959=CARTESIAN_POINT('Ctrl Pts',(-3.04009307362458,-6.04566978123184,
51.6545305615406));
#60960=CARTESIAN_POINT('Ctrl Pts',(-2.87996436834894,-6.12619124294121,
51.6629548443895));
#60961=CARTESIAN_POINT('Ctrl Pts',(-2.71665989177677,-6.20033424236853,
51.6713791272386));
#60962=CARTESIAN_POINT('Ctrl Pts',(-2.55071897302026,-6.26786420726187,
51.6798034100875));
#60963=CARTESIAN_POINT('Ctrl Pts',(-2.38466598390274,-6.33543977939665,
51.6882333823857));
#60964=CARTESIAN_POINT('Ctrl Pts',(-2.21597330377069,-6.39639326673437,
51.6966633546838));
#60965=CARTESIAN_POINT('Ctrl Pts',(-2.0451992380346,-6.45053866562652,51.705093326982));
#60966=CARTESIAN_POINT('Ctrl Pts',(-1.87436412332623,-6.50470342062488,
51.7135263128592));
#60967=CARTESIAN_POINT('Ctrl Pts',(-1.70144645902587,-6.55205513943922,
51.7219592987364));
#60968=CARTESIAN_POINT('Ctrl Pts',(-1.52701824724029,-6.59245813582424,
51.7303922846136));
#60969=CARTESIAN_POINT('Ctrl Pts',(-1.3524295625626,-6.63289830271977,51.7388330287864));
#60970=CARTESIAN_POINT('Ctrl Pts',(-1.17632788015482,-6.66637690539049,
51.7472737729592));
#60971=CARTESIAN_POINT('Ctrl Pts',(-0.99929498448611,-6.69280946493929,
51.755714517132));
#60972=CARTESIAN_POINT('Ctrl Pts',(-0.901408768343539,-6.70742473306458,
51.7603816300173));
#60973=CARTESIAN_POINT('Ctrl Pts',(-0.803237970703355,-6.71988674641108,
51.7650487429027));
#60974=CARTESIAN_POINT('Ctrl Pts',(-0.704881448882504,-6.73018804663149,
51.769715855788));
#60975=CARTESIAN_POINT('Ctrl Pts',(-0.53330716257365,-6.74815775723785,
51.777857223006));
#60976=CARTESIAN_POINT('Ctrl Pts',(-0.360826604970594,-6.75958510253059,
51.7859985902239));
#60977=CARTESIAN_POINT('Ctrl Pts',(-0.187984118427604,-6.76438844029665,
51.7941399574419));
#60978=CARTESIAN_POINT('Ctrl Pts',(-0.0152925102300434,-6.76918758511416,
51.8022742178654));
#60979=CARTESIAN_POINT('Ctrl Pts',(0.157760034616686,-6.76737422195983,
51.810408478289));
#60980=CARTESIAN_POINT('Ctrl Pts',(0.330622948664547,-6.75891836508005,
51.8185427387125));
#60981=CARTESIAN_POINT('Ctrl Pts',(0.503367941876163,-6.75046827648041,
51.8266714502374));
#60982=CARTESIAN_POINT('Ctrl Pts',(0.675923197719367,-6.73538473358101,
51.8348001617624));
#60983=CARTESIAN_POINT('Ctrl Pts',(0.847737076126017,-6.71368980887271,
51.8429288732873));
#60984=CARTESIAN_POINT('Ctrl Pts',(1.01946901967,-6.69200523007299,51.8510537083799));
#60985=CARTESIAN_POINT('Ctrl Pts',(1.19045992742188,-6.66371559364873,51.8591785434725));
#60986=CARTESIAN_POINT('Ctrl Pts',(1.36016223062419,-6.6288949083828,51.8673033785652));
#60987=CARTESIAN_POINT('Ctrl Pts',(1.52981702519052,-6.59408397126542,51.8754259390874));
#60988=CARTESIAN_POINT('Ctrl Pts',(1.69818357564917,-6.55274570142064,51.8835484996097));
#60989=CARTESIAN_POINT('Ctrl Pts',(1.86472350392635,-6.50500539999043,51.8916710601319));
#60990=CARTESIAN_POINT('Ctrl Pts',(2.03127228336902,-6.45726256128695,51.8997940523472));
#60991=CARTESIAN_POINT('Ctrl Pts',(2.19599389372482,-6.40311710838076,51.9079170445625));
#60992=CARTESIAN_POINT('Ctrl Pts',(2.35836396200425,-6.34274454969768,51.9160400367778));
#60993=CARTESIAN_POINT('Ctrl Pts',(2.44124893369111,-6.31192619832211,51.9201865767584));
#60994=CARTESIAN_POINT('Ctrl Pts',(2.52352140191928,-6.2794859902824,51.924333116739));
#60995=CARTESIAN_POINT('Ctrl Pts',(2.60511347837492,-6.24545216656003,51.9284796567196));
#60996=CARTESIAN_POINT('Ctrl Pts',(2.78188625705105,-6.17171640875458,51.9374633157477));
#60997=CARTESIAN_POINT('Ctrl Pts',(2.95537670176367,-6.0905341743684,51.9464469747757));
#60998=CARTESIAN_POINT('Ctrl Pts',(3.12499490347401,-6.00222424216736,51.9554306338037));
#60999=CARTESIAN_POINT('Ctrl Pts',(3.29490450745654,-5.91376259443909,51.9644297266627));
#61000=CARTESIAN_POINT('Ctrl Pts',(3.46092835986613,-5.81814888441678,51.9734288195217));
#61001=CARTESIAN_POINT('Ctrl Pts',(3.62250298626108,-5.7157467678799,51.9824279123807));
#61002=CARTESIAN_POINT('Ctrl Pts',(3.78445646000414,-5.61310454699523,51.9914481055977));
#61003=CARTESIAN_POINT('Ctrl Pts',(3.94193963195968,-5.50364220120201,52.0004682988147));
#61004=CARTESIAN_POINT('Ctrl Pts',(4.09441750374241,-5.3877670982558,52.0094884920317));
#61005=CARTESIAN_POINT('Ctrl Pts',(4.24704979755183,-5.27177464275194,52.0185178204531));
#61006=CARTESIAN_POINT('Ctrl Pts',(4.39466647775626,-5.14935660501642,52.0275471488744));
#61007=CARTESIAN_POINT('Ctrl Pts',(4.53676606718758,-5.02096033161141,52.0365764772958));
#61008=CARTESIAN_POINT('Ctrl Pts',(4.67906598839709,-4.89238304534164,52.0456185352502));
#61009=CARTESIAN_POINT('Ctrl Pts',(4.81583308913101,-4.75781083171856,52.0546605932046));
#61010=CARTESIAN_POINT('Ctrl Pts',(4.9466015016186,-4.61772915881655,52.063702651159));
#61011=CARTESIAN_POINT('Ctrl Pts',(5.06008576626844,-4.49616260204803,52.0715495866563));
#61012=CARTESIAN_POINT('Ctrl Pts',(5.16905281435452,-4.37044738490407,52.0793965221536));
#61013=CARTESIAN_POINT('Ctrl Pts',(5.27322252168006,-4.24092127218205,52.087243457651));
#61014=CARTESIAN_POINT('Ctrl Pts',(5.38809906729759,-4.09808212269426,52.0958969219522));
#61015=CARTESIAN_POINT('Ctrl Pts',(5.49724163451786,-3.9504816874404,52.1045503862535));
#61016=CARTESIAN_POINT('Ctrl Pts',(5.60026293498195,-3.79859764374531,52.1132038505548));
#61017=CARTESIAN_POINT('Ctrl Pts',(5.70318933175574,-3.6468535163217,52.1218493432454));
#61018=CARTESIAN_POINT('Ctrl Pts',(5.80000553872059,-3.49083390173163,52.130494835936));
#61019=CARTESIAN_POINT('Ctrl Pts',(5.8903658238081,-3.33104780237593,52.1391403286267));
#61020=CARTESIAN_POINT('Ctrl Pts',(5.98344444294921,-3.16645481252903,52.148045906123));
#61021=CARTESIAN_POINT('Ctrl Pts',(6.06967243221642,-2.99786542904594,52.1569514836193));
#61022=CARTESIAN_POINT('Ctrl Pts',(6.14872001898878,-2.82586820784103,52.1658570611157));
#61023=CARTESIAN_POINT('Ctrl Pts',(6.22531343434019,-2.65921094300921,52.1744861492886));
#61024=CARTESIAN_POINT('Ctrl Pts',(6.29516546568033,-2.48935456885595,52.1831152374617));
#61025=CARTESIAN_POINT('Ctrl Pts',(6.35802242980817,-2.31685989694159,52.1917443256347));
#61026=CARTESIAN_POINT('Ctrl Pts',(6.42390044537226,-2.13607473114859,52.2007881477927));
#61027=CARTESIAN_POINT('Ctrl Pts',(6.48209425047706,-1.95239170379207,52.2098319699507));
#61028=CARTESIAN_POINT('Ctrl Pts',(6.53236815440517,-1.76648104867085,52.2188757921087));
#61029=CARTESIAN_POINT('Ctrl Pts',(6.58264205833331,-1.58057039354951,52.2279196142667));
#61030=CARTESIAN_POINT('Ctrl Pts',(6.62499592706467,-1.3924324735803,52.2369634364247));
#61031=CARTESIAN_POINT('Ctrl Pts',(6.65925397533326,-1.20275745352427,52.2460072585827));
#61032=CARTESIAN_POINT('Ctrl Pts',(6.6911709138044,-1.02604435249828,52.2544330484321));
#61033=CARTESIAN_POINT('Ctrl Pts',(6.71604695694967,-0.848074481819348,
52.2628588382814));
#61034=CARTESIAN_POINT('Ctrl Pts',(6.73380635353076,-0.669433337344986,
52.2712846281308));
#61035=CARTESIAN_POINT('Ctrl Pts',(6.75156987088937,-0.490750742114677,
52.2797123730469));
#61036=CARTESIAN_POINT('Ctrl Pts',(6.76221341643423,-0.311396892409265,
52.288140117963));
#61037=CARTESIAN_POINT('Ctrl Pts',(6.76571320457185,-0.131961484843546,
52.2965678628792));
#61038=CARTESIAN_POINT('Ctrl Pts',(6.76921427870605,0.0475398562333889,
52.3049987045688));
#61039=CARTESIAN_POINT('Ctrl Pts',(6.76556635501422,0.227122483642489,52.3134295462584));
#61040=CARTESIAN_POINT('Ctrl Pts',(6.75479776247298,0.406197228067859,52.321860387948));
#61041=CARTESIAN_POINT('Ctrl Pts',(6.74401927496982,0.585436519324339,52.3302989765049));
#61042=CARTESIAN_POINT('Ctrl Pts',(6.72610706626208,0.764166664077337,52.3387375650618));
#61043=CARTESIAN_POINT('Ctrl Pts',(6.70114140146456,0.941803014211341,52.3471761536188));
#61044=CARTESIAN_POINT('Ctrl Pts',(6.67616264577572,1.11953250899722,52.3556191669986));
#61045=CARTESIAN_POINT('Ctrl Pts',(6.64412311152221,1.29616673850666,52.3640621803784));
#61046=CARTESIAN_POINT('Ctrl Pts',(6.60515420132416,1.47113118950344,52.3725051937583));
#61047=CARTESIAN_POINT('Ctrl Pts',(6.56614435156976,1.64627945285122,52.3809570771121));
#61048=CARTESIAN_POINT('Ctrl Pts',(6.52019066354873,1.81975411200359,52.389408960466));
#61049=CARTESIAN_POINT('Ctrl Pts',(6.46747470330079,1.99099471675952,52.3978608438199));
#61050=CARTESIAN_POINT('Ctrl Pts',(6.453107938696,2.03766319150115,52.4001642490512));
#61051=CARTESIAN_POINT('Ctrl Pts',(6.43823919613608,2.08416584121069,52.4024676542827));
#61052=CARTESIAN_POINT('Ctrl Pts',(6.4228727731184,2.13049157246264,52.404771059514));
#61053=CARTESIAN_POINT('Ctrl Pts',(6.36738086532369,2.29778510617565,52.4130892185655));
#61054=CARTESIAN_POINT('Ctrl Pts',(6.3052951123939,2.46307085402694,52.421407377617));
#61055=CARTESIAN_POINT('Ctrl Pts',(6.23678219864711,2.62580212632988,52.4297255366685));
#61056=CARTESIAN_POINT('Ctrl Pts',(6.16832901318762,2.78839153252826,52.4380364441033));
#61057=CARTESIAN_POINT('Ctrl Pts',(6.09345996602735,2.94843058148975,52.446347351538));
#61058=CARTESIAN_POINT('Ctrl Pts',(6.0123910045044,3.10538941341575,52.4546582589727));
#61059=CARTESIAN_POINT('Ctrl Pts',(5.93138455436805,3.26222721610888,52.4629627579579));
#61060=CARTESIAN_POINT('Ctrl Pts',(5.84418788003804,3.41598922888365,52.4712672569432));
#61061=CARTESIAN_POINT('Ctrl Pts',(5.75106434729964,3.56616711235171,52.4795717559284));
#61062=CARTESIAN_POINT('Ctrl Pts',(5.65798147319061,3.71627942671255,52.4878726290895));
#61063=CARTESIAN_POINT('Ctrl Pts',(5.55897707888453,3.86281043432944,52.4961735022507));
#61064=CARTESIAN_POINT('Ctrl Pts',(5.45435986044519,4.00527745765064,52.5044743754119));
#61065=CARTESIAN_POINT('Ctrl Pts',(5.34977095072652,4.14770593034672,52.5127730024122));
#61066=CARTESIAN_POINT('Ctrl Pts',(5.2395724489538,4.28607232998326,52.5210716294125));
#61067=CARTESIAN_POINT('Ctrl Pts',(5.12411577081687,4.41992381916994,52.5293702564128));
#61068=CARTESIAN_POINT('Ctrl Pts',(5.00867116985319,4.55376130702166,52.5376680153476));
#61069=CARTESIAN_POINT('Ctrl Pts',(4.8879697163121,4.68308456287043,52.5459657742825));
#61070=CARTESIAN_POINT('Ctrl Pts',(4.76240254220935,4.8074744956118,52.5542635332173));
#61071=CARTESIAN_POINT('Ctrl Pts',(4.6367879929511,4.93191135934806,52.5625644228081));
#61072=CARTESIAN_POINT('Ctrl Pts',(4.50630429949227,5.05141093309213,52.5708653123988));
#61073=CARTESIAN_POINT('Ctrl Pts',(4.37137935344313,5.16559111315357,52.5791662019896));
#61074=CARTESIAN_POINT('Ctrl Pts',(4.23643146787009,5.27979070577766,52.5874685028721));
#61075=CARTESIAN_POINT('Ctrl Pts',(4.09704109408353,5.38866888184995,52.5957708037545));
#61076=CARTESIAN_POINT('Ctrl Pts',(3.95366873319091,5.49188424388102,52.604073104637));
#61077=CARTESIAN_POINT('Ctrl Pts',(3.81017955451864,5.59518370433485,52.6123821701172));
#61078=CARTESIAN_POINT('Ctrl Pts',(3.66270219075019,5.69281093105934,52.6206912355975));
#61079=CARTESIAN_POINT('Ctrl Pts',(3.51172644757303,5.78446768142204,52.6290003010777));
#61080=CARTESIAN_POINT('Ctrl Pts',(3.37684927108676,5.86635105841143,52.6364233696292));
#61081=CARTESIAN_POINT('Ctrl Pts',(3.23918053584598,5.94346986229731,52.6438464381807));
#61082=CARTESIAN_POINT('Ctrl Pts',(3.09908550384727,6.01564277861009,52.6512695067322));
#61083=CARTESIAN_POINT('Origin',(0.,0.,-63.6971797838103));
#61084=CARTESIAN_POINT('',(3.09908550384712,6.01564277861017,55.0459286315074));
#61085=CARTESIAN_POINT('',(3.09908550384732,6.01564277861007,54.6514561368909));
#61086=CARTESIAN_POINT('',(3.09908550384721,6.01564277861012,-63.6971797838103));
#61087=CARTESIAN_POINT('',(-6.76699920371004,0.00328283226919929,53.6971797837668));
#61088=CARTESIAN_POINT('Ctrl Pts',(-6.76699920371048,0.00328283135813808,
53.6971797838098));
#61089=CARTESIAN_POINT('Ctrl Pts',(-6.76708603743267,-0.175710136846427,
53.7056136196247));
#61090=CARTESIAN_POINT('Ctrl Pts',(-6.76006682462507,-0.35484151860626,
53.7140474554396));
#61091=CARTESIAN_POINT('Ctrl Pts',(-6.7459351913362,-0.533523564889031,
53.7224812912544));
#61092=CARTESIAN_POINT('Ctrl Pts',(-6.73181716702949,-0.712033537588325,
53.7309070051545));
#61093=CARTESIAN_POINT('Ctrl Pts',(-6.71060041001333,-0.890094707423162,
53.7393327190547));
#61094=CARTESIAN_POINT('Ctrl Pts',(-6.68233058255984,-1.06712088602251,
53.7477584329548));
#61095=CARTESIAN_POINT('Ctrl Pts',(-6.65407696605256,-1.24404555137908,
53.7561793152444));
#61096=CARTESIAN_POINT('Ctrl Pts',(-6.61877839217973,-1.41993608078952,
53.764600197534));
#61097=CARTESIAN_POINT('Ctrl Pts',(-6.57653226760037,-1.59421213557394,
53.7730210798236));
#61098=CARTESIAN_POINT('Ctrl Pts',(-6.53430748982804,-1.76840012932673,
53.7814377070733));
#61099=CARTESIAN_POINT('Ctrl Pts',(-6.4851422404297,-1.94097495261594,53.7898543343229));
#61100=CARTESIAN_POINT('Ctrl Pts',(-6.42918491865352,-2.1113669225784,53.7982709615725));
#61101=CARTESIAN_POINT('Ctrl Pts',(-6.40715469026425,-2.17844972595102,
53.801584562272));
#61102=CARTESIAN_POINT('Ctrl Pts',(-6.38407226218484,-2.24519432628294,
53.8048981629714));
#61103=CARTESIAN_POINT('Ctrl Pts',(-6.35994882873542,-2.3115665458444,53.8082117636709));
#61104=CARTESIAN_POINT('Ctrl Pts',(-6.29860800963492,-2.48033714485365,
53.8166375535363));
#61105=CARTESIAN_POINT('Ctrl Pts',(-6.23055026012783,-2.64665081014075,
53.8250633434016));
#61106=CARTESIAN_POINT('Ctrl Pts',(-6.15600474122764,-2.80996345634296,
53.833489133267));
#61107=CARTESIAN_POINT('Ctrl Pts',(-6.08144192525173,-2.97331399658961,
53.8419168781999));
#61108=CARTESIAN_POINT('Ctrl Pts',(-6.00038847602705,-3.13366182778156,
53.8503446231329));
#61109=CARTESIAN_POINT('Ctrl Pts',(-5.9131205754788,-3.29048538362492,53.8587723680658));
#61110=CARTESIAN_POINT('Ctrl Pts',(-5.82582060834682,-3.44736656427252,
53.867203209773));
#61111=CARTESIAN_POINT('Ctrl Pts',(-5.73230179791808,-3.60072059793408,
53.8756340514802));
#61112=CARTESIAN_POINT('Ctrl Pts',(-5.63288509655736,-3.75005259816206,
53.8840648931874));
#61113=CARTESIAN_POINT('Ctrl Pts',(-5.53337704392559,-3.89952181545561,
53.892503481763));
#61114=CARTESIAN_POINT('Ctrl Pts',(-5.42796045673013,-4.04496133944536,
53.9009420703386));
#61115=CARTESIAN_POINT('Ctrl Pts',(-5.31699889383973,-4.18590632514717,
53.9093806589143));
#61116=CARTESIAN_POINT('Ctrl Pts',(-5.20597914760166,-4.32692521618063,
53.9178236723134));
#61117=CARTESIAN_POINT('Ctrl Pts',(-5.08940883785281,-4.46344461334333,
53.9262666857126));
#61118=CARTESIAN_POINT('Ctrl Pts',(-4.96769061499627,-4.59503416240598,
53.9347096991117));
#61119=CARTESIAN_POINT('Ctrl Pts',(-4.84584451865206,-4.72676195547338,
53.9431615824857));
#61120=CARTESIAN_POINT('Ctrl Pts',(-4.71883993640617,-4.85354931693117,
53.9516134658596));
#61121=CARTESIAN_POINT('Ctrl Pts',(-4.58711579176472,-4.97500328773185,
53.9600653492335));
#61122=CARTESIAN_POINT('Ctrl Pts',(-4.55121680260995,-5.00810333019139,
53.9623687543565));
#61123=CARTESIAN_POINT('Ctrl Pts',(-4.51496746341224,-5.0408074754383,53.9646721594794));
#61124=CARTESIAN_POINT('Ctrl Pts',(-4.47837707016986,-5.07310829939366,
53.9669755646023));
#61125=CARTESIAN_POINT('Ctrl Pts',(-4.34625441333081,-5.18974193737625,
53.9752928298091));
#61126=CARTESIAN_POINT('Ctrl Pts',(-4.20944489272645,-5.30132355843371,
53.9836100950158));
#61127=CARTESIAN_POINT('Ctrl Pts',(-4.06836751014018,-5.4074647296525,53.9919273602225));
#61128=CARTESIAN_POINT('Ctrl Pts',(-3.92740911549309,-5.51351637894372,
54.0002376104548));
#61129=CARTESIAN_POINT('Ctrl Pts',(-3.78219030721473,-5.61413651256725,
54.008547860687));
#61130=CARTESIAN_POINT('Ctrl Pts',(-3.63316421449497,-5.70897598440501,
54.0168581109192));
#61131=CARTESIAN_POINT('Ctrl Pts',(-3.48423652142652,-5.80375283518905,
54.0251628740202));
#61132=CARTESIAN_POINT('Ctrl Pts',(-3.33150684562223,-5.8927564436729,54.0334676371213));
#61133=CARTESIAN_POINT('Ctrl Pts',(-3.17545861822658,-5.97568000849532,
54.0417724002223));
#61134=CARTESIAN_POINT('Ctrl Pts',(-3.01948486146417,-6.05856399984429,
54.0500732000551));
#61135=CARTESIAN_POINT('Ctrl Pts',(-2.86019601580814,-6.13537356719643,
54.058373999888));
#61136=CARTESIAN_POINT('Ctrl Pts',(-2.69810171373961,-6.2058469319115,54.0666747997209));
#61137=CARTESIAN_POINT('Ctrl Pts',(-2.53605510534114,-6.27629956095998,
54.0749731571754));
#61138=CARTESIAN_POINT('Ctrl Pts',(-2.37120500452698,-6.34041956500934,
54.0832715146299));
#61139=CARTESIAN_POINT('Ctrl Pts',(-2.20408290716049,-6.39799246157441,
54.0915698720845));
#61140=CARTESIAN_POINT('Ctrl Pts',(-2.03694380551152,-6.45557121604703,
54.0998690738775));
#61141=CARTESIAN_POINT('Ctrl Pts',(-1.86753257180285,-6.50660141160177,
54.1081682756705));
#61142=CARTESIAN_POINT('Ctrl Pts',(-1.69639838236628,-6.55091760964104,
54.1164674774635));
#61143=CARTESIAN_POINT('Ctrl Pts',(-1.52524684317089,-6.5952383005017,54.124767520638));
#61144=CARTESIAN_POINT('Ctrl Pts',(-1.35237233685554,-6.63284354936003,
54.1330675638126));
#61145=CARTESIAN_POINT('Ctrl Pts',(-1.17833673677863,-6.6636185015919,54.1413676069872));
#61146=CARTESIAN_POINT('Ctrl Pts',(-1.00425460250013,-6.69440168253003,
54.1496698694541));
#61147=CARTESIAN_POINT('Ctrl Pts',(-0.829011098310984,-6.71835086624514,
54.1579721319211));
#61148=CARTESIAN_POINT('Ctrl Pts',(-0.653175958323883,-6.73540274723551,
54.166274394388));
#61149=CARTESIAN_POINT('Ctrl Pts',(-0.477264610449473,-6.75246201860204,
54.1745802550998));
#61150=CARTESIAN_POINT('Ctrl Pts',(-0.300761461791976,-6.76261799591101,
54.1828861158115));
#61151=CARTESIAN_POINT('Ctrl Pts',(-0.12423920052669,-6.76585941481587,
54.1911919765233));
#61152=CARTESIAN_POINT('Ctrl Pts',(0.0524917225304711,-6.76910466530701,
54.1995076553496));
#61153=CARTESIAN_POINT('Ctrl Pts',(0.229241455126148,-6.76541902060758,
54.2078233341759));
#61154=CARTESIAN_POINT('Ctrl Pts',(0.405438289691852,-6.75484335815804,
54.2161390130022));
#61155=CARTESIAN_POINT('Ctrl Pts',(0.581746567362717,-6.74426100668559,
54.2244599514297));
#61156=CARTESIAN_POINT('Ctrl Pts',(0.757500903913943,-6.72677998111688,
54.2327808898571));
#61157=CARTESIAN_POINT('Ctrl Pts',(0.932136719472763,-6.70249283000068,
54.2411018282845));
#61158=CARTESIAN_POINT('Ctrl Pts',(1.10703209799069,-6.6781695806489,54.2494351342059));
#61159=CARTESIAN_POINT('Ctrl Pts',(1.28080529089778,-6.6470200506663,54.2577684401274));
#61160=CARTESIAN_POINT('Ctrl Pts',(1.45290255069757,-6.60918778505926,54.2661017460488));
#61161=CARTESIAN_POINT('Ctrl Pts',(1.57957632858622,-6.58134099646945,54.2722355528544));
#61162=CARTESIAN_POINT('Ctrl Pts',(1.7053423704799,-6.54987467526457,54.2783693596598));
#61163=CARTESIAN_POINT('Ctrl Pts',(1.82998604543604,-6.51486301264343,54.2845031664653));
#61164=CARTESIAN_POINT('Ctrl Pts',(1.99400337844069,-6.46879152502724,54.2925745799066));
#61165=CARTESIAN_POINT('Ctrl Pts',(2.15658146711973,-6.41643724252702,54.3006459933478));
#61166=CARTESIAN_POINT('Ctrl Pts',(2.31719014143117,-6.35790207918101,54.308717406789));
#61167=CARTESIAN_POINT('Ctrl Pts',(2.47759718485303,-6.29944040188491,54.3167786872391));
#61168=CARTESIAN_POINT('Ctrl Pts',(2.63603938745271,-6.23481340941637,54.3248399676892));
#61169=CARTESIAN_POINT('Ctrl Pts',(2.79199755016757,-6.16417380350833,54.3329012481394));
#61170=CARTESIAN_POINT('Ctrl Pts',(2.94779412266858,-6.09360738818438,54.3409541761954));
#61171=CARTESIAN_POINT('Ctrl Pts',(3.10111144025382,-6.01704090937111,54.3490071042514));
#61172=CARTESIAN_POINT('Ctrl Pts',(3.25144633841069,-5.93467654623533,54.3570600323075));
#61173=CARTESIAN_POINT('Ctrl Pts',(3.40165839257871,-5.85237948594827,54.3651063800298));
#61174=CARTESIAN_POINT('Ctrl Pts',(3.54889255243549,-5.76429414918577,54.3731527277521));
#61175=CARTESIAN_POINT('Ctrl Pts',(3.69266659323872,-5.67067036876406,54.3811990754744));
#61176=CARTESIAN_POINT('Ctrl Pts',(3.83635460148843,-5.57710261161927,54.3892406083648));
#61177=CARTESIAN_POINT('Ctrl Pts',(3.97658630068248,-5.47800321130974,54.3972821412551));
#61178=CARTESIAN_POINT('Ctrl Pts',(4.11290509995189,-5.3736673360741,54.4053236741455));
#61179=CARTESIAN_POINT('Ctrl Pts',(4.25184458684422,-5.26732563524198,54.4135198030698));
#61180=CARTESIAN_POINT('Ctrl Pts',(4.38671884754325,-5.15554426260775,54.4217159319941));
#61181=CARTESIAN_POINT('Ctrl Pts',(4.51707610318979,-5.03868162101871,54.4299120609184));
#61182=CARTESIAN_POINT('Ctrl Pts',(4.64493040063383,-4.92406283080473,54.4379508179494));
#61183=CARTESIAN_POINT('Ctrl Pts',(4.7684393074851,-4.80455640640591,54.4459895749804));
#61184=CARTESIAN_POINT('Ctrl Pts',(4.88721097112896,-4.68054034526749,54.4540283320115));
#61185=CARTESIAN_POINT('Ctrl Pts',(5.00599413059985,-4.55651228070045,54.4620678671082));
#61186=CARTESIAN_POINT('Ctrl Pts',(5.12003887546847,-4.42797397994076,54.470107402205));
#61187=CARTESIAN_POINT('Ctrl Pts',(5.22899137774639,-4.29533912182192,54.4781469373018));
#61188=CARTESIAN_POINT('Ctrl Pts',(5.33797599809285,-4.16266516432148,54.4861888423701));
#61189=CARTESIAN_POINT('Ctrl Pts',(5.44186515093747,-4.02589253415222,54.4942307474385));
#61190=CARTESIAN_POINT('Ctrl Pts',(5.54034643447907,-3.88546655962383,54.5022726525069));
#61191=CARTESIAN_POINT('Ctrl Pts',(5.64214970959698,-3.74030370629267,54.5105858288254));
#61192=CARTESIAN_POINT('Ctrl Pts',(5.73817364412583,-3.59123708396416,54.5188990051438));
#61193=CARTESIAN_POINT('Ctrl Pts',(5.8281234671109,-3.43878842793669,54.5272121814623));
#61194=CARTESIAN_POINT('Ctrl Pts',(5.91528917306922,-3.29105834594156,54.5352680492618));
#61195=CARTESIAN_POINT('Ctrl Pts',(5.99675106521978,-3.14015283067604,54.5433239170613));
#61196=CARTESIAN_POINT('Ctrl Pts',(6.07228927373558,-2.98656859557516,54.5513797848608));
#61197=CARTESIAN_POINT('Ctrl Pts',(6.15144657550925,-2.82562602247965,54.5598216154387));
#61198=CARTESIAN_POINT('Ctrl Pts',(6.22409841601709,-2.66174218003829,54.5682634460166));
#61199=CARTESIAN_POINT('Ctrl Pts',(6.29005010226811,-2.4955077060504,54.5767052765946));
#61200=CARTESIAN_POINT('Ctrl Pts',(6.35600178851914,-2.32927323206251,54.5851471071725));
#61201=CARTESIAN_POINT('Ctrl Pts',(6.41525324836093,-2.1606885899224,54.5935889377505));
#61202=CARTESIAN_POINT('Ctrl Pts',(6.46767094968941,-1.99035712537818,54.6020307683284));
#61203=CARTESIAN_POINT('Ctrl Pts',(6.51877616789689,-1.82429057834318,54.6102612245068));
#61204=CARTESIAN_POINT('Ctrl Pts',(6.5635560881325,-1.6560114131142,54.6184916806853));
#61205=CARTESIAN_POINT('Ctrl Pts',(6.60181548125312,-1.48604217688688,54.6267221368637));
#61206=CARTESIAN_POINT('Ctrl Pts',(6.64002945822782,-1.31627470412216,54.6349428230074));
#61207=CARTESIAN_POINT('Ctrl Pts',(6.67173824269077,-1.14482150151238,54.643163509151));
#61208=CARTESIAN_POINT('Ctrl Pts',(6.69679574766902,-0.972222049740749,
54.6513841952947));
#61209=CARTESIAN_POINT('Ctrl Pts',(6.72182853522794,-0.799792854865408,
54.6595967723251));
#61210=CARTESIAN_POINT('Ctrl Pts',(6.74022305831992,-0.626220014951361,
54.6678093493556));
#61211=CARTESIAN_POINT('Ctrl Pts',(6.75188382348002,-0.452055122998117,
54.676021926386));
#61212=CARTESIAN_POINT('Ctrl Pts',(6.76353542480675,-0.278027101827061,
54.684228049407));
#61213=CARTESIAN_POINT('Ctrl Pts',(6.7684637845503,-0.103408311454082,54.692434172428));
#61214=CARTESIAN_POINT('Ctrl Pts',(6.76662497176018,0.0712424841759877,
54.7006402954491));
#61215=CARTESIAN_POINT('Ctrl Pts',(6.76478723534056,0.245791045927125,54.7088416149204));
#61216=CARTESIAN_POINT('Ctrl Pts',(6.75619022140809,0.420371218071724,54.7170429343917));
#61217=CARTESIAN_POINT('Ctrl Pts',(6.74084203881244,0.594422078811799,54.725244253863));
#61218=CARTESIAN_POINT('Ctrl Pts',(6.72549825924385,0.768423008516526,54.7334432205716));
#61219=CARTESIAN_POINT('Ctrl Pts',(6.70340719629511,0.941894572244566,54.7416421872802));
#61220=CARTESIAN_POINT('Ctrl Pts',(6.67462899987217,1.11427856214928,54.7498411539888));
#61221=CARTESIAN_POINT('Ctrl Pts',(6.64585460373696,1.28663978798802,54.7580390379876));
#61222=CARTESIAN_POINT('Ctrl Pts',(6.61039489109573,1.45791337229763,54.7662369219865));
#61223=CARTESIAN_POINT('Ctrl Pts',(6.56836155679014,1.62754891148666,54.7744348059854));
#61224=CARTESIAN_POINT('Ctrl Pts',(6.52632613769632,1.7971928643355,54.7826330965866));
#61225=CARTESIAN_POINT('Ctrl Pts',(6.47771653360083,1.96519826208167,54.7908313871879));
#61226=CARTESIAN_POINT('Ctrl Pts',(6.42269498685902,2.13102747654177,54.7990296777891));
#61227=CARTESIAN_POINT('Ctrl Pts',(6.36766071633917,2.29689503914444,54.8072298642518));
#61228=CARTESIAN_POINT('Ctrl Pts',(6.30621166284734,2.46058507585072,54.8154300507144));
#61229=CARTESIAN_POINT('Ctrl Pts',(6.23855912760033,2.62157758066295,54.8236302371771));
#61230=CARTESIAN_POINT('Ctrl Pts',(6.17084263218773,2.78272229126066,54.8318381762729));
#61231=CARTESIAN_POINT('Ctrl Pts',(6.09691107670023,2.94116404370452,54.8400461153687));
#61232=CARTESIAN_POINT('Ctrl Pts',(6.01702328136955,3.09640433914191,54.8482540544645));
#61233=CARTESIAN_POINT('Ctrl Pts',(5.9370967300461,3.25171994635556,54.8564659754805));
#61234=CARTESIAN_POINT('Ctrl Pts',(5.85120835399626,3.40383068791653,54.8646778964966));
#61235=CARTESIAN_POINT('Ctrl Pts',(5.75966163813225,3.55226502589936,54.8728898175126));
#61236=CARTESIAN_POINT('Ctrl Pts',(5.66798938045788,3.70090291804941,54.8811129998766));
#61237=CARTESIAN_POINT('Ctrl Pts',(5.57064347575273,3.84585403334481,54.8893361822407));
#61238=CARTESIAN_POINT('Ctrl Pts',(5.46796992541074,3.98667704922328,54.8975593646048));
#61239=CARTESIAN_POINT('Ctrl Pts',(5.37641104923287,4.1122556138182,54.904892366467));
#61240=CARTESIAN_POINT('Ctrl Pts',(5.28061624399103,4.23455177911574,54.9122253683293));
#61241=CARTESIAN_POINT('Ctrl Pts',(5.18085617329314,4.35327673272104,54.9195583701915));
#61242=CARTESIAN_POINT('Ctrl Pts',(5.05927297191148,4.4979735021022,54.9284955114336));
#61243=CARTESIAN_POINT('Ctrl Pts',(4.93154733487648,4.63766584221061,54.9374326526757));
#61244=CARTESIAN_POINT('Ctrl Pts',(4.79809671928477,4.7718504662645,54.9463697939178));
#61245=CARTESIAN_POINT('Ctrl Pts',(4.66494098883499,4.90573858324173,54.9552871868047));
#61246=CARTESIAN_POINT('Ctrl Pts',(4.52608571207779,5.03414309339944,54.9642045796915));
#61247=CARTESIAN_POINT('Ctrl Pts',(4.38198602301382,5.15659650293791,54.9731219725784));
#61248=CARTESIAN_POINT('Ctrl Pts',(4.23809251033577,5.27887470736952,54.9820266065492));
#61249=CARTESIAN_POINT('Ctrl Pts',(4.08896975004594,5.39521863024622,54.99093124052));
#61250=CARTESIAN_POINT('Ctrl Pts',(3.93510884940687,5.50519821108376,54.9998358744908));
#61251=CARTESIAN_POINT('Ctrl Pts',(3.78160036162273,5.61492588764992,55.008720112718));
#61252=CARTESIAN_POINT('Ctrl Pts',(3.6233756001165,5.71831816228657,55.0176043509451));
#61253=CARTESIAN_POINT('Ctrl Pts',(3.46095742154545,5.81498604695226,55.0264885891723));
#61254=CARTESIAN_POINT('Ctrl Pts',(3.34249233064842,5.88549397805022,55.032968603284));
#61255=CARTESIAN_POINT('Ctrl Pts',(3.22179708303814,5.95242531536962,55.0394486173957));
#61256=CARTESIAN_POINT('Ctrl Pts',(3.09908550384712,6.01564277861017,55.0459286315074));
#61257=CARTESIAN_POINT('Ctrl Pts',(3.09908550384738,6.01564277861003,53.0457619208681));
#61258=CARTESIAN_POINT('Ctrl Pts',(2.94005757428153,6.09756937720674,53.0542010555753));
#61259=CARTESIAN_POINT('Ctrl Pts',(2.77766693021921,6.17324381468496,53.0626401902825));
#61260=CARTESIAN_POINT('Ctrl Pts',(2.61243358892099,6.24239375107638,53.0710793249896));
#61261=CARTESIAN_POINT('Ctrl Pts',(2.44731973230398,6.31149368328559,53.0795123571311));
#61262=CARTESIAN_POINT('Ctrl Pts',(2.27936758307977,6.37407839180963,53.0879453892726));
#61263=CARTESIAN_POINT('Ctrl Pts',(2.10911964718684,6.42992249672191,53.096378421414));
#61264=CARTESIAN_POINT('Ctrl Pts',(1.93896868511028,6.48573479263782,53.1048066500711));
#61265=CARTESIAN_POINT('Ctrl Pts',(1.7665248597525,6.53481403638633,53.1132348787281));
#61266=CARTESIAN_POINT('Ctrl Pts',(1.59234882218039,6.57698367251286,53.1216631073851));
#61267=CARTESIAN_POINT('Ctrl Pts',(1.41130160981969,6.62081688386268,53.1304238262806));
#61268=CARTESIAN_POINT('Ctrl Pts',(1.22838308135514,6.65718409709552,53.1391845451761));
#61269=CARTESIAN_POINT('Ctrl Pts',(1.04423928235286,6.68594445992421,53.1479452640715));
#61270=CARTESIAN_POINT('Ctrl Pts',(0.867189729917508,6.71359681310844,53.1563684711947));
#61271=CARTESIAN_POINT('Ctrl Pts',(0.689007907804055,6.73421742414931,53.164791678318));
#61272=CARTESIAN_POINT('Ctrl Pts',(0.510277575700802,6.74773338208742,53.1732148854412));
#61273=CARTESIAN_POINT('Ctrl Pts',(0.331560321883366,6.76124835101846,53.1816374762107));
#61274=CARTESIAN_POINT('Ctrl Pts',(0.152294970515892,6.7676596782313,53.1900600669802));
#61275=CARTESIAN_POINT('Ctrl Pts',(-0.0269305010389215,6.76694641238674,
53.1984826577496));
#61276=CARTESIAN_POINT('Ctrl Pts',(-0.206167850202632,6.76623309927272,
53.2069058067));
#61277=CARTESIAN_POINT('Ctrl Pts',(-0.385364980889819,6.75839425355299,
53.2153289556504));
#61278=CARTESIAN_POINT('Ctrl Pts',(-0.563934447482844,6.74346105045045,
53.2237521046008));
#61279=CARTESIAN_POINT('Ctrl Pts',(-0.742540651901937,6.72852477507901,
53.2321769864801));
#61280=CARTESIAN_POINT('Ctrl Pts',(-0.920518602661822,6.70649126080709,
53.2406018683593));
#61281=CARTESIAN_POINT('Ctrl Pts',(-1.09728612991938,6.67744353394969,53.2490267502386));
#61282=CARTESIAN_POINT('Ctrl Pts',(-1.27417574263058,6.64837574512183,53.2574574508083));
#61283=CARTESIAN_POINT('Ctrl Pts',(-1.44985293240845,6.61228411930036,53.265888151378));
#61284=CARTESIAN_POINT('Ctrl Pts',(-1.62374491164964,6.56930296621277,53.2743188519477));
#61285=CARTESIAN_POINT('Ctrl Pts',(-1.79770522804939,6.52630492212258,53.2827528656669));
#61286=CARTESIAN_POINT('Ctrl Pts',(-1.96987861305709,6.47641203825159,53.2911868793861));
#61287=CARTESIAN_POINT('Ctrl Pts',(-2.13970703579232,6.41980862650756,53.2996208931053));
#61288=CARTESIAN_POINT('Ctrl Pts',(-2.30968337277309,6.36315591529523,53.3080622525371));
#61289=CARTESIAN_POINT('Ctrl Pts',(-2.47731035402599,6.29978111381898,53.3165036119689));
#61290=CARTESIAN_POINT('Ctrl Pts',(-2.64204863773189,6.22991717407696,53.3249449714006));
#61291=CARTESIAN_POINT('Ctrl Pts',(-2.68742496602256,6.2106735046997,53.3272701012258));
#61292=CARTESIAN_POINT('Ctrl Pts',(-2.73258226158266,6.19093777935084,53.329595231051));
#61293=CARTESIAN_POINT('Ctrl Pts',(-2.77750956863203,6.17071548494642,53.3319203608762));
#61294=CARTESIAN_POINT('Ctrl Pts',(-2.93482108857445,6.09990777181137,53.34006172814));
#61295=CARTESIAN_POINT('Ctrl Pts',(-3.08962364653538,6.02299031381432,53.3482030954038));
#61296=CARTESIAN_POINT('Ctrl Pts',(-3.24140575636373,5.94016647263459,53.3563444626677));
#61297=CARTESIAN_POINT('Ctrl Pts',(-3.39305537194837,5.85741493037211,53.3644787231368));
#61298=CARTESIAN_POINT('Ctrl Pts',(-3.54168946849646,5.76876744180524,53.3726129836059));
#61299=CARTESIAN_POINT('Ctrl Pts',(-3.68681717397462,5.67447514098756,53.380747244075));
#61300=CARTESIAN_POINT('Ctrl Pts',(-3.83184587856846,5.58024716297534,53.3888759556451));
#61301=CARTESIAN_POINT('Ctrl Pts',(-3.97337264865834,5.48038223792717,53.3970046672151));
#61302=CARTESIAN_POINT('Ctrl Pts',(-4.1109318811139,5.37517702674445,53.4051333787852));
#61303=CARTESIAN_POINT('Ctrl Pts',(-4.24842551410248,5.27002198599127,53.4132582139224));
#61304=CARTESIAN_POINT('Ctrl Pts',(-4.38195508703994,5.15953195235009,53.4213830490595));
#61305=CARTESIAN_POINT('Ctrl Pts',(-4.51108464955587,5.0440464197449,53.4295078841966));
#61306=CARTESIAN_POINT('Ctrl Pts',(-4.64017806188347,4.92859321764308,53.437630444763));
#61307=CARTESIAN_POINT('Ctrl Pts',(-4.76487364522968,4.80814754655193,53.4457530053294));
#61308=CARTESIAN_POINT('Ctrl Pts',(-4.88476920195721,4.68308860087126,53.4538755658958));
#61309=CARTESIAN_POINT('Ctrl Pts',(-5.00467113081215,4.55802300864289,53.4619985581546));
#61310=CARTESIAN_POINT('Ctrl Pts',(-5.11977226725638,4.42834391355026,53.4701215504132));
#61311=CARTESIAN_POINT('Ctrl Pts',(-5.2297077808273,4.29446685016364,53.4782445426719));
#61312=CARTESIAN_POINT('Ctrl Pts',(-5.28582650632384,4.22612669395352,53.4823910823839));
#61313=CARTESIAN_POINT('Ctrl Pts',(-5.34059980372301,4.15669319334044,53.4865376220959));
#61314=CARTESIAN_POINT('Ctrl Pts',(-5.39398321700727,4.08622491483814,53.4906841618079));
#61315=CARTESIAN_POINT('Ctrl Pts',(-5.50964070727787,3.93355231985311,53.4996678207178));
#61316=CARTESIAN_POINT('Ctrl Pts',(-5.61871462356346,3.77609639131443,53.5086514796278));
#61317=CARTESIAN_POINT('Ctrl Pts',(-5.72085559517629,3.61442945139896,53.5176351385377));
#61318=CARTESIAN_POINT('Ctrl Pts',(-5.82317204386379,3.45248476944483,53.5266342312756));
#61319=CARTESIAN_POINT('Ctrl Pts',(-5.9185316139385,3.28631481864143,53.5356333240135));
#61320=CARTESIAN_POINT('Ctrl Pts',(-6.00663036087874,3.11651740052414,53.5446324167514));
#61321=CARTESIAN_POINT('Ctrl Pts',(-6.09493567474315,2.94632185494635,53.5536526098451));
#61322=CARTESIAN_POINT('Ctrl Pts',(-6.17594599168649,2.77248203739202,53.5626728029389));
#61323=CARTESIAN_POINT('Ctrl Pts',(-6.2494039712688,2.59561919469897,53.5716929960326));
#61324=CARTESIAN_POINT('Ctrl Pts',(-6.3229363454474,2.41857723409586,53.5807223243302));
#61325=CARTESIAN_POINT('Ctrl Pts',(-6.3889010161122,2.23850635506613,53.5897516526279));
#61326=CARTESIAN_POINT('Ctrl Pts',(-6.44708972823528,2.05604548492565,53.5987809809255));
#61327=CARTESIAN_POINT('Ctrl Pts',(-6.50536047472599,1.8733273816973,53.607823038758));
#61328=CARTESIAN_POINT('Ctrl Pts',(-6.55583327026295,1.68821277814971,53.6168650965905));
#61329=CARTESIAN_POINT('Ctrl Pts',(-6.59834981517535,1.50135562628429,53.6259071544229));
#61330=CARTESIAN_POINT('Ctrl Pts',(-6.63524679344428,1.33919606496578,53.6337540905284));
#61331=CARTESIAN_POINT('Ctrl Pts',(-6.66615251845092,1.17572443489703,53.6416010266338));
#61332=CARTESIAN_POINT('Ctrl Pts',(-6.69099487965077,1.01137358107042,53.6494479627392));
#61333=CARTESIAN_POINT('Ctrl Pts',(-6.72167052148441,0.80843120025239,53.6591374523785));
#61334=CARTESIAN_POINT('Ctrl Pts',(-6.74311813259488,0.604030993469634,
53.6688269420178));
#61335=CARTESIAN_POINT('Ctrl Pts',(-6.7552299124238,0.398945898957237,53.6785164316571));
#61336=CARTESIAN_POINT('Ctrl Pts',(-6.76300625634691,0.267271425761757,
53.6847375490271));
#61337=CARTESIAN_POINT('Ctrl Pts',(-6.76693515184334,0.13531483858658,53.690958666397));
#61338=CARTESIAN_POINT('Ctrl Pts',(-6.76699920371004,0.00328283226939312,
53.6971797837669));
#61339=CARTESIAN_POINT('',(-6.76699774277413,-0.00552714119481092,53.3028202162163));
#61340=CARTESIAN_POINT('Ctrl Pts',(3.09908550384727,6.01564277861009,52.6512695067322));
#61341=CARTESIAN_POINT('Ctrl Pts',(2.94205676261785,6.09653945308715,52.6595898239773));
#61342=CARTESIAN_POINT('Ctrl Pts',(2.78197968006646,6.17122140541269,52.6679101412225));
#61343=CARTESIAN_POINT('Ctrl Pts',(2.61938682177641,6.23947927938735,52.6762304584677));
#61344=CARTESIAN_POINT('Ctrl Pts',(2.45654726276985,6.30784072043497,52.6845634000571));
#61345=CARTESIAN_POINT('Ctrl Pts',(2.2911846245389,6.36975847955866,52.6928963416466));
#61346=CARTESIAN_POINT('Ctrl Pts',(2.12384835750788,6.42507254078202,52.7012292832361));
#61347=CARTESIAN_POINT('Ctrl Pts',(1.98281488415703,6.47169204722784,52.7082524092831));
#61348=CARTESIAN_POINT('Ctrl Pts',(1.84037982600834,6.51362155783438,52.7152755353301));
#61349=CARTESIAN_POINT('Ctrl Pts',(1.6968774011468,6.55079354624135,52.7222986613771));
#61350=CARTESIAN_POINT('Ctrl Pts',(1.53195548964767,6.59351390715661,52.7303700746197));
#61351=CARTESIAN_POINT('Ctrl Pts',(1.3651158112376,6.63008064296225,52.7384414878622));
#61352=CARTESIAN_POINT('Ctrl Pts',(1.19686780559995,6.66031504179182,52.7465129011048));
#61353=CARTESIAN_POINT('Ctrl Pts',(1.02883102139834,6.6905114838378,52.7545741813566));
#61354=CARTESIAN_POINT('Ctrl Pts',(0.859389790336993,6.71439134169229,52.7626354616083));
#61355=CARTESIAN_POINT('Ctrl Pts',(0.68906962780824,6.73182531324397,52.7706967418601));
#61356=CARTESIAN_POINT('Ctrl Pts',(0.51892593613637,6.74924122123902,52.7787496697183));
#61357=CARTESIAN_POINT('Ctrl Pts',(0.347905493140503,6.7602244960111,52.7868025975764));
#61358=CARTESIAN_POINT('Ctrl Pts',(0.176544854816426,6.7646966609182,52.7948555254346));
#61359=CARTESIAN_POINT('Ctrl Pts',(0.00532424135297324,6.76916517146061,
52.8029018729596));
#61360=CARTESIAN_POINT('Ctrl Pts',(-0.166235643212382,6.7671331519865,52.8109482204846));
#61361=CARTESIAN_POINT('Ctrl Pts',(-0.337592358950583,6.75857384358403,
52.8189945680095));
#61362=CARTESIAN_POINT('Ctrl Pts',(-0.508846537024973,6.75001965696207,
52.8270361007032));
#61363=CARTESIAN_POINT('Ctrl Pts',(-0.679897416728472,6.73494597538439,
52.8350776333968));
#61364=CARTESIAN_POINT('Ctrl Pts',(-0.850201897232936,6.71337811641364,
52.8431191660905));
#61365=CARTESIAN_POINT('Ctrl Pts',(-1.02378043665129,6.69139562101812,52.8513152951384));
#61366=CARTESIAN_POINT('Ctrl Pts',(-1.19658319035935,6.66266670040916,52.8595114241863));
#61367=CARTESIAN_POINT('Ctrl Pts',(-1.36803939605063,6.62727373894073,52.8677075532342));
#61368=CARTESIAN_POINT('Ctrl Pts',(-1.53620350591642,6.59256035054598,52.8757463100708));
#61369=CARTESIAN_POINT('Ctrl Pts',(-1.70307193424474,6.55143661169157,52.8837850669075));
#61370=CARTESIAN_POINT('Ctrl Pts',(-1.86811584513093,6.50403199478376,52.8918238237441));
#61371=CARTESIAN_POINT('Ctrl Pts',(-2.03317573052384,6.45662278960991,52.8998633586475));
#61372=CARTESIAN_POINT('Ctrl Pts',(-2.19641038783759,6.40293159890401,52.9079028935508));
#61373=CARTESIAN_POINT('Ctrl Pts',(-2.35730588590162,6.34313786388831,52.9159424284542));
#61374=CARTESIAN_POINT('Ctrl Pts',(-2.51824881431329,6.28332650229093,52.9239843333303));
#61375=CARTESIAN_POINT('Ctrl Pts',(-2.67685086103619,6.21740914561525,52.9320262382063));
#61376=CARTESIAN_POINT('Ctrl Pts',(-2.83261796802381,6.14561343132064,52.9400681430824));
#61377=CARTESIAN_POINT('Ctrl Pts',(-2.99363945500359,6.0713958837391,52.9483813197622));
#61378=CARTESIAN_POINT('Ctrl Pts',(-3.15163100226007,5.99089664338606,52.956694496442));
#61379=CARTESIAN_POINT('Ctrl Pts',(-3.30607533949969,5.9044182481894,52.9650076731218));
#61380=CARTESIAN_POINT('Ctrl Pts',(-3.45573932259533,5.82061652837128,52.9730635407329));
#61381=CARTESIAN_POINT('Ctrl Pts',(-3.60207213402685,5.73120052677407,52.9811194083439));
#61382=CARTESIAN_POINT('Ctrl Pts',(-3.74463382187001,5.63648884857473,52.9891752759549));
#61383=CARTESIAN_POINT('Ctrl Pts',(-3.89402576380447,5.53723945174072,52.9976171071691));
#61384=CARTESIAN_POINT('Ctrl Pts',(-4.03927594287096,5.43217473828971,53.0060589383833));
#61385=CARTESIAN_POINT('Ctrl Pts',(-4.17991890109239,5.32170714905383,53.0145007695975));
#61386=CARTESIAN_POINT('Ctrl Pts',(-4.32056185931392,5.21123955981787,53.0229426008117));
#61387=CARTESIAN_POINT('Ctrl Pts',(-4.45659730115733,5.09536945894082,53.0313844320259));
#61388=CARTESIAN_POINT('Ctrl Pts',(-4.58760622731821,4.97455104537798,53.0398262632401));
#61389=CARTESIAN_POINT('Ctrl Pts',(-4.71430015623976,4.85771198754503,53.0479900486795));
#61390=CARTESIAN_POINT('Ctrl Pts',(-4.83672775852154,4.73584515673678,53.0561538341188));
#61391=CARTESIAN_POINT('Ctrl Pts',(-4.95446066932031,4.60929587639567,53.0643176195582));
#61392=CARTESIAN_POINT('Ctrl Pts',(-5.07205172863916,4.4828990700109,53.0724715687925));
#61393=CARTESIAN_POINT('Ctrl Pts',(-5.1849591110035,4.35183131024003,53.0806255180269));
#61394=CARTESIAN_POINT('Ctrl Pts',(-5.29278811920486,4.2164775494723,53.0887794672613));
#61395=CARTESIAN_POINT('Ctrl Pts',(-5.40050982819502,4.08125847743077,53.0969253026093));
#61396=CARTESIAN_POINT('Ctrl Pts',(-5.50316299893138,3.94176218007957,53.1050711379572));
#61397=CARTESIAN_POINT('Ctrl Pts',(-5.6003903684417,3.79840976213276,53.1132169733052));
#61398=CARTESIAN_POINT('Ctrl Pts',(-5.6975313295111,3.65518474513282,53.1213555692417));
#61399=CARTESIAN_POINT('Ctrl Pts',(-5.78925589283027,3.50811073656579,53.1294941651782));
#61400=CARTESIAN_POINT('Ctrl Pts',(-5.87524772452096,3.35764101349614,53.1376327611147));
#61401=CARTESIAN_POINT('Ctrl Pts',(-5.96119691033611,3.20724591278252,53.1457673208825));
#61402=CARTESIAN_POINT('Ctrl Pts',(-6.04141884315825,3.05345876605319,53.1539018806502));
#61403=CARTESIAN_POINT('Ctrl Pts',(-6.11564093687291,2.89676111048948,53.1620364404179));
#61404=CARTESIAN_POINT('Ctrl Pts',(-6.18984030787155,2.74011142711506,53.1701685098316));
#61405=CARTESIAN_POINT('Ctrl Pts',(-6.25804334094355,2.58055333878037,53.1783005792453));
#61406=CARTESIAN_POINT('Ctrl Pts',(-6.32002379943877,2.41859218855257,53.1864326486589));
#61407=CARTESIAN_POINT('Ctrl Pts',(-6.3819970455106,2.25664988510999,53.1945637717755));
#61408=CARTESIAN_POINT('Ctrl Pts',(-6.43774902943269,2.09230541801023,53.202694894892));
#61409=CARTESIAN_POINT('Ctrl Pts',(-6.48710199961309,1.92608323979413,53.2108260180086));
#61410=CARTESIAN_POINT('Ctrl Pts',(-6.53647515653617,1.75979307206641,53.2189604669815));
#61411=CARTESIAN_POINT('Ctrl Pts',(-6.57944396316227,1.59162400828446,53.2270949159545));
#61412=CARTESIAN_POINT('Ctrl Pts',(-6.61588067992854,1.42211526570397,53.2352293649274));
#61413=CARTESIAN_POINT('Ctrl Pts',(-6.65232474112214,1.25257235581225,53.243365453534));
#61414=CARTESIAN_POINT('Ctrl Pts',(-6.68223402057906,1.08168958800622,53.2515015421407));
#61415=CARTESIAN_POINT('Ctrl Pts',(-6.70553213345339,0.910015278566287,
53.2596376307474));
#61416=CARTESIAN_POINT('Ctrl Pts',(-6.72885072143747,0.738190096377742,
53.267780869603));
#61417=CARTESIAN_POINT('Ctrl Pts',(-6.74554649480596,0.565572346076884,
53.2759241084586));
#61418=CARTESIAN_POINT('Ctrl Pts',(-6.75559500211094,0.392715122517212,
53.2840673473142));
#61419=CARTESIAN_POINT('Ctrl Pts',(-6.76330849069643,0.260025541828338,
53.2903183036061));
#61420=CARTESIAN_POINT('Ctrl Pts',(-6.76710614738299,0.127194964573707,
53.2965692598979));
#61421=CARTESIAN_POINT('Ctrl Pts',(-6.7669977427746,-0.00552714063103698,
53.3028202161897));
#61422=CARTESIAN_POINT('Ctrl Pts',(-6.76699774277413,-0.00552714119462325,
53.3028202162162));
#61423=CARTESIAN_POINT('Ctrl Pts',(-6.76680339762221,-0.243468087172391,
53.3140267778591));
#61424=CARTESIAN_POINT('Ctrl Pts',(-6.75405577165269,-0.480929767539937,
53.325233339502));
#61425=CARTESIAN_POINT('Ctrl Pts',(-6.72892737728901,-0.716816120891868,
53.3364399011449));
#61426=CARTESIAN_POINT('Ctrl Pts',(-6.71329563251903,-0.863555113322262,
53.3434112224644));
#61427=CARTESIAN_POINT('Ctrl Pts',(-6.69287375263082,-1.00968507150458,
53.3503825437838));
#61428=CARTESIAN_POINT('Ctrl Pts',(-6.66771230148202,-1.1549466068461,53.3573538651032));
#61429=CARTESIAN_POINT('Ctrl Pts',(-6.63546270984458,-1.34112923867007,
53.3662890518854));
#61430=CARTESIAN_POINT('Ctrl Pts',(-6.59539020231709,-1.52607862653588,
53.3752242386676));
#61431=CARTESIAN_POINT('Ctrl Pts',(-6.54760220106742,-1.70915020304744,
53.3841594254498));
#61432=CARTESIAN_POINT('Ctrl Pts',(-6.49988577146036,-1.89194759497073,
53.3930812300862));
#61433=CARTESIAN_POINT('Ctrl Pts',(-6.44447697029663,-2.07287253783184,
53.4020030347227));
#61434=CARTESIAN_POINT('Ctrl Pts',(-6.38153410230253,-2.2512910742838,53.4109248393592));
#61435=CARTESIAN_POINT('Ctrl Pts',(-6.318744766891,-2.4292744056116,53.4198248815983));
#61436=CARTESIAN_POINT('Ctrl Pts',(-6.24845812854586,-2.60476328930247,
53.4287249238373));
#61437=CARTESIAN_POINT('Ctrl Pts',(-6.17088185859762,-2.77713991135318,
53.4376249660764));
#61438=CARTESIAN_POINT('Ctrl Pts',(-6.09342501845778,-2.94925115705933,
53.4465113065696));
#61439=CARTESIAN_POINT('Ctrl Pts',(-6.00870103817247,-3.11825946426911,
53.4553976470627));
#61440=CARTESIAN_POINT('Ctrl Pts',(-5.91696619009577,-3.2835651516703,53.4642839875559));
#61441=CARTESIAN_POINT('Ctrl Pts',(-5.82546589201355,-3.44844818128242,
53.4731476072275));
#61442=CARTESIAN_POINT('Ctrl Pts',(-5.72699062046693,-3.6096472565997,53.4820112268992));
#61443=CARTESIAN_POINT('Ctrl Pts',(-5.62184287493263,-3.76658621162045,
53.4908748465708));
#61444=CARTESIAN_POINT('Ctrl Pts',(-5.52202565744206,-3.91556905216016,
53.4992891197254));
#61445=CARTESIAN_POINT('Ctrl Pts',(-5.41619576806538,-4.06071272219559,
53.5077033928799));
#61446=CARTESIAN_POINT('Ctrl Pts',(-5.30465117116774,-4.20154316319953,
53.5161176660345));
#61447=CARTESIAN_POINT('Ctrl Pts',(-5.19581125000061,-4.33895882046231,
53.5243279142428));
#61448=CARTESIAN_POINT('Ctrl Pts',(-5.08163420007673,-4.4721351858391,53.5325381624511));
#61449=CARTESIAN_POINT('Ctrl Pts',(-4.96249228527308,-4.60064770642191,
53.5407484106594));
#61450=CARTESIAN_POINT('Ctrl Pts',(-4.84332204806029,-4.72919077699372,
53.5489606106075));
#61451=CARTESIAN_POINT('Ctrl Pts',(-4.71918483657764,-4.85306753291011,
53.5571728105555));
#61452=CARTESIAN_POINT('Ctrl Pts',(-4.59049031070317,-4.9718897521305,53.5653850105035));
#61453=CARTESIAN_POINT('Ctrl Pts',(-4.46174227468526,-5.09076137666904,
53.5736006250179));
#61454=CARTESIAN_POINT('Ctrl Pts',(-4.32843341053945,-5.20457403632901,
53.5818162395323));
#61455=CARTESIAN_POINT('Ctrl Pts',(-4.19100708116593,-5.31297926267523,
53.5900318540467));
#61456=CARTESIAN_POINT('Ctrl Pts',(-4.05342642804842,-5.42150622333884,
53.598256694336));
#61457=CARTESIAN_POINT('Ctrl Pts',(-3.91171935418317,-5.52461340178658,
53.6064815346254));
#61458=CARTESIAN_POINT('Ctrl Pts',(-3.76635967012437,-5.62199464916685,
53.6147063749148));
#61459=CARTESIAN_POINT('Ctrl Pts',(-3.62090687813434,-5.71943827262164,
53.6229364835003));
#61460=CARTESIAN_POINT('Ctrl Pts',(-3.47179711443141,-5.81114846771948,
53.6311665920858));
#61461=CARTESIAN_POINT('Ctrl Pts',(-3.3195294390031,-5.89686470114346,53.6393967006713));
#61462=CARTESIAN_POINT('Ctrl Pts',(-3.1670530022546,-5.98269845283914,53.6476380928621));
#61463=CARTESIAN_POINT('Ctrl Pts',(-3.01141032175888,-6.06252166669002,
53.6558794850528));
#61464=CARTESIAN_POINT('Ctrl Pts',(-2.85312201217741,-6.1361212328008,53.6641208772435));
#61465=CARTESIAN_POINT('Ctrl Pts',(-2.78423091878326,-6.16815363365284,
53.6677077404844));
#61466=CARTESIAN_POINT('Ctrl Pts',(-2.71483890667416,-6.19900777537673,
53.6712946037254));
#61467=CARTESIAN_POINT('Ctrl Pts',(-2.64498979819209,-6.2286690365968,53.6748814669663));
#61468=CARTESIAN_POINT('Ctrl Pts',(-2.48046726377903,-6.29853314761931,
53.6833299617834));
#61469=CARTESIAN_POINT('Ctrl Pts',(-2.31303257010345,-6.36193526230486,
53.6917784566006));
#61470=CARTESIAN_POINT('Ctrl Pts',(-2.14322108452927,-6.41863633358591,
53.7002269514177));
#61471=CARTESIAN_POINT('Ctrl Pts',(-1.97356471188428,-6.47528561173162,
53.7086677290255));
#61472=CARTESIAN_POINT('Ctrl Pts',(-1.80153618968942,-6.52524594240804,
53.7171085066334));
#61473=CARTESIAN_POINT('Ctrl Pts',(-1.62769051121065,-6.56832646872206,
53.7255492842412));
#61474=CARTESIAN_POINT('Ctrl Pts',(-1.45397689693279,-6.61137426833656,
53.7339836496991));
#61475=CARTESIAN_POINT('Ctrl Pts',(-1.27844920078841,-6.64755260242074,
53.742418015157));
#61476=CARTESIAN_POINT('Ctrl Pts',(-1.10167759735194,-6.67672041285936,
53.7508523806149));
#61477=CARTESIAN_POINT('Ctrl Pts',(-0.925013134425863,-6.70587054481322,
53.7592816340401));
#61478=CARTESIAN_POINT('Ctrl Pts',(-0.747106595525708,-6.72801857046729,
53.7677108874653));
#61479=CARTESIAN_POINT('Ctrl Pts',(-0.568538762665382,-6.74307442309122,
53.7761401408905));
#61480=CARTESIAN_POINT('Ctrl Pts',(-0.390051767215453,-6.75812345995153,
53.7845655784043));
#61481=CARTESIAN_POINT('Ctrl Pts',(-0.21090440645474,-6.76608669783246,
53.7929910159183));
#61482=CARTESIAN_POINT('Ctrl Pts',(-0.0316834057099282,-6.76692582801102,
53.8014164534321));
#61483=CARTESIAN_POINT('Ctrl Pts',(0.147498225001867,-6.76776477385525,
53.809840040104));
#61484=CARTESIAN_POINT('Ctrl Pts',(0.326753130332813,-6.76148272806156,
53.8182636267758));
#61485=CARTESIAN_POINT('Ctrl Pts',(0.505493215601638,-6.74809347956745,
53.8266872134477));
#61486=CARTESIAN_POINT('Ctrl Pts',(0.684213300793744,-6.73470572925991,
53.8351098575645));
#61487=CARTESIAN_POINT('Ctrl Pts',(0.862418348359472,-6.71421238655197,
53.8435325016813));
#61488=CARTESIAN_POINT('Ctrl Pts',(1.03952370131174,-6.68667925613388,53.851955145798));
#61489=CARTESIAN_POINT('Ctrl Pts',(1.21663393373037,-6.6591453671448,53.8603780219688));
#61490=CARTESIAN_POINT('Ctrl Pts',(1.39264408174607,-6.62457135535248,53.8688008981396));
#61491=CARTESIAN_POINT('Ctrl Pts',(1.56697764901718,-6.58307451328637,53.8772237743104));
#61492=CARTESIAN_POINT('Ctrl Pts',(1.74134033096391,-6.54157074101678,53.8856480571484));
#61493=CARTESIAN_POINT('Ctrl Pts',(1.91402554977653,-6.49314191123189,53.8940723399863));
#61494=CARTESIAN_POINT('Ctrl Pts',(2.08446962294295,-6.43795583947483,53.9024966228243));
#61495=CARTESIAN_POINT('Ctrl Pts',(2.25502880773952,-6.38273249708369,53.9109265951117));
#61496=CARTESIAN_POINT('Ctrl Pts',(2.42334350489641,-6.32074289644361,53.919356567399));
#61497=CARTESIAN_POINT('Ctrl Pts',(2.5888667875922,-6.25220423179714,53.9277865396864));
#61498=CARTESIAN_POINT('Ctrl Pts',(2.75444924219275,-6.18364106568314,53.936219525553));
#61499=CARTESIAN_POINT('Ctrl Pts',(2.9172379869409,-6.10852430056944,53.9446525114195));
#61500=CARTESIAN_POINT('Ctrl Pts',(3.07670801617771,-6.0271184477483,53.953085497286));
#61501=CARTESIAN_POINT('Ctrl Pts',(3.2363247568757,-5.94563770203553,53.9615262414485));
#61502=CARTESIAN_POINT('Ctrl Pts',(3.39261638763213,-5.85785646569089,53.969966985611));
#61503=CARTESIAN_POINT('Ctrl Pts',(3.54508339183175,-5.76408472742713,53.9784077297735));
#61504=CARTESIAN_POINT('Ctrl Pts',(3.62938647299413,-5.71223582737767,53.983074842792));
#61505=CARTESIAN_POINT('Ctrl Pts',(3.71252076059832,-5.65855624031891,53.9877419558105));
#61506=CARTESIAN_POINT('Ctrl Pts',(3.7944058170641,-5.60310391617272,53.9924090688291));
#61507=CARTESIAN_POINT('Ctrl Pts',(3.93724708005844,-5.50637222471541,54.0005504360929));
#61508=CARTESIAN_POINT('Ctrl Pts',(4.07656896193991,-5.40405145202004,54.0086918033567));
#61509=CARTESIAN_POINT('Ctrl Pts',(4.21190241936764,-5.29642964738748,54.0168331706206));
#61510=CARTESIAN_POINT('Ctrl Pts',(4.3471177409749,-5.18890178840909,54.0249674310897));
#61511=CARTESIAN_POINT('Ctrl Pts',(4.47835128373244,-5.07608233467336,54.0331016915588));
#61512=CARTESIAN_POINT('Ctrl Pts',(4.60516250417448,-4.95830286591546,54.0412359520279));
#61513=CARTESIAN_POINT('Ctrl Pts',(4.73188721857703,-4.8406037420619,54.049364663598));
#61514=CARTESIAN_POINT('Ctrl Pts',(4.85419534979951,-4.71795158780571,54.0574933751681));
#61515=CARTESIAN_POINT('Ctrl Pts',(4.97167905508774,-4.59071850293633,54.0656220867382));
#61516=CARTESIAN_POINT('Ctrl Pts',(5.08910673455894,-4.46354609318366,54.0737469218753));
#61517=CARTESIAN_POINT('Ctrl Pts',(5.20171432175762,-4.33179737141275,54.0818717570124));
#61518=CARTESIAN_POINT('Ctrl Pts',(5.30913053169631,-4.19588155188037,54.0899965921495));
#61519=CARTESIAN_POINT('Ctrl Pts',(5.41651667016116,-4.0600037823687,54.0981191527159));
#61520=CARTESIAN_POINT('Ctrl Pts',(5.51871410001962,-3.91996152617119,54.1062417132823));
#61521=CARTESIAN_POINT('Ctrl Pts',(5.61539159620327,-3.77619732287519,54.1143642738487));
#61522=CARTESIAN_POINT('Ctrl Pts',(5.71207423053681,-3.63242547889697,54.1224872661074));
#61523=CARTESIAN_POINT('Ctrl Pts',(5.80323613760412,-3.48493159422831,54.1306102583661));
#61524=CARTESIAN_POINT('Ctrl Pts',(5.88858913701548,-3.33418760351353,54.1387332506248));
#61525=CARTESIAN_POINT('Ctrl Pts',(5.93215923905719,-3.25723739551951,54.1428797903368));
#61526=CARTESIAN_POINT('Ctrl Pts',(5.97421637291487,-3.17944072073768,54.1470263300488));
#61527=CARTESIAN_POINT('Ctrl Pts',(6.01472678269927,-3.10086290078748,54.1511728697608));
#61528=CARTESIAN_POINT('Ctrl Pts',(6.10249435013694,-2.93062063100326,54.1601565286708));
#61529=CARTESIAN_POINT('Ctrl Pts',(6.18295569056279,-2.75679467971065,54.1691401875807));
#61530=CARTESIAN_POINT('Ctrl Pts',(6.2558647371488,-2.58000879659319,54.1781238464906));
#61531=CARTESIAN_POINT('Ctrl Pts',(6.3288990406813,-2.40291919725752,54.1871229392285));
#61532=CARTESIAN_POINT('Ctrl Pts',(6.39435502628826,-2.22285972346298,54.1961220319664));
#61533=CARTESIAN_POINT('Ctrl Pts',(6.45203574927775,-2.04047143818332,54.2051211247044));
#61534=CARTESIAN_POINT('Ctrl Pts',(6.50985171743181,-1.85765550338093,54.2141413177981));
#61535=CARTESIAN_POINT('Ctrl Pts',(6.55985587393634,-1.67250006070934,54.2231615108918));
#61536=CARTESIAN_POINT('Ctrl Pts',(6.60190120794937,-1.48566128053357,54.2321817039855));
#61537=CARTESIAN_POINT('Ctrl Pts',(6.64398912339014,-1.29863327931332,54.2412110322832));
#61538=CARTESIAN_POINT('Ctrl Pts',(6.67810206728113,-1.10991876924692,54.2502403605809));
#61539=CARTESIAN_POINT('Ctrl Pts',(6.70414441878094,-0.920182923188831,
54.2592696888785));
#61540=CARTESIAN_POINT('Ctrl Pts',(6.73022348475264,-0.730179587791919,
54.268311746711));
#61541=CARTESIAN_POINT('Ctrl Pts',(6.74820917553739,-0.539152274397078,
54.2773538045435));
#61542=CARTESIAN_POINT('Ctrl Pts',(6.75805766199569,-0.347772392724564,
54.2863958623759));
#61543=CARTESIAN_POINT('Ctrl Pts',(6.76660443811736,-0.181687887275826,
54.2942427984813));
#61544=CARTESIAN_POINT('Ctrl Pts',(6.76902371777479,-0.0153380007074978,
54.3020897345867));
#61545=CARTESIAN_POINT('Ctrl Pts',(6.76531867369218,0.150838467878465,54.3099366706921));
#61546=CARTESIAN_POINT('Ctrl Pts',(6.7612328156501,0.334094981279396,54.3185901350712));
#61547=CARTESIAN_POINT('Ctrl Pts',(6.74969404463363,0.517302093070697,54.3272435994503));
#61548=CARTESIAN_POINT('Ctrl Pts',(6.73071363539664,0.699844953033015,54.3358970638295));
#61549=CARTESIAN_POINT('Ctrl Pts',(6.71175071100041,0.882219653668543,54.3445425565972));
#61550=CARTESIAN_POINT('Ctrl Pts',(6.68535985272872,1.06393102162104,54.3531880493649));
#61551=CARTESIAN_POINT('Ctrl Pts',(6.65160430059668,1.24436699903353,54.3618335421326));
#61552=CARTESIAN_POINT('Ctrl Pts',(6.61683327108885,1.4302310806028,54.3707391195902));
#61553=CARTESIAN_POINT('Ctrl Pts',(6.57424751678385,1.61474151269027,54.3796446970478));
#61554=CARTESIAN_POINT('Ctrl Pts',(6.52397371427464,1.79723564828142,54.3885502745054));
#61555=CARTESIAN_POINT('Ctrl Pts',(6.47526074979517,1.97406393460679,54.3971793627523));
#61556=CARTESIAN_POINT('Ctrl Pts',(6.4193300311417,2.14899892080663,54.4058084509993));
#61557=CARTESIAN_POINT('Ctrl Pts',(6.35634858520071,2.32144818236741,54.4144375392462));
#61558=CARTESIAN_POINT('Ctrl Pts',(6.29034010619849,2.50218575183112,54.4234813613091));
#61559=CARTESIAN_POINT('Ctrl Pts',(6.21658650343977,2.68019243368415,54.4325251833721));
#61560=CARTESIAN_POINT('Ctrl Pts',(6.13533902892131,2.85480367104201,54.4415690054351));
#61561=CARTESIAN_POINT('Ctrl Pts',(6.0540915544029,3.02941490839975,54.450612827498));
#61562=CARTESIAN_POINT('Ctrl Pts',(5.96535033927651,3.20063033729916,54.4596566495609));
#61563=CARTESIAN_POINT('Ctrl Pts',(5.86942530269928,3.36780872616506,54.4687004716238));
#61564=CARTESIAN_POINT('Ctrl Pts',(5.78005554338682,3.52356256174645,54.4771262614892));
#61565=CARTESIAN_POINT('Ctrl Pts',(5.68448958826155,3.67574416625311,54.4855520513545));
#61566=CARTESIAN_POINT('Ctrl Pts',(5.5830464933457,3.82385680343031,54.4939778412199));
#61567=CARTESIAN_POINT('Ctrl Pts',(5.48157986020914,3.97200380773666,54.5024055861528));
#61568=CARTESIAN_POINT('Ctrl Pts',(5.37423355559814,4.11607968873494,54.5108333310857));
#61569=CARTESIAN_POINT('Ctrl Pts',(5.26136909901297,4.25561795794118,54.5192610760187));
#61570=CARTESIAN_POINT('Ctrl Pts',(5.14846317039171,4.39520750047395,54.5276919177258));
#61571=CARTESIAN_POINT('Ctrl Pts',(5.03003525523271,4.53025584905723,54.536122759433));
#61572=CARTESIAN_POINT('Ctrl Pts',(4.90648640596404,4.66033047627419,54.5445536011402));
#61573=CARTESIAN_POINT('Ctrl Pts',(4.78282403105726,4.79052462548707,54.5529921897158));
#61574=CARTESIAN_POINT('Ctrl Pts',(4.65403154938654,4.9157356819451,54.5614307782914));
#61575=CARTESIAN_POINT('Ctrl Pts',(4.5205468380363,5.03556802010657,54.569869366867));
#61576=CARTESIAN_POINT('Ctrl Pts',(4.38699213319283,5.15546319305912,54.5783123802662));
#61577=CARTESIAN_POINT('Ctrl Pts',(4.24874054328489,5.26997380743445,54.5867553936653));
#61578=CARTESIAN_POINT('Ctrl Pts',(4.10626254426284,5.37874492029359,54.5951984070645));
#61579=CARTESIAN_POINT('Ctrl Pts',(3.96363486215945,5.48763030479778,54.6036502904385));
#61580=CARTESIAN_POINT('Ctrl Pts',(3.81677216936223,5.59076394819946,54.6121021738124));
#61581=CARTESIAN_POINT('Ctrl Pts',(3.66617426600214,5.68783396833133,54.6205540571864));
#61582=CARTESIAN_POINT('Ctrl Pts',(3.62513158157831,5.71428861420884,54.6228574623093));
#61583=CARTESIAN_POINT('Ctrl Pts',(3.58381161573429,5.74029315479914,54.6251608674323));
#61584=CARTESIAN_POINT('Ctrl Pts',(3.54222479973447,5.76584186985267,54.6274642725552));
#61585=CARTESIAN_POINT('Ctrl Pts',(3.39783780246129,5.85454551696003,54.6354615606671));
#61586=CARTESIAN_POINT('Ctrl Pts',(3.24998281800364,5.93790483836299,54.643458848779));
#61587=CARTESIAN_POINT('Ctrl Pts',(3.09908550384732,6.01564277861007,54.6514561368909));
#61588=CARTESIAN_POINT('Origin',(0.,0.,-63.6971797838103));
#61589=CARTESIAN_POINT('',(3.09908550384732,6.01564277861007,57.0457563580462));
#61590=CARTESIAN_POINT('',(3.09908550384733,6.01564277861006,56.6515377972971));
#61591=CARTESIAN_POINT('',(3.09908550384721,6.01564277861012,-63.6971797838103));
#61592=CARTESIAN_POINT('',(-6.767,6.12423652101343E-12,55.6971797838098));
#61593=CARTESIAN_POINT('Ctrl Pts',(-6.767,6.12423655037739E-12,55.6971797838098));
#61594=CARTESIAN_POINT('Ctrl Pts',(-6.76700000000017,-0.186007249553793,
55.7059292956226));
#61595=CARTESIAN_POINT('Ctrl Pts',(-6.75932637294281,-0.372014355809892,
55.7146788074353));
#61596=CARTESIAN_POINT('Ctrl Pts',(-6.74400518263414,-0.55738953758019,
55.723428319248));
#61597=CARTESIAN_POINT('Ctrl Pts',(-6.72868405703796,-0.742763936376777,
55.7321777941052));
#61598=CARTESIAN_POINT('Ctrl Pts',(-6.70571545643644,-0.927506130399208,
55.7409272689624));
#61599=CARTESIAN_POINT('Ctrl Pts',(-6.67517739401668,-1.11098864008985,
55.7496767438196));
#61600=CARTESIAN_POINT('Ctrl Pts',(-6.64463945804495,-1.29447039003999,
55.7584261824482));
#61601=CARTESIAN_POINT('Ctrl Pts',(-6.60653217002842,-1.47669218338753,
55.7671756210767));
#61602=CARTESIAN_POINT('Ctrl Pts',(-6.56098496085608,-1.65703510627276,
55.7759250597052));
#61603=CARTESIAN_POINT('Ctrl Pts',(-6.51543793649696,-1.83737729739512,
55.7846744628319));
#61604=CARTESIAN_POINT('Ctrl Pts',(-6.46245112157048,-2.01584035544466,
55.7934238659585));
#61605=CARTESIAN_POINT('Ctrl Pts',(-6.4022044836188,-2.19181813796934,55.8021732690851));
#61606=CARTESIAN_POINT('Ctrl Pts',(-6.3419580851215,-2.36779522105827,55.8109226374366));
#61607=CARTESIAN_POINT('Ctrl Pts',(-6.27445201416547,-2.54128677725268,
55.8196720057881));
#61608=CARTESIAN_POINT('Ctrl Pts',(-6.19991555052933,-2.71170355428182,
55.8284213741397));
#61609=CARTESIAN_POINT('Ctrl Pts',(-6.12537937695335,-2.8821196681306,55.8371707084429));
#61610=CARTESIAN_POINT('Ctrl Pts',(-6.04381298028571,-3.04946076419433,
55.8459200427461));
#61611=CARTESIAN_POINT('Ctrl Pts',(-5.95549339309104,-3.21315848424085,
55.8546693770492));
#61612=CARTESIAN_POINT('Ctrl Pts',(-5.86717414225929,-3.37685558084874,
55.8634186780308));
#61613=CARTESIAN_POINT('Ctrl Pts',(-5.77210188844183,-3.5369090769981,55.8721679790124));
#61614=CARTESIAN_POINT('Ctrl Pts',(-5.67059953311484,-3.69277537023819,
55.8809172799939));
#61615=CARTESIAN_POINT('Ctrl Pts',(-5.56909755592814,-3.84864108280873,
55.8896665483806));
#61616=CARTESIAN_POINT('Ctrl Pts',(-5.46116568155066,-4.00031938354693,
55.8984158167672));
#61617=CARTESIAN_POINT('Ctrl Pts',(-5.34717048488469,-4.14729511918046,
55.9071650851538));
#61618=CARTESIAN_POINT('Ctrl Pts',(-5.23317570343388,-4.29427031947079,
55.9159143216722));
#61619=CARTESIAN_POINT('Ctrl Pts',(-5.1131178195162,-4.43654276249472,55.9246635581905));
#61620=CARTESIAN_POINT('Ctrl Pts',(-4.98740458929306,-4.57362924412315,
55.9334127947089));
#61621=CARTESIAN_POINT('Ctrl Pts',(-4.86169180652812,-4.71071523781193,
55.9421620000856));
#61622=CARTESIAN_POINT('Ctrl Pts',(-4.73032391141655,-4.84261509584409,
55.9509112054623));
#61623=CARTESIAN_POINT('Ctrl Pts',(-4.5937470694742,-4.96888084599512,55.959660410839));
#61624=CARTESIAN_POINT('Ctrl Pts',(-4.45717070231623,-5.09514615720641,
55.9684095858007));
#61625=CARTESIAN_POINT('Ctrl Pts',(-4.31538563497501,-5.21577720520468,
55.9771587607624));
#61626=CARTESIAN_POINT('Ctrl Pts',(-4.16887340952202,-5.33036429293348,
55.9859079357241));
#61627=CARTESIAN_POINT('Ctrl Pts',(-4.02236168122661,-5.44495099183577,
55.9946570809974));
#61628=CARTESIAN_POINT('Ctrl Pts',(-3.87112305263335,-5.55349359497822,
56.0034062262706));
#61629=CARTESIAN_POINT('Ctrl Pts',(-3.71567116929126,-5.65562346357126,
56.0121553715439));
#61630=CARTESIAN_POINT('Ctrl Pts',(-3.56021980053452,-5.7577529940884,56.0209044878553));
#61631=CARTESIAN_POINT('Ctrl Pts',(-3.40055544442236,-5.85346967519791,
56.0296536041666));
#61632=CARTESIAN_POINT('Ctrl Pts',(-3.23722035887006,-5.94244843041294,
56.038402720478));
#61633=CARTESIAN_POINT('Ctrl Pts',(-3.07388580043661,-6.03142689847363,
56.047151808554));
#61634=CARTESIAN_POINT('Ctrl Pts',(-2.90688078789402,-6.11366734707816,
56.05590089663));
#61635=CARTESIAN_POINT('Ctrl Pts',(-2.73677250610581,-6.18889047001346,
56.064649984706));
#61636=CARTESIAN_POINT('Ctrl Pts',(-2.56666475917122,-6.26411335643257,
56.0733990452732));
#61637=CARTESIAN_POINT('Ctrl Pts',(-2.39345402457279,-6.33231884545185,
56.0821481058404));
#61638=CARTESIAN_POINT('Ctrl Pts',(-2.21772855944251,-6.39327529804818,
56.0908971664076));
#61639=CARTESIAN_POINT('Ctrl Pts',(-2.0420036322376,-6.4542315640465,56.0996462001924));
#61640=CARTESIAN_POINT('Ctrl Pts',(-1.86376426061186,-6.5079387441241,56.1083952339772));
#61641=CARTESIAN_POINT('Ctrl Pts',(-1.68361577621823,-6.55421443943278,
56.117144267762));
#61642=CARTESIAN_POINT('Ctrl Pts',(-1.50346782833358,-6.60048999692555,
56.1258932754909));
#61643=CARTESIAN_POINT('Ctrl Pts',(-1.32141105657539,-6.63933404265132,
56.1346422832198));
#61644=CARTESIAN_POINT('Ctrl Pts',(-1.13806375346695,-6.67061465631502,
56.1433912909487));
#61645=CARTESIAN_POINT('Ctrl Pts',(-0.954716981171704,-6.70189517941747,
56.1521402733481));
#61646=CARTESIAN_POINT('Ctrl Pts',(-0.770079967444078,-6.72561226608983,
56.1608892557475));
#61647=CARTESIAN_POINT('Ctrl Pts',(-0.584779764074965,-6.74168536995968,
56.1696382381469));
#61648=CARTESIAN_POINT('Ctrl Pts',(-0.391489587594831,-6.75845153117862,
56.1787644685625));
#61649=CARTESIAN_POINT('Ctrl Pts',(-0.197478091807088,-6.76689985146389,
56.1878906989782));
#61650=CARTESIAN_POINT('Ctrl Pts',(-0.00346214753285774,-6.76699911434415,
56.1970169293938));
#61651=CARTESIAN_POINT('Ctrl Pts',(0.184490798482887,-6.7670952752594,56.2058579651089));
#61652=CARTESIAN_POINT('Ctrl Pts',(0.372447602153101,-6.75935633790773,
56.2146990008241));
#61653=CARTESIAN_POINT('Ctrl Pts',(0.559756448192614,-6.74380914014526,
56.2235400365392));
#61654=CARTESIAN_POINT('Ctrl Pts',(0.745136131041716,-6.72842206873173,
56.2322900151525));
#61655=CARTESIAN_POINT('Ctrl Pts',(0.929880851943366,-6.70538686355747,
56.2410399937658));
#61656=CARTESIAN_POINT('Ctrl Pts',(1.11336305057292,-6.67478177303341,56.2497899723791));
#61657=CARTESIAN_POINT('Ctrl Pts',(1.29684337089958,-6.64417699581293,56.2585398614191));
#61658=CARTESIAN_POINT('Ctrl Pts',(1.47906091205031,-6.60600253548095,56.2672897504591));
#61659=CARTESIAN_POINT('Ctrl Pts',(1.65939671095068,-6.56038806441251,56.2760396394991));
#61660=CARTESIAN_POINT('Ctrl Pts',(1.83973072369019,-6.5147740451389,56.2847894418746));
#61661=CARTESIAN_POINT('Ctrl Pts',(2.01818275356906,-6.46172023288702,56.29353924425));
#61662=CARTESIAN_POINT('Ctrl Pts',(2.19414664033207,-6.40140683918149,56.3022890466255));
#61663=CARTESIAN_POINT('Ctrl Pts',(2.37010884271142,-6.34109402281541,56.3110387652451));
#61664=CARTESIAN_POINT('Ctrl Pts',(2.54358267847691,-6.27352185699838,56.3197884838646));
#61665=CARTESIAN_POINT('Ctrl Pts',(2.71397890841629,-6.19891986435311,56.3285382024841));
#61666=CARTESIAN_POINT('Ctrl Pts',(2.88437356388838,-6.12431856103292,56.337287840256));
#61667=CARTESIAN_POINT('Ctrl Pts',(3.05169040787076,-6.04268767582606,56.3460374780278));
#61668=CARTESIAN_POINT('Ctrl Pts',(3.21536112511966,-5.95430447953993,56.3547871157996));
#61669=CARTESIAN_POINT('Ctrl Pts',(3.37903038442757,-5.86592207055092,56.3635366756317));
#61670=CARTESIAN_POINT('Ctrl Pts',(3.5390533297989,-5.77078760703428,56.3722862354637));
#61671=CARTESIAN_POINT('Ctrl Pts',(3.69488643041811,-5.66922422085351,56.3810357952958));
#61672=CARTESIAN_POINT('Ctrl Pts',(3.85071819468664,-5.56766170563212,56.3897852800958));
#61673=CARTESIAN_POINT('Ctrl Pts',(4.00235994599149,-5.45967053456307,56.3985347648958));
#61674=CARTESIAN_POINT('Ctrl Pts',(4.14929662974228,-5.34561750206741,56.4072842496958));
#61675=CARTESIAN_POINT('Ctrl Pts',(4.29623210224969,-5.23156540974528,56.4160336623712));
#61676=CARTESIAN_POINT('Ctrl Pts',(4.43846235842039,-5.11145173172254,56.4247830750465));
#61677=CARTESIAN_POINT('Ctrl Pts',(4.57550431797349,-4.98568443006635,56.4335324877219));
#61678=CARTESIAN_POINT('Ctrl Pts',(4.71254519337425,-4.85991812336756,56.4422818311798));
#61679=CARTESIAN_POINT('Ctrl Pts',(4.84439764314925,-4.72849847631161,56.4510311746377));
#61680=CARTESIAN_POINT('Ctrl Pts',(4.97061384196638,-4.59187184425396,56.4597805180956));
#61681=CARTESIAN_POINT('Ctrl Pts',(5.09682908420159,-4.45524624767801,56.4685297952429));
#61682=CARTESIAN_POINT('Ctrl Pts',(5.21740796650125,-4.31341395556948,56.4772790723903));
#61683=CARTESIAN_POINT('Ctrl Pts',(5.33194095942206,-4.16685668162913,56.4860283495377));
#61684=CARTESIAN_POINT('Ctrl Pts',(5.44647312235093,-4.02030046975269,56.4947775632812));
#61685=CARTESIAN_POINT('Ctrl Pts',(5.55495930712253,-3.86901957035598,56.5035267770247));
#61686=CARTESIAN_POINT('Ctrl Pts',(5.65703106079764,-3.71352778058422,56.5122759907683));
#61687=CARTESIAN_POINT('Ctrl Pts',(5.75910210868695,-3.55803706597667,56.5210251440145));
#61688=CARTESIAN_POINT('Ctrl Pts',(5.85475865698501,-3.39833575880982,56.5297742972607));
#61689=CARTESIAN_POINT('Ctrl Pts',(5.94367583069008,-3.23496624706822,56.5385234505069));
#61690=CARTESIAN_POINT('Ctrl Pts',(6.03259241910023,-3.07159781070207,56.547272546162));
#61691=CARTESIAN_POINT('Ctrl Pts',(6.11476958470914,-2.90456146975947,56.5560216418171));
#61692=CARTESIAN_POINT('Ctrl Pts',(6.18992823574333,-2.73442451648376,56.5647707374722));
#61693=CARTESIAN_POINT('Ctrl Pts',(6.26508641700898,-2.56428862662509,56.5735197784423));
#61694=CARTESIAN_POINT('Ctrl Pts',(6.33322605570272,-2.39105242531344,56.5822688194125));
#61695=CARTESIAN_POINT('Ctrl Pts',(6.39411573747753,-2.21530425353768,56.5910178603826));
#61696=CARTESIAN_POINT('Ctrl Pts',(6.45500505889114,-2.03955712188598,56.5997668495736));
#61697=CARTESIAN_POINT('Ctrl Pts',(6.5086444154492,-1.86129832025606,56.6085158387646));
#61698=CARTESIAN_POINT('Ctrl Pts',(6.55485164049898,-1.6811332401234,56.6172648279556));
#61699=CARTESIAN_POINT('Ctrl Pts',(6.60199852639105,-1.4973043591292,56.6261917348325));
#61700=CARTESIAN_POINT('Ctrl Pts',(6.64140767441008,-1.31149113173663,56.6351186417094));
#61701=CARTESIAN_POINT('Ctrl Pts',(6.67293975269602,-1.12435050446434,56.6440455485863));
#61702=CARTESIAN_POINT('Ctrl Pts',(6.70384664831506,-0.94092029156382,56.6527954627703));
#61703=CARTESIAN_POINT('Ctrl Pts',(6.72718585889664,-0.756215114278064,
56.6615453769543));
#61704=CARTESIAN_POINT('Ctrl Pts',(6.74287810451863,-0.570862389375311,
56.6702952911382));
#61705=CARTESIAN_POINT('Ctrl Pts',(6.75857004154122,-0.385513309568294,
56.6790450332488));
#61706=CARTESIAN_POINT('Ctrl Pts',(6.76661529035555,-0.199516993259425,
56.6877947753594));
#61707=CARTESIAN_POINT('Ctrl Pts',(6.76698652348896,-0.0135052182052907,
56.69654451747));
#61708=CARTESIAN_POINT('Ctrl Pts',(6.76735774981525,0.172503146037646,56.7052940991406));
#61709=CARTESIAN_POINT('Ctrl Pts',(6.76005524147486,0.358526681832213,56.7140436808113));
#61710=CARTESIAN_POINT('Ctrl Pts',(6.74510380214892,0.543933542113598,56.7227932624819));
#61711=CARTESIAN_POINT('Ctrl Pts',(6.73015261710994,0.729337249083357,56.7315426953438));
#61712=CARTESIAN_POINT('Ctrl Pts',(6.70755278444625,0.914124015853203,56.7402921282058));
#61713=CARTESIAN_POINT('Ctrl Pts',(6.67738106408314,1.0976662174923,56.7490415610677));
#61714=CARTESIAN_POINT('Ctrl Pts',(6.64720981677284,1.28120554143164,56.75779085675));
#61715=CARTESIAN_POINT('Ctrl Pts',(6.60946696581558,1.46350005650459,56.7665401524324));
#61716=CARTESIAN_POINT('Ctrl Pts',(6.56428070011035,1.64393062206371,56.7752894481147));
#61717=CARTESIAN_POINT('Ctrl Pts',(6.51909508282788,1.82435859844484,56.7840386182447));
#61718=CARTESIAN_POINT('Ctrl Pts',(6.46646633415715,2.00292240086389,56.7927877883747));
#61719=CARTESIAN_POINT('Ctrl Pts',(6.40657319597253,2.17901557696276,56.8015369585047));
#61720=CARTESIAN_POINT('Ctrl Pts',(6.34668083768359,2.35510646007261,56.8102860147078));
#61721=CARTESIAN_POINT('Ctrl Pts',(6.27952437143953,2.52872650996363,56.8190350709108));
#61722=CARTESIAN_POINT('Ctrl Pts',(6.20533187335206,2.69928607997764,56.8277841271139));
#61723=CARTESIAN_POINT('Ctrl Pts',(6.12831449784326,2.87633970115239,56.8368663034028));
#61724=CARTESIAN_POINT('Ctrl Pts',(6.04371489463231,3.05009490562194,56.8459484796916));
#61725=CARTESIAN_POINT('Ctrl Pts',(5.95184265120572,3.21991584599481,56.8550306559805));
#61726=CARTESIAN_POINT('Ctrl Pts',(5.86333281335579,3.38352155905151,56.8637804363349));
#61727=CARTESIAN_POINT('Ctrl Pts',(5.76807337235776,3.54347560903676,56.8725302166893));
#61728=CARTESIAN_POINT('Ctrl Pts',(5.66638790086451,3.69923467178501,56.8812799970437));
#61729=CARTESIAN_POINT('Ctrl Pts',(5.56470608502837,3.85498813489629,56.890029462838));
#61730=CARTESIAN_POINT('Ctrl Pts',(5.45659885767044,4.00654667256137,56.8987789286322));
#61731=CARTESIAN_POINT('Ctrl Pts',(5.34243340580596,4.15339551506096,56.9075283944265));
#61732=CARTESIAN_POINT('Ctrl Pts',(5.2282714514068,4.30023985883765,56.9162775921804));
#61733=CARTESIAN_POINT('Ctrl Pts',(5.10805181978173,4.44237456992946,56.9250267899343));
#61734=CARTESIAN_POINT('Ctrl Pts',(4.98218281282632,4.5793169162636,56.9337759876881));
#61735=CARTESIAN_POINT('Ctrl Pts',(4.856316992963,4.7162557951209,56.9425249639061));
#61736=CARTESIAN_POINT('Ctrl Pts',(4.72480227791897,4.84800236135713,56.9512739401242));
#61737=CARTESIAN_POINT('Ctrl Pts',(4.58808530848159,4.97410918678867,56.9600229163422));
#61738=CARTESIAN_POINT('Ctrl Pts',(4.45135945057013,5.10022421088972,56.9687724613634));
#61739=CARTESIAN_POINT('Ctrl Pts',(4.30943087208079,5.22069856611954,56.9775220063846));
#61740=CARTESIAN_POINT('Ctrl Pts',(4.16278164322503,5.33512305301656,56.9862715514058));
#61741=CARTESIAN_POINT('Ctrl Pts',(4.01614103534424,5.44954081331402,56.995020582073));
#61742=CARTESIAN_POINT('Ctrl Pts',(3.86478055833445,5.55790924068316,57.0037696127403));
#61743=CARTESIAN_POINT('Ctrl Pts',(3.70921425811981,5.65986029751272,57.0125186434076));
#61744=CARTESIAN_POINT('Ctrl Pts',(3.55364584530154,5.76181273884632,57.0212677928874));
#61745=CARTESIAN_POINT('Ctrl Pts',(3.39387173464384,5.8573474781804,57.0300169423673));
#61746=CARTESIAN_POINT('Ctrl Pts',(3.2304345609245,5.94614005448783,57.0387660918471));
#61747=CARTESIAN_POINT('Ctrl Pts',(3.18690768806426,5.96978744811264,57.0410961805802));
#61748=CARTESIAN_POINT('Ctrl Pts',(3.14312114982904,5.99295688499288,57.0434262693132));
#61749=CARTESIAN_POINT('Ctrl Pts',(3.09908550384732,6.01564277861007,57.0457563580462));
#61750=CARTESIAN_POINT('Ctrl Pts',(3.09908550384712,6.01564277861017,55.0459286315074));
#61751=CARTESIAN_POINT('Ctrl Pts',(2.93138389954939,6.10203780404269,55.0547844279169));
#61752=CARTESIAN_POINT('Ctrl Pts',(2.75991540541463,6.18149472625787,55.0636402243264));
#61753=CARTESIAN_POINT('Ctrl Pts',(2.58525146459081,6.25370001397821,55.0724960207359));
#61754=CARTESIAN_POINT('Ctrl Pts',(2.54694817563464,6.26953442139322,55.0744380708649));
#61755=CARTESIAN_POINT('Ctrl Pts',(2.50849132126405,6.28502025628159,55.0763801209939));
#61756=CARTESIAN_POINT('Ctrl Pts',(2.4698871053878,6.30015449704522,55.0783221711229));
#61757=CARTESIAN_POINT('Ctrl Pts',(2.3066830922166,6.36413633873944,55.0865324240095));
#61758=CARTESIAN_POINT('Ctrl Pts',(2.14100011934271,6.42176905429941,55.0947426768961));
#61759=CARTESIAN_POINT('Ctrl Pts',(1.97337352215316,6.47287308249319,55.1029529297827));
#61760=CARTESIAN_POINT('Ctrl Pts',(1.80570707583378,6.52398925942164,55.1111651344564));
#61761=CARTESIAN_POINT('Ctrl Pts',(1.63609642514703,6.56857355308037,55.1193773391301));
#61762=CARTESIAN_POINT('Ctrl Pts',(1.46509094013261,6.60649661599409,55.1275895438039));
#61763=CARTESIAN_POINT('Ctrl Pts',(1.29401435157499,6.64443544719818,55.1358051630865));
#61764=CARTESIAN_POINT('Ctrl Pts',(1.121542120486,6.67570745276881,55.1440207823692));
#61765=CARTESIAN_POINT('Ctrl Pts',(0.948232737877954,6.70023459849105,55.1522364016518));
#61766=CARTESIAN_POINT('Ctrl Pts',(0.774728735607956,6.72478928723916,55.1604612467537));
#61767=CARTESIAN_POINT('Ctrl Pts',(0.600386056726659,6.74258393808573,55.1686860918556));
#61768=CARTESIAN_POINT('Ctrl Pts',(0.425768208834028,6.75359240940303,55.1769109369575));
#61769=CARTESIAN_POINT('Ctrl Pts',(0.251038511608425,6.76460793206239,55.1851410503837));
#61770=CARTESIAN_POINT('Ctrl Pts',(0.0760336489349973,6.76882860149252,
55.1933711638098));
#61771=CARTESIAN_POINT('Ctrl Pts',(-0.0986840056641186,6.76628040115292,
55.201601277236));
#61772=CARTESIAN_POINT('Ctrl Pts',(-0.273641201045822,6.76372870718867,
55.2098426742832));
#61773=CARTESIAN_POINT('Ctrl Pts',(-0.448310047454821,6.75438962611889,
55.2180840713304));
#61774=CARTESIAN_POINT('Ctrl Pts',(-0.622133408069195,6.7383409695981,55.2263254683777));
#61775=CARTESIAN_POINT('Ctrl Pts',(-0.697785100789709,6.73135624655859,
55.2299123029366));
#61776=CARTESIAN_POINT('Ctrl Pts',(-0.773276771492053,6.72310126585528,
55.2334991374956));
#61777=CARTESIAN_POINT('Ctrl Pts',(-0.848563193888382,6.71358544341084,
55.2370859720545));
#61778=CARTESIAN_POINT('Ctrl Pts',(-1.02589409518704,6.69117171571653,55.2455344622989));
#61779=CARTESIAN_POINT('Ctrl Pts',(-1.20248990432317,6.66170833558372,55.2539829525433));
#61780=CARTESIAN_POINT('Ctrl Pts',(-1.37776768511531,6.62525812371503,55.2624314427876));
#61781=CARTESIAN_POINT('Ctrl Pts',(-1.55288535925302,6.58884120711885,55.2708722157988));
#61782=CARTESIAN_POINT('Ctrl Pts',(-1.72668707997948,6.54545024778862,55.2793129888099));
#61783=CARTESIAN_POINT('Ctrl Pts',(-1.89859720039446,6.49519958666817,55.2877537618211));
#61784=CARTESIAN_POINT('Ctrl Pts',(-2.0703767266301,6.44498709923891,55.2961881226686));
#61785=CARTESIAN_POINT('Ctrl Pts',(-2.2402671982649,6.38792539158564,55.3046224835162));
#61786=CARTESIAN_POINT('Ctrl Pts',(-2.40770490801787,6.32417947847044,55.3130568443637));
#61787=CARTESIAN_POINT('Ctrl Pts',(-2.57504113436593,6.26047220152819,55.3214860931749));
#61788=CARTESIAN_POINT('Ctrl Pts',(-2.73992725189055,6.19008891465632,55.3299153419861));
#61789=CARTESIAN_POINT('Ctrl Pts',(-2.90181604565359,6.11324403546819,55.3383445907973));
#61790=CARTESIAN_POINT('Ctrl Pts',(-3.06363155267199,6.03643394380863,55.3467700237038));
#61791=CARTESIAN_POINT('Ctrl Pts',(-3.22245214084822,5.95316823537392,55.3551954566103));
#61792=CARTESIAN_POINT('Ctrl Pts',(-3.3777515039518,5.86370904612016,55.3636208895168));
#61793=CARTESIAN_POINT('Ctrl Pts',(-3.53301675259904,5.77426950827735,55.3720444716168));
#61794=CARTESIAN_POINT('Ctrl Pts',(-3.68476202841597,5.67863936622023,55.3804680537169));
#61795=CARTESIAN_POINT('Ctrl Pts',(-3.83248605746805,5.57712646613944,55.388891635817));
#61796=CARTESIAN_POINT('Ctrl Pts',(-3.98019355747117,5.47562492447954,55.3973142753906));
#61797=CARTESIAN_POINT('Ctrl Pts',(-4.12388043297538,5.36824212580545,55.4057369149642));
#61798=CARTESIAN_POINT('Ctrl Pts',(-4.26307455523596,5.25532913683812,55.4141595545379));
#61799=CARTESIAN_POINT('Ctrl Pts',(-4.40227251308705,5.14241303647513,55.4225824262032));
#61800=CARTESIAN_POINT('Ctrl Pts',(-4.53697721219067,5.02396665233598,55.4310052978685));
#61801=CARTESIAN_POINT('Ctrl Pts',(-4.66674948477618,4.90038143886181,55.4394281695338));
#61802=CARTESIAN_POINT('Ctrl Pts',(-4.7965434307853,4.77677558527221,55.447852447913));
#61803=CARTESIAN_POINT('Ctrl Pts',(-4.92140306693598,4.64802942159968,55.4562767262923));
#61804=CARTESIAN_POINT('Ctrl Pts',(-5.04092572206951,4.51457161473578,55.4647010046716));
#61805=CARTESIAN_POINT('Ctrl Pts',(-5.16052909986028,4.3810236737564,55.4731309726009));
#61806=CARTESIAN_POINT('Ctrl Pts',(-5.27478807145375,4.24275797959035,55.4815609405303));
#61807=CARTESIAN_POINT('Ctrl Pts',(-5.38333929291249,4.10023743914721,55.4899909084597));
#61808=CARTESIAN_POINT('Ctrl Pts',(-5.491929320432,3.95766594892497,55.4984238900248));
#61809=CARTESIAN_POINT('Ctrl Pts',(-5.59480733211847,3.81083684841703,55.50685687159));
#61810=CARTESIAN_POINT('Ctrl Pts',(-5.69165273767726,3.660242903646,55.5152898531552));
#61811=CARTESIAN_POINT('Ctrl Pts',(-5.78858724190164,3.50951041105802,55.5237305931411));
#61812=CARTESIAN_POINT('Ctrl Pts',(-5.87947787598317,3.35500643774,55.532171333127));
#61813=CARTESIAN_POINT('Ctrl Pts',(-5.96404896081116,3.19725022371527,55.540612073113));
#61814=CARTESIAN_POINT('Ctrl Pts',(-6.01081113704409,3.11002154624153,55.5452792400479));
#61815=CARTESIAN_POINT('Ctrl Pts',(-6.05564202835132,3.0217989628261,55.5499464069828));
#61816=CARTESIAN_POINT('Ctrl Pts',(-6.09850128228028,2.93267303155769,55.5546135739177));
#61817=CARTESIAN_POINT('Ctrl Pts',(-6.17399149377114,2.77569093821738,55.5628340954312));
#61818=CARTESIAN_POINT('Ctrl Pts',(-6.24350787023843,2.6156021268131,55.5710546169448));
#61819=CARTESIAN_POINT('Ctrl Pts',(-6.30678734622761,2.45290080709826,55.5792751384584));
#61820=CARTESIAN_POINT('Ctrl Pts',(-6.37000755867763,2.29035186310843,55.5874879611535));
#61821=CARTESIAN_POINT('Ctrl Pts',(-6.42700237321618,2.12519561424854,55.5957007838486));
#61822=CARTESIAN_POINT('Ctrl Pts',(-6.47755534204111,1.9579493841248,55.6039136065437));
#61823=CARTESIAN_POINT('Ctrl Pts',(-6.52806387776402,1.7908501536527,55.6121192106482));
#61824=CARTESIAN_POINT('Ctrl Pts',(-6.5721417481635,1.62166494372084,55.6203248147527));
#61825=CARTESIAN_POINT('Ctrl Pts',(-6.60962124146166,1.45092937265011,55.6285304188571));
#61826=CARTESIAN_POINT('Ctrl Pts',(-6.6470813752321,1.28028199274019,55.6367317844672));
#61827=CARTESIAN_POINT('Ctrl Pts',(-6.67794984266258,1.10808619492482,55.6449331500773));
#61828=CARTESIAN_POINT('Ctrl Pts',(-6.70210915377087,0.934891379220476,
55.6531345156874));
#61829=CARTESIAN_POINT('Ctrl Pts',(-6.72626158895542,0.761745856078312,
55.6613335471265));
#61830=CARTESIAN_POINT('Ctrl Pts',(-6.74370861889685,0.587602234875273,
55.6695325785656));
#61831=CARTESIAN_POINT('Ctrl Pts',(-6.75438408941495,0.413018852666844,
55.6777316100046));
#61832=CARTESIAN_POINT('Ctrl Pts',(-6.76279155916818,0.275525661819018,
55.6841887594776));
#61833=CARTESIAN_POINT('Ctrl Pts',(-6.76700007299065,0.137759960526222,
55.6906459089506));
#61834=CARTESIAN_POINT('Ctrl Pts',(-6.76699999999905,-3.5853761194E-6,55.6971030584236));
#61835=CARTESIAN_POINT('',(-6.76699931626774,0.0030419782871798,55.3028202162181));
#61836=CARTESIAN_POINT('Ctrl Pts',(3.09908550384732,6.01564277861007,54.6514561368909));
#61837=CARTESIAN_POINT('Ctrl Pts',(2.94227848457418,6.09642522833577,54.6597666288178));
#61838=CARTESIAN_POINT('Ctrl Pts',(2.78218626615245,6.17113690883049,54.6680771207447));
#61839=CARTESIAN_POINT('Ctrl Pts',(2.61931417507843,6.23950977659569,54.6763876126716));
#61840=CARTESIAN_POINT('Ctrl Pts',(2.45655077372096,6.30783701697582,54.6846925587435));
#61841=CARTESIAN_POINT('Ctrl Pts',(2.29101151582971,6.36983373938531,54.6929975048154));
#61842=CARTESIAN_POINT('Ctrl Pts',(2.1232244900123,6.42527873053084,54.7013024508872));
#61843=CARTESIAN_POINT('Ctrl Pts',(1.95551871884651,6.48069687118887,54.7096033751016));
#61844=CARTESIAN_POINT('Ctrl Pts',(1.78556767865217,6.52956949477253,54.717904299316));
#61845=CARTESIAN_POINT('Ctrl Pts',(1.61391772826252,6.57172416998766,54.7262052235304));
#61846=CARTESIAN_POINT('Ctrl Pts',(1.44231949193471,6.61386614499824,54.7345036468731));
#61847=CARTESIAN_POINT('Ctrl Pts',(1.2690237030364,6.64929412309598,54.7428020702157));
#61848=CARTESIAN_POINT('Ctrl Pts',(1.09459033265363,6.67788596815349,54.7511004935584));
#61849=CARTESIAN_POINT('Ctrl Pts',(0.920140701170592,6.70648047861188,54.7593996905001));
#61850=CARTESIAN_POINT('Ctrl Pts',(0.744553618279898,6.72823751880162,54.7676988874419));
#61851=CARTESIAN_POINT('Ctrl Pts',(0.568398247883257,6.74308626904649,54.7759980843837));
#61852=CARTESIAN_POINT('Ctrl Pts',(0.39222614389965,6.75793642982373,54.7842980696939));
#61853=CARTESIAN_POINT('Ctrl Pts',(0.215485991550797,6.76587696282492,54.792598055004));
#61854=CARTESIAN_POINT('Ctrl Pts',(0.0387509799454699,6.76688904605013,
54.8008980403142));
#61855=CARTESIAN_POINT('Ctrl Pts',(-0.138030158621772,6.76790139342405,
54.8092001918794));
#61856=CARTESIAN_POINT('Ctrl Pts',(-0.314805805832689,6.76198168490955,
54.8175023434447));
#61857=CARTESIAN_POINT('Ctrl Pts',(-0.491003677021281,6.74916323622059,
54.8258044950099));
#61858=CARTESIAN_POINT('Ctrl Pts',(-0.667276787544288,6.73633931384718,
54.8341101917278));
#61859=CARTESIAN_POINT('Ctrl Pts',(-0.842971283549303,6.7166108053603,54.8424158884456));
#61860=CARTESIAN_POINT('Ctrl Pts',(-1.01752070452666,6.69006282600243,54.8507215851635));
#61861=CARTESIAN_POINT('Ctrl Pts',(-1.19227617906004,6.6634835070645,54.8590370866595));
#61862=CARTESIAN_POINT('Ctrl Pts',(-1.36588353342741,6.6300686850292,54.8673525881556));
#61863=CARTESIAN_POINT('Ctrl Pts',(-1.5377860191125,6.58995471603729,54.8756680896516));
#61864=CARTESIAN_POINT('Ctrl Pts',(-1.70979624110599,6.54981560644944,54.8839888027153));
#61865=CARTESIAN_POINT('Ctrl Pts',(-1.88009912856106,6.50296906899714,54.892309515779));
#61866=CARTESIAN_POINT('Ctrl Pts',(-2.04815363330913,6.44960120428873,54.9006302288426));
#61867=CARTESIAN_POINT('Ctrl Pts',(-2.21645978561914,6.3961534256675,54.908963401478));
#61868=CARTESIAN_POINT('Ctrl Pts',(-2.3825104995194,6.33616492192162,54.9172965741135));
#61869=CARTESIAN_POINT('Ctrl Pts',(-2.54578394029261,6.26987026415605,54.9256297467489));
#61870=CARTESIAN_POINT('Ctrl Pts',(-2.6722392270364,6.21852504892921,54.9320837893053));
#61871=CARTESIAN_POINT('Ctrl Pts',(-2.79702896078766,6.16339806925064,54.9385378318618));
#61872=CARTESIAN_POINT('Ctrl Pts',(-2.91992138371005,6.10461695055085,54.9449918744183));
#61873=CARTESIAN_POINT('Ctrl Pts',(-3.07361041589699,6.03110539443531,54.9530632878595));
#61874=CARTESIAN_POINT('Ctrl Pts',(-3.22480427228096,5.95165085645071,54.9611347013008));
#61875=CARTESIAN_POINT('Ctrl Pts',(-3.37299810815277,5.86644464410923,54.969206114742));
#61876=CARTESIAN_POINT('Ctrl Pts',(-3.52100589893652,5.78134540111087,54.9772673951921));
#61877=CARTESIAN_POINT('Ctrl Pts',(-3.66602084390755,5.69050903474158,54.9853286756422));
#61878=CARTESIAN_POINT('Ctrl Pts',(-3.80755761490248,5.59417500702276,54.9933899560923));
#61879=CARTESIAN_POINT('Ctrl Pts',(-3.9489477378689,5.49794079220164,55.0014428841483));
#61880=CARTESIAN_POINT('Ctrl Pts',(-4.08686655277689,5.39622045970253,55.0094958122044));
#61881=CARTESIAN_POINT('Ctrl Pts',(-4.22085301193727,5.28929946700128,55.0175487402604));
#61882=CARTESIAN_POINT('Ctrl Pts',(-4.35472998599872,5.18246584324418,55.0255950879826));
#61883=CARTESIAN_POINT('Ctrl Pts',(-4.48468070977489,5.07044024897661,55.0336414357049));
#61884=CARTESIAN_POINT('Ctrl Pts',(-4.61027293592524,4.95355149930585,55.0416877834271));
#61885=CARTESIAN_POINT('Ctrl Pts',(-4.73579000928887,4.83673269437247,55.0497293163175));
#61886=CARTESIAN_POINT('Ctrl Pts',(-4.85695350461245,4.71505678056249,55.0577708492078));
#61887=CARTESIAN_POINT('Ctrl Pts',(-4.97336420201081,4.58889284186909,55.0658123820982));
#61888=CARTESIAN_POINT('Ctrl Pts',(-5.09201285980435,4.46030343967101,55.0740085110225));
#61889=CARTESIAN_POINT('Ctrl Pts',(-5.20572380913926,4.32705194261169,55.0822046399468));
#61890=CARTESIAN_POINT('Ctrl Pts',(-5.31411341305573,4.18956890779722,55.0904007688711));
#61891=CARTESIAN_POINT('Ctrl Pts',(-5.42042185434818,4.05472565155148,55.0984395259021));
#61892=CARTESIAN_POINT('Ctrl Pts',(-5.52161122379691,3.91581219988204,55.1064782829332));
#61893=CARTESIAN_POINT('Ctrl Pts',(-5.61736028292918,3.77326813939453,55.1145170399642));
#61894=CARTESIAN_POINT('Ctrl Pts',(-5.71311860954653,3.63071028216618,55.122556575061));
#61895=CARTESIAN_POINT('Ctrl Pts',(-5.80343536901764,3.48452142639071,55.1305961101577));
#61896=CARTESIAN_POINT('Ctrl Pts',(-5.88803290230934,3.33516979197801,55.1386356452545));
#61897=CARTESIAN_POINT('Ctrl Pts',(-5.9726553740777,3.18577413025029,55.1466775503229));
#61898=CARTESIAN_POINT('Ctrl Pts',(-6.05155507982264,3.03321415884263,55.1547194553913));
#61899=CARTESIAN_POINT('Ctrl Pts',(-6.12450059982879,2.87798217553494,55.1627613604598));
#61900=CARTESIAN_POINT('Ctrl Pts',(-6.19990673361083,2.71751387399201,55.1710745367782));
#61901=CARTESIAN_POINT('Ctrl Pts',(-6.26894977373616,2.55419053669711,55.1793877130967));
#61902=CARTESIAN_POINT('Ctrl Pts',(-6.33142877094932,2.38857671394394,55.1877008894152));
#61903=CARTESIAN_POINT('Ctrl Pts',(-6.39197392511329,2.22808895201547,55.1957567572147));
#61904=CARTESIAN_POINT('Ctrl Pts',(-6.44635527403393,2.06545075447282,55.2038126250141));
#61905=CARTESIAN_POINT('Ctrl Pts',(-6.49444137014837,1.90118917777936,55.2118684928136));
#61906=CARTESIAN_POINT('Ctrl Pts',(-6.54483130785059,1.72905770350139,55.2203103233916));
#61907=CARTESIAN_POINT('Ctrl Pts',(-6.58830781395067,1.55514393992903,55.2287521539696));
#61908=CARTESIAN_POINT('Ctrl Pts',(-6.62478034910879,1.38006316017131,55.2371939845475));
#61909=CARTESIAN_POINT('Ctrl Pts',(-6.66125288426691,1.20498238041358,55.2456358151255));
#61910=CARTESIAN_POINT('Ctrl Pts',(-6.69072145685252,1.02873505337369,55.2540776457034));
#61911=CARTESIAN_POINT('Ctrl Pts',(-6.71315796159003,0.85193848530306,55.2625194762814));
#61912=CARTESIAN_POINT('Ctrl Pts',(-6.74886142398984,0.570600117568218,
55.2759530562508));
#61913=CARTESIAN_POINT('Ctrl Pts',(-6.76687162267472,0.287101299100329,
55.2893866362202));
#61914=CARTESIAN_POINT('Ctrl Pts',(-6.76699931626747,0.00304197888748282,
55.3028202161897));
#61915=CARTESIAN_POINT('Ctrl Pts',(-6.76699931626774,0.0030419782871798,
55.3028202162181));
#61916=CARTESIAN_POINT('Ctrl Pts',(-6.76707603531081,-0.167622524530384,
55.3108911897205));
#61917=CARTESIAN_POINT('Ctrl Pts',(-6.76069231177937,-0.338562701080097,
55.3189621632228));
#61918=CARTESIAN_POINT('Ctrl Pts',(-6.74781185599331,-0.509238800678179,
55.3270331367252));
#61919=CARTESIAN_POINT('Ctrl Pts',(-6.7349453089077,-0.679730599131792,
55.3350953949496));
#61920=CARTESIAN_POINT('Ctrl Pts',(-6.71559601838924,-0.849958519438639,
55.3431576531739));
#61921=CARTESIAN_POINT('Ctrl Pts',(-6.68977966328148,-1.01938072217672,
55.3512199113983));
#61922=CARTESIAN_POINT('Ctrl Pts',(-6.66398552832,-1.18865710316302,55.3592752304341));
#61923=CARTESIAN_POINT('Ctrl Pts',(-6.63173546357944,-1.35712878009417,
55.3673305494698));
#61924=CARTESIAN_POINT('Ctrl Pts',(-6.59309710352087,-1.52425705953581,
55.3753858685056));
#61925=CARTESIAN_POINT('Ctrl Pts',(-6.55448354241268,-1.69127807236716,
55.3834360174602));
#61926=CARTESIAN_POINT('Ctrl Pts',(-6.50948993230037,-1.85695704176339,
55.3914861664149));
#61927=CARTESIAN_POINT('Ctrl Pts',(-6.45823531313495,-2.02076362798245,
55.3995363153695));
#61928=CARTESIAN_POINT('Ctrl Pts',(-6.4069980401316,-2.18451477694257,55.4075837399026));
#61929=CARTESIAN_POINT('Ctrl Pts',(-6.34950408402667,-2.34639444737347,
55.4156311644356));
#61930=CARTESIAN_POINT('Ctrl Pts',(-6.28592285366406,-2.50588564738774,
55.4236785889687));
#61931=CARTESIAN_POINT('Ctrl Pts',(-6.22235112075414,-2.66535302338795,
55.4317248114169));
#61932=CARTESIAN_POINT('Ctrl Pts',(-6.15269406092773,-2.82243229206626,
55.4397710338652));
#61933=CARTESIAN_POINT('Ctrl Pts',(-6.0771698586151,-2.97662485199936,55.4478172563134));
#61934=CARTESIAN_POINT('Ctrl Pts',(-6.00164198210172,-3.13082491329496,
55.4558638702049));
#61935=CARTESIAN_POINT('Ctrl Pts',(-5.9202465595136,-3.2821376510774,55.4639104840963));
#61936=CARTESIAN_POINT('Ctrl Pts',(-5.83324844597768,-3.4300876909343,55.4719570979878));
#61937=CARTESIAN_POINT('Ctrl Pts',(-5.74622886969504,-3.57807423059681,
55.4800056970077));
#61938=CARTESIAN_POINT('Ctrl Pts',(-5.65360404128081,-3.72269609982622,
55.4880542960277));
#61939=CARTESIAN_POINT('Ctrl Pts',(-5.55568289035785,-3.86350574242942,
55.4961028950476));
#61940=CARTESIAN_POINT('Ctrl Pts',(-5.45767045548426,-4.00444665044709,
55.504158997124));
#61941=CARTESIAN_POINT('Ctrl Pts',(-5.35435205319902,-4.14156792933665,
55.5122150992003));
#61942=CARTESIAN_POINT('Ctrl Pts',(-5.24607815011016,-4.27445353734682,
55.5202712012767));
#61943=CARTESIAN_POINT('Ctrl Pts',(-5.13774703862206,-4.40740935777846,
55.5283315599346));
#61944=CARTESIAN_POINT('Ctrl Pts',(-5.0244554574765,-4.53612477036807,55.5363919185925));
#61945=CARTESIAN_POINT('Ctrl Pts',(-4.90659133798229,-4.66021999931732,
55.5444522772505));
#61946=CARTESIAN_POINT('Ctrl Pts',(-4.78857774209641,-4.78447260701023,
55.5525228581315));
#61947=CARTESIAN_POINT('Ctrl Pts',(-4.6659802964762,-4.90409307297317,55.5605934390126));
#61948=CARTESIAN_POINT('Ctrl Pts',(-4.53922117807697,-5.01874088756309,
55.5686640198936));
#61949=CARTESIAN_POINT('Ctrl Pts',(-4.47962586311644,-5.07264211933486,
55.5724583726439));
#61950=CARTESIAN_POINT('Ctrl Pts',(-4.4191111051235,-5.12544481452318,55.5762527253942));
#61951=CARTESIAN_POINT('Ctrl Pts',(-4.3577229824208,-5.17711690117981,55.5800470781445));
#61952=CARTESIAN_POINT('Ctrl Pts',(-4.21316232017549,-5.29879762275609,
55.5889822617309));
#61953=CARTESIAN_POINT('Ctrl Pts',(-4.06341051789947,-5.41449746818261,
55.5979174453173));
#61954=CARTESIAN_POINT('Ctrl Pts',(-3.90896481314798,-5.52379245533094,
55.6068526289037));
#61955=CARTESIAN_POINT('Ctrl Pts',(-3.75475041987423,-5.6329237526892,55.6157744303729));
#61956=CARTESIAN_POINT('Ctrl Pts',(-3.5958563617981,-5.73566918320373,55.6246962318421));
#61957=CARTESIAN_POINT('Ctrl Pts',(-3.43281197432303,-5.8316456467231,55.6336180333113));
#61958=CARTESIAN_POINT('Ctrl Pts',(-3.27016528922406,-5.92738800180008,
55.6425180724758));
#61959=CARTESIAN_POINT('Ctrl Pts',(-3.10338870192026,-6.01639421231828,
55.6514181116403));
#61960=CARTESIAN_POINT('Ctrl Pts',(-2.93303892282319,-6.09832531742971,
55.6603181508048));
#61961=CARTESIAN_POINT('Ctrl Pts',(-2.76295139848448,-6.18013028899235,
55.6692044882925));
#61962=CARTESIAN_POINT('Ctrl Pts',(-2.58930188697861,-6.25488177080588,
55.6780908257801));
#61963=CARTESIAN_POINT('Ctrl Pts',(-2.41267260699273,-6.32228597039607,
55.6869771632678));
#61964=CARTESIAN_POINT('Ctrl Pts',(-2.23649493445352,-6.38951783027862,
55.695840780082));
#61965=CARTESIAN_POINT('Ctrl Pts',(-2.05735293670873,-6.44943980161332,
55.7047043968963));
#61966=CARTESIAN_POINT('Ctrl Pts',(-1.87584905849836,-6.50180584989515,
55.7135680137106));
#61967=CARTESIAN_POINT('Ctrl Pts',(-1.7035462594288,-6.55151727636238,55.7219823021657));
#61968=CARTESIAN_POINT('Ctrl Pts',(-1.52911532216133,-6.59441967566255,
55.7303965906208));
#61969=CARTESIAN_POINT('Ctrl Pts',(-1.35308947604772,-6.63034221362736,
55.7388108790758));
#61970=CARTESIAN_POINT('Ctrl Pts',(-1.18133202812021,-6.66539367669451,
55.7470211319624));
#61971=CARTESIAN_POINT('Ctrl Pts',(-1.00822094912745,-6.69376499554051,
55.755231384849));
#61972=CARTESIAN_POINT('Ctrl Pts',(-0.834314434246282,-6.71537105637569,
55.7634416377356));
#61973=CARTESIAN_POINT('Ctrl Pts',(-0.660366577337444,-6.73698225352428,
55.7716538424094));
#61974=CARTESIAN_POINT('Ctrl Pts',(-0.485623261046444,-6.75182494463065,
55.7798660470832));
#61975=CARTESIAN_POINT('Ctrl Pts',(-0.310647897739216,-6.75986589242939,
55.7880782517569));
#61976=CARTESIAN_POINT('Ctrl Pts',(-0.13559978022844,-6.76791018362884,
55.7962938710394));
#61977=CARTESIAN_POINT('Ctrl Pts',(0.0396802212367957,-6.76914708091198,
55.804509490322));
#61978=CARTESIAN_POINT('Ctrl Pts',(0.214628506536059,-6.76359546426175,
55.8127251096046));
#61979=CARTESIAN_POINT('Ctrl Pts',(0.389773251922865,-6.75803761336297,
55.8209499547065));
#61980=CARTESIAN_POINT('Ctrl Pts',(0.564585181229354,-6.74567603375523,
55.8291747998084));
#61981=CARTESIAN_POINT('Ctrl Pts',(0.738504649515448,-6.72658158968165,
55.8373996449103));
#61982=CARTESIAN_POINT('Ctrl Pts',(0.91253551979508,-6.70747491489488,55.8456297583364));
#61983=CARTESIAN_POINT('Ctrl Pts',(1.08567243835513,-6.68162683100076,55.8538598717626));
#61984=CARTESIAN_POINT('Ctrl Pts',(1.25736581488153,-6.64915936096942,55.8620899851887));
#61985=CARTESIAN_POINT('Ctrl Pts',(1.42929458585647,-6.61664737750164,55.8703313822359));
#61986=CARTESIAN_POINT('Ctrl Pts',(1.59977551582118,-6.57749796039881,55.8785727792831));
#61987=CARTESIAN_POINT('Ctrl Pts',(1.76827306004991,-6.53188329542879,55.8868141763304));
#61988=CARTESIAN_POINT('Ctrl Pts',(1.8416068420885,-6.51203080491336,55.8904010108894));
#61989=CARTESIAN_POINT('Ctrl Pts',(1.91456517407644,-6.49095430506856,55.8939878454485));
#61990=CARTESIAN_POINT('Ctrl Pts',(1.98710511392414,-6.4686708268559,55.8975746800075));
#61991=CARTESIAN_POINT('Ctrl Pts',(2.15796690418466,-6.4161839487493,55.9060231702519));
#61992=CARTESIAN_POINT('Ctrl Pts',(2.32689575810249,-6.35687785389252,55.9144716604962));
#61993=CARTESIAN_POINT('Ctrl Pts',(2.49332814330936,-6.29091438264594,55.9229201507406));
#61994=CARTESIAN_POINT('Ctrl Pts',(2.65960850164581,-6.22501116541832,55.9313609237517));
#61995=CARTESIAN_POINT('Ctrl Pts',(2.82339662827288,-6.15246281564555,55.9398016967628));
#61996=CARTESIAN_POINT('Ctrl Pts',(2.98414500579366,-6.07348068115778,55.948242469774));
#61997=CARTESIAN_POINT('Ctrl Pts',(3.14477126832602,-5.99455854666869,55.9566768306215));
#61998=CARTESIAN_POINT('Ctrl Pts',(3.30236208692806,-5.90921251732464,55.965111191469));
#61999=CARTESIAN_POINT('Ctrl Pts',(3.45639039551898,-5.81770181719243,55.9735455523165));
#62000=CARTESIAN_POINT('Ctrl Pts',(3.61032534809626,-5.72624658137226,55.9819748011277));
#62001=CARTESIAN_POINT('Ctrl Pts',(3.76070180963412,-5.62863429403779,55.9904040499389));
#62002=CARTESIAN_POINT('Ctrl Pts',(3.9070174327515,-5.5251700227392,55.99883329875));
#62003=CARTESIAN_POINT('Ctrl Pts',(4.05326681906635,-5.42175258951819,56.0072587316564));
#62004=CARTESIAN_POINT('Ctrl Pts',(4.19545876082964,-5.31248864703721,56.0156841645628));
#62005=CARTESIAN_POINT('Ctrl Pts',(4.33311969149858,-5.19772668953911,56.0241095974692));
#62006=CARTESIAN_POINT('Ctrl Pts',(4.47075038233014,-5.08298994168413,56.0325331795693));
#62007=CARTESIAN_POINT('Ctrl Pts',(4.60385178898657,-4.96275779810857,56.0409567616693));
#62008=CARTESIAN_POINT('Ctrl Pts',(4.73198284397695,-4.83741949434901,56.0493803437694));
#62009=CARTESIAN_POINT('Ctrl Pts',(4.86009956220309,-4.71209521486881,56.057802983343));
#62010=CARTESIAN_POINT('Ctrl Pts',(4.98324679917651,-4.58166614729252,56.0662256229166));
#62011=CARTESIAN_POINT('Ctrl Pts',(5.10101961156118,-4.44655911042103,56.0746482624902));
#62012=CARTESIAN_POINT('Ctrl Pts',(5.2187956692579,-4.31144835058083,56.0830711341555));
#62013=CARTESIAN_POINT('Ctrl Pts',(5.33119678831939,-4.17165961602029,56.0914940058208));
#62014=CARTESIAN_POINT('Ctrl Pts',(5.43785742312932,-4.02765386369253,56.0999168774861));
#62015=CARTESIAN_POINT('Ctrl Pts',(5.54453587145941,-3.88362406079188,56.1083411558653));
#62016=CARTESIAN_POINT('Ctrl Pts',(5.64547172619947,-3.73537610422097,56.1167654342445));
#62017=CARTESIAN_POINT('Ctrl Pts',(5.74034177830179,-3.58340135461869,56.1251897126237));
#62018=CARTESIAN_POINT('Ctrl Pts',(5.83527590330132,-3.4313239650126,56.1336196805531));
#62019=CARTESIAN_POINT('Ctrl Pts',(5.92413586282424,-3.27551503597956,56.1420496484824));
#62020=CARTESIAN_POINT('Ctrl Pts',(6.00664306343095,-3.1164929180951,56.1504796164117));
#62021=CARTESIAN_POINT('Ctrl Pts',(6.08917975960071,-2.95741395127055,56.1589125979769));
#62022=CARTESIAN_POINT('Ctrl Pts',(6.16535902041043,-2.79511980391235,56.167345579542));
#62023=CARTESIAN_POINT('Ctrl Pts',(6.23494949256094,-2.6301509130113,56.1757785611072));
#62024=CARTESIAN_POINT('Ctrl Pts',(6.30460398858736,-2.46503024920979,56.1842193010931));
#62025=CARTESIAN_POINT('Ctrl Pts',(6.36765746086084,-2.29723023499947,56.192660041079));
#62026=CARTESIAN_POINT('Ctrl Pts',(6.42392734140331,-2.12730968887255,56.2011007810649));
#62027=CARTESIAN_POINT('Ctrl Pts',(6.45504083694441,-2.03335494606355,56.2057679480001));
#62028=CARTESIAN_POINT('Ctrl Pts',(6.48408123300088,-1.93875215309201,56.2104351149353));
#62029=CARTESIAN_POINT('Ctrl Pts',(6.51102430173953,-1.84359744579918,56.2151022818705));
#62030=CARTESIAN_POINT('Ctrl Pts',(6.55802361925107,-1.67761018042295,56.2232436581478));
#62031=CARTESIAN_POINT('Ctrl Pts',(6.59873134817497,-1.50961294844202,56.2313850344251));
#62032=CARTESIAN_POINT('Ctrl Pts',(6.63297410745331,-1.34012816172708,56.2395264107024));
#62033=CARTESIAN_POINT('Ctrl Pts',(6.66718697503581,-1.17079132417862,56.2476606800892));
#62034=CARTESIAN_POINT('Ctrl Pts',(6.69494603443017,-0.999969873007824,
56.2557949494759));
#62035=CARTESIAN_POINT('Ctrl Pts',(6.71612773974867,-0.82820117325347,56.2639292188626));
#62036=CARTESIAN_POINT('Ctrl Pts',(6.73729499542218,-0.656549649934848,
56.2720579392483));
#62037=CARTESIAN_POINT('Ctrl Pts',(6.75189378570168,-0.483952526390221,
56.280186659634));
#62038=CARTESIAN_POINT('Ctrl Pts',(6.7598516754522,-0.310957112615279,56.2883153800197));
#62039=CARTESIAN_POINT('Ctrl Pts',(6.7678057700652,-0.138044200785899,56.2964402237983));
#62040=CARTESIAN_POINT('Ctrl Pts',(6.76912525409912,0.0352662581381283,
56.3045650675769));
#62041=CARTESIAN_POINT('Ctrl Pts',(6.76378956125084,0.208422098430536,56.3126899113555));
#62042=CARTESIAN_POINT('Ctrl Pts',(6.758455362207,0.381529461239114,56.3208124804665));
#62043=CARTESIAN_POINT('Ctrl Pts',(6.74646970953452,0.554481926106745,56.3289350495774));
#62044=CARTESIAN_POINT('Ctrl Pts',(6.72786414533262,0.726727625694658,56.3370576186884));
#62045=CARTESIAN_POINT('Ctrl Pts',(6.70925759269357,0.898982475988572,56.3451806193181));
#62046=CARTESIAN_POINT('Ctrl Pts',(6.68403046137004,1.07053012163054,56.3533036199478));
#62047=CARTESIAN_POINT('Ctrl Pts',(6.65226615470249,1.24082392264162,56.3614266205775));
#62048=CARTESIAN_POINT('Ctrl Pts',(6.63605166653127,1.32775252621626,56.3655731079856));
#62049=CARTESIAN_POINT('Ctrl Pts',(6.61813460331876,1.41435453243038,56.3697195953938));
#62050=CARTESIAN_POINT('Ctrl Pts',(6.59853119987784,1.50055823087234,56.3738660828019));
#62051=CARTESIAN_POINT('Ctrl Pts',(6.55605905001241,1.68732459571376,56.3828497388871));
#62052=CARTESIAN_POINT('Ctrl Pts',(6.50568935920778,1.87212817942224,56.3918333949723));
#62053=CARTESIAN_POINT('Ctrl Pts',(6.44763550895984,2.05433330878904,56.4008170510576));
#62054=CARTESIAN_POINT('Ctrl Pts',(6.38948192194162,2.23685146737018,56.4098161411035));
#62055=CARTESIAN_POINT('Ctrl Pts',(6.3236178621624,2.41676202112508,56.4188152311494));
#62056=CARTESIAN_POINT('Ctrl Pts',(6.25030544246359,2.59344768135199,56.4278143211954));
#62057=CARTESIAN_POINT('Ctrl Pts',(6.17682112349692,2.7705476252127,56.4368345118542));
#62058=CARTESIAN_POINT('Ctrl Pts',(6.09585359318461,2.94440732441414,56.4458547025131));
#62059=CARTESIAN_POINT('Ctrl Pts',(6.00771289633479,3.11443008513799,56.4548748931719));
#62060=CARTESIAN_POINT('Ctrl Pts',(5.91948293339877,3.28462503949042,56.4639042191921));
#62061=CARTESIAN_POINT('Ctrl Pts',(5.82406540606469,3.45097508289248,56.4729335452124));
#62062=CARTESIAN_POINT('Ctrl Pts',(5.72181547411105,3.61290972489259,56.4819628712326));
#62063=CARTESIAN_POINT('Ctrl Pts',(5.61942138691336,3.77507266756136,56.4910049270871));
#62064=CARTESIAN_POINT('Ctrl Pts',(5.51017576246176,3.93280755960706,56.5000469829417));
#62065=CARTESIAN_POINT('Ctrl Pts',(5.39447740201476,4.08557248854456,56.5090890387963));
#62066=CARTESIAN_POINT('Ctrl Pts',(5.29407113723749,4.21814615548606,56.5169359871087));
#62067=CARTESIAN_POINT('Ctrl Pts',(5.18880587225101,4.34697723133431,56.5247829354212));
#62068=CARTESIAN_POINT('Ctrl Pts',(5.07896658780163,4.47173203579941,56.5326298837336));
#62069=CARTESIAN_POINT('Ctrl Pts',(4.95782024282555,4.6093293322031,56.541284611521));
#62070=CARTESIAN_POINT('Ctrl Pts',(4.83100187746522,4.74208834403588,56.5499393393084));
#62071=CARTESIAN_POINT('Ctrl Pts',(4.69891621343056,4.86954570973098,56.5585940670958));
#62072=CARTESIAN_POINT('Ctrl Pts',(4.56699455858291,4.99684481314169,56.5672380484114));
#62073=CARTESIAN_POINT('Ctrl Pts',(4.42981887556032,5.11885519753723,56.5758820297269));
#62074=CARTESIAN_POINT('Ctrl Pts',(4.28783143721378,5.23514952661729,56.5845260110424));
#62075=CARTESIAN_POINT('Ctrl Pts',(4.14595390111223,5.3513538406369,56.5931633016749));
#62076=CARTESIAN_POINT('Ctrl Pts',(3.99927227098851,5.46185073004917,56.6018005923074));
#62077=CARTESIAN_POINT('Ctrl Pts',(3.84826372117765,5.5662514614656,56.6104378829399));
#62078=CARTESIAN_POINT('Ctrl Pts',(3.69739703195112,5.67055411665535,56.6190670595212));
#62079=CARTESIAN_POINT('Ctrl Pts',(3.5422117836102,5.76877186920301,56.6276962361025));
#62080=CARTESIAN_POINT('Ctrl Pts',(3.38321630546358,5.86055768937098,56.6363254126838));
#62081=CARTESIAN_POINT('Ctrl Pts',(3.28978520604009,5.91449412951221,56.6413962075549));
#62082=CARTESIAN_POINT('Ctrl Pts',(3.19503897899121,5.96621031813891,56.646467002426));
#62083=CARTESIAN_POINT('Ctrl Pts',(3.09908550384732,6.01564277861007,56.6515377972971));
#62084=CARTESIAN_POINT('Origin',(0.,0.,-63.6971797838103));
#62085=CARTESIAN_POINT('',(3.0990855038472,6.01564277861012,59.0457563580462));
#62086=CARTESIAN_POINT('',(3.09908550384712,6.01564277861017,58.6513967904261));
#62087=CARTESIAN_POINT('',(3.09908550384721,6.01564277861012,-63.6971797838103));
#62088=CARTESIAN_POINT('',(-6.767,-6.2375472749954E-10,57.6971797838394));
#62089=CARTESIAN_POINT('Ctrl Pts',(-6.767,-6.23560221358631E-10,57.6971797838395));
#62090=CARTESIAN_POINT('Ctrl Pts',(-6.76699999998286,-0.186007250183476,
57.7059292956522));
#62091=CARTESIAN_POINT('Ctrl Pts',(-6.75932637290819,-0.372014356438861,
57.7146788074649));
#62092=CARTESIAN_POINT('Ctrl Pts',(-6.74400518258228,-0.557389538207732,
57.7234283192776));
#62093=CARTESIAN_POINT('Ctrl Pts',(-6.72868405696884,-0.742763937002891,
57.7321777941348));
#62094=CARTESIAN_POINT('Ctrl Pts',(-6.70571545635014,-0.927506131023182,
57.7409272689921));
#62095=CARTESIAN_POINT('Ctrl Pts',(-6.6751773939133,-1.11098864071098,57.7496767438493));
#62096=CARTESIAN_POINT('Ctrl Pts',(-6.64463945792454,-1.29447039065802,
57.7584261824778));
#62097=CARTESIAN_POINT('Ctrl Pts',(-6.60653216989111,-1.47669218400177,
57.7671756211063));
#62098=CARTESIAN_POINT('Ctrl Pts',(-6.56098496070208,-1.65703510688252,
57.7759250597348));
#62099=CARTESIAN_POINT('Ctrl Pts',(-6.5154379363262,-1.83737729800064,57.7846744628614));
#62100=CARTESIAN_POINT('Ctrl Pts',(-6.46245112138313,-2.01584035604526,
57.7934238659881));
#62101=CARTESIAN_POINT('Ctrl Pts',(-6.4022044834151,-2.19181813856434,57.8021732691147));
#62102=CARTESIAN_POINT('Ctrl Pts',(-6.34195808490141,-2.36779522164779,
57.8109226374662));
#62103=CARTESIAN_POINT('Ctrl Pts',(-6.2744520139292,-2.54128677783604,57.8196720058178));
#62104=CARTESIAN_POINT('Ctrl Pts',(-6.19991555027716,-2.71170355485836,
57.8284213741693));
#62105=CARTESIAN_POINT('Ctrl Pts',(-6.12537937668529,-2.88211966870033,
57.8371707084725));
#62106=CARTESIAN_POINT('Ctrl Pts',(-6.04381298000202,-3.04946076475658,
57.8459200427757));
#62107=CARTESIAN_POINT('Ctrl Pts',(-5.95549339279206,-3.213158484795,57.8546693770788));
#62108=CARTESIAN_POINT('Ctrl Pts',(-5.86717414194521,-3.37685558139444,
57.8634186780604));
#62109=CARTESIAN_POINT('Ctrl Pts',(-5.772101888113,-3.53690907753474,57.872167979042));
#62110=CARTESIAN_POINT('Ctrl Pts',(-5.67059953277166,-3.69277537076518,
57.8809172800235));
#62111=CARTESIAN_POINT('Ctrl Pts',(-5.56909755557055,-3.84864108332618,
57.8896665484101));
#62112=CARTESIAN_POINT('Ctrl Pts',(-5.46116568117904,-4.00031938405425,
57.8984158167967));
#62113=CARTESIAN_POINT('Ctrl Pts',(-5.3471704844995,-4.14729511967709,57.9071650851834));
#62114=CARTESIAN_POINT('Ctrl Pts',(-5.2331757030352,-4.29427031995662,57.9159143217017));
#62115=CARTESIAN_POINT('Ctrl Pts',(-5.11311781910449,-4.43654276296921,
57.9246635582201));
#62116=CARTESIAN_POINT('Ctrl Pts',(-4.9874045888688,-4.57362924458579,57.9334127947384));
#62117=CARTESIAN_POINT('Ctrl Pts',(-4.86169180609106,-4.710715238263,57.9421620001151));
#62118=CARTESIAN_POINT('Ctrl Pts',(-4.73032391096716,-4.84261509628306,
57.9509112054918));
#62119=CARTESIAN_POINT('Ctrl Pts',(-4.59374706901301,-4.9688808464215,57.9596604108686));
#62120=CARTESIAN_POINT('Ctrl Pts',(-4.45717070184369,-5.09514615761976,
57.9684095858302));
#62121=CARTESIAN_POINT('Ctrl Pts',(-4.31538563449167,-5.21577720560456,
57.9771587607919));
#62122=CARTESIAN_POINT('Ctrl Pts',(-4.16887340902849,-5.33036429331947,
57.9859079357536));
#62123=CARTESIAN_POINT('Ctrl Pts',(-4.02236168072287,-5.44495099220788,
57.9946570810268));
#62124=CARTESIAN_POINT('Ctrl Pts',(-3.87112305211999,-5.55349359533604,
58.0034062263001));
#62125=CARTESIAN_POINT('Ctrl Pts',(-3.7156711687689,-5.65562346391444,58.0121553715733));
#62126=CARTESIAN_POINT('Ctrl Pts',(-3.56021980000273,-5.75775299441722,
58.0209044878847));
#62127=CARTESIAN_POINT('Ctrl Pts',(-3.40055544388173,-5.85346967551198,
58.029653604196));
#62128=CARTESIAN_POINT('Ctrl Pts',(-3.23722035832121,-5.94244843071194,
58.0384027205074));
#62129=CARTESIAN_POINT('Ctrl Pts',(-3.07388579987965,-6.03142689875748,
58.0471518085834));
#62130=CARTESIAN_POINT('Ctrl Pts',(-2.90688078732959,-6.11366734734653,
58.0559008966594));
#62131=CARTESIAN_POINT('Ctrl Pts',(-2.73677250553455,-6.18889047026607,
58.0646499847354));
#62132=CARTESIAN_POINT('Ctrl Pts',(-2.56666475859314,-6.26411335666943,
58.0733990453026));
#62133=CARTESIAN_POINT('Ctrl Pts',(-2.39345402398854,-6.33231884567268,
58.0821481058697));
#62134=CARTESIAN_POINT('Ctrl Pts',(-2.21772855885275,-6.39327529825276,
58.0908971664369));
#62135=CARTESIAN_POINT('Ctrl Pts',(-2.04200363164235,-6.45423156423482,
58.0996462002217));
#62136=CARTESIAN_POINT('Ctrl Pts',(-1.86376426001178,-6.50793874429595,
58.1083952340065));
#62137=CARTESIAN_POINT('Ctrl Pts',(-1.68361577561401,-6.55421443958799,
58.1171442677913));
#62138=CARTESIAN_POINT('Ctrl Pts',(-1.50346782772448,-6.60048999706431,
58.1258932755203));
#62139=CARTESIAN_POINT('Ctrl Pts',(-1.32141105596206,-6.6393340427734,58.1346422832492));
#62140=CARTESIAN_POINT('Ctrl Pts',(-1.1380637528501,-6.67061465642026,58.1433912909781));
#62141=CARTESIAN_POINT('Ctrl Pts',(-0.954716980551841,-6.70189517950577,
58.1521402733775));
#62142=CARTESIAN_POINT('Ctrl Pts',(-0.7700799668219,-6.72561226616107,58.160889255777));
#62143=CARTESIAN_POINT('Ctrl Pts',(-0.584779763451173,-6.74168537001379,
58.1696382381764));
#62144=CARTESIAN_POINT('Ctrl Pts',(-0.391489586975877,-6.75845153121429,
58.1787644685917));
#62145=CARTESIAN_POINT('Ctrl Pts',(-0.197478091193787,-6.7668998514816,
58.187890699007));
#62146=CARTESIAN_POINT('Ctrl Pts',(-0.00346214692596143,-6.76699911434446,
58.1970169294223));
#62147=CARTESIAN_POINT('Ctrl Pts',(0.184490799083379,-6.76709527524285,
58.2058579651372));
#62148=CARTESIAN_POINT('Ctrl Pts',(0.372447602746487,-6.75935633787485,
58.214699000852));
#62149=CARTESIAN_POINT('Ctrl Pts',(0.559756448778259,-6.74380914009665,
58.2235400365668));
#62150=CARTESIAN_POINT('Ctrl Pts',(0.745136131626023,-6.72842206866702,
58.2322900151801));
#62151=CARTESIAN_POINT('Ctrl Pts',(0.929880852525672,-6.70538686347671,
58.2410399937934));
#62152=CARTESIAN_POINT('Ctrl Pts',(1.11336305115256,-6.67478177293672,58.2497899724067));
#62153=CARTESIAN_POINT('Ctrl Pts',(1.29684337147669,-6.64417699570029,58.2585398614467));
#62154=CARTESIAN_POINT('Ctrl Pts',(1.47906091262423,-6.60600253535246,58.2672897504867));
#62155=CARTESIAN_POINT('Ctrl Pts',(1.65939671152076,-6.56038806426831,58.2760396395267));
#62156=CARTESIAN_POINT('Ctrl Pts',(1.8397307242563,-6.51477404497903,58.2847894419022));
#62157=CARTESIAN_POINT('Ctrl Pts',(2.01818275413056,-6.46172023271164,58.2935392442777));
#62158=CARTESIAN_POINT('Ctrl Pts',(2.19414664088833,-6.40140683899082,58.3022890466532));
#62159=CARTESIAN_POINT('Ctrl Pts',(2.37010884326244,-6.34109402260946,58.3110387652728));
#62160=CARTESIAN_POINT('Ctrl Pts',(2.54358267902205,-6.27352185677736,58.3197884838923));
#62161=CARTESIAN_POINT('Ctrl Pts',(2.71397890895495,-6.19891986411727,58.3285382025118));
#62162=CARTESIAN_POINT('Ctrl Pts',(2.88437356442055,-6.12431856078229,58.3372878402836));
#62163=CARTESIAN_POINT('Ctrl Pts',(3.05169040839584,-6.04268767556088,58.3460374780555));
#62164=CARTESIAN_POINT('Ctrl Pts',(3.21536112563705,-5.95430447926053,58.3547871158273));
#62165=CARTESIAN_POINT('Ctrl Pts',(3.37903038493717,-5.86592207025736,58.3635366756594));
#62166=CARTESIAN_POINT('Ctrl Pts',(3.53905333030013,-5.77078760672689,58.3722862354914));
#62167=CARTESIAN_POINT('Ctrl Pts',(3.69488643091041,-5.66922422053266,58.3810357953235));
#62168=CARTESIAN_POINT('Ctrl Pts',(3.85071819517023,-5.56766170529767,58.3897852801235));
#62169=CARTESIAN_POINT('Ctrl Pts',(4.0023599464658,-5.45967053421537,58.3985347649235));
#62170=CARTESIAN_POINT('Ctrl Pts',(4.14929663020678,-5.34561750170686,58.4072842497235));
#62171=CARTESIAN_POINT('Ctrl Pts',(4.29623210270428,-5.23156540937196,58.4160336623988));
#62172=CARTESIAN_POINT('Ctrl Pts',(4.43846235886454,-5.11145173133687,58.4247830750742));
#62173=CARTESIAN_POINT('Ctrl Pts',(4.57550431840671,-4.98568442966877,58.4335324877495));
#62174=CARTESIAN_POINT('Ctrl Pts',(4.71254519379645,-4.85991812295817,58.4422818312074));
#62175=CARTESIAN_POINT('Ctrl Pts',(4.84439764355994,-4.72849847589085,58.4510311746653));
#62176=CARTESIAN_POINT('Ctrl Pts',(4.97061384236511,-4.59187184382234,58.4597805181232));
#62177=CARTESIAN_POINT('Ctrl Pts',(5.09682908458846,-4.45524624723543,58.4685297952706));
#62178=CARTESIAN_POINT('Ctrl Pts',(5.2174079668758,-4.31341395511643,58.4772790724179));
#62179=CARTESIAN_POINT('Ctrl Pts',(5.33194095978389,-4.16685668116614,58.4860283495653));
#62180=CARTESIAN_POINT('Ctrl Pts',(5.44647312270003,-4.02030046927975,58.4947775633088));
#62181=CARTESIAN_POINT('Ctrl Pts',(5.55495930745849,-3.86901956987362,58.5035267770524));
#62182=CARTESIAN_POINT('Ctrl Pts',(5.6570310611201,-3.713527780093,58.5122759907959));
#62183=CARTESIAN_POINT('Ctrl Pts',(5.75910210899612,-3.55803706547627,58.5210251440421));
#62184=CARTESIAN_POINT('Ctrl Pts',(5.85475865728049,-3.39833575830077,58.5297742972883));
#62185=CARTESIAN_POINT('Ctrl Pts',(5.94367583097153,-3.2349662465511,58.5385234505345));
#62186=CARTESIAN_POINT('Ctrl Pts',(6.03259241936753,-3.0715978101771,58.5472725461897));
#62187=CARTESIAN_POINT('Ctrl Pts',(6.11476958496196,-2.90456146922724,58.5560216418448));
#62188=CARTESIAN_POINT('Ctrl Pts',(6.18992823598139,-2.73442451594487,58.5647707374999));
#62189=CARTESIAN_POINT('Ctrl Pts',(6.26508641723222,-2.56428862607966,58.5735197784701));
#62190=CARTESIAN_POINT('Ctrl Pts',(6.33322605591089,-2.39105242476208,58.5822688194402));
#62191=CARTESIAN_POINT('Ctrl Pts',(6.3941157376704,-2.21530425298102,58.5910178604103));
#62192=CARTESIAN_POINT('Ctrl Pts',(6.45500505906866,-2.03955712132414,58.5997668496013));
#62193=CARTESIAN_POINT('Ctrl Pts',(6.50864441561116,-1.86129831968967,58.6085158387923));
#62194=CARTESIAN_POINT('Ctrl Pts',(6.55485164064525,-1.68113323955312,58.6172648279833));
#62195=CARTESIAN_POINT('Ctrl Pts',(6.60199852651826,-1.49730435856674,58.6261917348596));
#62196=CARTESIAN_POINT('Ctrl Pts',(6.64140767451907,-1.31149113118293,58.6351186417359));
#62197=CARTESIAN_POINT('Ctrl Pts',(6.6729397527877,-1.12435050392021,58.6440455486122));
#62198=CARTESIAN_POINT('Ctrl Pts',(6.70384664839178,-0.940920291017168,
58.6527954627962));
#62199=CARTESIAN_POINT('Ctrl Pts',(6.72718585895831,-0.756215113729511,
58.6615453769802));
#62200=CARTESIAN_POINT('Ctrl Pts',(6.74287810456518,-0.57086238882548,58.6702952911642));
#62201=CARTESIAN_POINT('Ctrl Pts',(6.75857004157265,-0.385513309017313,
58.6790450332748));
#62202=CARTESIAN_POINT('Ctrl Pts',(6.76661529037181,-0.199516992707917,
58.6877947753854));
#62203=CARTESIAN_POINT('Ctrl Pts',(6.76698652349006,-0.0135052176538825,
58.6965445174959));
#62204=CARTESIAN_POINT('Ctrl Pts',(6.76735774980119,0.172503146589083,58.7052940991666));
#62205=CARTESIAN_POINT('Ctrl Pts',(6.76005524144565,0.358526682383054,58.7140436808372));
#62206=CARTESIAN_POINT('Ctrl Pts',(6.74510380210459,0.543933542663219,58.7227932625079));
#62207=CARTESIAN_POINT('Ctrl Pts',(6.7301526170505,0.729337249631886,58.7315426953698));
#62208=CARTESIAN_POINT('Ctrl Pts',(6.70755278437173,0.914124016400014,58.7402921282317));
#62209=CARTESIAN_POINT('Ctrl Pts',(6.67738106399364,1.09766621803678,58.7490415610936));
#62210=CARTESIAN_POINT('Ctrl Pts',(6.64720981666837,1.28120554197365,58.757790856776));
#62211=CARTESIAN_POINT('Ctrl Pts',(6.60946696569625,1.46350005704353,58.7665401524583));
#62212=CARTESIAN_POINT('Ctrl Pts',(6.56428069997631,1.64393062259896,58.7752894481407));
#62213=CARTESIAN_POINT('Ctrl Pts',(6.51909508267909,1.82435859897652,58.7840386182707));
#62214=CARTESIAN_POINT('Ctrl Pts',(6.46646633399376,2.00292240139141,58.7927877884007));
#62215=CARTESIAN_POINT('Ctrl Pts',(6.40657319579473,2.1790155774855,58.8015369585307));
#62216=CARTESIAN_POINT('Ctrl Pts',(6.34668083749142,2.35510646059047,58.8102860147337));
#62217=CARTESIAN_POINT('Ctrl Pts',(6.27952437123319,2.52872651047601,58.8190350709368));
#62218=CARTESIAN_POINT('Ctrl Pts',(6.20533187313181,2.69928608048396,58.8277841271399));
#62219=CARTESIAN_POINT('Ctrl Pts',(6.12831449761773,2.87633970163138,58.8368663034277));
#62220=CARTESIAN_POINT('Ctrl Pts',(6.04371489440355,3.05009490607377,58.8459484797154));
#62221=CARTESIAN_POINT('Ctrl Pts',(5.95184265097576,3.21991584641988,58.8550306560032));
#62222=CARTESIAN_POINT('Ctrl Pts',(5.86333281311414,3.38352155947026,58.8637804363576));
#62223=CARTESIAN_POINT('Ctrl Pts',(5.76807337210469,3.54347560944871,58.872530216712));
#62224=CARTESIAN_POINT('Ctrl Pts',(5.66638790060032,3.69923467218969,58.8812799970664));
#62225=CARTESIAN_POINT('Ctrl Pts',(5.56470608475312,3.8549881352936,58.8900294628607));
#62226=CARTESIAN_POINT('Ctrl Pts',(5.45659885738445,4.00654667295086,58.898778928655));
#62227=CARTESIAN_POINT('Ctrl Pts',(5.34243340550957,4.15339551544221,58.9075283944492));
#62228=CARTESIAN_POINT('Ctrl Pts',(5.22827145109994,4.30023985921074,58.9162775922031));
#62229=CARTESIAN_POINT('Ctrl Pts',(5.10805181946473,4.44237457029397,58.925026789957));
#62230=CARTESIAN_POINT('Ctrl Pts',(4.98218281249954,4.57931691661913,58.9337759877109));
#62231=CARTESIAN_POINT('Ctrl Pts',(4.85631699262644,4.71625579546744,58.9425249639289));
#62232=CARTESIAN_POINT('Ctrl Pts',(4.72480227757301,4.84800236169429,58.9512739401469));
#62233=CARTESIAN_POINT('Ctrl Pts',(4.58808530812664,4.97410918711607,58.9600229163649));
#62234=CARTESIAN_POINT('Ctrl Pts',(4.45135945020618,5.10022421120736,58.9687724613861));
#62235=CARTESIAN_POINT('Ctrl Pts',(4.30943087170825,5.22069856642706,58.9775220064073));
#62236=CARTESIAN_POINT('Ctrl Pts',(4.16278164284432,5.33512305331361,58.9862715514285));
#62237=CARTESIAN_POINT('Ctrl Pts',(4.01614103495537,5.44954081360061,58.9950205820958));
#62238=CARTESIAN_POINT('Ctrl Pts',(3.86478055793785,5.55790924095894,59.003769612763));
#62239=CARTESIAN_POINT('Ctrl Pts',(3.70921425771593,5.6598602977774,59.0125186434303));
#62240=CARTESIAN_POINT('Ctrl Pts',(3.55364584489039,5.7618127390999,59.0212677929101));
#62241=CARTESIAN_POINT('Ctrl Pts',(3.39387173422587,5.85734747842258,59.03001694239));
#62242=CARTESIAN_POINT('Ctrl Pts',(3.2304345605002,5.94614005471835,59.0387660918698));
#62243=CARTESIAN_POINT('Ctrl Pts',(3.18690768777967,5.96978744826323,59.0410961805953));
#62244=CARTESIAN_POINT('Ctrl Pts',(3.14312114968588,5.99295688506664,59.0434262693208));
#62245=CARTESIAN_POINT('Ctrl Pts',(3.0990855038472,6.01564277861012,59.0457563580462));
#62246=CARTESIAN_POINT('Ctrl Pts',(3.09908550384732,6.01564277861007,57.0457563580462));
#62247=CARTESIAN_POINT('Ctrl Pts',(2.93373232018333,6.10082796552478,57.0545058059455));
#62248=CARTESIAN_POINT('Ctrl Pts',(2.76486502144423,6.17919158180192,57.0632552538448));
#62249=CARTESIAN_POINT('Ctrl Pts',(2.59305716434342,6.25046746591383,57.0720047017441));
#62250=CARTESIAN_POINT('Ctrl Pts',(2.4212506945927,6.32174277447229,57.0807540789915));
#62251=CARTESIAN_POINT('Ctrl Pts',(2.24650397871044,6.38593035557831,57.089503456239));
#62252=CARTESIAN_POINT('Ctrl Pts',(2.06941053323754,6.44281220003544,57.0982528334864));
#62253=CARTESIAN_POINT('Ctrl Pts',(1.89231845896678,6.49969360406686,57.107002142989));
#62254=CARTESIAN_POINT('Ctrl Pts',(1.71287996431511,6.54926929700879,57.1157514524916));
#62255=CARTESIAN_POINT('Ctrl Pts',(1.53170449173522,6.59137090065475,57.1245007619941));
#62256=CARTESIAN_POINT('Ctrl Pts',(1.350530361782,6.63347219230077,57.1332500066587));
#62257=CARTESIAN_POINT('Ctrl Pts',(1.16761955878886,6.66809944062446,57.1419992513233));
#62258=CARTESIAN_POINT('Ctrl Pts',(0.983593309311028,6.69513503985383,57.1507484959879));
#62259=CARTESIAN_POINT('Ctrl Pts',(0.799568362460467,6.72217044771209,57.1594976787211));
#62260=CARTESIAN_POINT('Ctrl Pts',(0.614428268439024,6.74161427235973,57.1682468614543));
#62261=CARTESIAN_POINT('Ctrl Pts',(0.42880181633064,6.753400476968,57.1769960441874));
#62262=CARTESIAN_POINT('Ctrl Pts',(0.243176616523071,6.76518660206241,57.1857451678956));
#62263=CARTESIAN_POINT('Ctrl Pts',(0.0570653511656648,6.76931519233997,
57.1944942916037));
#62264=CARTESIAN_POINT('Ctrl Pts',(-0.12889990079991,6.76577222610795,57.2032434153118));
#62265=CARTESIAN_POINT('Ctrl Pts',(-0.31486395994192,6.76222928260133,57.2119924829011));
#62266=CARTESIAN_POINT('Ctrl Pts',(-0.500681721080598,6.75101488651277,
57.2207415504904));
#62267=CARTESIAN_POINT('Ctrl Pts',(-0.685722110173234,6.73216712415992,
57.2294906180796));
#62268=CARTESIAN_POINT('Ctrl Pts',(-0.87076137382758,6.71331947644146,57.238239632456));
#62269=CARTESIAN_POINT('Ctrl Pts',(-1.05502298984343,6.68683858439996,57.2469886468323));
#62270=CARTESIAN_POINT('Ctrl Pts',(-1.23788117676063,6.65281438131425,57.2557376612087));
#62271=CARTESIAN_POINT('Ctrl Pts',(-1.43009641451788,6.61704912302378,57.2649343720962));
#62272=CARTESIAN_POINT('Ctrl Pts',(-1.62076048992682,6.57294837083168,57.2741310829838));
#62273=CARTESIAN_POINT('Ctrl Pts',(-1.8091579896111,6.52067760042055,57.2833277938713));
#62274=CARTESIAN_POINT('Ctrl Pts',(-1.98840443002993,6.47094578577415,57.2920777915778));
#62275=CARTESIAN_POINT('Ctrl Pts',(-2.16559895952176,6.41381888474481,57.3008277892843));
#62276=CARTESIAN_POINT('Ctrl Pts',(-2.3401396624231,6.34949095285239,57.3095777869908));
#62277=CARTESIAN_POINT('Ctrl Pts',(-2.51467682554003,6.2851643255669,57.3183276072424));
#62278=CARTESIAN_POINT('Ctrl Pts',(-2.68656000078831,6.21363705879665,57.327077427494));
#62279=CARTESIAN_POINT('Ctrl Pts',(-2.85520533840878,6.13515211510864,57.3358272477456));
#62280=CARTESIAN_POINT('Ctrl Pts',(-3.02384747998314,6.05666865881128,57.3445769021768));
#62281=CARTESIAN_POINT('Ctrl Pts',(-3.1892516468452,5.97122791039853,57.3533265566081));
#62282=CARTESIAN_POINT('Ctrl Pts',(-3.35085601829138,5.87912008251919,57.3620762110393));
#62283=CARTESIAN_POINT('Ctrl Pts',(-3.51245754191393,5.78701387778189,57.3708257112825));
#62284=CARTESIAN_POINT('Ctrl Pts',(-3.67025915510905,5.68824097061002,57.3795752115256));
#62285=CARTESIAN_POINT('Ctrl Pts',(-3.82372487928799,5.58313684656879,57.3883247117687));
#62286=CARTESIAN_POINT('Ctrl Pts',(-3.97718810300752,5.47803443501806,57.3970740694539));
#62287=CARTESIAN_POINT('Ctrl Pts',(-4.12631534262969,5.36660117496419,57.4058234271389));
#62288=CARTESIAN_POINT('Ctrl Pts',(-4.2706000988616,5.24921554097404,57.4145727848241));
#62289=CARTESIAN_POINT('Ctrl Pts',(-4.4148826959415,5.13183166360346,57.4233220115792));
#62290=CARTESIAN_POINT('Ctrl Pts',(-4.55432273235027,5.00849577139527,57.4320712383344));
#62291=CARTESIAN_POINT('Ctrl Pts',(-4.68844662480147,4.879626752774,57.4408204650896));
#62292=CARTESIAN_POINT('Ctrl Pts',(-4.822568688351,4.75075949139941,57.4495695725411));
#62293=CARTESIAN_POINT('Ctrl Pts',(-4.95137454637806,4.61635945312585,57.4583186799926));
#62294=CARTESIAN_POINT('Ctrl Pts',(-5.07442674461024,4.47688309134652,57.4670677874441));
#62295=CARTESIAN_POINT('Ctrl Pts',(-5.19747742838485,4.33740844616415,57.4758167872165));
#62296=CARTESIAN_POINT('Ctrl Pts',(-5.31477440450874,4.19285781736096,57.4845657869888));
#62297=CARTESIAN_POINT('Ctrl Pts',(-5.42591931531101,4.04372211999476,57.4933147867612));
#62298=CARTESIAN_POINT('Ctrl Pts',(-5.53707636462927,3.89457013500878,57.5020647420418));
#62299=CARTESIAN_POINT('Ctrl Pts',(-5.64207983273414,3.74083230916505,57.5108146973224));
#62300=CARTESIAN_POINT('Ctrl Pts',(-5.74057303468689,3.5830308725192,57.5195646526029));
#62301=CARTESIAN_POINT('Ctrl Pts',(-5.83906243363715,3.42523552887517,57.5283142700317));
#62302=CARTESIAN_POINT('Ctrl Pts',(-5.93104191768382,3.26337713157073,57.5370638874605));
#62303=CARTESIAN_POINT('Ctrl Pts',(-6.01619906699618,3.09800545291229,57.5458135048894));
#62304=CARTESIAN_POINT('Ctrl Pts',(-6.10135338095344,2.93263928039676,57.5545628309947));
#62305=CARTESIAN_POINT('Ctrl Pts',(-6.17968568352799,2.76376031540312,57.5633121571001));
#62306=CARTESIAN_POINT('Ctrl Pts',(-6.25092992694846,2.59194213831638,57.5720614832055));
#62307=CARTESIAN_POINT('Ctrl Pts',(-6.32217217691075,2.42012876880897,57.5808105644993));
#62308=CARTESIAN_POINT('Ctrl Pts',(-6.38632665483831,2.24537661647728,57.5895596457931));
#62309=CARTESIAN_POINT('Ctrl Pts',(-6.44317547869338,2.06827917621493,57.5983087270869));
#62310=CARTESIAN_POINT('Ctrl Pts',(-6.50002944235922,1.89116572423472,57.6070585994019));
#62311=CARTESIAN_POINT('Ctrl Pts',(-6.54957634250382,1.71170683289258,57.6158084717169));
#62312=CARTESIAN_POINT('Ctrl Pts',(-6.59164787708379,1.53051209225436,57.6245583440318));
#62313=CARTESIAN_POINT('Ctrl Pts',(-6.63371649074999,1.34932993148083,57.6333076088666));
#62314=CARTESIAN_POINT('Ctrl Pts',(-6.66831071257119,1.16641244174038,57.6420568737014));
#62315=CARTESIAN_POINT('Ctrl Pts',(-6.69531304840331,0.982380875160158,
57.6508061385362));
#62316=CARTESIAN_POINT('Ctrl Pts',(-6.72231677033042,0.798339861795985,
57.6595558524919));
#62317=CARTESIAN_POINT('Ctrl Pts',(-6.74172778477889,0.613184940730294,
57.6683055664475));
#62318=CARTESIAN_POINT('Ctrl Pts',(-6.75348015835517,0.42754502769069,57.6770552804032));
#62319=CARTESIAN_POINT('Ctrl Pts',(-6.76249038365208,0.285219953548979,
57.6837634482054));
#62320=CARTESIAN_POINT('Ctrl Pts',(-6.76699999999987,0.142609995761489,
57.6904716160076));
#62321=CARTESIAN_POINT('Ctrl Pts',(-6.767,6.12589398735536E-12,57.6971797838098));
#62322=CARTESIAN_POINT('',(-6.76724680008539,0.000596459099932123,57.3032472956769));
#62323=CARTESIAN_POINT('Ctrl Pts',(3.09908550384732,6.01564277861007,56.6515377972971));
#62324=CARTESIAN_POINT('Ctrl Pts',(2.93599067927878,6.09966452411166,56.6601567701762));
#62325=CARTESIAN_POINT('Ctrl Pts',(2.76940673124068,6.17708587161028,56.6687757430553));
#62326=CARTESIAN_POINT('Ctrl Pts',(2.59988413276071,6.24763087067563,56.6773947159345));
#62327=CARTESIAN_POINT('Ctrl Pts',(2.50810438171936,6.28582402314901,56.6820610388447));
#62328=CARTESIAN_POINT('Ctrl Pts',(2.41546370318375,6.3220023997654,56.6867273617549));
#62329=CARTESIAN_POINT('Ctrl Pts',(2.3220522869404,6.35612792324973,56.691393684665));
#62330=CARTESIAN_POINT('Ctrl Pts',(2.15338129672925,6.41774764885778,56.6998195638301));
#62331=CARTESIAN_POINT('Ctrl Pts',(1.98226984749979,6.47264427983321,56.7082454429952));
#62332=CARTESIAN_POINT('Ctrl Pts',(1.80928191798352,6.52064321530153,56.7166713221602));
#62333=CARTESIAN_POINT('Ctrl Pts',(1.6362538245622,6.5686532950427,56.7250991576249));
#62334=CARTESIAN_POINT('Ctrl Pts',(1.46134870160362,6.6097623975066,56.7335269930895));
#62335=CARTESIAN_POINT('Ctrl Pts',(1.28514353867964,6.64384640739007,56.7419548285541));
#62336=CARTESIAN_POINT('Ctrl Pts',(1.10887360822069,6.677942945495,56.7503857618288));
#62337=CARTESIAN_POINT('Ctrl Pts',(0.93130301030162,6.70500917940863,56.7588166951035));
#62338=CARTESIAN_POINT('Ctrl Pts',(0.753017112247756,6.72497243330128,56.7672476283782));
#62339=CARTESIAN_POINT('Ctrl Pts',(0.574567372966716,6.74495403303087,56.7756863095144));
#62340=CARTESIAN_POINT('Ctrl Pts',(0.39540134989818,6.75781957449781,56.7841249906507));
#62341=CARTESIAN_POINT('Ctrl Pts',(0.216108822565234,6.76354832738035,56.7925636717869));
#62342=CARTESIAN_POINT('Ctrl Pts',(0.0367222718658691,6.76928008449647,
56.8010067782789));
#62343=CARTESIAN_POINT('Ctrl Pts',(-0.142790584228386,6.76786758600262,
56.8094498847708));
#62344=CARTESIAN_POINT('Ctrl Pts',(-0.321841221534579,6.75934221859799,
56.8178929912628));
#62345=CARTESIAN_POINT('Ctrl Pts',(-0.501079966452768,6.75080789458461,
56.8263449679415));
#62346=CARTESIAN_POINT('Ctrl Pts',(-0.679855192202551,6.73514579800707,
56.8347969446202));
#62347=CARTESIAN_POINT('Ctrl Pts',(-0.8575836666143,6.71243914346763,56.843248921299));
#62348=CARTESIAN_POINT('Ctrl Pts',(-0.906008180769598,6.70625240992476,
56.8455517760648));
#62349=CARTESIAN_POINT('Ctrl Pts',(-0.954355044586321,6.69954300753287,
56.8478546308306));
#62350=CARTESIAN_POINT('Ctrl Pts',(-1.00261260229868,6.6923132749231,56.8501574855964));
#62351=CARTESIAN_POINT('Ctrl Pts',(-1.17690391505033,6.66620172582829,56.8584746818914));
#62352=CARTESIAN_POINT('Ctrl Pts',(-1.35034293822587,6.63325193364448,56.8667918781864));
#62353=CARTESIAN_POINT('Ctrl Pts',(-1.52236274074635,6.59353476411456,56.8751090744814));
#62354=CARTESIAN_POINT('Ctrl Pts',(-1.69423744372123,6.55385109621159,56.8834192551806));
#62355=CARTESIAN_POINT('Ctrl Pts',(-1.8646949739395,6.50741150195246,56.8917294358798));
#62356=CARTESIAN_POINT('Ctrl Pts',(-2.03317652023222,6.45433824939292,56.900039616579));
#62357=CARTESIAN_POINT('Ctrl Pts',(-2.20154680928724,6.40130004389701,56.9083443096282));
#62358=CARTESIAN_POINT('Ctrl Pts',(-2.36794338382564,6.34163701305229,56.9166490026775));
#62359=CARTESIAN_POINT('Ctrl Pts',(-2.5318203548967,6.27552186599097,56.9249536957267));
#62360=CARTESIAN_POINT('Ctrl Pts',(-2.69561911035898,6.20943827453165,56.9332544250914));
#62361=CARTESIAN_POINT('Ctrl Pts',(-2.85690033703638,6.13690883383908,56.941555154456));
#62362=CARTESIAN_POINT('Ctrl Pts',(-3.01513575662215,6.05815527773419,56.9498558838207));
#62363=CARTESIAN_POINT('Ctrl Pts',(-3.17332461156488,5.97942489678969,56.9581541704927));
#62364=CARTESIAN_POINT('Ctrl Pts',(-3.32846913498271,5.8944742061522,56.9664524571647));
#62365=CARTESIAN_POINT('Ctrl Pts',(-3.48006319063366,5.80357210597031,56.9747507438367));
#62366=CARTESIAN_POINT('Ctrl Pts',(-3.63167266766553,5.71266075848709,56.983049874678));
#62367=CARTESIAN_POINT('Ctrl Pts',(-3.77973065308717,5.61579696418062,56.9913490055192));
#62368=CARTESIAN_POINT('Ctrl Pts',(-3.92375718192527,5.51329471163023,56.9996481363604));
#62369=CARTESIAN_POINT('Ctrl Pts',(-4.06779831126174,5.41078206804992,57.0079481085151));
#62370=CARTESIAN_POINT('Ctrl Pts',(-4.20780688556142,5.30263002828526,57.0162480806697));
#62371=CARTESIAN_POINT('Ctrl Pts',(-4.34333349638092,5.18919484498467,57.0245480528243));
#62372=CARTESIAN_POINT('Ctrl Pts',(-4.47889634541887,5.07572933045299,57.0328502442937));
#62373=CARTESIAN_POINT('Ctrl Pts',(-4.60997457558108,4.95697808015974,57.041152435763));
#62374=CARTESIAN_POINT('Ctrl Pts',(-4.73615318537281,4.83333652921903,57.0494546272324));
#62375=CARTESIAN_POINT('Ctrl Pts',(-4.86238648383141,4.70964138923021,57.0577604170595));
#62376=CARTESIAN_POINT('Ctrl Pts',(-4.98371568120406,4.58105196761277,57.0660662068867));
#62377=CARTESIAN_POINT('Ctrl Pts',(-5.09976371645401,4.44799944203449,57.0743719967138));
#62378=CARTESIAN_POINT('Ctrl Pts',(-5.21594893825968,4.31478962798792,57.0826876052569));
#62379=CARTESIAN_POINT('Ctrl Pts',(-5.32684029541498,4.17710643101975,57.0910032138001));
#62380=CARTESIAN_POINT('Ctrl Pts',(-5.43210127579277,4.03541382382657,57.0993188223432));
#62381=CARTESIAN_POINT('Ctrl Pts',(-5.5374288366751,3.89363159210926,57.1076396907406));
#62382=CARTESIAN_POINT('Ctrl Pts',(-5.63711872241454,3.74783517938533,57.1159605591379));
#62383=CARTESIAN_POINT('Ctrl Pts',(-5.73087856432538,3.59851634440583,57.1242814275352));
#62384=CARTESIAN_POINT('Ctrl Pts',(-5.82477777575151,3.4489755541283,57.132614664505));
#62385=CARTESIAN_POINT('Ctrl Pts',(-5.91272915426113,3.29590217932676,57.1409479014748));
#62386=CARTESIAN_POINT('Ctrl Pts',(-5.99448634151743,3.13981249461827,57.1492811384446));
#62387=CARTESIAN_POINT('Ctrl Pts',(-6.05467324173071,3.02490450190048,57.1554157881162));
#62388=CARTESIAN_POINT('Ctrl Pts',(-6.11150423265171,2.90836233345991,57.1615504377878));
#62389=CARTESIAN_POINT('Ctrl Pts',(-6.16489799614201,2.79039812520798,57.1676850874594));
#62390=CARTESIAN_POINT('Ctrl Pts',(-6.24111848062213,2.62200225804067,57.1764424017883));
#62391=CARTESIAN_POINT('Ctrl Pts',(-6.31054009248221,2.45025035891108,57.1851997161172));
#62392=CARTESIAN_POINT('Ctrl Pts',(-6.37287157082253,2.27569702328804,57.1939570304461));
#62393=CARTESIAN_POINT('Ctrl Pts',(-6.43744238794568,2.09487263386455,57.2030289625914));
#62394=CARTESIAN_POINT('Ctrl Pts',(-6.494403976871,1.91104198712258,57.2121008947367));
#62395=CARTESIAN_POINT('Ctrl Pts',(-6.54348336297778,1.72485201638661,57.221172826882));
#62396=CARTESIAN_POINT('Ctrl Pts',(-6.59058882189029,1.54615043284722,57.2298798943665));
#62397=CARTESIAN_POINT('Ctrl Pts',(-6.63043352000807,1.3652759072758,57.2385869618509));
#62398=CARTESIAN_POINT('Ctrl Pts',(-6.66282352986,1.18282357515561,57.2472940293354));
#62399=CARTESIAN_POINT('Ctrl Pts',(-6.69514768823904,1.00074218317589,57.2559833946573));
#62400=CARTESIAN_POINT('Ctrl Pts',(-6.72004731754403,0.817089655723656,
57.2646727599792));
#62401=CARTESIAN_POINT('Ctrl Pts',(-6.73737803352117,0.632476271038214,
57.2733621253011));
#62402=CARTESIAN_POINT('Ctrl Pts',(-6.75466194895993,0.448361423505387,
57.2820280255235));
#62403=CARTESIAN_POINT('Ctrl Pts',(-6.76441768063083,0.263291174265457,
57.290693925746));
#62404=CARTESIAN_POINT('Ctrl Pts',(-6.76655176891214,0.0778855482874975,
57.2993598259684));
#62405=CARTESIAN_POINT('Ctrl Pts',(-6.76683582396433,0.053207372962864,
57.3005132893755));
#62406=CARTESIAN_POINT('Ctrl Pts',(-6.76698492294256,0.0285232737042095,
57.3016667527825));
#62407=CARTESIAN_POINT('Ctrl Pts',(-6.76699891346671,0.00383472820380105,
57.3028202161896));
#62408=CARTESIAN_POINT('Ctrl Pts',(-6.767,5.9890047246399E-12,57.3028202161897));
#62409=CARTESIAN_POINT('Ctrl Pts',(-6.76700000000017,-0.186007249554085,
57.3115697280025));
#62410=CARTESIAN_POINT('Ctrl Pts',(-6.75932637294279,-0.37201435581034,
57.3203192398152));
#62411=CARTESIAN_POINT('Ctrl Pts',(-6.74400518263409,-0.557389537580792,
57.329068751628));
#62412=CARTESIAN_POINT('Ctrl Pts',(-6.7286840570379,-0.742763936377278,
57.3378182264852));
#62413=CARTESIAN_POINT('Ctrl Pts',(-6.70571545643639,-0.927506130399604,
57.3465677013423));
#62414=CARTESIAN_POINT('Ctrl Pts',(-6.67517739401663,-1.11098864009015,
57.3553171761995));
#62415=CARTESIAN_POINT('Ctrl Pts',(-6.64463945804491,-1.29447039004018,
57.3640666148281));
#62416=CARTESIAN_POINT('Ctrl Pts',(-6.60653217002839,-1.47669218338763,
57.3728160534566));
#62417=CARTESIAN_POINT('Ctrl Pts',(-6.56098496085608,-1.65703510627276,
57.3815654920851));
#62418=CARTESIAN_POINT('Ctrl Pts',(-6.51543793649699,-1.83737729739503,
57.3903148952117));
#62419=CARTESIAN_POINT('Ctrl Pts',(-6.46245112157053,-2.01584035544447,
57.3990642983384));
#62420=CARTESIAN_POINT('Ctrl Pts',(-6.40220448361889,-2.19181813796906,
57.407813701465));
#62421=CARTESIAN_POINT('Ctrl Pts',(-6.34195808512156,-2.36779522105814,
57.4165630698165));
#62422=CARTESIAN_POINT('Ctrl Pts',(-6.27445201416547,-2.54128677725269,
57.4253124381681));
#62423=CARTESIAN_POINT('Ctrl Pts',(-6.19991555052926,-2.71170355428198,
57.4340618065196));
#62424=CARTESIAN_POINT('Ctrl Pts',(-6.12537937695322,-2.8821196681309,57.4428111408228));
#62425=CARTESIAN_POINT('Ctrl Pts',(-6.0438129802855,-3.04946076419476,57.451560475126));
#62426=CARTESIAN_POINT('Ctrl Pts',(-5.95549339309074,-3.21315848424142,
57.4603098094292));
#62427=CARTESIAN_POINT('Ctrl Pts',(-5.86717414225902,-3.37685558084921,
57.4690591104107));
#62428=CARTESIAN_POINT('Ctrl Pts',(-5.7721018884416,-3.53690907699847,57.4778084113923));
#62429=CARTESIAN_POINT('Ctrl Pts',(-5.67059953311466,-3.69277537023847,
57.4865577123738));
#62430=CARTESIAN_POINT('Ctrl Pts',(-5.56909755592801,-3.84864108280892,
57.4953069807605));
#62431=CARTESIAN_POINT('Ctrl Pts',(-5.46116568155057,-4.00031938354704,
57.5040562491471));
#62432=CARTESIAN_POINT('Ctrl Pts',(-5.34717048488466,-4.14729511918049,
57.5128055175337));
#62433=CARTESIAN_POINT('Ctrl Pts',(-5.23317570343384,-4.29427031947084,
57.5215547540521));
#62434=CARTESIAN_POINT('Ctrl Pts',(-5.11311781951614,-4.43654276249479,
57.5303039905704));
#62435=CARTESIAN_POINT('Ctrl Pts',(-4.98740458929298,-4.57362924412324,
57.5390532270888));
#62436=CARTESIAN_POINT('Ctrl Pts',(-4.86169180652793,-4.71071523781213,
57.5478024324655));
#62437=CARTESIAN_POINT('Ctrl Pts',(-4.73032391141624,-4.84261509584439,
57.5565516378422));
#62438=CARTESIAN_POINT('Ctrl Pts',(-4.59374706947377,-4.96888084599552,
57.5653008432189));
#62439=CARTESIAN_POINT('Ctrl Pts',(-4.45717070231576,-5.09514615720682,
57.5740500181806));
#62440=CARTESIAN_POINT('Ctrl Pts',(-4.31538563497451,-5.21577720520509,
57.5827991931423));
#62441=CARTESIAN_POINT('Ctrl Pts',(-4.16887340952149,-5.33036429293389,
57.591548368104));
#62442=CARTESIAN_POINT('Ctrl Pts',(-4.02236168122615,-5.44495099183611,
57.6002975133773));
#62443=CARTESIAN_POINT('Ctrl Pts',(-3.87112305263296,-5.55349359497849,
57.6090466586505));
#62444=CARTESIAN_POINT('Ctrl Pts',(-3.71567116929095,-5.65562346357146,
57.6177958039238));
#62445=CARTESIAN_POINT('Ctrl Pts',(-3.56021980053429,-5.75775299408854,
57.6265449202352));
#62446=CARTESIAN_POINT('Ctrl Pts',(-3.4005554444222,-5.85346967519799,57.6352940365465));
#62447=CARTESIAN_POINT('Ctrl Pts',(-3.23722035886999,-5.94244843041298,
57.6440431528579));
#62448=CARTESIAN_POINT('Ctrl Pts',(-3.07388580043652,-6.03142689847368,
57.6527922409339));
#62449=CARTESIAN_POINT('Ctrl Pts',(-2.90688078789391,-6.11366734707822,
57.6615413290099));
#62450=CARTESIAN_POINT('Ctrl Pts',(-2.73677250610566,-6.18889047001352,
57.670290417086));
#62451=CARTESIAN_POINT('Ctrl Pts',(-2.56666475917128,-6.26411335643254,
57.6790394776531));
#62452=CARTESIAN_POINT('Ctrl Pts',(-2.39345402457307,-6.33231884545174,
57.6877885382203));
#62453=CARTESIAN_POINT('Ctrl Pts',(-2.21772855944301,-6.39327529804801,
57.6965375987874));
#62454=CARTESIAN_POINT('Ctrl Pts',(-2.04200363223832,-6.45423156404626,
57.7052866325722));
#62455=CARTESIAN_POINT('Ctrl Pts',(-1.86376426061281,-6.50793874412382,
57.714035666357));
#62456=CARTESIAN_POINT('Ctrl Pts',(-1.68361577621941,-6.55421443943247,
57.7227847001418));
#62457=CARTESIAN_POINT('Ctrl Pts',(-1.50346782833437,-6.60048999692538,
57.7315337078707));
#62458=CARTESIAN_POINT('Ctrl Pts',(-1.32141105657577,-6.63933404265125,
57.7402827155996));
#62459=CARTESIAN_POINT('Ctrl Pts',(-1.13806375346692,-6.67061465631502,
57.7490317233286));
#62460=CARTESIAN_POINT('Ctrl Pts',(-0.954716981171651,-6.70189517941747,
57.757780705728));
#62461=CARTESIAN_POINT('Ctrl Pts',(-0.770079967444,-6.72561226608984,57.7665296881274));
#62462=CARTESIAN_POINT('Ctrl Pts',(-0.584779764074859,-6.74168536995969,
57.7752786705269));
#62463=CARTESIAN_POINT('Ctrl Pts',(-0.391489587594695,-6.75845153117863,
57.7844049009425));
#62464=CARTESIAN_POINT('Ctrl Pts',(-0.197478091806922,-6.76689985146389,
57.7935311313581));
#62465=CARTESIAN_POINT('Ctrl Pts',(-0.00346214753266241,-6.76699911434415,
57.8026573617737));
#62466=CARTESIAN_POINT('Ctrl Pts',(0.184490798482982,-6.76709527525939,
57.8114983974888));
#62467=CARTESIAN_POINT('Ctrl Pts',(0.372447602153097,-6.75935633790772,
57.8203394332039));
#62468=CARTESIAN_POINT('Ctrl Pts',(0.559756448192511,-6.74380914014527,
57.8291804689191));
#62469=CARTESIAN_POINT('Ctrl Pts',(0.745136131041769,-6.72842206873172,
57.8379304475324));
#62470=CARTESIAN_POINT('Ctrl Pts',(0.929880851943572,-6.70538686355744,
57.8466804261457));
#62471=CARTESIAN_POINT('Ctrl Pts',(1.11336305057327,-6.67478177303335,57.855430404759));
#62472=CARTESIAN_POINT('Ctrl Pts',(1.29684337089997,-6.64417699581286,57.864180293799));
#62473=CARTESIAN_POINT('Ctrl Pts',(1.47906091205072,-6.60600253548086,57.872930182839));
#62474=CARTESIAN_POINT('Ctrl Pts',(1.65939671095112,-6.5603880644124,57.881680071879));
#62475=CARTESIAN_POINT('Ctrl Pts',(1.83973072369064,-6.51477404513877,57.8904298742545));
#62476=CARTESIAN_POINT('Ctrl Pts',(2.01818275356954,-6.46172023288687,57.89917967663));
#62477=CARTESIAN_POINT('Ctrl Pts',(2.19414664033257,-6.40140683918131,57.9079294790055));
#62478=CARTESIAN_POINT('Ctrl Pts',(2.37010884271195,-6.34109402281522,57.916679197625));
#62479=CARTESIAN_POINT('Ctrl Pts',(2.54358267847746,-6.27352185699816,57.9254289162445));
#62480=CARTESIAN_POINT('Ctrl Pts',(2.71397890841686,-6.19891986435286,57.9341786348641));
#62481=CARTESIAN_POINT('Ctrl Pts',(2.88437356388884,-6.1243185610327,57.9429282726359));
#62482=CARTESIAN_POINT('Ctrl Pts',(3.05169040787113,-6.04268767582587,57.9516779104077));
#62483=CARTESIAN_POINT('Ctrl Pts',(3.21536112511993,-5.95430447953978,57.9604275481795));
#62484=CARTESIAN_POINT('Ctrl Pts',(3.37903038442775,-5.86592207055081,57.9691771080116));
#62485=CARTESIAN_POINT('Ctrl Pts',(3.53905332979899,-5.77078760703422,57.9779266678436));
#62486=CARTESIAN_POINT('Ctrl Pts',(3.69488643041812,-5.66922422085351,57.9866762276757));
#62487=CARTESIAN_POINT('Ctrl Pts',(3.85071819468668,-5.5676617056321,57.9954257124757));
#62488=CARTESIAN_POINT('Ctrl Pts',(4.00235994599154,-5.45967053456303,58.0041751972757));
#62489=CARTESIAN_POINT('Ctrl Pts',(4.14929662974236,-5.34561750206735,58.0129246820757));
#62490=CARTESIAN_POINT('Ctrl Pts',(4.29623210224969,-5.23156540974528,58.0216740947511));
#62491=CARTESIAN_POINT('Ctrl Pts',(4.43846235842032,-5.1114517317226,58.0304235074264));
#62492=CARTESIAN_POINT('Ctrl Pts',(4.57550431797334,-4.98568443006648,58.0391729201018));
#62493=CARTESIAN_POINT('Ctrl Pts',(4.71254519337403,-4.85991812336777,58.0479222635597));
#62494=CARTESIAN_POINT('Ctrl Pts',(4.84439764314897,-4.7284984763119,58.0566716070175));
#62495=CARTESIAN_POINT('Ctrl Pts',(4.97061384196603,-4.59187184425433,58.0654209504754));
#62496=CARTESIAN_POINT('Ctrl Pts',(5.09682908420128,-4.45524624767837,58.0741702276228));
#62497=CARTESIAN_POINT('Ctrl Pts',(5.21740796650096,-4.31341395556983,58.0829195047702));
#62498=CARTESIAN_POINT('Ctrl Pts',(5.3319409594218,-4.16685668162946,58.0916687819176));
#62499=CARTESIAN_POINT('Ctrl Pts',(5.44647312235062,-4.02030046975311,58.1004179956611));
#62500=CARTESIAN_POINT('Ctrl Pts',(5.55495930712217,-3.86901957035649,58.1091672094046));
#62501=CARTESIAN_POINT('Ctrl Pts',(5.65703106079724,-3.71352778058482,58.1179164231481));
#62502=CARTESIAN_POINT('Ctrl Pts',(5.75910210868666,-3.55803706597715,58.1266655763943));
#62503=CARTESIAN_POINT('Ctrl Pts',(5.85475865698481,-3.39833575881017,58.1354147296406));
#62504=CARTESIAN_POINT('Ctrl Pts',(5.94367583068996,-3.23496624706844,58.1441638828867));
#62505=CARTESIAN_POINT('Ctrl Pts',(6.03259241910019,-3.07159781070215,58.1529129785419));
#62506=CARTESIAN_POINT('Ctrl Pts',(6.11476958470917,-2.90456146975942,58.161662074197));
#62507=CARTESIAN_POINT('Ctrl Pts',(6.18992823574342,-2.73442451648356,58.1704111698521));
#62508=CARTESIAN_POINT('Ctrl Pts',(6.26508641700891,-2.56428862662522,58.1791602108222));
#62509=CARTESIAN_POINT('Ctrl Pts',(6.33322605570254,-2.3910524253139,58.1879092517923));
#62510=CARTESIAN_POINT('Ctrl Pts',(6.39411573747726,-2.21530425353849,58.1966582927625));
#62511=CARTESIAN_POINT('Ctrl Pts',(6.45500505889081,-2.03955712188701,58.2054072819534));
#62512=CARTESIAN_POINT('Ctrl Pts',(6.50864441544883,-1.86129832025731,58.2141562711444));
#62513=CARTESIAN_POINT('Ctrl Pts',(6.5548516404986,-1.68113324012488,58.2229052603354));
#62514=CARTESIAN_POINT('Ctrl Pts',(6.60199852639072,-1.49730435913067,58.2318321672123));
#62515=CARTESIAN_POINT('Ctrl Pts',(6.64140767440979,-1.31149113173809,58.2407590740892));
#62516=CARTESIAN_POINT('Ctrl Pts',(6.67293975269578,-1.12435050446577,58.2496859809661));
#62517=CARTESIAN_POINT('Ctrl Pts',(6.70384664831486,-0.940920291565231,
58.2584358951501));
#62518=CARTESIAN_POINT('Ctrl Pts',(6.72718585889649,-0.756215114279452,
58.2671858093341));
#62519=CARTESIAN_POINT('Ctrl Pts',(6.74287810451851,-0.570862389376674,
58.2759357235181));
#62520=CARTESIAN_POINT('Ctrl Pts',(6.75857004154115,-0.385513309569632,
58.2846854656286));
#62521=CARTESIAN_POINT('Ctrl Pts',(6.76661529035551,-0.199516993260737,
58.2934352077392));
#62522=CARTESIAN_POINT('Ctrl Pts',(6.76698652348896,-0.0135052182065746,
58.3021849498498));
#62523=CARTESIAN_POINT('Ctrl Pts',(6.76735774981528,0.17250314603639,58.3109345315205));
#62524=CARTESIAN_POINT('Ctrl Pts',(6.76005524147492,0.358526681830987,58.3196841131911));
#62525=CARTESIAN_POINT('Ctrl Pts',(6.74510380214901,0.543933542112403,58.3284336948618));
#62526=CARTESIAN_POINT('Ctrl Pts',(6.73015261711005,0.72933724908232,58.3371831277237));
#62527=CARTESIAN_POINT('Ctrl Pts',(6.70755278444637,0.914124015852325,58.3459325605856));
#62528=CARTESIAN_POINT('Ctrl Pts',(6.67738106408326,1.09766621749158,58.3546819934475));
#62529=CARTESIAN_POINT('Ctrl Pts',(6.64720981677298,1.28120554143095,58.3634312891299));
#62530=CARTESIAN_POINT('Ctrl Pts',(6.60946696581573,1.46350005650393,58.3721805848122));
#62531=CARTESIAN_POINT('Ctrl Pts',(6.56428070011051,1.64393062206308,58.3809298804946));
#62532=CARTESIAN_POINT('Ctrl Pts',(6.51909508282804,1.82435859844424,58.3896790506246));
#62533=CARTESIAN_POINT('Ctrl Pts',(6.46646633415733,2.00292240086333,58.3984282207546));
#62534=CARTESIAN_POINT('Ctrl Pts',(6.40657319597271,2.17901557696222,58.4071773908846));
#62535=CARTESIAN_POINT('Ctrl Pts',(6.34668083768378,2.35510646007211,58.4159264470876));
#62536=CARTESIAN_POINT('Ctrl Pts',(6.27952437143972,2.52872650996316,58.4246755032907));
#62537=CARTESIAN_POINT('Ctrl Pts',(6.20533187335225,2.6992860799772,58.4334245594938));
#62538=CARTESIAN_POINT('Ctrl Pts',(6.12831449784346,2.87633970115199,58.4425067357826));
#62539=CARTESIAN_POINT('Ctrl Pts',(6.0437148946325,3.05009490562157,58.4515889120715));
#62540=CARTESIAN_POINT('Ctrl Pts',(5.95184265120591,3.21991584599446,58.4606710883603));
#62541=CARTESIAN_POINT('Ctrl Pts',(5.86333281335597,3.3835215590512,58.4694208687147));
#62542=CARTESIAN_POINT('Ctrl Pts',(5.76807337235793,3.54347560903648,58.4781706490692));
#62543=CARTESIAN_POINT('Ctrl Pts',(5.66638790086468,3.69923467178475,58.4869204294236));
#62544=CARTESIAN_POINT('Ctrl Pts',(5.56470608502853,3.85498813489606,58.4956698952179));
#62545=CARTESIAN_POINT('Ctrl Pts',(5.45659885767059,4.00654667256116,58.5044193610121));
#62546=CARTESIAN_POINT('Ctrl Pts',(5.3424334058061,4.15339551506079,58.5131688268064));
#62547=CARTESIAN_POINT('Ctrl Pts',(5.22827145140693,4.3002398588375,58.5219180245603));
#62548=CARTESIAN_POINT('Ctrl Pts',(5.10805181978185,4.44237456992933,58.5306672223141));
#62549=CARTESIAN_POINT('Ctrl Pts',(4.98218281282642,4.5793169162635,58.539416420068));
#62550=CARTESIAN_POINT('Ctrl Pts',(4.85631699296316,4.71625579512072,58.548165396286));
#62551=CARTESIAN_POINT('Ctrl Pts',(4.72480227791921,4.84800236135689,58.556914372504));
#62552=CARTESIAN_POINT('Ctrl Pts',(4.58808530848191,4.97410918678837,58.5656633487221));
#62553=CARTESIAN_POINT('Ctrl Pts',(4.45135945057053,5.10022421088936,58.5744128937433));
#62554=CARTESIAN_POINT('Ctrl Pts',(4.30943087208128,5.22069856611913,58.5831624387645));
#62555=CARTESIAN_POINT('Ctrl Pts',(4.16278164322561,5.3351230530161,58.5919119837856));
#62556=CARTESIAN_POINT('Ctrl Pts',(4.01614103534492,5.44954081331352,58.6006610144529));
#62557=CARTESIAN_POINT('Ctrl Pts',(3.86478055833522,5.55790924068262,58.6094100451201));
#62558=CARTESIAN_POINT('Ctrl Pts',(3.70921425812068,5.65986029751214,58.6181590757874));
#62559=CARTESIAN_POINT('Ctrl Pts',(3.55364584530241,5.76181273884579,58.6269082252672));
#62560=CARTESIAN_POINT('Ctrl Pts',(3.39387173464469,5.85734747817991,58.6356573747471));
#62561=CARTESIAN_POINT('Ctrl Pts',(3.23043456092534,5.94614005448738,58.6444065242269));
#62562=CARTESIAN_POINT('Ctrl Pts',(3.18690768806476,5.96978744811237,58.64673661296));
#62563=CARTESIAN_POINT('Ctrl Pts',(3.1431211498292,5.99295688499281,58.6490667016931));
#62564=CARTESIAN_POINT('Ctrl Pts',(3.09908550384712,6.01564277861017,58.6513967904261));
#62565=CARTESIAN_POINT('Origin',(0.,0.,0.));
#62566=CARTESIAN_POINT('',(-7.91099963985057,0.00238710789585057,-59.3576684805928));
#62567=CARTESIAN_POINT('',(3.42067962509752,7.13322310757505,-60.));
#62568=CARTESIAN_POINT('Ctrl Pts',(-7.91099962156735,0.00238334057144554,
-59.3577643889973));
#62569=CARTESIAN_POINT('Ctrl Pts',(-7.9103007141194,2.20325225569619,-59.4463198589853));
#62570=CARTESIAN_POINT('Ctrl Pts',(-6.94155688867303,4.38663744883245,-59.5348753289732));
#62571=CARTESIAN_POINT('Ctrl Pts',(-3.67820201488299,7.34180684107625,-59.7120182346939));
#62572=CARTESIAN_POINT('Ctrl Pts',(-1.40868175871762,8.08992666571332,-59.8006056704266));
#62573=CARTESIAN_POINT('Ctrl Pts',(1.69567364519639,7.78146992497721,-59.9261287374395));
#62574=CARTESIAN_POINT('Ctrl Pts',(2.5929638990806,7.53014751000292,-59.9630643687198));
#62575=CARTESIAN_POINT('Ctrl Pts',(3.42067962509752,7.13322310757505,-60.));
#62576=CARTESIAN_POINT('',(-3.4206796250969,7.13322310757535,-60.));
#62577=CARTESIAN_POINT('Origin',(0.,0.,-60.));
#62578=CARTESIAN_POINT('',(-7.91099727798874,0.000376848761340583,-57.6331939826542));
#62579=CARTESIAN_POINT('Ctrl Pts',(-3.4206796250969,7.13322310757535,-60.));
#62580=CARTESIAN_POINT('Ctrl Pts',(-3.4459264372686,7.12111620236687,-59.9988733970903));
#62581=CARTESIAN_POINT('Ctrl Pts',(-3.47110875087086,7.10887536904488,-59.9977454074563));
#62582=CARTESIAN_POINT('Ctrl Pts',(-3.53231864403775,7.07871915747642,-59.9949935134598));
#62583=CARTESIAN_POINT('Ctrl Pts',(-3.56827552297465,7.06066212837666,-59.9933683534081));
#62584=CARTESIAN_POINT('Ctrl Pts',(-3.73986127625415,6.9728487385684,-59.985573364225));
#62585=CARTESIAN_POINT('Ctrl Pts',(-3.87359132289936,6.89945445647857,-59.9793789923031));
#62586=CARTESIAN_POINT('Ctrl Pts',(-4.14154292460681,6.74214879691367,-59.9667494258034));
#62587=CARTESIAN_POINT('Ctrl Pts',(-4.27553746991937,6.65798225487813,-59.9603167584883));
#62588=CARTESIAN_POINT('Ctrl Pts',(-4.50324071723858,6.50524378023639,-59.9491914171497));
#62589=CARTESIAN_POINT('Ctrl Pts',(-4.59813091208061,6.438522027936,-59.9444936391356));
#62590=CARTESIAN_POINT('Ctrl Pts',(-4.72878633738448,6.34229003878124,-59.9379374915465));
#62591=CARTESIAN_POINT('Ctrl Pts',(-4.76581109958602,6.31451563768646,-59.936069455004));
#62592=CARTESIAN_POINT('Ctrl Pts',(-4.83839149732099,6.25906690631354,-59.9323870354179));
#62593=CARTESIAN_POINT('Ctrl Pts',(-4.87395870121748,6.23141054757177,-59.9305726128382));
#62594=CARTESIAN_POINT('Ctrl Pts',(-4.94434822953616,6.17570568186931,-59.926961558764));
#62595=CARTESIAN_POINT('Ctrl Pts',(-4.97917289452374,6.14766275790506,-59.9251649617938));
#62596=CARTESIAN_POINT('Ctrl Pts',(-5.07527846604082,6.06892041372507,-59.9201781018495));
#62597=CARTESIAN_POINT('Ctrl Pts',(-5.13603547531563,6.01758973112876,-59.9169924759526));
#62598=CARTESIAN_POINT('Ctrl Pts',(-5.3929838235426,5.79377965768501,-59.903369340895));
#62599=CARTESIAN_POINT('Ctrl Pts',(-5.581341431085,5.61255616283981,-59.8930031273601));
#62600=CARTESIAN_POINT('Ctrl Pts',(-5.887524466436,5.28728490298797,-59.8752917929499));
#62601=CARTESIAN_POINT('Ctrl Pts',(-6.00987007291324,5.1477944078182,-59.8679462273013));
#62602=CARTESIAN_POINT('Ctrl Pts',(-6.18641501837817,4.93162790625738,-59.856841896567));
#62603=CARTESIAN_POINT('Ctrl Pts',(-6.24433900024942,4.85807728042496,-59.8531092781247));
#62604=CARTESIAN_POINT('Ctrl Pts',(-6.30270618684108,4.78119485258985,-59.8492451466788));
#62605=CARTESIAN_POINT('Ctrl Pts',(-6.3044673868978,4.77887230040852,-59.8491284493683));
#62606=CARTESIAN_POINT('Ctrl Pts',(-6.30714241262381,4.77534060397661,-59.8489510506931));
#62607=CARTESIAN_POINT('Ctrl Pts',(-6.3080571753171,4.77413216930942,-59.8488903598089));
#62608=CARTESIAN_POINT('Ctrl Pts',(-6.31081668684292,4.7704845768176,-59.8487071957852));
#62609=CARTESIAN_POINT('Ctrl Pts',(-6.31266036833301,4.7680446124863,-59.8485847106565));
#62610=CARTESIAN_POINT('Ctrl Pts',(-6.32865199990914,4.74685543927622,-59.8475213487363));
#62611=CARTESIAN_POINT('Ctrl Pts',(-6.34271777491939,4.72804440770974,-59.8465795411014));
#62612=CARTESIAN_POINT('Ctrl Pts',(-6.36857658136316,4.69313876052984,-59.8448357349542));
#62613=CARTESIAN_POINT('Ctrl Pts',(-6.3803929074599,4.67706162479774,-59.8440340384655));
#62614=CARTESIAN_POINT('Ctrl Pts',(-6.40456487313833,4.64391149006302,-59.842383837772));
#62615=CARTESIAN_POINT('Ctrl Pts',(-6.41691333586168,4.62683351543582,-59.8415352287777));
#62616=CARTESIAN_POINT('Ctrl Pts',(-6.4486980556545,4.58250311890471,-59.8393362602182));
#62617=CARTESIAN_POINT('Ctrl Pts',(-6.46802978504492,4.5551764110769,-59.8379845292245));
#62618=CARTESIAN_POINT('Ctrl Pts',(-6.59223271260789,4.37722232710768,-59.8292084583593));
#62619=CARTESIAN_POINT('Ctrl Pts',(-6.69200795852055,4.2231074175154,-59.8217323044393));
#62620=CARTESIAN_POINT('Ctrl Pts',(-6.86784288495032,3.92960689993277,-59.8077962574485));
#62621=CARTESIAN_POINT('Ctrl Pts',(-6.94524387020208,3.79112968113832,-59.8013390675116));
#62622=CARTESIAN_POINT('Ctrl Pts',(-7.04996389827288,3.58979110454189,-59.7921343906334));
#62623=CARTESIAN_POINT('Ctrl Pts',(-7.08071087612344,3.52875681902811,-59.7893673585976));
#62624=CARTESIAN_POINT('Ctrl Pts',(-7.12891734355118,3.42989694827871,-59.7849231196874));
#62625=CARTESIAN_POINT('Ctrl Pts',(-7.14687554257249,3.39231861136134,-59.7832424107286));
#62626=CARTESIAN_POINT('Ctrl Pts',(-7.16957043761407,3.34384833461796,-59.7810855577106));
#62627=CARTESIAN_POINT('Ctrl Pts',(-7.17458047216048,3.33308520648557,-59.7806073077722));
#62628=CARTESIAN_POINT('Ctrl Pts',(-7.19244536492334,3.29447889065369,-59.778894344821));
#62629=CARTESIAN_POINT('Ctrl Pts',(-7.20516254188411,3.26657224622705,-59.7776607302692));
#62630=CARTESIAN_POINT('Ctrl Pts',(-7.23015905452989,3.21086354920085,-59.7752071867263));
#62631=CARTESIAN_POINT('Ctrl Pts',(-7.24244108764251,3.18306327046938,-59.7739872546977));
#62632=CARTESIAN_POINT('Ctrl Pts',(-7.27045336588329,3.11865616885249,-59.7711710868554));
#62633=CARTESIAN_POINT('Ctrl Pts',(-7.28606788640061,3.08199987253495,-59.769575836333));
#62634=CARTESIAN_POINT('Ctrl Pts',(-7.32534676476923,2.98782266210745,-59.7654960925743));
#62635=CARTESIAN_POINT('Ctrl Pts',(-7.34861093754915,2.93013768054889,-59.7630150036069));
#62636=CARTESIAN_POINT('Ctrl Pts',(-7.48787000943251,2.57274227276288,-59.7477467210624));
#62637=CARTESIAN_POINT('Ctrl Pts',(-7.58619303541677,2.26646819955346,-59.7351263362707));
#62638=CARTESIAN_POINT('Ctrl Pts',(-7.72505206006592,1.72201487909103,-59.7130348060401));
#62639=CARTESIAN_POINT('Ctrl Pts',(-7.7738297566213,1.48638218733415,-59.7035770834101));
#62640=CARTESIAN_POINT('Ctrl Pts',(-7.81636392565079,1.22033307449028,-59.6928082845712));
#62641=CARTESIAN_POINT('Ctrl Pts',(-7.82077402221008,1.19174305676959,-59.6916498278369));
#62642=CARTESIAN_POINT('Ctrl Pts',(-7.82716829164918,1.14872520855486,-59.6899043567589));
#62643=CARTESIAN_POINT('Ctrl Pts',(-7.8292696099069,1.13431496701531,-59.6893192487828));
#62644=CARTESIAN_POINT('Ctrl Pts',(-7.83325541747186,1.10644265180621,-59.688186654681));
#62645=CARTESIAN_POINT('Ctrl Pts',(-7.8351450226978,1.09298135804842,-59.6876392586051));
#62646=CARTESIAN_POINT('Ctrl Pts',(-7.83879606303384,1.0664757557661,-59.6865605662517));
#62647=CARTESIAN_POINT('Ctrl Pts',(-7.84055965627872,1.05343178731285,-59.6860293109369));
#62648=CARTESIAN_POINT('Ctrl Pts',(-7.84457499133327,1.02316465542566,-59.6847955581156));
#62649=CARTESIAN_POINT('Ctrl Pts',(-7.84680257931179,1.00593836103101,-59.6840926026132));
#62650=CARTESIAN_POINT('Ctrl Pts',(-7.85493373560022,0.941388028693867,
-59.6814552734856));
#62651=CARTESIAN_POINT('Ctrl Pts',(-7.86046602801377,0.8940185521262,-59.6795134996335));
#62652=CARTESIAN_POINT('Ctrl Pts',(-7.90202460416147,0.507908237927866,
-59.6636408433056));
#62653=CARTESIAN_POINT('Ctrl Pts',(-7.9165644024708,0.167219606303168,-59.6493630031096));
#62654=CARTESIAN_POINT('Ctrl Pts',(-7.90255536625646,-0.471997523821098,
-59.6225177961226));
#62655=CARTESIAN_POINT('Ctrl Pts',(-7.87909802108942,-0.770052694171588,
-59.6099767063755));
#62656=CARTESIAN_POINT('Ctrl Pts',(-7.81495291347873,-1.24171419120209,
-59.5901979168344));
#62657=CARTESIAN_POINT('Ctrl Pts',(-7.78516824712496,-1.41650983377954,
-59.5828810171525));
#62658=CARTESIAN_POINT('Ctrl Pts',(-7.72620181574655,-1.70387885600593,
-59.5708678846878));
#62659=CARTESIAN_POINT('Ctrl Pts',(-7.70036670579315,-1.81707202261445,
-59.5661398954469));
#62660=CARTESIAN_POINT('Ctrl Pts',(-7.66229985999402,-1.9684205752268,-59.5598181584276));
#62661=CARTESIAN_POINT('Ctrl Pts',(-7.65225635196562,-2.00711022340071,
-59.5582020923904));
#62662=CARTESIAN_POINT('Ctrl Pts',(-7.63562138922832,-2.06925114082611,
-59.5556060668173));
#62663=CARTESIAN_POINT('Ctrl Pts',(-7.62921411121102,-2.09275090087644,
-59.5546242375841));
#62664=CARTESIAN_POINT('Ctrl Pts',(-7.61564438710486,-2.1416295042748,-59.5525817573179));
#62665=CARTESIAN_POINT('Ctrl Pts',(-7.60846336906581,-2.16700289142561,
-59.5515213084641));
#62666=CARTESIAN_POINT('Ctrl Pts',(-7.59174790765712,-2.22495778262732,
-59.5490985741664));
#62667=CARTESIAN_POINT('Ctrl Pts',(-7.58213033106392,-2.25751480215078,
-59.5477371452025));
#62668=CARTESIAN_POINT('Ctrl Pts',(-7.55587237897535,-2.34434117835645,
-59.5441047338352));
#62669=CARTESIAN_POINT('Ctrl Pts',(-7.53885694212114,-2.39849515819621,
-59.5418374981111));
#62670=CARTESIAN_POINT('Ctrl Pts',(-7.43319341199761,-2.72254627372299,
-59.5282547819213));
#62671=CARTESIAN_POINT('Ctrl Pts',(-7.33064037972315,-2.98769795250401,
-59.5170527560092));
#62672=CARTESIAN_POINT('Ctrl Pts',(-6.97638573002518,-3.77482444152793,
-59.4833575876151));
#62673=CARTESIAN_POINT('Ctrl Pts',(-6.68146134200265,-4.27520317095094,
-59.4616208667055));
#62674=CARTESIAN_POINT('Ctrl Pts',(-6.11934654606272,-5.02658863221662,
-59.4266599583711));
#62675=CARTESIAN_POINT('Ctrl Pts',(-5.88479468297627,-5.29926116520742,
-59.4133255803661));
#62676=CARTESIAN_POINT('Ctrl Pts',(-5.54778736634356,-5.64097003549056,
-59.3947698599548));
#62677=CARTESIAN_POINT('Ctrl Pts',(-5.46108495315945,-5.72494866829096,
-59.3900409529335));
#62678=CARTESIAN_POINT('Ctrl Pts',(-5.36004982944706,-5.81842542396096,
-59.3845425792284));
#62679=CARTESIAN_POINT('Ctrl Pts',(-5.34756489296684,-5.82990208312555,
-59.3838633471491));
#62680=CARTESIAN_POINT('Ctrl Pts',(-5.32863549398049,-5.84719078539398,
-59.3828336706946));
#62681=CARTESIAN_POINT('Ctrl Pts',(-5.32221817112008,-5.85303255131997,
-59.3824846242076));
#62682=CARTESIAN_POINT('Ctrl Pts',(-5.31116841896764,-5.86305807480769,
-59.3818836392594));
#62683=CARTESIAN_POINT('Ctrl Pts',(-5.306540618737,-5.86724693741863,-59.3816319454594));
#62684=CARTESIAN_POINT('Ctrl Pts',(-5.29700207877371,-5.87586024924435,
-59.3811131751957));
#62685=CARTESIAN_POINT('Ctrl Pts',(-5.29209074335091,-5.88028402842771,
-59.3808460666681));
#62686=CARTESIAN_POINT('Ctrl Pts',(-5.28025946536739,-5.89091396818371,
-59.3802026027233));
#62687=CARTESIAN_POINT('Ctrl Pts',(-5.27333412678471,-5.8971140898339,-59.3798259511921));
#62688=CARTESIAN_POINT('Ctrl Pts',(-5.24797698068945,-5.91973546705514,
-59.3784467619585));
#62689=CARTESIAN_POINT('Ctrl Pts',(-5.22947938152763,-5.93608252722146,
-59.3774405161016));
#62690=CARTESIAN_POINT('Ctrl Pts',(-4.91736416025596,-6.20931998904849,
-59.3604541820488));
#62691=CARTESIAN_POINT('Ctrl Pts',(-4.60527531323464,-6.44417906201417,
-59.3431486505051));
#62692=CARTESIAN_POINT('Ctrl Pts',(-3.91638842436794,-6.88692919797293,
-59.3060294077928));
#62693=CARTESIAN_POINT('Ctrl Pts',(-3.53728693960655,-7.08911259424554,
-59.2862585949185));
#62694=CARTESIAN_POINT('Ctrl Pts',(-2.87658924348169,-7.37521922655691,
-59.2541881757267));
#62695=CARTESIAN_POINT('Ctrl Pts',(-2.60332435251557,-7.47605157714246,
-59.2415434614148));
#62696=CARTESIAN_POINT('Ctrl Pts',(-2.20581565289815,-7.59828099225087,
-59.2241381129987));
#62697=CARTESIAN_POINT('Ctrl Pts',(-2.08567057548906,-7.63213448379057,
-59.2190005874771));
#62698=CARTESIAN_POINT('Ctrl Pts',(-1.94627435684804,-7.66787465666578,
-59.2131793898532));
#62699=CARTESIAN_POINT('Ctrl Pts',(-1.92776036488935,-7.67255013697899,
-59.2124090495315));
#62700=CARTESIAN_POINT('Ctrl Pts',(-1.89966519369616,-7.67953711405647,
-59.211244277576));
#62701=CARTESIAN_POINT('Ctrl Pts',(-1.89009638579219,-7.68189779856543,
-59.2108483151821));
#62702=CARTESIAN_POINT('Ctrl Pts',(-1.87352604788985,-7.68595296887718,
-59.2101639055587));
#62703=CARTESIAN_POINT('Ctrl Pts',(-1.86652657934321,-7.68765578189194,
-59.2098751992342));
#62704=CARTESIAN_POINT('Ctrl Pts',(-1.85200667935601,-7.69116714725609,
-59.2092771149652));
#62705=CARTESIAN_POINT('Ctrl Pts',(-1.84448589963048,-7.69297423587983,
-59.2089677828621));
#62706=CARTESIAN_POINT('Ctrl Pts',(-1.8262067778567,-7.6973379867607,-59.2082170557314));
#62707=CARTESIAN_POINT('Ctrl Pts',(-1.81544568860651,-7.69988313098826,
-59.2077760199063));
#62708=CARTESIAN_POINT('Ctrl Pts',(-1.775053658752,-7.70934701301787,-59.20612403128));
#62709=CARTESIAN_POINT('Ctrl Pts',(-1.74538804702498,-7.71611738178104,
-59.2049177035166));
#62710=CARTESIAN_POINT('Ctrl Pts',(-1.27515424950573,-7.82058483957626,
-59.1859046151966));
#62711=CARTESIAN_POINT('Ctrl Pts',(-0.827043152580916,-7.88058525983827,
-59.1693598710052));
#62712=CARTESIAN_POINT('Ctrl Pts',(-0.237690842262585,-7.90864448060468,
-59.1486528950393));
#62713=CARTESIAN_POINT('Ctrl Pts',(-0.0990120393069514,-7.91159604499181,
-59.1438502081861));
#62714=CARTESIAN_POINT('Ctrl Pts',(0.476889815531139,-7.90870782026273,
-59.1240447092042));
#62715=CARTESIAN_POINT('Ctrl Pts',(0.91315294975192,-7.87027366434301,-59.1094105838292));
#62716=CARTESIAN_POINT('Ctrl Pts',(1.52876823838439,-7.76414498771538,-59.0871505562018));
#62717=CARTESIAN_POINT('Ctrl Pts',(1.71234985434018,-7.72573175310781,-59.0802962568309));
#62718=CARTESIAN_POINT('Ctrl Pts',(1.9622733308688,-7.66409118506773,-59.0704754096278));
#62719=CARTESIAN_POINT('Ctrl Pts',(2.02993596545076,-7.6464481827517,-59.0677664877448));
#62720=CARTESIAN_POINT('Ctrl Pts',(2.13413635877705,-7.61779746504728,-59.0635056615875));
#62721=CARTESIAN_POINT('Ctrl Pts',(2.17084438644799,-7.60741814130901,-59.0619874244073));
#62722=CARTESIAN_POINT('Ctrl Pts',(2.21587631772579,-7.59433273436178,-59.0601022234073));
#62723=CARTESIAN_POINT('Ctrl Pts',(2.2242732068877,-7.59187764888496,-59.0597497262076));
#62724=CARTESIAN_POINT('Ctrl Pts',(2.23743663351647,-7.58800520821032,-59.0591955829961));
#62725=CARTESIAN_POINT('Ctrl Pts',(2.24220595743785,-7.58659727236446,-59.0589944885884));
#62726=CARTESIAN_POINT('Ctrl Pts',(2.25066077169313,-7.58409268642563,-59.0586374276204));
#62727=CARTESIAN_POINT('Ctrl Pts',(2.2543467994072,-7.58299784342751,-59.0584815678906));
#62728=CARTESIAN_POINT('Ctrl Pts',(2.26219731879996,-7.58065981161029,-59.0581492040888));
#62729=CARTESIAN_POINT('Ctrl Pts',(2.26636158586512,-7.57941587792406,-59.0579726557118));
#62730=CARTESIAN_POINT('Ctrl Pts',(2.27828958108099,-7.57584208445301,-59.0574662410867));
#62731=CARTESIAN_POINT('Ctrl Pts',(2.28605073609237,-7.57350372911317,-59.0571358653761));
#62732=CARTESIAN_POINT('Ctrl Pts',(2.32033766784586,-7.56311592657507,-59.0556724538278));
#62733=CARTESIAN_POINT('Ctrl Pts',(2.34682352638379,-7.5549393563353,-59.0545315695538));
#62734=CARTESIAN_POINT('Ctrl Pts',(2.79279801382885,-7.41468909035607,-59.0351483538088));
#62735=CARTESIAN_POINT('Ctrl Pts',(3.20056175071994,-7.24801127253715,-59.0148990901773));
#62736=CARTESIAN_POINT('Ctrl Pts',(4.01246070454874,-6.83421176941562,-58.972413498533));
#62737=CARTESIAN_POINT('Ctrl Pts',(4.41264946758004,-6.58292342671961,-58.9502529872018));
#62738=CARTESIAN_POINT('Ctrl Pts',(4.98165656842049,-6.1502966555222,-58.9184213497782));
#62739=CARTESIAN_POINT('Ctrl Pts',(5.16834832232988,-5.99426737959803,-58.9079004679273));
#62740=CARTESIAN_POINT('Ctrl Pts',(5.42701160047605,-5.75700334724194,-58.8932587613058));
#62741=CARTESIAN_POINT('Ctrl Pts',(5.50495925989744,-5.68251417274034,-58.888836268167));
#62742=CARTESIAN_POINT('Ctrl Pts',(5.59326921457186,-5.59459942867227,-58.8838115436756));
#62743=CARTESIAN_POINT('Ctrl Pts',(5.60513819703576,-5.58270804100133,-58.8831359008525));
#62744=CARTESIAN_POINT('Ctrl Pts',(5.62309381999027,-5.56460353813917,-58.8821132780589));
#62745=CARTESIAN_POINT('Ctrl Pts',(5.62920820561393,-5.55841808643556,-58.8817649586013));
#62746=CARTESIAN_POINT('Ctrl Pts',(5.63978114828469,-5.54768691809375,-58.8811624909846));
#62747=CARTESIAN_POINT('Ctrl Pts',(5.64424443420745,-5.54314588558856,-58.8809081153956));
#62748=CARTESIAN_POINT('Ctrl Pts',(5.65349533536068,-5.53371108416854,-58.8803807770538));
#62749=CARTESIAN_POINT('Ctrl Pts',(5.65828209142069,-5.52881647771395,-58.880107855544));
#62750=CARTESIAN_POINT('Ctrl Pts',(5.67132284621369,-5.51544722771031,-58.8793641647569));
#62751=CARTESIAN_POINT('Ctrl Pts',(5.67956421538554,-5.50696025704371,-58.8788939994189));
#62752=CARTESIAN_POINT('Ctrl Pts',(5.7107014355378,-5.47475086950203,-58.877116951627));
#62753=CARTESIAN_POINT('Ctrl Pts',(5.73346811158974,-5.45090372496284,-58.8758162121081));
#62754=CARTESIAN_POINT('Ctrl Pts',(6.10917135080501,-5.05241213819627,-58.8543248382643));
#62755=CARTESIAN_POINT('Ctrl Pts',(6.42488629524542,-4.6443251986883,-58.8360038212009));
#62756=CARTESIAN_POINT('Ctrl Pts',(7.07990477990277,-3.60170424344757,-58.7939700944));
#62757=CARTESIAN_POINT('Ctrl Pts',(7.37681372107505,-2.94611794032011,-58.7712334759982));
#62758=CARTESIAN_POINT('Ctrl Pts',(7.59325028642241,-2.21995242192804,-58.7415007279314));
#62759=CARTESIAN_POINT('Ctrl Pts',(7.60477599339017,-2.1801423548741,-58.7398561056385));
#62760=CARTESIAN_POINT('Ctrl Pts',(7.61821263001633,-2.1323285220095,-58.7378612931551));
#62761=CARTESIAN_POINT('Ctrl Pts',(7.62042467266289,-2.12440966134322,-58.7375302794479));
#62762=CARTESIAN_POINT('Ctrl Pts',(7.62403348362295,-2.11141236667999,-58.7369859581946));
#62763=CARTESIAN_POINT('Ctrl Pts',(7.62543753704038,-2.10633594423047,-58.7367731033253));
#62764=CARTESIAN_POINT('Ctrl Pts',(7.62794608626106,-2.09723078268198,-58.7363908681864));
#62765=CARTESIAN_POINT('Ctrl Pts',(7.6290524644497,-2.09320255715398,-58.7362216035491));
#62766=CARTESIAN_POINT('Ctrl Pts',(7.63139189969614,-2.08465838628327,-58.7358622450738));
#62767=CARTESIAN_POINT('Ctrl Pts',(7.63262413951624,-2.08014222084407,-58.735672101534));
#62768=CARTESIAN_POINT('Ctrl Pts',(7.63589908407241,-2.06809744225059,-58.7351644574492));
#62769=CARTESIAN_POINT('Ctrl Pts',(7.63793465841979,-2.06056691365319,-58.7348465268661));
#62770=CARTESIAN_POINT('Ctrl Pts',(7.64739334118732,-2.02536829054338,-58.7333579710847));
#62771=CARTESIAN_POINT('Ctrl Pts',(7.65467718357615,-1.99766333537058,-58.7321790854677));
#62772=CARTESIAN_POINT('Ctrl Pts',(7.71024991795732,-1.78151862068495,-58.7229288553855));
#62773=CARTESIAN_POINT('Ctrl Pts',(7.75172079547663,-1.59140716676455,-58.7144804942424));
#62774=CARTESIAN_POINT('Ctrl Pts',(7.87261211728222,-0.919054488189767,
-58.6839708052031));
#62775=CARTESIAN_POINT('Ctrl Pts',(7.91433893120551,-0.431169202491736,
-58.660768834043));
#62776=CARTESIAN_POINT('Ctrl Pts',(7.90632283241643,0.672926640116866,-58.609447729467));
#62777=CARTESIAN_POINT('Ctrl Pts',(7.83003965222594,1.28587526484475,-58.5819068285109));
#62778=CARTESIAN_POINT('Ctrl Pts',(7.67396649017517,1.92242992753545,-58.5551605778619));
#62779=CARTESIAN_POINT('Ctrl Pts',(7.66421794379883,1.96093393288385,-58.5535491780094));
#62780=CARTESIAN_POINT('Ctrl Pts',(7.65083471628223,2.01216905891255,-58.5514132957557));
#62781=CARTESIAN_POINT('Ctrl Pts',(7.64745754802089,2.02496647650056,-58.5508804925977));
#62782=CARTESIAN_POINT('Ctrl Pts',(7.64189341264258,2.04583871632838,-58.5500126236111));
#62783=CARTESIAN_POINT('Ctrl Pts',(7.63972573204582,2.05391862621002,-58.5496769344199));
#62784=CARTESIAN_POINT('Ctrl Pts',(7.63555689422966,2.06935983041954,-58.5490359312259));
#62785=CARTESIAN_POINT('Ctrl Pts',(7.63355789866526,2.07672169558616,-58.5487305477267));
#62786=CARTESIAN_POINT('Ctrl Pts',(7.6289919149959,2.09344154966,-58.5480374874218));
#62787=CARTESIAN_POINT('Ctrl Pts',(7.62641834904931,2.1027977380295,-58.5476500239188));
#62788=CARTESIAN_POINT('Ctrl Pts',(7.61854584390188,2.13121363880509,-58.5464743408914));
#62789=CARTESIAN_POINT('Ctrl Pts',(7.61319260330413,2.15025829660143,-58.5456878787417));
#62790=CARTESIAN_POINT('Ctrl Pts',(7.56402878554174,2.32267792017561,-58.5385809194193));
#62791=CARTESIAN_POINT('Ctrl Pts',(7.51565901637437,2.47471962895778,-58.5324099532277));
#62792=CARTESIAN_POINT('Ctrl Pts',(7.3739742728133,2.87749039789218,-58.5162519161989));
#62793=CARTESIAN_POINT('Ctrl Pts',(7.27248564354219,3.12512584812754,-58.5065233425138));
#62794=CARTESIAN_POINT('Ctrl Pts',(7.07126113877967,3.5529334834802,-58.4897312974183));
#62795=CARTESIAN_POINT('Ctrl Pts',(6.97667819462898,3.73524215531146,-58.482578256606));
#62796=CARTESIAN_POINT('Ctrl Pts',(6.58220468137923,4.42821083809226,-58.4549079593774));
#62797=CARTESIAN_POINT('Ctrl Pts',(6.23245577683505,4.90825688708141,-58.4347148077986));
#62798=CARTESIAN_POINT('Ctrl Pts',(5.80177952933379,5.37822775221955,-58.4095976786779));
#62799=CARTESIAN_POINT('Ctrl Pts',(5.77083995151678,5.411412533882,-58.4077948022521));
#62800=CARTESIAN_POINT('Ctrl Pts',(5.73012878427687,5.45433178309791,-58.4054262504025));
#62801=CARTESIAN_POINT('Ctrl Pts',(5.72061443048031,5.46430980266998,-58.4048729718365));
#62802=CARTESIAN_POINT('Ctrl Pts',(5.705362606649,5.48022140535944,-58.4039865227265));
#62803=CARTESIAN_POINT('Ctrl Pts',(5.69964182742705,5.48617099292213,-58.4036541322502));
#62804=CARTESIAN_POINT('Ctrl Pts',(5.68931683244669,5.49687536577112,-58.4030544311775));
#62805=CARTESIAN_POINT('Ctrl Pts',(5.68471593614967,5.50163335126914,-58.4027872728435));
#62806=CARTESIAN_POINT('Ctrl Pts',(5.67390329032995,5.51278713030602,-58.4021595999697));
#62807=CARTESIAN_POINT('Ctrl Pts',(5.66768669515483,5.5191782012303,-58.4017988667234));
#62808=CARTESIAN_POINT('Ctrl Pts',(5.64971801805141,5.53758881622766,-58.4007566194385));
#62809=CARTESIAN_POINT('Ctrl Pts',(5.6379384449675,5.54958139568611,-58.400073890485));
#62810=CARTESIAN_POINT('Ctrl Pts',(5.55748597211704,5.63096813958138,-58.3954149885322));
#62811=CARTESIAN_POINT('Ctrl Pts',(5.48757303144064,5.69912221248253,-58.3913863832793));
#62812=CARTESIAN_POINT('Ctrl Pts',(5.24799744073205,5.924174207527,-58.3776868363816));
#62813=CARTESIAN_POINT('Ctrl Pts',(5.07272922687759,6.07492637077634,-58.3678406087008));
#62814=CARTESIAN_POINT('Ctrl Pts',(4.56671258868079,6.47297601319317,-58.3402252236996));
#62815=CARTESIAN_POINT('Ctrl Pts',(4.22282339294515,6.70239183842981,-58.3223895227089));
#62816=CARTESIAN_POINT('Ctrl Pts',(3.32694261274612,7.2036188589356,-58.2787652400962));
#62817=CARTESIAN_POINT('Ctrl Pts',(2.75820443675451,7.43996087664976,-58.2534134599075));
#62818=CARTESIAN_POINT('Ctrl Pts',(2.09783073103737,7.62812762666884,-58.2254922928406));
#62819=CARTESIAN_POINT('Ctrl Pts',(2.0275182751841,7.64711675275886,-58.2225408133375));
#62820=CARTESIAN_POINT('Ctrl Pts',(1.93007900803549,7.67199356902648,-58.2184800547628));
#62821=CARTESIAN_POINT('Ctrl Pts',(1.90316880504124,7.67871335622515,-58.2173616519004));
#62822=CARTESIAN_POINT('Ctrl Pts',(1.856840747658,7.69002350651805,-58.2154414777458));
#62823=CARTESIAN_POINT('Ctrl Pts',(1.83743987325117,7.6946821771822,-58.2146389398095));
#62824=CARTESIAN_POINT('Ctrl Pts',(1.79735988808042,7.7041462304307,-58.2129842182205));
#62825=CARTESIAN_POINT('Ctrl Pts',(1.77667863429032,7.70894186908173,-58.2121321527477));
#62826=CARTESIAN_POINT('Ctrl Pts',(1.72835992617602,7.71994140317062,-58.210145518529));
#62827=CARTESIAN_POINT('Ctrl Pts',(1.70070792937487,7.72608023836373,-58.2090117183649));
#62828=CARTESIAN_POINT('Ctrl Pts',(1.6111773099385,7.74545238850073,-58.2053506612399));
#62829=CARTESIAN_POINT('Ctrl Pts',(1.54917247353694,7.75809188923687,-58.2028304873983));
#62830=CARTESIAN_POINT('Ctrl Pts',(1.23404542944061,7.81840099921673,-58.1900959851136));
#62831=CARTESIAN_POINT('Ctrl Pts',(0.978851326724744,7.85443297248859,-58.1800297517057));
#62832=CARTESIAN_POINT('Ctrl Pts',(0.454569647660311,7.9025057080662,-58.1596538546884));
#62833=CARTESIAN_POINT('Ctrl Pts',(0.185711353493977,7.91339008240242,-58.1493665080907));
#62834=CARTESIAN_POINT('Ctrl Pts',(-0.283888863772529,7.90845223810738,
-58.1313444569159));
#62835=CARTESIAN_POINT('Ctrl Pts',(-0.48444283122238,7.89870387312902,-58.1236286385092));
#62836=CARTESIAN_POINT('Ctrl Pts',(-0.834019387507697,7.86834707379376,
-58.1099588789463));
#62837=CARTESIAN_POINT('Ctrl Pts',(-0.983229693180036,7.85109747139714,
-58.1040527964759));
#62838=CARTESIAN_POINT('Ctrl Pts',(-1.15318616015388,7.8265284259937,-58.0971844010288));
#62839=CARTESIAN_POINT('Ctrl Pts',(-1.17450432832977,7.82335766167694,-58.0963202998011));
#62840=CARTESIAN_POINT('Ctrl Pts',(-1.20926241530967,7.81804263396186,-58.0949070516125));
#62841=CARTESIAN_POINT('Ctrl Pts',(-1.22271006623472,7.81595076159331,-58.094359220368));
#62842=CARTESIAN_POINT('Ctrl Pts',(-1.2469190813266,7.81212087920173,-58.0933711333621));
#62843=CARTESIAN_POINT('Ctrl Pts',(-1.25768239115995,7.81039530553384,-58.0929311682447));
#62844=CARTESIAN_POINT('Ctrl Pts',(-1.28062793535186,7.80666801552453,-58.0919918507307));
#62845=CARTESIAN_POINT('Ctrl Pts',(-1.292809115668,7.80466001838646,-58.091492357611));
#62846=CARTESIAN_POINT('Ctrl Pts',(-1.32563273935285,7.79917028105371,-58.0901442121902));
#62847=CARTESIAN_POINT('Ctrl Pts',(-1.34626610163646,7.79563511269136,-58.0892944001892));
#62848=CARTESIAN_POINT('Ctrl Pts',(-1.44848928509931,7.77770299979589,-58.0850729666095));
#62849=CARTESIAN_POINT('Ctrl Pts',(-1.52986264908757,7.76210700315878,-58.0816770584102));
#62850=CARTESIAN_POINT('Ctrl Pts',(-1.76729348753218,7.71272243196745,-58.0716788481982));
#62851=CARTESIAN_POINT('Ctrl Pts',(-1.92258988276634,7.67548437677564,-58.0650256891158));
#62852=CARTESIAN_POINT('Ctrl Pts',(-2.45118993896757,7.53168308785487,-58.0420904965337));
#62853=CARTESIAN_POINT('Ctrl Pts',(-2.81772816400553,7.40236422159256,-58.0257073361606));
#62854=CARTESIAN_POINT('Ctrl Pts',(-3.2859207033958,7.19734424288913,-58.0044276092246));
#62855=CARTESIAN_POINT('Ctrl Pts',(-3.39738650033991,7.14540443221087,-57.9993312654881));
#62856=CARTESIAN_POINT('Ctrl Pts',(-3.5211537910845,7.0841813731803,-57.9936385347636));
#62857=CARTESIAN_POINT('Ctrl Pts',(-3.53469107360173,7.077436595536,-57.9930154147489));
#62858=CARTESIAN_POINT('Ctrl Pts',(-3.69864343101218,6.99516170256768,-57.9854629939728));
#62859=CARTESIAN_POINT('Ctrl Pts',(-3.84663221451611,6.91488775044269,-57.9785885333203));
#62860=CARTESIAN_POINT('Ctrl Pts',(-4.03382985354334,6.8054750645888,-57.969803852816));
#62861=CARTESIAN_POINT('Ctrl Pts',(-4.07548433971067,6.78061218290063,-57.967843211347));
#62862=CARTESIAN_POINT('Ctrl Pts',(-4.1418261063328,6.74018167763235,-57.9647103551485));
#62863=CARTESIAN_POINT('Ctrl Pts',(-4.16666038280748,6.72485790218505,-57.9635352862622));
#62864=CARTESIAN_POINT('Ctrl Pts',(-4.21147763075942,6.69686023987177,-57.9614102846109));
#62865=CARTESIAN_POINT('Ctrl Pts',(-4.23148958860743,6.68423344686934,-57.9604598142409));
#62866=CARTESIAN_POINT('Ctrl Pts',(-4.27881058540442,6.65407799697948,-57.9582083290824));
#62867=CARTESIAN_POINT('Ctrl Pts',(-4.30606904589383,6.63647070343678,-57.9569082432509));
#62868=CARTESIAN_POINT('Ctrl Pts',(-4.38712040982637,6.58340688865285,-57.9530325428425));
#62869=CARTESIAN_POINT('Ctrl Pts',(-4.44058948185256,6.54746033798625,-57.9504625587053));
#62870=CARTESIAN_POINT('Ctrl Pts',(-4.77512635201042,6.31657249423832,-57.9342894558847));
#62871=CARTESIAN_POINT('Ctrl Pts',(-5.04375296713457,6.10421888488895,-57.9208321884541));
#62872=CARTESIAN_POINT('Ctrl Pts',(-5.65414098254889,5.55381385463925,-57.8890405546432));
#62873=CARTESIAN_POINT('Ctrl Pts',(-5.98051846906027,5.20072847229302,-57.8711111327854));
#62874=CARTESIAN_POINT('Ctrl Pts',(-6.46536864527627,4.56976086197131,-57.8415804864115));
#62875=CARTESIAN_POINT('Ctrl Pts',(-6.6426616683718,4.3079858564548,-57.8299106187649));
#62876=CARTESIAN_POINT('Ctrl Pts',(-6.80718002875471,4.03066549121774,-57.817629579387));
#62877=CARTESIAN_POINT('Ctrl Pts',(-6.81052823181651,4.02500552164033,-57.8173789561614));
#62878=CARTESIAN_POINT('Ctrl Pts',(-6.8189644323913,4.01070388285557,-57.8167457343179));
#62879=CARTESIAN_POINT('Ctrl Pts',(-6.82404305844904,4.00205670899502,-57.8163629203958));
#62880=CARTESIAN_POINT('Ctrl Pts',(-6.83081036103721,3.99048395835019,-57.8158506319247));
#62881=CARTESIAN_POINT('Ctrl Pts',(-6.8325136322778,3.98756691166661,-57.8157215071982));
#62882=CARTESIAN_POINT('Ctrl Pts',(-6.83815734767537,3.97788717154885,-57.8152930374419));
#62883=CARTESIAN_POINT('Ctrl Pts',(-6.84208961998828,3.97111972784656,-57.8149934945661));
#62884=CARTESIAN_POINT('Ctrl Pts',(-6.85392466982884,3.9506818342451,-57.814088884912));
#62885=CARTESIAN_POINT('Ctrl Pts',(-6.86179655224738,3.93699357481537,-57.8134830495285));
#62886=CARTESIAN_POINT('Ctrl Pts',(-6.93637871859901,3.8064009464151,-57.8077026338968));
#62887=CARTESIAN_POINT('Ctrl Pts',(-7.00013441528284,3.68783865392314,-57.8024516756647));
#62888=CARTESIAN_POINT('Ctrl Pts',(-7.06821835051053,3.55309422442241,-57.7964264298944));
#62889=CARTESIAN_POINT('Ctrl Pts',(-7.07555879149618,3.53845404116284,-57.7957710216537));
#62890=CARTESIAN_POINT('Ctrl Pts',(-7.08657790562254,3.51630551763269,-57.7947782024863));
#62891=CARTESIAN_POINT('Ctrl Pts',(-7.09029024763186,3.50881391776053,-57.7944421671794));
#62892=CARTESIAN_POINT('Ctrl Pts',(-7.0967177650101,3.49579117361541,-57.7938576287531));
#62893=CARTESIAN_POINT('Ctrl Pts',(-7.09943837192253,3.49026270769964,-57.7936093520244));
#62894=CARTESIAN_POINT('Ctrl Pts',(-7.10509185007218,3.47874048026342,-57.7930916296629));
#62895=CARTESIAN_POINT('Ctrl Pts',(-7.10802360112179,3.47274617738132,-57.7928221370639));
#62896=CARTESIAN_POINT('Ctrl Pts',(-7.11492244893895,3.4585953525109,-57.7921855653948));
#62897=CARTESIAN_POINT('Ctrl Pts',(-7.11888310437012,3.4504357133911,-57.7918182106894));
#62898=CARTESIAN_POINT('Ctrl Pts',(-7.13184649088081,3.42361154990645,-57.7906095403176));
#62899=CARTESIAN_POINT('Ctrl Pts',(-7.14078987251964,3.40491855989797,-57.7897656315175));
#62900=CARTESIAN_POINT('Ctrl Pts',(-7.29862595491948,3.07166082403764,-57.7746882666538));
#62901=CARTESIAN_POINT('Ctrl Pts',(-7.42664381947607,2.74770945124755,-57.759363722193));
#62902=CARTESIAN_POINT('Ctrl Pts',(-7.78336729504308,1.63567953015698,-57.7064230228309));
#62903=CARTESIAN_POINT('Ctrl Pts',(-7.91096002178626,0.8205463410372,-57.6677770401829));
#62904=CARTESIAN_POINT('Ctrl Pts',(-7.9109999906061,0.00038552601831901,
-57.6331896426682));
#62905=CARTESIAN_POINT('',(-7.91099999999297,1.05515043374329E-5,-53.643655794299));
#62906=CARTESIAN_POINT('Ctrl Pts',(-7.91099999101477,0.000377046938387499,
-57.633189285093));
#62907=CARTESIAN_POINT('Ctrl Pts',(-7.9110051185265,-0.107205699848678,
-57.6286523644339));
#62908=CARTESIAN_POINT('Ctrl Pts',(-7.90881570339247,-0.21478056331028,
-57.6241782588173));
#62909=CARTESIAN_POINT('Ctrl Pts',(-7.90254087123815,-0.368680460629765,
-57.6178655557648));
#62910=CARTESIAN_POINT('Ctrl Pts',(-7.90024052184193,-0.415062998218047,
-57.615974464361));
#62911=CARTESIAN_POINT('Ctrl Pts',(-7.89680408507951,-0.473879665821541,
-57.613590645267));
#62912=CARTESIAN_POINT('Ctrl Pts',(-7.8960468223857,-0.486334531233799,
-57.61308666367));
#62913=CARTESIAN_POINT('Ctrl Pts',(-7.89470559684908,-0.507564659447974,
-57.6122289656369));
#62914=CARTESIAN_POINT('Ctrl Pts',(-7.89413646358415,-0.516340817067683,
-57.6118748081674));
#62915=CARTESIAN_POINT('Ctrl Pts',(-7.89304804236509,-0.532701982674763,
-57.6112153028712));
#62916=CARTESIAN_POINT('Ctrl Pts',(-7.89253245287299,-0.540287221923677,
-57.6109098452336));
#62917=CARTESIAN_POINT('Ctrl Pts',(-7.89146549924196,-0.555656521133576,
-57.610291522918));
#62918=CARTESIAN_POINT('Ctrl Pts',(-7.89091355051302,-0.563440532766269,
-57.6099786760182));
#62919=CARTESIAN_POINT('Ctrl Pts',(-7.88960282026343,-0.581545733959428,
-57.6092517320608));
#62920=CARTESIAN_POINT('Ctrl Pts',(-7.88883530071511,-0.591866286744273,
-57.6088378959365));
#62921=CARTESIAN_POINT('Ctrl Pts',(-7.88650678653762,-0.622367578713689,
-57.607616448767));
#62922=CARTESIAN_POINT('Ctrl Pts',(-7.88488858514545,-0.642543931884694,
-57.6068105443644));
#62923=CARTESIAN_POINT('Ctrl Pts',(-7.8735285938336,-0.777674638369109,
-57.6014266972127));
#62924=CARTESIAN_POINT('Ctrl Pts',(-7.8613504682385,-0.892412736649149,
-57.5969219556929));
#62925=CARTESIAN_POINT('Ctrl Pts',(-7.84088096810435,-1.0519379081305,-57.5907410310072));
#62926=CARTESIAN_POINT('Ctrl Pts',(-7.83470642121581,-1.09697907336804,
-57.5890050203785));
#62927=CARTESIAN_POINT('Ctrl Pts',(-7.6987165210187,-2.02918677873542,-57.55325203661));
#62928=CARTESIAN_POINT('Ctrl Pts',(-7.41943779744514,-2.88782805293668,
-57.5244540280875));
#62929=CARTESIAN_POINT('Ctrl Pts',(-6.96843914075548,-3.74567221643675,
-57.4893354875045));
#62930=CARTESIAN_POINT('Ctrl Pts',(-6.93373007052172,-3.80953952529224,
-57.4866744632899));
#62931=CARTESIAN_POINT('Ctrl Pts',(-6.81786359509259,-4.0159120376024,-57.4778992763193));
#62932=CARTESIAN_POINT('Ctrl Pts',(-6.73315740171557,-4.15636863900462,
-57.4716485604281));
#62933=CARTESIAN_POINT('Ctrl Pts',(-6.62867604807068,-4.31803053785839,
-57.4640187870748));
#62934=CARTESIAN_POINT('Ctrl Pts',(-6.61307112574171,-4.34189176850066,
-57.4628812498572));
#62935=CARTESIAN_POINT('Ctrl Pts',(-6.59218815915625,-4.3734498226116,-57.4613621799622));
#62936=CARTESIAN_POINT('Ctrl Pts',(-6.587024850867,-4.38122262497346,-57.4609868476811));
#62937=CARTESIAN_POINT('Ctrl Pts',(-6.5785193788084,-4.3939776712509,-57.4603690119709));
#62938=CARTESIAN_POINT('Ctrl Pts',(-6.57518526876945,-4.3989652958256,-57.4601269347862));
#62939=CARTESIAN_POINT('Ctrl Pts',(-6.56871000325737,-4.40862808787751,
-57.4596570141754));
#62940=CARTESIAN_POINT('Ctrl Pts',(-6.56556952118199,-4.41330370430207,
-57.4594292059375));
#62941=CARTESIAN_POINT('Ctrl Pts',(-6.55830187838315,-4.42409899934586,
-57.4589022584821));
#62942=CARTESIAN_POINT('Ctrl Pts',(-6.55417114469429,-4.43021625765049,
-57.4586029352165));
#62943=CARTESIAN_POINT('Ctrl Pts',(-6.54305431014482,-4.44662974765537,
-57.4577978821625));
#62944=CARTESIAN_POINT('Ctrl Pts',(-6.53605248691869,-4.45691526776444,
-57.4572913563012));
#62945=CARTESIAN_POINT('Ctrl Pts',(-6.48602297727284,-4.53003604776227,
-57.4536761143513));
#62946=CARTESIAN_POINT('Ctrl Pts',(-6.44211506546661,-4.59226236580237,
-57.4505242040204));
#62947=CARTESIAN_POINT('Ctrl Pts',(-6.04366486905114,-5.13998426307063,
-57.4221713700948));
#62948=CARTESIAN_POINT('Ctrl Pts',(-5.6357549958174,-5.58422909254062,-57.3950677438011));
#62949=CARTESIAN_POINT('Ctrl Pts',(-4.84391306934859,-6.27056353976016,
-57.3495045593447));
#62950=CARTESIAN_POINT('Ctrl Pts',(-4.48217217610062,-6.53403748987729,
-57.3306474779736));
#62951=CARTESIAN_POINT('Ctrl Pts',(-4.06413967728926,-6.78737487744593,
-57.3108251889001));
#62952=CARTESIAN_POINT('Ctrl Pts',(-4.02800625261219,-6.80888057713724,
-57.3091262498831));
#62953=CARTESIAN_POINT('Ctrl Pts',(-3.97548323797543,-6.8395765188118,-57.3066768613934));
#62954=CARTESIAN_POINT('Ctrl Pts',(-3.95922984789392,-6.84899795205211,
-57.3059216595689));
#62955=CARTESIAN_POINT('Ctrl Pts',(-3.93079907922474,-6.86534309540146,
-57.3046053919431));
#62956=CARTESIAN_POINT('Ctrl Pts',(-3.91863660382568,-6.87229251323125,
-57.3040438110042));
#62957=CARTESIAN_POINT('Ctrl Pts',(-3.89507753793784,-6.88567085941025,
-57.302958889796));
#62958=CARTESIAN_POINT('Ctrl Pts',(-3.88368333184739,-6.89210388704103,
-57.3024354699977));
#62959=CARTESIAN_POINT('Ctrl Pts',(-3.85416114729629,-6.90867528967045,
-57.3010826059953));
#62960=CARTESIAN_POINT('Ctrl Pts',(-3.83600908108455,-6.91877060913069,
-57.3002539980776));
#62961=CARTESIAN_POINT('Ctrl Pts',(-3.7988915083269,-6.93922266885189,-57.2985660615507));
#62962=CARTESIAN_POINT('Ctrl Pts',(-3.7799228919311,-6.9495734311769,-57.2977068442333));
#62963=CARTESIAN_POINT('Ctrl Pts',(-3.63391565816748,-7.02847177748308,
-57.2911186819552));
#62964=CARTESIAN_POINT('Ctrl Pts',(-3.50506274915314,-7.09360945638501,
-57.2854534601743));
#62965=CARTESIAN_POINT('Ctrl Pts',(-2.70529488909303,-7.47079245640969,
-57.2511407294273));
#62966=CARTESIAN_POINT('Ctrl Pts',(-1.9951579041801,-7.69094742817544,-57.2246725819699));
#62967=CARTESIAN_POINT('Ctrl Pts',(-1.06022670992192,-7.84237150886734,
-57.1893599941162));
#62968=CARTESIAN_POINT('Ctrl Pts',(-0.854430566780976,-7.86745285493904,
-57.1815296474756));
#62969=CARTESIAN_POINT('Ctrl Pts',(-0.555640021265778,-7.89200567687153,
-57.169859152757));
#62970=CARTESIAN_POINT('Ctrl Pts',(-0.463261210358789,-7.89796668205734,
-57.1662091802437));
#62971=CARTESIAN_POINT('Ctrl Pts',(-0.355894420758969,-7.903004673239,-57.1619016951472));
#62972=CARTESIAN_POINT('Ctrl Pts',(-0.340985666546359,-7.90366196616611,
-57.1613021037016));
#62973=CARTESIAN_POINT('Ctrl Pts',(-0.318291381785576,-7.90459817367684,
-57.1603870787388));
#62974=CARTESIAN_POINT('Ctrl Pts',(-0.31050710601753,-7.90490778109251,
-57.160072804393));
#62975=CARTESIAN_POINT('Ctrl Pts',(-0.296387815559982,-7.90544846600326,
-57.1595019973823));
#62976=CARTESIAN_POINT('Ctrl Pts',(-0.290052950382796,-7.90568342849107,
-57.159245614056));
#62977=CARTESIAN_POINT('Ctrl Pts',(-0.276441700923589,-7.90617189264842,
-57.1586941287821));
#62978=CARTESIAN_POINT('Ctrl Pts',(-0.269165239214332,-7.90642296387229,
-57.1583989325512));
#62979=CARTESIAN_POINT('Ctrl Pts',(-0.24964252644527,-7.90706960487489,
-57.1576058921898));
#62980=CARTESIAN_POINT('Ctrl Pts',(-0.237395715992339,-7.90744676865447,
-57.1571073218363));
#62981=CARTESIAN_POINT('Ctrl Pts',(-0.18179934548302,-7.90902969004254,
-57.1548388873426));
#62982=CARTESIAN_POINT('Ctrl Pts',(-0.138441766483694,-7.90990742104768,
-57.1530557623367));
#62983=CARTESIAN_POINT('Ctrl Pts',(0.626113125322077,-7.91909702702051,
-57.1213375345691));
#62984=CARTESIAN_POINT('Ctrl Pts',(1.34500692906579,-7.82910258346065,-57.0869272436465));
#62985=CARTESIAN_POINT('Ctrl Pts',(2.38437934778349,-7.55145601499462,-57.0381478117924));
#62986=CARTESIAN_POINT('Ctrl Pts',(2.72056703746041,-7.43695546067846,-57.0224810060503));
#62987=CARTESIAN_POINT('Ctrl Pts',(3.13298828165304,-7.26476396960482,-57.0036693857707));
#62988=CARTESIAN_POINT('Ctrl Pts',(3.21739169817972,-7.2277799175295,-56.999840236044));
#62989=CARTESIAN_POINT('Ctrl Pts',(3.33368829595093,-7.17437988593016,-56.994593241278));
#62990=CARTESIAN_POINT('Ctrl Pts',(3.3661432041858,-7.15920975922467,-56.993132133364));
#62991=CARTESIAN_POINT('Ctrl Pts',(3.4145312035279,-7.13619037364201,-56.9909583948226));
#62992=CARTESIAN_POINT('Ctrl Pts',(3.43054250214233,-7.12850717438436,-56.9902398871585));
#62993=CARTESIAN_POINT('Ctrl Pts',(3.45618227578814,-7.11609725338303,-56.9890905208007));
#62994=CARTESIAN_POINT('Ctrl Pts',(3.46582719975796,-7.11140477442471,-56.9886584409365));
#62995=CARTESIAN_POINT('Ctrl Pts',(3.4842097161493,-7.1024149741573,-56.9878354538307));
#62996=CARTESIAN_POINT('Ctrl Pts',(3.49294897160148,-7.09812111012051,-56.9874444236528));
#62997=CARTESIAN_POINT('Ctrl Pts',(3.50833917597229,-7.09052412528659,-56.9867561996525));
#62998=CARTESIAN_POINT('Ctrl Pts',(3.51499343397836,-7.08722775875119,-56.986458763546));
#62999=CARTESIAN_POINT('Ctrl Pts',(3.52803679441936,-7.08074348922605,-56.9858759987093));
#63000=CARTESIAN_POINT('Ctrl Pts',(3.53442624006699,-7.07755629697504,-56.9855906448145));
#63001=CARTESIAN_POINT('Ctrl Pts',(3.54967514299524,-7.06992401851332,-56.9849099112374));
#63002=CARTESIAN_POINT('Ctrl Pts',(3.55853058918476,-7.06547091814642,-56.9845148214944));
#63003=CARTESIAN_POINT('Ctrl Pts',(3.59020534688004,-7.04946811340048,-56.9831024537603));
#63004=CARTESIAN_POINT('Ctrl Pts',(3.61297710533012,-7.03782434898807,-56.9820885873691));
#63005=CARTESIAN_POINT('Ctrl Pts',(3.94273274650287,-6.8671898485744,-56.9674282094977));
#63006=CARTESIAN_POINT('Ctrl Pts',(4.23904225013443,-6.6883474456591,-56.954548142343));
#63007=CARTESIAN_POINT('Ctrl Pts',(4.80753832998855,-6.29221747680268,-56.9298604559548));
#63008=CARTESIAN_POINT('Ctrl Pts',(5.07898731727145,-6.07522230664863,-56.9180826586979));
#63009=CARTESIAN_POINT('Ctrl Pts',(5.35684074036114,-5.82142839882124,-56.9054139467907));
#63010=CARTESIAN_POINT('Ctrl Pts',(5.37826234937195,-5.80164333814783,-56.9044328531998));
#63011=CARTESIAN_POINT('Ctrl Pts',(5.4716561918071,-5.71442271826948,-56.9001343579225));
#63012=CARTESIAN_POINT('Ctrl Pts',(5.54247296549684,-5.64576317597658,-56.8968196518867));
#63013=CARTESIAN_POINT('Ctrl Pts',(5.66468067362727,-5.52276228092883,-56.8909701314387));
#63014=CARTESIAN_POINT('Ctrl Pts',(5.71661935587087,-5.4689828465595,-56.8884409583832));
#63015=CARTESIAN_POINT('Ctrl Pts',(5.85656531244334,-5.31990496306322,-56.8814846766845));
#63016=CARTESIAN_POINT('Ctrl Pts',(5.94300217255408,-5.22316667573517,-56.8770301713073));
#63017=CARTESIAN_POINT('Ctrl Pts',(6.23354336144865,-4.88144569109814,-56.8613419624065));
#63018=CARTESIAN_POINT('Ctrl Pts',(6.42517482006858,-4.62630140289441,-56.8497118356704));
#63019=CARTESIAN_POINT('Ctrl Pts',(6.60791425739633,-4.34966129566134,-56.8364408334894));
#63020=CARTESIAN_POINT('Ctrl Pts',(6.61493002516844,-4.33898432567641,-56.8359276529697));
#63021=CARTESIAN_POINT('Ctrl Pts',(6.62497859401741,-4.32361086169865,-56.8351872593192));
#63022=CARTESIAN_POINT('Ctrl Pts',(6.62803236015783,-4.3189280252128,-56.8349615348053));
#63023=CARTESIAN_POINT('Ctrl Pts',(6.63332253121521,-4.31079692040851,-56.8345692470497));
#63024=CARTESIAN_POINT('Ctrl Pts',(6.63556122114052,-4.3073501334928,-56.8344028473825));
#63025=CARTESIAN_POINT('Ctrl Pts',(6.63985916050586,-4.30072153169045,-56.834082628925));
#63026=CARTESIAN_POINT('Ctrl Pts',(6.64191881198113,-4.29753997764384,-56.8339288391609));
#63027=CARTESIAN_POINT('Ctrl Pts',(6.64677762827943,-4.29002270320983,-56.8335652463695));
#63028=CARTESIAN_POINT('Ctrl Pts',(6.64957482247711,-4.28568574601521,-56.8333553020261));
#63029=CARTESIAN_POINT('Ctrl Pts',(6.65794561255129,-4.2726791884625,-56.8327251571326));
#63030=CARTESIAN_POINT('Ctrl Pts',(6.6635064936162,-4.26400145810449,-56.8323040447077));
#63031=CARTESIAN_POINT('Ctrl Pts',(6.71662708099417,-4.18074932619382,-56.8282575888176));
#63032=CARTESIAN_POINT('Ctrl Pts',(6.7629482041704,-4.10539580112422,-56.8245459425109));
#63033=CARTESIAN_POINT('Ctrl Pts',(6.84894424862533,-3.96009442192178,-56.8173231129596));
#63034=CARTESIAN_POINT('Ctrl Pts',(6.88883580524605,-3.89028606386178,-56.8138247903952));
#63035=CARTESIAN_POINT('Ctrl Pts',(7.29229268290991,-3.15858577901082,-56.7769725311015));
#63036=CARTESIAN_POINT('Ctrl Pts',(7.56038534060125,-2.44846857765005,-56.7401392692563));
#63037=CARTESIAN_POINT('Ctrl Pts',(7.80042314666375,-1.36491530495265,-56.6905957112567));
#63038=CARTESIAN_POINT('Ctrl Pts',(7.85375165175807,-1.01401483210752,-56.6754255962818));
#63039=CARTESIAN_POINT('Ctrl Pts',(7.88548171605885,-0.635407321156414,
-56.6600425611962));
#63040=CARTESIAN_POINT('Ctrl Pts',(7.88747846062381,-0.610121224054738,
-56.6590196934819));
#63041=CARTESIAN_POINT('Ctrl Pts',(7.89012290573929,-0.574447417004055,
-56.6575829280983));
#63042=CARTESIAN_POINT('Ctrl Pts',(7.89087176130505,-0.564067505147878,
-56.6571656283729));
#63043=CARTESIAN_POINT('Ctrl Pts',(7.89210918600974,-0.546430687739474,
-56.6564578529139));
#63044=CARTESIAN_POINT('Ctrl Pts',(7.89260823240736,-0.539174545513565,
-56.6561670251689));
#63045=CARTESIAN_POINT('Ctrl Pts',(7.89359031385127,-0.524601493718695,
-56.6555836649419));
#63046=CARTESIAN_POINT('Ctrl Pts',(7.8940731839628,-0.517284580069527,-56.6552911382767));
#63047=CARTESIAN_POINT('Ctrl Pts',(7.89521799866798,-0.499562271846002,
-56.6545835010817));
#63048=CARTESIAN_POINT('Ctrl Pts',(7.89586954788158,-0.489156206056432,
-56.6541687400881));
#63049=CARTESIAN_POINT('Ctrl Pts',(7.89801118497569,-0.453831968181256,
-56.6527633120335));
#63050=CARTESIAN_POINT('Ctrl Pts',(7.89940391076771,-0.428907919491899,
-56.6517759133521));
#63051=CARTESIAN_POINT('Ctrl Pts',(7.91930405803316,-0.0397163090076934,
-56.6364227282477));
#63052=CARTESIAN_POINT('Ctrl Pts',(7.91271751605975,0.325410780283869,-56.6229414459906));
#63053=CARTESIAN_POINT('Ctrl Pts',(7.85146309809681,1.02624491709948,-56.5980335107253));
#63054=CARTESIAN_POINT('Ctrl Pts',(7.80032930329605,1.36144088503841,-56.5865491425165));
#63055=CARTESIAN_POINT('Ctrl Pts',(7.69618567560514,1.83700340995465,-56.5699926984763));
#63056=CARTESIAN_POINT('Ctrl Pts',(7.66044716840923,1.98075840516805,-56.5649492416154));
#63057=CARTESIAN_POINT('Ctrl Pts',(7.60708458895948,2.17226983230576,-56.5580904832827));
#63058=CARTESIAN_POINT('Ctrl Pts',(7.59300496777793,2.22098349031854,-56.5563334928583));
#63059=CARTESIAN_POINT('Ctrl Pts',(7.56179233023832,2.32520803729195,-56.5525417239012));
#63060=CARTESIAN_POINT('Ctrl Pts',(7.54451425593942,2.38067221164975,-56.5505038807333));
#63061=CARTESIAN_POINT('Ctrl Pts',(7.50500781911477,2.50274014158415,-56.5459649438605));
#63062=CARTESIAN_POINT('Ctrl Pts',(7.48250056748997,2.5692480515603,-56.5434561195527));
#63063=CARTESIAN_POINT('Ctrl Pts',(7.39331424795949,2.82167233063979,-56.5337667190644));
#63064=CARTESIAN_POINT('Ctrl Pts',(7.32057019925716,3.00535724369664,-56.5263675322659));
#63065=CARTESIAN_POINT('Ctrl Pts',(7.22960523936015,3.21209192340681,-56.5174247353167));
#63066=CARTESIAN_POINT('Ctrl Pts',(7.21803562468271,3.23800681462385,-56.5162924232389));
#63067=CARTESIAN_POINT('Ctrl Pts',(7.20314389236692,3.27088651415949,-56.514840675133));
#63068=CARTESIAN_POINT('Ctrl Pts',(7.19995059173247,3.27790969955461,-56.5145296989864));
#63069=CARTESIAN_POINT('Ctrl Pts',(7.19479183269735,3.28921170732236,-56.5140278597299));
#63070=CARTESIAN_POINT('Ctrl Pts',(7.19283281192515,3.29349348123548,-56.513837412748));
#63071=CARTESIAN_POINT('Ctrl Pts',(7.18909710861266,3.30163926711951,-56.5134744853762));
#63072=CARTESIAN_POINT('Ctrl Pts',(7.18732112983918,3.30550360212758,-56.5133020501257));
#63073=CARTESIAN_POINT('Ctrl Pts',(7.18326960438862,3.31430057474595,-56.5129089121036));
#63074=CARTESIAN_POINT('Ctrl Pts',(7.18099209357794,3.31923229991244,-56.5126880843669));
#63075=CARTESIAN_POINT('Ctrl Pts',(7.17405082234038,3.33422235602046,-56.5120155810414));
#63076=CARTESIAN_POINT('Ctrl Pts',(7.16937101244632,3.34427319524262,-56.5115628939466));
#63077=CARTESIAN_POINT('Ctrl Pts',(7.13615175745839,3.41522808951705,-56.5083547350272));
#63078=CARTESIAN_POINT('Ctrl Pts',(7.10685850729854,3.4757742252649,-56.505552719706));
#63079=CARTESIAN_POINT('Ctrl Pts',(7.03544522710466,3.61870019447284,-56.4987970935544));
#63080=CARTESIAN_POINT('Ctrl Pts',(6.9926454563373,3.70072817718354,-56.4948067819572));
#63081=CARTESIAN_POINT('Ctrl Pts',(6.5567874690899,4.50150463892688,-56.4548638828426));
#63082=CARTESIAN_POINT('Ctrl Pts',(6.05577003958546,5.15586211913936,-56.4148574635399));
#63083=CARTESIAN_POINT('Ctrl Pts',(5.20512774356921,5.96806930877752,-56.3625204805348));
#63084=CARTESIAN_POINT('Ctrl Pts',(4.9307030587227,6.19672632500656,-56.3472819637384));
#63085=CARTESIAN_POINT('Ctrl Pts',(4.62149012044424,6.42077690857281,-56.331790401979));
#63086=CARTESIAN_POINT('Ctrl Pts',(4.60115931459744,6.43536168522438,-56.3307790203603));
#63087=CARTESIAN_POINT('Ctrl Pts',(4.57188407152779,6.45615330858379,-56.3293328946496));
#63088=CARTESIAN_POINT('Ctrl Pts',(4.56299558458341,6.46243845647448,-56.328895166889));
#63089=CARTESIAN_POINT('Ctrl Pts',(4.54756781872209,6.47329990326894,-56.3281377157034));
#63090=CARTESIAN_POINT('Ctrl Pts',(4.54103454635026,6.47788468196677,-56.3278176706827));
#63091=CARTESIAN_POINT('Ctrl Pts',(4.52847384345462,6.48667092050229,-56.3272037311762));
#63092=CARTESIAN_POINT('Ctrl Pts',(4.52244747898099,6.49087388430473,-56.3269097799735));
#63093=CARTESIAN_POINT('Ctrl Pts',(4.50825990519403,6.50073936535008,-56.3262191609981));
#63094=CARTESIAN_POINT('Ctrl Pts',(4.50009385970311,6.50639492528747,-56.3258227556818));
#63095=CARTESIAN_POINT('Ctrl Pts',(4.47193977447099,6.52581524730864,-56.3244598342721));
#63096=CARTESIAN_POINT('Ctrl Pts',(4.45189896872856,6.53950346539863,-56.3234961918986));
#63097=CARTESIAN_POINT('Ctrl Pts',(4.22529034305106,6.69275660719473,-56.3126724593198));
#63098=CARTESIAN_POINT('Ctrl Pts',(4.01229163140428,6.8225799858531,-56.3031817128721));
#63099=CARTESIAN_POINT('Ctrl Pts',(3.2785275325376,7.2235428165947,-56.2723276062744));
#63100=CARTESIAN_POINT('Ctrl Pts',(2.73385687563266,7.44676709726335,-56.2525093989169));
#63101=CARTESIAN_POINT('Ctrl Pts',(1.97458675983539,7.66328985610069,-56.2248462048486));
#63102=CARTESIAN_POINT('Ctrl Pts',(1.77760884480998,7.7113621407906,-56.217650084488));
#63103=CARTESIAN_POINT('Ctrl Pts',(1.50081568757249,7.76774363707935,-56.2072838855619));
#63104=CARTESIAN_POINT('Ctrl Pts',(1.42238700787742,7.78248698319818,-56.2043184519667));
#63105=CARTESIAN_POINT('Ctrl Pts',(1.21810433766294,7.81769779065375,-56.196494326728));
#63106=CARTESIAN_POINT('Ctrl Pts',(1.09196857937718,7.83631153413647,-56.1915551115205));
#63107=CARTESIAN_POINT('Ctrl Pts',(0.936864840197922,7.85538247680505,-56.185348728966));
#63108=CARTESIAN_POINT('Ctrl Pts',(0.90827608838852,7.85873934591705,-56.1841996811346));
#63109=CARTESIAN_POINT('Ctrl Pts',(0.868683368133643,7.86316936231992,-56.1826018014735));
#63110=CARTESIAN_POINT('Ctrl Pts',(0.857694321414441,7.86437560548892,-56.1821576079923));
#63111=CARTESIAN_POINT('Ctrl Pts',(0.839123165517238,7.86637473235932,-56.1814057870647));
#63112=CARTESIAN_POINT('Ctrl Pts',(0.831542355979256,7.86717969964912,-56.181098568313));
#63113=CARTESIAN_POINT('Ctrl Pts',(0.816524872956141,7.86875238048455,-56.1804893449923));
#63114=CARTESIAN_POINT('Ctrl Pts',(0.809088250119467,7.86952051249878,-56.1801873545846));
#63115=CARTESIAN_POINT('Ctrl Pts',(0.792671221820548,7.87119271770173,-56.179520024034));
#63116=CARTESIAN_POINT('Ctrl Pts',(0.783690341102463,7.8720919655227,-56.179154528005));
#63117=CARTESIAN_POINT('Ctrl Pts',(0.752205463862471,7.87519010599056,-56.1778716949695));
#63118=CARTESIAN_POINT('Ctrl Pts',(0.729693694627155,7.87730787557035,-56.1769518006395));
#63119=CARTESIAN_POINT('Ctrl Pts',(0.425234455430575,7.90463322720225,-56.1644768483184));
#63120=CARTESIAN_POINT('Ctrl Pts',(0.142149800189738,7.91478569305607,-56.1524939345744));
#63121=CARTESIAN_POINT('Ctrl Pts',(-0.805552406661437,7.89790900730645,
-56.1119425953446));
#63122=CARTESIAN_POINT('Ctrl Pts',(-1.46616141161784,7.80232894986433,-56.0832399781104));
#63123=CARTESIAN_POINT('Ctrl Pts',(-2.52509117634157,7.50972519142205,-56.0374179087135));
#63124=CARTESIAN_POINT('Ctrl Pts',(-2.93297883909377,7.36000750917241,-56.0195951352827));
#63125=CARTESIAN_POINT('Ctrl Pts',(-3.37482375808801,7.15523014124652,-55.9998551342719));
#63126=CARTESIAN_POINT('Ctrl Pts',(-3.4228865459982,7.1323629683599,-55.9977030306103));
#63127=CARTESIAN_POINT('Ctrl Pts',(-3.49491425616442,7.0971980752756,-55.9944704460744));
#63128=CARTESIAN_POINT('Ctrl Pts',(-3.51905297469963,7.08526021718412,-55.9933858396881));
#63129=CARTESIAN_POINT('Ctrl Pts',(-3.56249510414999,7.06349904247396,-55.9914315588432));
#63130=CARTESIAN_POINT('Ctrl Pts',(-3.58182000477595,7.05371927048796,-55.9905613745348));
#63131=CARTESIAN_POINT('Ctrl Pts',(-3.62310889075006,7.03261073208286,-55.9887003417512));
#63132=CARTESIAN_POINT('Ctrl Pts',(-3.64506045766456,7.02125814994953,-55.9877097947332));
#63133=CARTESIAN_POINT('Ctrl Pts',(-3.70374260459236,6.99056042531679,-55.9850587419356));
#63134=CARTESIAN_POINT('Ctrl Pts',(-3.74037478836277,6.97102867643353,-55.9834005936722));
#63135=CARTESIAN_POINT('Ctrl Pts',(-3.91354769005435,6.87693737207559,-55.9755457166084));
#63136=CARTESIAN_POINT('Ctrl Pts',(-4.04802464174732,6.79864845775353,-55.9693985470876));
#63137=CARTESIAN_POINT('Ctrl Pts',(-4.60927648801326,6.44934265914479,-55.9434725910887));
#63138=CARTESIAN_POINT('Ctrl Pts',(-5.01185322770294,6.14172432425867,-55.9242689433172));
#63139=CARTESIAN_POINT('Ctrl Pts',(-5.50689407882182,5.68215893836712,-55.8981743734901));
#63140=CARTESIAN_POINT('Ctrl Pts',(-5.6277040006146,5.56253165607085,-55.8915697760371));
#63141=CARTESIAN_POINT('Ctrl Pts',(-5.80217058828601,5.37826715126918,-55.88156464109));
#63142=CARTESIAN_POINT('Ctrl Pts',(-5.85880565161739,5.31651549999864,-55.8782380314659));
#63143=CARTESIAN_POINT('Ctrl Pts',(-5.92742763606071,5.23926565129193,-55.8740973684555));
#63144=CARTESIAN_POINT('Ctrl Pts',(-5.9403525706433,5.22460661469507,-55.8733125167763));
#63145=CARTESIAN_POINT('Ctrl Pts',(-5.96112482600534,5.20087067428051,-55.872043027975));
#63146=CARTESIAN_POINT('Ctrl Pts',(-5.96900597782746,5.19182362925176,-55.871559480729));
#63147=CARTESIAN_POINT('Ctrl Pts',(-5.9841083484137,5.17440725741117,-55.8706292606443));
#63148=CARTESIAN_POINT('Ctrl Pts',(-5.99133267064603,5.16604065216632,-55.8701826819754));
#63149=CARTESIAN_POINT('Ctrl Pts',(-6.00780430702971,5.14688355761278,-55.8691608313342));
#63150=CARTESIAN_POINT('Ctrl Pts',(-6.01704012174154,5.13608324685826,-55.8685852306889));
#63151=CARTESIAN_POINT('Ctrl Pts',(-6.04143956876111,5.10739452820873,-55.8670576484932));
#63152=CARTESIAN_POINT('Ctrl Pts',(-6.05655281452251,5.08946352051693,-55.8661042927006));
#63153=CARTESIAN_POINT('Ctrl Pts',(-6.16290819730177,4.96213428201292,-55.8593452467601));
#63154=CARTESIAN_POINT('Ctrl Pts',(-6.25125914364643,4.85035791077833,-55.8534682487453));
#63155=CARTESIAN_POINT('Ctrl Pts',(-6.4782697424781,4.54664516700848,-55.8377106137285));
#63156=CARTESIAN_POINT('Ctrl Pts',(-6.61141355276991,4.35076661848367,-55.8277645734934));
#63157=CARTESIAN_POINT('Ctrl Pts',(-6.94189623509074,3.81428204311281,-55.8012958665957));
#63158=CARTESIAN_POINT('Ctrl Pts',(-7.1229553825257,3.46441789577465,-55.7848325679527));
#63159=CARTESIAN_POINT('Ctrl Pts',(-7.31693430575079,3.00942491103916,-55.7645080043756));
#63160=CARTESIAN_POINT('Ctrl Pts',(-7.3548393813469,2.91556237010038,-55.7603686120139));
#63161=CARTESIAN_POINT('Ctrl Pts',(-7.4181337538715,2.74973292056485,-55.7531447938877));
#63162=CARTESIAN_POINT('Ctrl Pts',(-7.44430232529682,2.6780781459825,-55.7500520799141));
#63163=CARTESIAN_POINT('Ctrl Pts',(-7.48087684049921,2.57324891858899,-55.7455669322779));
#63164=CARTESIAN_POINT('Ctrl Pts',(-7.49210676994035,2.54036699329138,-55.7441656539896));
#63165=CARTESIAN_POINT('Ctrl Pts',(-7.5114890668149,2.48236787288347,-55.7417035004907));
#63166=CARTESIAN_POINT('Ctrl Pts',(-7.51973297341991,2.45728188681206,-55.7406416730075));
#63167=CARTESIAN_POINT('Ctrl Pts',(-7.53558576116841,2.40821534948107,-55.7385707138626));
#63168=CARTESIAN_POINT('Ctrl Pts',(-7.54320615177066,2.38423884919182,-55.7375614745711));
#63169=CARTESIAN_POINT('Ctrl Pts',(-7.5635162237632,2.31926393497324,-55.7348336912542));
#63170=CARTESIAN_POINT('Ctrl Pts',(-7.5759868893089,2.27819787168256,-55.7331173816548));
#63171=CARTESIAN_POINT('Ctrl Pts',(-7.62387371744798,2.11576340791,-55.7263573899878));
#63172=CARTESIAN_POINT('Ctrl Pts',(-7.65671267005228,1.9936541386152,-55.721338967626));
#63173=CARTESIAN_POINT('Ctrl Pts',(-7.68845622645815,1.86322911090229,-55.7160318767724));
#63174=CARTESIAN_POINT('Ctrl Pts',(-7.69028996399285,1.85564601569213,-55.7157235032714));
#63175=CARTESIAN_POINT('Ctrl Pts',(-7.83752454740121,1.2428169714209,-55.6908171746891));
#63176=CARTESIAN_POINT('Ctrl Pts',(-7.91100180423729,0.622499836634585,
-55.666937553817));
#63177=CARTESIAN_POINT('Ctrl Pts',(-7.91099845657851,-0.532535813923126,
-55.6238481307725));
#63178=CARTESIAN_POINT('Ctrl Pts',(-7.85723020891476,-1.0636513855998,-55.6045015296109));
#63179=CARTESIAN_POINT('Ctrl Pts',(-7.74990284520874,-1.58837550848826,
-55.5836168389627));
#63180=CARTESIAN_POINT('Ctrl Pts',(-7.74927157453051,-1.59145245932399,
-55.583494305611));
#63181=CARTESIAN_POINT('Ctrl Pts',(-7.74423889981475,-1.61590881988658,
-55.5825198447304));
#63182=CARTESIAN_POINT('Ctrl Pts',(-7.73975088130106,-1.63727020923664,
-55.5816654479737));
#63183=CARTESIAN_POINT('Ctrl Pts',(-7.72278761683751,-1.71638079086475,
-55.5784884040048));
#63184=CARTESIAN_POINT('Ctrl Pts',(-7.70975412148755,-1.77400754719334,
-55.5761487545977));
#63185=CARTESIAN_POINT('Ctrl Pts',(-7.69311887990501,-1.84391054982302,
-55.573274621882));
#63186=CARTESIAN_POINT('Ctrl Pts',(-7.69013109713555,-1.85633184605752,
-55.5727625167274));
#63187=CARTESIAN_POINT('Ctrl Pts',(-7.68516576318915,-1.87675681998095,
-55.5719180743792));
#63188=CARTESIAN_POINT('Ctrl Pts',(-7.68320575973477,-1.88476476568983,
-55.5715863988233));
#63189=CARTESIAN_POINT('Ctrl Pts',(-7.67965620408566,-1.89916956417051,
-55.5709886785668));
#63190=CARTESIAN_POINT('Ctrl Pts',(-7.67807116664546,-1.90556752859101,
-55.570722807939));
#63191=CARTESIAN_POINT('Ctrl Pts',(-7.67467881183064,-1.91918773508362,
-55.5701559694763));
#63192=CARTESIAN_POINT('Ctrl Pts',(-7.67286929246645,-1.9264094184512,-55.5698549155698));
#63193=CARTESIAN_POINT('Ctrl Pts',(-7.66798139670256,-1.94580057366551,
-55.5690451643568));
#63194=CARTESIAN_POINT('Ctrl Pts',(-7.66488425276642,-1.9579652606602,-55.5685357180314));
#63195=CARTESIAN_POINT('Ctrl Pts',(-7.64982344735919,-2.01653636490782,
-55.5660755527685));
#63196=CARTESIAN_POINT('Ctrl Pts',(-7.6374673909556,-2.06284012801415,-55.5641086825192));
#63197=CARTESIAN_POINT('Ctrl Pts',(-7.603799098474,-2.18455987054575,-55.5588740026004));
#63198=CARTESIAN_POINT('Ctrl Pts',(-7.58178686316967,-2.25977193784916,
-55.5555716405067));
#63199=CARTESIAN_POINT('Ctrl Pts',(-7.52667515768994,-2.43820220542041,
-55.547588302883));
#63200=CARTESIAN_POINT('Ctrl Pts',(-7.49256449695593,-2.54109124659927,
-55.5428659183496));
#63201=CARTESIAN_POINT('Ctrl Pts',(-7.38780807938719,-2.83659965150273,
-55.5290125342096));
#63202=CARTESIAN_POINT('Ctrl Pts',(-7.31177130844375,-3.02720999963955,
-55.5197159469372));
#63203=CARTESIAN_POINT('Ctrl Pts',(-6.97343703411647,-3.78798538396104,
-55.4816120433421));
#63204=CARTESIAN_POINT('Ctrl Pts',(-6.65111500182147,-4.32902682033968,
-55.452365440589));
#63205=CARTESIAN_POINT('Ctrl Pts',(-6.11280593547542,-5.02816363891197,
-55.4141211414029));
#63206=CARTESIAN_POINT('Ctrl Pts',(-5.94771284151276,-5.22240873526371,
-55.4034081083382));
#63207=CARTESIAN_POINT('Ctrl Pts',(-5.75635002591773,-5.42669202613192,
-55.3920414765225));
#63208=CARTESIAN_POINT('Ctrl Pts',(-5.73909005137082,-5.44494236554374,
-55.3910250113978));
#63209=CARTESIAN_POINT('Ctrl Pts',(-5.71462805941281,-5.47056243033573,
-55.3895966239102));
#63210=CARTESIAN_POINT('Ctrl Pts',(-5.70749820542755,-5.47800067521219,
-55.3891817466346));
#63211=CARTESIAN_POINT('Ctrl Pts',(-5.69506360702925,-5.49092248358392,
-55.3884607057034));
#63212=CARTESIAN_POINT('Ctrl Pts',(-5.68976543106216,-5.49641233430998,
-55.3881542721157));
#63213=CARTESIAN_POINT('Ctrl Pts',(-5.67868946254114,-5.5078558274845,-55.3875153086717));
#63214=CARTESIAN_POINT('Ctrl Pts',(-5.67291022777081,-5.51380806489604,
-55.3871828390426));
#63215=CARTESIAN_POINT('Ctrl Pts',(-5.65921619352339,-5.52786771264241,
-55.3863972355055));
#63216=CARTESIAN_POINT('Ctrl Pts',(-5.65129330984199,-5.53596724168018,
-55.3859444378222));
#63217=CARTESIAN_POINT('Ctrl Pts',(-5.62505673278056,-5.56267376012855,
-55.3844506707206));
#63218=CARTESIAN_POINT('Ctrl Pts',(-5.60666824705465,-5.58120719844518,
-55.3834128217441));
#63219=CARTESIAN_POINT('Ctrl Pts',(-5.31472250470243,-5.87255539814665,
-55.3670771640219));
#63220=CARTESIAN_POINT('Ctrl Pts',(-5.0216222160986,-6.1250740224363,-55.3526667189258));
#63221=CARTESIAN_POINT('Ctrl Pts',(-4.49814111733228,-6.51314057549209,
-55.3293109718319));
#63222=CARTESIAN_POINT('Ctrl Pts',(-4.27725093900374,-6.66028553317942,
-55.3200747146529));
#63223=CARTESIAN_POINT('Ctrl Pts',(-3.82922638058848,-6.92723778879926,
-55.3020266643066));
#63224=CARTESIAN_POINT('Ctrl Pts',(-3.60282775155223,-7.04763984001828,
-55.2932204435217));
#63225=CARTESIAN_POINT('Ctrl Pts',(-3.02509029888152,-7.31976361230073,
-55.2707988941708));
#63226=CARTESIAN_POINT('Ctrl Pts',(-2.66785583847887,-7.45738689122056,
-55.2569781168214));
#63227=CARTESIAN_POINT('Ctrl Pts',(-2.2795820804605,-7.57548549945729,-55.2408490092121));
#63228=CARTESIAN_POINT('Ctrl Pts',(-2.25703293581027,-7.5822343225758,-55.2399085715611));
#63229=CARTESIAN_POINT('Ctrl Pts',(-2.22586865214535,-7.59141026722428,
-55.2386040125424));
#63230=CARTESIAN_POINT('Ctrl Pts',(-2.21727884871055,-7.59392359772011,
-55.2382439332683));
#63231=CARTESIAN_POINT('Ctrl Pts',(-2.20357551004866,-7.59790788858827,
-55.2376687151734));
#63232=CARTESIAN_POINT('Ctrl Pts',(-2.19846470673627,-7.5993882809737,-55.2374540081885));
#63233=CARTESIAN_POINT('Ctrl Pts',(-2.18850769401081,-7.60226153845866,
-55.2370353776009));
#63234=CARTESIAN_POINT('Ctrl Pts',(-2.18366163803773,-7.60365492879917,
-55.2368314778365));
#63235=CARTESIAN_POINT('Ctrl Pts',(-2.17204936964131,-7.60698179673731,
-55.2363425255854));
#63236=CARTESIAN_POINT('Ctrl Pts',(-2.16528190982576,-7.60891087939554,
-55.2360572776687));
#63237=CARTESIAN_POINT('Ctrl Pts',(-2.14492160107624,-7.61468527763998,
-55.235198227941));
#63238=CARTESIAN_POINT('Ctrl Pts',(-2.13132106284457,-7.61850320441981,
-55.2346232313804));
#63239=CARTESIAN_POINT('Ctrl Pts',(-2.00895972791461,-7.65249903204976,
-55.2294401519018));
#63240=CARTESIAN_POINT('Ctrl Pts',(-1.89957795843188,-7.68038167387948,
-55.2247364600537));
#63241=CARTESIAN_POINT('Ctrl Pts',(-1.6009105569652,-7.74974494082192,-55.2117685234611));
#63242=CARTESIAN_POINT('Ctrl Pts',(-1.41063882166443,-7.78662667780105,
-55.2033741580621));
#63243=CARTESIAN_POINT('Ctrl Pts',(-0.762131857371492,-7.88778048372765,
-55.1746688886916));
#63244=CARTESIAN_POINT('Ctrl Pts',(-0.2996540427684,-7.91884865599477,-55.1541084505469));
#63245=CARTESIAN_POINT('Ctrl Pts',(0.520687287788129,-7.90195422711492,
-55.1188307209384));
#63246=CARTESIAN_POINT('Ctrl Pts',(0.877588525604872,-7.87031519222064,
-55.1038662783691));
#63247=CARTESIAN_POINT('Ctrl Pts',(1.26992637823986,-7.80850495511669,-55.0877714276107));
#63248=CARTESIAN_POINT('Ctrl Pts',(1.30866590547101,-7.80210588377465,-55.0861857423325));
#63249=CARTESIAN_POINT('Ctrl Pts',(1.36516216870489,-7.79234109685443,-55.0838778715657));
#63250=CARTESIAN_POINT('Ctrl Pts',(1.38295738154021,-7.78920255228993,-55.083151609686));
#63251=CARTESIAN_POINT('Ctrl Pts',(1.4144628695433,-7.7835345540384,-55.0818669245178));
#63252=CARTESIAN_POINT('Ctrl Pts',(1.42817748632771,-7.78102977967554,-55.081308067353));
#63253=CARTESIAN_POINT('Ctrl Pts',(1.4566565951586,-7.77575065496306,-55.0801483179159));
#63254=CARTESIAN_POINT('Ctrl Pts',(1.47141995361585,-7.77297047506448,-55.0795475297301));
#63255=CARTESIAN_POINT('Ctrl Pts',(1.50954510166274,-7.76567838066628,-55.0779970600195));
#63256=CARTESIAN_POINT('Ctrl Pts',(1.53289465464886,-7.76110308592623,-55.0770484699124));
#63257=CARTESIAN_POINT('Ctrl Pts',(1.62735465395755,-7.74215094015142,-55.0732145595764));
#63258=CARTESIAN_POINT('Ctrl Pts',(1.69828723292825,-7.72690138648523,-55.0703436068045));
#63259=CARTESIAN_POINT('Ctrl Pts',(2.14578345272487,-7.62423583244075,-55.0522776679822));
#63260=CARTESIAN_POINT('Ctrl Pts',(2.51573295400785,-7.5102908542568,-55.0375832247385));
#63261=CARTESIAN_POINT('Ctrl Pts',(3.38700965856274,-7.17029422832482,-55.0027578942878));
#63262=CARTESIAN_POINT('Ctrl Pts',(3.87597666938707,-6.9182161861047,-54.9830738033588));
#63263=CARTESIAN_POINT('Ctrl Pts',(4.33965173363069,-6.61448229573179,-54.962016916029));
#63264=CARTESIAN_POINT('Ctrl Pts',(4.3443958525004,-6.6113673235132,-54.9618011901168));
#63265=CARTESIAN_POINT('Ctrl Pts',(4.3974363263187,-6.57645938835733,-54.9593861362115));
#63266=CARTESIAN_POINT('Ctrl Pts',(4.4453856116793,-6.54414325641568,-54.9571733577931));
#63267=CARTESIAN_POINT('Ctrl Pts',(4.59519688106566,-6.4407694412966,-54.9501555438857));
#63268=CARTESIAN_POINT('Ctrl Pts',(4.69573992322429,-6.36783873595535,-54.9452917982395));
#63269=CARTESIAN_POINT('Ctrl Pts',(4.80844199040373,-6.28196727989032,-54.9396215895873));
#63270=CARTESIAN_POINT('Ctrl Pts',(4.82232724922656,-6.27131462901099,-54.9389191316937));
#63271=CARTESIAN_POINT('Ctrl Pts',(4.84268646293899,-6.25558762068886,-54.9378833047485));
#63272=CARTESIAN_POINT('Ctrl Pts',(4.84918808710363,-6.25054906017829,-54.9375516365831));
#63273=CARTESIAN_POINT('Ctrl Pts',(4.86073761865742,-6.24156965948325,-54.9369608707167));
#63274=CARTESIAN_POINT('Ctrl Pts',(4.86578862728181,-6.23763280787818,-54.9367019664899));
#63275=CARTESIAN_POINT('Ctrl Pts',(4.87631014924028,-6.22941157822333,-54.9361615137879));
#63276=CARTESIAN_POINT('Ctrl Pts',(4.88177980762432,-6.22512611855818,-54.9358799120873));
#63277=CARTESIAN_POINT('Ctrl Pts',(4.89595552391453,-6.21398931800964,-54.935148393218));
#63278=CARTESIAN_POINT('Ctrl Pts',(4.904652830353,-6.20712689966362,-54.9346979211494));
#63279=CARTESIAN_POINT('Ctrl Pts',(4.94160509759953,-6.17784437039839,-54.9327768172258));
#63280=CARTESIAN_POINT('Ctrl Pts',(4.9697206627543,-6.15524966826104,-54.9312972045296));
#63281=CARTESIAN_POINT('Ctrl Pts',(5.25984438735853,-5.91881196421239,-54.9158329396264));
#63282=CARTESIAN_POINT('Ctrl Pts',(5.50798872129549,-5.68860916505424,-54.9008070963306));
#63283=CARTESIAN_POINT('Ctrl Pts',(6.03214537722044,-5.13582259156433,-54.8661360406876));
#63284=CARTESIAN_POINT('Ctrl Pts',(6.2985253196356,-4.80541867519549,-54.8463934387766));
#63285=CARTESIAN_POINT('Ctrl Pts',(6.78842564247443,-4.0865946783684,-54.8071227023162));
#63286=CARTESIAN_POINT('Ctrl Pts',(7.00807421978223,-3.69729074594163,-54.787744617808));
#63287=CARTESIAN_POINT('Ctrl Pts',(7.20589821174535,-3.26493570680751,-54.7684269573946));
#63288=CARTESIAN_POINT('Ctrl Pts',(7.21790426194962,-3.23830701100864,-54.7672453917297));
#63289=CARTESIAN_POINT('Ctrl Pts',(7.23402020937555,-3.20202788821996,-54.7656466811127));
#63290=CARTESIAN_POINT('Ctrl Pts',(7.2382587250096,-3.19243506081349,-54.7652250009554));
#63291=CARTESIAN_POINT('Ctrl Pts',(7.24541350942567,-3.17615448412737,-54.7645111103161));
#63292=CARTESIAN_POINT('Ctrl Pts',(7.24833961969394,-3.16947108956614,-54.7642185529997));
#63293=CARTESIAN_POINT('Ctrl Pts',(7.25396054134746,-3.15658410481679,-54.7636554106787));
#63294=CARTESIAN_POINT('Ctrl Pts',(7.256656650154,-3.15038108937497,-54.7633847801005));
#63295=CARTESIAN_POINT('Ctrl Pts',(7.26300349355916,-3.13572734702164,-54.762746471548));
#63296=CARTESIAN_POINT('Ctrl Pts',(7.26664744309853,-3.12727368178568,-54.7623790328226));
#63297=CARTESIAN_POINT('Ctrl Pts',(7.27724324812621,-3.10257376629456,-54.7613077724458));
#63298=CARTESIAN_POINT('Ctrl Pts',(7.28415545578017,-3.08631051080405,-54.7606053470367));
#63299=CARTESIAN_POINT('Ctrl Pts',(7.33372162733152,-2.96859560391608,-54.7555421433691));
#63300=CARTESIAN_POINT('Ctrl Pts',(7.37430993498511,-2.86628452979121,-54.7512543531303));
#63301=CARTESIAN_POINT('Ctrl Pts',(7.49720447543486,-2.53659401286478,-54.7377762512702));
#63302=CARTESIAN_POINT('Ctrl Pts',(7.57122921646478,-2.3062704185657,-54.7288726969598));
#63303=CARTESIAN_POINT('Ctrl Pts',(7.78021302806817,-1.53657481876719,-54.7004080150176));
#63304=CARTESIAN_POINT('Ctrl Pts',(7.86891080164407,-0.98641532140443,-54.6822068182024));
#63305=CARTESIAN_POINT('Ctrl Pts',(7.91985465720725,-0.0538123649053755,
-54.6504379347047));
#63306=CARTESIAN_POINT('Ctrl Pts',(7.91337000618335,0.324836871746122,-54.6372436818979));
#63307=CARTESIAN_POINT('Ctrl Pts',(7.87327200216501,0.775231485755742,-54.619811775851));
#63308=CARTESIAN_POINT('Ctrl Pts',(7.86567703515646,0.84883449291347,-54.6169067280316));
#63309=CARTESIAN_POINT('Ctrl Pts',(7.85576524074399,0.933271187966665,-54.6134988001413));
#63310=CARTESIAN_POINT('Ctrl Pts',(7.85445656603355,0.944221731294924,-54.6130553700091));
#63311=CARTESIAN_POINT('Ctrl Pts',(7.85249638782133,0.960337745646011,-54.612400578634));
#63312=CARTESIAN_POINT('Ctrl Pts',(7.85186267142784,0.965505409223002,-54.6121902853711));
#63313=CARTESIAN_POINT('Ctrl Pts',(7.85072544155476,0.974703822634847,-54.6118153680675));
#63314=CARTESIAN_POINT('Ctrl Pts',(7.85022392345908,0.978734822084512,-54.611650864954));
#63315=CARTESIAN_POINT('Ctrl Pts',(7.84917084580588,0.987146151749603,-54.6113071738757));
#63316=CARTESIAN_POINT('Ctrl Pts',(7.84861872384529,0.991526408678677,-54.6111279516508));
#63317=CARTESIAN_POINT('Ctrl Pts',(7.84716333717579,1.00299532640415,-54.6106580495513));
#63318=CARTESIAN_POINT('Ctrl Pts',(7.84625413587649,1.01008321421707,-54.610367004847));
#63319=CARTESIAN_POINT('Ctrl Pts',(7.84215581171683,1.04169320323664,-54.6090662002666));
#63320=CARTESIAN_POINT('Ctrl Pts',(7.83886135644933,1.06620125290702,-54.6080500618417));
#63321=CARTESIAN_POINT('Ctrl Pts',(7.81369071433686,1.2470251224477,-54.6004990826753));
#63322=CARTESIAN_POINT('Ctrl Pts',(7.78725676529886,1.40266187281416,-54.5937034431917));
#63323=CARTESIAN_POINT('Ctrl Pts',(7.70506796774039,1.81198142835418,-54.5752509547224));
#63324=CARTESIAN_POINT('Ctrl Pts',(7.64144676829595,2.06388651160993,-54.5633017912286));
#63325=CARTESIAN_POINT('Ctrl Pts',(7.47887793826145,2.59581610504982,-54.5374347302143));
#63326=CARTESIAN_POINT('Ctrl Pts',(7.37631452000722,2.8743461955747,-54.5235027177867));
#63327=CARTESIAN_POINT('Ctrl Pts',(7.04605136604026,3.63620759033023,-54.4851950114512));
#63328=CARTESIAN_POINT('Ctrl Pts',(6.78470450018962,4.10326537204607,-54.4615825201537));
#63329=CARTESIAN_POINT('Ctrl Pts',(6.45876003852165,4.56831410171105,-54.4384992005601));
#63330=CARTESIAN_POINT('Ctrl Pts',(6.43908386116293,4.59600631378975,-54.4371257891758));
#63331=CARTESIAN_POINT('Ctrl Pts',(6.41215176109188,4.63339804657379,-54.4352727123481));
#63332=CARTESIAN_POINT('Ctrl Pts',(6.40505119591575,4.64320867986584,-54.4347866427965));
#63333=CARTESIAN_POINT('Ctrl Pts',(6.39381803244136,4.65865439789752,-54.4340215785352));
#63334=CARTESIAN_POINT('Ctrl Pts',(6.38970046314842,4.66430035724578,-54.4337419618911));
#63335=CARTESIAN_POINT('Ctrl Pts',(6.3817465600791,4.6751763510422,-54.4332034051865));
#63336=CARTESIAN_POINT('Ctrl Pts',(6.37791126535237,4.68040713635017,-54.4329444223479));
#63337=CARTESIAN_POINT('Ctrl Pts',(6.36883352970287,4.69275597282373,-54.4323330957064));
#63338=CARTESIAN_POINT('Ctrl Pts',(6.36358557674847,4.6998699724186,-54.4319809815307));
#63339=CARTESIAN_POINT('Ctrl Pts',(6.34820472643205,4.72064689436233,-54.430952784423));
#63340=CARTESIAN_POINT('Ctrl Pts',(6.33803964259337,4.73428599091872,-54.430278043914));
#63341=CARTESIAN_POINT('Ctrl Pts',(6.26353355945322,4.83358518469697,-54.4253670949496));
#63342=CARTESIAN_POINT('Ctrl Pts',(6.19750097002333,4.91796515815086,-54.4212023316967));
#63343=CARTESIAN_POINT('Ctrl Pts',(5.97891491343344,5.1858892174626,-54.4079836331619));
#63344=CARTESIAN_POINT('Ctrl Pts',(5.8197617867117,5.36388418691865,-54.3992147139541));
#63345=CARTESIAN_POINT('Ctrl Pts',(5.33027516492885,5.86384052010145,-54.3742520668002));
#63346=CARTESIAN_POINT('Ctrl Pts',(4.97956829569996,6.16444331915136,-54.3588510296888));
#63347=CARTESIAN_POINT('Ctrl Pts',(4.37634108328926,6.59624298780893,-54.3334674905199));
#63348=CARTESIAN_POINT('Ctrl Pts',(4.13945996405782,6.74741715699987,-54.3237195428597));
#63349=CARTESIAN_POINT('Ctrl Pts',(3.82726271215184,6.92401964554158,-54.3105162097722));
#63350=CARTESIAN_POINT('Ctrl Pts',(3.7589064297778,6.96136551161078,-54.307604097445));
#63351=CARTESIAN_POINT('Ctrl Pts',(3.60447522246403,7.04279988979407,-54.3009525199181));
#63352=CARTESIAN_POINT('Ctrl Pts',(3.51812227366375,7.08633093732711,-54.2971837011257));
#63353=CARTESIAN_POINT('Ctrl Pts',(3.42133577018634,7.13291647927615,-54.2928806013251));
#63354=CARTESIAN_POINT('Ctrl Pts',(3.4116657194556,7.13754670530057,-54.2924498027213));
#63355=CARTESIAN_POINT('Ctrl Pts',(3.3970822320114,7.14449318102415,-54.2917987827865));
#63356=CARTESIAN_POINT('Ctrl Pts',(3.39217591269258,7.14682398564675,-54.2915795360823));
#63357=CARTESIAN_POINT('Ctrl Pts',(3.38365866963553,7.15085945548636,-54.2911985456685));
#63358=CARTESIAN_POINT('Ctrl Pts',(3.38004884333335,7.15256644577872,-54.2910369526625));
#63359=CARTESIAN_POINT('Ctrl Pts',(3.37253689852509,7.15611168679145,-54.2907004361862));
#63360=CARTESIAN_POINT('Ctrl Pts',(3.36863456654996,7.15794948030829,-54.2905254834173));
#63361=CARTESIAN_POINT('Ctrl Pts',(3.3594473907408,7.16226698102246,-54.2901132747033));
#63362=CARTESIAN_POINT('Ctrl Pts',(3.35416130734875,7.16474402910058,-54.2898758496834));
#63363=CARTESIAN_POINT('Ctrl Pts',(3.33690059896053,7.17280907387874,-54.2890997796702));
#63364=CARTESIAN_POINT('Ctrl Pts',(3.32491476919125,7.17837289302026,-54.2885596162353));
#63365=CARTESIAN_POINT('Ctrl Pts',(3.2967952988251,7.19134040826854,-54.2872895073843));
#63366=CARTESIAN_POINT('Ctrl Pts',(3.28065061923264,7.19871985945701,-54.2865580848041));
#63367=CARTESIAN_POINT('Ctrl Pts',(3.22445435503362,7.22417788266252,-54.2840048889515));
#63368=CARTESIAN_POINT('Ctrl Pts',(3.18427766640323,7.24197677251273,-54.282166727798));
#63369=CARTESIAN_POINT('Ctrl Pts',(3.0010058660068,7.32134906706468,-54.273730655506));
#63370=CARTESIAN_POINT('Ctrl Pts',(2.85626581382342,7.37901951401763,-54.2669279512671));
#63371=CARTESIAN_POINT('Ctrl Pts',(2.36597498690947,7.55778490999441,-54.2436384530356));
#63372=CARTESIAN_POINT('Ctrl Pts',(2.01374597081392,7.65916174261451,-54.2265237130789));
#63373=CARTESIAN_POINT('Ctrl Pts',(0.954777347137354,7.88582517094258,-54.1760220124996));
#63374=CARTESIAN_POINT('Ctrl Pts',(0.236505269843306,7.93991533835738,-54.143326706896));
#63375=CARTESIAN_POINT('Ctrl Pts',(-0.527536777721723,7.89353919428657,
-54.1119875467441));
#63376=CARTESIAN_POINT('Ctrl Pts',(-0.575743200093329,7.89016957608742,
-54.1100229434521));
#63377=CARTESIAN_POINT('Ctrl Pts',(-0.638558583107613,7.88520004022847,
-54.1074791035554));
#63378=CARTESIAN_POINT('Ctrl Pts',(-0.653197666611395,7.88400085932392,
-54.1068874066684));
#63379=CARTESIAN_POINT('Ctrl Pts',(-0.676593578275714,7.88201874025823,
-54.1059435772616));
#63380=CARTESIAN_POINT('Ctrl Pts',(-0.685352554448037,7.88126196549125,
-54.1055906314457));
#63381=CARTESIAN_POINT('Ctrl Pts',(-0.701132244824671,7.87987209705478,
-54.104955509869));
#63382=CARTESIAN_POINT('Ctrl Pts',(-0.70815340196265,7.87924421821569,-54.1046731723242));
#63383=CARTESIAN_POINT('Ctrl Pts',(-0.724622764837934,7.87774922606578,
-54.1040115045075));
#63384=CARTESIAN_POINT('Ctrl Pts',(-0.734070277839707,7.87687449741978,
-54.1036324113009));
#63385=CARTESIAN_POINT('Ctrl Pts',(-0.761298783026993,7.87430404548855,
-54.102541169781));
#63386=CARTESIAN_POINT('Ctrl Pts',(-0.779075686902149,7.87256509132898,
-54.101830364832));
#63387=CARTESIAN_POINT('Ctrl Pts',(-0.898106115901136,7.86051429523538,
-54.0970818016465));
#63388=CARTESIAN_POINT('Ctrl Pts',(-0.999160426027807,7.84830930590992,
-54.0931030971454));
#63389=CARTESIAN_POINT('Ctrl Pts',(-1.28813586429848,7.80773576039618,-54.0818599010228));
#63390=CARTESIAN_POINT('Ctrl Pts',(-1.47531081369862,7.7745414531394,-54.0747426720493));
#63391=CARTESIAN_POINT('Ctrl Pts',(-1.83166968149462,7.69800867037327,-54.0613989607363));
#63392=CARTESIAN_POINT('Ctrl Pts',(-2.00096880400117,7.65574802760517,-54.0551507118788));
#63393=CARTESIAN_POINT('Ctrl Pts',(-2.28597915186834,7.57450217896144,-54.0446809017212));
#63394=CARTESIAN_POINT('Ctrl Pts',(-2.40243493916674,7.53837454788521,-54.0404167511492));
#63395=CARTESIAN_POINT('Ctrl Pts',(-2.81028230597749,7.40143817982617,-54.0254402659087));
#63396=CARTESIAN_POINT('Ctrl Pts',(-3.09656329809623,7.2863066337836,-54.0148577191107));
#63397=CARTESIAN_POINT('Ctrl Pts',(-3.40956978446522,7.13864014658615,-54.0026343744809));
#63398=CARTESIAN_POINT('Ctrl Pts',(-3.44363326145886,7.12227064854316,-54.0012950392811));
#63399=CARTESIAN_POINT('Ctrl Pts',(-3.76574166829126,6.96462766408025,-53.9885334794922));
#63400=CARTESIAN_POINT('Ctrl Pts',(-4.04505660463857,6.80620108412178,-53.9766925878763));
#63401=CARTESIAN_POINT('Ctrl Pts',(-4.33844329437361,6.61533686096317,-53.9627985377571));
#63402=CARTESIAN_POINT('Ctrl Pts',(-4.36280775354252,6.59929393807605,-53.9616345004365));
#63403=CARTESIAN_POINT('Ctrl Pts',(-4.39663083261573,6.57675375666423,-53.9600048083122));
#63404=CARTESIAN_POINT('Ctrl Pts',(-4.40616505888879,6.57037001441782,-53.9595438886546));
#63405=CARTESIAN_POINT('Ctrl Pts',(-4.4214421071285,6.56009289807269,-53.9588029098848));
#63406=CARTESIAN_POINT('Ctrl Pts',(-4.42719377251512,6.55621265963195,-53.9585233838279));
#63407=CARTESIAN_POINT('Ctrl Pts',(-4.43906753975161,6.54817952596347,-53.9579451917989));
#63408=CARTESIAN_POINT('Ctrl Pts',(-4.4451889342762,6.54402560087327,-53.9576464848813));
#63409=CARTESIAN_POINT('Ctrl Pts',(-4.45732492998902,6.53576533437485,-53.9570530497392));
#63410=CARTESIAN_POINT('Ctrl Pts',(-4.46333970672917,6.53165926082139,-53.9567583321149));
#63411=CARTESIAN_POINT('Ctrl Pts',(-4.47726592047649,6.52212411282612,-53.9560745773543));
#63412=CARTESIAN_POINT('Ctrl Pts',(-4.48517315990093,6.51668894382885,-53.9556853060677));
#63413=CARTESIAN_POINT('Ctrl Pts',(-4.50566675118284,6.50254737353732,-53.9546737452906));
#63414=CARTESIAN_POINT('Ctrl Pts',(-4.51823773553338,6.49381882867644,-53.9540506256486));
#63415=CARTESIAN_POINT('Ctrl Pts',(-4.55523033899245,6.46797394418664,-53.9522093826615));
#63416=CARTESIAN_POINT('Ctrl Pts',(-4.57958047769725,6.45075600290295,-53.9509876024828));
#63417=CARTESIAN_POINT('Ctrl Pts',(-4.66479673544995,6.38977404577522,-53.9466785186104));
#63418=CARTESIAN_POINT('Ctrl Pts',(-4.7251369363859,6.34528341028031,-53.943567207087));
#63419=CARTESIAN_POINT('Ctrl Pts',(-4.97783665199664,6.15335683717133,-53.9303023267239));
#63420=CARTESIAN_POINT('Ctrl Pts',(-5.1639967069711,5.99798225554863,-53.919948609754));
#63421=CARTESIAN_POINT('Ctrl Pts',(-5.56753592953707,5.62844433692675,-53.8964533828573));
#63422=CARTESIAN_POINT('Ctrl Pts',(-5.7802616289256,5.40975237373494,-53.8833066262118));
#63423=CARTESIAN_POINT('Ctrl Pts',(-6.24458390832893,4.87366548593838,-53.853022640944));
#63424=CARTESIAN_POINT('Ctrl Pts',(-6.48551043081799,4.54814423017104,-53.8360489401067));
#63425=CARTESIAN_POINT('Ctrl Pts',(-6.70282136106142,4.20191931343049,-53.8191356191575));
#63426=CARTESIAN_POINT('Ctrl Pts',(-6.70514255138793,4.19821432045426,-53.8189547476318));
#63427=CARTESIAN_POINT('Ctrl Pts',(-6.87885152113025,3.92043531800506,-53.8054029773147));
#63428=CARTESIAN_POINT('Ctrl Pts',(-7.0332886609483,3.6361065271504,-53.7921346187607));
#63429=CARTESIAN_POINT('Ctrl Pts',(-7.18961545053255,3.30083744898722,-53.7771431321115));
#63430=CARTESIAN_POINT('Ctrl Pts',(-7.20895930240743,3.25837444117939,-53.7752562593331));
#63431=CARTESIAN_POINT('Ctrl Pts',(-7.23934303553309,3.19008185295821,-53.7722404787148));
#63432=CARTESIAN_POINT('Ctrl Pts',(-7.25062294358469,3.16436040169295,-53.7711088712501));
#63433=CARTESIAN_POINT('Ctrl Pts',(-7.27043170174463,3.11852865971118,-53.7691000058417));
#63434=CARTESIAN_POINT('Ctrl Pts',(-7.27901467459513,3.09844210880646,-53.7682221276886));
#63435=CARTESIAN_POINT('Ctrl Pts',(-7.29677053647698,3.05640746370622,-53.7663902825494));
#63436=CARTESIAN_POINT('Ctrl Pts',(-7.30592784959485,3.03445301614396,-53.7654365069312));
#63437=CARTESIAN_POINT('Ctrl Pts',(-7.32425095668012,2.98996001677971,-53.7635095607009));
#63438=CARTESIAN_POINT('Ctrl Pts',(-7.33341207479184,2.9674198092773,-53.7625364546635));
#63439=CARTESIAN_POINT('Ctrl Pts',(-7.35570370444462,2.91183929149015,-53.7601444383015));
#63440=CARTESIAN_POINT('Ctrl Pts',(-7.36871576535513,2.87875199201673,-53.7587269627814));
#63441=CARTESIAN_POINT('Ctrl Pts',(-7.47764032933658,2.59619880073618,-53.7466764401149));
#63442=CARTESIAN_POINT('Ctrl Pts',(-7.56107837369439,2.34210426292137,-53.7362052059926));
#63443=CARTESIAN_POINT('Ctrl Pts',(-7.78632216112692,1.51738015987966,-53.7030462575338));
#63444=CARTESIAN_POINT('Ctrl Pts',(-7.87749459837603,0.935029773221766,
-53.6809717783752));
#63445=CARTESIAN_POINT('Ctrl Pts',(-7.90556123071894,0.297601721963366,
-53.6556410791621));
#63446=CARTESIAN_POINT('Ctrl Pts',(-7.90729799371476,0.247191245373527,
-53.6536290007675));
#63447=CARTESIAN_POINT('Ctrl Pts',(-7.9089784646963,0.179649317186588,-53.6509186451043));
#63448=CARTESIAN_POINT('Ctrl Pts',(-7.90934879906975,0.162529388289797,
-53.6502303822926));
#63449=CARTESIAN_POINT('Ctrl Pts',(-7.90985409391974,0.13504327102425,-53.6491233474437));
#63450=CARTESIAN_POINT('Ctrl Pts',(-7.91002426783803,0.124677799078725,
-53.6487054081451));
#63451=CARTESIAN_POINT('Ctrl Pts',(-7.91032660525457,0.10375662961902,-53.6478609566455));
#63452=CARTESIAN_POINT('Ctrl Pts',(-7.91045801604645,0.0932009418190795,
-53.6474344283171));
#63453=CARTESIAN_POINT('Ctrl Pts',(-7.9106823020334,0.0717328708784928,
-53.6465660377603));
#63454=CARTESIAN_POINT('Ctrl Pts',(-7.91077372669421,0.0608204953856951,
-53.6461241447665));
#63455=CARTESIAN_POINT('Ctrl Pts',(-7.91094750178523,0.0332756570924339,
-53.6450075353264));
#63456=CARTESIAN_POINT('Ctrl Pts',(-7.91099997780887,0.016643096219158,
-53.644332190979));
#63457=CARTESIAN_POINT('Ctrl Pts',(-7.91099999999297,1.05515043374329E-5,
-53.643655794299));
#63458=CARTESIAN_POINT('',(-7.89680882399629,-0.000256294892049957,-49.6423315082368));
#63459=CARTESIAN_POINT('Ctrl Pts',(-7.91099999999197,1.12721192983993E-5,
-53.6436558236043));
#63460=CARTESIAN_POINT('Ctrl Pts',(-7.91100002702492,-0.0189609985400898,
-53.6428842771856));
#63461=CARTESIAN_POINT('Ctrl Pts',(-7.91093180470916,-0.0379331745797025,
-53.6421113645619));
#63462=CARTESIAN_POINT('Ctrl Pts',(-7.91048557968446,-0.0999664205042712,
-53.6395798981015));
#63463=CARTESIAN_POINT('Ctrl Pts',(-7.90982423016865,-0.143024459786413,
-53.6378160390351));
#63464=CARTESIAN_POINT('Ctrl Pts',(-7.90073970735434,-0.529147779870896,
-53.6219444644952));
#63465=CARTESIAN_POINT('Ctrl Pts',(-7.87035369665328,-0.871327190126642,
-53.6075096709314));
#63466=CARTESIAN_POINT('Ctrl Pts',(-7.76213187703278,-1.5702950088947,-53.5778013395704));
#63467=CARTESIAN_POINT('Ctrl Pts',(-7.68163567755936,-1.92587693057893,
-53.5625699733064));
#63468=CARTESIAN_POINT('Ctrl Pts',(-7.54580730289272,-2.37832499210327,
-53.5431354014342));
#63469=CARTESIAN_POINT('Ctrl Pts',(-7.51255932009513,-2.48134852123084,
-53.5387046220139));
#63470=CARTESIAN_POINT('Ctrl Pts',(-7.45924604033683,-2.63563923007961,
-53.5320571036591));
#63471=CARTESIAN_POINT('Ctrl Pts',(-7.44074298114661,-2.68743178207014,
-53.5298235762763));
#63472=CARTESIAN_POINT('Ctrl Pts',(-7.40980630311237,-2.77125817332328,
-53.5262043965742));
#63473=CARTESIAN_POINT('Ctrl Pts',(-7.39770146552207,-2.80341119935944,
-53.5248151816664));
#63474=CARTESIAN_POINT('Ctrl Pts',(-7.37607954411903,-2.85972830219121,
-53.5223798726228));
#63475=CARTESIAN_POINT('Ctrl Pts',(-7.3666522171318,-2.88392623359077,-53.5213328164106));
#63476=CARTESIAN_POINT('Ctrl Pts',(-7.34733957858663,-2.93278501879802,
-53.5192171699519));
#63477=CARTESIAN_POINT('Ctrl Pts',(-7.33744884296905,-2.9574433776601,-53.5181486530537));
#63478=CARTESIAN_POINT('Ctrl Pts',(-7.3180684927669,-3.00506436558251,-53.5160834273292));
#63479=CARTESIAN_POINT('Ctrl Pts',(-7.30859454848868,-3.02803303094017,
-53.5150865653112));
#63480=CARTESIAN_POINT('Ctrl Pts',(-7.28572123517774,-3.08275442350778,
-53.5127096164695));
#63481=CARTESIAN_POINT('Ctrl Pts',(-7.27222225325317,-3.11446500435225,
-53.5113305899829));
#63482=CARTESIAN_POINT('Ctrl Pts',(-7.22195588171039,-3.23043743296493,
-53.5062805077389));
#63483=CARTESIAN_POINT('Ctrl Pts',(-7.18392752531771,-3.31414517998115,
-53.5026224676579));
#63484=CARTESIAN_POINT('Ctrl Pts',(-6.87478793413653,-3.96428365237463,
-53.4740724235326));
#63485=CARTESIAN_POINT('Ctrl Pts',(-6.53854507107019,-4.49730640849635,
-53.4498176057152));
#63486=CARTESIAN_POINT('Ctrl Pts',(-5.97557082726451,-5.19104145605043,
-53.4163758555366));
#63487=CARTESIAN_POINT('Ctrl Pts',(-5.79807018158413,-5.38857501834833,
-53.4065603048889));
#63488=CARTESIAN_POINT('Ctrl Pts',(-5.36046472943528,-5.82886124220214,
-53.3834768605279));
#63489=CARTESIAN_POINT('Ctrl Pts',(-5.09326571789599,-6.06373013307058,
-53.3702017227878));
#63490=CARTESIAN_POINT('Ctrl Pts',(-4.77484522693447,-6.30768355747168,
-53.3543740885788));
#63491=CARTESIAN_POINT('Ctrl Pts',(-4.73824652610216,-6.33522206106347,
-53.3525544075141));
#63492=CARTESIAN_POINT('Ctrl Pts',(-4.69406355250205,-6.36787027438284,
-53.3503546979899));
#63493=CARTESIAN_POINT('Ctrl Pts',(-4.68670652980634,-6.37328693602695,
-53.3499883215119));
#63494=CARTESIAN_POINT('Ctrl Pts',(-4.67390153620025,-6.38268054396916,
-53.3493504422283));
#63495=CARTESIAN_POINT('Ctrl Pts',(-4.66845782315042,-6.38666329546004,
-53.3490792028215));
#63496=CARTESIAN_POINT('Ctrl Pts',(-4.65753742873333,-6.39463149664297,
-53.3485349453204));
#63497=CARTESIAN_POINT('Ctrl Pts',(-4.65206070892645,-6.39861688476756,
-53.3482619247411));
#63498=CARTESIAN_POINT('Ctrl Pts',(-4.64161709505353,-6.40619616692135,
-53.3477411563492));
#63499=CARTESIAN_POINT('Ctrl Pts',(-4.63665112701863,-6.40979133140875,
-53.347493468229));
#63500=CARTESIAN_POINT('Ctrl Pts',(-4.62508553787768,-6.4181438870735,-53.3469164562783));
#63501=CARTESIAN_POINT('Ctrl Pts',(-4.61848275423037,-6.42289687260343,
-53.3465869244099));
#63502=CARTESIAN_POINT('Ctrl Pts',(-4.59531119625548,-6.4395226140326,-53.345430030395));
#63503=CARTESIAN_POINT('Ctrl Pts',(-4.57870396493736,-6.45134144794868,
-53.3446000755267));
#63504=CARTESIAN_POINT('Ctrl Pts',(-4.36692899180706,-6.60082527398464,
-53.3340040559917));
#63505=CARTESIAN_POINT('Ctrl Pts',(-4.16570619869486,-6.72962258959657,
-53.3237352679951));
#63506=CARTESIAN_POINT('Ctrl Pts',(-3.89865460003981,-6.88398652516736,
-53.310048830646));
#63507=CARTESIAN_POINT('Ctrl Pts',(-3.83785873621647,-6.91806462862786,
-53.3069307604148));
#63508=CARTESIAN_POINT('Ctrl Pts',(-3.72617696676273,-6.97874071467036,
-53.3012076582846));
#63509=CARTESIAN_POINT('Ctrl Pts',(-3.67543608525703,-7.0055967775992,-53.2986092187451));
#63510=CARTESIAN_POINT('Ctrl Pts',(-3.46542712837245,-7.11384040233811,
-53.2878726130681));
#63511=CARTESIAN_POINT('Ctrl Pts',(-3.3037151895838,-7.19036680263977,-53.2796482495858));
#63512=CARTESIAN_POINT('Ctrl Pts',(-2.79942460730235,-7.40840436506582,
-53.2543485302309));
#63513=CARTESIAN_POINT('Ctrl Pts',(-2.4493707651624,-7.5313902550396,-53.237286030588));
#63514=CARTESIAN_POINT('Ctrl Pts',(-1.82198656211996,-7.70341873800769,
-53.2082899639828));
#63515=CARTESIAN_POINT('Ctrl Pts',(-1.54824521200786,-7.76306968124812,
-53.1961371237463));
#63516=CARTESIAN_POINT('Ctrl Pts',(-1.1502316833176,-7.82790419135908,-53.179251288626));
#63517=CARTESIAN_POINT('Ctrl Pts',(-1.02811373373937,-7.84487736208303,
-53.174173430987));
#63518=CARTESIAN_POINT('Ctrl Pts',(-0.886452852558304,-7.86120191727009,
-53.168398556748));
#63519=CARTESIAN_POINT('Ctrl Pts',(-0.867252224354421,-7.86334329848461,
-53.1676182726197));
#63520=CARTESIAN_POINT('Ctrl Pts',(-0.838082974517854,-7.86648830803632,
-53.1664365500466));
#63521=CARTESIAN_POINT('Ctrl Pts',(-0.828120036341239,-7.86754336365334,
-53.1660335751573));
#63522=CARTESIAN_POINT('Ctrl Pts',(-0.810852193222569,-7.86933883053438,
-53.1653362562627));
#63523=CARTESIAN_POINT('Ctrl Pts',(-0.803548222908068,-7.87008800222871,
-53.1650416507617));
#63524=CARTESIAN_POINT('Ctrl Pts',(-0.788380924656921,-7.87162238460148,
-53.1644305961292));
#63525=CARTESIAN_POINT('Ctrl Pts',(-0.78051743965155,-7.87240598387672,
-53.1641141954394));
#63526=CARTESIAN_POINT('Ctrl Pts',(-0.761377482731788,-7.87428432846523,
-53.1633450373065));
#63527=CARTESIAN_POINT('Ctrl Pts',(-0.75009979337468,-7.87536663641831,
-53.1628926517963));
#63528=CARTESIAN_POINT('Ctrl Pts',(-0.707584451377801,-7.87935463568644,
-53.1611902893438));
#63529=CARTESIAN_POINT('Ctrl Pts',(-0.676331749001465,-7.88209874484733,
-53.1599451391207));
#63530=CARTESIAN_POINT('Ctrl Pts',(-0.139654209866519,-7.92600566489746,
-53.138668157586));
#63531=CARTESIAN_POINT('Ctrl Pts',(0.368573939751416,-7.91866740911749,
-53.1202152915526));
#63532=CARTESIAN_POINT('Ctrl Pts',(1.15287861987413,-7.83162110008994,-53.0925550642215));
#63533=CARTESIAN_POINT('Ctrl Pts',(1.43124899721987,-7.78556006609077,-53.0828787207781));
#63534=CARTESIAN_POINT('Ctrl Pts',(2.02037120439611,-7.65540997558865,-53.0619686508084));
#63535=CARTESIAN_POINT('Ctrl Pts',(2.32964800912201,-7.56702867024691,-53.0507245832274));
#63536=CARTESIAN_POINT('Ctrl Pts',(2.75242743429345,-7.41782924016103,-53.0341127852327));
#63537=CARTESIAN_POINT('Ctrl Pts',(2.87113992820904,-7.37269290110939,-53.029305586341));
#63538=CARTESIAN_POINT('Ctrl Pts',(3.04632359976529,-7.30121260201027,-53.0219365156387));
#63539=CARTESIAN_POINT('Ctrl Pts',(3.10365348030273,-7.27702740358645,-53.0194792903216));
#63540=CARTESIAN_POINT('Ctrl Pts',(3.1711544788704,-7.24760860241437,-53.0165299997432));
#63541=CARTESIAN_POINT('Ctrl Pts',(3.18160411427374,-7.24302743614106,-53.0160718703603));
#63542=CARTESIAN_POINT('Ctrl Pts',(3.19707522586062,-7.23620489199369,-53.0153913197354));
#63543=CARTESIAN_POINT('Ctrl Pts',(3.20210436562234,-7.23398084529981,-53.015169739179));
#63544=CARTESIAN_POINT('Ctrl Pts',(3.21227539615853,-7.22947020512913,-53.0147208950278));
#63545=CARTESIAN_POINT('Ctrl Pts',(3.21741717395064,-7.22718336533366,-53.014493619703));
#63546=CARTESIAN_POINT('Ctrl Pts',(3.22737650677894,-7.2227411512545,-53.0140526883302));
#63547=CARTESIAN_POINT('Ctrl Pts',(3.23219435455598,-7.22058643800766,-53.013839063575));
#63548=CARTESIAN_POINT('Ctrl Pts',(3.2436599360143,-7.21544484653496,-53.0133299125973));
#63549=CARTESIAN_POINT('Ctrl Pts',(3.25030569732191,-7.21245360382402,-53.013034182912));
#63550=CARTESIAN_POINT('Ctrl Pts',(3.2738930285119,-7.2017977756235,-53.0119824201069));
#63551=CARTESIAN_POINT('Ctrl Pts',(3.29081161635932,-7.19408268375149,-53.0112240736656));
#63552=CARTESIAN_POINT('Ctrl Pts',(3.59139985970576,-7.05572839257941,-52.9976824491142));
#63553=CARTESIAN_POINT('Ctrl Pts',(3.86710227865614,-6.90846984218416,-52.9841908795885));
#63554=CARTESIAN_POINT('Ctrl Pts',(4.54289989184964,-6.49435763903491,-52.9494867387107));
#63555=CARTESIAN_POINT('Ctrl Pts',(4.92875672625827,-6.20661073241221,-52.928156868474));
#63556=CARTESIAN_POINT('Ctrl Pts',(5.45361778779953,-5.73521180589861,-52.8979547851229));
#63557=CARTESIAN_POINT('Ctrl Pts',(5.61461250349194,-5.57769975749903,-52.8884824431236));
#63558=CARTESIAN_POINT('Ctrl Pts',(5.8226450180353,-5.35601961679021,-52.8759407528129));
#63559=CARTESIAN_POINT('Ctrl Pts',(5.87575217778226,-5.29770495360397,-52.8727098871846));
#63560=CARTESIAN_POINT('Ctrl Pts',(5.95270327768995,-5.21062747916333,-52.8679818155184));
#63561=CARTESIAN_POINT('Ctrl Pts',(5.9772291981772,-5.18247490884502,-52.8664676575379));
#63562=CARTESIAN_POINT('Ctrl Pts',(6.01567415556181,-5.13770912892152,-52.8640822325936));
#63563=CARTESIAN_POINT('Ctrl Pts',(6.02972570971153,-5.12121064891564,-52.8632077962738));
#63564=CARTESIAN_POINT('Ctrl Pts',(6.05346525922978,-5.09310396029484,-52.861725985687));
#63565=CARTESIAN_POINT('Ctrl Pts',(6.06318806952148,-5.08152536454749,-52.8611178006525));
#63566=CARTESIAN_POINT('Ctrl Pts',(6.08242592134681,-5.05848177713828,-52.8599118088436));
#63567=CARTESIAN_POINT('Ctrl Pts',(6.09194188579058,-5.04701763819135,-52.8593139825223));
#63568=CARTESIAN_POINT('Ctrl Pts',(6.11032991156404,-5.02473731370604,-52.8581562391133));
#63569=CARTESIAN_POINT('Ctrl Pts',(6.11920577843296,-5.01392434551207,-52.8575962382175));
#63570=CARTESIAN_POINT('Ctrl Pts',(6.13967113511034,-4.98885726848925,-52.8563022898844));
#63571=CARTESIAN_POINT('Ctrl Pts',(6.15123975863613,-4.97458620666899,-52.8555688017202));
#63572=CARTESIAN_POINT('Ctrl Pts',(6.18224014556943,-4.93607061970106,-52.8535976201832));
#63573=CARTESIAN_POINT('Ctrl Pts',(6.20157901639117,-4.91175163219555,-52.8523618919502));
#63574=CARTESIAN_POINT('Ctrl Pts',(6.32577904400391,-4.75366490269811,-52.8443850291563));
#63575=CARTESIAN_POINT('Ctrl Pts',(6.42645115662078,-4.61665879369899,-52.8377319897511));
#63576=CARTESIAN_POINT('Ctrl Pts',(6.54444612974146,-4.44473078544374,-52.829676839139));
#63577=CARTESIAN_POINT('Ctrl Pts',(6.56602602861521,-4.41278926735364,-52.8281922947841));
#63578=CARTESIAN_POINT('Ctrl Pts',(6.65530053349824,-4.27854461822577,-52.8220017005931));
#63579=CARTESIAN_POINT('Ctrl Pts',(6.72084506145249,-4.17483073539156,-52.8173366316686));
#63580=CARTESIAN_POINT('Ctrl Pts',(7.08487275782888,-3.5680078834272,-52.7906434222177));
#63581=CARTESIAN_POINT('Ctrl Pts',(7.32921812444578,-3.03457336670946,-52.7696645232624));
#63582=CARTESIAN_POINT('Ctrl Pts',(7.58610694931989,-2.2561117262073,-52.7389391062643));
#63583=CARTESIAN_POINT('Ctrl Pts',(7.64972400461407,-2.02996842347896,-52.7299800208232));
#63584=CARTESIAN_POINT('Ctrl Pts',(7.70869948872653,-1.77776807519418,-52.7197024752829));
#63585=CARTESIAN_POINT('Ctrl Pts',(7.71410390660696,-1.75416876033622,-52.7187380155588));
#63586=CARTESIAN_POINT('Ctrl Pts',(7.72334957399867,-1.71292684116246,-52.7170472764588));
#63587=CARTESIAN_POINT('Ctrl Pts',(7.72723892429009,-1.69529513823244,-52.7163227795032));
#63588=CARTESIAN_POINT('Ctrl Pts',(7.73275670556999,-1.66986770567176,-52.7152753825));
#63589=CARTESIAN_POINT('Ctrl Pts',(7.73443379454953,-1.66208251874812,-52.7149543515154));
#63590=CARTESIAN_POINT('Ctrl Pts',(7.73745670238156,-1.64794627520262,-52.7143707814436));
#63591=CARTESIAN_POINT('Ctrl Pts',(7.7388064657309,-1.64159606262795,-52.7141083965554));
#63592=CARTESIAN_POINT('Ctrl Pts',(7.74137834962042,-1.62942249069487,-52.7136049329361));
#63593=CARTESIAN_POINT('Ctrl Pts',(7.74260172054804,-1.62359939698613,-52.7133639038175));
#63594=CARTESIAN_POINT('Ctrl Pts',(7.74545563358543,-1.60993854460412,-52.7127979697225));
#63595=CARTESIAN_POINT('Ctrl Pts',(7.7470808484334,-1.60209968991191,-52.712472851856));
#63596=CARTESIAN_POINT('Ctrl Pts',(7.75180614388307,-1.57913298061151,-52.7115191795198));
#63597=CARTESIAN_POINT('Ctrl Pts',(7.75487382108652,-1.56399855408818,-52.7108893083089));
#63598=CARTESIAN_POINT('Ctrl Pts',(7.782224164587,-1.4270063188038,-52.7051743687861));
#63599=CARTESIAN_POINT('Ctrl Pts',(7.80367416563023,-1.30461766666458,-52.6999637659348));
#63600=CARTESIAN_POINT('Ctrl Pts',(7.84117742111788,-1.05637987885594,-52.68917316117));
#63601=CARTESIAN_POINT('Ctrl Pts',(7.85710242186937,-0.930559546041092,
-52.6835999825171));
#63602=CARTESIAN_POINT('Ctrl Pts',(7.93065946988354,-0.210914545287183,
-52.6513330725044));
#63603=CARTESIAN_POINT('Ctrl Pts',(7.92399604971076,0.387550362873824,-52.6231564290536));
#63604=CARTESIAN_POINT('Ctrl Pts',(7.8011078152088,1.37232105446176,-52.5787878422552));
#63605=CARTESIAN_POINT('Ctrl Pts',(7.72269823713091,1.76083492376877,-52.5617773198753));
#63606=CARTESIAN_POINT('Ctrl Pts',(7.60931988864801,2.16395408861853,-52.5448129476295));
#63607=CARTESIAN_POINT('Ctrl Pts',(7.60301760707755,2.18599399444951,-52.5438875203673));
#63608=CARTESIAN_POINT('Ctrl Pts',(7.59376218832772,2.21783715296122,-52.5425534351542));
#63609=CARTESIAN_POINT('Ctrl Pts',(7.59088570658172,2.2276624521231,-52.542142208943));
#63610=CARTESIAN_POINT('Ctrl Pts',(7.58583759785336,2.24478214135517,-52.5414263949472));
#63611=CARTESIAN_POINT('Ctrl Pts',(7.58367450555498,2.25207902112035,-52.5411215207078));
#63612=CARTESIAN_POINT('Ctrl Pts',(7.57947874693681,2.26615821510045,-52.5405337043885));
#63613=CARTESIAN_POINT('Ctrl Pts',(7.57744749947612,2.27294094163086,-52.5402507149134));
#63614=CARTESIAN_POINT('Ctrl Pts',(7.57261570315503,2.28899677709366,-52.5395812897497));
#63615=CARTESIAN_POINT('Ctrl Pts',(7.56980721958029,2.29826749803552,-52.5391951221967));
#63616=CARTESIAN_POINT('Ctrl Pts',(7.55990958804265,2.33072432308706,-52.5378444077641));
#63617=CARTESIAN_POINT('Ctrl Pts',(7.55273084925143,2.35388308592757,-52.5368828931832));
#63618=CARTESIAN_POINT('Ctrl Pts',(7.46232250866173,2.64087036090666,-52.5249950893046));
#63619=CARTESIAN_POINT('Ctrl Pts',(7.36541257242053,2.9002015642793,-52.5145512182811));
#63620=CARTESIAN_POINT('Ctrl Pts',(7.12674886395633,3.4492071834908,-52.4928082906876));
#63621=CARTESIAN_POINT('Ctrl Pts',(6.98048116937463,3.73637221448944,-52.4816734275056));
#63622=CARTESIAN_POINT('Ctrl Pts',(6.60216276518799,4.37890997598966,-52.4563792469477));
#63623=CARTESIAN_POINT('Ctrl Pts',(6.35824027697082,4.72611508094225,-52.4424273341736));
#63624=CARTESIAN_POINT('Ctrl Pts',(5.96980495537363,5.19417289012871,-52.4211834513752));
#63625=CARTESIAN_POINT('Ctrl Pts',(5.84697543773632,5.33206108968397,-52.4145758744677));
#63626=CARTESIAN_POINT('Ctrl Pts',(5.65238512565059,5.53569182749666,-52.4040603209864));
#63627=CARTESIAN_POINT('Ctrl Pts',(5.58404534539639,5.60462112066307,-52.4003588169086));
#63628=CARTESIAN_POINT('Ctrl Pts',(5.48002523511382,5.70574714492927,-52.394681705838));
#63629=CARTESIAN_POINT('Ctrl Pts',(5.44528995727355,5.73890618090714,-52.3927790298638));
#63630=CARTESIAN_POINT('Ctrl Pts',(5.40369271140936,5.77789814714745,-52.3904893711769));
#63631=CARTESIAN_POINT('Ctrl Pts',(5.39711930433196,5.7840388252189,-52.390127222238));
#63632=CARTESIAN_POINT('Ctrl Pts',(5.38698938303814,5.79346958743522,-52.3895686089832));
#63633=CARTESIAN_POINT('Ctrl Pts',(5.38344027707442,5.79676765589825,-52.3893727951164));
#63634=CARTESIAN_POINT('Ctrl Pts',(5.37722856001985,5.80252937712869,-52.3890299005343));
#63635=CARTESIAN_POINT('Ctrl Pts',(5.37456727662865,5.80499446580583,-52.3888829375943));
#63636=CARTESIAN_POINT('Ctrl Pts',(5.36898273534355,5.81016017218064,-52.3885744236157));
#63637=CARTESIAN_POINT('Ctrl Pts',(5.36605913386094,5.8128604155447,-52.3884128418346));
#63638=CARTESIAN_POINT('Ctrl Pts',(5.35785377439249,5.82042743402754,-52.3879591487498));
#63639=CARTESIAN_POINT('Ctrl Pts',(5.3525674371411,5.82528921279591,-52.3876666244402));
#63640=CARTESIAN_POINT('Ctrl Pts',(5.3307643088617,5.84528654331986,-52.3864592112173));
#63641=CARTESIAN_POINT('Ctrl Pts',(5.3141900322955,5.86035896257719,-52.3855391976666));
#63642=CARTESIAN_POINT('Ctrl Pts',(5.04434088963895,6.10366996801012,-52.3705290887467));
#63643=CARTESIAN_POINT('Ctrl Pts',(4.77665722413495,6.31535139484789,-52.3552083962517));
#63644=CARTESIAN_POINT('Ctrl Pts',(4.04824236441221,6.81850800380864,-52.3144007927183));
#63645=CARTESIAN_POINT('Ctrl Pts',(3.5695024999634,7.08089340082615,-52.2885144927858));
#63646=CARTESIAN_POINT('Ctrl Pts',(2.71618024454574,7.43986843705048,-52.2469874924611));
#63647=CARTESIAN_POINT('Ctrl Pts',(2.35450097964251,7.56212006460558,-52.2306214389443));
#63648=CARTESIAN_POINT('Ctrl Pts',(1.96347746520389,7.66349717170413,-52.2142862625562));
#63649=CARTESIAN_POINT('Ctrl Pts',(1.94155716979059,7.66908002470962,-52.2133748159648));
#63650=CARTESIAN_POINT('Ctrl Pts',(1.90997785344604,7.67697884884465,-52.212067853168));
#63651=CARTESIAN_POINT('Ctrl Pts',(1.90033805074685,7.67937073855313,-52.2116697109006));
#63652=CARTESIAN_POINT('Ctrl Pts',(1.88358904636068,7.68349314042776,-52.2109793575367));
#63653=CARTESIAN_POINT('Ctrl Pts',(1.8764819128227,7.68523195263545,-52.2106868599002));
#63654=CARTESIAN_POINT('Ctrl Pts',(1.86280423899916,7.68855819115315,-52.2101247941411));
#63655=CARTESIAN_POINT('Ctrl Pts',(1.85623405910754,7.69014706034183,-52.2098551764426));
#63656=CARTESIAN_POINT('Ctrl Pts',(1.84074085060018,7.69387277690071,-52.2092202693648));
#63657=CARTESIAN_POINT('Ctrl Pts',(1.83181611497211,7.69600252780231,-52.2088552248557));
#63658=CARTESIAN_POINT('Ctrl Pts',(1.80089854231039,7.7033237030865,-52.2075929896733));
#63659=CARTESIAN_POINT('Ctrl Pts',(1.77888708044802,7.70843644332623,-52.2066985082712));
#63660=CARTESIAN_POINT('Ctrl Pts',(1.52487292395613,7.76629193975539,-52.1964233911832));
#63661=CARTESIAN_POINT('Ctrl Pts',(1.2906175486389,7.80863919253579,-52.1874074763967));
#63662=CARTESIAN_POINT('Ctrl Pts',(0.905913718999365,7.86039491587526,-52.1731863518083));
#63663=CARTESIAN_POINT('Ctrl Pts',(0.756488696690766,7.87618022622692,-52.1678032308911));
#63664=CARTESIAN_POINT('Ctrl Pts',(0.0764748867062996,7.92848507510148,
-52.1437663093828));
#63665=CARTESIAN_POINT('Ctrl Pts',(-0.456480890272077,7.91570058333451,
-52.126304291775));
#63666=CARTESIAN_POINT('Ctrl Pts',(-1.31263247889229,7.80836343996087,-52.0961333439424));
#63667=CARTESIAN_POINT('Ctrl Pts',(-1.6382144281175,7.74659630279577,-52.0841136890893));
#63668=CARTESIAN_POINT('Ctrl Pts',(-1.97184319933447,7.66132710062903,-52.0703347168536));
#63669=CARTESIAN_POINT('Ctrl Pts',(-1.98474433396213,7.65799506876364,-52.0697995648192));
#63670=CARTESIAN_POINT('Ctrl Pts',(-2.00328121652762,7.65315747865286,-52.0690272416492));
#63671=CARTESIAN_POINT('Ctrl Pts',(-2.00892368045347,7.65167829115342,-52.0687917033403));
#63672=CARTESIAN_POINT('Ctrl Pts',(-2.01873496751384,7.64909463465776,-52.0683813656391));
#63673=CARTESIAN_POINT('Ctrl Pts',(-2.02290453985602,7.64799299303434,-52.0682067373896));
#63674=CARTESIAN_POINT('Ctrl Pts',(-2.03093525397468,7.64586417337647,-52.0678699308539));
#63675=CARTESIAN_POINT('Ctrl Pts',(-2.03479652357463,7.64483747839677,-52.0677077816061));
#63676=CARTESIAN_POINT('Ctrl Pts',(-2.04391325595666,7.64240598211994,-52.0673244462228));
#63677=CARTESIAN_POINT('Ctrl Pts',(-2.04916804469141,7.64099868588791,-52.0671031114254));
#63678=CARTESIAN_POINT('Ctrl Pts',(-2.06743480624309,7.63608642685687,-52.0663323780964));
#63679=CARTESIAN_POINT('Ctrl Pts',(-2.08043920847536,7.63255365471261,-52.0657813388633));
#63680=CARTESIAN_POINT('Ctrl Pts',(-2.23229172628981,7.59088452323878,-52.0593199823909));
#63681=CARTESIAN_POINT('Ctrl Pts',(-2.37007545257036,7.54899940413262,-52.0531947498979));
#63682=CARTESIAN_POINT('Ctrl Pts',(-2.60168303749548,7.47162696093144,-52.0425393809127));
#63683=CARTESIAN_POINT('Ctrl Pts',(-2.69611990071184,7.4380710128333,-52.0380911567544));
#63684=CARTESIAN_POINT('Ctrl Pts',(-3.45070691149286,7.15368739651151,-52.0018452066305));
#63685=CARTESIAN_POINT('Ctrl Pts',(-4.07522237928604,6.81728234884755,-51.9678085769398));
#63686=CARTESIAN_POINT('Ctrl Pts',(-4.86606314810196,6.24329487968668,-51.9241099679494));
#63687=CARTESIAN_POINT('Ctrl Pts',(-5.07698861820723,6.07301462714687,-51.9123412604108));
#63688=CARTESIAN_POINT('Ctrl Pts',(-5.36790319137211,5.81238811973075,-51.8959905922589));
#63689=CARTESIAN_POINT('Ctrl Pts',(-5.45520950872661,5.73052625856688,-51.8910653468149));
#63690=CARTESIAN_POINT('Ctrl Pts',(-5.55393232665606,5.63365814943078,-51.8854702522365));
#63691=CARTESIAN_POINT('Ctrl Pts',(-5.56719075829702,5.62055651164667,-51.8847182716075));
#63692=CARTESIAN_POINT('Ctrl Pts',(-5.58724444294296,5.60059940547699,-51.8835799927851));
#63693=CARTESIAN_POINT('Ctrl Pts',(-5.59407361410657,5.59377820141565,-51.8831922002885));
#63694=CARTESIAN_POINT('Ctrl Pts',(-5.60635820195487,5.58146294950753,-51.8824943321489));
#63695=CARTESIAN_POINT('Ctrl Pts',(-5.61181806386953,5.57597336469755,-51.8821840617384));
#63696=CARTESIAN_POINT('Ctrl Pts',(-5.62354035283546,5.56415260406781,-51.8815176846796));
#63697=CARTESIAN_POINT('Ctrl Pts',(-5.62980016955799,5.55781884850796,-51.8811616920667));
#63698=CARTESIAN_POINT('Ctrl Pts',(-5.64671302372387,5.54064833293842,-51.8801994769993));
#63699=CARTESIAN_POINT('Ctrl Pts',(-5.65734557731959,5.52979140145784,-51.8795941442827));
#63700=CARTESIAN_POINT('Ctrl Pts',(-5.70475215607721,5.48110456544492,-51.8768932397982));
#63701=CARTESIAN_POINT('Ctrl Pts',(-5.74117887027941,5.44293760141292,-51.8748126271556));
#63702=CARTESIAN_POINT('Ctrl Pts',(-6.33560021263209,4.80751123021564,-51.8407604969326));
#63703=CARTESIAN_POINT('Ctrl Pts',(-6.79806115087063,4.12775191221742,-51.8134309984279));
#63704=CARTESIAN_POINT('Ctrl Pts',(-7.23260456860779,3.21125255831868,-51.777802732156));
#63705=CARTESIAN_POINT('Ctrl Pts',(-7.31030530489373,3.03020515981736,-51.7707841542783));
#63706=CARTESIAN_POINT('Ctrl Pts',(-7.44795201078235,2.67327214306416,-51.7566918276523));
#63707=CARTESIAN_POINT('Ctrl Pts',(-7.50861251308763,2.49782109226252,-51.7496330668647));
#63708=CARTESIAN_POINT('Ctrl Pts',(-7.57372968107876,2.28557750604726,-51.7408475337281));
#63709=CARTESIAN_POINT('Ctrl Pts',(-7.58416520886395,2.25070741097705,-51.7393975943091));
#63710=CARTESIAN_POINT('Ctrl Pts',(-7.59775409898043,2.20413260282507,-51.7374531962301));
#63711=CARTESIAN_POINT('Ctrl Pts',(-7.60112182798788,2.19249055497184,-51.7369665211825));
#63712=CARTESIAN_POINT('Ctrl Pts',(-7.60662724639801,2.17329348730776,-51.7361630022699));
#63713=CARTESIAN_POINT('Ctrl Pts',(-7.60878047072409,2.16574291998235,-51.7358467036186));
#63714=CARTESIAN_POINT('Ctrl Pts',(-7.61294566986035,2.15105421337129,-51.7352308919514));
#63715=CARTESIAN_POINT('Ctrl Pts',(-7.61495885539926,2.1439164235754,-51.734931420812));
#63716=CARTESIAN_POINT('Ctrl Pts',(-7.61960567029669,2.12735192858325,-51.7342359362108));
#63717=CARTESIAN_POINT('Ctrl Pts',(-7.62223184562949,2.11792315474802,-51.7338396731333));
#63718=CARTESIAN_POINT('Ctrl Pts',(-7.62928334386571,2.09242312355431,-51.7327669858963));
#63719=CARTESIAN_POINT('Ctrl Pts',(-7.63367536873292,2.07634275334951,-51.7320894775174));
#63720=CARTESIAN_POINT('Ctrl Pts',(-7.66635511477985,1.95518823359428,-51.7269773494542));
#63721=CARTESIAN_POINT('Ctrl Pts',(-7.69252247064552,1.84955637934844,-51.7224775718625));
#63722=CARTESIAN_POINT('Ctrl Pts',(-7.84562356914092,1.17192027586025,-51.6934449805958));
#63723=CARTESIAN_POINT('Ctrl Pts',(-7.91085769820133,0.587841411826712,
-51.6678539456649));
#63724=CARTESIAN_POINT('Ctrl Pts',(-7.91115880092942,-0.653968790779282,
-51.6149583235055));
#63725=CARTESIAN_POINT('Ctrl Pts',(-7.82975041299619,-1.30734903275606,
-51.5878788503464));
#63726=CARTESIAN_POINT('Ctrl Pts',(-7.6496804303836,-2.01798571026065,-51.5580644153787));
#63727=CARTESIAN_POINT('Ctrl Pts',(-7.62963011481745,-2.09251558247885,
-51.5549362491295));
#63728=CARTESIAN_POINT('Ctrl Pts',(-7.6005735868381,-2.19454735098087,-51.550652001369));
#63729=CARTESIAN_POINT('Ctrl Pts',(-7.59250239519923,-2.22231057938892,
-51.5494860538214));
#63730=CARTESIAN_POINT('Ctrl Pts',(-7.57839448709955,-2.2698647724461,-51.5474886053196));
#63731=CARTESIAN_POINT('Ctrl Pts',(-7.5724320021874,-2.28967741449144,-51.5466562954138));
#63732=CARTESIAN_POINT('Ctrl Pts',(-7.55999145597246,-2.33043576655436,
-51.5449438326371));
#63733=CARTESIAN_POINT('Ctrl Pts',(-7.55350390798825,-2.35137840253406,
-51.5440637943952));
#63734=CARTESIAN_POINT('Ctrl Pts',(-7.5382003007495,-2.40006345208207,-51.5420176321078));
#63735=CARTESIAN_POINT('Ctrl Pts',(-7.52931800349152,-2.42778474308957,
-51.5408522814545));
#63736=CARTESIAN_POINT('Ctrl Pts',(-7.50026087280275,-2.51677750164869,
-51.5371101786234));
#63737=CARTESIAN_POINT('Ctrl Pts',(-7.47948948210573,-2.57785168889583,
-51.5345405042055));
#63738=CARTESIAN_POINT('Ctrl Pts',(-7.37101298124165,-2.88445171254307,
-51.5216288181685));
#63739=CARTESIAN_POINT('Ctrl Pts',(-7.27195434326239,-3.12579253703037,
-51.5114336306219));
#63740=CARTESIAN_POINT('Ctrl Pts',(-7.01490772950438,-3.6733409917938,-51.4879998169136));
#63741=CARTESIAN_POINT('Ctrl Pts',(-6.84848470130402,-3.97499954234526,
-51.4748631892665));
#63742=CARTESIAN_POINT('Ctrl Pts',(-6.52197142381995,-4.48510793736571,
-51.4514962852165));
#63743=CARTESIAN_POINT('Ctrl Pts',(-6.37016410401951,-4.69822368477,-51.4413349417497));
#63744=CARTESIAN_POINT('Ctrl Pts',(-6.19175974097778,-4.92409649654297,
-51.4298292383923));
#63745=CARTESIAN_POINT('Ctrl Pts',(-6.1753281031961,-4.94468783739816,-51.4287732418327));
#63746=CARTESIAN_POINT('Ctrl Pts',(-6.15047299402803,-4.97551793445031,
-51.4271810477261));
#63747=CARTESIAN_POINT('Ctrl Pts',(-6.14212613181137,-4.98581822227533,
-51.4266472283091));
#63748=CARTESIAN_POINT('Ctrl Pts',(-6.12684693887751,-5.00457662380944,
-51.4256716831409));
#63749=CARTESIAN_POINT('Ctrl Pts',(-6.11992287945425,-5.01304144653195,
-51.4252302012787));
#63750=CARTESIAN_POINT('Ctrl Pts',(-6.10489343052953,-5.03133775023564,
-51.4242732490831));
#63751=CARTESIAN_POINT('Ctrl Pts',(-6.0967817992794,-5.04116405661127,-51.4237576010309));
#63752=CARTESIAN_POINT('Ctrl Pts',(-6.07426441811411,-5.06830742799209,
-51.4223285501622));
#63753=CARTESIAN_POINT('Ctrl Pts',(-6.0598084250752,-5.08558258707628,-51.4214137625465));
#63754=CARTESIAN_POINT('Ctrl Pts',(-5.97859906784162,-5.18179126208211,
-51.41629010409));
#63755=CARTESIAN_POINT('Ctrl Pts',(-5.91037810030055,-5.25947123228704,
-51.41204351051));
#63756=CARTESIAN_POINT('Ctrl Pts',(-5.59255185305285,-5.60736972679043,
-51.3925595134165));
#63757=CARTESIAN_POINT('Ctrl Pts',(-5.32581065192357,-5.86131114711035,
-51.3770407265267));
#63758=CARTESIAN_POINT('Ctrl Pts',(-4.70553156696177,-6.3744013776366,-51.3432766963854));
#63759=CARTESIAN_POINT('Ctrl Pts',(-4.34616362434512,-6.62464381515314,
-51.3251420144015));
#63760=CARTESIAN_POINT('Ctrl Pts',(-3.92260981431283,-6.87021111458166,
-51.3052716912954));
#63761=CARTESIAN_POINT('Ctrl Pts',(-3.87700297907093,-6.8960507872474,-51.3031498256281));
#63762=CARTESIAN_POINT('Ctrl Pts',(-3.80216552578969,-6.93747470193981,
-51.2996959001553));
#63763=CARTESIAN_POINT('Ctrl Pts',(-3.77308801813951,-6.95333191672927,
-51.2983606902068));
#63764=CARTESIAN_POINT('Ctrl Pts',(-3.72082538975083,-6.98140861285222,
-51.2959726885243));
#63765=CARTESIAN_POINT('Ctrl Pts',(-3.69767753350805,-6.99369635202022,
-51.2949191349702));
#63766=CARTESIAN_POINT('Ctrl Pts',(-3.64832019010333,-7.01958350917208,
-51.2926812591103));
#63767=CARTESIAN_POINT('Ctrl Pts',(-3.62209474538898,-7.0331516772173,-51.2914972974356));
#63768=CARTESIAN_POINT('Ctrl Pts',(-3.55097434433926,-7.06944368949022,
-51.2882999583313));
#63769=CARTESIAN_POINT('Ctrl Pts',(-3.50593745475715,-7.09188659467569,
-51.2862896332745));
#63770=CARTESIAN_POINT('Ctrl Pts',(-3.26474904857026,-7.2092172209269,-51.2755962495039));
#63771=CARTESIAN_POINT('Ctrl Pts',(-3.06495174181175,-7.29640128959952,
-51.2669867264147));
#63772=CARTESIAN_POINT('Ctrl Pts',(-2.59334614902039,-7.47939846638989,
-51.2471211487817));
#63773=CARTESIAN_POINT('Ctrl Pts',(-2.31938973368994,-7.56883640588344,
-51.2359588529723));
#63774=CARTESIAN_POINT('Ctrl Pts',(-1.28385742608788,-7.84538349478491,
-51.1950867690578));
#63775=CARTESIAN_POINT('Ctrl Pts',(-0.50079728503031,-7.9339326311962,-51.1673286297828));
#63776=CARTESIAN_POINT('Ctrl Pts',(0.350595666864294,-7.90352210794903,
-51.1339748743647));
#63777=CARTESIAN_POINT('Ctrl Pts',(0.418766487416467,-7.90020337423685,
-51.1312774087229));
#63778=CARTESIAN_POINT('Ctrl Pts',(0.50028633030346,-7.89517668427529,-51.1280118677253));
#63779=CARTESIAN_POINT('Ctrl Pts',(0.513685846673798,-7.89431619182426,
-51.1274738154278));
#63780=CARTESIAN_POINT('Ctrl Pts',(0.535509064584842,-7.89285894691583,
-51.1265953265743));
#63781=CARTESIAN_POINT('Ctrl Pts',(0.543934145133511,-7.89228281039404,
-51.1262556458331));
#63782=CARTESIAN_POINT('Ctrl Pts',(0.558954867062194,-7.89123147454816,
-51.1256490738963));
#63783=CARTESIAN_POINT('Ctrl Pts',(0.565550873262386,-7.89076149289352,
-51.1253823782969));
#63784=CARTESIAN_POINT('Ctrl Pts',(0.579452283226118,-7.88975346319276,
-51.1248195884137));
#63785=CARTESIAN_POINT('Ctrl Pts',(0.586757541634805,-7.88921353782308,
-51.1245234228963));
#63786=CARTESIAN_POINT('Ctrl Pts',(0.606045453088392,-7.88776104643983,
-51.1237403412208));
#63787=CARTESIAN_POINT('Ctrl Pts',(0.618026767350007,-7.8868313237754,-51.1232527603647));
#63788=CARTESIAN_POINT('Ctrl Pts',(0.672205628635941,-7.88250295136452,
-51.1210426027769));
#63789=CARTESIAN_POINT('Ctrl Pts',(0.714377071824375,-7.87879295867929,
-51.1193076118357));
#63790=CARTESIAN_POINT('Ctrl Pts',(1.02485158869387,-7.84896609050352,-51.1064140820309));
#63791=CARTESIAN_POINT('Ctrl Pts',(1.29165694320329,-7.80949245402892,-51.0946222498107));
#63792=CARTESIAN_POINT('Ctrl Pts',(1.80780471731166,-7.70595724358861,-51.0709642130253));
#63793=CARTESIAN_POINT('Ctrl Pts',(2.05710147070141,-7.64318405877536,-51.0591459303334));
#63794=CARTESIAN_POINT('Ctrl Pts',(2.62007621950843,-7.47188328610893,-51.0320449107439));
#63795=CARTESIAN_POINT('Ctrl Pts',(2.93088805981931,-7.35552511223655,-51.0167873922339));
#63796=CARTESIAN_POINT('Ctrl Pts',(3.61514140498033,-7.04908125357026,-50.983205550084));
#63797=CARTESIAN_POINT('Ctrl Pts',(3.98266857793027,-6.84815377889291,-50.9651943943171));
#63798=CARTESIAN_POINT('Ctrl Pts',(4.35605752954808,-6.603746543205,-50.9470512397213));
#63799=CARTESIAN_POINT('Ctrl Pts',(4.37941254673051,-6.5882813671881,-50.9459168771084));
#63800=CARTESIAN_POINT('Ctrl Pts',(4.41165501386604,-6.56668391198242,-50.9443514196605));
#63801=CARTESIAN_POINT('Ctrl Pts',(4.42061265601532,-6.56065707897303,-50.943916563782));
#63802=CARTESIAN_POINT('Ctrl Pts',(4.43598542116435,-6.55026827868145,-50.943170379889));
#63803=CARTESIAN_POINT('Ctrl Pts',(4.44240650607878,-6.54591518541474,-50.9428587345088));
#63804=CARTESIAN_POINT('Ctrl Pts',(4.45561412152811,-6.53693286536937,-50.9422177654212));
#63805=CARTESIAN_POINT('Ctrl Pts',(4.46239986687624,-6.53230249719979,-50.9418884832708));
#63806=CARTESIAN_POINT('Ctrl Pts',(4.47812364828313,-6.52153717433555,-50.9411255475665));
#63807=CARTESIAN_POINT('Ctrl Pts',(4.48705631977775,-6.51539439403655,-50.940692176628));
#63808=CARTESIAN_POINT('Ctrl Pts',(4.51526295771662,-6.49591185710497,-50.9393238758649));
#63809=CARTESIAN_POINT('Ctrl Pts',(4.53449035493805,-6.48250473698929,-50.9383913821458));
#63810=CARTESIAN_POINT('Ctrl Pts',(4.8412070250609,-6.26660117227177,-50.9235190035972));
#63811=CARTESIAN_POINT('Ctrl Pts',(5.11495265432941,-6.0452349940009,-50.9103086314897));
#63812=CARTESIAN_POINT('Ctrl Pts',(6.00115951643161,-5.22515986270115,-50.8666751865921));
#63813=CARTESIAN_POINT('Ctrl Pts',(6.53068747688535,-4.5459855468661,-50.8394422880699));
#63814=CARTESIAN_POINT('Ctrl Pts',(6.9901067209013,-3.70577236652726,-50.8028310642281));
#63815=CARTESIAN_POINT('Ctrl Pts',(7.03733979483702,-3.6152716995536,-50.7988462732997));
#63816=CARTESIAN_POINT('Ctrl Pts',(7.08923850508311,-3.51095809404536,-50.7941875172756));
#63817=CARTESIAN_POINT('Ctrl Pts',(7.09563227369168,-3.49801828933242,-50.7936085765508));
#63818=CARTESIAN_POINT('Ctrl Pts',(7.10511799575358,-3.47868792290354,-50.7927422542781));
#63819=CARTESIAN_POINT('Ctrl Pts',(7.10823684082791,-3.47231052942442,-50.7924562042512));
#63820=CARTESIAN_POINT('Ctrl Pts',(7.11378826614767,-3.46092018855829,-50.7919448941995));
#63821=CARTESIAN_POINT('Ctrl Pts',(7.11622414549413,-3.45590884688926,-50.7917197945082));
#63822=CARTESIAN_POINT('Ctrl Pts',(7.1213525220973,-3.44532981075189,-50.7912443127918));
#63823=CARTESIAN_POINT('Ctrl Pts',(7.12404378802492,-3.43976152586636,-50.7909938721382));
#63824=CARTESIAN_POINT('Ctrl Pts',(7.13114405624069,-3.42502684826846,-50.7903307220744));
#63825=CARTESIAN_POINT('Ctrl Pts',(7.13554190529191,-3.41585511675836,-50.7899174893364));
#63826=CARTESIAN_POINT('Ctrl Pts',(7.15544462876395,-3.37414174649278,-50.7880361381745));
#63827=CARTESIAN_POINT('Ctrl Pts',(7.17074451252823,-3.34150317067397,-50.78655868445));
#63828=CARTESIAN_POINT('Ctrl Pts',(7.29108978723452,-3.08014267467658,-50.7746912762179));
#63829=CARTESIAN_POINT('Ctrl Pts',(7.38538420009903,-2.84663972505008,-50.7638726948913));
#63830=CARTESIAN_POINT('Ctrl Pts',(7.62286631188374,-2.1668498815343,-50.7324654800523));
#63831=CARTESIAN_POINT('Ctrl Pts',(7.73777630141721,-1.71177553406259,-50.7116101036829));
#63832=CARTESIAN_POINT('Ctrl Pts',(7.87134101354573,-0.8765501012583,-50.6751467221012));
#63833=CARTESIAN_POINT('Ctrl Pts',(7.90419477168064,-0.500086066636779,
-50.6593350359073));
#63834=CARTESIAN_POINT('Ctrl Pts',(7.91065019298988,-0.0839022222059317,
-50.6424664431928));
#63835=CARTESIAN_POINT('Ctrl Pts',(7.91096652669874,-0.0451076997346217,
-50.6408994828876));
#63836=CARTESIAN_POINT('Ctrl Pts',(7.91101205126465,0.0119475677737271,
-50.6386024496337));
#63837=CARTESIAN_POINT('Ctrl Pts',(7.91096340131129,0.0302073834516963,
-50.637868442496));
#63838=CARTESIAN_POINT('Ctrl Pts',(7.91076565430058,0.0624839856616776,
-50.6365729156257));
#63839=CARTESIAN_POINT('Ctrl Pts',(7.91064252193986,0.0765008317092797,
-50.6360109458787));
#63840=CARTESIAN_POINT('Ctrl Pts',(7.91031238700873,0.105351961879948,-50.6348555163186));
#63841=CARTESIAN_POINT('Ctrl Pts',(7.91010090888753,0.120186142443491,-50.6342621355591));
#63842=CARTESIAN_POINT('Ctrl Pts',(7.90945614677868,0.157958195428076,-50.6327529375033));
#63843=CARTESIAN_POINT('Ctrl Pts',(7.90896480859124,0.180894974566873,-50.6318381032264));
#63844=CARTESIAN_POINT('Ctrl Pts',(7.90666199048649,0.270241996525144,-50.6282804268825));
#63845=CARTESIAN_POINT('Ctrl Pts',(7.90411374765819,0.336631249599331,-50.6256494706157));
#63846=CARTESIAN_POINT('Ctrl Pts',(7.88373632351083,0.736145225041601,-50.6098890953637));
#63847=CARTESIAN_POINT('Ctrl Pts',(7.84568628200952,1.06790943464732,-50.5971220975674));
#63848=CARTESIAN_POINT('Ctrl Pts',(7.65787819692602,2.11527191240606,-50.5572287282404));
#63849=CARTESIAN_POINT('Ctrl Pts',(7.43001352765958,2.81286287181111,-50.5315422631011));
#63850=CARTESIAN_POINT('Ctrl Pts',(7.0783016175668,3.53365356080735,-50.5001301446837));
#63851=CARTESIAN_POINT('Ctrl Pts',(7.04598689262584,3.59765612791403,-50.497292467389));
#63852=CARTESIAN_POINT('Ctrl Pts',(7.00663198479293,3.67303788120783,-50.4938843704703));
#63853=CARTESIAN_POINT('Ctrl Pts',(7.00042675450575,3.68485064815832,-50.4933483627922));
#63854=CARTESIAN_POINT('Ctrl Pts',(6.9903300437204,3.70395399206473,-50.4924783275316));
#63855=CARTESIAN_POINT('Ctrl Pts',(6.98645695910169,3.71125429651992,-50.4921450825857));
#63856=CARTESIAN_POINT('Ctrl Pts',(6.97956877002564,3.72418871952677,-50.4915532785027));
#63857=CARTESIAN_POINT('Ctrl Pts',(6.97655826112576,3.72982528585153,-50.4912949188243));
#63858=CARTESIAN_POINT('Ctrl Pts',(6.97023740806948,3.74162537175719,-50.4907530647431));
#63859=CARTESIAN_POINT('Ctrl Pts',(6.96692571159675,3.74778815784844,-50.4904695109031));
#63860=CARTESIAN_POINT('Ctrl Pts',(6.95824751850061,3.76388628704237,-50.4897273390218));
#63861=CARTESIAN_POINT('Ctrl Pts',(6.95286792860482,3.77381452592923,-50.4892681351879));
#63862=CARTESIAN_POINT('Ctrl Pts',(6.92929962532464,3.81708927362661,-50.4872599839791));
#63863=CARTESIAN_POINT('Ctrl Pts',(6.91089233878381,3.85031567933861,-50.4857010032407));
#63864=CARTESIAN_POINT('Ctrl Pts',(6.62758785284108,4.35312262233801,-50.4618323809549));
#63865=CARTESIAN_POINT('Ctrl Pts',(6.31565441203594,4.79446475130553,-50.4369048889312));
#63866=CARTESIAN_POINT('Ctrl Pts',(5.53213177991521,5.69260531977242,-50.3820704303982));
#63867=CARTESIAN_POINT('Ctrl Pts',(5.04357587745989,6.1296689204548,-50.352628476872));
#63868=CARTESIAN_POINT('Ctrl Pts',(4.47382734249726,6.52459952005059,-50.324341785341));
#63869=CARTESIAN_POINT('Ctrl Pts',(4.44068703382505,6.54720006711995,-50.3227148465226));
#63870=CARTESIAN_POINT('Ctrl Pts',(4.39634303016149,6.57694955673791,-50.3205621157626));
#63871=CARTESIAN_POINT('Ctrl Pts',(4.38529146731117,6.58432352332115,-50.3200275904864));
#63872=CARTESIAN_POINT('Ctrl Pts',(4.3680389154279,6.59577228893435,-50.3191962263211));
#63873=CARTESIAN_POINT('Ctrl Pts',(4.36185070641929,6.59986624633198,-50.3188986451421));
#63874=CARTESIAN_POINT('Ctrl Pts',(4.34948272019712,6.60802359008308,-50.3183051143201));
#63875=CARTESIAN_POINT('Ctrl Pts',(4.34330298615006,6.61208702841166,-50.3180091628021));
#63876=CARTESIAN_POINT('Ctrl Pts',(4.32952667154837,6.62111789528892,-50.3173507599687));
#63877=CARTESIAN_POINT('Ctrl Pts',(4.32192721663954,6.62608093202653,-50.3169884786351));
#63878=CARTESIAN_POINT('Ctrl Pts',(4.29982316844608,6.64046239420716,-50.3159373826134));
#63879=CARTESIAN_POINT('Ctrl Pts',(4.28529616837165,6.64984637741067,-50.3152498977376));
#63880=CARTESIAN_POINT('Ctrl Pts',(4.25246038938186,6.67090497130716,-50.3137033619748));
#63881=CARTESIAN_POINT('Ctrl Pts',(4.23413404784577,6.6825520105902,-50.3128453725298));
#63882=CARTESIAN_POINT('Ctrl Pts',(4.17605096460324,6.7191310088871,-50.3101422526924));
#63883=CARTESIAN_POINT('Ctrl Pts',(4.13611989101968,6.74378495497205,-50.3083077447178));
#63884=CARTESIAN_POINT('Ctrl Pts',(3.96935566372673,6.84470888815572,-50.3007429622345));
#63885=CARTESIAN_POINT('Ctrl Pts',(3.84061113646125,6.91776937268805,-50.2951338091314));
#63886=CARTESIAN_POINT('Ctrl Pts',(3.4628219752736,7.11835902720264,-50.2792727371081));
#63887=CARTESIAN_POINT('Ctrl Pts',(3.20896340045187,7.23634842036956,-50.2693503883374));
#63888=CARTESIAN_POINT('Ctrl Pts',(2.18649523964833,7.64716282654438,-50.2313021393824));
#63889=CARTESIAN_POINT('Ctrl Pts',(1.3806450503099,7.83282971056397,-50.2058365755785));
#63890=CARTESIAN_POINT('Ctrl Pts',(0.515590293249944,7.89431093915223,-50.1718655069737));
#63891=CARTESIAN_POINT('Ctrl Pts',(0.470318198440033,7.89713740469457,-50.1700676385573));
#63892=CARTESIAN_POINT('Ctrl Pts',(0.416543549603061,7.9000306719362,-50.1679058752051));
#63893=CARTESIAN_POINT('Ctrl Pts',(0.408061223877586,7.90047335181657,-50.1675641075957));
#63894=CARTESIAN_POINT('Ctrl Pts',(0.394386074585608,7.90116495535142,-50.1670118414062));
#63895=CARTESIAN_POINT('Ctrl Pts',(0.389193672276127,7.90142242337732,-50.1668018527531));
#63896=CARTESIAN_POINT('Ctrl Pts',(0.379944842484468,7.90187189267213,-50.1664272844804));
#63897=CARTESIAN_POINT('Ctrl Pts',(0.375888509097299,7.90206588938216,-50.1662628249936));
#63898=CARTESIAN_POINT('Ctrl Pts',(0.367418333469839,7.90246444421802,-50.1659190279133));
#63899=CARTESIAN_POINT('Ctrl Pts',(0.363004467074932,7.90266842785537,-50.1657396555847));
#63900=CARTESIAN_POINT('Ctrl Pts',(0.351434551364988,7.90319340952089,-50.1652688984083));
#63901=CARTESIAN_POINT('Ctrl Pts',(0.344278247815564,7.90350838549429,-50.1649771462506));
#63902=CARTESIAN_POINT('Ctrl Pts',(0.312250244393492,7.9048744766831,-50.1636688665219));
#63903=CARTESIAN_POINT('Ctrl Pts',(0.287374350005182,7.90581789962738,-50.1626458703736));
#63904=CARTESIAN_POINT('Ctrl Pts',(0.103012979485181,7.91193856015273,-50.1550156939559));
#63905=CARTESIAN_POINT('Ctrl Pts',(-0.0565832717197611,7.91240643719036,
-50.1481420524796));
#63906=CARTESIAN_POINT('Ctrl Pts',(-0.474797623077827,7.90097943838766,
-50.1296390512189));
#63907=CARTESIAN_POINT('Ctrl Pts',(-0.733007093242634,7.8812179796775,-50.117726170947));
#63908=CARTESIAN_POINT('Ctrl Pts',(-1.06788231419738,7.83898890330095,-50.1020280120369));
#63909=CARTESIAN_POINT('Ctrl Pts',(-1.14584356729661,7.82797305084484,-50.0983551795533));
#63910=CARTESIAN_POINT('Ctrl Pts',(-1.46745850095647,7.77762158786638,-50.0831574566117));
#63911=CARTESIAN_POINT('Ctrl Pts',(-1.7093753562552,7.72805751626557,-50.0716215927051));
#63912=CARTESIAN_POINT('Ctrl Pts',(-2.12067099191058,7.62352953502085,-50.0521205553961));
#63913=CARTESIAN_POINT('Ctrl Pts',(-2.29124305111174,7.57401199007608,-50.0440656354579));
#63914=CARTESIAN_POINT('Ctrl Pts',(-2.78182531772033,7.41350256084451,-50.0211054739684));
#63915=CARTESIAN_POINT('Ctrl Pts',(-3.09656993286252,7.28765168696647,-50.0066540517767));
#63916=CARTESIAN_POINT('Ctrl Pts',(-3.42453938820976,7.13141340801815,-49.9919468024326));
#63917=CARTESIAN_POINT('Ctrl Pts',(-3.44671809519011,7.12072058187303,-49.9909538876192));
#63918=CARTESIAN_POINT('Ctrl Pts',(-3.4781623918426,7.10537928727822,-49.9895484531765));
#63919=CARTESIAN_POINT('Ctrl Pts',(-3.4874692029791,7.10081593899745,-49.9891327620558));
#63920=CARTESIAN_POINT('Ctrl Pts',(-3.50333300515518,7.0929988323063,-49.9884246834869));
#63921=CARTESIAN_POINT('Ctrl Pts',(-3.50989448543127,7.08975424691479,-49.9881319538266));
#63922=CARTESIAN_POINT('Ctrl Pts',(-3.52247300259231,7.08351255614379,-49.9875710520813));
#63923=CARTESIAN_POINT('Ctrl Pts',(-3.52849073919045,7.08051688019976,-49.9873028268835));
#63924=CARTESIAN_POINT('Ctrl Pts',(-3.54099465700996,7.07427243353015,-49.9867457398022));
#63925=CARTESIAN_POINT('Ctrl Pts',(-3.54748020415842,7.0710224031796,-49.9864569254204));
#63926=CARTESIAN_POINT('Ctrl Pts',(-3.5700381493954,7.05967934330331,-49.9854528442587));
#63927=CARTESIAN_POINT('Ctrl Pts',(-3.58608745660496,7.05154036915597,-49.9847393006769));
#63928=CARTESIAN_POINT('Ctrl Pts',(-3.72265105237299,6.98169900387593,-49.9786746377811));
#63929=CARTESIAN_POINT('Ctrl Pts',(-3.84159406186037,6.91696532092125,-49.9734388779074));
#63930=CARTESIAN_POINT('Ctrl Pts',(-4.2567869070942,6.67698514880334,-49.9552771346581));
#63931=CARTESIAN_POINT('Ctrl Pts',(-4.54320870177555,6.48549493197682,-49.9429811493431));
#63932=CARTESIAN_POINT('Ctrl Pts',(-5.3770783347942,5.84556995998697,-49.9065470307282));
#63933=CARTESIAN_POINT('Ctrl Pts',(-5.87758571081711,5.34203741898331,-49.8839677383611));
#63934=CARTESIAN_POINT('Ctrl Pts',(-6.35051900834556,4.71811755601942,-49.8538224746301));
#63935=CARTESIAN_POINT('Ctrl Pts',(-6.39565875514631,4.6567449269159,-49.8508337888967));
#63936=CARTESIAN_POINT('Ctrl Pts',(-6.44637085893052,4.58566764327877,-49.8473335936902));
#63937=CARTESIAN_POINT('Ctrl Pts',(-6.45281876227475,4.57658988809689,-49.8468858344942));
#63938=CARTESIAN_POINT('Ctrl Pts',(-6.46238351516107,4.56306364247085,-49.8462175727975));
#63939=CARTESIAN_POINT('Ctrl Pts',(-6.46551492957519,4.55862558206055,-49.8459981402066));
#63940=CARTESIAN_POINT('Ctrl Pts',(-6.471090095203,4.5507067657032,-49.8456063078174));
#63941=CARTESIAN_POINT('Ctrl Pts',(-6.47353561785015,4.54722725316642,-49.845434034498));
#63942=CARTESIAN_POINT('Ctrl Pts',(-6.478683128316,4.53989075859541,-49.8450705852104));
#63943=CARTESIAN_POINT('Ctrl Pts',(-6.48138447942148,4.5360333339643,-49.8448793643845));
#63944=CARTESIAN_POINT('Ctrl Pts',(-6.48850361921426,4.5258481350072,-49.8443741392364));
#63945=CARTESIAN_POINT('Ctrl Pts',(-6.49291558631341,4.51951631769417,-49.8440597282011));
#63946=CARTESIAN_POINT('Ctrl Pts',(-6.51273126346036,4.49098902297851,-49.8426417448845));
#63947=CARTESIAN_POINT('Ctrl Pts',(-6.52803031447734,4.46872141601819,-49.8415309910108));
#63948=CARTESIAN_POINT('Ctrl Pts',(-6.64140116739109,4.30188671240078,-49.8331824512981));
#63949=CARTESIAN_POINT('Ctrl Pts',(-6.73476871017237,4.15419325531452,-49.8256444414951));
#63950=CARTESIAN_POINT('Ctrl Pts',(-7.30785402088005,3.17749382740418,-49.7754643099273));
#63951=CARTESIAN_POINT('Ctrl Pts',(-7.63858723699549,2.27022401886193,-49.7284877914644));
#63952=CARTESIAN_POINT('Ctrl Pts',(-7.80633479458858,1.28331654043723,-49.6857447098148));
#63953=CARTESIAN_POINT('Ctrl Pts',(-7.813184502083,1.24093202099951,-49.6839219044292));
#63954=CARTESIAN_POINT('Ctrl Pts',(-7.84171190431721,1.05480215838642,-49.6759735533229));
#63955=CARTESIAN_POINT('Ctrl Pts',(-7.8597708115176,0.91052674374437,-49.6699605067032));
#63956=CARTESIAN_POINT('Ctrl Pts',(-7.8757113327133,0.746635079015344,-49.6632905931188));
#63957=CARTESIAN_POINT('Ctrl Pts',(-7.87750810772939,0.727433128841045,
-49.6625116059943));
#63958=CARTESIAN_POINT('Ctrl Pts',(-7.88012320654811,0.698339287697318,
-49.6613350352185));
#63959=CARTESIAN_POINT('Ctrl Pts',(-7.88099315503344,0.688452178677763,
-49.6609358439442));
#63960=CARTESIAN_POINT('Ctrl Pts',(-7.88247453774052,0.671245197680348,
-49.6602422357563));
#63961=CARTESIAN_POINT('Ctrl Pts',(-7.88309438760575,0.663926072716579,
-49.6599475572496));
#63962=CARTESIAN_POINT('Ctrl Pts',(-7.88432197881017,0.649186693958512,
-49.659354836624));
#63963=CARTESIAN_POINT('Ctrl Pts',(-7.88492944083915,0.641766423669323,
-49.6590568034539));
#63964=CARTESIAN_POINT('Ctrl Pts',(-7.88614962268587,0.626598381449461,
-49.658448317774));
#63965=CARTESIAN_POINT('Ctrl Pts',(-7.88676140196441,0.61885054087986,-49.658137894759));
#63966=CARTESIAN_POINT('Ctrl Pts',(-7.88815103450292,0.600914847350158,
-49.6574201896538));
#63967=CARTESIAN_POINT('Ctrl Pts',(-7.88892057080252,0.590726354119546,
-49.6570131656898));
#63968=CARTESIAN_POINT('Ctrl Pts',(-7.89085908622961,0.564381324933235,
-49.655962426544));
#63969=CARTESIAN_POINT('Ctrl Pts',(-7.89199818678615,0.548222602932063,
-49.6553196358621));
#63970=CARTESIAN_POINT('Ctrl Pts',(-7.90502435428461,0.354980115724583,
-49.647652334971));
#63971=CARTESIAN_POINT('Ctrl Pts',(-7.91099882920443,0.177544359459989,
-49.6408130228063));
#63972=CARTESIAN_POINT('Ctrl Pts',(-7.91099999982794,5.21758335036288E-5,
-49.6341351303446));
#63973=CARTESIAN_POINT('',(-7.92228552985236,-0.00797182984248199,-47.642334701651));
#63974=CARTESIAN_POINT('Ctrl Pts',(-7.89680882399629,-0.000256294892049957,
-49.6423315082368));
#63975=CARTESIAN_POINT('Ctrl Pts',(-7.90103566610738,-1.00262630581715,
-49.6020840516645));
#63976=CARTESIAN_POINT('Ctrl Pts',(-7.49007435790851,-3.32159447341453,
-49.508915328115));
#63977=CARTESIAN_POINT('Ctrl Pts',(-5.25514852513718,-6.34001891784867,
-49.3628253375884));
#63978=CARTESIAN_POINT('Ctrl Pts',(-1.58860116256843,-8.09809403774528,
-49.2040615366568));
#63979=CARTESIAN_POINT('Ctrl Pts',(2.4623766104365,-7.85805627968503,-49.0452977357255));
#63980=CARTESIAN_POINT('Ctrl Pts',(7.12803414838975,-5.02805760499318,-48.8336126678165));
#63981=CARTESIAN_POINT('Ctrl Pts',(8.69862114564058,0.679830947526981,-48.621927599908));
#63982=CARTESIAN_POINT('Ctrl Pts',(6.13163661536245,5.48447080059073,-48.4102425319994));
#63983=CARTESIAN_POINT('Ctrl Pts',(1.66597412306723,8.5573936163116,-48.1985574640906));
#63984=CARTESIAN_POINT('Ctrl Pts',(-5.44962191887428,7.46990471586691,-47.9425881873078));
#63985=CARTESIAN_POINT('Ctrl Pts',(-7.90759395183775,2.39848959991299,-47.7395401775023));
#63986=CARTESIAN_POINT('Ctrl Pts',(-7.92228552985236,-0.007971829842482,
-47.642334701651));
#63987=CARTESIAN_POINT('',(-7.91099978972198,-0.00182401173648303,-43.6333998034544));
#63988=CARTESIAN_POINT('Ctrl Pts',(-7.91099573933849,-0.00821049135054118,
-47.6488343437815));
#63989=CARTESIAN_POINT('Ctrl Pts',(-7.91081080808585,-0.186395972497414,
-47.6423568197832));
#63990=CARTESIAN_POINT('Ctrl Pts',(-7.90460580372303,-0.364516329474105,
-47.635666846442));
#63991=CARTESIAN_POINT('Ctrl Pts',(-7.8903646074285,-0.571789395021273,
-47.6274730261266));
#63992=CARTESIAN_POINT('Ctrl Pts',(-7.88817050756462,-0.601300880753049,
-47.6262966852719));
#63993=CARTESIAN_POINT('Ctrl Pts',(-7.8851863919924,-0.638606221840542,
-47.6247965949078));
#63994=CARTESIAN_POINT('Ctrl Pts',(-7.8845502874544,-0.646412490263166,
-47.624481969626));
#63995=CARTESIAN_POINT('Ctrl Pts',(-7.88347754936708,-0.659339931389938,
-47.6239597245305));
#63996=CARTESIAN_POINT('Ctrl Pts',(-7.88304751993685,-0.66446159759016,
-47.6237525038514));
#63997=CARTESIAN_POINT('Ctrl Pts',(-7.88226742940965,-0.673645153490175,
-47.6233803807103));
#63998=CARTESIAN_POINT('Ctrl Pts',(-7.88191921859132,-0.67770720302512,
-47.623215587559));
#63999=CARTESIAN_POINT('Ctrl Pts',(-7.88120989304127,-0.685907337785932,
-47.6228825223307));
#64000=CARTESIAN_POINT('Ctrl Pts',(-7.88084865890561,-0.690045411185815,
-47.6227142432993));
#64001=CARTESIAN_POINT('Ctrl Pts',(-7.88011861584145,-0.698332982660445,
-47.6223768171713));
#64002=CARTESIAN_POINT('Ctrl Pts',(-7.87974978808002,-0.702482477736017,
-47.6222076690253));
#64003=CARTESIAN_POINT('Ctrl Pts',(-7.87872074563448,-0.713956933812933,
-47.6217393726878));
#64004=CARTESIAN_POINT('Ctrl Pts',(-7.87805359497069,-0.721281252424524,
-47.6214398244835));
#64005=CARTESIAN_POINT('Ctrl Pts',(-7.8753969433784,-0.750003887355095,
-47.620262699611));
#64006=CARTESIAN_POINT('Ctrl Pts',(-7.87333048123411,-0.771394816526295,
-47.6193807477432));
#64007=CARTESIAN_POINT('Ctrl Pts',(-7.86512809104895,-0.852833197753838,
-47.6160035217687));
#64008=CARTESIAN_POINT('Ctrl Pts',(-7.85839228578871,-0.912816892416241,
-47.6134755989487));
#64009=CARTESIAN_POINT('Ctrl Pts',(-7.83628256849354,-1.09126848847356,
-47.6058461731687));
#64010=CARTESIAN_POINT('Ctrl Pts',(-7.81891140243297,-1.20946830906336,
-47.6006494970985));
#64011=CARTESIAN_POINT('Ctrl Pts',(-7.79426482707434,-1.3542934530718,-47.5941418230878));
#64012=CARTESIAN_POINT('Ctrl Pts',(-7.78951731860821,-1.38133807281919,
-47.5929205191432));
#64013=CARTESIAN_POINT('Ctrl Pts',(-7.63534153071512,-2.23353758484971,
-47.5542556795445));
#64014=CARTESIAN_POINT('Ctrl Pts',(-7.35580726828862,-3.02978797298011,
-47.5134615717166));
#64015=CARTESIAN_POINT('Ctrl Pts',(-6.86664322150951,-3.93301634601935,
-47.4685807219584));
#64016=CARTESIAN_POINT('Ctrl Pts',(-6.77104338455511,-4.09541018667361,
-47.4605383077332));
#64017=CARTESIAN_POINT('Ctrl Pts',(-6.61702076499226,-4.33688426368195,
-47.4486262081206));
#64018=CARTESIAN_POINT('Ctrl Pts',(-6.56277672367486,-4.41853952181064,
-47.4446061716372));
#64019=CARTESIAN_POINT('Ctrl Pts',(-6.49697339058278,-4.51370915209901,
-47.4399277741486));
#64020=CARTESIAN_POINT('Ctrl Pts',(-6.48687016831328,-4.52821697496735,
-47.4392147809419));
#64021=CARTESIAN_POINT('Ctrl Pts',(-6.47129255251722,-4.55042668129623,
-47.4381235369378));
#64022=CARTESIAN_POINT('Ctrl Pts',(-6.46585288223967,-4.55815278244807,
-47.4377439741418));
#64023=CARTESIAN_POINT('Ctrl Pts',(-6.45633306360225,-4.57162268894201,
-47.4370823130549));
#64024=CARTESIAN_POINT('Ctrl Pts',(-6.45225906547943,-4.57737081636275,
-47.4367999821844));
#64025=CARTESIAN_POINT('Ctrl Pts',(-6.44306803429431,-4.59030206919125,
-47.4361648916574));
#64026=CARTESIAN_POINT('Ctrl Pts',(-6.43794665357822,-4.59748210081245,
-47.4358122975664));
#64027=CARTESIAN_POINT('Ctrl Pts',(-6.42419174187811,-4.61669804771272,
-47.4348687419172));
#64028=CARTESIAN_POINT('Ctrl Pts',(-6.41553637799922,-4.62871833078726,
-47.4342786114712));
#64029=CARTESIAN_POINT('Ctrl Pts',(-6.37787985757637,-4.68070592600241,
-47.4317266687814));
#64030=CARTESIAN_POINT('Ctrl Pts',(-6.34853831978792,-4.72042590827255,
-47.4297778602427));
#64031=CARTESIAN_POINT('Ctrl Pts',(-5.78363054813279,-5.47035288388846,
-47.3929902536307));
#64032=CARTESIAN_POINT('Ctrl Pts',(-5.13253035028886,-6.08540461357812,
-47.3638063292011));
#64033=CARTESIAN_POINT('Ctrl Pts',(-4.12004779212685,-6.76141255821326,
-47.3205103034668));
#64034=CARTESIAN_POINT('Ctrl Pts',(-3.83621882830373,-6.92639346719417,
-47.3084042144463));
#64035=CARTESIAN_POINT('Ctrl Pts',(-3.5191600522768,-7.08520584512437,-47.29430595933));
#64036=CARTESIAN_POINT('Ctrl Pts',(-3.49530382824877,-7.09700503516655,
-47.2932428822244));
#64037=CARTESIAN_POINT('Ctrl Pts',(-3.46176248589624,-7.11338430371735,
-47.2917453936115));
#64038=CARTESIAN_POINT('Ctrl Pts',(-3.45212676686707,-7.11806550583347,
-47.2913148711693));
#64039=CARTESIAN_POINT('Ctrl Pts',(-3.4363443899559,-7.12569327834722,-47.2906092133009));
#64040=CARTESIAN_POINT('Ctrl Pts',(-3.43020336326552,-7.12865150991296,
-47.2903345126682));
#64041=CARTESIAN_POINT('Ctrl Pts',(-3.41744693800903,-7.13477618540431,
-47.2897636427108));
#64042=CARTESIAN_POINT('Ctrl Pts',(-3.41083094528969,-7.13794137354602,
-47.2894674278895));
#64043=CARTESIAN_POINT('Ctrl Pts',(-3.39516850316283,-7.14540776819984,
-47.2887658653787));
#64044=CARTESIAN_POINT('Ctrl Pts',(-3.38611827691685,-7.14970099741707,
-47.2883602333194));
#64045=CARTESIAN_POINT('Ctrl Pts',(-3.35692769239853,-7.16348051522755,
-47.2870511537397));
#64046=CARTESIAN_POINT('Ctrl Pts',(-3.33675551858699,-7.17289894135313,
-47.2861453579588));
#64047=CARTESIAN_POINT('Ctrl Pts',(-3.03983713260541,-7.31000713769421,
-47.2727980296533));
#64048=CARTESIAN_POINT('Ctrl Pts',(-2.7559863766488,-7.42168037881745,-47.2598626832925));
#64049=CARTESIAN_POINT('Ctrl Pts',(-2.16861771682077,-7.61441065150595,
-47.2333759346065));
#64050=CARTESIAN_POINT('Ctrl Pts',(-1.86527609733113,-7.69434205688113,
-47.2198429762008));
#64051=CARTESIAN_POINT('Ctrl Pts',(-0.923671471035601,-7.88348589578352,
-47.1787512640205));
#64052=CARTESIAN_POINT('Ctrl Pts',(-0.276099562582266,-7.93261210645452,
-47.1519016549248));
#64053=CARTESIAN_POINT('Ctrl Pts',(0.464415530699387,-7.89791944996969,
-47.1215697064018));
#64054=CARTESIAN_POINT('Ctrl Pts',(0.558525976136821,-7.89182250038105,
-47.1177241621843));
#64055=CARTESIAN_POINT('Ctrl Pts',(0.7198357008134,-7.87847205841443,-47.1111503518853));
#64056=CARTESIAN_POINT('Ctrl Pts',(0.787092112245193,-7.87203731649334,
-47.1084147241325));
#64057=CARTESIAN_POINT('Ctrl Pts',(0.883689393133947,-7.86154504356056,
-47.104493167488));
#64058=CARTESIAN_POINT('Ctrl Pts',(0.913102494607912,-7.85818307614163,
-47.1033000828654));
#64059=CARTESIAN_POINT('Ctrl Pts',(0.964340771219736,-7.8520348914912,-47.1012234006919));
#64060=CARTESIAN_POINT('Ctrl Pts',(0.986174450426143,-7.84932258332225,
-47.1003390218964));
#64061=CARTESIAN_POINT('Ctrl Pts',(1.0283692298457,-7.8439020660569,-47.0986309237827));
#64062=CARTESIAN_POINT('Ctrl Pts',(1.04873165403313,-7.84120557156168,-47.0978070835589));
#64063=CARTESIAN_POINT('Ctrl Pts',(1.10269476887119,-7.83384554274431,-47.0956249690934));
#64064=CARTESIAN_POINT('Ctrl Pts',(1.13627641701961,-7.82904513066987,-47.094268229384));
#64065=CARTESIAN_POINT('Ctrl Pts',(1.25648721952042,-7.81107155794474,-47.0894155843942));
#64066=CARTESIAN_POINT('Ctrl Pts',(1.34292752780436,-7.79667524624111,-47.0859337405068));
#64067=CARTESIAN_POINT('Ctrl Pts',(2.16096770243014,-7.64642543890663,-47.0530341839737));
#64068=CARTESIAN_POINT('Ctrl Pts',(2.87016735658576,-7.40943125419746,-47.0252880528389));
#64069=CARTESIAN_POINT('Ctrl Pts',(3.62380988329656,-7.03289481278728,-46.9921599443215));
#64070=CARTESIAN_POINT('Ctrl Pts',(3.71102301907194,-6.98726807143252,-46.9882599576255));
#64071=CARTESIAN_POINT('Ctrl Pts',(3.8153274110473,-6.93019604263933,-46.9834971434339));
#64072=CARTESIAN_POINT('Ctrl Pts',(3.83325561713376,-6.92029564493929,-46.9826749058896));
#64073=CARTESIAN_POINT('Ctrl Pts',(3.86178547296399,-6.9043958705667,-46.9813605919302));
#64074=CARTESIAN_POINT('Ctrl Pts',(3.87241194497495,-6.89844149818201,-46.9808697612837));
#64075=CARTESIAN_POINT('Ctrl Pts',(3.89261357290445,-6.88706045449287,-46.9799342336741));
#64076=CARTESIAN_POINT('Ctrl Pts',(3.9021912446441,-6.88163829484771,-46.9794896545158));
#64077=CARTESIAN_POINT('Ctrl Pts',(3.92357562209219,-6.86947306601572,-46.9784947249004));
#64078=CARTESIAN_POINT('Ctrl Pts',(3.93537631378454,-6.86271951446659,-46.9779441114432));
#64079=CARTESIAN_POINT('Ctrl Pts',(3.97028834699748,-6.842619651787,-46.9763105342148));
#64080=CARTESIAN_POINT('Ctrl Pts',(3.99334955875609,-6.82918681448292,-46.9752254787562));
#64081=CARTESIAN_POINT('Ctrl Pts',(4.16325696793383,-6.72906319468068,-46.967188022899));
#64082=CARTESIAN_POINT('Ctrl Pts',(4.3073314793589,-6.63776268406193,-46.9601343609143));
#64083=CARTESIAN_POINT('Ctrl Pts',(4.92806501999091,-6.21567699823795,-46.9288527910563));
#64084=CARTESIAN_POINT('Ctrl Pts',(5.37047476700102,-5.83767934230883,-46.9042852855195));
#64085=CARTESIAN_POINT('Ctrl Pts',(5.84435346736302,-5.33292045592954,-46.8757833709088));
#64086=CARTESIAN_POINT('Ctrl Pts',(5.91939567274526,-5.24950124830275,-46.8711886540498));
#64087=CARTESIAN_POINT('Ctrl Pts',(6.04659681284652,-5.1019035124837,-46.8632516007834));
#64088=CARTESIAN_POINT('Ctrl Pts',(6.09957053243825,-5.03845134620229,-46.8598984971033));
#64089=CARTESIAN_POINT('Ctrl Pts',(6.17409083206231,-4.94629251480734,-46.8551093434953));
#64090=CARTESIAN_POINT('Ctrl Pts',(6.19645126950599,-4.91825161247471,-46.8536626455808));
#64091=CARTESIAN_POINT('Ctrl Pts',(6.23504857306082,-4.86916796154105,-46.8511481318721));
#64092=CARTESIAN_POINT('Ctrl Pts',(6.25137148204905,-4.84819367860421,-46.8500792305038));
#64093=CARTESIAN_POINT('Ctrl Pts',(6.28273945739343,-4.80746528436973,-46.8480142252346));
#64094=CARTESIAN_POINT('Ctrl Pts',(6.29779782106404,-4.78772181308015,-46.8470179657835));
#64095=CARTESIAN_POINT('Ctrl Pts',(6.33349818969855,-4.74045412693079,-46.8446439943562));
#64096=CARTESIAN_POINT('Ctrl Pts',(6.35405410991627,-4.71286547954811,-46.8432673366394));
#64097=CARTESIAN_POINT('Ctrl Pts',(6.42853642956144,-4.61152764706807,-46.8382424324697));
#64098=CARTESIAN_POINT('Ctrl Pts',(6.48136439604962,-4.53697957074589,-46.8346070219429));
#64099=CARTESIAN_POINT('Ctrl Pts',(6.87038007757268,-3.96735549623886,-46.8072495586798));
#64100=CARTESIAN_POINT('Ctrl Pts',(7.15072881016182,-3.43644921757755,-46.7840798838598));
#64101=CARTESIAN_POINT('Ctrl Pts',(7.53228906133853,-2.45988228830297,-46.744736981882));
#64102=CARTESIAN_POINT('Ctrl Pts',(7.65998412699178,-2.02756667580617,-46.728284660055));
#64103=CARTESIAN_POINT('Ctrl Pts',(7.78362586869896,-1.42365861976096,-46.7050306428745));
#64104=CARTESIAN_POINT('Ctrl Pts',(7.81185973333916,-1.25955550757048,-46.6986766141416));
#64105=CARTESIAN_POINT('Ctrl Pts',(7.84550096603101,-1.0187788924089,-46.6891790795465));
#64106=CARTESIAN_POINT('Ctrl Pts',(7.85500315086523,-0.942719952492079,
-46.686153475079));
#64107=CARTESIAN_POINT('Ctrl Pts',(7.8649920554046,-0.852075482128857,-46.6825066092279));
#64108=CARTESIAN_POINT('Ctrl Pts',(7.86654573419024,-0.837610212058618,
-46.6819233907563));
#64109=CARTESIAN_POINT('Ctrl Pts',(7.86886823925142,-0.815410355033859,
-46.6810263205606));
#64110=CARTESIAN_POINT('Ctrl Pts',(7.86966558769957,-0.807678742472628,
-46.6807135223358));
#64111=CARTESIAN_POINT('Ctrl Pts',(7.87110179489947,-0.793548289435133,
-46.6801411466819));
#64112=CARTESIAN_POINT('Ctrl Pts',(7.87174424893307,-0.78714981573849,-46.6798817048132));
#64113=CARTESIAN_POINT('Ctrl Pts',(7.87311112089516,-0.773367521752226,
-46.6793222917062));
#64114=CARTESIAN_POINT('Ctrl Pts',(7.87383295423602,-0.765983455415304,
-46.6790222219281));
#64115=CARTESIAN_POINT('Ctrl Pts',(7.87574848486042,-0.746099507689448,
-46.6782132068987));
#64116=CARTESIAN_POINT('Ctrl Pts',(7.87692280772485,-0.733597812768984,
-46.6777035081889));
#64117=CARTESIAN_POINT('Ctrl Pts',(7.88212990727205,-0.676709371332206,
-46.6753792036738));
#64118=CARTESIAN_POINT('Ctrl Pts',(7.88581724566145,-0.632292416603385,
-46.6735507708098));
#64119=CARTESIAN_POINT('Ctrl Pts',(7.94899980271243,0.21564088930325,-46.6383480578211));
#64120=CARTESIAN_POINT('Ctrl Pts',(7.88577226059548,1.02348818189203,-46.5996498958108));
#64121=CARTESIAN_POINT('Ctrl Pts',(7.66032504632049,1.98395773844054,-46.5551195563703));
#64122=CARTESIAN_POINT('Ctrl Pts',(7.61293865587728,2.15866566095496,-46.5470608666512));
#64123=CARTESIAN_POINT('Ctrl Pts',(7.50084403057775,2.52210296041095,-46.530443748767));
#64124=CARTESIAN_POINT('Ctrl Pts',(7.43490532711301,2.71032365760512,-46.5219241720325));
#64125=CARTESIAN_POINT('Ctrl Pts',(7.32417347436791,2.99182865848988,-46.5093293312852));
#64126=CARTESIAN_POINT('Ctrl Pts',(7.28455027390585,3.08705103926472,-46.5050948076135));
#64127=CARTESIAN_POINT('Ctrl Pts',(7.23566449572441,3.19834643441602,-46.5001740420391));
#64128=CARTESIAN_POINT('Ctrl Pts',(7.22819436232519,3.21519313189428,-46.4994299632057));
#64129=CARTESIAN_POINT('Ctrl Pts',(7.21664936332346,3.24098589887956,-46.4982919185032));
#64130=CARTESIAN_POINT('Ctrl Pts',(7.21261659934645,3.24995067986846,-46.4978965844961));
#64131=CARTESIAN_POINT('Ctrl Pts',(7.2055511563716,3.26557914219114,-46.4972077632018));
#64132=CARTESIAN_POINT('Ctrl Pts',(7.20252592075397,3.27224616467548,-46.4969140337519));
#64133=CARTESIAN_POINT('Ctrl Pts',(7.19569727936826,3.28723979374393,-46.4962537217343));
#64134=CARTESIAN_POINT('Ctrl Pts',(7.19188866460989,3.29556402371873,-46.4958873097886));
#64135=CARTESIAN_POINT('Ctrl Pts',(7.18165521225326,3.31782835847886,-46.4949077723015));
#64136=CARTESIAN_POINT('Ctrl Pts',(7.1752042238846,3.33175643659699,-46.4942955032666));
#64137=CARTESIAN_POINT('Ctrl Pts',(7.14715713228492,3.39185256104063,-46.4916558585567));
#64138=CARTESIAN_POINT('Ctrl Pts',(7.12515545689423,3.4378305224918,-46.4896418166548));
#64139=CARTESIAN_POINT('Ctrl Pts',(6.66393456249095,4.37821547257291,-46.4485501715703));
#64140=CARTESIAN_POINT('Ctrl Pts',(6.06019181408714,5.18175372986905,-46.4166301706448));
#64141=CARTESIAN_POINT('Ctrl Pts',(5.13946478140763,6.01926165108473,-46.3717855922758));
#64142=CARTESIAN_POINT('Ctrl Pts',(4.94797626957656,6.1776309287007,-46.3625450263026));
#64143=CARTESIAN_POINT('Ctrl Pts',(4.7208296306728,6.34814636189649,-46.35133239936));
#64144=CARTESIAN_POINT('Ctrl Pts',(4.69214489657217,6.36937758141047,-46.3499118253417));
#64145=CARTESIAN_POINT('Ctrl Pts',(4.65513844145907,6.39638254203304,-46.3480740719181));
#64146=CARTESIAN_POINT('Ctrl Pts',(4.64694745986555,6.40233573291896,-46.3476669938368));
#64147=CARTESIAN_POINT('Ctrl Pts',(4.63374358944189,6.41189359471545,-46.3470103137547));
#64148=CARTESIAN_POINT('Ctrl Pts',(4.62873785281334,6.41550816477266,-46.3467612505415));
#64149=CARTESIAN_POINT('Ctrl Pts',(4.61920492860361,6.42237478654887,-46.3462867366303));
#64150=CARTESIAN_POINT('Ctrl Pts',(4.6146785233206,6.42562792242978,-46.3460613440979));
#64151=CARTESIAN_POINT('Ctrl Pts',(4.60436453730023,6.43302408424657,-46.3455475730646));
#64152=CARTESIAN_POINT('Ctrl Pts',(4.5985748008839,6.43716408529797,-46.3452590358056));
#64153=CARTESIAN_POINT('Ctrl Pts',(4.58134054206066,6.44945247375808,-46.3443997738154));
#64154=CARTESIAN_POINT('Ctrl Pts',(4.56987992981583,6.45757816810056,-46.343827881491));
#64155=CARTESIAN_POINT('Ctrl Pts',(4.48993862549141,6.51393800106107,-46.3398356821975));
#64156=CARTESIAN_POINT('Ctrl Pts',(4.42071877357429,6.56111133929279,-46.3363632941156));
#64157=CARTESIAN_POINT('Ctrl Pts',(4.02135508916013,6.82408867567449,-46.3162983662107));
#64158=CARTESIAN_POINT('Ctrl Pts',(3.67619450692529,7.01605725040587,-46.2988732920287));
#64159=CARTESIAN_POINT('Ctrl Pts',(2.98172504576119,7.33693393827933,-46.2651941957141));
#64160=CARTESIAN_POINT('Ctrl Pts',(2.63475557387146,7.46855871800295,-46.2489737479029));
#64161=CARTESIAN_POINT('Ctrl Pts',(2.03455713219143,7.64918971749609,-46.2223375073545));
#64162=CARTESIAN_POINT('Ctrl Pts',(1.78584145007397,7.71105092273632,-46.2116837921155));
#64163=CARTESIAN_POINT('Ctrl Pts',(1.48087482201751,7.77135282386084,-46.1990382743033));
#64164=CARTESIAN_POINT('Ctrl Pts',(1.42708803839516,7.78140956215893,-46.196823183032));
#64165=CARTESIAN_POINT('Ctrl Pts',(1.35263810591344,7.79453187276956,-46.1937768138725));
#64166=CARTESIAN_POINT('Ctrl Pts',(1.33206106015131,7.7980747815172,-46.1929369040217));
#64167=CARTESIAN_POINT('Ctrl Pts',(1.29727163054062,7.80392302704917,-46.1915202710039));
#64168=CARTESIAN_POINT('Ctrl Pts',(1.28306657425787,7.80627109848949,-46.1909427928282));
#64169=CARTESIAN_POINT('Ctrl Pts',(1.25489896044459,7.81084819450168,-46.1897995461573));
#64170=CARTESIAN_POINT('Ctrl Pts',(1.24093668106705,7.81307859128018,-46.1892337557156));
#64171=CARTESIAN_POINT('Ctrl Pts',(1.21005885675839,7.81792629448048,-46.1879844455336));
#64172=CARTESIAN_POINT('Ctrl Pts',(1.19314063463265,7.82052615949026,-46.1873012269771));
#64173=CARTESIAN_POINT('Ctrl Pts',(1.13390901955557,7.82943174889413,-46.1849136198153));
#64174=CARTESIAN_POINT('Ctrl Pts',(1.0915527382616,7.83544917886948,-46.1832139959015));
#64175=CARTESIAN_POINT('Ctrl Pts',(0.66942373535693,7.89193043690149,-46.1663490122429));
#64176=CARTESIAN_POINT('Ctrl Pts',(0.286498496674969,7.91508913926764,-46.1516800474058));
#64177=CARTESIAN_POINT('Ctrl Pts',(-0.491860302685967,7.90558271175945,
-46.1225543993435));
#64178=CARTESIAN_POINT('Ctrl Pts',(-0.886187022359869,7.87113954983068,
-46.1081597352916));
#64179=CARTESIAN_POINT('Ctrl Pts',(-1.55499311477938,7.76180846047775,-46.0831269836869));
#64180=CARTESIAN_POINT('Ctrl Pts',(-1.83105045775446,7.70135808951158,-46.0725983276471));
#64181=CARTESIAN_POINT('Ctrl Pts',(-2.20519709555398,7.59817120309017,-46.0575479044527));
#64182=CARTESIAN_POINT('Ctrl Pts',(-2.30654569286578,7.56802125350935,-46.0533895694548));
#64183=CARTESIAN_POINT('Ctrl Pts',(-2.42195202978884,7.53115577779498,-46.0485357448582));
#64184=CARTESIAN_POINT('Ctrl Pts',(-2.4366333785046,7.52641858779002,-46.0479160475372));
#64185=CARTESIAN_POINT('Ctrl Pts',(-2.45880955982573,7.51919137406076,-46.0469765296921));
#64186=CARTESIAN_POINT('Ctrl Pts',(-2.46631472108787,7.5167330049173,-46.0466579642458));
#64187=CARTESIAN_POINT('Ctrl Pts',(-2.47979216542416,7.5122960138325,-46.0460848009101));
#64188=CARTESIAN_POINT('Ctrl Pts',(-2.48576579941761,7.51032149600094,-46.0458303688146));
#64189=CARTESIAN_POINT('Ctrl Pts',(-2.49856054540299,7.50607539854739,-46.0452845671158));
#64190=CARTESIAN_POINT('Ctrl Pts',(-2.50538092557005,7.50380164350481,-46.0449931086137));
#64191=CARTESIAN_POINT('Ctrl Pts',(-2.52372411924307,7.49765865563016,-46.0442078407993));
#64192=CARTESIAN_POINT('Ctrl Pts',(-2.5352411020684,7.49377216751113,-46.0437133140088));
#64193=CARTESIAN_POINT('Ctrl Pts',(-2.58572074934318,7.4766077602358,-46.0415390939463));
#64194=CARTESIAN_POINT('Ctrl Pts',(-2.62458791699199,7.46305256368384,-46.0398475636577));
#64195=CARTESIAN_POINT('Ctrl Pts',(-3.43318739480252,7.17395004562452,-46.0042635044944));
#64196=CARTESIAN_POINT('Ctrl Pts',(-4.15562220808074,6.78107312963025,-45.9647341281851));
#64197=CARTESIAN_POINT('Ctrl Pts',(-5.11796982472318,6.04528758692267,-45.9105894038012));
#64198=CARTESIAN_POINT('Ctrl Pts',(-5.41263985942702,5.78294955417933,-45.8936601956213));
#64199=CARTESIAN_POINT('Ctrl Pts',(-5.70263496842228,5.48310220251716,-45.8767599997803));
#64200=CARTESIAN_POINT('Ctrl Pts',(-5.71863232259236,5.46641561880391,-45.8758267317313));
#64201=CARTESIAN_POINT('Ctrl Pts',(-5.74163308798811,5.44221241912649,-45.8744834321203));
#64202=CARTESIAN_POINT('Ctrl Pts',(-5.74869528104079,5.43475198134925,-45.8740707825273));
#64203=CARTESIAN_POINT('Ctrl Pts',(-5.76096829275034,5.42173619272754,-45.8733533060573));
#64204=CARTESIAN_POINT('Ctrl Pts',(-5.76618564892686,5.4161870422041,-45.8730481888646));
#64205=CARTESIAN_POINT('Ctrl Pts',(-5.77623138959779,5.40547148161288,-45.8724604832198));
#64206=CARTESIAN_POINT('Ctrl Pts',(-5.78106087508253,5.40030611758432,-45.8721778460438));
#64207=CARTESIAN_POINT('Ctrl Pts',(-5.79246602286586,5.38807493810376,-45.8715101455475));
#64208=CARTESIAN_POINT('Ctrl Pts',(-5.79903569988085,5.38100354182154,-45.871125347038));
#64209=CARTESIAN_POINT('Ctrl Pts',(-5.82192938116851,5.35627087370684,-45.8697837650972));
#64210=CARTESIAN_POINT('Ctrl Pts',(-5.83818585476969,5.33854711794419,-45.8688299599811));
#64211=CARTESIAN_POINT('Ctrl Pts',(-6.03442265878631,5.12262994648761,-45.8573015188262));
#64212=CARTESIAN_POINT('Ctrl Pts',(-6.20431871039024,4.915489818738,-45.8471776854424));
#64213=CARTESIAN_POINT('Ctrl Pts',(-6.70320704563663,4.24005511599285,-45.8165993517304));
#64214=CARTESIAN_POINT('Ctrl Pts',(-6.99213411407292,3.7444796510817,-45.7976890116023));
#64215=CARTESIAN_POINT('Ctrl Pts',(-7.4197574403165,2.78559736458829,-45.7622219736168));
#64216=CARTESIAN_POINT('Ctrl Pts',(-7.57444341709705,2.33239309061962,-45.7457952744723));
#64217=CARTESIAN_POINT('Ctrl Pts',(-7.69588628559903,1.83264405283303,-45.725533234582));
#64218=CARTESIAN_POINT('Ctrl Pts',(-7.70424944171213,1.79716176283651,-45.7240831241887));
#64219=CARTESIAN_POINT('Ctrl Pts',(-7.71420897086044,1.7535590614912,-45.7222857213359));
#64220=CARTESIAN_POINT('Ctrl Pts',(-7.7160383554138,1.745491771679,-45.7219525229698));
#64221=CARTESIAN_POINT('Ctrl Pts',(-7.71888447954771,1.73284891466236,-45.7214293107346));
#64222=CARTESIAN_POINT('Ctrl Pts',(-7.7199098161388,1.728275267469,-45.7212398234076));
#64223=CARTESIAN_POINT('Ctrl Pts',(-7.72171924607018,1.72017033160128,-45.7209036553157));
#64224=CARTESIAN_POINT('Ctrl Pts',(-7.72250498409914,1.7166394074838,-45.7207570760731));
#64225=CARTESIAN_POINT('Ctrl Pts',(-7.72430599307227,1.70851983071402,-45.7204197131408));
#64226=CARTESIAN_POINT('Ctrl Pts',(-7.72531959673453,1.70393081281934,-45.7202288258396));
#64227=CARTESIAN_POINT('Ctrl Pts',(-7.72810193807077,1.69128044639467,-45.7197020124517));
#64228=CARTESIAN_POINT('Ctrl Pts',(-7.72986214199745,1.68321727006244,-45.7193655572016));
#64229=CARTESIAN_POINT('Ctrl Pts',(-7.73866554974908,1.6425854122323,-45.7176667741155));
#64230=CARTESIAN_POINT('Ctrl Pts',(-7.74551545103198,1.60997567013182,-45.7162926430861));
#64231=CARTESIAN_POINT('Ctrl Pts',(-7.85712288276098,1.06145267070195,-45.6930111743576));
#64232=CARTESIAN_POINT('Ctrl Pts',(-7.91032359295643,0.536430839407822,
-45.6683285380629));
#64233=CARTESIAN_POINT('Ctrl Pts',(-7.91131182240876,-0.239937634875093,
-45.6320774332878));
#64234=CARTESIAN_POINT('Ctrl Pts',(-7.89977858925934,-0.489826479416971,
-45.620431413072));
#64235=CARTESIAN_POINT('Ctrl Pts',(-7.85216932097601,-0.997424927092319,
-45.5971534571454));
#64236=CARTESIAN_POINT('Ctrl Pts',(-7.81517914549196,-1.25475508284187,
-45.5855548581645));
#64237=CARTESIAN_POINT('Ctrl Pts',(-7.72747818539019,-1.70583678516334,
-45.5657374871808));
#64238=CARTESIAN_POINT('Ctrl Pts',(-7.68195679462964,-1.90035426354798,
-45.5573629996407));
#64239=CARTESIAN_POINT('Ctrl Pts',(-7.61990714418702,-2.12653445498801,
-45.5478264935644));
#64240=CARTESIAN_POINT('Ctrl Pts',(-7.61047244758596,-2.16005621277204,
-45.5464182765945));
#64241=CARTESIAN_POINT('Ctrl Pts',(-7.59742428039041,-2.20526982254841,
-45.5445257369249));
#64242=CARTESIAN_POINT('Ctrl Pts',(-7.59400465629136,-2.21701690760492,
-45.5440346561769));
#64243=CARTESIAN_POINT('Ctrl Pts',(-7.58858210884531,-2.2354846801254,-45.5432635960282));
#64244=CARTESIAN_POINT('Ctrl Pts',(-7.58659748428991,-2.24221069248022,
-45.5429829776822));
#64245=CARTESIAN_POINT('Ctrl Pts',(-7.58276179317837,-2.2551466865685,-45.5424436604605));
#64246=CARTESIAN_POINT('Ctrl Pts',(-7.58091203544779,-2.26135704856781,
-45.5421849160937));
#64247=CARTESIAN_POINT('Ctrl Pts',(-7.57653585646197,-2.27598388290856,
-45.5415759191349));
#64248=CARTESIAN_POINT('Ctrl Pts',(-7.57400303562984,-2.28439844083197,
-45.5412258907679));
#64249=CARTESIAN_POINT('Ctrl Pts',(-7.56659878752784,-2.30884921084181,
-45.54020970256));
#64250=CARTESIAN_POINT('Ctrl Pts',(-7.56169039969263,-2.32487423181379,
-45.5395448373039));
#64251=CARTESIAN_POINT('Ctrl Pts',(-7.52679158624773,-2.43753295128165,
-45.5348786373005));
#64252=CARTESIAN_POINT('Ctrl Pts',(-7.4949999812168,-2.5336011430177,-45.5309408457111));
#64253=CARTESIAN_POINT('Ctrl Pts',(-7.39020687791995,-2.83101076822703,
-45.5188618106794));
#64254=CARTESIAN_POINT('Ctrl Pts',(-7.31086629345214,-3.03002004204275,
-45.5109436891407));
#64255=CARTESIAN_POINT('Ctrl Pts',(-6.91431833129005,-3.91807343023484,
-45.4759700650823));
#64256=CARTESIAN_POINT('Ctrl Pts',(-6.50718026558615,-4.56239587239376,
-45.4520390599114));
#64257=CARTESIAN_POINT('Ctrl Pts',(-5.89333776720512,-5.28084843272612,
-45.4174652914252));
#64258=CARTESIAN_POINT('Ctrl Pts',(-5.7670575190648,-5.41847106450267,-45.4103879356583));
#64259=CARTESIAN_POINT('Ctrl Pts',(-5.62634023128691,-5.56133145084387,
-45.4023690535234));
#64260=CARTESIAN_POINT('Ctrl Pts',(-5.6166186990233,-5.57114945892926,-45.4018144041505));
#64261=CARTESIAN_POINT('Ctrl Pts',(-5.60301223786957,-5.584819136508,-45.401037129599));
#64262=CARTESIAN_POINT('Ctrl Pts',(-5.59914904886678,-5.58869223105992,
-45.4008163367014));
#64263=CARTESIAN_POINT('Ctrl Pts',(-5.59245198137082,-5.59539255640104,
-45.4004333996879));
#64264=CARTESIAN_POINT('Ctrl Pts',(-5.58961996430724,-5.59822165322737,
-45.4002714100843));
#64265=CARTESIAN_POINT('Ctrl Pts',(-5.58373667952937,-5.60408995651756,
-45.3999347773274));
#64266=CARTESIAN_POINT('Ctrl Pts',(-5.5806850754036,-5.60712882285447,-45.399760106395));
#64267=CARTESIAN_POINT('Ctrl Pts',(-5.57351947741971,-5.61425286645683,
-45.3993498107253));
#64268=CARTESIAN_POINT('Ctrl Pts',(-5.56940347570227,-5.61833601150611,
-45.3991140213328));
#64269=CARTESIAN_POINT('Ctrl Pts',(-5.55604753505774,-5.6315562370619,-45.3983485650238));
#64270=CARTESIAN_POINT('Ctrl Pts',(-5.54678961246672,-5.6406750353316,-45.3978174365163));
#64271=CARTESIAN_POINT('Ctrl Pts',(-5.31587719976169,-5.86699919123651,
-45.3845575846435));
#64272=CARTESIAN_POINT('Ctrl Pts',(-5.08167441891715,-6.0709783650749,-45.3708316321397));
#64273=CARTESIAN_POINT('Ctrl Pts',(-4.65342953800843,-6.40178167051542,
-45.3461622491373));
#64274=CARTESIAN_POINT('Ctrl Pts',(-4.46464806289698,-6.53483956533783,
-45.3354166971247));
#64275=CARTESIAN_POINT('Ctrl Pts',(-3.95845565660522,-6.85943179932433,
-45.3073755364382));
#64276=CARTESIAN_POINT('Ctrl Pts',(-3.63290975909653,-7.03726989980414,
-45.2901021890545));
#64277=CARTESIAN_POINT('Ctrl Pts',(-2.91856779895789,-7.36466851416871,
-45.2546967839063));
#64278=CARTESIAN_POINT('Ctrl Pts',(-2.52798116618026,-7.50771337743377,
-45.2367807096817));
#64279=CARTESIAN_POINT('Ctrl Pts',(-2.10121423891686,-7.62689902997033,
-45.2187800556535));
#64280=CARTESIAN_POINT('Ctrl Pts',(-2.07446461545123,-7.63421814404193,
-45.217657983075));
#64281=CARTESIAN_POINT('Ctrl Pts',(-2.03751758159717,-7.64411889804656,
-45.216116602081));
#64282=CARTESIAN_POINT('Ctrl Pts',(-2.02735284147749,-7.64682104406813,
-45.2156934219346));
#64283=CARTESIAN_POINT('Ctrl Pts',(-2.00993027837801,-7.65141539399573,
-45.2149695809295));
#64284=CARTESIAN_POINT('Ctrl Pts',(-2.00267510957927,-7.65331755915798,
-45.2146686007973));
#64285=CARTESIAN_POINT('Ctrl Pts',(-1.98854536880815,-7.65700063649053,
-45.2140832912774));
#64286=CARTESIAN_POINT('Ctrl Pts',(-1.98167108286418,-7.65878261545047,
-45.2137989279234));
#64287=CARTESIAN_POINT('Ctrl Pts',(-1.96520804139635,-7.66302657957349,
-45.2131188595991));
#64288=CARTESIAN_POINT('Ctrl Pts',(-1.95561703554585,-7.66547982949513,
-45.2127234342194));
#64289=CARTESIAN_POINT('Ctrl Pts',(-1.92679183894951,-7.67279530569442,
-45.2115372988393));
#64290=CARTESIAN_POINT('Ctrl Pts',(-1.90754387333352,-7.67760320492577,
-45.2107483223068));
#64291=CARTESIAN_POINT('Ctrl Pts',(-1.73649819091085,-7.71964532282843,
-45.2037639917618));
#64292=CARTESIAN_POINT('Ctrl Pts',(-1.58364181847314,-7.75244682354744,
-45.1977109030058));
#64293=CARTESIAN_POINT('Ctrl Pts',(-1.18553483729385,-7.82560946630156,
-45.1823687021595));
#64294=CARTESIAN_POINT('Ctrl Pts',(-0.939173244481577,-7.85898336470746,
-45.1732880575031));
#64295=CARTESIAN_POINT('Ctrl Pts',(0.129995793870823,-7.95281751627099,
-45.1349809229434));
#64296=CARTESIAN_POINT('Ctrl Pts',(0.957828023675432,-7.89599430028632,
-45.1084586478026));
#64297=CARTESIAN_POINT('Ctrl Pts',(1.80848824980824,-7.70166066423514,-45.0741234542654));
#64298=CARTESIAN_POINT('Ctrl Pts',(1.85499876553423,-7.6905907571515,-45.0722250975418));
#64299=CARTESIAN_POINT('Ctrl Pts',(1.91501472248869,-7.67573033532885,-45.0697502989462));
#64300=CARTESIAN_POINT('Ctrl Pts',(1.92861497835151,-7.67232440857544,-45.0691878026162));
#64301=CARTESIAN_POINT('Ctrl Pts',(1.95022814899501,-7.6668506995021,-45.0682912864331));
#64302=CARTESIAN_POINT('Ctrl Pts',(1.95824703068331,-7.66480645860213,-45.0679580899528));
#64303=CARTESIAN_POINT('Ctrl Pts',(1.97326850842459,-7.66095194522913,-45.0673328667234));
#64304=CARTESIAN_POINT('Ctrl Pts',(1.98027186255802,-7.65914464306761,-45.0670409418176));
#64305=CARTESIAN_POINT('Ctrl Pts',(1.99605121294747,-7.65504949740419,-45.0663822406648));
#64306=CARTESIAN_POINT('Ctrl Pts',(2.00482576667705,-7.65275616343229,-45.0660152804689));
#64307=CARTESIAN_POINT('Ctrl Pts',(2.03070576644008,-7.6459445526041,-45.0649310045302));
#64308=CARTESIAN_POINT('Ctrl Pts',(2.04779996948997,-7.64138399055018,-45.0642123053483));
#64309=CARTESIAN_POINT('Ctrl Pts',(2.18268437504961,-7.6049130649026,-45.0585220147928));
#64310=CARTESIAN_POINT('Ctrl Pts',(2.29973467972043,-7.57033901535893,-45.0534680757386));
#64311=CARTESIAN_POINT('Ctrl Pts',(2.74374870694774,-7.42793905649057,-45.0339382037399));
#64312=CARTESIAN_POINT('Ctrl Pts',(3.06434465874631,-7.30152173758252,-45.019104241431));
#64313=CARTESIAN_POINT('Ctrl Pts',(3.88083126550361,-6.91628902789055,-44.9802681980221));
#64314=CARTESIAN_POINT('Ctrl Pts',(4.35934292189458,-6.6251100900236,-44.9565246107859));
#64315=CARTESIAN_POINT('Ctrl Pts',(4.85946314109944,-6.24296029957444,-44.9304128801675));
#64316=CARTESIAN_POINT('Ctrl Pts',(4.91514953653958,-6.19921288828366,-44.9274828472938));
#64317=CARTESIAN_POINT('Ctrl Pts',(4.98261429184455,-6.14473178792635,-44.9239020125934));
#64318=CARTESIAN_POINT('Ctrl Pts',(4.99495713294828,-6.13470269594719,-44.9232455948541));
#64319=CARTESIAN_POINT('Ctrl Pts',(5.22818074404094,-5.94402794789168,-44.9108170763868));
#64320=CARTESIAN_POINT('Ctrl Pts',(5.4391645057724,-5.75159438011302,-44.8991153935043));
#64321=CARTESIAN_POINT('Ctrl Pts',(5.66981237664644,-5.51715892151711,-44.8857945654762));
#64322=CARTESIAN_POINT('Ctrl Pts',(5.70007731670018,-5.48588493873102,-44.8840354158309));
#64323=CARTESIAN_POINT('Ctrl Pts',(5.74901493522847,-5.43447350553338,-44.881172386596));
#64324=CARTESIAN_POINT('Ctrl Pts',(5.76784347151739,-5.41448582070249,-44.8800662851112));
#64325=CARTESIAN_POINT('Ctrl Pts',(5.80137060070719,-5.37852130513472,-44.8780884452025));
#64326=CARTESIAN_POINT('Ctrl Pts',(5.81610820099359,-5.36258125106156,-44.8772161437571));
#64327=CARTESIAN_POINT('Ctrl Pts',(5.84725222962449,-5.32861674363766,-44.8753665552628));
#64328=CARTESIAN_POINT('Ctrl Pts',(5.86364135858383,-5.31057671634118,-44.8743895303016));
#64329=CARTESIAN_POINT('Ctrl Pts',(5.90739974449084,-5.26196096360556,-44.871770847484));
#64330=CARTESIAN_POINT('Ctrl Pts',(5.93461496046871,-5.23124748199467,-44.8701314969858));
#64331=CARTESIAN_POINT('Ctrl Pts',(6.07004079832293,-5.07599688568197,-44.8619190020448));
#64332=CARTESIAN_POINT('Ctrl Pts',(6.17457707950895,-4.94830668042966,-44.8554023219878));
#64333=CARTESIAN_POINT('Ctrl Pts',(6.46776497958753,-4.56640932576637,-44.8365342983207));
#64334=CARTESIAN_POINT('Ctrl Pts',(6.64524879998031,-4.30403894886653,-44.8243466543364));
#64335=CARTESIAN_POINT('Ctrl Pts',(6.94804926018985,-3.79283938164235,-44.8015130314557));
#64336=CARTESIAN_POINT('Ctrl Pts',(7.07688024818179,-3.54665771125622,-44.7908739850804));
#64337=CARTESIAN_POINT('Ctrl Pts',(7.25457570584618,-3.15868255042331,-44.7742298738312));
#64338=CARTESIAN_POINT('Ctrl Pts',(7.31280706914215,-3.02142269764379,-44.7683624429864));
#64339=CARTESIAN_POINT('Ctrl Pts',(7.3758477494229,-2.86030839469314,-44.7614416826826));
#64340=CARTESIAN_POINT('Ctrl Pts',(7.38446980394693,-2.83797460285967,-44.7604815638511));
#64341=CARTESIAN_POINT('Ctrl Pts',(7.39760687681806,-2.80348029150055,-44.7589972114741));
#64342=CARTESIAN_POINT('Ctrl Pts',(7.40219357857654,-2.79134725043559,-44.7584748396518));
#64343=CARTESIAN_POINT('Ctrl Pts',(7.41020457897124,-2.76999743172974,-44.7575552228572));
#64344=CARTESIAN_POINT('Ctrl Pts',(7.41364157835485,-2.76078543552947,-44.7571582875394));
#64345=CARTESIAN_POINT('Ctrl Pts',(7.42143726232586,-2.7397715677649,-44.7562525233606));
#64346=CARTESIAN_POINT('Ctrl Pts',(7.42578498214266,-2.7279656669084,-44.7557434374359));
#64347=CARTESIAN_POINT('Ctrl Pts',(7.43758749551783,-2.69567955421509,-44.7543506841743));
#64348=CARTESIAN_POINT('Ctrl Pts',(7.44498582980727,-2.67517887250671,-44.7534657433738));
#64349=CARTESIAN_POINT('Ctrl Pts',(7.4834511116676,-2.56719664687747,-44.7488019662596));
#64350=CARTESIAN_POINT('Ctrl Pts',(7.51306077962544,-2.47920480516808,-44.7449927779498));
#64351=CARTESIAN_POINT('Ctrl Pts',(7.59866283024998,-2.20918713104892,-44.7332981265431));
#64352=CARTESIAN_POINT('Ctrl Pts',(7.64963710808998,-2.0256443056373,-44.7253422308271));
#64353=CARTESIAN_POINT('Ctrl Pts',(7.82265265429128,-1.30235638319295,-44.6941556173193));
#64354=CARTESIAN_POINT('Ctrl Pts',(7.8945690814699,-0.752226771582995,-44.6708898658725));
#64355=CARTESIAN_POINT('Ctrl Pts',(7.91122720184627,-0.0905400669992552,
-44.6438350874794));
#64356=CARTESIAN_POINT('Ctrl Pts',(7.91172468266514,0.0180637388576222,
-44.6394200639881));
#64357=CARTESIAN_POINT('Ctrl Pts',(7.90934834411637,0.166485818170939,-44.6334161883937));
#64358=CARTESIAN_POINT('Ctrl Pts',(7.90840944598711,0.206322104156794,-44.6318076789081));
#64359=CARTESIAN_POINT('Ctrl Pts',(7.90640499519587,0.270711909233743,-44.6292120722264));
#64360=CARTESIAN_POINT('Ctrl Pts',(7.90552593140272,0.295270449449205,-44.6282231139418));
#64361=CARTESIAN_POINT('Ctrl Pts',(7.90345141816608,0.3465424911911,-44.6261604067414));
#64362=CARTESIAN_POINT('Ctrl Pts',(7.90223492731764,0.37325484149204,-44.6250868794899));
#64363=CARTESIAN_POINT('Ctrl Pts',(7.89901986948427,0.43676559278134,-44.6225369504241));
#64364=CARTESIAN_POINT('Ctrl Pts',(7.89689955789119,0.47355724942195,-44.6210617538831));
#64365=CARTESIAN_POINT('Ctrl Pts',(7.88873349368569,0.59988103282007,-44.6160025734615));
#64366=CARTESIAN_POINT('Ctrl Pts',(7.88142150774053,0.689324735200001,-44.6124306478669));
#64367=CARTESIAN_POINT('Ctrl Pts',(7.80137745721727,1.49864091254664,-44.5801643225063));
#64368=CARTESIAN_POINT('Ctrl Pts',(7.63172077361449,2.20552977340986,-44.5524402960951));
#64369=CARTESIAN_POINT('Ctrl Pts',(7.18194481785759,3.35646032186492,-44.5064496494739));
#64370=CARTESIAN_POINT('Ctrl Pts',(6.94969292536717,3.81416528856029,-44.4877776552294));
#64371=CARTESIAN_POINT('Ctrl Pts',(6.67321101181492,4.24878633463581,-44.4675680141162));
#64372=CARTESIAN_POINT('Ctrl Pts',(6.6715529056615,4.25138946140321,-44.4674468714398));
#64373=CARTESIAN_POINT('Ctrl Pts',(6.63819046336895,4.3036989038502,-44.4650105307815));
#64374=CARTESIAN_POINT('Ctrl Pts',(6.60593341904417,4.35304954538979,-44.4626757536));
#64375=CARTESIAN_POINT('Ctrl Pts',(6.56602459655137,4.4126414960672,-44.4598069651511));
#64376=CARTESIAN_POINT('Ctrl Pts',(6.55889528270141,4.4232314707251,-44.4592952354856));
#64377=CARTESIAN_POINT('Ctrl Pts',(6.54712137839123,4.44062952499507,-44.4584512847815));
#64378=CARTESIAN_POINT('Ctrl Pts',(6.54249171277528,4.44744770731264,-44.4581197240461));
#64379=CARTESIAN_POINT('Ctrl Pts',(6.53414027003356,4.4597057498507,-44.4575221266501));
#64380=CARTESIAN_POINT('Ctrl Pts',(6.53042232892211,4.46514822254661,-44.4572562637464));
#64381=CARTESIAN_POINT('Ctrl Pts',(6.52248924768152,4.47672988586845,-44.4566893513785));
#64382=CARTESIAN_POINT('Ctrl Pts',(6.51827223386542,4.48286778099488,-44.4563882156077));
#64383=CARTESIAN_POINT('Ctrl Pts',(6.50691866336469,4.49934309663846,-44.4555780258122));
#64384=CARTESIAN_POINT('Ctrl Pts',(6.49976615902982,4.50966946332464,-44.4550682213655));
#64385=CARTESIAN_POINT('Ctrl Pts',(6.46515267481044,4.55938897426312,-44.4526037666466));
#64386=CARTESIAN_POINT('Ctrl Pts',(6.43735839255185,4.59854799986632,-44.4506328965492));
#64387=CARTESIAN_POINT('Ctrl Pts',(6.10443628261212,5.05866449098989,-44.4270913703434));
#64388=CARTESIAN_POINT('Ctrl Pts',(5.75892180876415,5.44875254975246,-44.4031993467315));
#64389=CARTESIAN_POINT('Ctrl Pts',(5.17862629303202,5.98660453099862,-44.3667604549579));
#64390=CARTESIAN_POINT('Ctrl Pts',(4.9701723592034,6.16076274054971,-44.3542610464885));
#64391=CARTESIAN_POINT('Ctrl Pts',(4.37230274434813,6.61013656869777,-44.3204537852897));
#64392=CARTESIAN_POINT('Ctrl Pts',(3.96631509282608,6.86144133614805,-44.2997475536641));
#64393=CARTESIAN_POINT('Ctrl Pts',(3.51378452998848,7.08788454175108,-44.279163188166));
#64394=CARTESIAN_POINT('Ctrl Pts',(3.48736358200873,7.10092136772575,-44.2779696203012));
#64395=CARTESIAN_POINT('Ctrl Pts',(3.45095111220224,7.11863604192004,-44.2763358981831));
#64396=CARTESIAN_POINT('Ctrl Pts',(3.44102187503583,7.1234409615633,-44.2758915424382));
#64397=CARTESIAN_POINT('Ctrl Pts',(3.4240358399727,7.13161697850625,-44.2751333191468));
#64398=CARTESIAN_POINT('Ctrl Pts',(3.4169840464456,7.13499840142198,-44.2748191109533));
#64399=CARTESIAN_POINT('Ctrl Pts',(3.40268787822359,7.14182753716762,-44.2741832646201));
#64400=CARTESIAN_POINT('Ctrl Pts',(3.39544324884939,7.14527469811882,-44.2738616449055));
#64401=CARTESIAN_POINT('Ctrl Pts',(3.37884540730548,7.15314138877483,-44.2731261594983));
#64402=CARTESIAN_POINT('Ctrl Pts',(3.36948873674098,7.1575536091772,-44.2727125347048));
#64403=CARTESIAN_POINT('Ctrl Pts',(3.34986867032473,7.16675862566739,-44.2718472640278));
#64404=CARTESIAN_POINT('Ctrl Pts',(3.3396035769206,7.17154775883957,-44.2713957389301));
#64405=CARTESIAN_POINT('Ctrl Pts',(3.31252508512835,7.18411036074909,-44.2702077416731));
#64406=CARTESIAN_POINT('Ctrl Pts',(3.29569456757509,7.19184687253205,-44.2694724794255));
#64407=CARTESIAN_POINT('Ctrl Pts',(3.24532174250652,7.21478787188485,-44.2672811480845));
#64408=CARTESIAN_POINT('Ctrl Pts',(3.21170008565048,7.22981741486764,-44.2658307732497));
#64409=CARTESIAN_POINT('Ctrl Pts',(3.09291135834524,7.28192614760107,-44.2607486440928));
#64410=CARTESIAN_POINT('Ctrl Pts',(3.00719617425933,7.31774015175861,-44.2571575654721));
#64411=CARTESIAN_POINT('Ctrl Pts',(2.60008434714947,7.47948037006064,-44.240435744412));
#64412=CARTESIAN_POINT('Ctrl Pts',(2.27129058719802,7.58579774742386,-44.2279221395332));
#64413=CARTESIAN_POINT('Ctrl Pts',(1.16965892285502,7.8639361655957,-44.1878651200387));
#64414=CARTESIAN_POINT('Ctrl Pts',(0.378133496479003,7.94142856352877,-44.162259375322));
#64415=CARTESIAN_POINT('Ctrl Pts',(-0.454598790872861,7.89804507163571,
-44.1294837668276));
#64416=CARTESIAN_POINT('Ctrl Pts',(-0.497589125549506,7.89545317889029,
-44.127774030864));
#64417=CARTESIAN_POINT('Ctrl Pts',(-0.551678184800923,7.8917486311373,-44.1256011868434));
#64418=CARTESIAN_POINT('Ctrl Pts',(-0.562798408572342,7.89096339023692,
-44.1251533324544));
#64419=CARTESIAN_POINT('Ctrl Pts',(-0.580369493145021,7.88968529839876,
-44.124443919229));
#64420=CARTESIAN_POINT('Ctrl Pts',(-0.586821501426138,7.88920803258754,
-44.1241830518139));
#64421=CARTESIAN_POINT('Ctrl Pts',(-0.598243105009983,7.88834906871723,
-44.1237205991244));
#64422=CARTESIAN_POINT('Ctrl Pts',(-0.603212944556086,7.88797058729222,
-44.123519154298));
#64423=CARTESIAN_POINT('Ctrl Pts',(-0.614626382982608,7.88709053966962,
-44.1230560289645));
#64424=CARTESIAN_POINT('Ctrl Pts',(-0.621069725854733,7.8865857737598,-44.1227942107449));
#64425=CARTESIAN_POINT('Ctrl Pts',(-0.638898405614348,7.88516710594123,
-44.1220687637841));
#64426=CARTESIAN_POINT('Ctrl Pts',(-0.650282365318184,7.88423644399116,
-44.1216044253024));
#64427=CARTESIAN_POINT('Ctrl Pts',(-0.712264357565476,7.8790341346586,-44.1190702607237));
#64428=CARTESIAN_POINT('Ctrl Pts',(-0.762821681273152,7.87430011727032,
-44.1169814588417));
#64429=CARTESIAN_POINT('Ctrl Pts',(-1.49646675410485,7.79847232987358,-44.0863874625686));
#64430=CARTESIAN_POINT('Ctrl Pts',(-2.16750913615516,7.63921219173083,-44.0551920006656));
#64431=CARTESIAN_POINT('Ctrl Pts',(-3.17779515468966,7.25539122150705,-44.0085019889685));
#64432=CARTESIAN_POINT('Ctrl Pts',(-3.53507699169281,7.08818386040135,-43.9919710119758));
#64433=CARTESIAN_POINT('Ctrl Pts',(-3.8988190290467,6.88358032139274,-43.9750565924681));
#64434=CARTESIAN_POINT('Ctrl Pts',(-3.91915006175604,6.87202522280835,-43.9741107245761));
#64435=CARTESIAN_POINT('Ctrl Pts',(-3.95993679039919,6.84860429791978,-43.9722121322862));
#64436=CARTESIAN_POINT('Ctrl Pts',(-3.98039111488974,6.83673656017006,-43.9712594598489));
#64437=CARTESIAN_POINT('Ctrl Pts',(-4.01435675634706,6.81682536582943,-43.9696764541024));
#64438=CARTESIAN_POINT('Ctrl Pts',(-4.02789781762661,6.80883304306072,-43.9690450823159));
#64439=CARTESIAN_POINT('Ctrl Pts',(-4.05205855090279,6.79447538747914,-43.9679180127365));
#64440=CARTESIAN_POINT('Ctrl Pts',(-4.06268726649798,6.78812540151049,-43.9674220080568));
#64441=CARTESIAN_POINT('Ctrl Pts',(-4.08700758415542,6.77351796708618,-43.9662866037054));
#64442=CARTESIAN_POINT('Ctrl Pts',(-4.10068915796714,6.76524390360077,-43.9656475377697));
#64443=CARTESIAN_POINT('Ctrl Pts',(-4.13839705812951,6.74228327368155,-43.9638851918284));
#64444=CARTESIAN_POINT('Ctrl Pts',(-4.16237024968604,6.72750978214497,-43.9627636250008));
#64445=CARTESIAN_POINT('Ctrl Pts',(-4.28124024249631,6.65337747075567,-43.9571958515007));
#64446=CARTESIAN_POINT('Ctrl Pts',(-4.37494977807241,6.59213659655248,-43.9527859324027));
#64447=CARTESIAN_POINT('Ctrl Pts',(-5.12198473007164,6.08098808972116,-43.9174365848067));
#64448=CARTESIAN_POINT('Ctrl Pts',(-5.70551537586047,5.53716423219042,-43.8891417510623));
#64449=CARTESIAN_POINT('Ctrl Pts',(-6.29481586633187,4.79408964371179,-43.8537172574395));
#64450=CARTESIAN_POINT('Ctrl Pts',(-6.38764087108726,4.66969423305072,-43.8478580062982));
#64451=CARTESIAN_POINT('Ctrl Pts',(-6.49955185713226,4.5101357136543,-43.8403503720539));
#64452=CARTESIAN_POINT('Ctrl Pts',(-6.52211318770562,4.47744771221047,-43.838812688951));
#64453=CARTESIAN_POINT('Ctrl Pts',(-6.59520684119632,4.36982115103825,-43.8337473460104));
#64454=CARTESIAN_POINT('Ctrl Pts',(-6.64470025680236,4.2941876933423,-43.830183890962));
#64455=CARTESIAN_POINT('Ctrl Pts',(-6.70054731093767,4.20556693466053,-43.8259884268985));
#64456=CARTESIAN_POINT('Ctrl Pts',(-6.70817566551772,4.19338845627804,-43.825411441167));
#64457=CARTESIAN_POINT('Ctrl Pts',(-6.72025219105539,4.17399130127671,-43.8244916739843));
#64458=CARTESIAN_POINT('Ctrl Pts',(-6.72472203198342,4.16678610998573,-43.8241498506543));
#64459=CARTESIAN_POINT('Ctrl Pts',(-6.73256880097563,4.15409194320933,-43.8235473040035));
#64460=CARTESIAN_POINT('Ctrl Pts',(-6.73595062620695,4.14860599400494,-43.8232868008956));
#64461=CARTESIAN_POINT('Ctrl Pts',(-6.74290816332254,4.1372886401684,-43.8227491644229));
#64462=CARTESIAN_POINT('Ctrl Pts',(-6.74648302207489,4.13145671931096,-43.8224719926551));
#64463=CARTESIAN_POINT('Ctrl Pts',(-6.75557372088396,4.1165831556833,-43.8217647719074));
#64464=CARTESIAN_POINT('Ctrl Pts',(-6.76107896502204,4.10753507632421,-43.8213342361609));
#64465=CARTESIAN_POINT('Ctrl Pts',(-6.78315011483523,4.0710957042091,-43.8195990017079));
#64466=CARTESIAN_POINT('Ctrl Pts',(-6.79956771423268,4.04361528467046,-43.818287360785));
#64467=CARTESIAN_POINT('Ctrl Pts',(-6.96435157946995,3.76395226766393,-43.8049021163545));
#64468=CARTESIAN_POINT('Ctrl Pts',(-7.09875764317999,3.50387054291138,-43.7920500307316));
#64469=CARTESIAN_POINT('Ctrl Pts',(-7.55182419316041,2.49353953357784,-43.7420414547854));
#64470=CARTESIAN_POINT('Ctrl Pts',(-7.76843741877283,1.70283027448166,-43.7035157770758));
#64471=CARTESIAN_POINT('Ctrl Pts',(-7.8652569248955,0.850573682097738,-43.6675723436489));
#64472=CARTESIAN_POINT('Ctrl Pts',(-7.8697307651614,0.808133555404825,-43.6657947051532));
#64473=CARTESIAN_POINT('Ctrl Pts',(-7.88183650337382,0.68364090430447,-43.6606161618421));
#64474=CARTESIAN_POINT('Ctrl Pts',(-7.88853013505056,0.601501798532957,
-43.6572451382015));
#64475=CARTESIAN_POINT('Ctrl Pts',(-7.89496600620694,0.503663980293447,
-43.6532834618211));
#64476=CARTESIAN_POINT('Ctrl Pts',(-7.89594639005154,0.488053535393955,
-43.6526529784477));
#64477=CARTESIAN_POINT('Ctrl Pts',(-7.89745491676051,0.462838376977011,
-43.6516371759946));
#64478=CARTESIAN_POINT('Ctrl Pts',(-7.89801184716472,0.453235466824881,
-43.6512509281057));
#64479=CARTESIAN_POINT('Ctrl Pts',(-7.89896170445024,0.436323918044981,
-43.6505717811464));
#64480=CARTESIAN_POINT('Ctrl Pts',(-7.89936200502844,0.429015715012015,
-43.6502786440621));
#64481=CARTESIAN_POINT('Ctrl Pts',(-7.90012531107592,0.414716855233308,
-43.6497057922665));
#64482=CARTESIAN_POINT('Ctrl Pts',(-7.90048918131097,0.407726252577871,
-43.649426049842));
#64483=CARTESIAN_POINT('Ctrl Pts',(-7.90124949256747,0.392736052081179,
-43.6488268731163));
#64484=CARTESIAN_POINT('Ctrl Pts',(-7.90164306460424,0.384736312941631,
-43.6485075319314));
#64485=CARTESIAN_POINT('Ctrl Pts',(-7.90256087074338,0.365485359797262,
-43.6477400568437));
#64486=CARTESIAN_POINT('Ctrl Pts',(-7.90307322721607,0.354233582099445,
-43.6472923078335));
#64487=CARTESIAN_POINT('Ctrl Pts',(-7.90522771154322,0.304586186118256,
-43.6453202741824));
#64488=CARTESIAN_POINT('Ctrl Pts',(-7.90661408876186,0.266179680381141,
-43.6438042818066));
#64489=CARTESIAN_POINT('Ctrl Pts',(-7.90992443894157,0.151248008270138,
-43.6392956068646));
#64490=CARTESIAN_POINT('Ctrl Pts',(-7.91101765627593,0.0747029496055771,
-43.6363298934422));
#64491=CARTESIAN_POINT('Ctrl Pts',(-7.91099978439819,-0.00184695744787657,
-43.6333989249003));
#64492=CARTESIAN_POINT('',(-7.91099765047707,0.00609706046871071,-39.6423315082368));
#64493=CARTESIAN_POINT('Ctrl Pts',(-7.91099978972198,-0.00182401173648303,
-43.6333998034544));
#64494=CARTESIAN_POINT('Ctrl Pts',(-7.91081183821771,-0.816996568458522,
-43.6021881287131));
#64495=CARTESIAN_POINT('Ctrl Pts',(-7.78464881683108,-1.62722230157388,
-43.5757980757572));
#64496=CARTESIAN_POINT('Ctrl Pts',(-7.4589866112574,-2.64824243785534,-43.5392415117727));
#64497=CARTESIAN_POINT('Ctrl Pts',(-7.36924138152087,-2.88858752493205,
-43.5303177158346));
#64498=CARTESIAN_POINT('Ctrl Pts',(-7.21990949736473,-3.23599310220964,
-43.5164155290938));
#64499=CARTESIAN_POINT('Ctrl Pts',(-7.16925451213632,-3.34671956534006,
-43.5118274409518));
#64500=CARTESIAN_POINT('Ctrl Pts',(-7.09058732957546,-3.50868829766092,
-43.5048216944913));
#64501=CARTESIAN_POINT('Ctrl Pts',(-7.0645291626779,-3.56086360696497,-43.5025187266709));
#64502=CARTESIAN_POINT('Ctrl Pts',(-7.03356423302713,-3.62118560723126,
-43.4997969921473));
#64503=CARTESIAN_POINT('Ctrl Pts',(-7.02921615105167,-3.62961861941296,
-43.4994151389089));
#64504=CARTESIAN_POINT('Ctrl Pts',(-7.02257664445033,-3.64243912420972,
-43.4988325238346));
#64505=CARTESIAN_POINT('Ctrl Pts',(-7.02029624195143,-3.64683234818561,
-43.4986325034782));
#64506=CARTESIAN_POINT('Ctrl Pts',(-7.01615416623397,-3.65479382646461,
-43.4982693384759));
#64507=CARTESIAN_POINT('Ctrl Pts',(-7.01429388855268,-3.65836280912893,
-43.4981062886103));
#64508=CARTESIAN_POINT('Ctrl Pts',(-7.01029267735949,-3.66602494745113,
-43.4977557021633));
#64509=CARTESIAN_POINT('Ctrl Pts',(-7.00815087970693,-3.67011765272518,
-43.4975681063131));
#64510=CARTESIAN_POINT('Ctrl Pts',(-7.0023394284181,-3.68119896719949,-43.4970592732793));
#64511=CARTESIAN_POINT('Ctrl Pts',(-6.99866291404689,-3.68818393271218,
-43.4967375646631));
#64512=CARTESIAN_POINT('Ctrl Pts',(-6.981177638206,-3.72128371001466,-43.4952085127401));
#64513=CARTESIAN_POINT('Ctrl Pts',(-6.96723329617623,-3.74732622232824,
-43.493991978368));
#64514=CARTESIAN_POINT('Ctrl Pts',(-6.73296683984179,-4.17901539971919,
-43.473610134267));
#64515=CARTESIAN_POINT('Ctrl Pts',(-6.47771879030042,-4.56465715665231,
-43.4522658669892));
#64516=CARTESIAN_POINT('Ctrl Pts',(-5.93245091127666,-5.24990418329373,
-43.4114177311384));
#64517=CARTESIAN_POINT('Ctrl Pts',(-5.6494882618426,-5.55326838040774,-43.3920152701908));
#64518=CARTESIAN_POINT('Ctrl Pts',(-5.06392859816913,-6.08973639356223,
-43.3563853763366));
#64519=CARTESIAN_POINT('Ctrl Pts',(-4.76565274706613,-6.3258890846241,-43.3400695787678));
#64520=CARTESIAN_POINT('Ctrl Pts',(-4.43157774077439,-6.55329092311202,
-43.3237161081398));
#64521=CARTESIAN_POINT('Ctrl Pts',(-4.41156933500068,-6.56677692725913,
-43.3227434237852));
#64522=CARTESIAN_POINT('Ctrl Pts',(-4.38301731790371,-6.5858320796829,-43.3213649246844));
#64523=CARTESIAN_POINT('Ctrl Pts',(-4.37452425973476,-6.59147650325015,
-43.32095606936));
#64524=CARTESIAN_POINT('Ctrl Pts',(-4.36038332664269,-6.60083509393963,
-43.3202772989397));
#64525=CARTESIAN_POINT('Ctrl Pts',(-4.35474157537353,-6.60455846402135,
-43.3200070133658));
#64526=CARTESIAN_POINT('Ctrl Pts',(-4.34300117598336,-6.61228515758575,
-43.3194456326554));
#64527=CARTESIAN_POINT('Ctrl Pts',(-4.33690174709132,-6.61628728640856,
-43.3191545856371));
#64528=CARTESIAN_POINT('Ctrl Pts',(-4.32221702288224,-6.62589360923801,
-43.3184553217672));
#64529=CARTESIAN_POINT('Ctrl Pts',(-4.31362634143258,-6.631489568824,-43.3180474350915));
#64530=CARTESIAN_POINT('Ctrl Pts',(-4.28488911204101,-6.65012949677434,
-43.3166869384512));
#64531=CARTESIAN_POINT('Ctrl Pts',(-4.2646939914463,-6.66309854343295,-43.3157373204382));
#64532=CARTESIAN_POINT('Ctrl Pts',(-3.98718274791531,-6.83953415534704,
-43.3027757474687));
#64533=CARTESIAN_POINT('Ctrl Pts',(-3.72067635320959,-6.98809303667278,
-43.2913722855702));
#64534=CARTESIAN_POINT('Ctrl Pts',(-3.23102945415126,-7.22506283259982,
-43.2718174197311));
#64535=CARTESIAN_POINT('Ctrl Pts',(-3.01120352961416,-7.31940869168366,
-43.263501616798));
#64536=CARTESIAN_POINT('Ctrl Pts',(-2.41495038670087,-7.54389477985291,
-43.2416564017362));
#64537=CARTESIAN_POINT('Ctrl Pts',(-2.03242620888376,-7.65581860908378,
-43.2283866911835));
#64538=CARTESIAN_POINT('Ctrl Pts',(-1.49660847698611,-7.76958923368827,
-43.2091146435396));
#64539=CARTESIAN_POINT('Ctrl Pts',(-1.34924972032207,-7.79652973624795,
-43.2037411783932));
#64540=CARTESIAN_POINT('Ctrl Pts',(-1.09477686865112,-7.83562264838259,
-43.194203054522));
#64541=CARTESIAN_POINT('Ctrl Pts',(-0.988014039631855,-7.84979905750442,
-43.1901237789848));
#64542=CARTESIAN_POINT('Ctrl Pts',(-0.826025131388013,-7.86795167644452,
-43.1837717059559));
#64543=CARTESIAN_POINT('Ctrl Pts',(-0.770989221291343,-7.8735351930206,
-43.1815852750323));
#64544=CARTESIAN_POINT('Ctrl Pts',(-0.706519088023917,-7.87939341050408,
-43.1789861136164));
#64545=CARTESIAN_POINT('Ctrl Pts',(-0.697136198361799,-7.88022911196833,
-43.178606891156));
#64546=CARTESIAN_POINT('Ctrl Pts',(-0.682687991573719,-7.88148995713126,
-43.1780215073568));
#64547=CARTESIAN_POINT('Ctrl Pts',(-0.677623694750723,-7.88192698305918,
-43.177816050527));
#64548=CARTESIAN_POINT('Ctrl Pts',(-0.668388570352403,-7.88271496618133,
-43.1774408935832));
#64549=CARTESIAN_POINT('Ctrl Pts',(-0.664217874932868,-7.8830674951776,
-43.1772712855331));
#64550=CARTESIAN_POINT('Ctrl Pts',(-0.655125647587734,-7.88382875096019,
-43.1769011403839));
#64551=CARTESIAN_POINT('Ctrl Pts',(-0.650204011696049,-7.88423617933624,
-43.1767005279892));
#64552=CARTESIAN_POINT('Ctrl Pts',(-0.636794170269173,-7.88533364612062,
-43.1761532437376));
#64553=CARTESIAN_POINT('Ctrl Pts',(-0.628305247794709,-7.88601458535544,
-43.1758060490336));
#64554=CARTESIAN_POINT('Ctrl Pts',(-0.587711649431648,-7.88920484114297,
-43.1741422796069));
#64555=CARTESIAN_POINT('Ctrl Pts',(-0.555593357254782,-7.89153178874744,
-43.1728154082782));
#64556=CARTESIAN_POINT('Ctrl Pts',(-0.0109578040255894,-7.92764887924346,
-43.1501482014188));
#64557=CARTESIAN_POINT('Ctrl Pts',(0.503595250355316,-7.91163922487543,
-43.1262839227008));
#64558=CARTESIAN_POINT('Ctrl Pts',(1.41864730434796,-7.79350558893383,-43.083260556332));
#64559=CARTESIAN_POINT('Ctrl Pts',(1.81973671019622,-7.70972666276991,-43.0641908228352));
#64560=CARTESIAN_POINT('Ctrl Pts',(2.5778771201574,-7.48887516573073,-43.0288557539893));
#64561=CARTESIAN_POINT('Ctrl Pts',(2.93506507778931,-7.35623188741114,-43.0125304885158));
#64562=CARTESIAN_POINT('Ctrl Pts',(3.29836029107813,-7.19062512753387,-42.9963160462383));
#64563=CARTESIAN_POINT('Ctrl Pts',(3.31533969185014,-7.18281233698664,-42.9955590681318));
#64564=CARTESIAN_POINT('Ctrl Pts',(3.34250680367161,-7.17019498570641,-42.9943492132727));
#64565=CARTESIAN_POINT('Ctrl Pts',(3.35271216854238,-7.16542873678227,-42.9938950275704));
#64566=CARTESIAN_POINT('Ctrl Pts',(3.37215287073074,-7.1562986487085,-42.9930303859468));
#64567=CARTESIAN_POINT('Ctrl Pts',(3.38138999860773,-7.15193868901353,-42.992619798255));
#64568=CARTESIAN_POINT('Ctrl Pts',(3.39771488630759,-7.14419458296152,-42.9918945818404));
#64569=CARTESIAN_POINT('Ctrl Pts',(3.40480608941857,-7.14081775301371,-42.9915797029703));
#64570=CARTESIAN_POINT('Ctrl Pts',(3.41862015561495,-7.13421424121544,-42.9909665715115));
#64571=CARTESIAN_POINT('Ctrl Pts',(3.42534350623976,-7.13098860415294,-42.9906682835995));
#64572=CARTESIAN_POINT('Ctrl Pts',(3.44139280883428,-7.12326075460672,-42.9899565359143));
#64573=CARTESIAN_POINT('Ctrl Pts',(3.45071451247693,-7.11874972149438,-42.9895433793226));
#64574=CARTESIAN_POINT('Ctrl Pts',(3.48407754469506,-7.10252348758256,-42.9880655004954));
#64575=CARTESIAN_POINT('Ctrl Pts',(3.50806841229001,-7.09070463786781,-42.9870043410509));
#64576=CARTESIAN_POINT('Ctrl Pts',(3.87878355785397,-6.90573371863429,-42.9706298022709));
#64577=CARTESIAN_POINT('Ctrl Pts',(4.21239776005106,-6.70744840797596,-42.9562404715785));
#64578=CARTESIAN_POINT('Ctrl Pts',(4.69710314179151,-6.36887835826286,-42.9351127020209));
#64579=CARTESIAN_POINT('Ctrl Pts',(4.85948458113003,-6.24586276344972,-42.927985190256));
#64580=CARTESIAN_POINT('Ctrl Pts',(5.36167160179725,-5.83396819690105,-42.9054037916875));
#64581=CARTESIAN_POINT('Ctrl Pts',(5.68186560095015,-5.52259660427665,-42.8901979887975));
#64582=CARTESIAN_POINT('Ctrl Pts',(6.02580563033462,-5.12638333944188,-42.8709312177263));
#64583=CARTESIAN_POINT('Ctrl Pts',(6.0766057020977,-5.06606378741388,-42.8679990555525));
#64584=CARTESIAN_POINT('Ctrl Pts',(6.2065704002251,-4.9069771477098,-42.8602421887724));
#64585=CARTESIAN_POINT('Ctrl Pts',(6.28427293798439,-4.80706265987731,-42.8553375129544));
#64586=CARTESIAN_POINT('Ctrl Pts',(6.37659033729413,-4.68228979851745,-42.8491728299081));
#64587=CARTESIAN_POINT('Ctrl Pts',(6.39350819288933,-4.65916248363337,-42.8480289505576));
#64588=CARTESIAN_POINT('Ctrl Pts',(6.4167667466558,-4.62700197731813,-42.8464370736674));
#64589=CARTESIAN_POINT('Ctrl Pts',(6.42321486648299,-4.61804650871885,-42.8459936672717));
#64590=CARTESIAN_POINT('Ctrl Pts',(6.43408355269712,-4.60288473636843,-42.8452427854875));
#64591=CARTESIAN_POINT('Ctrl Pts',(6.43851393899757,-4.59668547066967,-42.8449357163325));
#64592=CARTESIAN_POINT('Ctrl Pts',(6.44727587630592,-4.58438771579683,-42.8443264780818));
#64593=CARTESIAN_POINT('Ctrl Pts',(6.45160774841539,-4.57828946377511,-42.8440243224111));
#64594=CARTESIAN_POINT('Ctrl Pts',(6.46115570408235,-4.56480773865446,-42.843356245642));
#64595=CARTESIAN_POINT('Ctrl Pts',(6.46636779077903,-4.55742145482825,-42.8429901674711));
#64596=CARTESIAN_POINT('Ctrl Pts',(6.48462145688415,-4.53145900544274,-42.8417032575424));
#64597=CARTESIAN_POINT('Ctrl Pts',(6.49759568525072,-4.51283574453198,-42.8407798473039));
#64598=CARTESIAN_POINT('Ctrl Pts',(6.7058668329626,-4.21112240394115,-42.8258176819473));
#64599=CARTESIAN_POINT('Ctrl Pts',(6.88257305811105,-3.91565741047275,-42.8111555985502));
#64600=CARTESIAN_POINT('Ctrl Pts',(7.32939738187478,-3.04426657739399,-42.7691109407579));
#64601=CARTESIAN_POINT('Ctrl Pts',(7.55015820567726,-2.44597837343103,-42.7418377464457));
#64602=CARTESIAN_POINT('Ctrl Pts',(7.79036741386173,-1.43440792637692,-42.6985816283015));
#64603=CARTESIAN_POINT('Ctrl Pts',(7.85348377275889,-1.03448450679828,-42.6819747236043));
#64604=CARTESIAN_POINT('Ctrl Pts',(7.88989833998355,-0.579757523518488,
-42.6634871925656));
#64605=CARTESIAN_POINT('Ctrl Pts',(7.89353203978945,-0.527983505120561,
-42.6613889208779));
#64606=CARTESIAN_POINT('Ctrl Pts',(7.89826098626518,-0.449561317177088,
-42.658220666819));
#64607=CARTESIAN_POINT('Ctrl Pts',(7.89973138660155,-0.422937360300898,
-42.6571468006313));
#64608=CARTESIAN_POINT('Ctrl Pts',(7.90204711831214,-0.376769166245137,
-42.6552876078282));
#64609=CARTESIAN_POINT('Ctrl Pts',(7.90295461202745,-0.357228312644079,
-42.654501623179));
#64610=CARTESIAN_POINT('Ctrl Pts',(7.90469252431315,-0.316550985936338,
-42.6528673768239));
#64611=CARTESIAN_POINT('Ctrl Pts',(7.90551066800371,-0.295414136178893,
-42.6520192547414));
#64612=CARTESIAN_POINT('Ctrl Pts',(7.9075301542098,-0.237200314182017,-42.6496863048612));
#64613=CARTESIAN_POINT('Ctrl Pts',(7.90855549702967,-0.200117706100361,
-42.6482034356713));
#64614=CARTESIAN_POINT('Ctrl Pts',(7.9115948087887,-0.0526662218354875,
-42.6423195051316));
#64615=CARTESIAN_POINT('Ctrl Pts',(7.91155948451444,0.0577331483655337,
-42.6379419032013));
#64616=CARTESIAN_POINT('Ctrl Pts',(7.89391523870753,0.8879231308623,-42.6051961937961));
#64617=CARTESIAN_POINT('Ctrl Pts',(7.78042415335899,1.6022601279125,-42.5783315359479));
#64618=CARTESIAN_POINT('Ctrl Pts',(7.54482416140158,2.38081669756805,-42.5463174223513));
#64619=CARTESIAN_POINT('Ctrl Pts',(7.5161647671828,2.46980292231212,-42.5426107179413));
#64620=CARTESIAN_POINT('Ctrl Pts',(7.47940883772384,2.57735752075816,-42.5380571001372));
#64621=CARTESIAN_POINT('Ctrl Pts',(7.47280907061646,2.59643080831596,-42.5372467271813));
#64622=CARTESIAN_POINT('Ctrl Pts',(7.46212823934856,2.62692027162976,-42.5359466306197));
#64623=CARTESIAN_POINT('Ctrl Pts',(7.45809383883152,2.63835256626456,-42.5354581025129));
#64624=CARTESIAN_POINT('Ctrl Pts',(7.450342210185,2.66015852559232,-42.5345243193796));
#64625=CARTESIAN_POINT('Ctrl Pts',(7.44662955301984,2.67053379108492,-42.5340791748039));
#64626=CARTESIAN_POINT('Ctrl Pts',(7.43808535272337,2.6942547646898,-42.533059521074));
#64627=CARTESIAN_POINT('Ctrl Pts',(7.43323955134159,2.70759528400082,-42.5324846816955));
#64628=CARTESIAN_POINT('Ctrl Pts',(7.41854954427258,2.74770029378803,-42.5307524527797));
#64629=CARTESIAN_POINT('Ctrl Pts',(7.40859652532278,2.77442458105489,-42.5295926432102));
#64630=CARTESIAN_POINT('Ctrl Pts',(7.31017698971493,3.03437900319004,-42.5182589680592));
#64631=CARTESIAN_POINT('Ctrl Pts',(7.21087222326577,3.26335103575648,-42.5078715040871));
#64632=CARTESIAN_POINT('Ctrl Pts',(6.90618907627086,3.88376392751844,-42.4789133209328));
#64633=CARTESIAN_POINT('Ctrl Pts',(6.67858280134164,4.26328689410199,-42.4602908977703));
#64634=CARTESIAN_POINT('Ctrl Pts',(6.29175713444509,4.80065246838734,-42.4329001559247));
#64635=CARTESIAN_POINT('Ctrl Pts',(6.15560975979426,4.97402691950493,-42.4238745544273));
#64636=CARTESIAN_POINT('Ctrl Pts',(5.97962108093384,5.17982591499766,-42.4128993836702));
#64637=CARTESIAN_POINT('Ctrl Pts',(5.94647597165847,5.21784326520502,-42.4108602468522));
#64638=CARTESIAN_POINT('Ctrl Pts',(5.89331773442231,5.27765119372362,-42.4076328801001));
#64639=CARTESIAN_POINT('Ctrl Pts',(5.87354212186838,5.29965083680797,-42.406441476891));
#64640=CARTESIAN_POINT('Ctrl Pts',(5.83602086554149,5.34092386999577,-42.4041980422957));
#64641=CARTESIAN_POINT('Ctrl Pts',(5.8183019764274,5.36022102572518,-42.4031456696459));
#64642=CARTESIAN_POINT('Ctrl Pts',(5.77801988167561,5.403656072691,-42.400768891833));
#64643=CARTESIAN_POINT('Ctrl Pts',(5.75540063243217,5.4277413604217,-42.3994452552681));
#64644=CARTESIAN_POINT('Ctrl Pts',(5.69641596879597,5.48976573660764,-42.396021350378));
#64645=CARTESIAN_POINT('Ctrl Pts',(5.65982214910994,5.52748550538911,-42.3939241179831));
#64646=CARTESIAN_POINT('Ctrl Pts',(5.45356060024357,5.73589746656889,-42.3822472723453));
#64647=CARTESIAN_POINT('Ctrl Pts',(5.27654490396205,5.89914566053216,-42.3727492807683));
#64648=CARTESIAN_POINT('Ctrl Pts',(4.45861384018537,6.58714590047324,-42.3309024817012));
#64649=CARTESIAN_POINT('Ctrl Pts',(3.74512058442697,7.01738825772705,-42.3007233616847));
#64650=CARTESIAN_POINT('Ctrl Pts',(2.80078388928725,7.40108732751654,-42.2624410359698));
#64651=CARTESIAN_POINT('Ctrl Pts',(2.6210871998957,7.46661782343709,-42.2551794897459));
#64652=CARTESIAN_POINT('Ctrl Pts',(2.35926653111254,7.55147951529407,-42.2444507851027));
#64653=CARTESIAN_POINT('Ctrl Pts',(2.27892776614147,7.57611174093569,-42.2411387322165));
#64654=CARTESIAN_POINT('Ctrl Pts',(2.18387550933831,7.60360648255676,-42.2371825647751));
#64655=CARTESIAN_POINT('Ctrl Pts',(2.169525771373,7.60771330332445,-42.2365843118217));
#64656=CARTESIAN_POINT('Ctrl Pts',(2.14750082524071,7.61394934621418,-42.2356644294713));
#64657=CARTESIAN_POINT('Ctrl Pts',(2.13983383837818,7.61610764004155,-42.2353439092076));
#64658=CARTESIAN_POINT('Ctrl Pts',(2.12644992670361,7.61985347055614,-42.2347838411365));
#64659=CARTESIAN_POINT('Ctrl Pts',(2.12073444404472,7.62144616336766,-42.2345444940052));
#64660=CARTESIAN_POINT('Ctrl Pts',(2.10786264490656,7.62501745558707,-42.2340050582863));
#64661=CARTESIAN_POINT('Ctrl Pts',(2.10070532950367,7.62699241155473,-42.2337048263829));
#64662=CARTESIAN_POINT('Ctrl Pts',(2.08152709347011,7.63225532018683,-42.2328995713882));
#64663=CARTESIAN_POINT('Ctrl Pts',(2.0695011953893,7.63552494025853,-42.2323938138036));
#64664=CARTESIAN_POINT('Ctrl Pts',(2.01741481335839,7.64955417551561,-42.2301995818011));
#64665=CARTESIAN_POINT('Ctrl Pts',(1.97727826212934,7.66002690558088,-42.2284992895499));
#64666=CARTESIAN_POINT('Ctrl Pts',(1.31687324853165,7.82680848588956,-42.2003422356022));
#64667=CARTESIAN_POINT('Ctrl Pts',(0.680064371117668,7.90761519724527,-42.1703841306729));
#64668=CARTESIAN_POINT('Ctrl Pts',(-0.324571243112215,7.91276924241778,
-42.124250103043));
#64669=CARTESIAN_POINT('Ctrl Pts',(-0.68943928843699,7.88935795499171,-42.1077049519506));
#64670=CARTESIAN_POINT('Ctrl Pts',(-1.24063437403823,7.81544619761173,-42.0834857769178));
#64671=CARTESIAN_POINT('Ctrl Pts',(-1.42889093076588,7.78322875417702,-42.0753489547174));
#64672=CARTESIAN_POINT('Ctrl Pts',(-1.71081449990175,7.72440640722361,-42.0633790781107));
#64673=CARTESIAN_POINT('Ctrl Pts',(-1.8054522319059,7.70283607999391,-42.0593977226977));
#64674=CARTESIAN_POINT('Ctrl Pts',(-1.91725887444196,7.67517867280289,-42.0547359906525));
#64675=CARTESIAN_POINT('Ctrl Pts',(-1.9348315368889,7.67076763957507,-42.054004537019));
#64676=CARTESIAN_POINT('Ctrl Pts',(-1.96185039238002,7.66388670078803,-42.0528817605837));
#64677=CARTESIAN_POINT('Ctrl Pts',(-1.97130737246376,7.6614596239034,-42.0524891262482));
#64678=CARTESIAN_POINT('Ctrl Pts',(-1.98784179670236,7.65718352265487,-42.0518032641221));
#64679=CARTESIAN_POINT('Ctrl Pts',(-1.99492120546629,7.65534217998639,-42.051509801001));
#64680=CARTESIAN_POINT('Ctrl Pts',(-2.01090158223136,7.65116203745574,-42.0508478073153));
#64681=CARTESIAN_POINT('Ctrl Pts',(-2.01980105009127,7.64881751747142,-42.0504794529638));
#64682=CARTESIAN_POINT('Ctrl Pts',(-2.04374421603517,7.64246510979039,-42.0494892578281));
#64683=CARTESIAN_POINT('Ctrl Pts',(-2.05878024103004,7.63842832639485,-42.048868306663));
#64684=CARTESIAN_POINT('Ctrl Pts',(-2.1248173697459,7.62048991217921,-42.0461449430197));
#64685=CARTESIAN_POINT('Ctrl Pts',(-2.17569082962811,7.60612154126863,-42.0440569366472));
#64686=CARTESIAN_POINT('Ctrl Pts',(-3.11149686375139,7.3316613245939,-42.0058219162382));
#64687=CARTESIAN_POINT('Ctrl Pts',(-3.9442575466547,6.91934799402131,-41.9756397270761));
#64688=CARTESIAN_POINT('Ctrl Pts',(-4.96486456524271,6.16869655541085,-41.9307579717741));
#64689=CARTESIAN_POINT('Ctrl Pts',(-5.22884871016925,5.94658088533544,-41.9181276287174));
#64690=CARTESIAN_POINT('Ctrl Pts',(-5.48938088826067,5.69656823412778,-41.9037092138061));
#64691=CARTESIAN_POINT('Ctrl Pts',(-5.50122696005389,5.68512920787922,-41.9030492676399));
#64692=CARTESIAN_POINT('Ctrl Pts',(-5.51841110818064,5.66843152801336,-41.9020856935766));
#64693=CARTESIAN_POINT('Ctrl Pts',(-5.52377762029411,5.66320209313052,-41.9017838837749));
#64694=CARTESIAN_POINT('Ctrl Pts',(-5.5331612756938,5.65403209777566,-41.9012546028455));
#64695=CARTESIAN_POINT('Ctrl Pts',(-5.53718166541381,5.65009485491111,-41.9010273348866));
#64696=CARTESIAN_POINT('Ctrl Pts',(-5.54496484835306,5.64245635238092,-41.9005863974892));
#64697=CARTESIAN_POINT('Ctrl Pts',(-5.54872814585027,5.63875560928773,-41.9003727592979));
#64698=CARTESIAN_POINT('Ctrl Pts',(-5.5576798519271,5.62993506139776,-41.8998635440783));
#64699=CARTESIAN_POINT('Ctrl Pts',(-5.56286488711169,5.62481185278913,-41.8995677634699));
#64700=CARTESIAN_POINT('Ctrl Pts',(-5.58125707950899,5.60658866436246,-41.8985156473082));
#64701=CARTESIAN_POINT('Ctrl Pts',(-5.59442504002702,5.59344933849766,-41.897756996418));
#64702=CARTESIAN_POINT('Ctrl Pts',(-5.82952261943001,5.35720233424159,-41.8841174553474));
#64703=CARTESIAN_POINT('Ctrl Pts',(-6.0379808617838,5.12110506706688,-41.8705177038608));
#64704=CARTESIAN_POINT('Ctrl Pts',(-6.68964401530127,4.28776942123393,-41.8241878296159));
#64705=CARTESIAN_POINT('Ctrl Pts',(-7.06276121718457,3.64059938964207,-41.7913266625748));
#64706=CARTESIAN_POINT('Ctrl Pts',(-7.37253253740109,2.87006393643871,-41.7573027399143));
#64707=CARTESIAN_POINT('Ctrl Pts',(-7.40367628172029,2.78874181438626,-41.7537629951243));
#64708=CARTESIAN_POINT('Ctrl Pts',(-7.4419800249354,2.68355596750651,-41.7492455813139));
#64709=CARTESIAN_POINT('Ctrl Pts',(-7.45037831651982,2.66015079861557,-41.7482442416188));
#64710=CARTESIAN_POINT('Ctrl Pts',(-7.46375304019118,2.62231662760657,-41.7466316218151));
#64711=CARTESIAN_POINT('Ctrl Pts',(-7.4687982924261,2.60791219356127,-41.7460190623004));
#64712=CARTESIAN_POINT('Ctrl Pts',(-7.47834891983583,2.58038966288955,-41.7448512812874));
#64713=CARTESIAN_POINT('Ctrl Pts',(-7.48286154058232,2.56727414683741,-41.7442959290753));
#64714=CARTESIAN_POINT('Ctrl Pts',(-7.49310971916191,2.53723217992936,-41.7430264194268));
#64715=CARTESIAN_POINT('Ctrl Pts',(-7.49882246338263,2.52029801091779,-41.7423126743188));
#64716=CARTESIAN_POINT('Ctrl Pts',(-7.51580419970742,2.46939049161486,-41.7401724560626));
#64717=CARTESIAN_POINT('Ctrl Pts',(-7.5269001007057,2.43535973984098,-41.738748997024));
#64718=CARTESIAN_POINT('Ctrl Pts',(-7.59778237742529,2.2128536026966,-41.729487243481));
#64719=CARTESIAN_POINT('Ctrl Pts',(-7.65071676690429,2.0222647615266,-41.7217693942327));
#64720=CARTESIAN_POINT('Ctrl Pts',(-7.7264090630307,1.70390519075901,-41.7091885546783));
#64721=CARTESIAN_POINT('Ctrl Pts',(-7.75326496031128,1.57720425805516,-41.7042609205742));
#64722=CARTESIAN_POINT('Ctrl Pts',(-7.86645885154126,0.970052656448543,
-41.6809599169124));
#64723=CARTESIAN_POINT('Ctrl Pts',(-7.91131610941931,0.482963186128997,
-41.6632635675703));
#64724=CARTESIAN_POINT('Ctrl Pts',(-7.91076872629169,-0.357807502292524,
-41.6321363169891));
#64725=CARTESIAN_POINT('Ctrl Pts',(-7.88695811714254,-0.710034828332207,
-41.6188952219463));
#64726=CARTESIAN_POINT('Ctrl Pts',(-7.83695990569885,-1.08000448836327,
-41.6039823309859));
#64727=CARTESIAN_POINT('Ctrl Pts',(-7.83410456311462,-1.10052530308577,
-41.6031518246918));
#64728=CARTESIAN_POINT('Ctrl Pts',(-7.8300008310785,-1.12919258889206,-41.6019867093645));
#64729=CARTESIAN_POINT('Ctrl Pts',(-7.82882025987236,-1.13734878356024,
-41.6016546636447));
#64730=CARTESIAN_POINT('Ctrl Pts',(-7.82675654894313,-1.15145084866713,
-41.6010795763058));
#64731=CARTESIAN_POINT('Ctrl Pts',(-7.82587937179862,-1.15739759423216,
-41.6008367642765));
#64732=CARTESIAN_POINT('Ctrl Pts',(-7.82404689701327,-1.16972336815349,
-41.6003328558814));
#64733=CARTESIAN_POINT('Ctrl Pts',(-7.82309057415665,-1.17610223742525,
-41.6000717197172));
#64734=CARTESIAN_POINT('Ctrl Pts',(-7.82083181453331,-1.19104397397079,
-41.5994592027343));
#64735=CARTESIAN_POINT('Ctrl Pts',(-7.81952311595772,-1.19960587584501,
-41.5991075745614));
#64736=CARTESIAN_POINT('Ctrl Pts',(-7.81524751667815,-1.22727384797813,
-41.5979691581138));
#64737=CARTESIAN_POINT('Ctrl Pts',(-7.81222464552318,-1.24637110190474,
-41.5971801164791));
#64738=CARTESIAN_POINT('Ctrl Pts',(-7.76506238628768,-1.53740928744274,
-41.5851032634546));
#64739=CARTESIAN_POINT('Ctrl Pts',(-7.70682706740391,-1.8068159369177,-41.5731273577745));
#64740=CARTESIAN_POINT('Ctrl Pts',(-7.39067179809481,-2.97141330746483,
-41.518976943685));
#64741=CARTESIAN_POINT('Ctrl Pts',(-6.98973801243016,-3.82043105359153,
-41.4746626591274));
#64742=CARTESIAN_POINT('Ctrl Pts',(-6.42203612067811,-4.61992987645502,
-41.4345250705146));
#64743=CARTESIAN_POINT('Ctrl Pts',(-6.39342979444065,-4.65943725968026,
-41.4325429584003));
#64744=CARTESIAN_POINT('Ctrl Pts',(-6.355932258651,-4.71022847118526,-41.4299961854272));
#64745=CARTESIAN_POINT('Ctrl Pts',(-6.34737349090102,-4.7217557007161,-41.429418284439));
#64746=CARTESIAN_POINT('Ctrl Pts',(-6.33370728516738,-4.74005748947649,
-41.4285008955895));
#64747=CARTESIAN_POINT('Ctrl Pts',(-6.32862026800039,-4.74684721491845,
-41.4281605881106));
#64748=CARTESIAN_POINT('Ctrl Pts',(-6.31947145713717,-4.75901743533498,
-41.4275506596682));
#64749=CARTESIAN_POINT('Ctrl Pts',(-6.31541369367337,-4.76440094087907,
-41.4272808766064));
#64750=CARTESIAN_POINT('Ctrl Pts',(-6.30592566202864,-4.7769554588536,-41.4266517763668));
#64751=CARTESIAN_POINT('Ctrl Pts',(-6.30049002975001,-4.78412241656116,
-41.4262926767733));
#64752=CARTESIAN_POINT('Ctrl Pts',(-6.28493897714689,-4.80455422807314,
-41.4252690313776));
#64753=CARTESIAN_POINT('Ctrl Pts',(-6.27479377954778,-4.81779641595894,
-41.4246056966922));
#64754=CARTESIAN_POINT('Ctrl Pts',(-6.21024598295809,-4.9014987590468,-41.420413421678));
#64755=CARTESIAN_POINT('Ctrl Pts',(-6.15469823776888,-4.97106985728453,
-41.4169316677854));
#64756=CARTESIAN_POINT('Ctrl Pts',(-5.98783674302622,-5.17297100070451,
-41.4068269341414));
#64757=CARTESIAN_POINT('Ctrl Pts',(-5.87334332640912,-5.30260882812959,
-41.4003394388996));
#64758=CARTESIAN_POINT('Ctrl Pts',(-5.51311335384148,-5.68449171454556,
-41.3811231561032));
#64759=CARTESIAN_POINT('Ctrl Pts',(-5.25470414713677,-5.9241851063745,-41.368931342189));
#64760=CARTESIAN_POINT('Ctrl Pts',(-4.8717255247844,-6.23458583329594,-41.3522139742931));
#64761=CARTESIAN_POINT('Ctrl Pts',(-4.75992306688475,-6.3203562264405,-41.347476428427));
#64762=CARTESIAN_POINT('Ctrl Pts',(-4.5212483824416,-6.49353125105699,-41.3375591025633));
#64763=CARTESIAN_POINT('Ctrl Pts',(-4.39399410028985,-6.58030775967649,
-41.3323813808221));
#64764=CARTESIAN_POINT('Ctrl Pts',(-3.902524625278,-6.89483113864197,-41.3125343122149));
#64765=CARTESIAN_POINT('Ctrl Pts',(-3.52254227305133,-7.09647878512309,
-41.2975081062685));
#64766=CARTESIAN_POINT('Ctrl Pts',(-3.10239720792502,-7.27735097823584,
-41.279398939432));
#64767=CARTESIAN_POINT('Ctrl Pts',(-3.07660938110214,-7.28829063457542,
-41.2782816083009));
#64768=CARTESIAN_POINT('Ctrl Pts',(-3.04353794050842,-7.30211333435504,
-41.27684063205));
#64769=CARTESIAN_POINT('Ctrl Pts',(-3.03630711301348,-7.30512295979145,
-41.2765250817361));
#64770=CARTESIAN_POINT('Ctrl Pts',(-3.02479018188331,-7.30989649979695,
-41.2760216886902));
#64771=CARTESIAN_POINT('Ctrl Pts',(-3.02050696036158,-7.31166740110527,
-41.2758342978797));
#64772=CARTESIAN_POINT('Ctrl Pts',(-3.0125027957268,-7.31496849567399,-41.2754837837171));
#64773=CARTESIAN_POINT('Ctrl Pts',(-3.00878223459501,-7.31649961741468,
-41.2753207209106));
#64774=CARTESIAN_POINT('Ctrl Pts',(-3.00049607188368,-7.31990223089548,
-41.2749572579134));
#64775=CARTESIAN_POINT('Ctrl Pts',(-2.99592991523275,-7.3217722779518,-41.2747567646821));
#64776=CARTESIAN_POINT('Ctrl Pts',(-2.98245821438458,-7.32727483465932,
-41.2741646376998));
#64777=CARTESIAN_POINT('Ctrl Pts',(-2.9735478616077,-7.33089534888164,-41.2737722220114));
#64778=CARTESIAN_POINT('Ctrl Pts',(-2.90402533921412,-7.35899660110856,
-41.2707045235178));
#64779=CARTESIAN_POINT('Ctrl Pts',(-2.84312010567347,-7.38274080015654,
-41.2679821594313));
#64780=CARTESIAN_POINT('Ctrl Pts',(-2.6336961820862,-7.46140999598996,-41.2585219952544));
#64781=CARTESIAN_POINT('Ctrl Pts',(-2.48383209146895,-7.51262719897673,
-41.2515833670681));
#64782=CARTESIAN_POINT('Ctrl Pts',(-1.82795972718848,-7.71500666962809,
-41.2208278000417));
#64783=CARTESIAN_POINT('Ctrl Pts',(-1.30906271879428,-7.81979113584119,
-41.1956137530407));
#64784=CARTESIAN_POINT('Ctrl Pts',(-0.268294000585628,-7.92338943159521,
-41.1474663403125));
#64785=CARTESIAN_POINT('Ctrl Pts',(0.250847845163416,-7.92396995462643,
-41.1246286101601));
#64786=CARTESIAN_POINT('Ctrl Pts',(0.799336731662875,-7.87058304382767,
-41.1022369240626));
#64787=CARTESIAN_POINT('Ctrl Pts',(0.832261621015753,-7.86716958581137,
-41.1008989568986));
#64788=CARTESIAN_POINT('Ctrl Pts',(0.877073872558543,-7.86223924683237,
-41.0990861907204));
#64789=CARTESIAN_POINT('Ctrl Pts',(0.888980385718612,-7.86090188387578,
-41.098605338419));
#64790=CARTESIAN_POINT('Ctrl Pts',(0.907800778729958,-7.8587446337576,-41.0978465136171));
#64791=CARTESIAN_POINT('Ctrl Pts',(0.914716668260801,-7.85794266265786,
-41.0975679367006));
#64792=CARTESIAN_POINT('Ctrl Pts',(0.928080612388626,-7.85637508907095,
-41.0970301409965));
#64793=CARTESIAN_POINT('Ctrl Pts',(0.934528799367214,-7.85561067560656,
-41.096770882297));
#64794=CARTESIAN_POINT('Ctrl Pts',(0.949810635946557,-7.85377997692017,
-41.0961569993789));
#64795=CARTESIAN_POINT('Ctrl Pts',(0.958643451263589,-7.85270672469646,
-41.0958026106864));
#64796=CARTESIAN_POINT('Ctrl Pts',(0.98463001658667,-7.84950466668104,-41.0947612461403));
#64797=CARTESIAN_POINT('Ctrl Pts',(1.00177867503754,-7.84733453302721,-41.0940756661462));
#64798=CARTESIAN_POINT('Ctrl Pts',(1.1321533298797,-7.83040151431789,-41.0888756386054));
#64799=CARTESIAN_POINT('Ctrl Pts',(1.24505756276356,-7.81324466076694,-41.084442602824));
#64800=CARTESIAN_POINT('Ctrl Pts',(1.66026340928925,-7.74092110546754,-41.0683689060161));
#64801=CARTESIAN_POINT('Ctrl Pts',(1.95965581483859,-7.6705999017265,-41.057242764371));
#64802=CARTESIAN_POINT('Ctrl Pts',(2.67903312191313,-7.45675001650187,-41.0309321763449));
#64803=CARTESIAN_POINT('Ctrl Pts',(3.09247466664108,-7.2949935885172,-41.0162025780311));
#64804=CARTESIAN_POINT('Ctrl Pts',(3.83095984203199,-6.9319444573193,-40.9878090161078));
#64805=CARTESIAN_POINT('Ctrl Pts',(4.15919029753097,-6.74011754176666,-40.9743090227546));
#64806=CARTESIAN_POINT('Ctrl Pts',(4.49273176996395,-6.51152004123016,-40.9582659505304));
#64807=CARTESIAN_POINT('Ctrl Pts',(4.51305539053108,-6.49745050214394,-40.9572786453223));
#64808=CARTESIAN_POINT('Ctrl Pts',(4.53958882484194,-6.47889751051672,-40.9559763704938));
#64809=CARTESIAN_POINT('Ctrl Pts',(4.54585866408004,-6.4744998768867,-40.9556676672064));
#64810=CARTESIAN_POINT('Ctrl Pts',(4.55557823238001,-6.46766154234924,-40.955187608314));
#64811=CARTESIAN_POINT('Ctrl Pts',(4.55903242330815,-6.46522715925784,-40.955016707087));
#64812=CARTESIAN_POINT('Ctrl Pts',(4.56594159770817,-6.46034954415488,-40.9546742766365));
#64813=CARTESIAN_POINT('Ctrl Pts',(4.56939657487203,-6.45790630527874,-40.9545027469217));
#64814=CARTESIAN_POINT('Ctrl Pts',(4.57709992751761,-6.4524494871278,-40.9541196417457));
#64815=CARTESIAN_POINT('Ctrl Pts',(4.58134728702753,-6.44943448418638,-40.9539079652952));
#64816=CARTESIAN_POINT('Ctrl Pts',(4.59373884826159,-6.44061987371016,-40.9532891102286));
#64817=CARTESIAN_POINT('Ctrl Pts',(4.6018750108861,-6.43480903726657,-40.9528811419198));
#64818=CARTESIAN_POINT('Ctrl Pts',(4.66030443647288,-6.39291132725107,-40.9499396960017));
#64819=CARTESIAN_POINT('Ctrl Pts',(4.71018239314291,-6.35625157687396,-40.9473666070419));
#64820=CARTESIAN_POINT('Ctrl Pts',(4.86560163578552,-6.23918625096984,-40.9391652586494));
#64821=CARTESIAN_POINT('Ctrl Pts',(4.96954997766387,-6.15671131102497,-40.9334093786302));
#64822=CARTESIAN_POINT('Ctrl Pts',(5.41790949455732,-5.78221816854286,-40.9075463089138));
#64823=CARTESIAN_POINT('Ctrl Pts',(5.73901990692258,-5.46364479344847,-40.8862852593344));
#64824=CARTESIAN_POINT('Ctrl Pts',(6.13601470784765,-4.99594659755881,-40.8577281434779));
#64825=CARTESIAN_POINT('Ctrl Pts',(6.23702158898411,-4.86926302251088,-40.8502202551786));
#64826=CARTESIAN_POINT('Ctrl Pts',(6.64362247519964,-4.32587183079825,-40.8191037278331));
#64827=CARTESIAN_POINT('Ctrl Pts',(6.91193388103915,-3.88280672604363,-40.7964197138117));
#64828=CARTESIAN_POINT('Ctrl Pts',(7.14932570246748,-3.38705502601568,-40.7740441729964));
#64829=CARTESIAN_POINT('Ctrl Pts',(7.16332630974431,-3.35734358730521,-40.7727135281773));
#64830=CARTESIAN_POINT('Ctrl Pts',(7.1824213615432,-3.3161577080871,-40.7708831225569));
#64831=CARTESIAN_POINT('Ctrl Pts',(7.18767403781135,-3.30475725094974,-40.7703779455581));
#64832=CARTESIAN_POINT('Ctrl Pts',(7.19601572168429,-3.28653841659955,-40.7695729943519));
#64833=CARTESIAN_POINT('Ctrl Pts',(7.19912221367841,-3.27972809595844,-40.7692726237954));
#64834=CARTESIAN_POINT('Ctrl Pts',(7.20548636568614,-3.26572344271429,-40.7686560216634));
#64835=CARTESIAN_POINT('Ctrl Pts',(7.20874292863689,-3.25852861882229,-40.7683398276544));
#64836=CARTESIAN_POINT('Ctrl Pts',(7.21625171008556,-3.24187289174032,-40.767609193049));
#64837=CARTESIAN_POINT('Ctrl Pts',(7.22049611052776,-3.23240846868263,-40.7671950182692));
#64838=CARTESIAN_POINT('Ctrl Pts',(7.23378083681923,-3.2026286462558,-40.7658949421695));
#64839=CARTESIAN_POINT('Ctrl Pts',(7.24275416643337,-3.18228338394865,-40.7650113090593));
#64840=CARTESIAN_POINT('Ctrl Pts',(7.37195678710983,-2.88596440786888,-40.7522071293867));
#64841=CARTESIAN_POINT('Ctrl Pts',(7.47642934830995,-2.60337517850799,-40.7408337454558));
#64842=CARTESIAN_POINT('Ctrl Pts',(7.78609698742599,-1.59171639857824,-40.7022504797429));
#64843=CARTESIAN_POINT('Ctrl Pts',(7.90260401769231,-0.839968278326332,
-40.6776529256632));
#64844=CARTESIAN_POINT('Ctrl Pts',(7.91270903614201,0.120915433268998,-40.6422210643717));
#64845=CARTESIAN_POINT('Ctrl Pts',(7.90695646312843,0.324992131708635,-40.6344159645815));
#64846=CARTESIAN_POINT('Ctrl Pts',(7.89192805825546,0.549385791618619,-40.6254484076656));
#64847=CARTESIAN_POINT('Ctrl Pts',(7.89045703498724,0.570123665650544,-40.6246164632991));
#64848=CARTESIAN_POINT('Ctrl Pts',(7.8881886719457,0.600410093513533,-40.6233969909907));
#64849=CARTESIAN_POINT('Ctrl Pts',(7.88745569659465,0.609963472639379,-40.6230116778194));
#64850=CARTESIAN_POINT('Ctrl Pts',(7.88612724313967,0.626875271386329,-40.6223284515789));
#64851=CARTESIAN_POINT('Ctrl Pts',(7.88553881639428,0.634234243475945,-40.6220307752064));
#64852=CARTESIAN_POINT('Ctrl Pts',(7.88430985428062,0.649337747093043,-40.6214190609975));
#64853=CARTESIAN_POINT('Ctrl Pts',(7.88366820695913,0.657082179199908,-40.6211049869075));
#64854=CARTESIAN_POINT('Ctrl Pts',(7.88200451251843,0.676809048514088,-40.6203039311986));
#64855=CARTESIAN_POINT('Ctrl Pts',(7.88096655331049,0.688790104042845,-40.6198164383797));
#64856=CARTESIAN_POINT('Ctrl Pts',(7.87864554482095,0.714889040092531,-40.6187524379704));
#64857=CARTESIAN_POINT('Ctrl Pts',(7.87735185983723,0.729005921937583,-40.6181756008765));
#64858=CARTESIAN_POINT('Ctrl Pts',(7.87350191834591,0.769809896595038,-40.6165045820007));
#64859=CARTESIAN_POINT('Ctrl Pts',(7.87084794943553,0.796487460580511,-40.6154074865756));
#64860=CARTESIAN_POINT('Ctrl Pts',(7.84072195577667,1.08444570913927,-40.6035186264793));
#64861=CARTESIAN_POINT('Ctrl Pts',(7.8003869403428,1.34420903164681,-40.592384305761));
#64862=CARTESIAN_POINT('Ctrl Pts',(7.67259103952429,1.96242783110019,-40.5653703836025));
#64863=CARTESIAN_POINT('Ctrl Pts',(7.57284101488135,2.31772737091015,-40.5494361751091));
#64864=CARTESIAN_POINT('Ctrl Pts',(7.35996956682926,2.91275300041657,-40.5224569150024));
#64865=CARTESIAN_POINT('Ctrl Pts',(7.25892752640277,3.15614614831353,-40.5113238892242));
#64866=CARTESIAN_POINT('Ctrl Pts',(7.12238311253849,3.44363072547556,-40.4980176937047));
#64867=CARTESIAN_POINT('Ctrl Pts',(7.09831877946582,3.49296497644646,-40.4957281640083));
#64868=CARTESIAN_POINT('Ctrl Pts',(6.89577504042249,3.89746078041413,-40.4768988231518));
#64869=CARTESIAN_POINT('Ctrl Pts',(6.69126657616328,4.2389714793584,-40.4605660371429));
#64870=CARTESIAN_POINT('Ctrl Pts',(6.43079143386363,4.60779355556764,-40.4422461420249));
#64871=CARTESIAN_POINT('Ctrl Pts',(6.39917319302399,4.65160428353957,-40.4400594651048));
#64872=CARTESIAN_POINT('Ctrl Pts',(6.35081871105179,4.71717882508442,-40.4367704530723));
#64873=CARTESIAN_POINT('Ctrl Pts',(6.33441400633733,4.73918490580629,-40.4356639256815));
#64874=CARTESIAN_POINT('Ctrl Pts',(6.30566793187097,4.77733039389061,-40.4337409891041));
#64875=CARTESIAN_POINT('Ctrl Pts',(6.29337831452153,4.79350843876057,-40.432923903403));
#64876=CARTESIAN_POINT('Ctrl Pts',(6.26754589871677,4.82724362936544,-40.4312168245302));
#64877=CARTESIAN_POINT('Ctrl Pts',(6.25399132618685,4.84479154818442,-40.4303269999983));
#64878=CARTESIAN_POINT('Ctrl Pts',(6.2215582331757,4.88641691385109,-40.4282117681163));
#64879=CARTESIAN_POINT('Ctrl Pts',(6.20261343387411,4.91044231248741,-40.4269872982482));
#64880=CARTESIAN_POINT('Ctrl Pts',(6.13793702241006,4.99149208024213,-40.4228440958205));
#64881=CARTESIAN_POINT('Ctrl Pts',(6.09155440947989,5.04799257975371,-40.4199348036114));
#64882=CARTESIAN_POINT('Ctrl Pts',(5.86635486834498,5.31469262296304,-40.406094940282));
#64883=CARTESIAN_POINT('Ctrl Pts',(5.67740130990779,5.51608529848486,-40.3953281644438));
#64884=CARTESIAN_POINT('Ctrl Pts',(5.14107604971754,6.03090110012436,-40.3665812496767));
#64885=CARTESIAN_POINT('Ctrl Pts',(4.77582654299774,6.32407255768823,-40.3488710249984));
#64886=CARTESIAN_POINT('Ctrl Pts',(4.28974959174131,6.64797588203683,-40.3259797207577));
#64887=CARTESIAN_POINT('Ctrl Pts',(4.1912355399102,6.71051999702798,-40.3213688298057));
#64888=CARTESIAN_POINT('Ctrl Pts',(4.07230449253366,6.78238554303078,-40.315807063516));
#64889=CARTESIAN_POINT('Ctrl Pts',(4.05318435206589,6.79382912205043,-40.3149130437107));
#64890=CARTESIAN_POINT('Ctrl Pts',(4.02331900479149,6.81153285413725,-40.3135165805301));
#64891=CARTESIAN_POINT('Ctrl Pts',(4.01260699002138,6.81784869145547,-40.3130157093874));
#64892=CARTESIAN_POINT('Ctrl Pts',(3.99326407303528,6.82919195878064,-40.3121113234708));
#64893=CARTESIAN_POINT('Ctrl Pts',(3.98463844732899,6.83422835514391,-40.3117080459762));
#64894=CARTESIAN_POINT('Ctrl Pts',(3.96493868402577,6.84568083059403,-40.3107870752994));
#64895=CARTESIAN_POINT('Ctrl Pts',(3.95385847661961,6.85208639378673,-40.3102691153952));
#64896=CARTESIAN_POINT('Ctrl Pts',(3.92300963252268,6.86982063524985,-40.3088272184641));
#64897=CARTESIAN_POINT('Ctrl Pts',(3.9032075719456,6.8810908132513,-40.3079018562612));
#64898=CARTESIAN_POINT('Ctrl Pts',(3.78974949869452,6.94501719558232,-40.3026016574966));
#64899=CARTESIAN_POINT('Ctrl Pts',(3.69507828950515,6.99584597562974,-40.2981860487181));
#64900=CARTESIAN_POINT('Ctrl Pts',(3.27083592900838,7.21260645710959,-40.278476415239));
#64901=CARTESIAN_POINT('Ctrl Pts',(2.93092971118178,7.35728937334601,-40.2629078050704));
#64902=CARTESIAN_POINT('Ctrl Pts',(2.17418842772657,7.61860388962891,-40.2293344260413));
#64903=CARTESIAN_POINT('Ctrl Pts',(1.7553462493612,7.72586583785553,-40.211434790284));
#64904=CARTESIAN_POINT('Ctrl Pts',(1.27823873834105,7.80722528306463,-40.1917919286573));
#64905=CARTESIAN_POINT('Ctrl Pts',(1.22655334363743,7.81551200072618,-40.1896730286218));
#64906=CARTESIAN_POINT('Ctrl Pts',(1.14205828081036,7.82820026321815,-40.1862229450668));
#64907=CARTESIAN_POINT('Ctrl Pts',(1.10929665281381,7.83290989512358,-40.1848886233092));
#64908=CARTESIAN_POINT('Ctrl Pts',(1.05054536920667,7.84097966552636,-40.1825015977743));
#64909=CARTESIAN_POINT('Ctrl Pts',(1.0245667795969,7.84441652435373,-40.1814481347195));
#64910=CARTESIAN_POINT('Ctrl Pts',(0.969267068633086,7.85145305060143,-40.1792098067353));
#64911=CARTESIAN_POINT('Ctrl Pts',(0.939941876738519,7.85501769139072,-40.1780253041434));
#64912=CARTESIAN_POINT('Ctrl Pts',(0.860551000913941,7.86421714103228,-40.174824892798));
#64913=CARTESIAN_POINT('Ctrl Pts',(0.810450232133061,7.86953808830135,-40.1728120465091));
#64914=CARTESIAN_POINT('Ctrl Pts',(0.557865441654368,7.89392612766439,-40.1626950192012));
#64915=CARTESIAN_POINT('Ctrl Pts',(0.354748409626442,7.90565863400223,-40.1546558608531));
#64916=CARTESIAN_POINT('Ctrl Pts',(-0.206941258283457,7.91641049302499,
-40.1325703480023));
#64917=CARTESIAN_POINT('Ctrl Pts',(-0.565346974519267,7.89890987858248,
-40.1187109082741));
#64918=CARTESIAN_POINT('Ctrl Pts',(-1.54237812293619,7.78434214235141,-40.081426527625));
#64919=CARTESIAN_POINT('Ctrl Pts',(-2.15255149708795,7.63815174885554,-40.0588693548574));
#64920=CARTESIAN_POINT('Ctrl Pts',(-2.77206934745137,7.40950650078815,-40.0336424348689));
#64921=CARTESIAN_POINT('Ctrl Pts',(-2.80494398026005,7.39712405551427,-40.0322957283807));
#64922=CARTESIAN_POINT('Ctrl Pts',(-2.8490165421248,7.38018778990801,-40.0304783840893));
#64923=CARTESIAN_POINT('Ctrl Pts',(-2.86028825044234,7.37582661094145,-40.0300125397745));
#64924=CARTESIAN_POINT('Ctrl Pts',(-2.87959047288601,7.36830741555266,-40.0292129428926));
#64925=CARTESIAN_POINT('Ctrl Pts',(-2.88762590664674,7.36516205418619,-40.0288795196797));
#64926=CARTESIAN_POINT('Ctrl Pts',(-2.9206916710006,7.35215647986442,-40.0275051503301));
#64927=CARTESIAN_POINT('Ctrl Pts',(-2.94567665703891,7.34218181187786,-40.0264611422381));
#64928=CARTESIAN_POINT('Ctrl Pts',(-3.04979054553636,7.29999981500444,-40.0220860566482));
#64929=CARTESIAN_POINT('Ctrl Pts',(-3.12844458258924,7.26663977228303,-40.0187212650157));
#64930=CARTESIAN_POINT('Ctrl Pts',(-3.219745101746,7.22615880643598,-40.0147306421476));
#64931=CARTESIAN_POINT('Ctrl Pts',(-3.23293287610872,7.22026832128495,-40.0141521318089));
#64932=CARTESIAN_POINT('Ctrl Pts',(-3.25399979638979,7.21078922747734,-40.013224537516));
#64933=CARTESIAN_POINT('Ctrl Pts',(-3.26188934387766,7.20722372800899,-40.0128763784793));
#64934=CARTESIAN_POINT('Ctrl Pts',(-3.27583979412024,7.20089154427038,-40.0122593593607));
#64935=CARTESIAN_POINT('Ctrl Pts',(-3.28190309245019,7.19813013778664,-40.0119907156508));
#64936=CARTESIAN_POINT('Ctrl Pts',(-3.29354234473155,7.19281151248553,-40.0114741092385));
#64937=CARTESIAN_POINT('Ctrl Pts',(-3.29911882860543,7.19025546035431,-40.0112261953097));
#64938=CARTESIAN_POINT('Ctrl Pts',(-3.31390259975156,7.18345831201984,-40.0105678713862));
#64939=CARTESIAN_POINT('Ctrl Pts',(-3.32310470007956,7.17920600848224,-40.0101569864204));
#64940=CARTESIAN_POINT('Ctrl Pts',(-3.35665045919183,7.16362615040749,-40.0086549789998));
#64941=CARTESIAN_POINT('Ctrl Pts',(-3.38094440406278,7.15219244988336,-40.0075592371313));
#64942=CARTESIAN_POINT('Ctrl Pts',(-3.43941617011596,7.12430881686727,-40.0049016447652));
#64943=CARTESIAN_POINT('Ctrl Pts',(-3.47353457567281,7.10773643192132,-40.003334092941));
#64944=CARTESIAN_POINT('Ctrl Pts',(-3.59947340678139,7.04544063514227,-39.9974808815868));
#64945=CARTESIAN_POINT('Ctrl Pts',(-3.69051730429007,6.9981799515626,-39.9931152838472));
#64946=CARTESIAN_POINT('Ctrl Pts',(-3.93059416943244,6.86756892209665,-39.9812867750648));
#64947=CARTESIAN_POINT('Ctrl Pts',(-4.07788928558076,6.78114206576112,-39.9736973323876));
#64948=CARTESIAN_POINT('Ctrl Pts',(-4.87654415300198,6.27708782578244,-39.9310801982133));
#64949=CARTESIAN_POINT('Ctrl Pts',(-5.46683546790264,5.77031334956111,-39.8944765460214));
#64950=CARTESIAN_POINT('Ctrl Pts',(-6.11642704986206,5.02198739181439,-39.8519133279298));
#64951=CARTESIAN_POINT('Ctrl Pts',(-6.2519177081555,4.85227488285968,-39.8428363942572));
#64952=CARTESIAN_POINT('Ctrl Pts',(-6.39335673692499,4.65933482988213,-39.8331259105448));
#64953=CARTESIAN_POINT('Ctrl Pts',(-6.40637475313049,4.64141939011161,-39.8322297800548));
#64954=CARTESIAN_POINT('Ctrl Pts',(-6.42565581552434,4.61464906162792,-39.8308989065396));
#64955=CARTESIAN_POINT('Ctrl Pts',(-6.43197610640599,4.60583564506453,-39.8304620645509));
#64956=CARTESIAN_POINT('Ctrl Pts',(-6.44279370922174,4.59068519973505,-39.8297133673501));
#64957=CARTESIAN_POINT('Ctrl Pts',(-6.44729983684922,4.58435450165353,-39.8294011899437));
#64958=CARTESIAN_POINT('Ctrl Pts',(-6.45654686876411,4.57132266553615,-39.8287599411487));
#64959=CARTESIAN_POINT('Ctrl Pts',(-6.46128668659713,4.56462076574895,-39.8284309095784));
#64960=CARTESIAN_POINT('Ctrl Pts',(-6.47223760445543,4.5490854024422,-39.827669914031));
#64961=CARTESIAN_POINT('Ctrl Pts',(-6.47844107243326,4.54024656592385,-39.8272382280842));
#64962=CARTESIAN_POINT('Ctrl Pts',(-6.4979249363231,4.51236429612383,-39.8258804857053));
#64963=CARTESIAN_POINT('Ctrl Pts',(-6.51113966176919,4.49327501218704,-39.8249568118256));
#64964=CARTESIAN_POINT('Ctrl Pts',(-6.70826564474867,4.20582162245222,-39.8111352178431));
#64965=CARTESIAN_POINT('Ctrl Pts',(-6.8755430524976,3.9264101354522,-39.7988574987771));
#64966=CARTESIAN_POINT('Ctrl Pts',(-7.38248377374669,2.9473413829766,-39.7587748485092));
#64967=CARTESIAN_POINT('Ctrl Pts',(-7.63614189350831,2.20840374459733,-39.7336235632478));
#64968=CARTESIAN_POINT('Ctrl Pts',(-7.78395816519833,1.41243584266472,-39.7038423927743));
#64969=CARTESIAN_POINT('Ctrl Pts',(-7.78970164853697,1.38040860688653,-39.702639100945));
#64970=CARTESIAN_POINT('Ctrl Pts',(-7.7990957047587,1.32609841331165,-39.7005890243852));
#64971=CARTESIAN_POINT('Ctrl Pts',(-7.80284877796693,1.30383348262326,-39.6997458532954));
#64972=CARTESIAN_POINT('Ctrl Pts',(-7.8073949721912,1.27614059995982,-39.698693459307));
#64973=CARTESIAN_POINT('Ctrl Pts',(-7.80827785336296,1.27072736931404,-39.6984875699799));
#64974=CARTESIAN_POINT('Ctrl Pts',(-7.81070562765827,1.25574383358761,-39.6979171888144));
#64975=CARTESIAN_POINT('Ctrl Pts',(-7.81223855733062,1.24617161735705,-39.6975522479067));
#64976=CARTESIAN_POINT('Ctrl Pts',(-7.83484572431392,1.10332241804954,-39.6920975951547));
#64977=CARTESIAN_POINT('Ctrl Pts',(-7.85252411320311,0.969532303097608,
-39.6868765365133));
#64978=CARTESIAN_POINT('Ctrl Pts',(-7.86840140557257,0.820011204379038,
-39.6808683304173));
#64979=CARTESIAN_POINT('Ctrl Pts',(-7.86998571960172,0.804663794838905,
-39.6802497281055));
#64980=CARTESIAN_POINT('Ctrl Pts',(-7.87224516436768,0.782131161641253,
-39.6793388277476));
#64981=CARTESIAN_POINT('Ctrl Pts',(-7.87295538323075,0.774949427428805,
-39.6790480999309));
#64982=CARTESIAN_POINT('Ctrl Pts',(-7.87419962718364,0.762189368993637,
-39.6785308539216));
#64983=CARTESIAN_POINT('Ctrl Pts',(-7.87473755481492,0.756611423056453,
-39.6783045072469));
#64984=CARTESIAN_POINT('Ctrl Pts',(-7.87576392313471,0.745849009109519,
-39.6778673293359));
#64985=CARTESIAN_POINT('Ctrl Pts',(-7.87625317258029,0.740664619496111,
-39.6776565332134));
#64986=CARTESIAN_POINT('Ctrl Pts',(-7.87729241098965,0.729534730686895,
-39.6772035661759));
#64987=CARTESIAN_POINT('Ctrl Pts',(-7.87784078822961,0.723589086806906,
-39.6769613265918));
#64988=CARTESIAN_POINT('Ctrl Pts',(-7.87914725952928,0.709246464024163,
-39.676376350878));
#64989=CARTESIAN_POINT('Ctrl Pts',(-7.87989866121983,0.7008488939964,-39.6760333338132));
#64990=CARTESIAN_POINT('Ctrl Pts',(-7.88189437793506,0.678136041678968,
-39.6751042134066));
#64991=CARTESIAN_POINT('Ctrl Pts',(-7.88311311339261,0.663818584941344,
-39.6745170602974));
#64992=CARTESIAN_POINT('Ctrl Pts',(-7.90192929177044,0.435407918223026,
-39.6651274982165));
#64993=CARTESIAN_POINT('Ctrl Pts',(-7.91083737108919,0.220699508074797,
-39.6559883201535));
#64994=CARTESIAN_POINT('Ctrl Pts',(-7.91099779352309,0.00590854236546028,
-39.6466906819873));
#64995=CARTESIAN_POINT('',(-7.91099999260968,0.000341949715757575,-37.6423315082368));
#64996=CARTESIAN_POINT('Ctrl Pts',(-7.91099765047707,0.00609706046871071,
-39.6423315082368));
#64997=CARTESIAN_POINT('Ctrl Pts',(-7.91114330160451,-0.182886751144705,
-39.6347110559693));
#64998=CARTESIAN_POINT('Ctrl Pts',(-7.90451297234196,-0.372147225623654,
-39.6270906037017));
#64999=CARTESIAN_POINT('Ctrl Pts',(-7.89107380823835,-0.561137374387657,
-39.6194701514342));
#65000=CARTESIAN_POINT('Ctrl Pts',(-7.87764520868798,-0.749978957625515,
-39.6118556896191));
#65001=CARTESIAN_POINT('Ctrl Pts',(-7.85741844921442,-0.938550270991757,
-39.6042412278041));
#65002=CARTESIAN_POINT('Ctrl Pts',(-7.83041270643092,-1.12630273326724,
-39.596626765989));
#65003=CARTESIAN_POINT('Ctrl Pts',(-7.80342401238723,-1.3139366673132,-39.5890171111878));
#65004=CARTESIAN_POINT('Ctrl Pts',(-7.76966490711269,-1.50075241408661,
-39.5814074563865));
#65005=CARTESIAN_POINT('Ctrl Pts',(-7.72920651725325,-1.68620509240422,
-39.5737978015853));
#65006=CARTESIAN_POINT('Ctrl Pts',(-7.68876294287454,-1.87158985970036,
-39.5661909333678));
#65007=CARTESIAN_POINT('Ctrl Pts',(-7.64162504534338,-2.05561219066511,
-39.5585840651504));
#65008=CARTESIAN_POINT('Ctrl Pts',(-7.58791530460303,-2.2377359831247,-39.5509771969329));
#65009=CARTESIAN_POINT('Ctrl Pts',(-7.53421063202268,-2.4198425900141,-39.543371046515));
#65010=CARTESIAN_POINT('Ctrl Pts',(-7.47393545193249,-2.60005065878146,
-39.535764896097));
#65011=CARTESIAN_POINT('Ctrl Pts',(-7.40726250799875,-2.77783785300656,
-39.5281587456791));
#65012=CARTESIAN_POINT('Ctrl Pts',(-7.38187403647389,-2.84553765523149,
-39.5252623903975));
#65013=CARTESIAN_POINT('Ctrl Pts',(-7.35555838855058,-2.91288659458526,
-39.522366035116));
#65014=CARTESIAN_POINT('Ctrl Pts',(-7.32832696856371,-2.97985651362978,
-39.5194696798344));
#65015=CARTESIAN_POINT('Ctrl Pts',(-7.24822733924639,-3.17684461390011,
-39.5109502201611));
#65016=CARTESIAN_POINT('Ctrl Pts',(-7.1602564859085,-3.37041596226114,-39.5024307604878));
#65017=CARTESIAN_POINT('Ctrl Pts',(-7.06473739458507,-3.55997282932768,
-39.4939113008145));
#65018=CARTESIAN_POINT('Ctrl Pts',(-6.96904628063741,-3.74987107390593,
-39.4853764982418));
#65019=CARTESIAN_POINT('Ctrl Pts',(-6.86577987219144,-3.93574016488276,
-39.4768416956691));
#65020=CARTESIAN_POINT('Ctrl Pts',(-6.75530589298582,-4.11700902260257,
-39.4683068930964));
#65021=CARTESIAN_POINT('Ctrl Pts',(-6.63924079654431,-4.30745194503894,
-39.4593401419136));
#65022=CARTESIAN_POINT('Ctrl Pts',(-6.51521994139232,-4.49281668990722,
-39.4503733907308));
#65023=CARTESIAN_POINT('Ctrl Pts',(-6.3837177659858,-4.67247990731231,-39.441406639548));
#65024=CARTESIAN_POINT('Ctrl Pts',(-6.25802762523127,-4.84420250440433,
-39.4328361941178));
#65025=CARTESIAN_POINT('Ctrl Pts',(-6.125503364898,-5.01071652534564,-39.4242657486876));
#65026=CARTESIAN_POINT('Ctrl Pts',(-5.9865983332433,-5.17151442001359,-39.4156953032573));
#65027=CARTESIAN_POINT('Ctrl Pts',(-5.84751972121477,-5.33251325310929,
-39.4071141479118));
#65028=CARTESIAN_POINT('Ctrl Pts',(-5.70204457486867,-5.4877815046477,-39.3985329925663));
#65029=CARTESIAN_POINT('Ctrl Pts',(-5.55066330241482,-5.63684822424956,
-39.3899518372208));
#65030=CARTESIAN_POINT('Ctrl Pts',(-5.39903015939884,-5.78616296342381,
-39.3813564044129));
#65031=CARTESIAN_POINT('Ctrl Pts',(-5.2414714220748,-5.9292553673493,-39.3727609716051));
#65032=CARTESIAN_POINT('Ctrl Pts',(-5.07851243344497,-6.06569307361862,
-39.3641655387972));
#65033=CARTESIAN_POINT('Ctrl Pts',(-5.05664878058053,-6.08399845629541,
-39.3630123188324));
#65034=CARTESIAN_POINT('Ctrl Pts',(-5.03468796465651,-6.10218411204924,
-39.3618590988676));
#65035=CARTESIAN_POINT('Ctrl Pts',(-5.01263129570722,-6.12024905484218,
-39.3607058789028));
#65036=CARTESIAN_POINT('Ctrl Pts',(-4.86136202219078,-6.24414223103694,
-39.3527968538963));
#65037=CARTESIAN_POINT('Ctrl Pts',(-4.70530392627715,-6.36258181591704,
-39.3448878288898));
#65038=CARTESIAN_POINT('Ctrl Pts',(-4.54488693057181,-6.4751775101782,-39.3369788038834));
#65039=CARTESIAN_POINT('Ctrl Pts',(-4.3846334554305,-6.58765843036975,-39.3290778409169));
#65040=CARTESIAN_POINT('Ctrl Pts',(-4.22003021091666,-6.69430712920731,
-39.3211768779504));
#65041=CARTESIAN_POINT('Ctrl Pts',(-4.05154106789086,-6.79477269488787,
-39.3132759149839));
#65042=CARTESIAN_POINT('Ctrl Pts',(-3.88319241760989,-6.89515448850556,
-39.305381540145));
#65043=CARTESIAN_POINT('Ctrl Pts',(-3.71096461826943,-6.98936324436329,
-39.297487165306));
#65044=CARTESIAN_POINT('Ctrl Pts',(-3.53535170331116,-7.07709045681168,
-39.2895927904671));
#65045=CARTESIAN_POINT('Ctrl Pts',(-3.35985265248481,-7.1647607885751,-39.2817035341933));
#65046=CARTESIAN_POINT('Ctrl Pts',(-3.18097316639855,-7.24595779649179,
-39.2738142779195));
#65047=CARTESIAN_POINT('Ctrl Pts',(-2.99923338572382,-7.32041802754185,
-39.2659250216457));
#65048=CARTESIAN_POINT('Ctrl Pts',(-2.81757774346421,-7.39484378641522,
-39.2580394177892));
#65049=CARTESIAN_POINT('Ctrl Pts',(-2.63306476376436,-7.46253885294553,
-39.2501538139328));
#65050=CARTESIAN_POINT('Ctrl Pts',(-2.44623640628078,-7.52328707710841,
-39.2422682100763));
#65051=CARTESIAN_POINT('Ctrl Pts',(-2.24969869307562,-7.58719234940788,
-39.2339727961997));
#65052=CARTESIAN_POINT('Ctrl Pts',(-2.0505989028863,-7.6434093441205,-39.2256773823232));
#65053=CARTESIAN_POINT('Ctrl Pts',(-1.84958913357896,-7.69174499297439,
-39.2173819684467));
#65054=CARTESIAN_POINT('Ctrl Pts',(-1.65854121144815,-7.7376851744402,-39.2094976671524));
#65055=CARTESIAN_POINT('Ctrl Pts',(-1.46576840672236,-7.77650619550339,
-39.201613365858));
#65056=CARTESIAN_POINT('Ctrl Pts',(-1.27184360280945,-7.8080941880841,-39.1937290645637));
#65057=CARTESIAN_POINT('Ctrl Pts',(-1.0778935148621,-7.83968629912659,-39.1858437353093));
#65058=CARTESIAN_POINT('Ctrl Pts',(-0.882791468855304,-7.8640434464469,
-39.177958406055));
#65059=CARTESIAN_POINT('Ctrl Pts',(-0.687118104711814,-7.88110333076386,
-39.1700730768006));
#65060=CARTESIAN_POINT('Ctrl Pts',(-0.49138635318538,-7.89816830561526,
-39.1621853946264));
#65061=CARTESIAN_POINT('Ctrl Pts',(-0.295083287350566,-7.90793164841032,
-39.1542977124522));
#65062=CARTESIAN_POINT('Ctrl Pts',(-0.0987924503084548,-7.9103831166235,
-39.1464100302781));
#65063=CARTESIAN_POINT('Ctrl Pts',(0.0975899382150019,-7.91283572821937,
-39.1385186692312));
#65064=CARTESIAN_POINT('Ctrl Pts',(0.293959742127451,-7.90796966517475,
-39.1306273081844));
#65065=CARTESIAN_POINT('Ctrl Pts',(0.4897353923057,-7.89582676136725,-39.1227359471376));
#65066=CARTESIAN_POINT('Ctrl Pts',(0.685736641728731,-7.88366986485981,
-39.1148354925948));
#65067=CARTESIAN_POINT('Ctrl Pts',(0.881142025725839,-7.86421940045347,
-39.106935038052));
#65068=CARTESIAN_POINT('Ctrl Pts',(1.07537591434748,-7.8375689880754,-39.0990345835091));
#65069=CARTESIAN_POINT('Ctrl Pts',(1.26973970529285,-7.81090075208004,-39.0911288451952));
#65070=CARTESIAN_POINT('Ctrl Pts',(1.46293010048366,-7.77702302808523,-39.0832231068814));
#65071=CARTESIAN_POINT('Ctrl Pts',(1.6543833391645,-7.73608019394156,-39.0753173685675));
#65072=CARTESIAN_POINT('Ctrl Pts',(1.84609467093527,-7.69508216583697,-39.0674009727351));
#65073=CARTESIAN_POINT('Ctrl Pts',(2.03606383617461,-7.64700008975067,-39.0594845769027));
#65074=CARTESIAN_POINT('Ctrl Pts',(2.22374278064302,-7.59202799293694,-39.0515681810703));
#65075=CARTESIAN_POINT('Ctrl Pts',(2.2900443470788,-7.57260793418003,-39.0487715463935));
#65076=CARTESIAN_POINT('Ctrl Pts',(2.35606027923801,-7.55232843405329,-39.0459749117166));
#65077=CARTESIAN_POINT('Ctrl Pts',(2.42176706436186,-7.53119945865014,-39.0431782770398));
#65078=CARTESIAN_POINT('Ctrl Pts',(2.60412977562313,-7.47255806821491,-39.0354164929088));
#65079=CARTESIAN_POINT('Ctrl Pts',(2.78468143073056,-7.40718596574286,-39.0276547087777));
#65080=CARTESIAN_POINT('Ctrl Pts',(2.96287496700522,-7.3352091265276,-39.0198929246467));
#65081=CARTESIAN_POINT('Ctrl Pts',(3.1408545273114,-7.26331871757352,-39.012140460917));
#65082=CARTESIAN_POINT('Ctrl Pts',(3.31648127664525,-7.18483949068495,-39.0043879971873));
#65083=CARTESIAN_POINT('Ctrl Pts',(3.48922086645204,-7.09994779875991,-38.9966355334577));
#65084=CARTESIAN_POINT('Ctrl Pts',(3.66178806420543,-7.01514082773239,-38.9888908065945));
#65085=CARTESIAN_POINT('Ctrl Pts',(3.83147351918181,-6.92393428806278,-38.9811460797312));
#65086=CARTESIAN_POINT('Ctrl Pts',(3.99776042318241,-6.82655349344282,-38.973401352868));
#65087=CARTESIAN_POINT('Ctrl Pts',(4.16391505251984,-6.72925016139807,-38.9656627866291));
#65088=CARTESIAN_POINT('Ctrl Pts',(4.32667620541288,-6.62578253307438,-38.9579242203902));
#65089=CARTESIAN_POINT('Ctrl Pts',(4.48554927957113,-6.51642299582669,-38.9501856541512));
#65090=CARTESIAN_POINT('Ctrl Pts',(4.64432811995388,-6.40712832395746,-38.9424516779558));
#65091=CARTESIAN_POINT('Ctrl Pts',(4.79922317918888,-6.29194890493478,-38.9347177017603));
#65092=CARTESIAN_POINT('Ctrl Pts',(4.94976651931873,-6.17120186059663,-38.9269837255648));
#65093=CARTESIAN_POINT('Ctrl Pts',(5.10025100350101,-6.0505020231406,-38.9192527730202));
#65094=CARTESIAN_POINT('Ctrl Pts',(5.24638687758578,-5.92423911990399,-38.9115218204755));
#65095=CARTESIAN_POINT('Ctrl Pts',(5.38773707494352,-5.79277223885758,-38.9037908679309));
#65096=CARTESIAN_POINT('Ctrl Pts',(5.52908747092009,-5.66130517307991,-38.8960599045231));
#65097=CARTESIAN_POINT('Ctrl Pts',(5.66565190623245,-5.52463435097297,-38.8883289411152));
#65098=CARTESIAN_POINT('Ctrl Pts',(5.79702787322901,-5.38315788705903,-38.8805979777074));
#65099=CARTESIAN_POINT('Ctrl Pts',(5.92841064115388,-5.24167409934526,-38.8728666140915));
#65100=CARTESIAN_POINT('Ctrl Pts',(6.05460416074512,-5.09538443698233,-38.8651352504756));
#65101=CARTESIAN_POINT('Ctrl Pts',(6.17524428003438,-4.94472234629031,-38.8574038868596));
#65102=CARTESIAN_POINT('Ctrl Pts',(6.29591273538659,-4.79402486794689,-38.8496707072938));
#65103=CARTESIAN_POINT('Ctrl Pts',(6.41102496835412,-4.63895319635809,-38.8419375277281));
#65104=CARTESIAN_POINT('Ctrl Pts',(6.52025842974105,-4.47997221078332,-38.8342043481623));
#65105=CARTESIAN_POINT('Ctrl Pts',(6.62953755649719,-4.3209247627408,-38.8264679357181));
#65106=CARTESIAN_POINT('Ctrl Pts',(6.73293281469685,-4.15796504196802,-38.8187315232739));
#65107=CARTESIAN_POINT('Ctrl Pts',(6.83016609837389,-3.99158515738095,-38.8109951108297));
#65108=CARTESIAN_POINT('Ctrl Pts',(6.92751508747393,-3.82500728446936,-38.8032494922285));
#65109=CARTESIAN_POINT('Ctrl Pts',(7.01868727693405,-3.65500142969943,-38.7955038736273));
#65110=CARTESIAN_POINT('Ctrl Pts',(7.10345101489146,-3.48208338197659,-38.7877582550261));
#65111=CARTESIAN_POINT('Ctrl Pts',(7.18826986520101,-3.30905290504087,-38.7800076003178));
#65112=CARTESIAN_POINT('Ctrl Pts',(7.26667181868098,-3.13310679001022,-38.7722569456096));
#65113=CARTESIAN_POINT('Ctrl Pts',(7.3384742033577,-2.95477873395853,-38.7645062909013));
#65114=CARTESIAN_POINT('Ctrl Pts',(7.41038566743114,-2.7761797688436,-38.7567438616992));
#65115=CARTESIAN_POINT('Ctrl Pts',(7.47567741825765,-2.59519197199196,-38.748981432497));
#65116=CARTESIAN_POINT('Ctrl Pts',(7.53421693182173,-2.4123632032202,-38.7412190032949));
#65117=CARTESIAN_POINT('Ctrl Pts',(7.57335254823366,-2.29013607613814,-38.7360295605888));
#65118=CARTESIAN_POINT('Ctrl Pts',(7.60947139783775,-2.16708638633235,-38.7308401178828));
#65119=CARTESIAN_POINT('Ctrl Pts',(7.64254676158435,-2.04337955284782,-38.7256506751768));
#65120=CARTESIAN_POINT('Ctrl Pts',(7.69362905697515,-1.85232408756769,-38.7176359894652));
#65121=CARTESIAN_POINT('Ctrl Pts',(7.7376057576374,-1.65911698728575,-38.7096213037537));
#65122=CARTESIAN_POINT('Ctrl Pts',(7.77429613102985,-1.46432259664815,-38.7016066180422));
#65123=CARTESIAN_POINT('Ctrl Pts',(7.81094479234527,-1.26974966133722,-38.6936010439628));
#65124=CARTESIAN_POINT('Ctrl Pts',(7.84032357099007,-1.07359335731651,-38.6855954698835));
#65125=CARTESIAN_POINT('Ctrl Pts',(7.86230162724109,-0.876432611375287,
-38.6775898958042));
#65126=CARTESIAN_POINT('Ctrl Pts',(7.88425842429107,-0.679462577473684,
-38.6695920654537));
#65127=CARTESIAN_POINT('Ctrl Pts',(7.89882872813028,-0.481490368201534,
-38.6615942351033));
#65128=CARTESIAN_POINT('Ctrl Pts',(7.90593274707188,-0.283104925383739,
-38.6535964047528));
#65129=CARTESIAN_POINT('Ctrl Pts',(7.9130310982357,-0.084877759818765,-38.645604955287));
#65130=CARTESIAN_POINT('Ctrl Pts',(7.91267502487342,0.113761649406268,-38.6376135058211));
#65131=CARTESIAN_POINT('Ctrl Pts',(7.90483651293712,0.312218999639936,-38.6296220563553));
#65132=CARTESIAN_POINT('Ctrl Pts',(7.89700292713308,0.510551628859768,-38.6216356291356));
#65133=CARTESIAN_POINT('Ctrl Pts',(7.88169628922905,0.708702093908644,-38.613649201916));
#65134=CARTESIAN_POINT('Ctrl Pts',(7.85894066079851,0.906075432868546,-38.6056627746964));
#65135=CARTESIAN_POINT('Ctrl Pts',(7.83548868449896,1.10948861838344,-38.5974319538054));
#65136=CARTESIAN_POINT('Ctrl Pts',(7.80412457699479,1.31207599825623,-38.5892011329145));
#65137=CARTESIAN_POINT('Ctrl Pts',(7.76493252859522,1.51318995052302,-38.5809703120236));
#65138=CARTESIAN_POINT('Ctrl Pts',(7.72692975904522,1.70820111971135,-38.5729892545821));
#65139=CARTESIAN_POINT('Ctrl Pts',(7.68156724094024,1.9018266242896,-38.5650081971406));
#65140=CARTESIAN_POINT('Ctrl Pts',(7.62897396363313,2.0934844786164,-38.5570271396992));
#65141=CARTESIAN_POINT('Ctrl Pts',(7.57638479645517,2.28512735501116,-38.5490467059719));
#65142=CARTESIAN_POINT('Ctrl Pts',(7.51656608476441,2.47480256510407,-38.5410662722447));
#65143=CARTESIAN_POINT('Ctrl Pts',(7.44969719269671,2.66194153525707,-38.5330858385175));
#65144=CARTESIAN_POINT('Ctrl Pts',(7.38282326122531,2.84909460866182,-38.5251048033652));
#65145=CARTESIAN_POINT('Ctrl Pts',(7.30889820321929,3.0337107462913,-38.5171237682129));
#65146=CARTESIAN_POINT('Ctrl Pts',(7.22815033052729,3.21523930669214,-38.5091427330607));
#65147=CARTESIAN_POINT('Ctrl Pts',(7.14738397653984,3.39680941472572,-38.5011598712365));
#65148=CARTESIAN_POINT('Ctrl Pts',(7.05979183164243,3.57529023167102,-38.4931770094123));
#65149=CARTESIAN_POINT('Ctrl Pts',(6.96564931355491,3.75015341560475,-38.4851941475882));
#65150=CARTESIAN_POINT('Ctrl Pts',(6.87143693663302,3.92514635746778,-38.4772053620493));
#65151=CARTESIAN_POINT('Ctrl Pts',(6.77066463560454,4.09651600926776,-38.4692165765104));
#65152=CARTESIAN_POINT('Ctrl Pts',(6.66365304698806,4.26375996854499,-38.4612277909715));
#65153=CARTESIAN_POINT('Ctrl Pts',(6.55659426377389,4.43107768629526,-38.4532354821925));
#65154=CARTESIAN_POINT('Ctrl Pts',(6.44329089350447,4.59426580675474,-38.4452431734135));
#65155=CARTESIAN_POINT('Ctrl Pts',(6.32410577346231,4.75285252938282,-38.4372508646345));
#65156=CARTESIAN_POINT('Ctrl Pts',(6.20480913217169,4.91158764125019,-38.4292510774702));
#65157=CARTESIAN_POINT('Ctrl Pts',(6.07961995739964,5.06571249501295,-38.4212512903059));
#65158=CARTESIAN_POINT('Ctrl Pts',(5.94894069895238,5.21478911945133,-38.4132515031416));
#65159=CARTESIAN_POINT('Ctrl Pts',(5.92101581407187,5.24664534227721,-38.4115420265323));
#65160=CARTESIAN_POINT('Ctrl Pts',(5.8928403652959,5.27827118024825,-38.409832549923));
#65161=CARTESIAN_POINT('Ctrl Pts',(5.86441849184323,5.30966258367961,-38.4081230733138));
#65162=CARTESIAN_POINT('Ctrl Pts',(5.72929214138113,5.45890699533412,-38.3999956943851));
#65163=CARTESIAN_POINT('Ctrl Pts',(5.58835543949867,5.6031116452127,-38.3918683154565));
#65164=CARTESIAN_POINT('Ctrl Pts',(5.44201034328428,5.74181542925118,-38.3837409365279));
#65165=CARTESIAN_POINT('Ctrl Pts',(5.2957895315639,5.8804014182281,-38.375620459827));
#65166=CARTESIAN_POINT('Ctrl Pts',(5.14416971282125,6.01349563669138,-38.3674999831261));
#65167=CARTESIAN_POINT('Ctrl Pts',(4.9875910098358,6.14067235069623,-38.3593795064252));
#65168=CARTESIAN_POINT('Ctrl Pts',(4.83112559544692,6.2677570491768,-38.3512649050917));
#65169=CARTESIAN_POINT('Ctrl Pts',(4.66970869721374,6.38893257959597,-38.3431503037582));
#65170=CARTESIAN_POINT('Ctrl Pts',(4.50381539255678,6.50381179845855,-38.3350357024247));
#65171=CARTESIAN_POINT('Ctrl Pts',(4.33803961153578,6.61860963354542,-38.3269268497105));
#65172=CARTESIAN_POINT('Ctrl Pts',(4.16779401220337,6.72711987488408,-38.3188179969963));
#65173=CARTESIAN_POINT('Ctrl Pts',(3.99358497150644,6.82899700361319,-38.3107091442821));
#65174=CARTESIAN_POINT('Ctrl Pts',(3.81945053928184,6.93083050144399,-38.3026037643447));
#65175=CARTESIAN_POINT('Ctrl Pts',(3.64135632485281,7.02603639028042,-38.2944983844073));
#65176=CARTESIAN_POINT('Ctrl Pts',(3.45983650205037,7.11431320501704,-38.2863930044699));
#65177=CARTESIAN_POINT('Ctrl Pts',(3.27837328238472,7.20256249248671,-38.2782901520247));
#65178=CARTESIAN_POINT('Ctrl Pts',(3.09348687109394,7.28388687586475,-38.2701872995794));
#65179=CARTESIAN_POINT('Ctrl Pts',(2.90573528503304,7.35803122127883,-38.2620844471342));
#65180=CARTESIAN_POINT('Ctrl Pts',(2.80745007174017,7.39684470326517,-38.2578427222169));
#65181=CARTESIAN_POINT('Ctrl Pts',(2.70838007268159,7.43369136736052,-38.2536009972996));
#65182=CARTESIAN_POINT('Ctrl Pts',(2.60860759688772,7.46853984427075,-38.2493592723822));
#65183=CARTESIAN_POINT('Ctrl Pts',(2.41363851383687,7.53663854117933,-38.2410703609254));
#65184=CARTESIAN_POINT('Ctrl Pts',(2.21606962171687,7.59707469984934,-38.2327814494686));
#65185=CARTESIAN_POINT('Ctrl Pts',(2.01651896469399,7.64967791903878,-38.2244925380117));
#65186=CARTESIAN_POINT('Ctrl Pts',(1.81685357638307,7.70231138235361,-38.2161988608603));
#65187=CARTESIAN_POINT('Ctrl Pts',(1.61520443171274,7.74710284233969,-38.2079051837089));
#65188=CARTESIAN_POINT('Ctrl Pts',(1.41220107318992,7.78393275464795,-38.1996115065575));
#65189=CARTESIAN_POINT('Ctrl Pts',(1.2090687712019,7.82078606054216,-38.1913125614367));
#65190=CARTESIAN_POINT('Ctrl Pts',(1.00458082601934,7.84966767223038,-38.1830136163159));
#65191=CARTESIAN_POINT('Ctrl Pts',(0.799374070348638,7.8705096465003,-38.1747146711952));
#65192=CARTESIAN_POINT('Ctrl Pts',(0.593929230478708,7.8913758019661,-38.1664060975039));
#65193=CARTESIAN_POINT('Ctrl Pts',(0.387764204450145,7.90418364551509,-38.1580975238127));
#65194=CARTESIAN_POINT('Ctrl Pts',(0.181519753465613,7.90891721913321,-38.1497889501215));
#65195=CARTESIAN_POINT('Ctrl Pts',(-0.0248516342685485,7.91365370611189,
-38.1414752627734));
#65196=CARTESIAN_POINT('Ctrl Pts',(-0.231302252182532,7.91030600339276,
-38.1331615754254));
#65197=CARTESIAN_POINT('Ctrl Pts',(-0.43719284541712,7.89891026762022,-38.1248478880774));
#65198=CARTESIAN_POINT('Ctrl Pts',(-0.643307520746114,7.88750212923957,
-38.1165251524847));
#65199=CARTESIAN_POINT('Ctrl Pts',(-0.848860661520386,7.86802847371838,
-38.1082024168919));
#65200=CARTESIAN_POINT('Ctrl Pts',(-1.05321799701201,7.84057732891973,-38.0998796812992));
#65201=CARTESIAN_POINT('Ctrl Pts',(-1.12920648924262,7.83036986023144,-38.096784944683));
#65202=CARTESIAN_POINT('Ctrl Pts',(-1.20502973461416,7.81905988640283,-38.0936902080669));
#65203=CARTESIAN_POINT('Ctrl Pts',(-1.28065549613145,7.80665373256867,-38.0905954714507));
#65204=CARTESIAN_POINT('Ctrl Pts',(-1.49318710159551,7.77178863185289,-38.0818983115369));
#65205=CARTESIAN_POINT('Ctrl Pts',(-1.70434647359446,7.72823160532294,-38.0732011516231));
#65206=CARTESIAN_POINT('Ctrl Pts',(-1.91344654627575,7.67610860492121,-38.0645039917092));
#65207=CARTESIAN_POINT('Ctrl Pts',(-2.12236348806853,7.62403125410368,-38.0558144488115));
#65208=CARTESIAN_POINT('Ctrl Pts',(-2.32922450981592,7.56340296467206,-38.0471249059138));
#65209=CARTESIAN_POINT('Ctrl Pts',(-2.53335406831927,7.4944004539743,-38.0384353630161));
#65210=CARTESIAN_POINT('Ctrl Pts',(-2.74204326463621,7.42385663559275,-38.0295517219747));
#65211=CARTESIAN_POINT('Ctrl Pts',(-2.94787731222795,7.34456015467706,-38.0206680809332));
#65212=CARTESIAN_POINT('Ctrl Pts',(-3.1501485870133,7.25675443154432,-38.0117844398918));
#65213=CARTESIAN_POINT('Ctrl Pts',(-3.34742030639273,7.17111900954913,-38.0031203765222));
#65214=CARTESIAN_POINT('Ctrl Pts',(-3.54130303678552,7.07739006003169,-37.9944563131526));
#65215=CARTESIAN_POINT('Ctrl Pts',(-3.73115693726987,6.97584324002933,-37.9857922497831));
#65216=CARTESIAN_POINT('Ctrl Pts',(-3.92822818064668,6.87043609259769,-37.9767988199057));
#65217=CARTESIAN_POINT('Ctrl Pts',(-4.12095806562072,6.75660511920194,-37.9678053900284));
#65218=CARTESIAN_POINT('Ctrl Pts',(-4.30865354453088,6.63471368132804,-37.9588119601511));
#65219=CARTESIAN_POINT('Ctrl Pts',(-4.49634902344105,6.51282224345414,-37.9498185302738));
#65220=CARTESIAN_POINT('Ctrl Pts',(-4.67900982833887,6.38287043622605,-37.9408251003964));
#65221=CARTESIAN_POINT('Ctrl Pts',(-4.85596988937692,6.24527640969274,-37.9318316705191));
#65222=CARTESIAN_POINT('Ctrl Pts',(-5.00968481138059,6.12575647433179,-37.9240196005863));
#65223=CARTESIAN_POINT('Ctrl Pts',(-5.15903177185281,6.00052123967778,-37.9162075306536));
#65224=CARTESIAN_POINT('Ctrl Pts',(-5.30356492179082,5.86993357035239,-37.9083954607208));
#65225=CARTESIAN_POINT('Ctrl Pts',(-5.44808776416868,5.73935521404797,-37.9005839479154));
#65226=CARTESIAN_POINT('Ctrl Pts',(-5.58779721865798,5.60342541942066,-37.8927724351101));
#65227=CARTESIAN_POINT('Ctrl Pts',(-5.72228207817539,5.46254600143493,-37.8849609223047));
#65228=CARTESIAN_POINT('Ctrl Pts',(-5.85678106193276,5.32165178762229,-37.8771485890971));
#65229=CARTESIAN_POINT('Ctrl Pts',(-5.98605411528906,5.17580717022823,-37.8693362558895));
#65230=CARTESIAN_POINT('Ctrl Pts',(-6.10972822563091,5.02544943352622,-37.8615239226819));
#65231=CARTESIAN_POINT('Ctrl Pts',(-6.23348995220829,4.87498517672201,-37.8537060548703));
#65232=CARTESIAN_POINT('Ctrl Pts',(-6.35164458732493,4.72000168508857,-37.8458881870587));
#65233=CARTESIAN_POINT('Ctrl Pts',(-6.46386009101385,4.56096850721406,-37.8380703192471));
#65234=CARTESIAN_POINT('Ctrl Pts',(-6.57611711920151,4.40187648031443,-37.8302495584926));
#65235=CARTESIAN_POINT('Ctrl Pts',(-6.68243044177497,4.23873207404659,-37.8224287977381));
#65236=CARTESIAN_POINT('Ctrl Pts',(-6.78251236144226,4.07203230179758,-37.8146080369836));
#65237=CARTESIAN_POINT('Ctrl Pts',(-6.8827051411969,3.90514787730196,-37.8067786132236));
#65238=CARTESIAN_POINT('Ctrl Pts',(-6.97665255602243,3.73470052589074,-37.7989491894636));
#65239=CARTESIAN_POINT('Ctrl Pts',(-7.06411322178446,3.56121122510446,-37.7911197657037));
#65240=CARTESIAN_POINT('Ctrl Pts',(-7.13133106143543,3.42787613212517,-37.7851024669983));
#65241=CARTESIAN_POINT('Ctrl Pts',(-7.19471832935731,3.29274475070456,-37.779085168293));
#65242=CARTESIAN_POINT('Ctrl Pts',(-7.25418513020149,3.15606069282002,-37.7730678695876));
#65243=CARTESIAN_POINT('Ctrl Pts',(-7.34246840311898,2.95314215988416,-37.7641347032446));
#65244=CARTESIAN_POINT('Ctrl Pts',(-7.4222494179899,2.74648092902733,-37.7552015369015));
#65245=CARTESIAN_POINT('Ctrl Pts',(-7.49324770286426,2.53676168835771,-37.7462683705585));
#65246=CARTESIAN_POINT('Ctrl Pts',(-7.56410161708253,2.32746889889639,-37.7373533692611));
#65247=CARTESIAN_POINT('Ctrl Pts',(-7.62620841446035,2.11513068903211,-37.7284383679637));
#65248=CARTESIAN_POINT('Ctrl Pts',(-7.67933726836815,1.9004473469823,-37.7195233666663));
#65249=CARTESIAN_POINT('Ctrl Pts',(-7.7323797293992,1.68611310170654,-37.7106228620605));
#65250=CARTESIAN_POINT('Ctrl Pts',(-7.776473349148,1.46944151070523,-37.7017223574547));
#65251=CARTESIAN_POINT('Ctrl Pts',(-7.81143731559288,1.25114669985702,-37.6928218528488));
#65252=CARTESIAN_POINT('Ctrl Pts',(-7.84628292098092,1.03359086708085,-37.6839514784954));
#65253=CARTESIAN_POINT('Ctrl Pts',(-7.87206052311267,0.814422958168712,
-37.6750811041419));
#65254=CARTESIAN_POINT('Ctrl Pts',(-7.8886406852852,0.594364482841163,-37.6662107297884));
#65255=CARTESIAN_POINT('Ctrl Pts',(-7.90351872575645,0.396897240488833,
-37.6582509892712));
#65256=CARTESIAN_POINT('Ctrl Pts',(-7.91099141809527,0.198713173039897,
-37.650291248754));
#65257=CARTESIAN_POINT('Ctrl Pts',(-7.91099999260968,0.000341949715757575,
-37.6423315082368));
#65258=CARTESIAN_POINT('',(-7.91099999400094,-0.000308086119090196,-33.6436736902287));
#65259=CARTESIAN_POINT('Ctrl Pts',(-7.91099999086604,0.000380154568757167,
-37.6333945227008));
#65260=CARTESIAN_POINT('Ctrl Pts',(-7.91100804081377,-0.167138906403437,
-37.6262687265125));
#65261=CARTESIAN_POINT('Ctrl Pts',(-7.90569518377744,-0.334622696508921,
-37.619293165992));
#65262=CARTESIAN_POINT('Ctrl Pts',(-7.89373004197606,-0.522868907718592,
-37.6116167499129));
#65263=CARTESIAN_POINT('Ctrl Pts',(-7.89230793117402,-0.543913043018763,
-37.6107608910436));
#65264=CARTESIAN_POINT('Ctrl Pts',(-7.88991667126631,-0.577312304649131,
-37.6094061542906));
#65265=CARTESIAN_POINT('Ctrl Pts',(-7.88900262693277,-0.589671205509749,
-37.6089056373613));
#65266=CARTESIAN_POINT('Ctrl Pts',(-7.88739293238899,-0.610762197319669,
-37.6080528118984));
#65267=CARTESIAN_POINT('Ctrl Pts',(-7.88671181393218,-0.619495356050412,
-37.6077000707848));
#65268=CARTESIAN_POINT('Ctrl Pts',(-7.88541266715558,-0.635803292941461,
-37.6070420991516));
#65269=CARTESIAN_POINT('Ctrl Pts',(-7.88479822618885,-0.643378342299304,
-37.6067367620263));
#65270=CARTESIAN_POINT('Ctrl Pts',(-7.88349958502888,-0.659107157046066,
-37.6061033626495));
#65271=CARTESIAN_POINT('Ctrl Pts',(-7.88281364832599,-0.667260772022794,
-37.6057753525923));
#65272=CARTESIAN_POINT('Ctrl Pts',(-7.88122373420322,-0.685815167712521,
-37.6050296924272));
#65273=CARTESIAN_POINT('Ctrl Pts',(-7.88031181509016,-0.696215261832065,
-37.6046122798259));
#65274=CARTESIAN_POINT('Ctrl Pts',(-7.87741867844866,-0.728476348754434,
-37.603319142472));
#65275=CARTESIAN_POINT('Ctrl Pts',(-7.87536705312983,-0.750331003093177,
-37.6024455206183));
#65276=CARTESIAN_POINT('Ctrl Pts',(-7.85913350215745,-0.915850566986409,
-37.5958468159735));
#65277=CARTESIAN_POINT('Ctrl Pts',(-7.84111208802052,-1.05911539898391,
-37.5902376764449));
#65278=CARTESIAN_POINT('Ctrl Pts',(-7.81233038629602,-1.24637379925773,
-37.583019522908));
#65279=CARTESIAN_POINT('Ctrl Pts',(-7.80510025786298,-1.29087712353991,
-37.5813124795044));
#65280=CARTESIAN_POINT('Ctrl Pts',(-7.63798994468429,-2.2667063709624,-37.5440523205259));
#65281=CARTESIAN_POINT('Ctrl Pts',(-7.31295421319051,-3.16182939678263,
-37.514238819932));
#65282=CARTESIAN_POINT('Ctrl Pts',(-6.75782772920575,-4.11594486905787,
-37.4732333980651));
#65283=CARTESIAN_POINT('Ctrl Pts',(-6.67368286036299,-4.2510223224782,-37.4671598010197));
#65284=CARTESIAN_POINT('Ctrl Pts',(-6.57000435691224,-4.40678436757921,
-37.4597409285784));
#65285=CARTESIAN_POINT('Ctrl Pts',(-6.55435898328399,-4.43002076738572,
-37.4586230902748));
#65286=CARTESIAN_POINT('Ctrl Pts',(-6.53337496386369,-4.46083158546764,
-37.4571265807389));
#65287=CARTESIAN_POINT('Ctrl Pts',(-6.52814580939585,-4.46848063020689,
-37.4567538807208));
#65288=CARTESIAN_POINT('Ctrl Pts',(-6.51951821717661,-4.48105333685371,
-37.456139356301));
#65289=CARTESIAN_POINT('Ctrl Pts',(-6.51612760101633,-4.4859823761148,-37.4558979497426));
#65290=CARTESIAN_POINT('Ctrl Pts',(-6.5095325528281,-4.49554654035601,-37.455428593167));
#65291=CARTESIAN_POINT('Ctrl Pts',(-6.50632875235116,-4.5001820984187,-37.4552006764631));
#65292=CARTESIAN_POINT('Ctrl Pts',(-6.49889977635036,-4.51090651902743,
-37.4546724018062));
#65293=CARTESIAN_POINT('Ctrl Pts',(-6.49467099596951,-4.51699286915906,
-37.4543718563921));
#65294=CARTESIAN_POINT('Ctrl Pts',(-6.48137044706001,-4.53607863800801,
-37.45342710173));
#65295=CARTESIAN_POINT('Ctrl Pts',(-6.47226819047899,-4.54905668767551,
-37.4527813341078));
#65296=CARTESIAN_POINT('Ctrl Pts',(-6.38907048960195,-4.66692526682044,
-37.4468864828682));
#65297=CARTESIAN_POINT('Ctrl Pts',(-6.31247247337594,-4.7700211987608,-37.4415147426215));
#65298=CARTESIAN_POINT('Ctrl Pts',(-6.20032993199196,-4.9135236342309,-37.4337763864183));
#65299=CARTESIAN_POINT('Ctrl Pts',(-6.16682813959291,-4.95550565985593,
-37.431479624319));
#65300=CARTESIAN_POINT('Ctrl Pts',(-6.05584973477682,-5.0917074226508,-37.4239275409087));
#65301=CARTESIAN_POINT('Ctrl Pts',(-5.97662192680819,-5.1844758551655,-37.4186238673784));
#65302=CARTESIAN_POINT('Ctrl Pts',(-5.41167651355209,-5.81580794641059,
-37.3815700789123));
#65303=CARTESIAN_POINT('Ctrl Pts',(-4.85596822372214,-6.28726235977595,
-37.3494025827222));
#65304=CARTESIAN_POINT('Ctrl Pts',(-4.14664146554219,-6.73814053072876,
-37.3147690013578));
#65305=CARTESIAN_POINT('Ctrl Pts',(-4.04815094056536,-6.7977678762687,-37.3100743517993));
#65306=CARTESIAN_POINT('Ctrl Pts',(-3.92472106725473,-6.86885956807116,
-37.3043217318996));
#65307=CARTESIAN_POINT('Ctrl Pts',(-3.90097910332909,-6.88237090457642,
-37.3032210636053));
#65308=CARTESIAN_POINT('Ctrl Pts',(-3.86338953558672,-6.90350578632141,
-37.3014874484482));
#65309=CARTESIAN_POINT('Ctrl Pts',(-3.84958831295894,-6.91121123018868,
-37.3008528496209));
#65310=CARTESIAN_POINT('Ctrl Pts',(-3.82371107118499,-6.92555734715423,
-37.2996664951357));
#65311=CARTESIAN_POINT('Ctrl Pts',(-3.8116406208102,-6.9322079241595,-37.2991145450163));
#65312=CARTESIAN_POINT('Ctrl Pts',(-3.78508059651708,-6.94675162389639,
-37.2979031119846));
#65313=CARTESIAN_POINT('Ctrl Pts',(-3.77058357404085,-6.95463102973133,
-37.2972438975247));
#65314=CARTESIAN_POINT('Ctrl Pts',(-3.7381551863088,-6.9721252696882,-37.2957737112228));
#65315=CARTESIAN_POINT('Ctrl Pts',(-3.72021115136542,-6.98171640548203,
-37.2949631914853));
#65316=CARTESIAN_POINT('Ctrl Pts',(-3.68402110957613,-7.00088094596724,
-37.293334403295));
#65317=CARTESIAN_POINT('Ctrl Pts',(-3.66577427122168,-7.01045252125632,
-37.2925161635183));
#65318=CARTESIAN_POINT('Ctrl Pts',(-3.45082124719638,-7.12213974821639,
-37.2829118562996));
#65319=CARTESIAN_POINT('Ctrl Pts',(-3.24994064461362,-7.21601918148237,
-37.2742819592309));
#65320=CARTESIAN_POINT('Ctrl Pts',(-2.50450852996305,-7.52693767661634,
-37.2433532648222));
#65321=CARTESIAN_POINT('Ctrl Pts',(-1.94025833784646,-7.69173280875099,
-37.2221441794592));
#65322=CARTESIAN_POINT('Ctrl Pts',(-1.10226686597287,-7.83830236860144,
-37.1906657194633));
#65323=CARTESIAN_POINT('Ctrl Pts',(-0.839429810923603,-7.87078926402653,
-37.1807676890986));
#65324=CARTESIAN_POINT('Ctrl Pts',(-0.473095344020291,-7.89750835825004,
-37.1665114592575));
#65325=CARTESIAN_POINT('Ctrl Pts',(-0.370586791446918,-7.9029818334549,
-37.1624719415133));
#65326=CARTESIAN_POINT('Ctrl Pts',(-0.252694815885022,-7.90697799124675,
-37.1577457021912));
#65327=CARTESIAN_POINT('Ctrl Pts',(-0.237384756964401,-7.90745244039719,
-37.1571303679746));
#65328=CARTESIAN_POINT('Ctrl Pts',(-0.214201750141736,-7.90810347828646,
-37.1561961438979));
#65329=CARTESIAN_POINT('Ctrl Pts',(-0.206329709239931,-7.90831278235552,
-37.1558784878495));
#65330=CARTESIAN_POINT('Ctrl Pts',(-0.192169871288246,-7.90866811152913,
-37.1553063136895));
#65331=CARTESIAN_POINT('Ctrl Pts',(-0.185882181307633,-7.90881839291601,
-37.1550519589696));
#65332=CARTESIAN_POINT('Ctrl Pts',(-0.17239137538223,-7.90912473811163,
-37.15450560673));
#65333=CARTESIAN_POINT('Ctrl Pts',(-0.165188215741935,-7.90927846027977,
-37.1542135184852));
#65334=CARTESIAN_POINT('Ctrl Pts',(-0.145763289389005,-7.90966645884243,
-37.1534248102971));
#65335=CARTESIAN_POINT('Ctrl Pts',(-0.133541203498214,-7.9098822476309,
-37.1529274618868));
#65336=CARTESIAN_POINT('Ctrl Pts',(-0.0795569260902536,-7.91071021796403,
-37.1507257067991));
#65337=CARTESIAN_POINT('Ctrl Pts',(-0.0377912921008751,-7.91101998350292,
-37.1490090899123));
#65338=CARTESIAN_POINT('Ctrl Pts',(0.746279780841901,-7.91062608934885,
-37.1165090588486));
#65339=CARTESIAN_POINT('Ctrl Pts',(1.48473784213369,-7.80578374461432,-37.0809906747664));
#65340=CARTESIAN_POINT('Ctrl Pts',(2.5239952840951,-7.50524873336213,-37.0320630245931));
#65341=CARTESIAN_POINT('Ctrl Pts',(2.84391900448066,-7.38995735815767,-37.0171048249811));
#65342=CARTESIAN_POINT('Ctrl Pts',(3.23762109589815,-7.2187088494996,-36.9990528123513));
#65343=CARTESIAN_POINT('Ctrl Pts',(3.31916674298965,-7.18157925903927,-36.9953324063199));
#65344=CARTESIAN_POINT('Ctrl Pts',(3.43174352031694,-7.1279932824626,-36.9902223764811));
#65345=CARTESIAN_POINT('Ctrl Pts',(3.46332068548813,-7.11270424636407,-36.9887919284498));
#65346=CARTESIAN_POINT('Ctrl Pts',(3.51048351028922,-7.08948039837846,-36.9866597050816));
#65347=CARTESIAN_POINT('Ctrl Pts',(3.52614605002107,-7.08170324386752,-36.985952311779));
#65348=CARTESIAN_POINT('Ctrl Pts',(3.55127170556941,-7.06912320485884,-36.9848186428435));
#65349=CARTESIAN_POINT('Ctrl Pts',(3.56075112431946,-7.06435312283342,-36.9843911894188));
#65350=CARTESIAN_POINT('Ctrl Pts',(3.5788350411953,-7.05520757517427,-36.9835762229094));
#65351=CARTESIAN_POINT('Ctrl Pts',(3.58744118064361,-7.05083540845978,-36.9831885917368));
#65352=CARTESIAN_POINT('Ctrl Pts',(3.60264165218483,-7.04307809622997,-36.9825043142645));
#65353=CARTESIAN_POINT('Ctrl Pts',(3.60923926056099,-7.03969941858782,-36.9822074343742));
#65354=CARTESIAN_POINT('Ctrl Pts',(3.62220456835119,-7.03303678339793,-36.9816242614886));
#65355=CARTESIAN_POINT('Ctrl Pts',(3.62857257285298,-7.02975343916738,-36.9813379466937));
#65356=CARTESIAN_POINT('Ctrl Pts',(3.64382363085682,-7.02186374646099,-36.9806525097189));
#65357=CARTESIAN_POINT('Ctrl Pts',(3.65270243345464,-7.01724918043411,-36.9802536869128));
#65358=CARTESIAN_POINT('Ctrl Pts',(3.68475668997787,-7.00051235156845,-36.9788146502941));
#65359=CARTESIAN_POINT('Ctrl Pts',(3.70788087016787,-6.98829196004266,-36.9777780210405));
#65360=CARTESIAN_POINT('Ctrl Pts',(4.06829471452783,-6.7955321817756,-36.9616437329532));
#65361=CARTESIAN_POINT('Ctrl Pts',(4.39212799681132,-6.59086745187698,-36.947494031072));
#65362=CARTESIAN_POINT('Ctrl Pts',(4.96383337233385,-6.16862482498478,-36.9224100057049));
#65363=CARTESIAN_POINT('Ctrl Pts',(5.21538206816902,-5.95746365722914,-36.9113207047966));
#65364=CARTESIAN_POINT('Ctrl Pts',(5.51660244329462,-5.67086438129691,-36.8973326211622));
#65365=CARTESIAN_POINT('Ctrl Pts',(5.5791010802608,-5.60938824274689,-36.8943869132303));
#65366=CARTESIAN_POINT('Ctrl Pts',(5.67104567810395,-5.51589083465691,-36.8899694860655));
#65367=CARTESIAN_POINT('Ctrl Pts',(5.70127024313005,-5.48464478187801,-36.8885033308486));
#65368=CARTESIAN_POINT('Ctrl Pts',(5.7972634321957,-5.38375640324336,-36.8837965646248));
#65369=CARTESIAN_POINT('Ctrl Pts',(5.86202486353776,-5.31316859436954,-36.880544399188));
#65370=CARTESIAN_POINT('Ctrl Pts',(6.03182102473429,-5.12121210985923,-36.8717621143674));
#65371=CARTESIAN_POINT('Ctrl Pts',(6.13446865397284,-4.99779650251522,-36.866179614706));
#65372=CARTESIAN_POINT('Ctrl Pts',(6.37046340959012,-4.69582190531446,-36.8524616648609));
#65373=CARTESIAN_POINT('Ctrl Pts',(6.50015349295495,-4.51459167351524,-36.8441825525713));
#65374=CARTESIAN_POINT('Ctrl Pts',(6.63864638757703,-4.3026990672836,-36.8341724311));
#65375=CARTESIAN_POINT('Ctrl Pts',(6.65513100642762,-4.27715750953957,-36.8329605374057));
#65376=CARTESIAN_POINT('Ctrl Pts',(6.67565321503586,-4.24495415826991,-36.8314251639933));
#65377=CARTESIAN_POINT('Ctrl Pts',(6.67982892877,-4.23838024895617,-36.8311113520266));
#65378=CARTESIAN_POINT('Ctrl Pts',(6.68644465939088,-4.22793091116827,-36.8306119153894));
#65379=CARTESIAN_POINT('Ctrl Pts',(6.6888910398079,-4.22405949651634,-36.830426740755));
#65380=CARTESIAN_POINT('Ctrl Pts',(6.69348320607412,-4.21677836749901,-36.8300782147641));
#65381=CARTESIAN_POINT('Ctrl Pts',(6.69562975276506,-4.21336913222301,-36.8299149176486));
#65382=CARTESIAN_POINT('Ctrl Pts',(6.70044078416009,-4.20571508971917,-36.8295480571607));
#65383=CARTESIAN_POINT('Ctrl Pts',(6.70310382214755,-4.2014694176372,-36.8293443923453));
#65384=CARTESIAN_POINT('Ctrl Pts',(6.70991397592451,-4.19058905797614,-36.828822028534));
#65385=CARTESIAN_POINT('Ctrl Pts',(6.71405525497882,-4.18395079432018,-36.8285029167931));
#65386=CARTESIAN_POINT('Ctrl Pts',(6.73781892124601,-4.1457326868581,-36.8266634130837));
#65387=CARTESIAN_POINT('Ctrl Pts',(6.75722802785665,-4.11402146489108,-36.8251280794695));
#65388=CARTESIAN_POINT('Ctrl Pts',(7.09368322141513,-3.55550569434129,-36.7979480552711));
#65389=CARTESIAN_POINT('Ctrl Pts',(7.34845571558426,-2.99367510098595,-36.7686212590121));
#65390=CARTESIAN_POINT('Ctrl Pts',(7.64558335139573,-2.06386546927526,-36.7232170676629));
#65391=CARTESIAN_POINT('Ctrl Pts',(7.7318685613809,-1.7125218871774,-36.7066763668442));
#65392=CARTESIAN_POINT('Ctrl Pts',(7.8362881398365,-1.1125678924626,-36.6800292468911));
#65393=CARTESIAN_POINT('Ctrl Pts',(7.86726945297144,-0.866779205352294,
-36.6695441449394));
#65394=CARTESIAN_POINT('Ctrl Pts',(7.88996304109896,-0.578071526730317,
-36.6577391462557));
#65395=CARTESIAN_POINT('Ctrl Pts',(7.89291966738994,-0.536192764212517,
-36.6560390689986));
#65396=CARTESIAN_POINT('Ctrl Pts',(7.89633415811472,-0.481651605205528,
-36.6538407098114));
#65397=CARTESIAN_POINT('Ctrl Pts',(7.89709514194546,-0.469009303260957,
-36.6533322439661));
#65398=CARTESIAN_POINT('Ctrl Pts',(7.89819957195826,-0.449896110454877,
-36.6525651753496));
#65399=CARTESIAN_POINT('Ctrl Pts',(7.89856543108893,-0.44342656637629,-36.6523058196505));
#65400=CARTESIAN_POINT('Ctrl Pts',(7.89928004152794,-0.430508456265079,
-36.6517885185563));
#65401=CARTESIAN_POINT('Ctrl Pts',(7.89962884623889,-0.424059898294344,
-36.6515305715585));
#65402=CARTESIAN_POINT('Ctrl Pts',(7.90039931244321,-0.409484944508133,
-36.6509482005867));
#65403=CARTESIAN_POINT('Ctrl Pts',(7.9008163329911,-0.401358304658727,-36.6506239326938));
#65404=CARTESIAN_POINT('Ctrl Pts',(7.90191173921254,-0.379348224021622,
-36.6497468975114));
#65405=CARTESIAN_POINT('Ctrl Pts',(7.90256607569152,-0.365463584242073,
-36.6491949375829));
#65406=CARTESIAN_POINT('Ctrl Pts',(7.90543006229951,-0.301083385969035,
-36.6466415937777));
#65407=CARTESIAN_POINT('Ctrl Pts',(7.90719237138449,-0.250568562800633,
-36.6446552198575));
#65408=CARTESIAN_POINT('Ctrl Pts',(7.92934324276393,0.625155307034691,-36.6105043400619));
#65409=CARTESIAN_POINT('Ctrl Pts',(7.82095457630954,1.44841150599309,-36.5835525351485));
#65410=CARTESIAN_POINT('Ctrl Pts',(7.57291219708224,2.28855420027638,-36.5533025338191));
#65411=CARTESIAN_POINT('Ctrl Pts',(7.55812497264545,2.33692667961003,-36.5515480011804));
#65412=CARTESIAN_POINT('Ctrl Pts',(7.44040459893448,2.70920879317726,-36.5379238560629));
#65413=CARTESIAN_POINT('Ctrl Pts',(7.31716695785351,3.0262938873901,-36.5256191386117));
#65414=CARTESIAN_POINT('Ctrl Pts',(7.16830818070849,3.34655905283701,-36.5114878601219));
#65415=CARTESIAN_POINT('Ctrl Pts',(7.16264357224805,3.3586659142455,-36.5109510316382));
#65416=CARTESIAN_POINT('Ctrl Pts',(7.15445974513855,3.37604218953926,-36.5101767287743));
#65417=CARTESIAN_POINT('Ctrl Pts',(7.15196539131631,3.38132313620158,-36.509940899095));
#65418=CARTESIAN_POINT('Ctrl Pts',(7.14761846766423,3.3904999410864,-36.509530219597));
#65419=CARTESIAN_POINT('Ctrl Pts',(7.14576855196236,3.39439706154809,-36.5093555417459));
#65420=CARTESIAN_POINT('Ctrl Pts',(7.14219990844338,3.40189908981225,-36.5090187580625));
#65421=CARTESIAN_POINT('Ctrl Pts',(7.14048163620965,3.40550421410387,-36.5088566815429));
#65422=CARTESIAN_POINT('Ctrl Pts',(7.13641934464273,3.41401075801059,-36.5084737007591));
#65423=CARTESIAN_POINT('Ctrl Pts',(7.13407300721182,3.4189110614175,-36.5082526484939));
#65424=CARTESIAN_POINT('Ctrl Pts',(7.12710460103978,3.43342610416973,-36.5075966059898));
#65425=CARTESIAN_POINT('Ctrl Pts',(7.12246814567264,3.44303388288791,-36.5071607058831));
#65426=CARTESIAN_POINT('Ctrl Pts',(7.08120074850047,3.52810914404482,-36.5032864100088));
#65427=CARTESIAN_POINT('Ctrl Pts',(7.04339221447428,3.60299643762418,-36.4997750132669));
#65428=CARTESIAN_POINT('Ctrl Pts',(6.90609219613828,3.86452348037295,-36.487190749631));
#65429=CARTESIAN_POINT('Ctrl Pts',(6.80031893456534,4.04775278822696,-36.4777901259391));
#65430=CARTESIAN_POINT('Ctrl Pts',(6.30128577960179,4.83734099834449,-36.4353460759295));
#65431=CARTESIAN_POINT('Ctrl Pts',(5.83327964164717,5.3925075386169,-36.4006266502012));
#65432=CARTESIAN_POINT('Ctrl Pts',(5.05880547240706,6.09054410989927,-36.3546380653008));
#65433=CARTESIAN_POINT('Ctrl Pts',(4.80841510011181,6.29010462281645,-36.3410639428603));
#65434=CARTESIAN_POINT('Ctrl Pts',(4.52824817609912,6.48686308355301,-36.327190282024));
#65435=CARTESIAN_POINT('Ctrl Pts',(4.50983582460034,6.49967730391375,-36.3262842061157));
#65436=CARTESIAN_POINT('Ctrl Pts',(4.48279948697111,6.5183232604816,-36.3249619908701));
#65437=CARTESIAN_POINT('Ctrl Pts',(4.47421817744401,6.52421651006624,-36.3245435306302));
#65438=CARTESIAN_POINT('Ctrl Pts',(4.45910166665309,6.5345539851972,-36.3238085045496));
#65439=CARTESIAN_POINT('Ctrl Pts',(4.45257140086587,6.53900538152787,-36.3234916693953));
#65440=CARTESIAN_POINT('Ctrl Pts',(4.43985255456151,6.54764737542861,-36.3228759198539));
#65441=CARTESIAN_POINT('Ctrl Pts',(4.43366468533356,6.55183900272528,-36.3225769670415));
#65442=CARTESIAN_POINT('Ctrl Pts',(4.41711828319405,6.56301326588214,-36.3217792063909));
#65443=CARTESIAN_POINT('Ctrl Pts',(4.40674911648145,6.56998015842378,-36.321280986726));
#65444=CARTESIAN_POINT('Ctrl Pts',(4.36936609337057,6.59496895178782,-36.3194909316489));
#65445=CARTESIAN_POINT('Ctrl Pts',(4.34225766850095,6.6128491518278,-36.3182043610287));
#65446=CARTESIAN_POINT('Ctrl Pts',(3.8958964077793,6.90333230344256,-36.2972050167528));
#65447=CARTESIAN_POINT('Ctrl Pts',(3.45181104172885,7.13576009545579,-36.2790748099056));
#65448=CARTESIAN_POINT('Ctrl Pts',(2.8020593427605,7.4008803862583,-36.2544801072376));
#65449=CARTESIAN_POINT('Ctrl Pts',(2.61254753033994,7.46988375050931,-36.2475078331805));
#65450=CARTESIAN_POINT('Ctrl Pts',(1.92434919993394,7.6910669604578,-36.2224343342477));
#65451=CARTESIAN_POINT('Ctrl Pts',(1.41352853388726,7.80112780467744,-36.2042562882558));
#65452=CARTESIAN_POINT('Ctrl Pts',(0.85807071809913,7.86441746461932,-36.1821469324375));
#65453=CARTESIAN_POINT('Ctrl Pts',(0.820515854500712,7.86842430783968,-36.1806429552084));
#65454=CARTESIAN_POINT('Ctrl Pts',(0.770703364800185,7.87337846131501,-36.1786370144707));
#65455=CARTESIAN_POINT('Ctrl Pts',(0.758469807700295,7.87456637666376,-36.1781434864491));
#65456=CARTESIAN_POINT('Ctrl Pts',(0.738379286970201,7.87646997532498,-36.177331582769));
#65457=CARTESIAN_POINT('Ctrl Pts',(0.730523909257359,7.87720242605999,-36.1770137756065));
#65458=CARTESIAN_POINT('Ctrl Pts',(0.715298655577549,7.87859908801104,-36.1763971318763));
#65459=CARTESIAN_POINT('Ctrl Pts',(0.707928915023725,7.87926471234134,-36.1760983424647));
#65460=CARTESIAN_POINT('Ctrl Pts',(0.69090621322045,7.88077810263616,-36.1754075049309));
#65461=CARTESIAN_POINT('Ctrl Pts',(0.681252615580431,7.8816184741035,-36.1750152172217));
#65462=CARTESIAN_POINT('Ctrl Pts',(0.65532220320219,7.88382778977752,-36.1739601548447));
#65463=CARTESIAN_POINT('Ctrl Pts',(0.639042691671107,7.8851640593566,-36.1732963497333));
#65464=CARTESIAN_POINT('Ctrl Pts',(0.521523476562182,7.89444404921093,-36.1684946251035));
#65465=CARTESIAN_POINT('Ctrl Pts',(0.420145120151339,7.90048801185732,-36.1642999520708));
#65466=CARTESIAN_POINT('Ctrl Pts',(-0.209180713104586,7.92585989448046,
-36.1380188316244));
#65467=CARTESIAN_POINT('Ctrl Pts',(-0.737844362038266,7.89421311080287,
-36.1150069505851));
#65468=CARTESIAN_POINT('Ctrl Pts',(-1.98910054495842,7.69244483530152,-36.0607932867541));
#65469=CARTESIAN_POINT('Ctrl Pts',(-2.698737292223,7.47309241050851,-36.0302256528162));
#65470=CARTESIAN_POINT('Ctrl Pts',(-3.4276097422322,7.13020419761666,-35.9975164125075));
#65471=CARTESIAN_POINT('Ctrl Pts',(-3.48727116714997,7.10121541291687,-35.9948309746968));
#65472=CARTESIAN_POINT('Ctrl Pts',(-3.57283208578464,7.05830402001027,-35.9909680213152));
#65473=CARTESIAN_POINT('Ctrl Pts',(-3.5990293312361,7.04498208891827,-35.9897836408525));
#65474=CARTESIAN_POINT('Ctrl Pts',(-3.6446765389618,7.02144831705688,-35.9877170574925));
#65475=CARTESIAN_POINT('Ctrl Pts',(-3.66415930814574,7.01130088576769,-35.9868340954848));
#65476=CARTESIAN_POINT('Ctrl Pts',(-3.70182855099322,6.99148129251876,-35.9851251051604));
#65477=CARTESIAN_POINT('Ctrl Pts',(-3.7200200097285,6.98181899039991,-35.9842989639616));
#65478=CARTESIAN_POINT('Ctrl Pts',(-3.76334164696845,6.95859153668349,-35.9823295588024));
#65479=CARTESIAN_POINT('Ctrl Pts',(-3.78843654579443,6.94496112822049,-35.9811871208501));
#65480=CARTESIAN_POINT('Ctrl Pts',(-3.87867729703123,6.89531179174015,-35.9770728889689));
#65481=CARTESIAN_POINT('Ctrl Pts',(-3.94338810630175,6.85850950723549,-35.9741112202626));
#65482=CARTESIAN_POINT('Ctrl Pts',(-4.42325726081035,6.57656170287584,-35.9520535054794));
#65483=CARTESIAN_POINT('Ctrl Pts',(-4.81574937525418,6.29483448008435,-35.9335449453065));
#65484=CARTESIAN_POINT('Ctrl Pts',(-5.4563141483298,5.73986644266791,-35.9009740292749));
#65485=CARTESIAN_POINT('Ctrl Pts',(-5.71555839624837,5.48177019544208,-35.8869375065442));
#65486=CARTESIAN_POINT('Ctrl Pts',(-5.97447397431258,5.18559228683308,-35.8712206481904));
#65487=CARTESIAN_POINT('Ctrl Pts',(-5.99280928880847,5.16439187650242,-35.8700975367698));
#65488=CARTESIAN_POINT('Ctrl Pts',(-6.01983591005004,5.13280430392408,-35.8684264615334));
#65489=CARTESIAN_POINT('Ctrl Pts',(-6.02861386087113,5.12249151498152,-35.8678812548076));
#65490=CARTESIAN_POINT('Ctrl Pts',(-6.04377031616883,5.10459201189912,-35.8669356417218));
#65491=CARTESIAN_POINT('Ctrl Pts',(-6.05016113397797,5.0970157440192,-35.8665356050787));
#65492=CARTESIAN_POINT('Ctrl Pts',(-6.0633977480039,5.08126386393095,-35.8657043403288));
#65493=CARTESIAN_POINT('Ctrl Pts',(-6.07024128559197,5.07308638200377,-35.8652730479767));
#65494=CARTESIAN_POINT('Ctrl Pts',(-6.08687056059915,5.05313389785313,-35.8642213681008));
#65495=CARTESIAN_POINT('Ctrl Pts',(-6.09663867715392,5.04134428987303,-35.8636004906358));
#65496=CARTESIAN_POINT('Ctrl Pts',(-6.13359387258776,4.99647680748224,-35.8612398147393));
#65497=CARTESIAN_POINT('Ctrl Pts',(-6.16054633187781,4.96320693986651,-35.8594938339987));
#65498=CARTESIAN_POINT('Ctrl Pts',(-6.44783167812667,4.60263886266071,-35.840627145596));
#65499=CARTESIAN_POINT('Ctrl Pts',(-6.6820859261543,4.25541250915445,-35.8229797949973));
#65500=CARTESIAN_POINT('Ctrl Pts',(-7.03994298738624,3.62198927814194,-35.7924469388437));
#65501=CARTESIAN_POINT('Ctrl Pts',(-7.17617196042905,3.34397466834248,-35.779536768843));
#65502=CARTESIAN_POINT('Ctrl Pts',(-7.33892386593008,2.95576942802021,-35.7622094778198));
#65503=CARTESIAN_POINT('Ctrl Pts',(-7.37989169441482,2.85194239758499,-35.7576391863045));
#65504=CARTESIAN_POINT('Ctrl Pts',(-7.4472357576786,2.67008923898223,-35.7497401651053));
#65505=CARTESIAN_POINT('Ctrl Pts',(-7.47461565903563,2.59245403093063,-35.7464008099209));
#65506=CARTESIAN_POINT('Ctrl Pts',(-7.51215983333576,2.48045515221475,-35.7416276414148));
#65507=CARTESIAN_POINT('Ctrl Pts',(-7.52330993310817,2.44642816948199,-35.7401832793307));
#65508=CARTESIAN_POINT('Ctrl Pts',(-7.54233007878435,2.38702405365369,-35.7376714786114));
#65509=CARTESIAN_POINT('Ctrl Pts',(-7.55030399794099,2.36168084093396,-35.7366029613231));
#65510=CARTESIAN_POINT('Ctrl Pts',(-7.565487595315,2.31256043178719,-35.7345377356777));
#65511=CARTESIAN_POINT('Ctrl Pts',(-7.5727132213212,2.28878849562426,-35.7335408741272));
#65512=CARTESIAN_POINT('Ctrl Pts',(-7.58969399611725,2.23196187114615,-35.7311639277338));
#65513=CARTESIAN_POINT('Ctrl Pts',(-7.59934537785147,2.19887666519629,-35.7297849032229));
#65514=CARTESIAN_POINT('Ctrl Pts',(-7.63394801414356,2.07730844877326,-35.724734842826));
#65515=CARTESIAN_POINT('Ctrl Pts',(-7.657572681896,1.98845505174388,-35.7210768224582));
#65516=CARTESIAN_POINT('Ctrl Pts',(-7.83053002696736,1.28908477186011,-35.6925051429103));
#65517=CARTESIAN_POINT('Ctrl Pts',(-7.90817944247995,0.663114381764724,
-35.6682303155321));
#65518=CARTESIAN_POINT('Ctrl Pts',(-7.91097491555085,0.0230183952757,-35.6442717049117));
#65519=CARTESIAN_POINT('Ctrl Pts',(-7.91100006308073,0.0114875306561859,
-35.6438403068342));
#65520=CARTESIAN_POINT('Ctrl Pts',(-7.91099762551218,-0.433264208104541,
-35.6272082196128));
#65521=CARTESIAN_POINT('Ctrl Pts',(-7.87540975307761,-0.86573933378559,
-35.6113586004474));
#65522=CARTESIAN_POINT('Ctrl Pts',(-7.77046872412384,-1.49911219422672,
-35.5870431545332));
#65523=CARTESIAN_POINT('Ctrl Pts',(-7.72819625901884,-1.70367164050496,
-35.5790038503414));
#65524=CARTESIAN_POINT('Ctrl Pts',(-7.67303583723596,-1.92583666242136,
-35.5698763507552));
#65525=CARTESIAN_POINT('Ctrl Pts',(-7.66811310799267,-1.94534499873562,
-35.5690714532635));
#65526=CARTESIAN_POINT('Ctrl Pts',(-7.6611046790867,-1.97267880785223,-35.567938657577));
#65527=CARTESIAN_POINT('Ctrl Pts',(-7.65908127959233,-1.98052026873652,
-35.5676131025769));
#65528=CARTESIAN_POINT('Ctrl Pts',(-7.65535334490466,-1.99487631444721,
-35.5670159954335));
#65529=CARTESIAN_POINT('Ctrl Pts',(-7.65365252415963,-2.00139186177033,
-35.5667445861702));
#65530=CARTESIAN_POINT('Ctrl Pts',(-7.6501940923712,-2.0145716294404,-35.5661947319215));
#65531=CARTESIAN_POINT('Ctrl Pts',(-7.64843608753133,-2.02123573975508,
-35.5659162717187));
#65532=CARTESIAN_POINT('Ctrl Pts',(-7.64409570543554,-2.03760218153334,
-35.5652313095971));
#65533=CARTESIAN_POINT('Ctrl Pts',(-7.64150356627544,-2.0473018950403,-35.5648244194402));
#65534=CARTESIAN_POINT('Ctrl Pts',(-7.63203110653457,-2.08247896122746,
-35.5633452922324));
#65535=CARTESIAN_POINT('Ctrl Pts',(-7.62504182683714,-2.10792659997468,
-35.5622686092578));
#65536=CARTESIAN_POINT('Ctrl Pts',(-7.52536283990521,-2.46386967251659,
-35.5471098150298));
#65537=CARTESIAN_POINT('Ctrl Pts',(-7.41140481046643,-2.78796166301723,
-35.5319719820265));
#65538=CARTESIAN_POINT('Ctrl Pts',(-7.00452647881092,-3.74194919107196,
-35.4849380674929));
#65539=CARTESIAN_POINT('Ctrl Pts',(-6.64938958715585,-4.3418175869482,-35.4522725299542));
#65540=CARTESIAN_POINT('Ctrl Pts',(-6.05762591733933,-5.09495916674867,
-35.4106724477684));
#65541=CARTESIAN_POINT('Ctrl Pts',(-5.8844549938626,-5.2940199062029,-35.399570596877));
#65542=CARTESIAN_POINT('Ctrl Pts',(-5.68409276339649,-5.50233152688531,
-35.3878326825618));
#65543=CARTESIAN_POINT('Ctrl Pts',(-5.66644350084613,-5.52050548783489,
-35.3868074887323));
#65544=CARTESIAN_POINT('Ctrl Pts',(-5.64146717168599,-5.5459783708589,-35.3853689022681));
#65545=CARTESIAN_POINT('Ctrl Pts',(-5.63421271468866,-5.55334809154366,
-35.3849524982774));
#65546=CARTESIAN_POINT('Ctrl Pts',(-5.62157429834714,-5.56613705925956,
-35.3842295461687));
#65547=CARTESIAN_POINT('Ctrl Pts',(-5.61619690874079,-5.57156276434006,
-35.3839227245571));
#65548=CARTESIAN_POINT('Ctrl Pts',(-5.60496829158744,-5.58285949632484,
-35.3832836658961));
#65549=CARTESIAN_POINT('Ctrl Pts',(-5.59911567676641,-5.58872913497522,
-35.3829514875609));
#65550=CARTESIAN_POINT('Ctrl Pts',(-5.58527084741467,-5.60257065879835,
-35.3821678434919));
#65551=CARTESIAN_POINT('Ctrl Pts',(-5.57727076473569,-5.61053466649369,
-35.3817167093311));
#65552=CARTESIAN_POINT('Ctrl Pts',(-5.55087901208505,-5.63669518040547,
-35.380233968605));
#65553=CARTESIAN_POINT('Ctrl Pts',(-5.53241503937061,-5.65481867182481,
-35.3792054187525));
#65554=CARTESIAN_POINT('Ctrl Pts',(-5.25445701072294,-5.92498656794431,
-35.3638516409251));
#65555=CARTESIAN_POINT('Ctrl Pts',(-4.97805269959303,-6.15904285466105,
-35.3502992519259));
#65556=CARTESIAN_POINT('Ctrl Pts',(-4.46722501297464,-6.53467320750191,
-35.3274539326845));
#65557=CARTESIAN_POINT('Ctrl Pts',(-4.23968781674317,-6.68454238024796,
-35.3179451525401));
#65558=CARTESIAN_POINT('Ctrl Pts',(-3.78392362052155,-6.95208484434698,
-35.2996388159202));
#65559=CARTESIAN_POINT('Ctrl Pts',(-3.5568070146853,-7.07097469710224,-35.2908416258373));
#65560=CARTESIAN_POINT('Ctrl Pts',(-3.21658183206928,-7.22852823133639,
-35.2777148970113));
#65561=CARTESIAN_POINT('Ctrl Pts',(-3.10773045924041,-7.27598994043385,
-35.2735217812319));
#65562=CARTESIAN_POINT('Ctrl Pts',(-2.72981047278163,-7.43074360231403,
-35.2588788098745));
#65563=CARTESIAN_POINT('Ctrl Pts',(-2.45594898219325,-7.52569735684425,
-35.248120713389));
#65564=CARTESIAN_POINT('Ctrl Pts',(-2.16049365823181,-7.61028917634762,
-35.2358616796864));
#65565=CARTESIAN_POINT('Ctrl Pts',(-2.14346375334845,-7.61510323799295,
-35.2351529788124));
#65566=CARTESIAN_POINT('Ctrl Pts',(-2.11954711484406,-7.62177747724523,
-35.2341548896942));
#65567=CARTESIAN_POINT('Ctrl Pts',(-2.11267371174344,-7.62368557011198,
-35.2338677253339));
#65568=CARTESIAN_POINT('Ctrl Pts',(-2.10074969967808,-7.62697837452272,
-35.2333690018159));
#65569=CARTESIAN_POINT('Ctrl Pts',(-2.09570027221066,-7.62836737414888,
-35.233157638081));
#65570=CARTESIAN_POINT('Ctrl Pts',(-2.08519915329935,-7.63124481507142,
-35.2327177228191));
#65571=CARTESIAN_POINT('Ctrl Pts',(-2.07974723900186,-7.63273243066278,
-35.2324891343224));
#65572=CARTESIAN_POINT('Ctrl Pts',(-2.0669228801507,-7.63621693956748,-35.2319509807382));
#65573=CARTESIAN_POINT('Ctrl Pts',(-2.0595491359283,-7.63820899797494,-35.2316412021114));
#65574=CARTESIAN_POINT('Ctrl Pts',(-2.03550566598467,-7.64466712877018,
-35.2306299923322));
#65575=CARTESIAN_POINT('Ctrl Pts',(-2.01882428102815,-7.64908931453851,
-35.2299266625003));
#65576=CARTESIAN_POINT('Ctrl Pts',(-1.97958629193512,-7.65935389218984,
-35.2282683895571));
#65577=CARTESIAN_POINT('Ctrl Pts',(-1.95701814457604,-7.66515126397186,
-35.2273115945122));
#65578=CARTESIAN_POINT('Ctrl Pts',(-1.70082120016819,-7.72975868291033,
-35.2164181869762));
#65579=CARTESIAN_POINT('Ctrl Pts',(-1.46465799305012,-7.77796428603496,
-35.2060823536449));
#65580=CARTESIAN_POINT('Ctrl Pts',(-0.748549508464131,-7.89036322858865,
-35.1745103794928));
#65581=CARTESIAN_POINT('Ctrl Pts',(-0.264515694422575,-7.92137748778909,
-35.1529389995076));
#65582=CARTESIAN_POINT('Ctrl Pts',(0.592938821828755,-7.89759768850724,
-35.1159785226326));
#65583=CARTESIAN_POINT('Ctrl Pts',(0.965377247226943,-7.86076988579311,
-35.1003244704665));
#65584=CARTESIAN_POINT('Ctrl Pts',(1.37281518020253,-7.7910758681119,-35.0835727804889));
#65585=CARTESIAN_POINT('Ctrl Pts',(1.41174239337147,-7.78411640141012,-35.0819757131983));
#65586=CARTESIAN_POINT('Ctrl Pts',(1.46843066395291,-7.77354235784925,-35.0796544182308));
#65587=CARTESIAN_POINT('Ctrl Pts',(1.48623389388585,-7.77015818500329,-35.0789260459248));
#65588=CARTESIAN_POINT('Ctrl Pts',(1.51772057623712,-7.76406078314223,-35.0776389191964));
#65589=CARTESIAN_POINT('Ctrl Pts',(1.53140875673541,-7.76137248256273,-35.0770797253856));
#65590=CARTESIAN_POINT('Ctrl Pts',(1.55980095615707,-7.755718340598,-35.0759205426458));
#65591=CARTESIAN_POINT('Ctrl Pts',(1.57450379788584,-7.75274685474108,-35.0753206548458));
#65592=CARTESIAN_POINT('Ctrl Pts',(1.61240549244743,-7.7449745485653,-35.0737751858412));
#65593=CARTESIAN_POINT('Ctrl Pts',(1.63559143000825,-7.74011129834192,-35.0728306827089));
#65594=CARTESIAN_POINT('Ctrl Pts',(1.7289456021244,-7.72009205588672,-35.0690311088362));
#65595=CARTESIAN_POINT('Ctrl Pts',(1.79892871156013,-7.70408527621593,-35.0661900825253));
#65596=CARTESIAN_POINT('Ctrl Pts',(2.23770390295012,-7.59742222810576,-35.0484192294951));
#65597=CARTESIAN_POINT('Ctrl Pts',(2.59979382924729,-7.4812590359623,-35.0339707284821));
#65598=CARTESIAN_POINT('Ctrl Pts',(3.5407244301004,-7.10279194348282,-34.9961758761288));
#65599=CARTESIAN_POINT('Ctrl Pts',(4.09864149704759,-6.79613295558115,-34.9736097722637));
#65600=CARTESIAN_POINT('Ctrl Pts',(4.70396036629784,-6.36152245801653,-34.9447716993639));
#65601=CARTESIAN_POINT('Ctrl Pts',(4.79264226889207,-6.29498132670956,-34.9404187951235));
#65602=CARTESIAN_POINT('Ctrl Pts',(4.89323880580509,-6.2161420872334,-34.9353025206132));
#65603=CARTESIAN_POINT('Ctrl Pts',(4.90654975584002,-6.20564081681379,-34.9346218504229));
#65604=CARTESIAN_POINT('Ctrl Pts',(4.92625388151001,-6.18999281534984,-34.9336086418575));
#65605=CARTESIAN_POINT('Ctrl Pts',(4.93267302013859,-6.18487875668803,-34.9332776733857));
#65606=CARTESIAN_POINT('Ctrl Pts',(4.94407013503759,-6.17576976898899,-34.9326884413778));
#65607=CARTESIAN_POINT('Ctrl Pts',(4.94905126260671,-6.17177878245103,-34.9324303712347));
#65608=CARTESIAN_POINT('Ctrl Pts',(4.95950457480096,-6.16338257156014,-34.9318876325583));
#65609=CARTESIAN_POINT('Ctrl Pts',(4.96497573052723,-6.15897607932861,-34.9316029009146));
#65610=CARTESIAN_POINT('Ctrl Pts',(4.97932597885788,-6.1473867803685,-34.9308543081485));
#65611=CARTESIAN_POINT('Ctrl Pts',(4.98819537985467,-6.14019203948405,-34.9303898423009));
#65612=CARTESIAN_POINT('Ctrl Pts',(5.02742522801277,-6.10822820814862,-34.9283274319327));
#65613=CARTESIAN_POINT('Ctrl Pts',(5.05761663504678,-6.08325325465704,-34.9267187660813));
#65614=CARTESIAN_POINT('Ctrl Pts',(5.26768446062512,-5.90683600722821,-34.9153669425712));
#65615=CARTESIAN_POINT('Ctrl Pts',(5.44088726497666,-5.74768861053685,-34.90513123598));
#65616=CARTESIAN_POINT('Ctrl Pts',(5.92339599696948,-5.26296353557398,-34.8745333269023));
#65617=CARTESIAN_POINT('Ctrl Pts',(6.21241409076899,-4.91846703608904,-34.8535621020513));
#65618=CARTESIAN_POINT('Ctrl Pts',(6.76706166340391,-4.12991917886488,-34.8096257209357));
#65619=CARTESIAN_POINT('Ctrl Pts',(7.02162366245384,-3.68052795501237,-34.7869716560156));
#65620=CARTESIAN_POINT('Ctrl Pts',(7.2440879241625,-3.17933972295181,-34.7646586182065));
#65621=CARTESIAN_POINT('Ctrl Pts',(7.25729289881124,-3.14908093629346,-34.7633218557471));
#65622=CARTESIAN_POINT('Ctrl Pts',(7.27514369911938,-3.10746771609591,-34.7614975728146));
#65623=CARTESIAN_POINT('Ctrl Pts',(7.27995300924211,-3.09618404402211,-34.7610043217873));
#65624=CARTESIAN_POINT('Ctrl Pts',(7.28755002653919,-3.07824425351844,-34.7602223444753));
#65625=CARTESIAN_POINT('Ctrl Pts',(7.29035489281484,-3.07159545038098,-34.7599330169151));
#65626=CARTESIAN_POINT('Ctrl Pts',(7.29578036711737,-3.05868532317851,-34.7593721660426));
#65627=CARTESIAN_POINT('Ctrl Pts',(7.29840202156909,-3.05242444678329,-34.759100606208));
#65628=CARTESIAN_POINT('Ctrl Pts',(7.30463164796263,-3.03749332146113,-34.7584540036308));
#65629=CARTESIAN_POINT('Ctrl Pts',(7.30823224945373,-3.02881999781881,-34.7580792192978));
#65630=CARTESIAN_POINT('Ctrl Pts',(7.31890395523677,-3.0029835937782,-34.7569652302405));
#65631=CARTESIAN_POINT('Ctrl Pts',(7.32593012786765,-2.98580195899009,-34.7562275988927));
#65632=CARTESIAN_POINT('Ctrl Pts',(7.38340376055676,-2.84383309373227,-34.7501587976858));
#65633=CARTESIAN_POINT('Ctrl Pts',(7.43072081848879,-2.71779840093948,-34.744937894455));
#65634=CARTESIAN_POINT('Ctrl Pts',(7.58321345841792,-2.27780529355867,-34.7272431528378));
#65635=CARTESIAN_POINT('Ctrl Pts',(7.6718886615137,-1.95848708701791,-34.7153392914277));
#65636=CARTESIAN_POINT('Ctrl Pts',(7.835197542763,-1.18514102093041,-34.6878886196244));
#65637=CARTESIAN_POINT('Ctrl Pts',(7.89077800856185,-0.728350936736043,
-34.6727928426398));
#65638=CARTESIAN_POINT('Ctrl Pts',(7.91631565513461,0.021349773999759,-34.6472012598829));
#65639=CARTESIAN_POINT('Ctrl Pts',(7.91017943541785,0.31233066044255,-34.6370514594814));
#65640=CARTESIAN_POINT('Ctrl Pts',(7.87744582784855,0.741032525252417,-34.6210032087692));
#65641=CARTESIAN_POINT('Ctrl Pts',(7.8631943369072,0.879461643933766,-34.615650124476));
#65642=CARTESIAN_POINT('Ctrl Pts',(7.84364293976988,1.03021969383116,-34.6095669673779));
#65643=CARTESIAN_POINT('Ctrl Pts',(7.84195375766663,1.04299973295427,-34.6090492897763));
#65644=CARTESIAN_POINT('Ctrl Pts',(7.83954109214129,1.06091628860935,-34.6083206796611));
#65645=CARTESIAN_POINT('Ctrl Pts',(7.83884377448122,1.06605637085358,-34.6081113172853));
#65646=CARTESIAN_POINT('Ctrl Pts',(7.83762636236382,1.07496440499251,-34.6077479013901));
#65647=CARTESIAN_POINT('Ctrl Pts',(7.83710860417076,1.07873267974389,-34.6075939893686));
#65648=CARTESIAN_POINT('Ctrl Pts',(7.83602713009787,1.08656183669143,-34.6072738376019));
#65649=CARTESIAN_POINT('Ctrl Pts',(7.83546297490771,1.09062265578152,-34.6071075711264));
#65650=CARTESIAN_POINT('Ctrl Pts',(7.8341263851294,1.10018893314528,-34.6067153891645));
#65651=CARTESIAN_POINT('Ctrl Pts',(7.83335130932743,1.10569397704878,-34.6064893116876));
#65652=CARTESIAN_POINT('Ctrl Pts',(7.83075246659903,1.1240125980999,-34.6057357182032));
#65653=CARTESIAN_POINT('Ctrl Pts',(7.82890306802288,1.13682244054341,-34.6052066367563));
#65654=CARTESIAN_POINT('Ctrl Pts',(7.78075620307085,1.46462126881256,-34.5916148029));
#65655=CARTESIAN_POINT('Ctrl Pts',(7.71552118288662,1.77650662751726,-34.5774421260612));
#65656=CARTESIAN_POINT('Ctrl Pts',(7.53610070933983,2.43368380429925,-34.5462216207576));
#65657=CARTESIAN_POINT('Ctrl Pts',(7.41653883908029,2.77679361749781,-34.5290970696112));
#65658=CARTESIAN_POINT('Ctrl Pts',(7.04737857539898,3.64007257618154,-34.4855560537162));
#65659=CARTESIAN_POINT('Ctrl Pts',(6.76372588247223,4.14341428172199,-34.4598467180261));
#65660=CARTESIAN_POINT('Ctrl Pts',(6.40530712137303,4.64300118916018,-34.4348069840798));
#65661=CARTESIAN_POINT('Ctrl Pts',(6.38251196662498,4.67428715606589,-34.4332401587761));
#65662=CARTESIAN_POINT('Ctrl Pts',(6.35189072963362,4.71567262455864,-34.4311690087661));
#65663=CARTESIAN_POINT('Ctrl Pts',(6.34426870957117,4.72592199323101,-34.430656195847));
#65664=CARTESIAN_POINT('Ctrl Pts',(6.33235885378093,4.74185649840118,-34.4298591118876));
#65665=CARTESIAN_POINT('Ctrl Pts',(6.32808812585682,4.74755435737609,-34.4295741260206));
#65666=CARTESIAN_POINT('Ctrl Pts',(6.31953825490305,4.75892926869899,-34.4290052631051));
#65667=CARTESIAN_POINT('Ctrl Pts',(6.31525914086791,4.76460633460062,-34.4287213852677));
#65668=CARTESIAN_POINT('Ctrl Pts',(6.30562048504548,4.77735806421826,-34.4280838172497));
#65669=CARTESIAN_POINT('Ctrl Pts',(6.30025667402075,4.78442949758283,-34.4277303068892));
#65670=CARTESIAN_POINT('Ctrl Pts',(6.28447615238046,4.80516135045984,-34.4266940361215));
#65671=CARTESIAN_POINT('Ctrl Pts',(6.27402680130437,4.81879692614263,-34.42601265078));
#65672=CARTESIAN_POINT('Ctrl Pts',(6.19549273585925,4.92058917790372,-34.4209271804231));
#65673=CARTESIAN_POINT('Ctrl Pts',(6.12559579001011,5.0073351835864,-34.416600475273));
#65674=CARTESIAN_POINT('Ctrl Pts',(5.89031539433097,5.28702869742106,-34.4026481045688));
#65675=CARTESIAN_POINT('Ctrl Pts',(5.71746297837752,5.47349221975548,-34.393349472242));
#65676=CARTESIAN_POINT('Ctrl Pts',(5.21931476104331,5.96146863092521,-34.3685918498023));
#65677=CARTESIAN_POINT('Ctrl Pts',(4.8771937497999,6.24446457849056,-34.3537799423491));
#65678=CARTESIAN_POINT('Ctrl Pts',(4.2517640016512,6.67890251538361,-34.3277169275132));
#65679=CARTESIAN_POINT('Ctrl Pts',(3.9796377923198,6.84453749619405,-34.3166434870554));
#65680=CARTESIAN_POINT('Ctrl Pts',(3.66920515596642,7.008704407714,-34.3034978306381));
#65681=CARTESIAN_POINT('Ctrl Pts',(3.64001889965825,7.02390677009814,-34.3022569942088));
#65682=CARTESIAN_POINT('Ctrl Pts',(3.52018126211033,7.08537955737316,-34.2971386388032));
#65683=CARTESIAN_POINT('Ctrl Pts',(3.42873911143441,7.13007896443768,-34.293178290537));
#65684=CARTESIAN_POINT('Ctrl Pts',(3.32550939752141,7.17809544456404,-34.2886180010974));
#65685=CARTESIAN_POINT('Ctrl Pts',(3.31454345721508,7.18316564143365,-34.2881324432548));
#65686=CARTESIAN_POINT('Ctrl Pts',(3.29852262923274,7.19052851117672,-34.2874214040077));
#65687=CARTESIAN_POINT('Ctrl Pts',(3.29347702608026,7.19284094666214,-34.2871972318837));
#65688=CARTESIAN_POINT('Ctrl Pts',(3.28453421728705,7.19692811645605,-34.2867994953801));
#65689=CARTESIAN_POINT('Ctrl Pts',(3.28063799115679,7.19870500220724,-34.2866260692451));
#65690=CARTESIAN_POINT('Ctrl Pts',(3.27254782269935,7.20238661593111,-34.2862656792296));
#65691=CARTESIAN_POINT('Ctrl Pts',(3.26835365679055,7.20429084582015,-34.2860786837615));
#65692=CARTESIAN_POINT('Ctrl Pts',(3.25754784847799,7.20918550680156,-34.2855965047311));
#65693=CARTESIAN_POINT('Ctrl Pts',(3.2509337628638,7.21217050030017,-34.2853009787966));
#65694=CARTESIAN_POINT('Ctrl Pts',(3.22346149783864,7.22452349957682,-34.28407188963));
#65695=CARTESIAN_POINT('Ctrl Pts',(3.20256704343217,7.23381007047417,-34.2831332797168));
#65696=CARTESIAN_POINT('Ctrl Pts',(3.10705129585717,7.27576724201358,-34.2788262157856));
#65697=CARTESIAN_POINT('Ctrl Pts',(3.03197055622898,7.30737370099201,-34.2753952287199));
#65698=CARTESIAN_POINT('Ctrl Pts',(2.79829834041538,7.40152062994559,-34.2646073244767));
#65699=CARTESIAN_POINT('Ctrl Pts',(2.63816879594159,7.46009656462854,-34.257060766031));
#65700=CARTESIAN_POINT('Ctrl Pts',(2.16998481309971,7.61440050673667,-34.2347985550791));
#65701=CARTESIAN_POINT('Ctrl Pts',(1.85781035825427,7.69652251551661,-34.2197228795837));
#65702=CARTESIAN_POINT('Ctrl Pts',(0.841785984186737,7.89837001423378,-34.1714190552531));
#65703=CARTESIAN_POINT('Ctrl Pts',(0.126352228757221,7.94211774774373,-34.1389048366125));
#65704=CARTESIAN_POINT('Ctrl Pts',(-0.633270771559198,7.88575932885764,
-34.1077214463337));
#65705=CARTESIAN_POINT('Ctrl Pts',(-0.681179630311586,7.88176544186874,
-34.1057670684238));
#65706=CARTESIAN_POINT('Ctrl Pts',(-0.743645628450338,7.87598419538801,
-34.1032345218652));
#65707=CARTESIAN_POINT('Ctrl Pts',(-0.758237850520886,7.87459276608903,
-34.1026440288978));
#65708=CARTESIAN_POINT('Ctrl Pts',(-0.781569086497848,7.87230258171593,
-34.1017016683943));
#65709=CARTESIAN_POINT('Ctrl Pts',(-0.79031058328466,7.87142981659932,-34.1013489920002));
#65710=CARTESIAN_POINT('Ctrl Pts',(-0.806064725748986,7.8698303896959,-34.1007141010258));
#65711=CARTESIAN_POINT('Ctrl Pts',(-0.813077881343419,7.86910891167922,
-34.1004317254306));
#65712=CARTESIAN_POINT('Ctrl Pts',(-0.829536348111731,7.86739351046913,
-34.0997696399199));
#65713=CARTESIAN_POINT('Ctrl Pts',(-0.838980861862348,7.86639195029397,
-34.0993901680515));
#65714=CARTESIAN_POINT('Ctrl Pts',(-0.866226760906352,7.8634529845493,-34.0982967664704));
#65715=CARTESIAN_POINT('Ctrl Pts',(-0.884023453044639,7.86147213830416,
-34.0975841884575));
#65716=CARTESIAN_POINT('Ctrl Pts',(-1.00386127618572,7.84772160733433,-34.0927966269589));
#65717=CARTESIAN_POINT('Ctrl Pts',(-1.1056735946487,7.83402570540929,-34.0887818242651));
#65718=CARTESIAN_POINT('Ctrl Pts',(-1.38576151356889,7.79077871807958,-34.0778655749685));
#65719=CARTESIAN_POINT('Ctrl Pts',(-1.56333844745471,7.75709644901095,-34.0710903483388));
#65720=CARTESIAN_POINT('Ctrl Pts',(-1.9133987348326,7.67818745085649,-34.0579264306725));
#65721=CARTESIAN_POINT('Ctrl Pts',(-2.08581565796202,7.63315355667764,-34.0515373613274));
#65722=CARTESIAN_POINT('Ctrl Pts',(-2.30940231155686,7.56661222368156,-34.0432900876323));
#65723=CARTESIAN_POINT('Ctrl Pts',(-2.36206998616337,7.55033674883141,-34.0413500465401));
#65724=CARTESIAN_POINT('Ctrl Pts',(-2.77134181080822,7.41916116884508,-34.0262772393355));
#65725=CARTESIAN_POINT('Ctrl Pts',(-3.119539543831,7.27961221287191,-34.0134931406521));
#65726=CARTESIAN_POINT('Ctrl Pts',(-3.77475243938495,6.96134483563091,-33.9877902085086));
#65727=CARTESIAN_POINT('Ctrl Pts',(-4.08224722029417,6.78559840237176,-33.9748998792063));
#65728=CARTESIAN_POINT('Ctrl Pts',(-4.40755640575439,6.5695294518865,-33.9594533526562));
#65729=CARTESIAN_POINT('Ctrl Pts',(-4.43801695643573,6.54899046638664,-33.9579904810914));
#65730=CARTESIAN_POINT('Ctrl Pts',(-4.47875111654204,6.52110947776384,-33.9560128820582));
#65731=CARTESIAN_POINT('Ctrl Pts',(-4.48915209373867,6.5139537810832,-33.9555060415567));
#65732=CARTESIAN_POINT('Ctrl Pts',(-4.50542879572151,6.50269818609319,-33.9547099627527));
#65733=CARTESIAN_POINT('Ctrl Pts',(-4.51131617923028,6.49861513427263,-33.9544214164643));
#65734=CARTESIAN_POINT('Ctrl Pts',(-4.52259967333522,6.49076701850407,-33.9538672601218));
#65735=CARTESIAN_POINT('Ctrl Pts',(-4.52799665074761,6.48700320828363,-33.9536017007683));
#65736=CARTESIAN_POINT('Ctrl Pts',(-4.54065392646536,6.4781526307505,-33.9529777261907));
#65737=CARTESIAN_POINT('Ctrl Pts',(-4.5479103759164,6.47306038896221,-33.9526190937365));
#65738=CARTESIAN_POINT('Ctrl Pts',(-4.56289789360019,6.46250519735602,-33.951876515904));
#65739=CARTESIAN_POINT('Ctrl Pts',(-4.57062774541276,6.4570405469782,-33.9514925047066));
#65740=CARTESIAN_POINT('Ctrl Pts',(-4.60793025930997,6.43056883681158,-33.9496344524702));
#65741=CARTESIAN_POINT('Ctrl Pts',(-4.63736778742327,6.40937257463789,-33.9481532470131));
#65742=CARTESIAN_POINT('Ctrl Pts',(-4.78777251946277,6.29949620433307,-33.9405116945555));
#65743=CARTESIAN_POINT('Ctrl Pts',(-4.90634320912309,6.20759310774439,-33.9342417078726));
#65744=CARTESIAN_POINT('Ctrl Pts',(-5.31970208808019,5.86795737886039,-33.9116316095972));
#65745=CARTESIAN_POINT('Ctrl Pts',(-5.59893574946353,5.60214870551604,-33.8949676080558));
#65746=CARTESIAN_POINT('Ctrl Pts',(-5.97609805917676,5.1866369664785,-33.8708841312394));
#65747=CARTESIAN_POINT('Ctrl Pts',(-6.09010428659148,5.05228483686145,-33.8633542715402));
#65748=CARTESIAN_POINT('Ctrl Pts',(-6.58127375678991,4.43265251240791,-33.8297807581608));
#65749=CARTESIAN_POINT('Ctrl Pts',(-6.9056123193095,3.90821284940221,-33.8044384159982));
#65750=CARTESIAN_POINT('Ctrl Pts',(-7.19813126015926,3.28277149173211,-33.7763617770897));
#65751=CARTESIAN_POINT('Ctrl Pts',(-7.22929696790898,3.2135568746672,-33.7732854786019));
#65752=CARTESIAN_POINT('Ctrl Pts',(-7.27088453514792,3.11752870281932,-33.7690596351629));
#65753=CARTESIAN_POINT('Ctrl Pts',(-7.28216330227458,3.09109119615708,-33.7679005749624));
#65754=CARTESIAN_POINT('Ctrl Pts',(-7.30129562816427,3.04555896363137,-33.7659118063905));
#65755=CARTESIAN_POINT('Ctrl Pts',(-7.30921896385016,3.02649391081043,-33.7650813047093));
#65756=CARTESIAN_POINT('Ctrl Pts',(-7.32541116249065,2.98709792438398,-33.7633697208899));
#65757=CARTESIAN_POINT('Ctrl Pts',(-7.3336702352314,2.96676315094066,-33.7624887592621));
#65758=CARTESIAN_POINT('Ctrl Pts',(-7.3498307880992,2.92649417867642,-33.7607490815807));
#65759=CARTESIAN_POINT('Ctrl Pts',(-7.35773605629634,2.90656170082227,-33.7598903274552));
#65760=CARTESIAN_POINT('Ctrl Pts',(-7.37584723585191,2.86034847127394,-33.7579047188519));
#65761=CARTESIAN_POINT('Ctrl Pts',(-7.38599390619506,2.83404478597447,-33.756778577526));
#65762=CARTESIAN_POINT('Ctrl Pts',(-7.41190360055456,2.76579356387896,-33.7538668056964));
#65763=CARTESIAN_POINT('Ctrl Pts',(-7.42745124224312,2.72376524248096,-33.7520837746251));
#65764=CARTESIAN_POINT('Ctrl Pts',(-7.59669977809516,2.25402596861566,-33.7322634098724));
#65765=CARTESIAN_POINT('Ctrl Pts',(-7.71362711179566,1.81396055494999,-33.7147474440197));
#65766=CARTESIAN_POINT('Ctrl Pts',(-7.82181301429372,1.19696049024682,-33.6906766901119));
#65767=CARTESIAN_POINT('Ctrl Pts',(-7.84597545822106,1.02671407996487,-33.6840775606361));
#65768=CARTESIAN_POINT('Ctrl Pts',(-7.87486832308192,0.761201646125015,
-33.6737573560437));
#65769=CARTESIAN_POINT('Ctrl Pts',(-7.88345596015881,0.666408967094082,
-33.6700670649077));
#65770=CARTESIAN_POINT('Ctrl Pts',(-7.90097122667123,0.424580745398112,
-33.6606078799385));
#65771=CARTESIAN_POINT('Ctrl Pts',(-7.90750635809786,0.277410544480438,
-33.6548094366254));
#65772=CARTESIAN_POINT('Ctrl Pts',(-7.91031987236066,0.106413949164605,
-33.6479680406686));
#65773=CARTESIAN_POINT('Ctrl Pts',(-7.91060355106177,0.0826792966977804,
-33.6470160946721));
#65774=CARTESIAN_POINT('Ctrl Pts',(-7.91087363748045,0.0464312653507314,
-33.6455583962039));
#65775=CARTESIAN_POINT('Ctrl Pts',(-7.91093718192898,0.0339186198397731,
-33.64505451301));
#65776=CARTESIAN_POINT('Ctrl Pts',(-7.91098859675916,0.0149172626381395,
-33.6442883065941));
#65777=CARTESIAN_POINT('Ctrl Pts',(-7.91099817097294,0.0084286091475209,
-33.6440264783865));
#65778=CARTESIAN_POINT('Ctrl Pts',(-7.91099994589624,0.00119061020498363,
-33.6437342135727));
#65779=CARTESIAN_POINT('Ctrl Pts',(-7.91100002318357,0.000441261981302332,
-33.6437039530873));
#65780=CARTESIAN_POINT('Ctrl Pts',(-7.91099999400094,-0.000308086119090196,
-33.6436736902287));
#65781=CARTESIAN_POINT('',(-7.91099998316719,0.000516070481359765,-29.6338967485033));
#65782=CARTESIAN_POINT('Ctrl Pts',(-7.91099999400114,-0.000308081041544692,
-33.6436736904337));
#65783=CARTESIAN_POINT('Ctrl Pts',(-7.91099975116352,-0.00654374027287683,
-33.6434218597107));
#65784=CARTESIAN_POINT('Ctrl Pts',(-7.91099213565916,-0.012779390569126,
-33.6431698646668));
#65785=CARTESIAN_POINT('Ctrl Pts',(-7.91094622120392,-0.0318815649900821,
-33.6423974103053));
#65786=CARTESIAN_POINT('Ctrl Pts',(-7.91088390541829,-0.0447479894069168,
-33.6418764260389));
#65787=CARTESIAN_POINT('Ctrl Pts',(-7.91060669521863,-0.0828106997961559,
-33.640333213343));
#65788=CARTESIAN_POINT('Ctrl Pts',(-7.91030281151989,-0.108006104068315,
-33.6393091173118));
#65789=CARTESIAN_POINT('Ctrl Pts',(-7.90759339903516,-0.268900999890681,
-33.6327538553811));
#65790=CARTESIAN_POINT('Ctrl Pts',(-7.90181651311258,-0.404519133671654,
-33.6271582775097));
#65791=CARTESIAN_POINT('Ctrl Pts',(-7.88637549202989,-0.630236467805673,
-33.6177630874385));
#65792=CARTESIAN_POINT('Ctrl Pts',(-7.87864718876571,-0.720440611788852,
-33.6139864299638));
#65793=CARTESIAN_POINT('Ctrl Pts',(-7.84943820910063,-1.00404175163524,
-33.602059726394));
#65794=CARTESIAN_POINT('Ctrl Pts',(-7.8223700537451,-1.19679003749189,-33.5938773133038));
#65795=CARTESIAN_POINT('Ctrl Pts',(-7.70641831644982,-1.84724733058121,
-33.5661346377338));
#65796=CARTESIAN_POINT('Ctrl Pts',(-7.58421084998201,-2.29803817935784,
-33.5467353136327));
#65797=CARTESIAN_POINT('Ctrl Pts',(-7.4066564329207,-2.77985630186073,-33.5258627700985));
#65798=CARTESIAN_POINT('Ctrl Pts',(-7.38989459555859,-2.82411375031992,
-33.5239436005063));
#65799=CARTESIAN_POINT('Ctrl Pts',(-7.36143836923563,-2.89726029611382,
-33.5207679244007));
#65800=CARTESIAN_POINT('Ctrl Pts',(-7.34996862211976,-2.92623535466211,
-33.5195089751718));
#65801=CARTESIAN_POINT('Ctrl Pts',(-7.32901452298634,-2.97826942052895,
-33.5172461328413));
#65802=CARTESIAN_POINT('Ctrl Pts',(-7.31959180344659,-3.00135277085317,
-33.5162415802156));
#65803=CARTESIAN_POINT('Ctrl Pts',(-7.30016355598999,-3.04831152900338,
-33.5141964220223));
#65804=CARTESIAN_POINT('Ctrl Pts',(-7.29014964339136,-3.07218314953111,
-33.5131559206929));
#65805=CARTESIAN_POINT('Ctrl Pts',(-7.26822744566847,-3.12373151517014,
-33.5109070720977));
#65806=CARTESIAN_POINT('Ctrl Pts',(-7.25627784508661,-3.15139026839842,
-33.5096991830757));
#65807=CARTESIAN_POINT('Ctrl Pts',(-7.22337076328335,-3.22637800053255,
-33.5064206157943));
#65808=CARTESIAN_POINT('Ctrl Pts',(-7.20210627459281,-3.27357074674933,
-33.5043531868903));
#65809=CARTESIAN_POINT('Ctrl Pts',(-7.0934302443917,-3.50857242883045,-33.4940338036087));
#65810=CARTESIAN_POINT('Ctrl Pts',(-6.99912780718079,-3.69310769745149,
-33.4858478040287));
#65811=CARTESIAN_POINT('Ctrl Pts',(-6.69806615845088,-4.22918808858231,
-33.4616902344549));
#65812=CARTESIAN_POINT('Ctrl Pts',(-6.47125863300228,-4.56869292762793,
-33.4459926729266));
#65813=CARTESIAN_POINT('Ctrl Pts',(-6.11656342129852,-5.01988039722635,
-33.4243657770923));
#65814=CARTESIAN_POINT('Ctrl Pts',(-6.00974699848067,-5.14727978717806,
-33.4181558888902));
#65815=CARTESIAN_POINT('Ctrl Pts',(-5.64252241837052,-5.55823890907365,
-33.3976443985068));
#65816=CARTESIAN_POINT('Ctrl Pts',(-5.36545142205661,-5.82614743134477,
-33.3835042222331));
#65817=CARTESIAN_POINT('Ctrl Pts',(-4.95439511978196,-6.16932463678031,
-33.3631157373137));
#65818=CARTESIAN_POINT('Ctrl Pts',(-4.83606915140695,-6.26250988370454,
-33.3573027937192));
#65819=CARTESIAN_POINT('Ctrl Pts',(-4.68239720516316,-6.37657762611485,
-33.3497399113811));
#65820=CARTESIAN_POINT('Ctrl Pts',(-4.64944723928385,-6.40064263247512,
-33.3481174870228));
#65821=CARTESIAN_POINT('Ctrl Pts',(-4.60888887047265,-6.42978599599392,
-33.346117736105));
#65822=CARTESIAN_POINT('Ctrl Pts',(-4.60145557970969,-6.43510770086762,
-33.3457511238254));
#65823=CARTESIAN_POINT('Ctrl Pts',(-4.58714950908,-6.4453123632409,-33.3450453017315));
#65824=CARTESIAN_POINT('Ctrl Pts',(-4.58027811266058,-6.45019724414681,
-33.3447061789804));
#65825=CARTESIAN_POINT('Ctrl Pts',(-4.56850809678264,-6.45853626584105,
-33.3441250911654));
#65826=CARTESIAN_POINT('Ctrl Pts',(-4.56361332744736,-6.46199584686292,
-33.3438833751956));
#65827=CARTESIAN_POINT('Ctrl Pts',(-4.55357960874533,-6.46907050699592,
-33.343387752268));
#65828=CARTESIAN_POINT('Ctrl Pts',(-4.54844027635345,-6.47268503248875,
-33.3431338199898));
#65829=CARTESIAN_POINT('Ctrl Pts',(-4.53472404981306,-6.48230733988631,
-33.3424559032936));
#65830=CARTESIAN_POINT('Ctrl Pts',(-4.52613954119064,-6.48830420903565,
-33.3420314068993));
#65831=CARTESIAN_POINT('Ctrl Pts',(-4.49534808729745,-6.5097233096708,-33.3405079509229));
#65832=CARTESIAN_POINT('Ctrl Pts',(-4.47307418059586,-6.52504860857923,
-33.3394043427976));
#65833=CARTESIAN_POINT('Ctrl Pts',(-4.13933728495706,-6.7521604389403,-33.3228389091674));
#65834=CARTESIAN_POINT('Ctrl Pts',(-3.81327791381509,-6.94151182641307,
-33.3061051961278));
#65835=CARTESIAN_POINT('Ctrl Pts',(-3.22345567403898,-7.22991599444711,
-33.2761890818522));
#65836=CARTESIAN_POINT('Ctrl Pts',(-2.96551324051819,-7.33948783377742,
-33.2632259919968));
#65837=CARTESIAN_POINT('Ctrl Pts',(-2.60312049815171,-7.47119949869815,
-33.2455187866376));
#65838=CARTESIAN_POINT('Ctrl Pts',(-2.50322273719411,-7.50526046411354,
-33.2406877605261));
#65839=CARTESIAN_POINT('Ctrl Pts',(-2.26771995944067,-7.58033178706349,
-33.2294387985025));
#65840=CARTESIAN_POINT('Ctrl Pts',(-2.13163373923896,-7.61971935969843,
-33.2230457069636));
#65841=CARTESIAN_POINT('Ctrl Pts',(-1.72251794331189,-7.72631114015468,
-33.2041967822373));
#65842=CARTESIAN_POINT('Ctrl Pts',(-1.44687696458316,-7.78264209645099,
-33.1919903336011));
#65843=CARTESIAN_POINT('Ctrl Pts',(-1.04657423384607,-7.84244075222704,
-33.1750408360357));
#65844=CARTESIAN_POINT('Ctrl Pts',(-0.92392997689602,-7.8578336525633,-33.1699497776056));
#65845=CARTESIAN_POINT('Ctrl Pts',(-0.781739138214376,-7.87230453199216,
-33.1641616305432));
#65846=CARTESIAN_POINT('Ctrl Pts',(-0.762499328266004,-7.87419135566427,
-33.1633808409355));
#65847=CARTESIAN_POINT('Ctrl Pts',(-0.733275815145492,-7.87694915584677,
-33.1621985097021));
#65848=CARTESIAN_POINT('Ctrl Pts',(-0.72329711811362,-7.87787171161783,
-33.1617954292195));
#65849=CARTESIAN_POINT('Ctrl Pts',(-0.706003986697468,-7.87943737106048,
-33.1610979917474));
#65850=CARTESIAN_POINT('Ctrl Pts',(-0.698690371053566,-7.88008925580459,
-33.1608033729948));
#65851=CARTESIAN_POINT('Ctrl Pts',(-0.683504845477504,-7.88142148065165,
-33.1601923519832));
#65852=CARTESIAN_POINT('Ctrl Pts',(-0.675632800335419,-7.88210021181129,
-33.1598759980345));
#65853=CARTESIAN_POINT('Ctrl Pts',(-0.656474966494718,-7.8837230975129,
-33.1591070566646));
#65854=CARTESIAN_POINT('Ctrl Pts',(-0.645188127303895,-7.88465481435837,
-33.1586548407356));
#65855=CARTESIAN_POINT('Ctrl Pts',(-0.602655710461948,-7.88807388178188,
-33.156953762904));
#65856=CARTESIAN_POINT('Ctrl Pts',(-0.571397260350143,-7.89039977872344,
-33.1557097183328));
#65857=CARTESIAN_POINT('Ctrl Pts',(-0.0348851117538426,-7.92711596220801,
-33.1344603052237));
#65858=CARTESIAN_POINT('Ctrl Pts',(0.472522377447815,-7.91310167155002,
-33.1160293912721));
#65859=CARTESIAN_POINT('Ctrl Pts',(1.2543879991653,-7.81598410215948,-33.0884101257007));
#65860=CARTESIAN_POINT('Ctrl Pts',(1.5315762728853,-7.76642594525951,-33.0787525461689));
#65861=CARTESIAN_POINT('Ctrl Pts',(2.11624890266608,-7.62936831474116,-33.0579415421913));
#65862=CARTESIAN_POINT('Ctrl Pts',(2.42225881325035,-7.53779902730156,-33.0467791582183));
#65863=CARTESIAN_POINT('Ctrl Pts',(2.8428723242534,-7.38367125612125,-33.0302010632184));
#65864=CARTESIAN_POINT('Ctrl Pts',(2.96275347547337,-7.33638969189162,-33.0253285447979));
#65865=CARTESIAN_POINT('Ctrl Pts',(3.14015679321238,-7.26136372225862,-33.0178320876334));
#65866=CARTESIAN_POINT('Ctrl Pts',(3.19858482446452,-7.23581666043191,-33.0153148580121));
#65867=CARTESIAN_POINT('Ctrl Pts',(3.26715385952687,-7.20484269249831,-33.0123013358167));
#65868=CARTESIAN_POINT('Ctrl Pts',(3.27759672206606,-7.20009807509195,-33.0118407943475));
#65869=CARTESIAN_POINT('Ctrl Pts',(3.29303702766819,-7.19304236395944,-33.0111575439482));
#65870=CARTESIAN_POINT('Ctrl Pts',(3.29804246726797,-7.19074872312905,-33.0109356867872));
#65871=CARTESIAN_POINT('Ctrl Pts',(3.30816227481626,-7.18609873802644,-33.0104864199762));
#65872=CARTESIAN_POINT('Ctrl Pts',(3.31327652928834,-7.1837421549929,-33.0102589988858));
#65873=CARTESIAN_POINT('Ctrl Pts',(3.32317344899002,-7.17916896410884,-33.0098181820529));
#65874=CARTESIAN_POINT('Ctrl Pts',(3.32795642441959,-7.17695303205271,-33.0096048184951));
#65875=CARTESIAN_POINT('Ctrl Pts',(3.33932479184172,-7.17167230811722,-33.0090969182399));
#65876=CARTESIAN_POINT('Ctrl Pts',(3.34590817657788,-7.16860322753352,-33.0088021803645));
#65877=CARTESIAN_POINT('Ctrl Pts',(3.36919929717044,-7.15770616344069,-33.0077572852488));
#65878=CARTESIAN_POINT('Ctrl Pts',(3.38588378471459,-7.14982883814051,-33.0070048536794));
#65879=CARTESIAN_POINT('Ctrl Pts',(3.65917911901093,-7.01962548740865,-32.9946171728656));
#65880=CARTESIAN_POINT('Ctrl Pts',(3.90902888102771,-6.88361897579363,-32.9823923633244));
#65881=CARTESIAN_POINT('Ctrl Pts',(4.51993206419288,-6.50706969771793,-32.9510556570855));
#65882=CARTESIAN_POINT('Ctrl Pts',(4.86956790317307,-6.24972560429389,-32.9317859898353));
#65883=CARTESIAN_POINT('Ctrl Pts',(5.47059121383305,-5.72615240501683,-32.8973174829665));
#65884=CARTESIAN_POINT('Ctrl Pts',(5.72803002127639,-5.46862779329378,-32.8819914389672));
#65885=CARTESIAN_POINT('Ctrl Pts',(6.01100357535518,-5.14356678559633,-32.8644090147828));
#65886=CARTESIAN_POINT('Ctrl Pts',(6.05450967967861,-5.0922839641663,-32.8616817998936));
#65887=CARTESIAN_POINT('Ctrl Pts',(6.11120313294994,-5.02370277025904,-32.8580935744274));
#65888=CARTESIAN_POINT('Ctrl Pts',(6.12498018024438,-5.0068963493628,-32.8572188452947));
#65889=CARTESIAN_POINT('Ctrl Pts',(6.14816722751216,-4.97837188150031,-32.8557418632176));
#65890=CARTESIAN_POINT('Ctrl Pts',(6.1576133824918,-4.96668342876062,-32.855138793822));
#65891=CARTESIAN_POINT('Ctrl Pts',(6.17575703400108,-4.94410157320073,-32.8539777716219));
#65892=CARTESIAN_POINT('Ctrl Pts',(6.18445915477627,-4.93321196315864,-32.8534197177471));
#65893=CARTESIAN_POINT('Ctrl Pts',(6.204370724138,-4.90815964982803,-32.8521400101731));
#65894=CARTESIAN_POINT('Ctrl Pts',(6.21556055231134,-4.89398143174669,-32.8514187841809));
#65895=CARTESIAN_POINT('Ctrl Pts',(6.25071236576182,-4.84912684158986,-32.8491464516005));
#65896=CARTESIAN_POINT('Ctrl Pts',(6.27449667331526,-4.81831170944602,-32.8475990536365));
#65897=CARTESIAN_POINT('Ctrl Pts',(6.45048905139206,-4.58678159439591,-32.8360721331522));
#65898=CARTESIAN_POINT('Ctrl Pts',(6.59326381190027,-4.3790700091061,-32.8262936934251));
#65899=CARTESIAN_POINT('Ctrl Pts',(7.02530206741455,-3.68137124254638,-32.7950208390114));
#65900=CARTESIAN_POINT('Ctrl Pts',(7.27169732556693,-3.16698266687693,-32.774464149447));
#65901=CARTESIAN_POINT('Ctrl Pts',(7.54446197269405,-2.39338586603758,-32.7440686361809));
#65902=CARTESIAN_POINT('Ctrl Pts',(7.61674565110016,-2.15229622553774,-32.7346402846619));
#65903=CARTESIAN_POINT('Ctrl Pts',(7.7016896927013,-1.81053084840643,-32.7209641919364));
#65904=CARTESIAN_POINT('Ctrl Pts',(7.72409479258239,-1.71242656060331,-32.7170028856897));
#65905=CARTESIAN_POINT('Ctrl Pts',(7.74767715787882,-1.59926355688924,-32.7123714068681));
#65906=CARTESIAN_POINT('Ctrl Pts',(7.75069067405599,-1.58459437662371,-32.7117698396851));
#65907=CARTESIAN_POINT('Ctrl Pts',(7.75493763748704,-1.5636190476616,-32.7109078686173));
#65908=CARTESIAN_POINT('Ctrl Pts',(7.75620509241316,-1.55731976537862,-32.7106487714502));
#65909=CARTESIAN_POINT('Ctrl Pts',(7.75873682595479,-1.54465722897979,-32.7101274713721));
#65910=CARTESIAN_POINT('Ctrl Pts',(7.76000095447597,-1.53829394970195,-32.7098652628382));
#65911=CARTESIAN_POINT('Ctrl Pts',(7.76241052815726,-1.52608625628955,-32.7093617551096));
#65912=CARTESIAN_POINT('Ctrl Pts',(7.76355720446431,-1.52024208666437,-32.7091205046364));
#65913=CARTESIAN_POINT('Ctrl Pts',(7.76623389114372,-1.50651803231158,-32.7085534729951));
#65914=CARTESIAN_POINT('Ctrl Pts',(7.76775850793353,-1.4986371126418,-32.708227476838));
#65915=CARTESIAN_POINT('Ctrl Pts',(7.77219662212758,-1.47550726382906,-32.7072695525705));
#65916=CARTESIAN_POINT('Ctrl Pts',(7.77507721932865,-1.46025211775057,-32.7066362908509));
#65917=CARTESIAN_POINT('Ctrl Pts',(7.80109650128312,-1.32019862599851,-32.7008083616989));
#65918=CARTESIAN_POINT('Ctrl Pts',(7.82127073023713,-1.1948860339039,-32.6954821733052));
#65919=CARTESIAN_POINT('Ctrl Pts',(7.85493456737977,-0.948077779458153,
-32.6847651062696));
#65920=CARTESIAN_POINT('Ctrl Pts',(7.86863920814285,-0.826658045808646,
-32.679395370693));
#65921=CARTESIAN_POINT('Ctrl Pts',(7.93283774152335,-0.109108229877746,
-32.6472747806219));
#65922=CARTESIAN_POINT('Ctrl Pts',(7.91839076644309,0.490888276221883,-32.6190150259049));
#65923=CARTESIAN_POINT('Ctrl Pts',(7.78256157320981,1.47323180602296,-32.5746772523025));
#65924=CARTESIAN_POINT('Ctrl Pts',(7.69968531600709,1.85838127856973,-32.5577631630825));
#65925=CARTESIAN_POINT('Ctrl Pts',(7.58151361412394,2.25946469655219,-32.5408113548146));
#65926=CARTESIAN_POINT('Ctrl Pts',(7.57443194662476,2.28309222259275,-32.5398150713345));
#65927=CARTESIAN_POINT('Ctrl Pts',(7.56416393225476,2.31677713438323,-32.5383980022589));
#65928=CARTESIAN_POINT('Ctrl Pts',(7.56106782853289,2.32686174447559,-32.5379741820458));
#65929=CARTESIAN_POINT('Ctrl Pts',(7.55568716098863,2.34426348430817,-32.5372435747448));
#65930=CARTESIAN_POINT('Ctrl Pts',(7.55341212064429,2.35158352918303,-32.5369364667325));
#65931=CARTESIAN_POINT('Ctrl Pts',(7.54903676536361,2.3655895731733,-32.53634927484));
#65932=CARTESIAN_POINT('Ctrl Pts',(7.54693819921652,2.37227610767411,-32.5360691322126));
#65933=CARTESIAN_POINT('Ctrl Pts',(7.54200334777107,2.38792690515176,-32.5354138488803));
#65934=CARTESIAN_POINT('Ctrl Pts',(7.539159957983,2.39688892753199,-32.5350389492426));
#65935=CARTESIAN_POINT('Ctrl Pts',(7.52927388934537,2.42785698975545,-32.5337446302023));
#65936=CARTESIAN_POINT('Ctrl Pts',(7.52215075158326,2.4498373305024,-32.5328279448631));
#65937=CARTESIAN_POINT('Ctrl Pts',(7.44531820945634,2.68343005160304,-32.5231067942964));
#65938=CARTESIAN_POINT('Ctrl Pts',(7.36679274350922,2.89204677443386,-32.5146110853235));
#65939=CARTESIAN_POINT('Ctrl Pts',(7.13872410506814,3.42811249674343,-32.4931078208729));
#65940=CARTESIAN_POINT('Ctrl Pts',(6.97546676642291,3.74916302766533,-32.480577571531));
#65941=CARTESIAN_POINT('Ctrl Pts',(6.58503702180654,4.40253312551474,-32.454700110483));
#65942=CARTESIAN_POINT('Ctrl Pts',(6.35324246340856,4.73088854210571,-32.441464045706));
#65943=CARTESIAN_POINT('Ctrl Pts',(5.92275830655111,5.25167726547717,-32.418104336083));
#65944=CARTESIAN_POINT('Ctrl Pts',(5.73710624632675,5.45387675820919,-32.4083269804624));
#65945=CARTESIAN_POINT('Ctrl Pts',(5.47491071862247,5.71121160557892,-32.3942918116502));
#65946=CARTESIAN_POINT('Ctrl Pts',(5.40733532785586,5.7752323545567,-32.3906557489583));
#65947=CARTESIAN_POINT('Ctrl Pts',(5.33084553661318,5.8451790965201,-32.386499268072));
#65948=CARTESIAN_POINT('Ctrl Pts',(5.32302816480776,5.85229903201796,-32.3860740047682));
#65949=CARTESIAN_POINT('Ctrl Pts',(5.31136523167655,5.86287874120508,-32.3854388134704));
#65950=CARTESIAN_POINT('Ctrl Pts',(5.30753048579824,5.86635047541383,-32.3852298468624));
#65951=CARTESIAN_POINT('Ctrl Pts',(5.30096940571265,5.8722787593301,-32.3848721088648));
#65952=CARTESIAN_POINT('Ctrl Pts',(5.29824475679287,5.87473718260022,-32.384723488992));
#65953=CARTESIAN_POINT('Ctrl Pts',(5.29266672137329,5.87976315089379,-32.3844191012588));
#65954=CARTESIAN_POINT('Ctrl Pts',(5.28981317538925,5.88233051634398,-32.3842633189152));
#65955=CARTESIAN_POINT('Ctrl Pts',(5.28297311986841,5.88847558431058,-32.3838897388713));
#65956=CARTESIAN_POINT('Ctrl Pts',(5.27898486140652,5.89205130024744,-32.3836717801424));
#65957=CARTESIAN_POINT('Ctrl Pts',(5.2644324553446,5.90507178012516,-32.3828760122147));
#65958=CARTESIAN_POINT('Ctrl Pts',(5.25384662044065,5.91449215816656,-32.3822962329614));
#65959=CARTESIAN_POINT('Ctrl Pts',(5.07941270129891,6.06888379338286,-32.3727285656124));
#65960=CARTESIAN_POINT('Ctrl Pts',(4.90965746375843,6.20701477127757,-32.363216270089));
#65961=CARTESIAN_POINT('Ctrl Pts',(4.37918376024788,6.60327728527229,-32.3335285653968));
#65962=CARTESIAN_POINT('Ctrl Pts',(4.00228358519768,6.83829200804005,-32.3125315517497));
#65963=CARTESIAN_POINT('Ctrl Pts',(3.30320535949796,7.19651358568546,-32.2760486399687));
#65964=CARTESIAN_POINT('Ctrl Pts',(2.98890427546332,7.33262958075132,-32.2604263714526));
#65965=CARTESIAN_POINT('Ctrl Pts',(2.40679434784978,7.54105467722124,-32.23337234627));
#65966=CARTESIAN_POINT('Ctrl Pts',(2.14212368382098,7.62046538319659,-32.2217270911215));
#65967=CARTESIAN_POINT('Ctrl Pts',(1.85394742782154,7.69072287483236,-32.2097445658143));
#65968=CARTESIAN_POINT('Ctrl Pts',(1.83405579931766,7.69549080542412,-32.2089209132692));
#65969=CARTESIAN_POINT('Ctrl Pts',(1.804868910847,7.70236717199143,-32.2077173889253));
#65970=CARTESIAN_POINT('Ctrl Pts',(1.79558806080767,7.70453602459496,-32.2073354343768));
#65971=CARTESIAN_POINT('Ctrl Pts',(1.77923898479974,7.70832551339784,-32.2066638873008));
#65972=CARTESIAN_POINT('Ctrl Pts',(1.77217241767054,7.70995321049081,-32.2063740518554));
#65973=CARTESIAN_POINT('Ctrl Pts',(1.75840745610898,7.71310387625409,-32.2058103112632));
#65974=CARTESIAN_POINT('Ctrl Pts',(1.75170929862791,7.71462784073159,-32.2055363720951));
#65975=CARTESIAN_POINT('Ctrl Pts',(1.73565106202119,7.71825941800575,-32.2048805401445));
#65976=CARTESIAN_POINT('Ctrl Pts',(1.72628910549807,7.72035873375667,-32.2044989327082));
#65977=CARTESIAN_POINT('Ctrl Pts',(1.69244201488533,7.72788392681384,-32.2031219449185));
#65978=CARTESIAN_POINT('Ctrl Pts',(1.66793480644154,7.73321042370125,-32.2021299754383));
#65979=CARTESIAN_POINT('Ctrl Pts',(1.27838780762894,7.81593822799994,-32.1864413953011));
#65980=CARTESIAN_POINT('Ctrl Pts',(0.908332360471245,7.86753688897652,-32.1726726555434));
#65981=CARTESIAN_POINT('Ctrl Pts',(0.00835074983038954,7.92865252690538,
-32.1407982816582));
#65982=CARTESIAN_POINT('Ctrl Pts',(-0.521515106097596,7.91148496056122,
-32.1234100645256));
#65983=CARTESIAN_POINT('Ctrl Pts',(-1.21729330654373,7.81870113380843,-32.0989485180566));
#65984=CARTESIAN_POINT('Ctrl Pts',(-1.38808789987639,7.79019242940608,-32.0927999834681));
#65985=CARTESIAN_POINT('Ctrl Pts',(-1.71207660744212,7.72511975176859,-32.0806346281471));
#65986=CARTESIAN_POINT('Ctrl Pts',(-1.86538329318018,7.689539726963,-32.0746592061713));
#65987=CARTESIAN_POINT('Ctrl Pts',(-2.04150312302437,7.64308846587454,-32.0674307113828));
#65988=CARTESIAN_POINT('Ctrl Pts',(-2.06545809478339,7.63664973296589,-32.0664396455627));
#65989=CARTESIAN_POINT('Ctrl Pts',(-2.09648790095491,7.62815270934539,-32.0651451671526));
#65990=CARTESIAN_POINT('Ctrl Pts',(-2.1035907835459,7.62619702673632,-32.0648481276027));
#65991=CARTESIAN_POINT('Ctrl Pts',(-2.11515392850836,7.62299588770096,-32.0643633895021));
#65992=CARTESIAN_POINT('Ctrl Pts',(-2.11961586177037,7.62175642772344,-32.0641760564711));
#65993=CARTESIAN_POINT('Ctrl Pts',(-2.12819363664245,7.61936553204851,-32.06381537719));
#65994=CARTESIAN_POINT('Ctrl Pts',(-2.13230963998533,7.61821467701593,-32.0636420660704));
#65995=CARTESIAN_POINT('Ctrl Pts',(-2.14171656790985,7.6155762322766,-32.0632454241767));
#65996=CARTESIAN_POINT('Ctrl Pts',(-2.14700687391039,7.61408646457101,-32.0630219628334));
#65997=CARTESIAN_POINT('Ctrl Pts',(-2.16098721046364,7.61013382659959,-32.0624303966404));
#65998=CARTESIAN_POINT('Ctrl Pts',(-2.16967456145709,7.60766159070037,-32.0620617358865));
#65999=CARTESIAN_POINT('Ctrl Pts',(-2.22580841298331,7.59158311628547,-32.059672823784));
#66000=CARTESIAN_POINT('Ctrl Pts',(-2.27312998747154,7.57754822889774,-32.0576275689743));
#66001=CARTESIAN_POINT('Ctrl Pts',(-2.38671856513298,7.54269976804518,-32.0526477087665));
#66002=CARTESIAN_POINT('Ctrl Pts',(-2.45284811076,7.52145470899978,-32.049690334444));
#66003=CARTESIAN_POINT('Ctrl Pts',(-2.58698096558104,7.47640559113867,-32.0435848420577));
#66004=CARTESIAN_POINT('Ctrl Pts',(-2.65495631547724,7.45253765890907,-32.0404339980243));
#66005=CARTESIAN_POINT('Ctrl Pts',(-2.77988267086951,7.40674666808781,-32.0345499131621));
#66006=CARTESIAN_POINT('Ctrl Pts',(-2.83692500027038,7.38508633429586,-32.0318267332487));
#66007=CARTESIAN_POINT('Ctrl Pts',(-3.5587836452981,7.10138196667477,-31.996947785242));
#66008=CARTESIAN_POINT('Ctrl Pts',(-4.18539840775809,6.75108696618127,-31.9624937419401));
#66009=CARTESIAN_POINT('Ctrl Pts',(-4.93936408894463,6.18376722407008,-31.9203867231155));
#66010=CARTESIAN_POINT('Ctrl Pts',(-5.11618277903207,6.0382927677589,-31.9104217604096));
#66011=CARTESIAN_POINT('Ctrl Pts',(-5.39781378012161,5.78532053022073,-31.8944358069358));
#66012=CARTESIAN_POINT('Ctrl Pts',(-5.50631490771182,5.68214982457405,-31.8882452908753));
#66013=CARTESIAN_POINT('Ctrl Pts',(-5.62568190793324,5.56201496216017,-31.881391030868));
#66014=CARTESIAN_POINT('Ctrl Pts',(-5.63948439736159,5.54801974651152,-31.8805977673115));
#66015=CARTESIAN_POINT('Ctrl Pts',(-5.66013375588702,5.52692537804683,-31.8794099005564));
#66016=CARTESIAN_POINT('Ctrl Pts',(-5.66701969465247,5.51986467681662,-31.8790135982288));
#66017=CARTESIAN_POINT('Ctrl Pts',(-5.67883746072272,5.50770155795427,-31.8783331331016));
#66018=CARTESIAN_POINT('Ctrl Pts',(-5.68377565104897,5.50260535616149,-31.878048695048));
#66019=CARTESIAN_POINT('Ctrl Pts',(-5.69392905745856,5.49209881180137,-31.8774636577124));
#66020=CARTESIAN_POINT('Ctrl Pts',(-5.69914343532038,5.48668766870981,-31.8771630946481));
#66021=CARTESIAN_POINT('Ctrl Pts',(-5.71167409476967,5.47364702660575,-31.876440539001));
#66022=CARTESIAN_POINT('Ctrl Pts',(-5.71898281967478,5.46601026765811,-31.8760188708912));
#66023=CARTESIAN_POINT('Ctrl Pts',(-5.74135282243992,5.44254225861115,-31.8747275532989));
#66024=CARTESIAN_POINT('Ctrl Pts',(-5.75636388964646,5.4266631780618,-31.8738600463295));
#66025=CARTESIAN_POINT('Ctrl Pts',(-5.92870775218247,5.24283379469023,-31.8638881040256));
#66026=CARTESIAN_POINT('Ctrl Pts',(-6.07871146979071,5.06815139237069,-31.8550974647243));
#66027=CARTESIAN_POINT('Ctrl Pts',(-6.67321262052441,4.31140878770776,-31.8194064573866));
#66028=CARTESIAN_POINT('Ctrl Pts',(-7.04337583036219,3.67570134342679,-31.7953324453942));
#66029=CARTESIAN_POINT('Ctrl Pts',(-7.36130324978087,2.89940210962108,-31.7652216831868));
#66030=CARTESIAN_POINT('Ctrl Pts',(-7.39975851398585,2.79980197502376,-31.7613391272579));
#66031=CARTESIAN_POINT('Ctrl Pts',(-7.46945580569004,2.607807025721,-31.7537712966342));
#66032=CARTESIAN_POINT('Ctrl Pts',(-7.50102796752054,2.51555280927087,-31.750098726213));
#66033=CARTESIAN_POINT('Ctrl Pts',(-7.56108482316893,2.32887115202488,-31.7425562914119));
#66034=CARTESIAN_POINT('Ctrl Pts',(-7.58952403819407,2.23445012072022,-31.73868237867));
#66035=CARTESIAN_POINT('Ctrl Pts',(-7.62073256200793,2.12335545137803,-31.7340710950086));
#66036=CARTESIAN_POINT('Ctrl Pts',(-7.62522389075164,2.10716961003202,-31.7333979525943));
#66037=CARTESIAN_POINT('Ctrl Pts',(-7.63201120865279,2.08240361106789,-31.7323660853802));
#66038=CARTESIAN_POINT('Ctrl Pts',(-7.63434436910622,2.07383363401384,-31.7320086746811));
#66039=CARTESIAN_POINT('Ctrl Pts',(-7.6385654724808,2.0582253580658,-31.7313571213943));
#66040=CARTESIAN_POINT('Ctrl Pts',(-7.64045813435538,2.05118833819628,-31.7310631417621));
#66041=CARTESIAN_POINT('Ctrl Pts',(-7.64423883960379,2.03705363330922,-31.7304722061582));
#66042=CARTESIAN_POINT('Ctrl Pts',(-7.64612672711592,2.02995591438787,-31.7301752452873));
#66043=CARTESIAN_POINT('Ctrl Pts',(-7.65145525925875,2.00980982032354,-31.7293317362019));
#66044=CARTESIAN_POINT('Ctrl Pts',(-7.65487239786894,1.99675528502656,-31.7287844125234));
#66045=CARTESIAN_POINT('Ctrl Pts',(-7.66918248491949,1.94150965955897,-31.726465222876));
#66046=CARTESIAN_POINT('Ctrl Pts',(-7.67976005484682,1.89923805015853,-31.7246833763051));
#66047=CARTESIAN_POINT('Ctrl Pts',(-7.83664148386959,1.24953790713281,-31.6972021956544));
#66048=CARTESIAN_POINT('Ctrl Pts',(-7.91082999871584,0.626958964402656,
-31.66983724223));
#66049=CARTESIAN_POINT('Ctrl Pts',(-7.91109466759892,-0.347457805831875,
-31.6282329859476));
#66050=CARTESIAN_POINT('Ctrl Pts',(-7.88801474621749,-0.696693083483909,
-31.6135149405729));
#66051=CARTESIAN_POINT('Ctrl Pts',(-7.83562621999283,-1.09048238114358,
-31.5970167840547));
#66052=CARTESIAN_POINT('Ctrl Pts',(-7.82891799512992,-1.1376436764792,-31.5950420537283));
#66053=CARTESIAN_POINT('Ctrl Pts',(-7.81745870441516,-1.21329907349436,
-31.5918748988473));
#66054=CARTESIAN_POINT('Ctrl Pts',(-7.81297682828593,-1.24183264687565,
-31.5906805534045));
#66055=CARTESIAN_POINT('Ctrl Pts',(-7.75905559585409,-1.5732674538819,-31.5768072149549));
#66056=CARTESIAN_POINT('Ctrl Pts',(-7.69218417252294,-1.87307889726213,
-31.5642139934612));
#66057=CARTESIAN_POINT('Ctrl Pts',(-7.59567359883595,-2.21172036286853,
-31.5499472757927));
#66058=CARTESIAN_POINT('Ctrl Pts',(-7.58291171445534,-2.25508632719177,
-31.5481196431667));
#66059=CARTESIAN_POINT('Ctrl Pts',(-7.56165552687678,-2.32509537312519,
-31.5451680282555));
#66060=CARTESIAN_POINT('Ctrl Pts',(-7.55339044700967,-2.35180687203545,
-31.5440415905585));
#66061=CARTESIAN_POINT('Ctrl Pts',(-7.5384401749273,-2.399232052998,-31.5420411291327));
#66062=CARTESIAN_POINT('Ctrl Pts',(-7.53181079206163,-2.41996299787068,
-31.541166491798));
#66063=CARTESIAN_POINT('Ctrl Pts',(-7.51766472171895,-2.4635783556302,-31.5393259586859));
#66064=CARTESIAN_POINT('Ctrl Pts',(-7.51012889729581,-2.48645634048862,
-31.5383602911232));
#66065=CARTESIAN_POINT('Ctrl Pts',(-7.48988525798992,-2.54698226377594,
-31.5358048334161));
#66066=CARTESIAN_POINT('Ctrl Pts',(-7.4769980624138,-2.58456956291366,-31.534217156352));
#66067=CARTESIAN_POINT('Ctrl Pts',(-7.41440487462207,-2.76274439590827,
-31.5266870249399));
#66068=CARTESIAN_POINT('Ctrl Pts',(-7.36101321425368,-2.90200650837284,
-31.5207899802911));
#66069=CARTESIAN_POINT('Ctrl Pts',(-7.02348621961875,-3.713013987416,-31.4863027288329));
#66070=CARTESIAN_POINT('Ctrl Pts',(-6.65150756393093,-4.34432729815641,
-31.4591922932361));
#66071=CARTESIAN_POINT('Ctrl Pts',(-6.16916204865855,-4.95253163277003,
-31.4283500456975));
#66072=CARTESIAN_POINT('Ctrl Pts',(-6.13963029584588,-4.98909508004706,
-31.426474196967));
#66073=CARTESIAN_POINT('Ctrl Pts',(-6.09910413680891,-5.03836599412793,
-31.4239145313122));
#66074=CARTESIAN_POINT('Ctrl Pts',(-6.08839234084904,-5.0513049661903,-31.4232393010717));
#66075=CARTESIAN_POINT('Ctrl Pts',(-6.07103919780077,-5.07213075193236,
-31.4221475882695));
#66076=CARTESIAN_POINT('Ctrl Pts',(-6.06442350095374,-5.08003886857636,
-31.4217318913639));
#66077=CARTESIAN_POINT('Ctrl Pts',(-6.05060564939187,-5.09649066916684,
-31.4208647227296));
#66078=CARTESIAN_POINT('Ctrl Pts',(-6.04340081586462,-5.1050320707336,-31.4204131727678));
#66079=CARTESIAN_POINT('Ctrl Pts',(-6.02635166138397,-5.12515733901525,
-31.4193461025629));
#66080=CARTESIAN_POINT('Ctrl Pts',(-6.01649201046782,-5.13672813978014,
-31.4187301459302));
#66081=CARTESIAN_POINT('Ctrl Pts',(-5.98386411175924,-5.17479581898658,
-31.4166956491679));
#66082=CARTESIAN_POINT('Ctrl Pts',(-5.9609537915148,-5.20117019004048,-31.4152732298421));
#66083=CARTESIAN_POINT('Ctrl Pts',(-5.90580608055135,-5.26381326938454,
-31.4118647957323));
#66084=CARTESIAN_POINT('Ctrl Pts',(-5.87340829052887,-5.29993873438837,
-31.4098748493547));
#66085=CARTESIAN_POINT('Ctrl Pts',(-5.75200465406127,-5.43283064896739,
-31.402467223556));
#66086=CARTESIAN_POINT('Ctrl Pts',(-5.66092392741577,-5.52767092563341,
-31.3970065564033));
#66087=CARTESIAN_POINT('Ctrl Pts',(-5.26077358381815,-5.92407104147126,
-31.3734943694112));
#66088=CARTESIAN_POINT('Ctrl Pts',(-4.9296589999206,-6.20232423878793,-31.3552500741704));
#66089=CARTESIAN_POINT('Ctrl Pts',(-4.47462468353753,-6.5251485024711,-31.3320447396165));
#66090=CARTESIAN_POINT('Ctrl Pts',(-4.37002468866521,-6.59565871001531,
-31.3268231857919));
#66091=CARTESIAN_POINT('Ctrl Pts',(-4.12213687538663,-6.7542717238362,-31.3147073967786));
#66092=CARTESIAN_POINT('Ctrl Pts',(-3.97763548498383,-6.84036668589475,
-31.3078391026435));
#66093=CARTESIAN_POINT('Ctrl Pts',(-3.78809977310634,-6.94525516157924,
-31.2990624028942));
#66094=CARTESIAN_POINT('Ctrl Pts',(-3.74548646663433,-6.96832837304617,
-31.2971037585309));
#66095=CARTESIAN_POINT('Ctrl Pts',(-3.6769023527847,-7.00465273192349,-31.2939740311931));
#66096=CARTESIAN_POINT('Ctrl Pts',(-3.65106573109852,-7.01815430448605,
-31.2928001024155));
#66097=CARTESIAN_POINT('Ctrl Pts',(-3.60414440196854,-7.04234498672688,
-31.2906771447898));
#66098=CARTESIAN_POINT('Ctrl Pts',(-3.58308530723572,-7.05308297607197,
-31.2897275795047));
#66099=CARTESIAN_POINT('Ctrl Pts',(-3.53303413109263,-7.07832194988251,
-31.2874783007508));
#66100=CARTESIAN_POINT('Ctrl Pts',(-3.5040003957738,-7.09273945905055,-31.2861795145715));
#66101=CARTESIAN_POINT('Ctrl Pts',(-3.41707677125766,-7.13523980924604,
-31.2823083771361));
#66102=CARTESIAN_POINT('Ctrl Pts',(-3.35893186966483,-7.16279537351854,
-31.2797416470523));
#66103=CARTESIAN_POINT('Ctrl Pts',(-2.97726518649957,-7.33800229979876,
-31.2630312364852));
#66104=CARTESIAN_POINT('Ctrl Pts',(-2.64442345671335,-7.46441046931321,
-31.2490443105964));
#66105=CARTESIAN_POINT('Ctrl Pts',(-1.83062750384364,-7.7121845546595,-31.2161459464004));
#66106=CARTESIAN_POINT('Ctrl Pts',(-1.34455963419208,-7.81160457120767,
-31.1976698995017));
#66107=CARTESIAN_POINT('Ctrl Pts',(-0.557261029012222,-7.89692975917552,
-31.1682678806545));
#66108=CARTESIAN_POINT('Ctrl Pts',(-0.260582110359735,-7.91227705620617,
-31.1572768914029));
#66109=CARTESIAN_POINT('Ctrl Pts',(0.144575850814257,-7.91042058861035,
-31.141845536624));
#66110=CARTESIAN_POINT('Ctrl Pts',(0.252879680932102,-7.90769922577814,
-31.1376779733704));
#66111=CARTESIAN_POINT('Ctrl Pts',(0.388978521577137,-7.90148062305087,
-31.1323571733784));
#66112=CARTESIAN_POINT('Ctrl Pts',(0.416858741833247,-7.90005880338862,
-31.131262759116));
#66113=CARTESIAN_POINT('Ctrl Pts',(0.460534313892255,-7.89759961586249,
-31.1295406836525));
#66114=CARTESIAN_POINT('Ctrl Pts',(0.4763351861932,-7.89666235402076,-31.1289161085196));
#66115=CARTESIAN_POINT('Ctrl Pts',(0.53053420741295,-7.89328415998898,-31.1267680880751));
#66116=CARTESIAN_POINT('Ctrl Pts',(0.568916992292914,-7.89061054501134,
-31.1252371718538));
#66117=CARTESIAN_POINT('Ctrl Pts',(0.619321065328954,-7.8867298866248,-31.1232124536208));
#66118=CARTESIAN_POINT('Ctrl Pts',(0.631361596800325,-7.8857751311256,-31.1227277132532));
#66119=CARTESIAN_POINT('Ctrl Pts',(0.649985009579569,-7.88425545884588,
-31.1219762312868));
#66120=CARTESIAN_POINT('Ctrl Pts',(0.656569477659818,-7.8837098610813,-31.1217102054028));
#66121=CARTESIAN_POINT('Ctrl Pts',(0.669706449459131,-7.88260474208809,
-31.1211787685045));
#66122=CARTESIAN_POINT('Ctrl Pts',(0.676258953935233,-7.88204529772041,
-31.1209133606));
#66123=CARTESIAN_POINT('Ctrl Pts',(0.690825885127546,-7.88078329362997,
-31.1203225695147));
#66124=CARTESIAN_POINT('Ctrl Pts',(0.698839946687277,-7.8800766781179,-31.1199970312885));
#66125=CARTESIAN_POINT('Ctrl Pts',(0.722093744835764,-7.87799059256053,
-31.1190509237418));
#66126=CARTESIAN_POINT('Ctrl Pts',(0.737330522670652,-7.87657913365695,
-31.1184291055345));
#66127=CARTESIAN_POINT('Ctrl Pts',(0.846367068153694,-7.86615937655385,
-31.1139651887446));
#66128=CARTESIAN_POINT('Ctrl Pts',(0.939994042255055,-7.85552107058926,
-31.1100547342848));
#66129=CARTESIAN_POINT('Ctrl Pts',(1.15435315451245,-7.82727727986818,-31.100904455957));
#66130=CARTESIAN_POINT('Ctrl Pts',(1.27490171354553,-7.80854815308775,-31.095622016279));
#66131=CARTESIAN_POINT('Ctrl Pts',(1.70456875705568,-7.7315779295109,-31.0764030940466));
#66132=CARTESIAN_POINT('Ctrl Pts',(2.01057796622553,-7.65770280881923,-31.0619939145715));
#66133=CARTESIAN_POINT('Ctrl Pts',(2.85686237701296,-7.39916218104642,-31.0212642570759));
#66134=CARTESIAN_POINT('Ctrl Pts',(3.38279802794428,-7.1739853360649,-30.9950230237459));
#66135=CARTESIAN_POINT('Ctrl Pts',(4.06947196698913,-6.78753305416735,-30.9611753859278));
#66136=CARTESIAN_POINT('Ctrl Pts',(4.2545058690236,-6.67310993921001,-30.9520815792078));
#66137=CARTESIAN_POINT('Ctrl Pts',(4.452947618013,-6.538781951025,-30.9423547502225));
#66138=CARTESIAN_POINT('Ctrl Pts',(4.47124318868071,-6.52628502667661,-30.9414581880409));
#66139=CARTESIAN_POINT('Ctrl Pts',(4.49841805062522,-6.50755512618639,-30.9401267786751));
#66140=CARTESIAN_POINT('Ctrl Pts',(4.50733733985906,-6.5013805291198,-30.9396898302069));
#66141=CARTESIAN_POINT('Ctrl Pts',(4.52262443695468,-6.49075108102595,-30.9389409982033));
#66142=CARTESIAN_POINT('Ctrl Pts',(4.5289984215394,-6.48630516485975,-30.9386287922143));
#66143=CARTESIAN_POINT('Ctrl Pts',(4.5420912619051,-6.47714407312334,-30.9379875280657));
#66144=CARTESIAN_POINT('Ctrl Pts',(4.54880935265136,-6.47242781722705,-30.9376585096318));
#66145=CARTESIAN_POINT('Ctrl Pts',(4.56434665209146,-6.46148413278624,-30.9368976166995));
#66146=CARTESIAN_POINT('Ctrl Pts',(4.57316048614798,-6.45524908332551,-30.9364660199888));
#66147=CARTESIAN_POINT('Ctrl Pts',(4.60087811428871,-6.43555592387886,-30.9351088354027));
#66148=CARTESIAN_POINT('Ctrl Pts',(4.61973554799491,-6.42203261823497,-30.9341856272678));
#66149=CARTESIAN_POINT('Ctrl Pts',(4.90103247327797,-6.21842488961355,-30.9204154852491));
#66150=CARTESIAN_POINT('Ctrl Pts',(5.15162069471398,-6.01246677347793,-30.9081836514859));
#66151=CARTESIAN_POINT('Ctrl Pts',(5.94882546433572,-5.27070814939611,-30.8685838381294));
#66152=CARTESIAN_POINT('Ctrl Pts',(6.4301978690022,-4.67132585070535,-30.8437682332246));
#66153=CARTESIAN_POINT('Ctrl Pts',(6.92775375727652,-3.82582519228611,-30.8078365056906));
#66154=CARTESIAN_POINT('Ctrl Pts',(7.02976558435145,-3.63498329576021,-30.7996450988271));
#66155=CARTESIAN_POINT('Ctrl Pts',(7.13051200700972,-3.42636188930724,-30.7903979936733));
#66156=CARTESIAN_POINT('Ctrl Pts',(7.13715605391671,-3.41250065723276,-30.7897823748592));
#66157=CARTESIAN_POINT('Ctrl Pts',(7.14697082519832,-3.39187041254928,-30.7888644081967));
#66158=CARTESIAN_POINT('Ctrl Pts',(7.15017244975129,-3.38511607039545,-30.7885635932995));
#66159=CARTESIAN_POINT('Ctrl Pts',(7.15563941755037,-3.37354026274542,-30.7880475934594));
#66160=CARTESIAN_POINT('Ctrl Pts',(7.15790947587095,-3.36872102041342,-30.7878326378659));
#66161=CARTESIAN_POINT('Ctrl Pts',(7.16231772733507,-3.35933790702278,-30.7874138609325));
#66162=CARTESIAN_POINT('Ctrl Pts',(7.16445643131997,-3.35477427622103,-30.7872100641228));
#66163=CARTESIAN_POINT('Ctrl Pts',(7.16956372523411,-3.34384902061821,-30.7867219017297));
#66164=CARTESIAN_POINT('Ctrl Pts',(7.17252820822192,-3.33748548831229,-30.7864373424223));
#66165=CARTESIAN_POINT('Ctrl Pts',(7.18139747888165,-3.31838039778606,-30.7855823635895));
#66166=CARTESIAN_POINT('Ctrl Pts',(7.18727679387116,-3.30562709615756,-30.7850107658882));
#66167=CARTESIAN_POINT('Ctrl Pts',(7.23882999771045,-3.19301110735589,-30.7799561324362));
#66168=CARTESIAN_POINT('Ctrl Pts',(7.28245270813326,-3.09222586318413,-30.7753826068113));
#66169=CARTESIAN_POINT('Ctrl Pts',(7.39619358228847,-2.81367219273417,-30.7626677858631));
#66170=CARTESIAN_POINT('Ctrl Pts',(7.46199051755742,-2.6342216983436,-30.754396543991));
#66171=CARTESIAN_POINT('Ctrl Pts',(7.67189178844118,-1.99052403353636,-30.724802594924));
#66172=CARTESIAN_POINT('Ctrl Pts',(7.77967009335558,-1.51554641116677,-30.7031871408693));
#66173=CARTESIAN_POINT('Ctrl Pts',(7.88771849966673,-0.695716921782237,
-30.667719962537));
#66174=CARTESIAN_POINT('Ctrl Pts',(7.91037113883237,-0.355213942632094,
-30.6534900027122));
#66175=CARTESIAN_POINT('Ctrl Pts',(7.91105602012169,0.0238600128303358,
-30.6381300520454));
#66176=CARTESIAN_POINT('Ctrl Pts',(7.91084894626896,0.0620131744865623,
-30.6365892061203));
#66177=CARTESIAN_POINT('Ctrl Pts',(7.91013643208999,0.118283622747458,-30.6343237316644));
#66178=CARTESIAN_POINT('Ctrl Pts',(7.90984472935629,0.136402897178744,-30.6335953192977));
#66179=CARTESIAN_POINT('Ctrl Pts',(7.90921744801982,0.168511634603927,-30.6323063591118));
#66180=CARTESIAN_POINT('Ctrl Pts',(7.908907005286,0.18250149105554,-30.6317453757599));
#66181=CARTESIAN_POINT('Ctrl Pts',(7.90818961924645,0.21137561387696,-30.630588784483));
#66182=CARTESIAN_POINT('Ctrl Pts',(7.90777776946245,0.22625970608043,-30.6299932630263));
#66183=CARTESIAN_POINT('Ctrl Pts',(7.90661705563113,0.264320758550473,-30.6284720976446));
#66184=CARTESIAN_POINT('Ctrl Pts',(7.90580830189384,0.287495787338779,-30.627547467775));
#66185=CARTESIAN_POINT('Ctrl Pts',(7.90222075301944,0.378780691624412,-30.6239113195488));
#66186=CARTESIAN_POINT('Ctrl Pts',(7.89866355399836,0.446857785799987,-30.6212123650041));
#66187=CARTESIAN_POINT('Ctrl Pts',(7.87156157505004,0.862389213760703,-30.6048124122027));
#66188=CARTESIAN_POINT('Ctrl Pts',(7.8259744721659,1.20803051391749,-30.5915094442729));
#66189=CARTESIAN_POINT('Ctrl Pts',(7.62220316891117,2.22819915116485,-30.552584810201));
#66190=CARTESIAN_POINT('Ctrl Pts',(7.39819884383389,2.88606464509801,-30.5281325351967));
#66191=CARTESIAN_POINT('Ctrl Pts',(7.05113323551834,3.58799949102011,-30.4976519169709));
#66192=CARTESIAN_POINT('Ctrl Pts',(7.00934880589826,3.66895745839981,-30.494060726343));
#66193=CARTESIAN_POINT('Ctrl Pts',(6.95934964213475,3.7618587255609,-30.4898352487537));
#66194=CARTESIAN_POINT('Ctrl Pts',(6.95248809044918,3.7745248523972,-30.4892568705016));
#66195=CARTESIAN_POINT('Ctrl Pts',(6.94152802215273,3.79462538135589,-30.488335297493));
#66196=CARTESIAN_POINT('Ctrl Pts',(6.93745205013071,3.8020720822456,-30.4879930667205));
#66197=CARTESIAN_POINT('Ctrl Pts',(6.93025991427406,3.81516186753541,-30.4873900429003));
#66198=CARTESIAN_POINT('Ctrl Pts',(6.92714882041902,3.82080773846862,-30.4871294711461));
#66199=CARTESIAN_POINT('Ctrl Pts',(6.92072410762015,3.83243337371045,-30.4865919252732));
#66200=CARTESIAN_POINT('Ctrl Pts',(6.91740963189957,3.83841265653451,-30.4863149133089));
#66201=CARTESIAN_POINT('Ctrl Pts',(6.90894911680448,3.85362879670824,-30.4856085737933));
#66202=CARTESIAN_POINT('Ctrl Pts',(6.90379231165114,3.86285962954263,-30.4851787618871));
#66203=CARTESIAN_POINT('Ctrl Pts',(6.88301737254324,3.89987290053247,-30.4834499609341));
#66204=CARTESIAN_POINT('Ctrl Pts',(6.86725005879419,3.92757092605988,-30.4821440951859));
#66205=CARTESIAN_POINT('Ctrl Pts',(6.76860172730848,4.09845370468132,-30.4740082398556));
#66206=CARTESIAN_POINT('Ctrl Pts',(6.68142618216043,4.23908297715535,-30.4669420226383));
#66207=CARTESIAN_POINT('Ctrl Pts',(6.51919463786934,4.48334252897653,-30.4540841834948));
#66208=CARTESIAN_POINT('Ctrl Pts',(6.44590830374343,4.58808491743453,-30.4483753981573));
#66209=CARTESIAN_POINT('Ctrl Pts',(6.31501405763401,4.76583197783503,-30.4384047701096));
#66210=CARTESIAN_POINT('Ctrl Pts',(6.25859556829831,4.83968367395317,-30.4341739281798));
#66211=CARTESIAN_POINT('Ctrl Pts',(6.15134952572091,4.97505624425465,-30.4262752009007));
#66212=CARTESIAN_POINT('Ctrl Pts',(6.1008662976941,5.0368359017448,-30.4226127841326));
#66213=CARTESIAN_POINT('Ctrl Pts',(5.58042171337021,5.65443213686781,-30.3854804491462));
#66214=CARTESIAN_POINT('Ctrl Pts',(5.03671743501126,6.14374077407838,-30.3521828128889));
#66215=CARTESIAN_POINT('Ctrl Pts',(4.40298918985832,6.57259326334364,-30.3209082476206));
#66216=CARTESIAN_POINT('Ctrl Pts',(4.37213294565909,6.59315930091494,-30.3194010359288));
#66217=CARTESIAN_POINT('Ctrl Pts',(4.32751036219462,6.62244974296305,-30.317243554153));
#66218=CARTESIAN_POINT('Ctrl Pts',(4.31386012184477,6.63134959012074,-30.3165865302608));
#66219=CARTESIAN_POINT('Ctrl Pts',(4.29194471543767,6.64554195523146,-30.3155363983548));
#66220=CARTESIAN_POINT('Ctrl Pts',(4.28369706581746,6.65086135536977,-30.3151422572139));
#66221=CARTESIAN_POINT('Ctrl Pts',(4.26907029292369,6.66025653698573,-30.3144451502541));
#66222=CARTESIAN_POINT('Ctrl Pts',(4.26269518647914,6.66433853071539,-30.3141419461005));
#66223=CARTESIAN_POINT('Ctrl Pts',(4.24958902082864,6.67270393531837,-30.3135199015106));
#66224=CARTESIAN_POINT('Ctrl Pts',(4.24285731990081,6.67698632751498,-30.3132011003094));
#66225=CARTESIAN_POINT('Ctrl Pts',(4.22563809724778,6.68790383328617,-30.3123874092189));
#66226=CARTESIAN_POINT('Ctrl Pts',(4.21514140173554,6.69452447731995,-30.3118930737478));
#66227=CARTESIAN_POINT('Ctrl Pts',(4.19236714760905,6.70881422091352,-30.3108241647312));
#66228=CARTESIAN_POINT('Ctrl Pts',(4.18008401940079,6.71647438354288,-30.3102499332002));
#66229=CARTESIAN_POINT('Ctrl Pts',(4.14477228199984,6.73836155524108,-30.3086056181984));
#66230=CARTESIAN_POINT('Ctrl Pts',(4.12169148490385,6.75250420519344,-30.3075387458022));
#66231=CARTESIAN_POINT('Ctrl Pts',(4.04459541712736,6.79920188896021,-30.3040010904465));
#66232=CARTESIAN_POINT('Ctrl Pts',(3.99026289614521,6.83122980659411,-30.3015502208364));
#66233=CARTESIAN_POINT('Ctrl Pts',(3.78671200957979,6.94796174178403,-30.2925201123927));
#66234=CARTESIAN_POINT('Ctrl Pts',(3.63512973373935,7.02845617994655,-30.2860966644913));
#66235=CARTESIAN_POINT('Ctrl Pts',(3.19316172133092,7.24502690815435,-30.2681148696377));
#66236=CARTESIAN_POINT('Ctrl Pts',(2.89696188599029,7.36846826317054,-30.2569698250116));
#66237=CARTESIAN_POINT('Ctrl Pts',(1.90094924939149,7.71418302410957,-30.2211059987988));
#66238=CARTESIAN_POINT('Ctrl Pts',(1.17783382901439,7.85713752256069,-30.197786284806));
#66239=CARTESIAN_POINT('Ctrl Pts',(0.403260771362742,7.90082867502684,-30.1673425235347));
#66240=CARTESIAN_POINT('Ctrl Pts',(0.360978219879948,7.90287337602871,-30.1656629086913));
#66241=CARTESIAN_POINT('Ctrl Pts',(0.310393605175625,7.90491275220911,-30.1636302553017));
#66242=CARTESIAN_POINT('Ctrl Pts',(0.302104657898855,7.90523387287599,-30.1632964322839));
#66243=CARTESIAN_POINT('Ctrl Pts',(0.288624248632822,7.90573488215121,-30.1627522976938));
#66244=CARTESIAN_POINT('Ctrl Pts',(0.283433071205645,7.90592269615651,-30.1625424589822));
#66245=CARTESIAN_POINT('Ctrl Pts',(0.274195440017041,7.90624779863203,-30.1621685185534));
#66246=CARTESIAN_POINT('Ctrl Pts',(0.270149053977545,7.90638709406591,-30.1620045376311));
#66247=CARTESIAN_POINT('Ctrl Pts',(0.261640806977383,7.90667344829711,-30.1616593512281));
#66248=CARTESIAN_POINT('Ctrl Pts',(0.257178922972824,7.90681983678431,-30.1614781050564));
#66249=CARTESIAN_POINT('Ctrl Pts',(0.245342475801262,7.90719814520814,-30.1609966974662));
#66250=CARTESIAN_POINT('Ctrl Pts',(0.237967728469296,7.90742352460471,-30.1606961378068));
#66251=CARTESIAN_POINT('Ctrl Pts',(0.203564688608862,7.90842674318086,-30.1592911958015));
#66252=CARTESIAN_POINT('Ctrl Pts',(0.176533141881781,7.90907631449856,-30.1581791195421));
#66253=CARTESIAN_POINT('Ctrl Pts',(-0.0336745918107459,7.91304945149483,
-30.1494708525657));
#66254=CARTESIAN_POINT('Ctrl Pts',(-0.21690176027324,7.91014729597411,-30.1415249856171));
#66255=CARTESIAN_POINT('Ctrl Pts',(-0.648250508851609,7.88831752313143,
-30.1222683675568));
#66256=CARTESIAN_POINT('Ctrl Pts',(-0.895910941305013,7.86403939117933,
-30.1107839212929));
#66257=CARTESIAN_POINT('Ctrl Pts',(-1.21906046256736,7.81689686316326,-30.0955776740002));
#66258=CARTESIAN_POINT('Ctrl Pts',(-1.29594598064942,7.80451849415018,-30.091942651396));
#66259=CARTESIAN_POINT('Ctrl Pts',(-1.64087612471697,7.74374797855015,-30.0755881460682));
#66260=CARTESIAN_POINT('Ctrl Pts',(-1.90650453261117,7.682665953918,-30.062874757192));
#66261=CARTESIAN_POINT('Ctrl Pts',(-2.33549162529119,7.56039458835516,-30.0425012568226));
#66262=CARTESIAN_POINT('Ctrl Pts',(-2.50091650644738,7.50729701304209,-30.0346825799805));
#66263=CARTESIAN_POINT('Ctrl Pts',(-2.94934599264981,7.34689187755918,-30.0136782152457));
#66264=CARTESIAN_POINT('Ctrl Pts',(-3.22816313801968,7.22872419540384,-30.0008421042003));
#66265=CARTESIAN_POINT('Ctrl Pts',(-3.52106894085083,7.08424803693792,-29.9876237250175));
#66266=CARTESIAN_POINT('Ctrl Pts',(-3.54253976029041,7.07353580580807,-29.9866562763712));
#66267=CARTESIAN_POINT('Ctrl Pts',(-3.5731138759585,7.05810763037794,-29.9852807244915));
#66268=CARTESIAN_POINT('Ctrl Pts',(-3.58225714495782,7.05347147446315,-29.9848696286543));
#66269=CARTESIAN_POINT('Ctrl Pts',(-3.5978920740052,7.04550543627943,-29.9841671079139));
#66270=CARTESIAN_POINT('Ctrl Pts',(-3.60438817455887,7.04218432848272,-29.9838753534939));
#66271=CARTESIAN_POINT('Ctrl Pts',(-3.61738559692894,7.03551674781922,-29.9832918746423));
#66272=CARTESIAN_POINT('Ctrl Pts',(-3.62388689188834,7.03217023833397,-29.9830001520037));
#66273=CARTESIAN_POINT('Ctrl Pts',(-3.63979032738198,7.02395611220406,-29.982286863193));
#66274=CARTESIAN_POINT('Ctrl Pts',(-3.64918736676555,7.019078618801,-29.9818656700143));
#66275=CARTESIAN_POINT('Ctrl Pts',(-3.68203957603911,7.00194301349661,-29.9803941208854));
#66276=CARTESIAN_POINT('Ctrl Pts',(-3.70544312699072,6.98958601456133,-29.9793475031024));
#66277=CARTESIAN_POINT('Ctrl Pts',(-4.09654791494488,6.78056751458441,-29.9618842723436));
#66278=CARTESIAN_POINT('Ctrl Pts',(-4.44821553869818,6.55524440088101,-29.9466396627183));
#66279=CARTESIAN_POINT('Ctrl Pts',(-5.05758943008729,6.09308185077178,-29.9198776352081));
#66280=CARTESIAN_POINT('Ctrl Pts',(-5.32051739514024,5.86489168612146,-29.9081768421803));
#66281=CARTESIAN_POINT('Ctrl Pts',(-5.89495300460541,5.29582917055988,-29.8805859109353));
#66282=CARTESIAN_POINT('Ctrl Pts',(-6.19333240531306,4.94356294329962,-29.8646281384437));
#66283=CARTESIAN_POINT('Ctrl Pts',(-6.47609337262869,4.54367462723823,-29.845251765124));
#66284=CARTESIAN_POINT('Ctrl Pts',(-6.49273025527776,4.51986927669983,-29.8440937411108));
#66285=CARTESIAN_POINT('Ctrl Pts',(-6.51385249860407,4.4892886547941,-29.8425995638788));
#66286=CARTESIAN_POINT('Ctrl Pts',(-6.51845921293386,4.48259706953394,-29.8422722108618));
#66287=CARTESIAN_POINT('Ctrl Pts',(-6.52577154285505,4.47194027395814,-29.8417502584495));
#66288=CARTESIAN_POINT('Ctrl Pts',(-6.52848388508983,4.46797965587464,-29.8415561377309));
#66289=CARTESIAN_POINT('Ctrl Pts',(-6.53356081859692,4.46055171961291,-29.841191823043));
#66290=CARTESIAN_POINT('Ctrl Pts',(-6.53592626027069,4.45708498166893,-29.8410216890955));
#66291=CARTESIAN_POINT('Ctrl Pts',(-6.54125105177545,4.44926773327967,-29.8406378214743));
#66292=CARTESIAN_POINT('Ctrl Pts',(-6.54420881976992,4.44491615306122,-29.8404239775491));
#66293=CARTESIAN_POINT('Ctrl Pts',(-6.55291636980478,4.43207774489391,-29.8397926169946));
#66294=CARTESIAN_POINT('Ctrl Pts',(-6.55865398074421,4.42358271601417,-29.8393742614107));
#66295=CARTESIAN_POINT('Ctrl Pts',(-6.60249254913352,4.35840314377062,-29.8361599787696));
#66296=CARTESIAN_POINT('Ctrl Pts',(-6.63987346627582,4.3012400132315,-29.8333157024461));
#66297=CARTESIAN_POINT('Ctrl Pts',(-6.76411840035756,4.10576399663811,-29.8235235792462));
#66298=CARTESIAN_POINT('Ctrl Pts',(-6.84743431510808,3.9652532546874,-29.8163752520347));
#66299=CARTESIAN_POINT('Ctrl Pts',(-7.38896915008159,2.98393845548317,-29.7662270800584));
#66300=CARTESIAN_POINT('Ctrl Pts',(-7.69563882200766,2.06849683217669,-29.7195093910852));
#66301=CARTESIAN_POINT('Ctrl Pts',(-7.83742618279089,1.07728973648198,-29.6771439962136));
#66302=CARTESIAN_POINT('Ctrl Pts',(-7.84321500574677,1.0343020834259,-29.6753195703304));
#66303=CARTESIAN_POINT('Ctrl Pts',(-7.86283508600912,0.878954527467531,
-29.6687729210172));
#66304=CARTESIAN_POINT('Ctrl Pts',(-7.87460802587007,0.766346197070954,
-29.664115099647));
#66305=CARTESIAN_POINT('Ctrl Pts',(-7.88558033158646,0.633978207912988,
-29.6587389001528));
#66306=CARTESIAN_POINT('Ctrl Pts',(-7.88712759804527,0.614429648812501,
-29.657947441783));
#66307=CARTESIAN_POINT('Ctrl Pts',(-7.88935323263258,0.584915662421159,
-29.6567562734582));
#66308=CARTESIAN_POINT('Ctrl Pts',(-7.89008543379534,0.574954441454825,
-29.6563548897692));
#66309=CARTESIAN_POINT('Ctrl Pts',(-7.89133631516723,0.557484360391646,
-29.65565206487));
#66310=CARTESIAN_POINT('Ctrl Pts',(-7.89186314712144,0.549976107359509,
-29.655350370752));
#66311=CARTESIAN_POINT('Ctrl Pts',(-7.89288103445576,0.535166816837853,
-29.654756024068));
#66312=CARTESIAN_POINT('Ctrl Pts',(-7.89337267674014,0.527865828005366,
-29.6544633535741));
#66313=CARTESIAN_POINT('Ctrl Pts',(-7.89441055682498,0.512127375832744,
-29.6538331906477));
#66314=CARTESIAN_POINT('Ctrl Pts',(-7.89495339960037,0.503689693650676,
-29.6534958037456));
#66315=CARTESIAN_POINT('Ctrl Pts',(-7.89623313480466,0.483287666565888,
-29.6526811083181));
#66316=CARTESIAN_POINT('Ctrl Pts',(-7.89695636427905,0.471322469351202,
-29.6522042229476));
#66317=CARTESIAN_POINT('Ctrl Pts',(-7.90026880855241,0.41437196929971,-29.6499386941727));
#66318=CARTESIAN_POINT('Ctrl Pts',(-7.90250086876657,0.369366320770449,
-29.6481610895407));
#66319=CARTESIAN_POINT('Ctrl Pts',(-7.90877563734356,0.216448369893865,
-29.6421629416023));
#66320=CARTESIAN_POINT('Ctrl Pts',(-7.91099340001276,0.108472183981981,
-29.6379982978424));
#66321=CARTESIAN_POINT('Ctrl Pts',(-7.91099998529096,0.000482417337385414,
-29.6338954699259));
#66322=CARTESIAN_POINT('',(-7.91099357096916,0.0100856375418233,-25.6423315082367));
#66323=CARTESIAN_POINT('Ctrl Pts',(-7.91099998316719,0.000516070481359765,
-29.6338967485033));
#66324=CARTESIAN_POINT('Ctrl Pts',(-7.91106109109898,-0.936225837637782,
-29.5983072379579));
#66325=CARTESIAN_POINT('Ctrl Pts',(-7.74476825623127,-1.86545424022548,
-29.5686551740999));
#66326=CARTESIAN_POINT('Ctrl Pts',(-7.3896962694167,-2.82557461689186,-29.5306286759953));
#66327=CARTESIAN_POINT('Ctrl Pts',(-7.35819158792394,-2.90663012849464,
-29.5273496043355));
#66328=CARTESIAN_POINT('Ctrl Pts',(-7.2870418028981,-3.08111015846711,-29.5201117040888));
#66329=CARTESIAN_POINT('Ctrl Pts',(-7.24692385690003,-3.17432044295903,
-29.5161277416962));
#66330=CARTESIAN_POINT('Ctrl Pts',(-7.19804016399774,-3.2821372659141,-29.511397454883));
#66331=CARTESIAN_POINT('Ctrl Pts',(-7.19100455296732,-3.2975234265895,-29.5107194944065));
#66332=CARTESIAN_POINT('Ctrl Pts',(-7.18018945622697,-3.3209757176619,-29.5096817613069));
#66333=CARTESIAN_POINT('Ctrl Pts',(-7.1764455899473,-3.32905828101778,-29.5093233265068));
#66334=CARTESIAN_POINT('Ctrl Pts',(-7.16961355284964,-3.34374275697509,
-29.508670695892));
#66335=CARTESIAN_POINT('Ctrl Pts',(-7.16652989105734,-3.35034676447669,
-29.50837666581));
#66336=CARTESIAN_POINT('Ctrl Pts',(-7.16032700665847,-3.36358319003425,
-29.5077862992548));
#66337=CARTESIAN_POINT('Ctrl Pts',(-7.1572076847347,-3.37021555330357,-29.5074899593864));
#66338=CARTESIAN_POINT('Ctrl Pts',(-7.14835125920349,-3.38897850994578,
-29.5066501409211));
#66339=CARTESIAN_POINT('Ctrl Pts',(-7.14259251424448,-3.40109882816688,
-29.5061058976552));
#66340=CARTESIAN_POINT('Ctrl Pts',(-7.11826957243991,-3.45195662142256,
-29.5038150098009));
#66341=CARTESIAN_POINT('Ctrl Pts',(-7.09942101555662,-3.49055688895462,
-29.5020586794983));
#66342=CARTESIAN_POINT('Ctrl Pts',(-6.86941582636518,-3.95201785168591,
-29.4808628278932));
#66343=CARTESIAN_POINT('Ctrl Pts',(-6.62109082776764,-4.35527931618148,
-29.4603983174135));
#66344=CARTESIAN_POINT('Ctrl Pts',(-5.9972238798474,-5.19057234523664,-29.41557834769));
#66345=CARTESIAN_POINT('Ctrl Pts',(-5.60782149410329,-5.60902168805794,
-29.3914868123181));
#66346=CARTESIAN_POINT('Ctrl Pts',(-5.01148041478717,-6.12509612416234,
-29.3588857124585));
#66347=CARTESIAN_POINT('Ctrl Pts',(-4.84026346110284,-6.2612770444313,-29.3498956108031));
#66348=CARTESIAN_POINT('Ctrl Pts',(-4.5654100381966,-6.46186785145347,-29.3359968767411));
#66349=CARTESIAN_POINT('Ctrl Pts',(-4.465554858833,-6.53127286687329,-29.3310535486224));
#66350=CARTESIAN_POINT('Ctrl Pts',(-4.3334061986132,-6.61867580254186,-29.3246488857999));
#66351=CARTESIAN_POINT('Ctrl Pts',(-4.30253185217634,-6.63878741475022,
-29.3231620483453));
#66352=CARTESIAN_POINT('Ctrl Pts',(-4.25178177865611,-6.67134338200633,
-29.3207334651445));
#66353=CARTESIAN_POINT('Ctrl Pts',(-4.23198929183552,-6.68391632592351,
-29.3197901189104));
#66354=CARTESIAN_POINT('Ctrl Pts',(-4.19355002944703,-6.70809522390468,
-29.3179653390826));
#66355=CARTESIAN_POINT('Ctrl Pts',(-4.1749102459602,-6.7197118854999,-29.3170837759764));
#66356=CARTESIAN_POINT('Ctrl Pts',(-4.13167576167638,-6.74640709162962,
-29.3150465895203));
#66357=CARTESIAN_POINT('Ctrl Pts',(-4.10704645061681,-6.76142904319136,
-29.3138917046242));
#66358=CARTESIAN_POINT('Ctrl Pts',(-4.06237225842249,-6.78834264045562,
-29.3118069668739));
#66359=CARTESIAN_POINT('Ctrl Pts',(-4.04235596726764,-6.8002810536311,-29.3108765205304));
#66360=CARTESIAN_POINT('Ctrl Pts',(-3.90819160345405,-6.87949967266792,
-29.3046638981426));
#66361=CARTESIAN_POINT('Ctrl Pts',(-3.7924204022117,-6.9439920512294,-29.2994188259116));
#66362=CARTESIAN_POINT('Ctrl Pts',(-3.04085383111548,-7.33826096562028,
-29.2660433643931));
#66363=CARTESIAN_POINT('Ctrl Pts',(-2.36441270184676,-7.58329347524111,
-29.2393558037556));
#66364=CARTESIAN_POINT('Ctrl Pts',(-1.59314994728801,-7.74926383300711,
-29.2081823562558));
#66365=CARTESIAN_POINT('Ctrl Pts',(-1.5217998712111,-7.7635907683359,-29.2052885943377));
#66366=CARTESIAN_POINT('Ctrl Pts',(-1.43186558811601,-7.78036195679973,
-29.2016212186808));
#66367=CARTESIAN_POINT('Ctrl Pts',(-1.413456061651,-7.7837274617579,-29.2008694435223));
#66368=CARTESIAN_POINT('Ctrl Pts',(-1.38338428959784,-7.78911477613938,
-29.1996396418152));
#66369=CARTESIAN_POINT('Ctrl Pts',(-1.3717292212564,-7.79117577975042,-29.1991625732938));
#66370=CARTESIAN_POINT('Ctrl Pts',(-1.34912126127317,-7.79512131651534,
-29.1982363790025));
#66371=CARTESIAN_POINT('Ctrl Pts',(-1.33816893293537,-7.797008940793,-29.1977873250286));
#66372=CARTESIAN_POINT('Ctrl Pts',(-1.312831366838,-7.80132088907797,-29.1967476556345));
#66373=CARTESIAN_POINT('Ctrl Pts',(-1.29844334160651,-7.80372851262283,
-29.1961566728842));
#66374=CARTESIAN_POINT('Ctrl Pts',(-1.25963417804321,-7.81011235120941,
-29.1945610546533));
#66375=CARTESIAN_POINT('Ctrl Pts',(-1.23520096789705,-7.81401380601213,
-29.1935548471101));
#66376=CARTESIAN_POINT('Ctrl Pts',(-1.03574133942523,-7.84490430186414,
-29.1853283988042));
#66377=CARTESIAN_POINT('Ctrl Pts',(-0.859875055411986,-7.86612332505235,
-29.1779986507248));
#66378=CARTESIAN_POINT('Ctrl Pts',(-0.110163712509447,-7.93113561746692,
-29.1466205779375));
#66379=CARTESIAN_POINT('Ctrl Pts',(0.466860514342553,-7.91815149700524,
-29.1222618340021));
#66380=CARTESIAN_POINT('Ctrl Pts',(1.14734958195007,-7.82814281222514,-29.094009778787));
#66381=CARTESIAN_POINT('Ctrl Pts',(1.25702445714687,-7.81128164242897,-29.0894666302711));
#66382=CARTESIAN_POINT('Ctrl Pts',(1.44701972670491,-7.7779669172184,-29.0816099025397));
#66383=CARTESIAN_POINT('Ctrl Pts',(1.52750589023526,-7.76256152219709,-29.0782858541982));
#66384=CARTESIAN_POINT('Ctrl Pts',(1.64273535455978,-7.73864452500787,-29.0735304911287));
#66385=CARTESIAN_POINT('Ctrl Pts',(1.67768246791217,-7.73114351701248,-29.072088737585));
#66386=CARTESIAN_POINT('Ctrl Pts',(1.73850535919063,-7.71765673087432,-29.0695799641694));
#66387=CARTESIAN_POINT('Ctrl Pts',(1.76440401304015,-7.71177701856108,-29.0685118733644));
#66388=CARTESIAN_POINT('Ctrl Pts',(1.81449042903207,-7.70014049499746,-29.0664463912986));
#66389=CARTESIAN_POINT('Ctrl Pts',(1.83868162280341,-7.69439985016794,-29.065448849489));
#66390=CARTESIAN_POINT('Ctrl Pts',(1.89640527066943,-7.68041407936262,-29.0630685472436));
#66391=CARTESIAN_POINT('Ctrl Pts',(1.92991162874521,-7.6720632490916,-29.0616868539979));
#66392=CARTESIAN_POINT('Ctrl Pts',(2.05238240223913,-7.64068663105737,-29.0566357002509));
#66393=CARTESIAN_POINT('Ctrl Pts',(2.14099883181857,-7.61633047590636,-29.052979231412));
#66394=CARTESIAN_POINT('Ctrl Pts',(2.88196908750552,-7.3987211499181,-29.0223525927401));
#66395=CARTESIAN_POINT('Ctrl Pts',(3.50734879203526,-7.12358211206623,-28.9961938106266));
#66396=CARTESIAN_POINT('Ctrl Pts',(4.42913738788019,-6.56687218225373,-28.956033772302));
#66397=CARTESIAN_POINT('Ctrl Pts',(4.75257750455889,-6.33672319210183,-28.9414930046943));
#66398=CARTESIAN_POINT('Ctrl Pts',(5.14148184237209,-6.01340523476452,-28.9223269706478));
#66399=CARTESIAN_POINT('Ctrl Pts',(5.22410749502594,-5.94176557208121,-28.9181456255602));
#66400=CARTESIAN_POINT('Ctrl Pts',(5.38143778013061,-5.79953490778136,-28.9099212535867));
#66401=CARTESIAN_POINT('Ctrl Pts',(5.45630420630964,-5.72915536034199,-28.9058858701553));
#66402=CARTESIAN_POINT('Ctrl Pts',(5.54102043583112,-5.64634932799137,-28.9011515709169));
#66403=CARTESIAN_POINT('Ctrl Pts',(5.5522312829077,-5.63532572092069,-28.9005215816529));
#66404=CARTESIAN_POINT('Ctrl Pts',(5.56919149154765,-5.6185490370615,-28.8995630905561));
#66405=CARTESIAN_POINT('Ctrl Pts',(5.57496500143965,-5.61282035909817,-28.8992358472747));
#66406=CARTESIAN_POINT('Ctrl Pts',(5.58539491217175,-5.60243946868339,-28.8986429212698));
#66407=CARTESIAN_POINT('Ctrl Pts',(5.59005436567966,-5.59779032419086,-28.8983774006648));
#66408=CARTESIAN_POINT('Ctrl Pts',(5.59934070528277,-5.58850137354454,-28.8978469303617));
#66409=CARTESIAN_POINT('Ctrl Pts',(5.6039676395646,-5.58386162349275,-28.8975819836987));
#66410=CARTESIAN_POINT('Ctrl Pts',(5.61693085708274,-5.57083015908879,-28.8968378749946));
#66411=CARTESIAN_POINT('Ctrl Pts',(5.62525407090698,-5.56242550965028,-28.8963580028937));
#66412=CARTESIAN_POINT('Ctrl Pts',(5.65908202407958,-5.52811300128049,-28.8943989185358));
#66413=CARTESIAN_POINT('Ctrl Pts',(5.68442661379711,-5.50204841131561,-28.8929108079608));
#66414=CARTESIAN_POINT('Ctrl Pts',(6.05329442048727,-5.11743245042505,-28.8709374505878));
#66415=CARTESIAN_POINT('Ctrl Pts',(6.36243439207665,-4.72755175129115,-28.8482805888229));
#66416=CARTESIAN_POINT('Ctrl Pts',(6.8578893374167,-3.96530284972688,-28.8064414376334));
#66417=CARTESIAN_POINT('Ctrl Pts',(7.05540865302301,-3.60215403996331,-28.7873925065042));
#66418=CARTESIAN_POINT('Ctrl Pts',(7.33283202367148,-2.98079829469735,-28.7571474678541));
#66419=CARTESIAN_POINT('Ctrl Pts',(7.42949820963403,-2.73096262786812,-28.7455544670296));
#66420=CARTESIAN_POINT('Ctrl Pts',(7.53803121207694,-2.40171575409068,-28.7310511573295));
#66421=CARTESIAN_POINT('Ctrl Pts',(7.56162285030325,-2.32637345231992,-28.72778279189));
#66422=CARTESIAN_POINT('Ctrl Pts',(7.59336449473806,-2.2194145395362,-28.723213100953));
#66423=CARTESIAN_POINT('Ctrl Pts',(7.60245225292419,-2.18808249892832,-28.7218829133489));
#66424=CARTESIAN_POINT('Ctrl Pts',(7.6159663128838,-2.1403890647661,-28.7198707918558));
#66425=CARTESIAN_POINT('Ctrl Pts',(7.62053422254066,-2.12406835932387,-28.719184491423));
#66426=CARTESIAN_POINT('Ctrl Pts',(7.62789144284665,-2.09745247901034,-28.7180689082519));
#66427=CARTESIAN_POINT('Ctrl Pts',(7.6307124300657,-2.08716615924759,-28.7176386491493));
#66428=CARTESIAN_POINT('Ctrl Pts',(7.63610513163827,-2.06734538404361,-28.7168112742887));
#66429=CARTESIAN_POINT('Ctrl Pts',(7.63867981252932,-2.05781176031477,-28.7164140676765));
#66430=CARTESIAN_POINT('Ctrl Pts',(7.6432990665153,-2.040579288221,-28.7156974535657));
#66431=CARTESIAN_POINT('Ctrl Pts',(7.64534987336381,-2.0328821328408,-28.7153778544967));
#66432=CARTESIAN_POINT('Ctrl Pts',(7.64974410009473,-2.01628887682175,-28.7146899215454));
#66433=CARTESIAN_POINT('Ctrl Pts',(7.65208363614419,-2.00739175496107,-28.7143217075091));
#66434=CARTESIAN_POINT('Ctrl Pts',(7.6583365684027,-1.9834424335918,-28.7133322826367));
#66435=CARTESIAN_POINT('Ctrl Pts',(7.66222111400438,-1.96838270816126,-28.7127119590087));
#66436=CARTESIAN_POINT('Ctrl Pts',(7.67907910699989,-1.90222101205837,-28.7099947229937));
#66437=CARTESIAN_POINT('Ctrl Pts',(7.69158605547179,-1.85100102399073,-28.7079121367047));
#66438=CARTESIAN_POINT('Ctrl Pts',(7.93071249994053,-0.827401825605291,
-28.6666979732494));
#66439=CARTESIAN_POINT('Ctrl Pts',(7.97173027098429,0.17889522674085,-28.6347507474529));
#66440=CARTESIAN_POINT('Ctrl Pts',(7.78850526491565,1.40816144164982,-28.5899213022138));
#66441=CARTESIAN_POINT('Ctrl Pts',(7.74125526478127,1.64823677330166,-28.5808126926365));
#66442=CARTESIAN_POINT('Ctrl Pts',(7.67743914785488,1.90824182202314,-28.5702421744213));
#66443=CARTESIAN_POINT('Ctrl Pts',(7.67181285556926,1.93073721569665,-28.5693216882624));
#66444=CARTESIAN_POINT('Ctrl Pts',(7.66175835496983,1.97019983653994,-28.5676967119715));
#66445=CARTESIAN_POINT('Ctrl Pts',(7.65737247737749,1.98717770244354,-28.5669942926999));
#66446=CARTESIAN_POINT('Ctrl Pts',(7.65098246125254,2.01157835777966,-28.5659801469876));
#66447=CARTESIAN_POINT('Ctrl Pts',(7.64902387024681,2.01901311131518,-28.5656705232232));
#66448=CARTESIAN_POINT('Ctrl Pts',(7.6456046246641,2.03191608051712,-28.5651321125693));
#66449=CARTESIAN_POINT('Ctrl Pts',(7.64414893177836,2.03738561482827,-28.5649035505595));
#66450=CARTESIAN_POINT('Ctrl Pts',(7.64133741353184,2.04790401678002,-28.5644633744909));
#66451=CARTESIAN_POINT('Ctrl Pts',(7.6399824505011,2.05295311326221,-28.5642517990459));
#66452=CARTESIAN_POINT('Ctrl Pts',(7.63677681591546,2.06485137480345,-28.5637525648457));
#66453=CARTESIAN_POINT('Ctrl Pts',(7.63492193553477,2.0716993927518,-28.5634647206182));
#66454=CARTESIAN_POINT('Ctrl Pts',(7.62940803942683,2.09194811972763,-28.5626121079663));
#66455=CARTESIAN_POINT('Ctrl Pts',(7.62572294801977,2.10534165501714,-28.5620462103866));
#66456=CARTESIAN_POINT('Ctrl Pts',(7.59234938490404,2.22540128649788,-28.5569565484836));
#66457=CARTESIAN_POINT('Ctrl Pts',(7.56046072658498,2.33143994406994,-28.5523412774118));
#66458=CARTESIAN_POINT('Ctrl Pts',(7.39466084342466,2.84353948750738,-28.5295764708306));
#66459=CARTESIAN_POINT('Ctrl Pts',(7.23020692954665,3.23895386463656,-28.5105789611331));
#66460=CARTESIAN_POINT('Ctrl Pts',(6.76520642749348,4.14278865434088,-28.4659154577401));
#66461=CARTESIAN_POINT('Ctrl Pts',(6.43814927524766,4.63476772279218,-28.4406954132187));
#66462=CARTESIAN_POINT('Ctrl Pts',(6.03497240257439,5.11512300004893,-28.4152896718719));
#66463=CARTESIAN_POINT('Ctrl Pts',(6.01024534967043,5.14415455375549,-28.413749910315));
#66464=CARTESIAN_POINT('Ctrl Pts',(5.97350491776182,5.18666423408005,-28.4114884492553));
#66465=CARTESIAN_POINT('Ctrl Pts',(5.96165387577313,5.20028171816147,-28.4107629668972));
#66466=CARTESIAN_POINT('Ctrl Pts',(5.94059921516042,5.22430808909983,-28.4094810121066));
#66467=CARTESIAN_POINT('Ctrl Pts',(5.93141460311106,5.23473350347544,-28.4089241038223));
#66468=CARTESIAN_POINT('Ctrl Pts',(5.91338088808173,5.25509509943758,-28.4078351131801));
#66469=CARTESIAN_POINT('Ctrl Pts',(5.90453409040301,5.2650332580284,-28.4073029806427));
#66470=CARTESIAN_POINT('Ctrl Pts',(5.88308962672749,5.28900113208535,-28.4060181069144));
#66471=CARTESIAN_POINT('Ctrl Pts',(5.87046677827221,5.30300823494344,-28.4052659389114));
#66472=CARTESIAN_POINT('Ctrl Pts',(5.83149619490156,5.34594277144678,-28.4029563132327));
#66473=CARTESIAN_POINT('Ctrl Pts',(5.80498366035441,5.37472015288788,-28.4014024673781));
#66474=CARTESIAN_POINT('Ctrl Pts',(5.48654949583485,5.71525187515873,-28.3829433440637));
#66475=CARTESIAN_POINT('Ctrl Pts',(5.17005010600584,6.00307768269678,-28.3666699365887));
#66476=CARTESIAN_POINT('Ctrl Pts',(4.4832223527339,6.53287813057973,-28.3343738332653));
#66477=CARTESIAN_POINT('Ctrl Pts',(4.11276170905502,6.77221979058195,-28.3184282208909));
#66478=CARTESIAN_POINT('Ctrl Pts',(3.5412480899392,7.07718461818058,-28.294272434203));
#66479=CARTESIAN_POINT('Ctrl Pts',(3.35440742571648,7.16763038927264,-28.2864305837784));
#66480=CARTESIAN_POINT('Ctrl Pts',(3.08028571539536,7.28725946526883,-28.2747840884502));
#66481=CARTESIAN_POINT('Ctrl Pts',(2.99570878388925,7.32243393490419,-28.2711716650385));
#66482=CARTESIAN_POINT('Ctrl Pts',(2.89669907079718,7.36160832461066,-28.2669044114181));
#66483=CARTESIAN_POINT('Ctrl Pts',(2.8828405733456,7.36704641336545,-28.266306252031));
#66484=CARTESIAN_POINT('Ctrl Pts',(2.86171208015673,7.37526850850629,-28.2653928923228));
#66485=CARTESIAN_POINT('Ctrl Pts',(2.8544531464668,7.37808097247224,-28.2650788437346));
#66486=CARTESIAN_POINT('Ctrl Pts',(2.84127379362208,7.38316493387341,-28.264508179904));
#66487=CARTESIAN_POINT('Ctrl Pts',(2.83535476666007,7.38544003820881,-28.2642517131174));
#66488=CARTESIAN_POINT('Ctrl Pts',(2.82262482354458,7.39031550450002,-28.2636997507483));
#66489=CARTESIAN_POINT('Ctrl Pts',(2.81581303906429,7.39291357173288,-28.2634041600687));
#66490=CARTESIAN_POINT('Ctrl Pts',(2.79751208260711,7.39986473514165,-28.2626093551761));
#66491=CARTESIAN_POINT('Ctrl Pts',(2.78601637343714,7.40420047779482,-28.2621094098849));
#66492=CARTESIAN_POINT('Ctrl Pts',(2.73363453699236,7.42381764439868,-28.2598280389522));
#66493=CARTESIAN_POINT('Ctrl Pts',(2.69263301095811,7.43878710258297,-28.258033174505));
#66494=CARTESIAN_POINT('Ctrl Pts',(2.10201054853958,7.64889767341104,-28.2320248170893));
#66495=CARTESIAN_POINT('Ctrl Pts',(1.53266637623529,7.78298197922414,-28.2048051267462));
#66496=CARTESIAN_POINT('Ctrl Pts',(0.384839772036364,7.92239770949138,-28.1517071741412));
#66497=CARTESIAN_POINT('Ctrl Pts',(-0.190081851935726,7.92947210523636,
-28.1260320686397));
#66498=CARTESIAN_POINT('Ctrl Pts',(-0.824803680846273,7.86814825909378,
-28.0997994097756));
#66499=CARTESIAN_POINT('Ctrl Pts',(-0.888749302406901,7.86118204086309,
-28.0971783753605));
#66500=CARTESIAN_POINT('Ctrl Pts',(-0.967595350660919,7.85161819546899,
-28.0939731060691));
#66501=CARTESIAN_POINT('Ctrl Pts',(-0.982581611011396,7.84975683898128,
-28.0933650644133));
#66502=CARTESIAN_POINT('Ctrl Pts',(-1.00614309531457,7.84676187276624,-28.0924109481948));
#66503=CARTESIAN_POINT('Ctrl Pts',(-1.01472190801242,7.84565709588272,-28.0920639374751));
#66504=CARTESIAN_POINT('Ctrl Pts',(-1.02996385580326,7.84366882479992,-28.0914480881507));
#66505=CARTESIAN_POINT('Ctrl Pts',(-1.03662770219387,7.84279090533138,-28.0911790684092));
#66506=CARTESIAN_POINT('Ctrl Pts',(-1.05200739279171,7.84074478451052,-28.0905587241565));
#66507=CARTESIAN_POINT('Ctrl Pts',(-1.0607224318006,7.83957054012894,-28.0902075969387));
#66508=CARTESIAN_POINT('Ctrl Pts',(-1.08462705246292,7.83630909522304,-28.0892455670826));
#66509=CARTESIAN_POINT('Ctrl Pts',(-1.09981258963091,7.83419225893851,-28.0886356324339));
#66510=CARTESIAN_POINT('Ctrl Pts',(-1.17426406351798,7.82359311934316,-28.0856510866978));
#66511=CARTESIAN_POINT('Ctrl Pts',(-1.23343929830801,7.81448226635349,-28.083297088091));
#66512=CARTESIAN_POINT('Ctrl Pts',(-2.3002793955211,7.63780699895001,-28.0411720287286));
#66513=CARTESIAN_POINT('Ctrl Pts',(-3.26595261456846,7.27739366888304,-28.0097278330247));
#66514=CARTESIAN_POINT('Ctrl Pts',(-4.35604485606599,6.60871683639882,-27.9645133355323));
#66515=CARTESIAN_POINT('Ctrl Pts',(-4.56887744331886,6.4634049318769,-27.9550463736945));
#66516=CARTESIAN_POINT('Ctrl Pts',(-4.80005364149785,6.28843821469499,-27.943595730092));
#66517=CARTESIAN_POINT('Ctrl Pts',(-4.82576012368288,6.26873267185341,-27.9423054077498));
#66518=CARTESIAN_POINT('Ctrl Pts',(-4.85762993385714,6.24399037027071,-27.9406834621312));
#66519=CARTESIAN_POINT('Ctrl Pts',(-4.86390797332854,6.23910118081247,-27.940362871161));
#66520=CARTESIAN_POINT('Ctrl Pts',(-4.87381727004453,6.23136000710423,-27.9398551160989));
#66521=CARTESIAN_POINT('Ctrl Pts',(-4.87745344016932,6.22851428983845,-27.9396684282131));
#66522=CARTESIAN_POINT('Ctrl Pts',(-4.88425445886473,6.22318211045409,-27.9393185547313));
#66523=CARTESIAN_POINT('Ctrl Pts',(-4.88741990716037,6.22069641196122,-27.9391554276967));
#66524=CARTESIAN_POINT('Ctrl Pts',(-4.89448046191163,6.21514332809244,-27.9387909368037));
#66525=CARTESIAN_POINT('Ctrl Pts',(-4.89837455752306,6.21207471581865,-27.9385894773447));
#66526=CARTESIAN_POINT('Ctrl Pts',(-4.90826709324148,6.20426414720608,-27.9380765885646));
#66527=CARTESIAN_POINT('Ctrl Pts',(-4.91426150021762,6.19951718874224,-27.9377647718871));
#66528=CARTESIAN_POINT('Ctrl Pts',(-4.94756648995815,6.17306438010286,-27.9360266285208));
#66529=CARTESIAN_POINT('Ctrl Pts',(-4.97473974314961,6.15118707445163,-27.9345871883522));
#66530=CARTESIAN_POINT('Ctrl Pts',(-5.70134220793611,5.55823251873582,-27.8955449161371));
#66531=CARTESIAN_POINT('Ctrl Pts',(-6.29805806490332,4.87176805505265,-27.8505574879898));
#66532=CARTESIAN_POINT('Ctrl Pts',(-6.89489647186251,3.88666130920369,-27.799231697136));
#66533=CARTESIAN_POINT('Ctrl Pts',(-7.01363742710394,3.66805656879702,-27.7884693232043));
#66534=CARTESIAN_POINT('Ctrl Pts',(-7.16980821494936,3.34512833641964,-27.7735019123845));
#66535=CARTESIAN_POINT('Ctrl Pts',(-7.21565190241228,3.24505815590305,-27.7689861010196));
#66536=CARTESIAN_POINT('Ctrl Pts',(-7.26620104460356,3.12834408820099,-27.7638564983357));
#66537=CARTESIAN_POINT('Ctrl Pts',(-7.27295702103943,3.1126051034531,-27.7631676113766));
#66538=CARTESIAN_POINT('Ctrl Pts',(-7.28313208703254,3.08868687112371,-27.7621250088209));
#66539=CARTESIAN_POINT('Ctrl Pts',(-7.28658860773067,3.08052366447897,-27.7617699277431));
#66540=CARTESIAN_POINT('Ctrl Pts',(-7.29281758615763,3.06574364928079,-27.7611283918311));
#66541=CARTESIAN_POINT('Ctrl Pts',(-7.29559477547872,3.05912885319581,-27.7608417648784));
#66542=CARTESIAN_POINT('Ctrl Pts',(-7.30111932847793,3.04591998922036,-27.7602703887025));
#66543=CARTESIAN_POINT('Ctrl Pts',(-7.30386676632562,3.03932595973891,-27.7599856369564));
#66544=CARTESIAN_POINT('Ctrl Pts',(-7.31154502175472,3.0208271105831,-27.7591881551756));
#66545=CARTESIAN_POINT('Ctrl Pts',(-7.31645570107348,3.00891392591512,-27.7586761563171));
#66546=CARTESIAN_POINT('Ctrl Pts',(-7.33632482683317,2.96037568213916,-27.7565964779631));
#66547=CARTESIAN_POINT('Ctrl Pts',(-7.35103767066584,2.9236503501859,-27.7550376883872));
#66548=CARTESIAN_POINT('Ctrl Pts',(-7.58042512149548,2.33838702433607,-27.7304255659623));
#66549=CARTESIAN_POINT('Ctrl Pts',(-7.7334623478822,1.76763698171038,-27.7098208176552));
#66550=CARTESIAN_POINT('Ctrl Pts',(-7.8816045555661,0.789947111044109,-27.6761198933998));
#66551=CARTESIAN_POINT('Ctrl Pts',(-7.91144566130026,0.390775051233245,
-27.6627266678462));
#66552=CARTESIAN_POINT('Ctrl Pts',(-7.91072732530986,-0.246282008699786,
-27.6398530282432));
#66553=CARTESIAN_POINT('Ctrl Pts',(-7.89977706852779,-0.483493966778849,
-27.6309960325901));
#66554=CARTESIAN_POINT('Ctrl Pts',(-7.8768534656682,-0.73437988567683,-27.6209278043275));
#66555=CARTESIAN_POINT('Ctrl Pts',(-7.87548416948709,-0.748921512842783,
-27.6203417171391));
#66556=CARTESIAN_POINT('Ctrl Pts',(-7.87353437670132,-0.769031049000135,
-27.6195276570814));
#66557=CARTESIAN_POINT('Ctrl Pts',(-7.87298824237683,-0.774602136914305,
-27.6193017565361));
#66558=CARTESIAN_POINT('Ctrl Pts',(-7.87203812900076,-0.784189382962326,
-27.6189123646765));
#66559=CARTESIAN_POINT('Ctrl Pts',(-7.87163698778819,-0.788205826642706,
-27.6187490406282));
#66560=CARTESIAN_POINT('Ctrl Pts',(-7.87084645888596,-0.796060237862896,
-27.6184292734702));
#66561=CARTESIAN_POINT('Ctrl Pts',(-7.87045733739571,-0.799898232136896,
-27.6182728459499));
#66562=CARTESIAN_POINT('Ctrl Pts',(-7.86951318149984,-0.809143269415839,
-27.6178956189523));
#66563=CARTESIAN_POINT('Ctrl Pts',(-7.86895538201957,-0.814550022870949,
-27.6176746589788));
#66564=CARTESIAN_POINT('Ctrl Pts',(-7.86724125600599,-0.83099896938901,
-27.6170013855905));
#66565=CARTESIAN_POINT('Ctrl Pts',(-7.86606726008854,-0.842039265530992,
-27.6165480573806));
#66566=CARTESIAN_POINT('Ctrl Pts',(-7.85436742566049,-0.949904882813457,
-27.612105159079));
#66567=CARTESIAN_POINT('Ctrl Pts',(-7.842077979138,-1.04652684205039,-27.6080166930794));
#66568=CARTESIAN_POINT('Ctrl Pts',(-7.80343947915181,-1.31117314124377,
-27.5965645854855));
#66569=CARTESIAN_POINT('Ctrl Pts',(-7.7734518012122,-1.47860878984053,-27.5890369594463));
#66570=CARTESIAN_POINT('Ctrl Pts',(-7.59911278605078,-2.29873149330377,
-27.5511769429548));
#66571=CARTESIAN_POINT('Ctrl Pts',(-7.37783632946214,-2.93229158722346,
-27.5190703790969));
#66572=CARTESIAN_POINT('Ctrl Pts',(-7.0125323180258,-3.66480966211215,-27.4823330398026));
#66573=CARTESIAN_POINT('Ctrl Pts',(-6.94175369762942,-3.79716972271399,
-27.4756977649427));
#66574=CARTESIAN_POINT('Ctrl Pts',(-6.74349025189868,-4.14383942122636,
-27.4583573334232));
#66575=CARTESIAN_POINT('Ctrl Pts',(-6.60956466793515,-4.35427787607738,
-27.4478757255589));
#66576=CARTESIAN_POINT('Ctrl Pts',(-6.45188981432674,-4.57795056814913,
-27.4367742409427));
#66577=CARTESIAN_POINT('Ctrl Pts',(-6.43777236246147,-4.59778213963121,
-27.4357902368387));
#66578=CARTESIAN_POINT('Ctrl Pts',(-6.41775800878671,-4.62562450582225,
-27.4344090941133));
#66579=CARTESIAN_POINT('Ctrl Pts',(-6.41193726322171,-4.63368972435727,
-27.4340090530539));
#66580=CARTESIAN_POINT('Ctrl Pts',(-6.40178836865561,-4.64769628035908,
-27.4333143811981));
#66581=CARTESIAN_POINT('Ctrl Pts',(-6.39746712647089,-4.65364259453183,
-27.4330194868146));
#66582=CARTESIAN_POINT('Ctrl Pts',(-6.38843793597988,-4.66603101181621,
-27.4324051493163));
#66583=CARTESIAN_POINT('Ctrl Pts',(-6.38372851496776,-4.67247203445605,
-27.4320857631051));
#66584=CARTESIAN_POINT('Ctrl Pts',(-6.37257951266082,-4.68767208142353,
-27.4313320966869));
#66585=CARTESIAN_POINT('Ctrl Pts',(-6.36613159761376,-4.69642498835094,
-27.4308981368789));
#66586=CARTESIAN_POINT('Ctrl Pts',(-6.34483367020274,-4.72521201469312,
-27.4294710107324));
#66587=CARTESIAN_POINT('Ctrl Pts',(-6.32990690333001,-4.74518930031956,
-27.4284807972041));
#66588=CARTESIAN_POINT('Ctrl Pts',(-6.10349662599432,-5.04523679511466,
-27.4136097917576));
#66589=CARTESIAN_POINT('Ctrl Pts',(-5.87369252688523,-5.3110123469392,-27.400480560774));
#66590=CARTESIAN_POINT('Ctrl Pts',(-5.34029090143199,-5.85077487943084,
-27.3731407842722));
#66591=CARTESIAN_POINT('Ctrl Pts',(-5.03159100800513,-6.11828184522846,
-27.3591460778023));
#66592=CARTESIAN_POINT('Ctrl Pts',(-4.53299344402663,-6.48698214240671,
-27.3375890347829));
#66593=CARTESIAN_POINT('Ctrl Pts',(-4.35733761268778,-6.60625246895442,
-27.3301623126459));
#66594=CARTESIAN_POINT('Ctrl Pts',(-3.93533168088193,-6.86863420418269,
-27.3122774620414));
#66595=CARTESIAN_POINT('Ctrl Pts',(-3.68567294192124,-7.00576817613231,
-27.3016174474028));
#66596=CARTESIAN_POINT('Ctrl Pts',(-3.4098730563285,-7.1384271764568,-27.2894194862543));
#66597=CARTESIAN_POINT('Ctrl Pts',(-3.39059593829015,-7.1476035135341,-27.2885654234527));
#66598=CARTESIAN_POINT('Ctrl Pts',(-3.36318136343904,-7.16051759992009,
-27.287348933279));
#66599=CARTESIAN_POINT('Ctrl Pts',(-3.35507424959395,-7.16431978356063,
-27.286988954194));
#66600=CARTESIAN_POINT('Ctrl Pts',(-3.34020106806225,-7.17126442683742,
-27.2863281300824));
#66601=CARTESIAN_POINT('Ctrl Pts',(-3.33343697097425,-7.17441109881701,
-27.2860274413432));
#66602=CARTESIAN_POINT('Ctrl Pts',(-3.31973459647433,-7.1807619104956,-27.2854180171989));
#66603=CARTESIAN_POINT('Ctrl Pts',(-3.31279610693833,-7.18396557339068,
-27.2851092649461));
#66604=CARTESIAN_POINT('Ctrl Pts',(-3.29572717635036,-7.19181671095949,
-27.2843493522136));
#66605=CARTESIAN_POINT('Ctrl Pts',(-3.2855915491317,-7.19645283427168,-27.2838977907962));
#66606=CARTESIAN_POINT('Ctrl Pts',(-3.24869492185973,-7.21323547336111,
-27.2822528795748));
#66607=CARTESIAN_POINT('Ctrl Pts',(-3.22187623944488,-7.22525419370994,
-27.2810551659734));
#66608=CARTESIAN_POINT('Ctrl Pts',(-2.93466166876387,-7.35205155061018,
-27.2682096172954));
#66609=CARTESIAN_POINT('Ctrl Pts',(-2.6683284178278,-7.45284598382061,-27.2561439982762));
#66610=CARTESIAN_POINT('Ctrl Pts',(-2.30749208127807,-7.56757912203419,
-27.2399323268636));
#66611=CARTESIAN_POINT('Ctrl Pts',(-2.21732680717962,-7.59448715663533,
-27.2358913576763));
#66612=CARTESIAN_POINT('Ctrl Pts',(-1.62766077078796,-7.75906470670896,
-27.2095691813035));
#66613=CARTESIAN_POINT('Ctrl Pts',(-1.11611994660299,-7.84899218240182,
-27.1873421409751));
#66614=CARTESIAN_POINT('Ctrl Pts',(-0.378316581510499,-7.90506063052417,
-27.1563756614105));
#66615=CARTESIAN_POINT('Ctrl Pts',(-0.156563979800241,-7.91255946086726,
-27.1471883215448));
#66616=CARTESIAN_POINT('Ctrl Pts',(0.106246507178032,-7.9103929433845,-27.1363586662188));
#66617=CARTESIAN_POINT('Ctrl Pts',(0.147276525232371,-7.90973542359412,
-27.1346694680072));
#66618=CARTESIAN_POINT('Ctrl Pts',(0.413490338914267,-7.90339714032062,
-27.123716062221));
#66619=CARTESIAN_POINT('Ctrl Pts',(0.638352249946675,-7.88841998441327,
-27.1145014200982));
#66620=CARTESIAN_POINT('Ctrl Pts',(0.906774129406987,-7.85898759493737,
-27.1035692865867));
#66621=CARTESIAN_POINT('Ctrl Pts',(0.951235169787291,-7.85373013408749,
-27.101760606931));
#66622=CARTESIAN_POINT('Ctrl Pts',(1.02088757557395,-7.84489367540608,-27.098930367042));
#66623=CARTESIAN_POINT('Ctrl Pts',(1.04611027056555,-7.84157009326246,-27.097906137784));
#66624=CARTESIAN_POINT('Ctrl Pts',(1.09252587231078,-7.83522599912955,-27.0960225079175));
#66625=CARTESIAN_POINT('Ctrl Pts',(1.11372338158077,-7.83224102487008,-27.0951627317109));
#66626=CARTESIAN_POINT('Ctrl Pts',(1.16057433521738,-7.82544955813506,-27.0932634247007));
#66627=CARTESIAN_POINT('Ctrl Pts',(1.18622172353228,-7.82160287939206,-27.0922243468334));
#66628=CARTESIAN_POINT('Ctrl Pts',(1.25955441885894,-7.81023521302536,-27.0892551142748));
#66629=CARTESIAN_POINT('Ctrl Pts',(1.30719054922633,-7.80240375285811,-27.0873284794851));
#66630=CARTESIAN_POINT('Ctrl Pts',(1.6616643946366,-7.74079022980866,-27.0730057420437));
#66631=CARTESIAN_POINT('Ctrl Pts',(1.96516251488765,-7.66936153525198,-27.0608332113915));
#66632=CARTESIAN_POINT('Ctrl Pts',(2.71257581264168,-7.44616323458239,-27.0306660500482));
#66633=CARTESIAN_POINT('Ctrl Pts',(3.14868098258042,-7.27249644154382,-27.0129172598648));
#66634=CARTESIAN_POINT('Ctrl Pts',(3.67215897578549,-7.00807327084671,-26.9899381938502));
#66635=CARTESIAN_POINT('Ctrl Pts',(3.77627004924275,-6.95252659780564,-26.9852762741621));
#66636=CARTESIAN_POINT('Ctrl Pts',(3.89867396298879,-6.88365940884823,-26.9796550380944));
#66637=CARTESIAN_POINT('Ctrl Pts',(3.91820291888899,-6.87256221581759,-26.9787538582107));
#66638=CARTESIAN_POINT('Ctrl Pts',(3.94868570221931,-6.85506842531772,-26.9773401786166));
#66639=CARTESIAN_POINT('Ctrl Pts',(3.95967181975755,-6.84872841986575,-26.9768292598422));
#66640=CARTESIAN_POINT('Ctrl Pts',(3.97915354067233,-6.83742312047786,-26.9759207501858));
#66641=CARTESIAN_POINT('Ctrl Pts',(3.98765522765118,-6.83246833973081,-26.975523435941));
#66642=CARTESIAN_POINT('Ctrl Pts',(4.00724743973372,-6.82100098006514,-26.9746058865539));
#66643=CARTESIAN_POINT('Ctrl Pts',(4.01833136270747,-6.81447719721559,-26.9740853657956));
#66644=CARTESIAN_POINT('Ctrl Pts',(4.049254555275,-6.79617472407491,-26.9726291996323));
#66645=CARTESIAN_POINT('Ctrl Pts',(4.06905822980302,-6.78433625701872,-26.9716920835983));
#66646=CARTESIAN_POINT('Ctrl Pts',(4.18485767054794,-6.71442291928582,-26.9661862466527));
#66647=CARTESIAN_POINT('Ctrl Pts',(4.27965980737125,-6.65439855179556,-26.9615730474371));
#66648=CARTESIAN_POINT('Ctrl Pts',(4.69914266024798,-6.37612842531886,-26.9407341068016));
#66649=CARTESIAN_POINT('Ctrl Pts',(5.00864224736656,-6.13599670245876,-26.9242110735848));
#66650=CARTESIAN_POINT('Ctrl Pts',(5.59883376851369,-5.60356429078551,-26.8909114857512));
#66651=CARTESIAN_POINT('Ctrl Pts',(5.87743511898193,-5.31061650709209,-26.8741964441616));
#66652=CARTESIAN_POINT('Ctrl Pts',(6.16568376860829,-4.9569173531308,-26.8556776178277));
#66653=CARTESIAN_POINT('Ctrl Pts',(6.19849540174365,-4.91582554419991,-26.8535489712848));
#66654=CARTESIAN_POINT('Ctrl Pts',(6.25133283012902,-4.8482841381268,-26.8500862628274));
#66655=CARTESIAN_POINT('Ctrl Pts',(6.27160615106713,-4.82203043688913,-26.8487490234751));
#66656=CARTESIAN_POINT('Ctrl Pts',(6.30760343923941,-4.77480333779046,-26.846358788992));
#66657=CARTESIAN_POINT('Ctrl Pts',(6.32338939578482,-4.75387785034587,-26.8453050262313));
#66658=CARTESIAN_POINT('Ctrl Pts',(6.35671767139323,-4.70923894865541,-26.8430681714588));
#66659=CARTESIAN_POINT('Ctrl Pts',(6.3742319633911,-4.68550508630174,-26.8418854362024));
#66660=CARTESIAN_POINT('Ctrl Pts',(6.42059623210256,-4.6219351147287,-26.8387346512104));
#66661=CARTESIAN_POINT('Ctrl Pts',(6.4492081826016,-4.58192689062148,-26.8367694508401));
#66662=CARTESIAN_POINT('Ctrl Pts',(6.58125215208702,-4.39360177240497,-26.8275984501725));
#66663=CARTESIAN_POINT('Ctrl Pts',(6.67995334818959,-4.24203260762008,-26.8204453044737));
#66664=CARTESIAN_POINT('Ctrl Pts',(7.27298807521295,-3.25924910162444,-26.7752464398691));
#66665=CARTESIAN_POINT('Ctrl Pts',(7.61654083547722,-2.34673663413072,-26.7403197360597));
#66666=CARTESIAN_POINT('Ctrl Pts',(7.82309166324541,-1.19371577026954,-26.6959217822952));
#66667=CARTESIAN_POINT('Ctrl Pts',(7.85132630488589,-0.991155424814066,
-26.6880442400835));
#66668=CARTESIAN_POINT('Ctrl Pts',(7.8736786850477,-0.767793432446921,-26.679093163955));
#66669=CARTESIAN_POINT('Ctrl Pts',(7.87559881607283,-0.747840938898423,
-26.6782912538544));
#66670=CARTESIAN_POINT('Ctrl Pts',(7.8781870613395,-0.719829847060135,-26.6771619599563));
#66671=CARTESIAN_POINT('Ctrl Pts',(7.87891869080055,-0.711777103689533,
-26.6768369000944));
#66672=CARTESIAN_POINT('Ctrl Pts',(7.88023669811501,-0.697019284945764,
-26.6762404169343));
#66673=CARTESIAN_POINT('Ctrl Pts',(7.8808268679918,-0.690314550255293,-26.6759691354154));
#66674=CARTESIAN_POINT('Ctrl Pts',(7.88200438442451,-0.67673882661333,-26.675419247869));
#66675=CARTESIAN_POINT('Ctrl Pts',(7.88259130464137,-0.669867807214394,
-26.6751406259219));
#66676=CARTESIAN_POINT('Ctrl Pts',(7.88399544173782,-0.653172307322653,
-26.6744628486587));
#66677=CARTESIAN_POINT('Ctrl Pts',(7.88480327856925,-0.64334706458688,-26.674063331828));
#66678=CARTESIAN_POINT('Ctrl Pts',(7.88756996709961,-0.608909372998559,
-26.6726606769803));
#66679=CARTESIAN_POINT('Ctrl Pts',(7.8894319462005,-0.584289446869026,-26.6716537153327));
#66680=CARTESIAN_POINT('Ctrl Pts',(7.91552171488661,-0.216425906159299,
-26.6565406554417));
#66681=CARTESIAN_POINT('Ctrl Pts',(7.91744021781857,0.127963835146736,-26.6413724820697));
#66682=CARTESIAN_POINT('Ctrl Pts',(7.87716927232321,0.802702023358791,-26.6107232663353));
#66683=CARTESIAN_POINT('Ctrl Pts',(7.8365521942496,1.13250761392438,-26.5953260484416));
#66684=CARTESIAN_POINT('Ctrl Pts',(7.66339555573778,2.05543543422849,-26.5522455904789));
#66685=CARTESIAN_POINT('Ctrl Pts',(7.4831358621491,2.63729385469906,-26.5252511741441));
#66686=CARTESIAN_POINT('Ctrl Pts',(7.22214464587847,3.22894766974172,-26.4988479644866));
#66687=CARTESIAN_POINT('Ctrl Pts',(7.20595788777413,3.26491153259682,-26.4972464884926));
#66688=CARTESIAN_POINT('Ctrl Pts',(7.18372509887963,3.31333766070552,-26.495094542088));
#66689=CARTESIAN_POINT('Ctrl Pts',(7.1779144222368,3.32590698901554,-26.4945363992654));
#66690=CARTESIAN_POINT('Ctrl Pts',(7.16872151558605,3.34565626158041,-26.4936600624466));
#66691=CARTESIAN_POINT('Ctrl Pts',(7.16536144467328,3.35284645582093,-26.493341143315));
#66692=CARTESIAN_POINT('Ctrl Pts',(7.15887574415441,3.36667088709225,-26.4927282158988));
#66693=CARTESIAN_POINT('Ctrl Pts',(7.15575169932326,3.37330585631193,-26.4924341560302));
#66694=CARTESIAN_POINT('Ctrl Pts',(7.14836924454377,3.38892860021987,-26.4917420209145));
#66695=CARTESIAN_POINT('Ctrl Pts',(7.14410309863472,3.39791271675712,-26.4913442004944));
#66696=CARTESIAN_POINT('Ctrl Pts',(7.13164961859254,3.42401148652931,-26.4901891177879));
#66697=CARTESIAN_POINT('Ctrl Pts',(7.12341762162699,3.44110481332186,-26.4894333279246));
#66698=CARTESIAN_POINT('Ctrl Pts',(7.06490429357745,3.56149501496587,-26.4841151858965));
#66699=CARTESIAN_POINT('Ctrl Pts',(7.0124384777503,3.66371769069153,-26.4796257220311));
#66700=CARTESIAN_POINT('Ctrl Pts',(6.84071711559277,3.98108064032858,-26.4657467119362));
#66701=CARTESIAN_POINT('Ctrl Pts',(6.71364250442224,4.19182874658243,-26.4566217365204));
#66702=CARTESIAN_POINT('Ctrl Pts',(6.21512883228206,4.93761088599112,-26.4242200574751));
#66703=CARTESIAN_POINT('Ctrl Pts',(5.7878964285974,5.43212886115796,-26.4026878403289));
#66704=CARTESIAN_POINT('Ctrl Pts',(5.0860750568429,6.06653091872794,-26.3688364267392));
#66705=CARTESIAN_POINT('Ctrl Pts',(4.85633125435657,6.25195896130502,-26.3579071863796));
#66706=CARTESIAN_POINT('Ctrl Pts',(4.60071082779649,6.43566410238741,-26.3453675531536));
#66707=CARTESIAN_POINT('Ctrl Pts',(4.58459895571675,6.44715169390477,-26.3445758064534));
#66708=CARTESIAN_POINT('Ctrl Pts',(4.56233554730994,6.46289960783889,-26.3434800844333));
#66709=CARTESIAN_POINT('Ctrl Pts',(4.55622071651262,6.46721190074518,-26.3431789608303));
#66710=CARTESIAN_POINT('Ctrl Pts',(4.54574027695638,6.47458066094199,-26.3426625683444));
#66711=CARTESIAN_POINT('Ctrl Pts',(4.54137767391532,6.47764140897164,-26.3424475295959));
#66712=CARTESIAN_POINT('Ctrl Pts',(4.53288394578318,6.4835877048677,-26.3420287030601));
#66713=CARTESIAN_POINT('Ctrl Pts',(4.52875314793903,6.48647371978808,-26.3418249400539));
#66714=CARTESIAN_POINT('Ctrl Pts',(4.52019601326417,6.49244007154966,-26.3414026895453));
#66715=CARTESIAN_POINT('Ctrl Pts',(4.51576927890193,6.49551983297078,-26.3411841721739));
#66716=CARTESIAN_POINT('Ctrl Pts',(4.50196850370122,6.50510036236643,-26.3405026800691));
#66717=CARTESIAN_POINT('Ctrl Pts',(4.49258357488468,6.5115853640684,-26.3400388969211));
#66718=CARTESIAN_POINT('Ctrl Pts',(4.441191713205,6.54693323752778,-26.3374974612629));
#66719=CARTESIAN_POINT('Ctrl Pts',(4.39892121571435,6.57540954089305,-26.3354006894831));
#66720=CARTESIAN_POINT('Ctrl Pts',(4.27515217488365,6.65706122820978,-26.3292494495808));
#66721=CARTESIAN_POINT('Ctrl Pts',(4.1929451703833,6.70914303202189,-26.3251491593789));
#66722=CARTESIAN_POINT('Ctrl Pts',(3.89135074835776,6.8925082739511,-26.3101080508249));
#66723=CARTESIAN_POINT('Ctrl Pts',(3.6665964464434,7.01465215189373,-26.2989080781976));
#66724=CARTESIAN_POINT('Ctrl Pts',(3.13158359812893,7.27265933744835,-26.2727773009049));
#66725=CARTESIAN_POINT('Ctrl Pts',(2.81771386701074,7.39992498569645,-26.2578490749036));
#66726=CARTESIAN_POINT('Ctrl Pts',(2.12813227768752,7.62927300188556,-26.2264755996703));
#66727=CARTESIAN_POINT('Ctrl Pts',(1.7510676111502,7.72454207138937,-26.2101860683649));
#66728=CARTESIAN_POINT('Ctrl Pts',(1.32933640382543,7.79861317309115,-26.1928323147608));
#66729=CARTESIAN_POINT('Ctrl Pts',(1.29011388881635,7.80519755591137,-26.1912260214675));
#66730=CARTESIAN_POINT('Ctrl Pts',(1.23290764069069,7.81435791867093,-26.1888938527981));
#66731=CARTESIAN_POINT('Ctrl Pts',(1.21496222993433,7.8171681390782,-26.1881637770749));
#66732=CARTESIAN_POINT('Ctrl Pts',(1.18321164343683,7.82202825264009,-26.1868746771612));
#66733=CARTESIAN_POINT('Ctrl Pts',(1.16941044226136,7.82410346283992,-26.1863152091249));
#66734=CARTESIAN_POINT('Ctrl Pts',(1.14078252472775,7.82833064522088,-26.1851564699651));
#66735=CARTESIAN_POINT('Ctrl Pts',(1.12595503788139,7.83047704255814,-26.1845572976074));
#66736=CARTESIAN_POINT('Ctrl Pts',(1.08774718134297,7.83589716776827,-26.183015802612));
#66737=CARTESIAN_POINT('Ctrl Pts',(1.06435805506313,7.83910838626123,-26.182074547487));
#66738=CARTESIAN_POINT('Ctrl Pts',(0.971855249926465,7.85138696366532,-26.1783609317616));
#66739=CARTESIAN_POINT('Ctrl Pts',(0.902636607513331,7.85964548971532,-26.1756017233081));
#66740=CARTESIAN_POINT('Ctrl Pts',(0.542230824946419,7.89782177759786,-26.1613335839797));
#66741=CARTESIAN_POINT('Ctrl Pts',(0.249650306886075,7.91247677627833,-26.1500948850438));
#66742=CARTESIAN_POINT('Ctrl Pts',(-0.52348962255973,7.90826661083432,-26.1209754254826));
#66743=CARTESIAN_POINT('Ctrl Pts',(-1.00265614419949,7.86189550403551,-26.1035604943761));
#66744=CARTESIAN_POINT('Ctrl Pts',(-1.81604546017868,7.70757064101029,-26.0728947493653));
#66745=CARTESIAN_POINT('Ctrl Pts',(-2.15278183807161,7.62037843932074,-26.0598358259865));
#66746=CARTESIAN_POINT('Ctrl Pts',(-2.50234178175803,7.50484082366656,-26.0451295875244));
#66747=CARTESIAN_POINT('Ctrl Pts',(-2.52198615509201,7.49826219900052,-26.0442991553091));
#66748=CARTESIAN_POINT('Ctrl Pts',(-2.54940835484547,7.48895893649532,-26.0431341272675));
#66749=CARTESIAN_POINT('Ctrl Pts',(-2.55720820240652,7.48629916054448,-26.0428020942493));
#66750=CARTESIAN_POINT('Ctrl Pts',(-2.57069014778048,7.48167824063792,-26.0422270229247));
#66751=CARTESIAN_POINT('Ctrl Pts',(-2.57637420169948,7.47972279599352,-26.0419842141776));
#66752=CARTESIAN_POINT('Ctrl Pts',(-2.58815299057617,7.47565560353843,-26.0414803069073));
#66753=CARTESIAN_POINT('Ctrl Pts',(-2.59424738058112,7.47354287693327,-26.0412191685736));
#66754=CARTESIAN_POINT('Ctrl Pts',(-2.60630304418866,7.46934704763521,-26.0407017645673));
#66755=CARTESIAN_POINT('Ctrl Pts',(-2.61226442141986,7.46726425596696,-26.0404455119087));
#66756=CARTESIAN_POINT('Ctrl Pts',(-2.63221520770664,7.4602670163953,-26.0395865529036));
#66757=CARTESIAN_POINT('Ctrl Pts',(-2.64619323979615,7.45532039480542,-26.0389824956307));
#66758=CARTESIAN_POINT('Ctrl Pts',(-2.74828808582239,7.41886722072071,-26.0345535847021));
#66759=CARTESIAN_POINT('Ctrl Pts',(-2.83585127866618,7.38583953741168,-26.0306615230953));
#66760=CARTESIAN_POINT('Ctrl Pts',(-3.03824872475572,7.30536778226849,-26.021420159309));
#66761=CARTESIAN_POINT('Ctrl Pts',(-3.1525863116302,7.25675898372272,-26.0160203417105));
#66762=CARTESIAN_POINT('Ctrl Pts',(-3.44219095796604,7.1255019713277,-26.0019662473122));
#66763=CARTESIAN_POINT('Ctrl Pts',(-3.61565148249121,7.03907070061639,-25.9931874837726));
#66764=CARTESIAN_POINT('Ctrl Pts',(-4.32980245154933,6.64985942573321,-25.955984556967));
#66765=CARTESIAN_POINT('Ctrl Pts',(-4.83720612773704,6.29042296392473,-25.9271292698404));
#66766=CARTESIAN_POINT('Ctrl Pts',(-5.45746633986913,5.73117697321142,-25.8912031962797));
#66767=CARTESIAN_POINT('Ctrl Pts',(-5.61150767334488,5.58044082207839,-25.8821914538865));
#66768=CARTESIAN_POINT('Ctrl Pts',(-5.77349428649123,5.4084303341021,-25.8726186590545));
#66769=CARTESIAN_POINT('Ctrl Pts',(-5.78771604756971,5.3932084992706,-25.8717773162712));
#66770=CARTESIAN_POINT('Ctrl Pts',(-5.80874335375377,5.37052359202541,-25.8705320110328));
#66771=CARTESIAN_POINT('Ctrl Pts',(-5.81559494149654,5.36310343734814,-25.8701260224298));
#66772=CARTESIAN_POINT('Ctrl Pts',(-5.82729969633738,5.35037857924892,-25.8694320875033));
#66773=CARTESIAN_POINT('Ctrl Pts',(-5.83215986790318,5.34508035185919,-25.8691438337372));
#66774=CARTESIAN_POINT('Ctrl Pts',(-5.84160090492786,5.33476017001521,-25.8685836740214));
#66775=CARTESIAN_POINT('Ctrl Pts',(-5.84618253361711,5.32973892306135,-25.8683117346831));
#66776=CARTESIAN_POINT('Ctrl Pts',(-5.85712468510994,5.31771576015617,-25.8676620291693));
#66777=CARTESIAN_POINT('Ctrl Pts',(-5.86347913868678,5.31070832128241,-25.8672845285229));
#66778=CARTESIAN_POINT('Ctrl Pts',(-5.88249023109461,5.2896679285158,-25.8661545356114));
#66779=CARTESIAN_POINT('Ctrl Pts',(-5.89510921470534,5.27560095782055,-25.8654036857886));
#66780=CARTESIAN_POINT('Ctrl Pts',(-6.00456458525174,5.15270284385823,-25.858883782831));
#66781=CARTESIAN_POINT('Ctrl Pts',(-6.09843096140382,5.04125828864852,-25.8532443731781));
#66782=CARTESIAN_POINT('Ctrl Pts',(-6.3285556555196,4.75219810265208,-25.8392550774896));
#66783=CARTESIAN_POINT('Ctrl Pts',(-6.46045438448535,4.57127345663248,-25.831081856693));
#66784=CARTESIAN_POINT('Ctrl Pts',(-6.72441131354408,4.17491529904849,-25.8141719020635));
#66785=CARTESIAN_POINT('Ctrl Pts',(-6.8541820150543,3.95825980541488,-25.805507473234));
#66786=CARTESIAN_POINT('Ctrl Pts',(-7.02474077471563,3.63988589744167,-25.7932750387913));
#66787=CARTESIAN_POINT('Ctrl Pts',(-7.07412271750674,3.54295642761574,-25.7896130722676));
#66788=CARTESIAN_POINT('Ctrl Pts',(-7.1453661606639,3.39568394126348,-25.7841100684482));
#66789=CARTESIAN_POINT('Ctrl Pts',(-7.16872818457411,3.34608176999011,-25.7822667750531));
#66790=CARTESIAN_POINT('Ctrl Pts',(-7.21752977791426,3.23960890309111,-25.7783254353854));
#66791=CARTESIAN_POINT('Ctrl Pts',(-7.24281696218559,3.18267251808447,-25.7762270429855));
#66792=CARTESIAN_POINT('Ctrl Pts',(-7.45824729347857,2.68174373697036,-25.7578065782573));
#66793=CARTESIAN_POINT('Ctrl Pts',(-7.60801025880316,2.22154794257502,-25.7412040442325));
#66794=CARTESIAN_POINT('Ctrl Pts',(-7.72180834420059,1.7200524883768,-25.7208888125697));
#66795=CARTESIAN_POINT('Ctrl Pts',(-7.728566774953,1.68942600283106,-25.7196394297873));
#66796=CARTESIAN_POINT('Ctrl Pts',(-7.73685655934682,1.65076902731365,-25.7180505917615));
#66797=CARTESIAN_POINT('Ctrl Pts',(-7.7385579085848,1.6427748768277,-25.7177213866442));
#66798=CARTESIAN_POINT('Ctrl Pts',(-7.74122106205984,1.63016554171537,-25.7172010997431));
#66799=CARTESIAN_POINT('Ctrl Pts',(-7.74219113870885,1.62555208977765,-25.7170105230912));
#66800=CARTESIAN_POINT('Ctrl Pts',(-7.74397271149544,1.6170415854928,-25.7166585604414));
#66801=CARTESIAN_POINT('Ctrl Pts',(-7.74478539181711,1.61314477967048,-25.7164972473494));
#66802=CARTESIAN_POINT('Ctrl Pts',(-7.74657568696197,1.6045277692481,-25.7161401880889));
#66803=CARTESIAN_POINT('Ctrl Pts',(-7.74755192346658,1.59980731004779,-25.715944357752));
#66804=CARTESIAN_POINT('Ctrl Pts',(-7.750351001544,1.58621009696657,-25.7153796030039));
#66805=CARTESIAN_POINT('Ctrl Pts',(-7.75216289150439,1.57733117037897,-25.7150100028913));
#66806=CARTESIAN_POINT('Ctrl Pts',(-7.76425995423043,1.51752678822539,-25.712515147549));
#66807=CARTESIAN_POINT('Ctrl Pts',(-7.77405827833374,1.46650531072789,-25.7103603479874));
#66808=CARTESIAN_POINT('Ctrl Pts',(-7.86769013711608,0.951616359210873,
-25.6883791981394));
#66809=CARTESIAN_POINT('Ctrl Pts',(-7.91039868325133,0.48127547722744,-25.666431686808));
#66810=CARTESIAN_POINT('Ctrl Pts',(-7.91099369507502,0.00998781674201629,
-25.6444276219939));
#66811=CARTESIAN_POINT('',(-7.91099983344385,-0.00162334571786968,-23.6423315082368));
#66812=CARTESIAN_POINT('Ctrl Pts',(-7.91099357096916,0.0100856375418233,
-25.6423315082367));
#66813=CARTESIAN_POINT('Ctrl Pts',(-7.91123506252348,-0.179336015354617,
-25.6347047121618));
#66814=CARTESIAN_POINT('Ctrl Pts',(-7.90466927635026,-0.369027385880647,
-25.6270779160869));
#66815=CARTESIAN_POINT('Ctrl Pts',(-7.8912651987913,-0.558439398990916,
-25.619451120012));
#66816=CARTESIAN_POINT('Ctrl Pts',(-7.87787160594339,-0.747703253436783,
-25.6118302896406));
#66817=CARTESIAN_POINT('Ctrl Pts',(-7.85765039173663,-0.936687819513366,
-25.6042094592693));
#66818=CARTESIAN_POINT('Ctrl Pts',(-7.83062257872658,-1.12484266879304,
-25.5965886288979));
#66819=CARTESIAN_POINT('Ctrl Pts',(-7.80361018813151,-1.31289015451486,
-25.5889721470696));
#66820=CARTESIAN_POINT('Ctrl Pts',(-7.7697989813212,-1.5001085016849,-25.5813556652413));
#66821=CARTESIAN_POINT('Ctrl Pts',(-7.7292619224564,-1.68595110666521,-25.573739183413));
#66822=CARTESIAN_POINT('Ctrl Pts',(-7.68840281620738,-1.87327014152192,
-25.5660621923095));
#66823=CARTESIAN_POINT('Ctrl Pts',(-7.64071055259476,-2.05919110115924,
-25.558385201206));
#66824=CARTESIAN_POINT('Ctrl Pts',(-7.586312756841,-2.24316289096255,-25.5507082101025));
#66825=CARTESIAN_POINT('Ctrl Pts',(-7.53236089607785,-2.4256265413786,-25.5430941524122));
#66826=CARTESIAN_POINT('Ctrl Pts',(-7.47181315887367,-2.60617250643201,
-25.5354800947219));
#66827=CARTESIAN_POINT('Ctrl Pts',(-7.40484452833836,-2.78427701767219,
-25.5278660370316));
#66828=CARTESIAN_POINT('Ctrl Pts',(-7.33786942044865,-2.96239875557548,
-25.5202512428927));
#66829=CARTESIAN_POINT('Ctrl Pts',(-7.26447231295879,-3.13807822384796,
-25.5126364487539));
#66830=CARTESIAN_POINT('Ctrl Pts',(-7.18487676777222,-3.31081060043112,
-25.505021654615));
#66831=CARTESIAN_POINT('Ctrl Pts',(-7.10525830259229,-3.48359271629195,
-25.4974046677526));
#66832=CARTESIAN_POINT('Ctrl Pts',(-7.01943800243577,-3.65342571655013,
-25.4897876808901));
#66833=CARTESIAN_POINT('Ctrl Pts',(-6.92768585912072,-3.81982848271212,
-25.4821706940276));
#66834=CARTESIAN_POINT('Ctrl Pts',(-6.83465340084418,-3.98855324314535,
-25.4744474192694));
#66835=CARTESIAN_POINT('Ctrl Pts',(-6.73552251516363,-4.15375098330507,
-25.4667241445113));
#66836=CARTESIAN_POINT('Ctrl Pts',(-6.63062013894973,-4.31495047166873,
-25.4590008697531));
#66837=CARTESIAN_POINT('Ctrl Pts',(-6.52698990291307,-4.47419511064673,
-25.4513712543425));
#66838=CARTESIAN_POINT('Ctrl Pts',(-6.41772764119896,-4.62953766908532,
-25.4437416389319));
#66839=CARTESIAN_POINT('Ctrl Pts',(-6.30318894457212,-4.78055751236441,
-25.4361120235213));
#66840=CARTESIAN_POINT('Ctrl Pts',(-6.18654117317038,-4.93435818126271,
-25.4283419190893));
#66841=CARTESIAN_POINT('Ctrl Pts',(-6.06442103802342,-5.08367509333987,
-25.4205718146573));
#66842=CARTESIAN_POINT('Ctrl Pts',(-5.93724273672725,-5.22810383267008,
-25.4128017102253));
#66843=CARTESIAN_POINT('Ctrl Pts',(-5.81006443543108,-5.37253257200029,
-25.4050316057933));
#66844=CARTESIAN_POINT('Ctrl Pts',(-5.67782829672822,-5.51207290763824,
-25.3972615013613));
#66845=CARTESIAN_POINT('Ctrl Pts',(-5.54098276437416,-5.64636440596146,
-25.3894913969293));
#66846=CARTESIAN_POINT('Ctrl Pts',(-5.39982971521734,-5.78488302719869,
-25.3814767112178));
#66847=CARTESIAN_POINT('Ctrl Pts',(-5.25330579159423,-5.91827595657096,
-25.3734620255063));
#66848=CARTESIAN_POINT('Ctrl Pts',(-5.10181324297096,-6.04610805674578,
-25.3654473397948));
#66849=CARTESIAN_POINT('Ctrl Pts',(-4.95049292123658,-6.17379482881623,
-25.3574417657154));
#66850=CARTESIAN_POINT('Ctrl Pts',(-4.79421548356322,-6.29593315497069,
-25.3494361916361));
#66851=CARTESIAN_POINT('Ctrl Pts',(-4.63342043398249,-6.41212414742209,
-25.3414306175568));
#66852=CARTESIAN_POINT('Ctrl Pts',(-4.47278092018917,-6.52820274923991,
-25.3334327872064));
#66853=CARTESIAN_POINT('Ctrl Pts',(-4.30763277227287,-6.63834528706121,
-25.3254349568559));
#66854=CARTESIAN_POINT('Ctrl Pts',(-4.13844934218697,-6.74219237653096,
-25.3174371265055));
#66855=CARTESIAN_POINT('Ctrl Pts',(-3.96940089120078,-6.84595661399425,
-25.3094456770396));
#66856=CARTESIAN_POINT('Ctrl Pts',(-3.79632385843553,-6.94343523941891,
-25.3014542275738));
#66857=CARTESIAN_POINT('Ctrl Pts',(-3.61972175177961,-7.03431129817934,
-25.2934627781079));
#66858=CARTESIAN_POINT('Ctrl Pts',(-3.44323063115577,-7.12513024565518,
-25.2854763508883));
#66859=CARTESIAN_POINT('Ctrl Pts',(-3.26321914907742,-7.20935474495823,
-25.2774899236687));
#66860=CARTESIAN_POINT('Ctrl Pts',(-3.08021702368259,-7.28671284510485,
-25.2695034964491));
#66861=CARTESIAN_POINT('Ctrl Pts',(-2.8916148270596,-7.36643819027641,-25.2612726755581));
#66862=CARTESIAN_POINT('Ctrl Pts',(-2.69983635889162,-7.438870040111,-25.2530418546672));
#66863=CARTESIAN_POINT('Ctrl Pts',(-2.50548677509752,-7.50376285738105,
-25.2448110337762));
#66864=CARTESIAN_POINT('Ctrl Pts',(-2.31703471028687,-7.56668650850076,
-25.2368299763348));
#66865=CARTESIAN_POINT('Ctrl Pts',(-2.12616562556187,-7.62252186081628,
-25.2288489188933));
#66866=CARTESIAN_POINT('Ctrl Pts',(-1.9334495992081,-7.67109468376724,-25.2208678614518));
#66867=CARTESIAN_POINT('Ctrl Pts',(-1.74074863348217,-7.71966371078476,
-25.2128874277246));
#66868=CARTESIAN_POINT('Ctrl Pts',(-1.54620133807989,-7.76097125783855,
-25.2049069939974));
#66869=CARTESIAN_POINT('Ctrl Pts',(-1.35039091616937,-7.79489354472062,
-25.1969265602702));
#66870=CARTESIAN_POINT('Ctrl Pts',(-1.15456573750393,-7.82881838806966,
-25.1889455251179));
#66871=CARTESIAN_POINT('Ctrl Pts',(-0.957477572220607,-7.85535680512861,
-25.1809644899656));
#66872=CARTESIAN_POINT('Ctrl Pts',(-0.759718111332479,-7.87443644912532,
-25.1729834548133));
#66873=CARTESIAN_POINT('Ctrl Pts',(-0.561913387939105,-7.89352046000533,
-25.1650005929891));
#66874=CARTESIAN_POINT('Ctrl Pts',(-0.363437395565307,-7.90514226350875,
-25.1570177311649));
#66875=CARTESIAN_POINT('Ctrl Pts',(-0.164885604876271,-7.9092814931133,
-25.1490348693408));
#66876=CARTESIAN_POINT('Ctrl Pts',(0.0338135219682023,-7.91342379424984,
-25.1410460838018));
#66877=CARTESIAN_POINT('Ctrl Pts',(0.232588224897808,-7.910072423161,-25.1330572982629));
#66878=CARTESIAN_POINT('Ctrl Pts',(0.430843350893744,-7.89925914291908,
-25.125068512724));
#66879=CARTESIAN_POINT('Ctrl Pts',(0.629185912007195,-7.8884410937693,-25.117076203945));
#66880=CARTESIAN_POINT('Ctrl Pts',(0.827008106243506,-7.87015460036465,
-25.109083895166));
#66881=CARTESIAN_POINT('Ctrl Pts',(1.0237206423262,-7.84448322367224,-25.101091586387));
#66882=CARTESIAN_POINT('Ctrl Pts',(1.22061724188688,-7.81878782633034,-25.0930917992226));
#66883=CARTESIAN_POINT('Ctrl Pts',(1.41640177977645,-7.7856937973946,-25.0850920120583));
#66884=CARTESIAN_POINT('Ctrl Pts',(1.61049490985842,-7.74533583166799,-25.0770922248939));
#66885=CARTESIAN_POINT('Ctrl Pts',(1.65197072153519,-7.73671172742779,-25.0753827482847));
#66886=CARTESIAN_POINT('Ctrl Pts',(1.69336934984051,-7.72775610821929,-25.0736732716755));
#66887=CARTESIAN_POINT('Ctrl Pts',(1.7346852321027,-7.71847058331667,-25.0719637950663));
#66888=CARTESIAN_POINT('Ctrl Pts',(1.93111367640522,-7.67432433467604,-25.0638364161376));
#66889=CARTESIAN_POINT('Ctrl Pts',(2.12601574851104,-7.62263954703202,-25.0557090372089));
#66890=CARTESIAN_POINT('Ctrl Pts',(2.31879220931818,-7.56353909820035,-25.0475816582802));
#66891=CARTESIAN_POINT('Ctrl Pts',(2.51140495350226,-7.50448884079694,-25.0394611815792));
#66892=CARTESIAN_POINT('Ctrl Pts',(2.70189538193847,-7.43803557075885,-25.0313407048783));
#66893=CARTESIAN_POINT('Ctrl Pts',(2.88967625408622,-7.36435279889348,-25.0232202281773));
#66894=CARTESIAN_POINT('Ctrl Pts',(3.0773212620885,-7.29072333835168,-25.0151056268438));
#66895=CARTESIAN_POINT('Ctrl Pts',(3.26226032689824,-7.20987492145338,-25.0069910255103));
#66896=CARTESIAN_POINT('Ctrl Pts',(3.44392259038269,-7.12203048234503,-24.9988764241768));
#66897=CARTESIAN_POINT('Ctrl Pts',(3.62545615904357,-7.03424827478866,-24.9907675714625));
#66898=CARTESIAN_POINT('Ctrl Pts',(3.80371727134879,-6.93948007122018,-24.9826587187483));
#66899=CARTESIAN_POINT('Ctrl Pts',(3.97815589200227,-6.83799654130708,-24.9745498660341));
#66900=CARTESIAN_POINT('Ctrl Pts',(4.15251980586028,-6.73655647372638,-24.9664444860967));
#66901=CARTESIAN_POINT('Ctrl Pts',(4.32306421720474,-6.6284069742295,-24.9583391061593));
#66902=CARTESIAN_POINT('Ctrl Pts',(4.48926375227958,-6.5138645950364,-24.9502337262218));
#66903=CARTESIAN_POINT('Ctrl Pts',(4.65541146152757,-6.39935793347336,-24.9421308737766));
#66904=CARTESIAN_POINT('Ctrl Pts',(4.81721673446147,-6.27846254868579,-24.9340280213313));
#66905=CARTESIAN_POINT('Ctrl Pts',(4.9741827877033,-6.15153855507029,-24.925925168886));
#66906=CARTESIAN_POINT('Ctrl Pts',(5.05635222416706,-6.08509569807211,-24.9216834439689));
#66907=CARTESIAN_POINT('Ctrl Pts',(5.13719602657742,-6.01700149142288,-24.9174417190518));
#66908=CARTESIAN_POINT('Ctrl Pts',(5.21664637008845,-5.94731213654059,-24.9131999941347));
#66909=CARTESIAN_POINT('Ctrl Pts',(5.3719032232417,-5.81112959208374,-24.9049110826779));
#66910=CARTESIAN_POINT('Ctrl Pts',(5.52177023652025,-5.66891189016605,-24.8966221712211));
#66911=CARTESIAN_POINT('Ctrl Pts',(5.66579482943032,-5.52111310795212,-24.8883332597643));
#66912=CARTESIAN_POINT('Ctrl Pts',(5.80990222901842,-5.37322934909687,-24.880039582613));
#66913=CARTESIAN_POINT('Ctrl Pts',(5.94816029916871,-5.21975831446292,-24.8717459054616));
#66914=CARTESIAN_POINT('Ctrl Pts',(6.08015506622352,-5.06118912615173,-24.8634522283103));
#66915=CARTESIAN_POINT('Ctrl Pts',(6.21223367357894,-4.90251921802632,-24.8551532831896));
#66916=CARTESIAN_POINT('Ctrl Pts',(6.33804084964781,-4.73874491702806,-24.8468543380689));
#66917=CARTESIAN_POINT('Ctrl Pts',(6.45720394705447,-4.57038709368738,-24.8385553929482));
#66918=CARTESIAN_POINT('Ctrl Pts',(6.57650529941532,-4.4018339388753,-24.830246819257));
#66919=CARTESIAN_POINT('Ctrl Pts',(6.68914699549787,-4.22868687099223,-24.8219382455659));
#66920=CARTESIAN_POINT('Ctrl Pts',(6.79479970344629,-4.05149577193981,-24.8136296718748));
#66921=CARTESIAN_POINT('Ctrl Pts',(6.90051743719965,-3.87419561752983,-24.8053159845268));
#66922=CARTESIAN_POINT('Ctrl Pts',(6.9992374524674,-3.69284671806907,-24.7970022971788));
#66923=CARTESIAN_POINT('Ctrl Pts',(7.09067652112688,-3.50802329991408,-24.7886886098308));
#66924=CARTESIAN_POINT('Ctrl Pts',(7.18221510797048,-3.32299872823435,-24.7803658742382));
#66925=CARTESIAN_POINT('Ctrl Pts',(7.26645678622909,-3.13449234482788,-24.7720431386455));
#66926=CARTESIAN_POINT('Ctrl Pts',(7.34316593170256,-2.943099573491,-24.7637204030528));
#66927=CARTESIAN_POINT('Ctrl Pts',(7.37168955818027,-2.87193184131968,-24.7606256664363));
#66928=CARTESIAN_POINT('Ctrl Pts',(7.39917218120556,-2.80036519070873,-24.7575309298198));
#66929=CARTESIAN_POINT('Ctrl Pts',(7.42560343635673,-2.72843079552462,-24.7544361932033));
#66930=CARTESIAN_POINT('Ctrl Pts',(7.49988337719257,-2.52627306265205,-24.7457390332893));
#66931=CARTESIAN_POINT('Ctrl Pts',(7.56592206394861,-2.32103079898211,-24.7370418733753));
#66932=CARTESIAN_POINT('Ctrl Pts',(7.62349089207904,-2.11336405249732,-24.7283447134613));
#66933=CARTESIAN_POINT('Ctrl Pts',(7.68100930114178,-1.90587918158805,-24.7196551705635));
#66934=CARTESIAN_POINT('Ctrl Pts',(7.73007260230958,-1.69597428817814,-24.7109656276657));
#66935=CARTESIAN_POINT('Ctrl Pts',(7.77050205128734,-1.48432438197962,-24.7022760847679));
#66936=CARTESIAN_POINT('Ctrl Pts',(7.81183457204725,-1.26794685611739,-24.6933924437265));
#66937=CARTESIAN_POINT('Ctrl Pts',(7.84414294455433,-1.04974567349245,-24.6845088026852));
#66938=CARTESIAN_POINT('Ctrl Pts',(7.86729069163524,-0.830456605313957,
-24.6756251616438));
#66939=CARTESIAN_POINT('Ctrl Pts',(7.88986629398568,-0.6165877227098,-24.6669610982742));
#66940=CARTESIAN_POINT('Ctrl Pts',(7.90372867389307,-0.401684340823563,
-24.6582970349045));
#66941=CARTESIAN_POINT('Ctrl Pts',(7.9088027830959,-0.18643910023009,-24.6496329715349));
#66942=CARTESIAN_POINT('Ctrl Pts',(7.91406978581251,0.0369887413136039,
-24.6406395416577));
#66943=CARTESIAN_POINT('Ctrl Pts',(7.9098672206449,0.260784714269032,-24.6316461117805));
#66944=CARTESIAN_POINT('Ctrl Pts',(7.89617018668819,0.484166689123351,-24.6226526819033));
#66945=CARTESIAN_POINT('Ctrl Pts',(7.88247315273147,0.707548663977633,-24.6136592520261));
#66946=CARTESIAN_POINT('Ctrl Pts',(7.85928160087558,0.930516360671599,-24.6046658221489));
#66947=CARTESIAN_POINT('Ctrl Pts',(7.82663160079334,1.15228416003304,-24.5956723922717));
#66948=CARTESIAN_POINT('Ctrl Pts',(7.79827044298945,1.34492096057421,-24.587860322339));
#66949=CARTESIAN_POINT('Ctrl Pts',(7.76278420421041,1.5365693507524,-24.5800482524063));
#66950=CARTESIAN_POINT('Ctrl Pts',(7.72026924495075,1.72666261483463,-24.5722361824735));
#66951=CARTESIAN_POINT('Ctrl Pts',(7.67775731769792,1.91674232218098,-24.5644246696682));
#66952=CARTESIAN_POINT('Ctrl Pts',(7.62821774528126,2.10526678082068,-24.5566131568629));
#66953=CARTESIAN_POINT('Ctrl Pts',(7.57179784568462,2.29168025345722,-24.5488016440576));
#66954=CARTESIAN_POINT('Ctrl Pts',(7.5153720206018,2.47811330412321,-24.5409893108501));
#66955=CARTESIAN_POINT('Ctrl Pts',(7.45206453178849,2.66243459048561,-24.5331769776426));
#66956=CARTESIAN_POINT('Ctrl Pts',(7.38207237361253,2.8441041596163,-24.525364644435));
#66957=CARTESIAN_POINT('Ctrl Pts',(7.31203062988117,3.02590243154338,-24.5175467766235));
#66958=CARTESIAN_POINT('Ctrl Pts',(7.235294882239,3.20504490420628,-24.5097289088119));
#66959=CARTESIAN_POINT('Ctrl Pts',(7.15211037938772,3.3810114050465,-24.5019110410003));
#66960=CARTESIAN_POINT('Ctrl Pts',(7.06889509473996,3.55704302096018,-24.4940902802459));
#66961=CARTESIAN_POINT('Ctrl Pts',(6.97922645886915,3.72989600934564,-24.4862695194914));
#66962=CARTESIAN_POINT('Ctrl Pts',(6.88339545620493,3.89907527415121,-24.478448758737));
#66963=CARTESIAN_POINT('Ctrl Pts',(6.7874583021662,4.06844193772125,-24.470619334977));
#66964=CARTESIAN_POINT('Ctrl Pts',(6.68534532667827,4.23412644693136,-24.4627899112171));
#66965=CARTESIAN_POINT('Ctrl Pts',(6.57739117288376,4.3956622207434,-24.4549604874571));
#66966=CARTESIAN_POINT('Ctrl Pts',(6.49442307589354,4.51981043809258,-24.4489431887515));
#66967=CARTESIAN_POINT('Ctrl Pts',(6.40800567594872,4.64150870828585,-24.4429258900459));
#66968=CARTESIAN_POINT('Ctrl Pts',(6.31830676552403,4.76055885550565,-24.4369085913403));
#66969=CARTESIAN_POINT('Ctrl Pts',(6.19730100926472,4.92116006045795,-24.4287911261775));
#66970=CARTESIAN_POINT('Ctrl Pts',(6.07008248282852,5.07725910620167,-24.4206736610147));
#66971=CARTESIAN_POINT('Ctrl Pts',(5.93701302250922,5.22836469372174,-24.4125561958519));
#66972=CARTESIAN_POINT('Ctrl Pts',(5.80404066699095,5.37936001493444,-24.4044446542485));
#66973=CARTESIAN_POINT('Ctrl Pts',(5.66522610178564,5.52536890359633,-24.396333112645));
#66974=CARTESIAN_POINT('Ctrl Pts',(5.52097203150046,5.66593229992996,-24.3882215710415));
#66975=CARTESIAN_POINT('Ctrl Pts',(5.37680273946463,5.80641308702672,-24.3801147965985));
#66976=CARTESIAN_POINT('Ctrl Pts',(5.2272005460241,5.94145454023021,-24.3720080221554));
#66977=CARTESIAN_POINT('Ctrl Pts',(5.07260607365836,6.07063329657494,-24.3639012477124));
#66978=CARTESIAN_POINT('Ctrl Pts',(4.91808052315557,6.19975446198252,-24.3557980874607));
#66979=CARTESIAN_POINT('Ctrl Pts',(4.75856737795069,6.32301793776689,-24.3476949272089));
#66980=CARTESIAN_POINT('Ctrl Pts',(4.59454193338072,6.44003924075049,-24.3395917669572));
#66981=CARTESIAN_POINT('Ctrl Pts',(4.43056636294747,6.55702496183715,-24.33149107058));
#66982=CARTESIAN_POINT('Ctrl Pts',(4.26208149043596,6.66777210977236,-24.3233903742029));
#66983=CARTESIAN_POINT('Ctrl Pts',(4.08959377008074,6.77193796455024,-24.3152896778257));
#66984=CARTESIAN_POINT('Ctrl Pts',(3.91578235993709,6.87690319958538,-24.3071268158112));
#66985=CARTESIAN_POINT('Ctrl Pts',(3.73790667150301,6.97518550845407,-24.2989639537967));
#66986=CARTESIAN_POINT('Ctrl Pts',(3.55651331511241,7.06647960723217,-24.2908010917821));
#66987=CARTESIAN_POINT('Ctrl Pts',(3.37650210555571,7.15707808048081,-24.2827004276017));
#66988=CARTESIAN_POINT('Ctrl Pts',(3.1930269502046,7.24079434660195,-24.2745997634213));
#66989=CARTESIAN_POINT('Ctrl Pts',(3.00664561236294,7.31737679511303,-24.2664990992409));
#66990=CARTESIAN_POINT('Ctrl Pts',(2.82023911686269,7.39396958068423,-24.2583973416369));
#66991=CARTESIAN_POINT('Ctrl Pts',(2.63092595321616,7.46342650635095,-24.250295584033));
#66992=CARTESIAN_POINT('Ctrl Pts',(2.43928317682044,7.52554440444549,-24.242193826429));
#66993=CARTESIAN_POINT('Ctrl Pts',(2.24758980797307,7.58767870126277,-24.2340899300135));
#66994=CARTESIAN_POINT('Ctrl Pts',(2.05356590493151,7.6424700078357,-24.225986033598));
#66995=CARTESIAN_POINT('Ctrl Pts',(1.85780349400208,7.68976509248974,-24.2178821371825));
#66996=CARTESIAN_POINT('Ctrl Pts',(1.6595159340693,7.73767023877568,-24.2096737082071));
#66997=CARTESIAN_POINT('Ctrl Pts',(1.45944503542726,7.77788435778688,-24.2014652792316));
#66998=CARTESIAN_POINT('Ctrl Pts',(1.25821628523376,7.8103017086136,-24.1932568502562));
#66999=CARTESIAN_POINT('Ctrl Pts',(1.05929224513906,7.84234777752482,-24.1851424339362));
#67000=CARTESIAN_POINT('Ctrl Pts',(0.859237060204384,7.86677472953465,-24.1770280176161));
#67001=CARTESIAN_POINT('Ctrl Pts',(0.658660039973107,7.88353270759643,-24.1689136012961));
#67002=CARTESIAN_POINT('Ctrl Pts',(0.454597227748876,7.9005819195477,-24.160658165993));
#67003=CARTESIAN_POINT('Ctrl Pts',(0.249994624954955,7.90969313899543,-24.1524027306898));
#67004=CARTESIAN_POINT('Ctrl Pts',(0.0454940565222883,7.91086918681008,
-24.1441472953866));
#67005=CARTESIAN_POINT('Ctrl Pts',(-0.159006511910379,7.91204523462473,
-24.1358918600835));
#67006=CARTESIAN_POINT('Ctrl Pts',(-0.363404700568143,7.90528615647321,
-24.1276364247803));
#67007=CARTESIAN_POINT('Ctrl Pts',(-0.567063678828794,7.89065014964883,
-24.1193809894772));
#67008=CARTESIAN_POINT('Ctrl Pts',(-0.762575431271365,7.87659964538218,
-24.1114558067178));
#67009=CARTESIAN_POINT('Ctrl Pts',(-0.95782422640749,7.85525971528149,-24.1035306239584));
#67010=CARTESIAN_POINT('Ctrl Pts',(-1.15222679269407,7.82664004654602,-24.0956054411991));
#67011=CARTESIAN_POINT('Ctrl Pts',(-1.34642164499087,7.79805095716809,-24.0876887262875));
#67012=CARTESIAN_POINT('Ctrl Pts',(-1.53977173385837,7.76219767094114,-24.0797720113759));
#67013=CARTESIAN_POINT('Ctrl Pts',(-1.73169585682538,7.71914182143675,-24.0718552964643));
#67014=CARTESIAN_POINT('Ctrl Pts',(-1.92344654674741,7.67612487953276,-24.0639457355255));
#67015=CARTESIAN_POINT('Ctrl Pts',(-2.11377350589463,7.62591841449473,-24.0560361745868));
#67016=CARTESIAN_POINT('Ctrl Pts',(-2.30210242628272,7.56863563787445,-24.0481266136481));
#67017=CARTESIAN_POINT('Ctrl Pts',(-2.49026575105275,7.51140322939083,-24.0402240075023));
#67018=CARTESIAN_POINT('Ctrl Pts',(-2.67643421347492,7.44710701282308,-24.0323214013564));
#67019=CARTESIAN_POINT('Ctrl Pts',(-2.86004540557255,7.37591087785525,-24.0244187952106));
#67020=CARTESIAN_POINT('Ctrl Pts',(-3.04356234462664,7.30475128996459,-24.0165202457057));
#67021=CARTESIAN_POINT('Ctrl Pts',(-3.22452431024445,7.22669896282485,-24.0086216962008));
#67022=CARTESIAN_POINT('Ctrl Pts',(-3.40238511850491,7.14196727137393,-24.0007231466959));
#67023=CARTESIAN_POINT('Ctrl Pts',(-3.5801856072484,7.05726431573473,-23.9928272758963));
#67024=CARTESIAN_POINT('Ctrl Pts',(-3.75488672539468,6.96588665561444,-23.9849314050967));
#67025=CARTESIAN_POINT('Ctrl Pts',(-3.92596303008034,6.86809546282245,-23.9770355342971));
#67026=CARTESIAN_POINT('Ctrl Pts',(-4.04453935060178,6.80031448145287,-23.97156275238));
#67027=CARTESIAN_POINT('Ctrl Pts',(-4.1613746770671,6.72945334943637,-23.9660899704629));
#67028=CARTESIAN_POINT('Ctrl Pts',(-4.27630092869887,6.65561202048385,-23.9606171885458));
#67029=CARTESIAN_POINT('Ctrl Pts',(-4.45520620594544,6.54066349270248,-23.9520977288724));
#67030=CARTESIAN_POINT('Ctrl Pts',(-4.62930592752166,6.41860602717389,-23.943578269199));
#67031=CARTESIAN_POINT('Ctrl Pts',(-4.79807192893164,6.28986699102598,-23.9350588095256));
#67032=CARTESIAN_POINT('Ctrl Pts',(-4.96714186508217,6.16089610565948,-23.926524006953));
#67033=CARTESIAN_POINT('Ctrl Pts',(-5.13085868478793,6.02521975164363,-23.9179892043803));
#67034=CARTESIAN_POINT('Ctrl Pts',(-5.28872864360726,5.88330437205896,-23.9094544018076));
#67035=CARTESIAN_POINT('Ctrl Pts',(-5.45458844269649,5.73420661766908,-23.9004876506248));
#67036=CARTESIAN_POINT('Ctrl Pts',(-5.61399403640044,5.5782222663753,-23.891520899442));
#67037=CARTESIAN_POINT('Ctrl Pts',(-5.7664199192343,5.41593226647619,-23.8825541482592));
#67038=CARTESIAN_POINT('Ctrl Pts',(-5.9121089970688,5.26081503843405,-23.8739837028289));
#67039=CARTESIAN_POINT('Ctrl Pts',(-6.05142189436461,5.0999377081641,-23.8654132573986));
#67040=CARTESIAN_POINT('Ctrl Pts',(-6.18394305456161,4.93383920471059,-23.8568428119683));
#67041=CARTESIAN_POINT('Ctrl Pts',(-6.31662981763305,4.76753313901139,-23.8482616566228));
#67042=CARTESIAN_POINT('Ctrl Pts',(-6.44250773683942,4.59599306323536,-23.8396805012772));
#67043=CARTESIAN_POINT('Ctrl Pts',(-6.56120404463471,4.41978760628485,-23.8310993459316));
#67044=CARTESIAN_POINT('Ctrl Pts',(-6.6800978412287,4.24328897590152,-23.8225039131237));
#67045=CARTESIAN_POINT('Ctrl Pts',(-6.79178599864974,4.06210965241128,-23.8139084803158));
#67046=CARTESIAN_POINT('Ctrl Pts',(-6.89594010202043,3.87684551012115,-23.8053130475079));
#67047=CARTESIAN_POINT('Ctrl Pts',(-6.90991410357315,3.85198925071088,-23.8041598275433));
#67048=CARTESIAN_POINT('Ctrl Pts',(-6.92375255642822,3.82705949472394,-23.8030066075787));
#67049=CARTESIAN_POINT('Ctrl Pts',(-6.93745473218874,3.80205771113906,-23.8018533876141));
#67050=CARTESIAN_POINT('Ctrl Pts',(-7.03379924037634,3.62626194078864,-23.7937447184316));
#67051=CARTESIAN_POINT('Ctrl Pts',(-7.12357291241415,3.44659227278591,-23.785636049249));
#67052=CARTESIAN_POINT('Ctrl Pts',(-7.20645898554778,3.26356704996506,-23.7775273800665));
#67053=CARTESIAN_POINT('Ctrl Pts',(-7.28924071827079,3.08077222685048,-23.7694289184115));
#67054=CARTESIAN_POINT('Ctrl Pts',(-7.3651520015754,2.89463055742132,-23.7613304567565));
#67055=CARTESIAN_POINT('Ctrl Pts',(-7.43392104025364,2.70568641332919,-23.7532319951014));
#67056=CARTESIAN_POINT('Ctrl Pts',(-7.50261247886534,2.51695547678565,-23.7451426718781));
#67057=CARTESIAN_POINT('Ctrl Pts',(-7.5641776284856,2.32542866839131,-23.7370533486548));
#67058=CARTESIAN_POINT('Ctrl Pts',(-7.61839182259162,2.1316723569698,-23.7289640254315));
#67059=CARTESIAN_POINT('Ctrl Pts',(-7.67253510355213,1.93816948230466,-23.7208852831891));
#67060=CARTESIAN_POINT('Ctrl Pts',(-7.71934652298509,1.742443229068,-23.7128065409468));
#67061=CARTESIAN_POINT('Ctrl Pts',(-7.75865048988188,1.54507720708569,-23.7047277987044));
#67062=CARTESIAN_POINT('Ctrl Pts',(-7.79792430116788,1.34786261238697,-23.6966552548035));
#67063=CARTESIAN_POINT('Ctrl Pts',(-7.8297020772218,1.14901106940106,-23.6885827109026));
#67064=CARTESIAN_POINT('Ctrl Pts',(-7.85385845500804,0.949119786275016,
-23.6805101670016));
#67065=CARTESIAN_POINT('Ctrl Pts',(-7.87799513818082,0.749391473838983,
-23.6724442046186));
#67066=CARTESIAN_POINT('Ctrl Pts',(-7.89452277826737,0.548625429427025,
-23.6643782422355));
#67067=CARTESIAN_POINT('Ctrl Pts',(-7.90336732057149,0.347427684738319,
-23.6563122798524));
#67068=CARTESIAN_POINT('Ctrl Pts',(-7.90847741655782,0.231182010034144,
-23.6516520226472));
#67069=CARTESIAN_POINT('Ctrl Pts',(-7.91102372207927,0.114792392926225,
-23.646991765442));
#67070=CARTESIAN_POINT('Ctrl Pts',(-7.91099983344385,-0.00162334571786968,
-23.6423315082368));
#67071=CARTESIAN_POINT('',(-7.91099783789749,0.00584882734057925,-19.6423315082367));
#67072=CARTESIAN_POINT('Ctrl Pts',(-7.91099989428398,-0.00129330542618517,
-23.6332372668359));
#67073=CARTESIAN_POINT('Ctrl Pts',(-7.91084051574585,-0.976193412347082,
-23.5954971353885));
#67074=CARTESIAN_POINT('Ctrl Pts',(-7.73051367551189,-1.94252686240568,
-23.5651777674233));
#67075=CARTESIAN_POINT('Ctrl Pts',(-7.31965879842538,-3.00561085447395,
-23.5251964480447));
#67076=CARTESIAN_POINT('Ctrl Pts',(-7.25543627084996,-3.15748978254176,
-23.5192774622992));
#67077=CARTESIAN_POINT('Ctrl Pts',(-7.13185426759604,-3.42602882992272,
-23.5082611349174));
#67078=CARTESIAN_POINT('Ctrl Pts',(-7.07425570650893,-3.54343361337518,
-23.5032486046814));
#67079=CARTESIAN_POINT('Ctrl Pts',(-7.00349681319634,-3.67905522057872,
-23.4971674565624));
#67080=CARTESIAN_POINT('Ctrl Pts',(-6.99313365172071,-3.69871553899137,
-23.4962786298811));
#67081=CARTESIAN_POINT('Ctrl Pts',(-6.97941705219739,-3.72447406193392,
-23.4951042094122));
#67082=CARTESIAN_POINT('Ctrl Pts',(-6.97613812619126,-3.73061205034906,
-23.4948236164228));
#67083=CARTESIAN_POINT('Ctrl Pts',(-6.97077561820131,-3.74061861032806,
-23.4943649532074));
#67084=CARTESIAN_POINT('Ctrl Pts',(-6.96869689823961,-3.74448979803012,
-23.4941872136849));
#67085=CARTESIAN_POINT('Ctrl Pts',(-6.96468708761452,-3.75194234055934,
-23.4938444624876));
#67086=CARTESIAN_POINT('Ctrl Pts',(-6.96275645652134,-3.75552394244948,
-23.4936794823449));
#67087=CARTESIAN_POINT('Ctrl Pts',(-6.95832008244876,-3.76373888265737,
-23.4933004798326));
#67088=CARTESIAN_POINT('Ctrl Pts',(-6.95581249244202,-3.76837117548673,
-23.4930863291968));
#67089=CARTESIAN_POINT('Ctrl Pts',(-6.94775177045063,-3.78322635863038,
-23.4923981761767));
#67090=CARTESIAN_POINT('Ctrl Pts',(-6.94218074931008,-3.79343944006282,
-23.4919229399362));
#67091=CARTESIAN_POINT('Ctrl Pts',(-6.89157876012235,-3.88572080741014,
-23.4876099472335));
#67092=CARTESIAN_POINT('Ctrl Pts',(-6.84511865525178,-3.96699296793113,
-23.4836757812747));
#67093=CARTESIAN_POINT('Ctrl Pts',(-6.57541061302697,-4.41994032987668,
-23.4610721512));
#67094=CARTESIAN_POINT('Ctrl Pts',(-6.32335693955479,-4.77357371037152,
-23.4408567516678));
#67095=CARTESIAN_POINT('Ctrl Pts',(-5.7850238442565,-5.41091796863225,-23.4019014654934));
#67096=CARTESIAN_POINT('Ctrl Pts',(-5.50351236041864,-5.69701027385652,
-23.3832241324591));
#67097=CARTESIAN_POINT('Ctrl Pts',(-4.93807177513233,-6.19044624449914,
-23.3497588865095));
#67098=CARTESIAN_POINT('Ctrl Pts',(-4.65965692572858,-6.40264156999199,
-23.3348086493368));
#67099=CARTESIAN_POINT('Ctrl Pts',(-4.34701574022773,-6.60969089504712,
-23.3196266583546));
#67100=CARTESIAN_POINT('Ctrl Pts',(-4.32588018113389,-6.62354287741171,
-23.3186076290462));
#67101=CARTESIAN_POINT('Ctrl Pts',(-4.29596035252199,-6.64294766089435,
-23.3171753079233));
#67102=CARTESIAN_POINT('Ctrl Pts',(-4.28723107677333,-6.64858471190051,
-23.3167586424165));
#67103=CARTESIAN_POINT('Ctrl Pts',(-4.27281963899332,-6.65785091372609,
-23.3160727623474));
#67104=CARTESIAN_POINT('Ctrl Pts',(-4.2671439127178,-6.66149001990078,-23.3158031504573));
#67105=CARTESIAN_POINT('Ctrl Pts',(-4.25535726192769,-6.66902602351231,
-23.3152443119733));
#67106=CARTESIAN_POINT('Ctrl Pts',(-4.2492456189772,-6.67292178876048,-23.3149551306023));
#67107=CARTESIAN_POINT('Ctrl Pts',(-4.23467195658778,-6.68218338700676,
-23.3142669548159));
#67108=CARTESIAN_POINT('Ctrl Pts',(-4.22620506967614,-6.68754155931461,
-23.3138682649928));
#67109=CARTESIAN_POINT('Ctrl Pts',(-4.19848077058032,-6.70501288541247,
-23.3125664282954));
#67110=CARTESIAN_POINT('Ctrl Pts',(-4.17918119788709,-6.71705911106172,
-23.3116659320452));
#67111=CARTESIAN_POINT('Ctrl Pts',(-3.95191828272223,-6.85755130339652,
-23.3011287875819));
#67112=CARTESIAN_POINT('Ctrl Pts',(-3.73815358238242,-6.97638075731118,
-23.2918776879057));
#67113=CARTESIAN_POINT('Ctrl Pts',(-3.31370427016879,-7.18720669631126,
-23.2745481922498));
#67114=CARTESIAN_POINT('Ctrl Pts',(-3.10384312130114,-7.28029811729927,
-23.2664402409466));
#67115=CARTESIAN_POINT('Ctrl Pts',(-2.57752173916738,-7.48686503018814,
-23.2468498041398));
#67116=CARTESIAN_POINT('Ctrl Pts',(-2.25731716572849,-7.58955100482637,
-23.2355757754633));
#67117=CARTESIAN_POINT('Ctrl Pts',(-1.67936939007355,-7.73506767771934,
-23.2151519638779));
#67118=CARTESIAN_POINT('Ctrl Pts',(-1.42421081325541,-7.78608789002875,
-23.2061038995402));
#67119=CARTESIAN_POINT('Ctrl Pts',(-1.04113369466977,-7.84322387867413,
-23.1918924784364));
#67120=CARTESIAN_POINT('Ctrl Pts',(-0.914820465146266,-7.85895801013937,
-23.1871055225053));
#67121=CARTESIAN_POINT('Ctrl Pts',(-0.729428076826358,-7.87752137782858,
-23.1798598037081));
#67122=CARTESIAN_POINT('Ctrl Pts',(-0.670605293340097,-7.88274676572456,
-23.177528553565));
#67123=CARTESIAN_POINT('Ctrl Pts',(-0.602180157707596,-7.88805374126582,
-23.1747734298128));
#67124=CARTESIAN_POINT('Ctrl Pts',(-0.592628105192426,-7.88877713547769,
-23.1743878329442));
#67125=CARTESIAN_POINT('Ctrl Pts',(-0.577971896351022,-7.8898603073054,
-23.1737946931248));
#67126=CARTESIAN_POINT('Ctrl Pts',(-0.572868648418705,-7.89023248663708,
-23.1735878855771));
#67127=CARTESIAN_POINT('Ctrl Pts',(-0.563549365801968,-7.89090305201829,
-23.1732097212759));
#67128=CARTESIAN_POINT('Ctrl Pts',(-0.559333442395606,-7.89120301121004,
-23.1730384565854));
#67129=CARTESIAN_POINT('Ctrl Pts',(-0.550204907701421,-7.89184514612619,
-23.1726672213147));
#67130=CARTESIAN_POINT('Ctrl Pts',(-0.54529221595035,-7.89218611348633,
-23.17246718073));
#67131=CARTESIAN_POINT('Ctrl Pts',(-0.531942772604608,-7.89310011300755,
-23.171922920315));
#67132=CARTESIAN_POINT('Ctrl Pts',(-0.523505436032349,-7.89366420394659,
-23.1715781871559));
#67133=CARTESIAN_POINT('Ctrl Pts',(-0.483533326667343,-7.89627223080815,
-23.1699415480746));
#67134=CARTESIAN_POINT('Ctrl Pts',(-0.451987788904008,-7.89814070562536,
-23.1686397421444));
#67135=CARTESIAN_POINT('Ctrl Pts',(0.0816944352461355,-7.9265435375431,
-23.1464533554239));
#67136=CARTESIAN_POINT('Ctrl Pts',(0.585182534074961,-7.9053296285658,-23.1231420560138));
#67137=CARTESIAN_POINT('Ctrl Pts',(1.49190222727378,-7.77999887878778,-23.0804691799043));
#67138=CARTESIAN_POINT('Ctrl Pts',(1.8955886470672,-7.6916146280026,-23.0612116250202));
#67139=CARTESIAN_POINT('Ctrl Pts',(2.66534341494268,-7.45876579349694,-23.0251686377036));
#67140=CARTESIAN_POINT('Ctrl Pts',(3.03122701283588,-7.31771570413891,-23.0083552476783));
#67141=CARTESIAN_POINT('Ctrl Pts',(3.40810512020531,-7.13928448250228,-22.9914361243897));
#67142=CARTESIAN_POINT('Ctrl Pts',(3.43096148138346,-7.12832846895099,-22.9904114965507));
#67143=CARTESIAN_POINT('Ctrl Pts',(3.46349110267295,-7.1125429528667,-22.9889552326629));
#67144=CARTESIAN_POINT('Ctrl Pts',(3.47320761126438,-7.10780323059943,-22.9885205070163));
#67145=CARTESIAN_POINT('Ctrl Pts',(3.48997260496885,-7.0995826646975,-22.9877708605858));
#67146=CARTESIAN_POINT('Ctrl Pts',(3.49702566180411,-7.09611121089908,-22.9874556165575));
#67147=CARTESIAN_POINT('Ctrl Pts',(3.51129968309165,-7.08905921104586,-22.9868178899528));
#67148=CARTESIAN_POINT('Ctrl Pts',(3.5185203739923,-7.08547813069001,-22.9864954263375));
#67149=CARTESIAN_POINT('Ctrl Pts',(3.53620143579023,-7.07667556753425,-22.985706154469));
#67150=CARTESIAN_POINT('Ctrl Pts',(3.54665574351732,-7.07144191244539,-22.9852397674271));
#67151=CARTESIAN_POINT('Ctrl Pts',(3.58309866424427,-7.05309664482877,-22.9836149559846));
#67152=CARTESIAN_POINT('Ctrl Pts',(3.60902662196105,-7.03986471345453,-22.9824606959615));
#67153=CARTESIAN_POINT('Ctrl Pts',(4.05595964764183,-6.80866130332363,-22.9625923036997));
#67154=CARTESIAN_POINT('Ctrl Pts',(4.45662792461579,-6.55341173095615,-22.9452928760393));
#67155=CARTESIAN_POINT('Ctrl Pts',(4.91888357792768,-6.19681629661714,-22.9247473390674));
#67156=CARTESIAN_POINT('Ctrl Pts',(5.00431449693323,-6.12803268761209,-22.9209190930447));
#67157=CARTESIAN_POINT('Ctrl Pts',(5.4325393369979,-5.7683243354554,-22.9014696783125));
#67158=CARTESIAN_POINT('Ctrl Pts',(5.75149633563491,-5.45034871983454,-22.8861467948277));
#67159=CARTESIAN_POINT('Ctrl Pts',(6.09275604566406,-5.04663240105663,-22.8667378087672));
#67160=CARTESIAN_POINT('Ctrl Pts',(6.14289823663191,-4.98547646606103,-22.8637977633662));
#67161=CARTESIAN_POINT('Ctrl Pts',(6.27102358523628,-4.82434031455888,-22.8560250074591));
#67162=CARTESIAN_POINT('Ctrl Pts',(6.34752650342914,-4.72322987791262,-22.8511121972765));
#67163=CARTESIAN_POINT('Ctrl Pts',(6.4383219813994,-4.59703751595736,-22.8449376903231));
#67164=CARTESIAN_POINT('Ctrl Pts',(6.45494850985224,-4.57366194299804,-22.8437925872339));
#67165=CARTESIAN_POINT('Ctrl Pts',(6.47779738291332,-4.54116548366674,-22.842199285572));
#67166=CARTESIAN_POINT('Ctrl Pts',(6.48412843280144,-4.53212106520379,-22.841755689226));
#67167=CARTESIAN_POINT('Ctrl Pts',(6.49479756797413,-4.51681122312205,-22.8410045780519));
#67168=CARTESIAN_POINT('Ctrl Pts',(6.4991455800311,-4.51055271595362,-22.8406974700386));
#67169=CARTESIAN_POINT('Ctrl Pts',(6.50774307078379,-4.49813928928504,-22.8400882278452));
#67170=CARTESIAN_POINT('Ctrl Pts',(6.51199287803341,-4.49198460562465,-22.8397861072629));
#67171=CARTESIAN_POINT('Ctrl Pts',(6.52135816336594,-4.47838032883842,-22.8391181975303));
#67172=CARTESIAN_POINT('Ctrl Pts',(6.52646961469048,-4.47092798336397,-22.8387522515846));
#67173=CARTESIAN_POINT('Ctrl Pts',(6.54436295633191,-4.44474394640974,-22.8374662843723));
#67174=CARTESIAN_POINT('Ctrl Pts',(6.5570770071564,-4.42596615041604,-22.836543689582));
#67175=CARTESIAN_POINT('Ctrl Pts',(6.76432861909984,-4.11701639132446,-22.8213608936073));
#67176=CARTESIAN_POINT('Ctrl Pts',(6.93950979941507,-3.81433505291634,-22.8064583039197));
#67177=CARTESIAN_POINT('Ctrl Pts',(7.37422346845891,-2.93349181234954,-22.7642753501626));
#67178=CARTESIAN_POINT('Ctrl Pts',(7.58522803413551,-2.3342953817592,-22.7371205485005));
#67179=CARTESIAN_POINT('Ctrl Pts',(7.80967299601987,-1.3244344980061,-22.6940905673222));
#67180=CARTESIAN_POINT('Ctrl Pts',(7.86682090775009,-0.92642465767085,-22.6775978506539));
#67181=CARTESIAN_POINT('Ctrl Pts',(7.89694819995191,-0.47414181696498,-22.6592280992672));
#67182=CARTESIAN_POINT('Ctrl Pts',(7.89988202566965,-0.422451605532426,
-22.6571350301828));
#67183=CARTESIAN_POINT('Ctrl Pts',(7.90355661638236,-0.344127030931268,
-22.6539730082449));
#67184=CARTESIAN_POINT('Ctrl Pts',(7.90467057463607,-0.317511754710679,
-22.6529001945161));
#67185=CARTESIAN_POINT('Ctrl Pts',(7.90636927135538,-0.27134570666822,-22.6510421762088));
#67186=CARTESIAN_POINT('Ctrl Pts',(7.90701597186309,-0.251797479580481,
-22.6502563161218));
#67187=CARTESIAN_POINT('Ctrl Pts',(7.90821151590552,-0.211091372095154,
-22.6486217082265));
#67188=CARTESIAN_POINT('Ctrl Pts',(7.90874796043926,-0.189933275316337,
-22.6477731013576));
#67189=CARTESIAN_POINT('Ctrl Pts',(7.90999222863793,-0.131623289698204,
-22.6454371865066));
#67190=CARTESIAN_POINT('Ctrl Pts',(7.91052321549963,-0.0944680990550924,
-22.6439518458459));
#67191=CARTESIAN_POINT('Ctrl Pts',(7.91159562359502,0.0535607596952131,
-22.6380460540293));
#67192=CARTESIAN_POINT('Ctrl Pts',(7.91006794023323,0.164437517092207,-22.6336492903225));
#67193=CARTESIAN_POINT('Ctrl Pts',(7.88117583046183,0.994337554661038,-22.6009046547237));
#67194=CARTESIAN_POINT('Ctrl Pts',(7.75815828832591,1.70662002243985,-22.574056958052));
#67195=CARTESIAN_POINT('Ctrl Pts',(7.51234785293637,2.48138342621886,-22.5420656792621));
#67196=CARTESIAN_POINT('Ctrl Pts',(7.48254725891005,2.56984824459782,-22.5383643831634));
#67197=CARTESIAN_POINT('Ctrl Pts',(7.44441096772453,2.67676546400133,-22.5338166259961));
#67198=CARTESIAN_POINT('Ctrl Pts',(7.43756062350818,2.69574108065189,-22.5330065951247));
#67199=CARTESIAN_POINT('Ctrl Pts',(7.42647815555818,2.72607595979644,-22.5317069085926));
#67200=CARTESIAN_POINT('Ctrl Pts',(7.42229242210684,2.73745194168732,-22.5312184469923));
#67201=CARTESIAN_POINT('Ctrl Pts',(7.41425149018237,2.75915155067683,-22.5302847133134));
#67202=CARTESIAN_POINT('Ctrl Pts',(7.41040083213919,2.76947683604567,-22.5298395514715));
#67203=CARTESIAN_POINT('Ctrl Pts',(7.40154016876304,2.7930853323432,-22.5288197485293));
#67204=CARTESIAN_POINT('Ctrl Pts',(7.39651596083298,2.80636315946921,-22.5282447768672));
#67205=CARTESIAN_POINT('Ctrl Pts',(7.38128637350956,2.84628645820132,-22.5265117843791));
#67206=CARTESIAN_POINT('Ctrl Pts',(7.37097258579096,2.87289022676991,-22.5253513404579));
#67207=CARTESIAN_POINT('Ctrl Pts',(7.26805159049797,3.13416557612076,-22.5139012392555));
#67208=CARTESIAN_POINT('Ctrl Pts',(7.16441453200506,3.36433153902463,-22.5033932031116));
#67209=CARTESIAN_POINT('Ctrl Pts',(6.85128875591306,3.97938713184054,-22.474473743837));
#67210=CARTESIAN_POINT('Ctrl Pts',(6.62055271442245,4.35246763972521,-22.4560163624423));
#67211=CARTESIAN_POINT('Ctrl Pts',(6.22857203166411,4.88239202367224,-22.4287463610505));
#67212=CARTESIAN_POINT('Ctrl Pts',(6.08960891259975,5.05465410361187,-22.4196841489124));
#67213=CARTESIAN_POINT('Ctrl Pts',(5.91028409020812,5.25880332711376,-22.4086708350538));
#67214=CARTESIAN_POINT('Ctrl Pts',(5.8765992036506,5.29641881846097,-22.4066294083844));
#67215=CARTESIAN_POINT('Ctrl Pts',(5.82260416059552,5.35556510108791,-22.4033992654985));
#67216=CARTESIAN_POINT('Ctrl Pts',(5.80252941559471,5.37730872761792,-22.4022073664768));
#67217=CARTESIAN_POINT('Ctrl Pts',(5.76445535173527,5.41808653770854,-22.3999635075256));
#67218=CARTESIAN_POINT('Ctrl Pts',(5.74648258251383,5.43714494624809,-22.3989112047847));
#67219=CARTESIAN_POINT('Ctrl Pts',(5.7056408383252,5.48002500487059,-22.3965352665139));
#67220=CARTESIAN_POINT('Ctrl Pts',(5.68271668598925,5.50379346516537,-22.3952123974081));
#67221=CARTESIAN_POINT('Ctrl Pts',(5.62297201499754,5.56496734486013,-22.3917918756111));
#67222=CARTESIAN_POINT('Ctrl Pts',(5.58592678674641,5.60215117639909,-22.389697248834));
#67223=CARTESIAN_POINT('Ctrl Pts',(5.3772485281138,5.80748221318233,-22.3780387654395));
#67224=CARTESIAN_POINT('Ctrl Pts',(5.19839109571368,5.96811394540662,-22.3685563541904));
#67225=CARTESIAN_POINT('Ctrl Pts',(4.37138269417036,6.64542419015001,-22.3267015104359));
#67226=CARTESIAN_POINT('Ctrl Pts',(3.65177385603422,7.06647964446705,-22.2965018722598));
#67227=CARTESIAN_POINT('Ctrl Pts',(2.70191170831728,7.43775153801269,-22.2581994294924));
#67228=CARTESIAN_POINT('Ctrl Pts',(2.52138058201012,7.50087398837203,-22.2509387627355));
#67229=CARTESIAN_POINT('Ctrl Pts',(2.25848251306327,7.58223166325244,-22.2402112474926));
#67230=CARTESIAN_POINT('Ctrl Pts',(2.17782954689089,7.6057897789489,-22.2368994663054));
#67231=CARTESIAN_POINT('Ctrl Pts',(2.08242666126868,7.63201434564827,-22.2329435918397));
#67232=CARTESIAN_POINT('Ctrl Pts',(2.06802383360748,7.635929621974,-22.2323453523953));
#67233=CARTESIAN_POINT('Ctrl Pts',(2.04591819467087,7.64187170663615,-22.231425486507));
#67234=CARTESIAN_POINT('Ctrl Pts',(2.03822321639418,7.6439276919373,-22.231104969135));
#67235=CARTESIAN_POINT('Ctrl Pts',(2.02479068657937,7.64749494141583,-22.2305449042382));
#67236=CARTESIAN_POINT('Ctrl Pts',(2.01905450835133,7.64901138026938,-22.230305557382));
#67237=CARTESIAN_POINT('Ctrl Pts',(2.00613624963292,7.65241095841575,-22.2297661198211));
#67238=CARTESIAN_POINT('Ctrl Pts',(1.9989532187864,7.65429044113134,-22.2294658857942));
#67239=CARTESIAN_POINT('Ctrl Pts',(1.97970632349646,7.65929756517387,-22.2286606192096));
#67240=CARTESIAN_POINT('Ctrl Pts',(1.96763772593491,7.66240680832761,-22.2281548521215));
#67241=CARTESIAN_POINT('Ctrl Pts',(1.91536699272888,7.67574172708604,-22.2259605296573));
#67242=CARTESIAN_POINT('Ctrl Pts',(1.87509260962544,7.68567950085647,-22.2242601552386));
#67243=CARTESIAN_POINT('Ctrl Pts',(1.21237203377993,7.84368784525397,-22.1960965708982));
#67244=CARTESIAN_POINT('Ctrl Pts',(0.57438533820619,7.91600567465618,-22.16613042399));
#67245=CARTESIAN_POINT('Ctrl Pts',(-0.430327308261512,7.90772028401306,
-22.1199923195091));
#67246=CARTESIAN_POINT('Ctrl Pts',(-0.794792461017725,7.87943897231964,
-22.1034501397239));
#67247=CARTESIAN_POINT('Ctrl Pts',(-1.34482866753871,7.79819102942153,-22.079236893331));
#67248=CARTESIAN_POINT('Ctrl Pts',(-1.53257303275275,7.76347690042345,-22.0711030495767));
#67249=CARTESIAN_POINT('Ctrl Pts',(-1.81359268262661,7.70092307848371,-22.0591373163976));
#67250=CARTESIAN_POINT('Ctrl Pts',(-1.9079049794263,7.67810094410115,-22.0551572315127));
#67251=CARTESIAN_POINT('Ctrl Pts',(-2.01930230789671,7.64896511835098,-22.0504968028438));
#67252=CARTESIAN_POINT('Ctrl Pts',(-2.03681310442316,7.64432087078328,-22.0497654149583));
#67253=CARTESIAN_POINT('Ctrl Pts',(-2.06373603137056,7.63708124289795,-22.0486427180843));
#67254=CARTESIAN_POINT('Ctrl Pts',(-2.07315951569555,7.63452853430494,-22.048250097854));
#67255=CARTESIAN_POINT('Ctrl Pts',(-2.08963516340578,7.63003272546929,-22.0475642511235));
#67256=CARTESIAN_POINT('Ctrl Pts',(-2.09668939321013,7.62809727891814,-22.0472707893284));
#67257=CARTESIAN_POINT('Ctrl Pts',(-2.11261290983539,7.62370463717358,-22.0466087865065));
#67258=CARTESIAN_POINT('Ctrl Pts',(-2.12148062020833,7.62124174137317,-22.0462404217226));
#67259=CARTESIAN_POINT('Ctrl Pts',(-2.14533845510019,7.61457065924654,-22.0452501693155));
#67260=CARTESIAN_POINT('Ctrl Pts',(-2.16032052078207,7.61033367615802,-22.0446291714907));
#67261=CARTESIAN_POINT('Ctrl Pts',(-2.22612395999562,7.59151424703583,-22.0419053517552));
#67262=CARTESIAN_POINT('Ctrl Pts',(-2.27681142968143,7.5764666099866,-22.0398169419149));
#67263=CARTESIAN_POINT('Ctrl Pts',(-3.20878527784575,7.28959320209711,-22.0015858713703));
#67264=CARTESIAN_POINT('Ctrl Pts',(-4.03589018235152,6.86628985562685,-21.9714063754079));
#67265=CARTESIAN_POINT('Ctrl Pts',(-5.04632440838532,6.10223592929356,-21.9265305360208));
#67266=CARTESIAN_POINT('Ctrl Pts',(-5.30731040620941,5.87665850646896,-21.9139019888801));
#67267=CARTESIAN_POINT('Ctrl Pts',(-5.56453915577041,5.62317517220759,-21.8994823445023));
#67268=CARTESIAN_POINT('Ctrl Pts',(-5.57629353057887,5.61151900005601,-21.8988189627167));
#67269=CARTESIAN_POINT('Ctrl Pts',(-5.59332656727204,5.59452190090836,-21.8978512874785));
#67270=CARTESIAN_POINT('Ctrl Pts',(-5.59863440074843,5.58921016191732,-21.897548834385));
#67271=CARTESIAN_POINT('Ctrl Pts',(-5.60790837810292,5.57990289497959,-21.8970188063976));
#67272=CARTESIAN_POINT('Ctrl Pts',(-5.61187784079932,5.57591066950652,-21.8967914364459));
#67273=CARTESIAN_POINT('Ctrl Pts',(-5.61955734312656,5.56817062220024,-21.8963505804115));
#67274=CARTESIAN_POINT('Ctrl Pts',(-5.62326790417411,5.56442332037533,-21.8961371262027));
#67275=CARTESIAN_POINT('Ctrl Pts',(-5.63208627988719,5.55549979920899,-21.8956287914814));
#67276=CARTESIAN_POINT('Ctrl Pts',(-5.63719070342746,5.55032024803654,-21.8953337089978));
#67277=CARTESIAN_POINT('Ctrl Pts',(-5.65525578417121,5.5319386555328,-21.8942864308354));
#67278=CARTESIAN_POINT('Ctrl Pts',(-5.66817720190492,5.51869825890218,-21.8935319473368));
#67279=CARTESIAN_POINT('Ctrl Pts',(-5.88412147885672,5.29586470930945,-21.8808339689964));
#67280=CARTESIAN_POINT('Ctrl Pts',(-6.07543200940952,5.0752513930314,-21.8682700522114));
#67281=CARTESIAN_POINT('Ctrl Pts',(-6.58990625490721,4.41109250300468,-21.8315558646562));
#67282=CARTESIAN_POINT('Ctrl Pts',(-6.87975077987268,3.94381775880358,-21.8071511957049));
#67283=CARTESIAN_POINT('Ctrl Pts',(-7.23135185271398,3.21837067568155,-21.7728822125021));
#67284=CARTESIAN_POINT('Ctrl Pts',(-7.33237056327463,2.98105878774141,-21.7621589383175));
#67285=CARTESIAN_POINT('Ctrl Pts',(-7.44064482000948,2.68770205201674,-21.7494384026835));
#67286=CARTESIAN_POINT('Ctrl Pts',(-7.45912562423524,2.63597850386946,-21.7472148616269));
#67287=CARTESIAN_POINT('Ctrl Pts',(-7.48389680483133,2.56430241570359,-21.744158853042));
#67288=CARTESIAN_POINT('Ctrl Pts',(-7.49064880782332,2.54451148697386,-21.7433176807792));
#67289=CARTESIAN_POINT('Ctrl Pts',(-7.50191917932764,2.5110430315408,-21.7418995294627));
#67290=CARTESIAN_POINT('Ctrl Pts',(-7.50647879443288,2.49737954458699,-21.7413217916635));
#67291=CARTESIAN_POINT('Ctrl Pts',(-7.51543841824509,2.47028462770188,-21.7401785069937));
#67292=CARTESIAN_POINT('Ctrl Pts',(-7.51983979973477,2.45685370913308,-21.739612937059));
#67293=CARTESIAN_POINT('Ctrl Pts',(-7.529485322523,2.42715142360607,-21.7383646925643));
#67294=CARTESIAN_POINT('Ctrl Pts',(-7.53471276508316,2.41087469716293,-21.7376823173708));
#67295=CARTESIAN_POINT('Ctrl Pts',(-7.55279928086023,2.35392515735811,-21.7353004581754));
#67296=CARTESIAN_POINT('Ctrl Pts',(-7.56538219985673,2.31316511146344,-21.7336057092668));
#67297=CARTESIAN_POINT('Ctrl Pts',(-7.68569922518216,1.91193445873651,-21.7170177936768));
#67298=CARTESIAN_POINT('Ctrl Pts',(-7.76792201408034,1.54430430970014,-21.7026016950373));
#67299=CARTESIAN_POINT('Ctrl Pts',(-7.88207626752522,0.782401121233623,
-21.6737517325164));
#67300=CARTESIAN_POINT('Ctrl Pts',(-7.91126590000934,0.388781467887902,
-21.6593907303491));
#67301=CARTESIAN_POINT('Ctrl Pts',(-7.9107453481563,-0.377594936895521,
-21.6310986099574));
#67302=CARTESIAN_POINT('Ctrl Pts',(-7.88422256037135,-0.74931394523605,
-21.6172139151197));
#67303=CARTESIAN_POINT('Ctrl Pts',(-7.82709551820483,-1.14957815692969,
-21.6011465364909));
#67304=CARTESIAN_POINT('Ctrl Pts',(-7.82236008985292,-1.18137072028408,
-21.5998624694306));
#67305=CARTESIAN_POINT('Ctrl Pts',(-7.81574373215853,-1.224006531189,-21.5981290760551));
#67306=CARTESIAN_POINT('Ctrl Pts',(-7.81403370580807,-1.23487623596033,
-21.5976861649682));
#67307=CARTESIAN_POINT('Ctrl Pts',(-7.8113183666466,-1.25190467500851,-21.5969907040537));
#67308=CARTESIAN_POINT('Ctrl Pts',(-7.8103284312545,-1.25806587112258,-21.5967387456762));
#67309=CARTESIAN_POINT('Ctrl Pts',(-7.8084163474171,-1.26987712751478,-21.5962550935644));
#67310=CARTESIAN_POINT('Ctrl Pts',(-7.80749535354654,-1.27552737239145,
-21.5960234449693));
#67311=CARTESIAN_POINT('Ctrl Pts',(-7.8053209589131,-1.28877656850025,-21.5954795894983));
#67312=CARTESIAN_POINT('Ctrl Pts',(-7.80406259431449,-1.29637469067541,
-21.5951671868897));
#67313=CARTESIAN_POINT('Ctrl Pts',(-7.80040402963538,-1.31826706755527,
-21.5942655600549));
#67314=CARTESIAN_POINT('Ctrl Pts',(-7.79797564567644,-1.33255653261232,
-21.5936752053667));
#67315=CARTESIAN_POINT('Ctrl Pts',(-7.78141620456644,-1.42840261280558,
-21.5897026151095));
#67316=CARTESIAN_POINT('Ctrl Pts',(-7.76604536180301,-1.5097388793009,-21.5862688377717));
#67317=CARTESIAN_POINT('Ctrl Pts',(-7.71184000235685,-1.77379093475102,
-21.5748850699228));
#67318=CARTESIAN_POINT('Ctrl Pts',(-7.66781245105766,-1.95536575576184,
-21.5666981148979));
#67319=CARTESIAN_POINT('Ctrl Pts',(-7.36151260778159,-3.048100702441,-21.5159179917715));
#67320=CARTESIAN_POINT('Ctrl Pts',(-6.94345973240831,-3.90794187958212,
-21.4706865502298));
#67321=CARTESIAN_POINT('Ctrl Pts',(-6.35960268692158,-4.70541822230912,
-21.430267071367));
#67322=CARTESIAN_POINT('Ctrl Pts',(-6.33583459448097,-4.73737343220393,
-21.4286480529591));
#67323=CARTESIAN_POINT('Ctrl Pts',(-6.30224815468107,-4.78182408831214,
-21.4263966707751));
#67324=CARTESIAN_POINT('Ctrl Pts',(-6.29263213145982,-4.79447121972945,
-21.4257561878589));
#67325=CARTESIAN_POINT('Ctrl Pts',(-6.27708819846478,-4.81478750314993,
-21.4247274382396));
#67326=CARTESIAN_POINT('Ctrl Pts',(-6.27118420340238,-4.82247484593607,
-21.4243382040122));
#67327=CARTESIAN_POINT('Ctrl Pts',(-6.26065547613108,-4.83613182544767,
-21.423646753508));
#67328=CARTESIAN_POINT('Ctrl Pts',(-6.25603630242249,-4.84210572035682,
-21.4233443116545));
#67329=CARTESIAN_POINT('Ctrl Pts',(-6.24638512293663,-4.85455055485945,
-21.4227142938342));
#67330=CARTESIAN_POINT('Ctrl Pts',(-6.24135159748562,-4.86102030759316,
-21.4223867805118));
#67331=CARTESIAN_POINT('Ctrl Pts',(-6.22826277664478,-4.87778994625331,
-21.4215379040403));
#67332=CARTESIAN_POINT('Ctrl Pts',(-6.22019196937048,-4.88807772453234,
-21.4210171776815));
#67333=CARTESIAN_POINT('Ctrl Pts',(-6.18571789394125,-4.93179784503496,
-21.4188043793465));
#67334=CARTESIAN_POINT('Ctrl Pts',(-6.15907007770094,-4.96503692839506,
-21.4171224107468));
#67335=CARTESIAN_POINT('Ctrl Pts',(-5.97655741977728,-5.18896300841103,
-21.4057918523416));
#67336=CARTESIAN_POINT('Ctrl Pts',(-5.81212428790815,-5.37250403766793,
-21.3965137693093));
#67337=CARTESIAN_POINT('Ctrl Pts',(-5.40897519610457,-5.78228743705215,
-21.375593996404));
#67338=CARTESIAN_POINT('Ctrl Pts',(-5.16419176956802,-6.00191637688304,
-21.3642256674013));
#67339=CARTESIAN_POINT('Ctrl Pts',(-4.80116549772192,-6.28893833943299,
-21.3485261259123));
#67340=CARTESIAN_POINT('Ctrl Pts',(-4.69377752270709,-6.36948886963239,
-21.3440099669713));
#67341=CARTESIAN_POINT('Ctrl Pts',(-4.4642599355813,-6.53268954279551,-21.3345381723446));
#67342=CARTESIAN_POINT('Ctrl Pts',(-4.34176465049529,-6.61473572084111,
-21.3295848862548));
#67343=CARTESIAN_POINT('Ctrl Pts',(-3.84086786837393,-6.93032041986989,
-21.3094941013542));
#67344=CARTESIAN_POINT('Ctrl Pts',(-3.44541288476946,-7.13516996035063,
-21.294017865501));
#67345=CARTESIAN_POINT('Ctrl Pts',(-3.00797075166161,-7.31689028865405,
-21.2752787874538));
#67346=CARTESIAN_POINT('Ctrl Pts',(-2.98097686664058,-7.32792934030669,
-21.2741160443696));
#67347=CARTESIAN_POINT('Ctrl Pts',(-2.94654501499779,-7.34178838748635,
-21.2726241013143));
#67348=CARTESIAN_POINT('Ctrl Pts',(-2.9391626799767,-7.34474689773294,-21.2723037084602));
#67349=CARTESIAN_POINT('Ctrl Pts',(-2.92744482765136,-7.34942239403138,
-21.2717943217546));
#67350=CARTESIAN_POINT('Ctrl Pts',(-2.92311221464665,-7.35114669457967,
-21.271605798405));
#67351=CARTESIAN_POINT('Ctrl Pts',(-2.91504043116856,-7.35435085212021,
-21.2712542339505));
#67352=CARTESIAN_POINT('Ctrl Pts',(-2.91130164966327,-7.35583169165633,
-21.2710912565613));
#67353=CARTESIAN_POINT('Ctrl Pts',(-2.90300656327971,-7.35910985676302,
-21.2707293609128));
#67354=CARTESIAN_POINT('Ctrl Pts',(-2.89844974518951,-7.36090579106245,
-21.2705303535507));
#67355=CARTESIAN_POINT('Ctrl Pts',(-2.88510607476708,-7.36615048987092,
-21.269947003274));
#67356=CARTESIAN_POINT('Ctrl Pts',(-2.8763147836479,-7.36958773378039,-21.269561913305));
#67357=CARTESIAN_POINT('Ctrl Pts',(-2.81100485424835,-7.39498813046937,
-21.266695613037));
#67358=CARTESIAN_POINT('Ctrl Pts',(-2.75424295948736,-7.41631600384348,
-21.2641739677269));
#67359=CARTESIAN_POINT('Ctrl Pts',(-2.5661021774853,-7.48455080145951,-21.2557307107967));
#67360=CARTESIAN_POINT('Ctrl Pts',(-2.43373237539814,-7.52863360485083,
-21.2496546623201));
#67361=CARTESIAN_POINT('Ctrl Pts',(-2.02692100712389,-7.65226337220843,
-21.2307340730246));
#67362=CARTESIAN_POINT('Ctrl Pts',(-1.74928006592286,-7.72046299806746,
-21.2174909062702));
#67363=CARTESIAN_POINT('Ctrl Pts',(-0.716985315266224,-7.91548474314031,
-21.1684926338017));
#67364=CARTESIAN_POINT('Ctrl Pts',(0.0514080090607971,-7.94775444566785,
-21.1330290838053));
#67365=CARTESIAN_POINT('Ctrl Pts',(0.861093271274686,-7.86414778730948,
-21.0997509164887));
#67366=CARTESIAN_POINT('Ctrl Pts',(0.909584295851367,-7.85868682231813,
-21.0977711891163));
#67367=CARTESIAN_POINT('Ctrl Pts',(0.971750152234671,-7.85110271871587,
-21.0952498150449));
#67368=CARTESIAN_POINT('Ctrl Pts',(0.985473616269634,-7.84939195177175,
-21.0946942499346));
#67369=CARTESIAN_POINT('Ctrl Pts',(1.00735506278086,-7.84660592127813,-21.0938100757642));
#67370=CARTESIAN_POINT('Ctrl Pts',(1.0155159434255,-7.84555390495557,-21.0934806813097));
#67371=CARTESIAN_POINT('Ctrl Pts',(1.03078586071227,-7.84356124041183,-21.0928650293529));
#67372=CARTESIAN_POINT('Ctrl Pts',(1.03789528425489,-7.84262365551421,-21.0925786686148));
#67373=CARTESIAN_POINT('Ctrl Pts',(1.0537463342409,-7.84051130085311,-21.0919408177637));
#67374=CARTESIAN_POINT('Ctrl Pts',(1.06248729705286,-7.83933157482365,-21.0915894956364));
#67375=CARTESIAN_POINT('Ctrl Pts',(1.0879854703983,-7.83584677827224,-21.0905658659417));
#67376=CARTESIAN_POINT('Ctrl Pts',(1.10473733351307,-7.83350257197665,-21.0898948825024));
#67377=CARTESIAN_POINT('Ctrl Pts',(1.2252407898825,-7.81624543933323,-21.0850790317458));
#67378=CARTESIAN_POINT('Ctrl Pts',(1.32869673371227,-7.79932521820932,-21.0810024810428));
#67379=CARTESIAN_POINT('Ctrl Pts',(1.65784436251976,-7.73875344090587,-21.0681982896105));
#67380=CARTESIAN_POINT('Ctrl Pts',(1.88198772269963,-7.68731970907369,-21.0597328815518));
#67381=CARTESIAN_POINT('Ctrl Pts',(2.59089059771522,-7.49177833125318,-21.0334222430698));
#67382=CARTESIAN_POINT('Ctrl Pts',(3.06420086715347,-7.31095925291493,-21.0166415176531));
#67383=CARTESIAN_POINT('Ctrl Pts',(3.87841461823988,-6.90685290355965,-20.9854044606381));
#67384=CARTESIAN_POINT('Ctrl Pts',(4.22554153965593,-6.70010797695943,-20.9711697654637));
#67385=CARTESIAN_POINT('Ctrl Pts',(4.57651302288907,-6.45291560692468,-20.9541510148781));
#67386=CARTESIAN_POINT('Ctrl Pts',(4.59760628541024,-6.43790398334244,-20.9531174201609));
#67387=CARTESIAN_POINT('Ctrl Pts',(4.62494905240061,-6.4182418100038,-20.95176297662));
#67388=CARTESIAN_POINT('Ctrl Pts',(4.6312660745367,-6.41368507294932,-20.9514490390346));
#67389=CARTESIAN_POINT('Ctrl Pts',(4.64102126382055,-6.40662631265038,-20.9509626702569));
#67390=CARTESIAN_POINT('Ctrl Pts',(4.64446417628442,-6.40413082285546,-20.9507907135492));
#67391=CARTESIAN_POINT('Ctrl Pts',(4.65132699056783,-6.39914807681759,-20.9504473496905));
#67392=CARTESIAN_POINT('Ctrl Pts',(4.65474691372872,-6.39666085166512,-20.9502759447799));
#67393=CARTESIAN_POINT('Ctrl Pts',(4.66233743626961,-6.3911311425309,-20.9498948532737));
#67394=CARTESIAN_POINT('Ctrl Pts',(4.66650705184479,-6.38808731824389,-20.9496850706653));
#67395=CARTESIAN_POINT('Ctrl Pts',(4.67856669156447,-6.37926565904119,-20.9490770506118));
#67396=CARTESIAN_POINT('Ctrl Pts',(4.68644896100156,-6.3734772903279,-20.9486780649796));
#67397=CARTESIAN_POINT('Ctrl Pts',(4.74016475745324,-6.33387740696146,-20.945948396311));
#67398=CARTESIAN_POINT('Ctrl Pts',(4.78564167308849,-6.29958716131757,-20.943584264623));
#67399=CARTESIAN_POINT('Ctrl Pts',(4.92270870249896,-6.1938959013837,-20.936306083309));
#67400=CARTESIAN_POINT('Ctrl Pts',(5.01309782457362,-6.12096850106347,-20.9312958938204));
#67401=CARTESIAN_POINT('Ctrl Pts',(5.26204440718154,-5.91090071255158,-20.9169727484844));
#67402=CARTESIAN_POINT('Ctrl Pts',(5.4168008110311,-5.76941240464089,-20.9074499974814));
#67403=CARTESIAN_POINT('Ctrl Pts',(6.0566700257703,-5.13594023590603,-20.8659544035823));
#67404=CARTESIAN_POINT('Ctrl Pts',(6.48190002103106,-4.58762806025694,-20.8331182224442));
#67405=CARTESIAN_POINT('Ctrl Pts',(6.96337518330853,-3.76360342082201,-20.7915312667113));
#67406=CARTESIAN_POINT('Ctrl Pts',(7.08482737137376,-3.52966619513001,-20.7804318718218));
#67407=CARTESIAN_POINT('Ctrl Pts',(7.20465465993677,-3.26764157597415,-20.7687419920021));
#67408=CARTESIAN_POINT('Ctrl Pts',(7.21481486307336,-3.24514664443682,-20.7677441563533));
#67409=CARTESIAN_POINT('Ctrl Pts',(7.22894556321345,-3.21346653280501,-20.7663468681306));
#67410=CARTESIAN_POINT('Ctrl Pts',(7.23300411495814,-3.20432092451304,-20.7659444221245));
#67411=CARTESIAN_POINT('Ctrl Pts',(7.24002024894259,-3.18842940155423,-20.7652467366101));
#67412=CARTESIAN_POINT('Ctrl Pts',(7.24298577669856,-3.18168701992172,-20.764951227853));
#67413=CARTESIAN_POINT('Ctrl Pts',(7.24913959588187,-3.16764259412185,-20.7643367223005));
#67414=CARTESIAN_POINT('Ctrl Pts',(7.25232628191619,-3.16033985289428,-20.7640177800442));
#67415=CARTESIAN_POINT('Ctrl Pts',(7.25980912798476,-3.14312093502805,-20.7632671278884));
#67416=CARTESIAN_POINT('Ctrl Pts',(7.26409601737321,-3.13320073384158,-20.7628357312266));
#67417=CARTESIAN_POINT('Ctrl Pts',(7.27806551724902,-3.10069143010521,-20.7614254943853));
#67418=CARTESIAN_POINT('Ctrl Pts',(7.28766323495301,-3.07806588716903,-20.7604495105374));
#67419=CARTESIAN_POINT('Ctrl Pts',(7.41945368213048,-2.76331276813066,-20.7469474682724));
#67420=CARTESIAN_POINT('Ctrl Pts',(7.52411015130992,-2.46413886800956,-20.7350279249475));
#67421=CARTESIAN_POINT('Ctrl Pts',(7.83730908795459,-1.36034373403431,-20.6933708981584));
#67422=CARTESIAN_POINT('Ctrl Pts',(7.93675504794735,-0.530610222401086,
-20.6668026261471));
#67423=CARTESIAN_POINT('Ctrl Pts',(7.90099305826384,0.414021654672896,-20.6307363749247));
#67424=CARTESIAN_POINT('Ctrl Pts',(7.89415216561908,0.528642865584702,-20.6262464721065));
#67425=CARTESIAN_POINT('Ctrl Pts',(7.8832934657749,0.661783695376,-20.6209142428322));
#67426=CARTESIAN_POINT('Ctrl Pts',(7.88170061581656,0.680491677098419,-20.6201623780103));
#67427=CARTESIAN_POINT('Ctrl Pts',(7.87921999114664,0.708448771278402,-20.6190350219986));
#67428=CARTESIAN_POINT('Ctrl Pts',(7.87838249044857,0.717702350405974,-20.6186612575323));
#67429=CARTESIAN_POINT('Ctrl Pts',(7.87688183353025,0.73396398629768,-20.6180033610302));
#67430=CARTESIAN_POINT('Ctrl Pts',(7.87622562111443,0.740972683389345,-20.6177194618003));
#67431=CARTESIAN_POINT('Ctrl Pts',(7.87481258675461,0.755850661115741,-20.6171160741727));
#67432=CARTESIAN_POINT('Ctrl Pts',(7.87405332207465,0.763719699270015,-20.6167965057939));
#67433=CARTESIAN_POINT('Ctrl Pts',(7.87205028162581,0.784158731005746,-20.6159653505631));
#67434=CARTESIAN_POINT('Ctrl Pts',(7.87078819566997,0.796726884704747,-20.6154531757187));
#67435=CARTESIAN_POINT('Ctrl Pts',(7.86795676486664,0.824259512673034,-20.6143288443649));
#67436=CARTESIAN_POINT('Ctrl Pts',(7.86637481784451,0.839222628415784,-20.613716298241));
#67437=CARTESIAN_POINT('Ctrl Pts',(7.86160515415308,0.88313862473828,-20.6119142148914));
#67438=CARTESIAN_POINT('Ctrl Pts',(7.85830022453001,0.912078390124585,-20.6107211993675));
#67439=CARTESIAN_POINT('Ctrl Pts',(7.81817691669445,1.24700113475295,-20.5968546234686));
#67440=CARTESIAN_POINT('Ctrl Pts',(7.76366911572295,1.55059080879836,-20.5837208832194));
#67441=CARTESIAN_POINT('Ctrl Pts',(7.56325130360046,2.38375512400206,-20.5469421744943));
#67442=CARTESIAN_POINT('Ctrl Pts',(7.37973385359114,2.90252132761531,-20.5233054107278));
#67443=CARTESIAN_POINT('Ctrl Pts',(6.98089664857006,3.74101422816054,-20.4843757783525));
#67444=CARTESIAN_POINT('Ctrl Pts',(6.79331301614788,4.07173329052805,-20.4687272326319));
#67445=CARTESIAN_POINT('Ctrl Pts',(6.50511686073495,4.50410307119251,-20.4474658234096));
#67446=CARTESIAN_POINT('Ctrl Pts',(6.42445548124228,4.61842639602404,-20.4417706248743));
#67447=CARTESIAN_POINT('Ctrl Pts',(6.31690899550406,4.76258108688293,-20.4344960518572));
#67448=CARTESIAN_POINT('Ctrl Pts',(6.29277115696986,4.79442896003501,-20.432882816315));
#67449=CARTESIAN_POINT('Ctrl Pts',(6.25367334350229,4.84521133733519,-20.4303005970997));
#67450=CARTESIAN_POINT('Ctrl Pts',(6.23886629392961,4.86426259177226,-20.4293296081516));
#67451=CARTESIAN_POINT('Ctrl Pts',(6.21188285561536,4.8986545060229,-20.4275726149645));
#67452=CARTESIAN_POINT('Ctrl Pts',(6.19973622522395,4.91401824593606,-20.426786212725));
#67453=CARTESIAN_POINT('Ctrl Pts',(6.17084754829864,4.9502806562434,-20.4249264894265));
#67454=CARTESIAN_POINT('Ctrl Pts',(6.15405618274825,4.97113976326378,-20.4238538680703));
#67455=CARTESIAN_POINT('Ctrl Pts',(6.10412495373399,5.03252622680137,-20.420688647242));
#67456=CARTESIAN_POINT('Ctrl Pts',(6.07068824774709,5.07281045585719,-20.4186003510109));
#67457=CARTESIAN_POINT('Ctrl Pts',(5.99418852521581,5.16313694408908,-20.4138916384752));
#67458=CARTESIAN_POINT('Ctrl Pts',(5.95089391630132,5.21297811920387,-20.4112747994626));
#67459=CARTESIAN_POINT('Ctrl Pts',(5.80721161052512,5.3742636968294,-20.4027417403601));
#67460=CARTESIAN_POINT('Ctrl Pts',(5.7042772129205,5.48339670637859,-20.3968647903666));
#67461=CARTESIAN_POINT('Ctrl Pts',(5.37641096625898,5.81177695730301,-20.3787971286387));
#67462=CARTESIAN_POINT('Ctrl Pts',(5.14148329493697,6.02060615998056,-20.3667574363342));
#67463=CARTESIAN_POINT('Ctrl Pts',(4.80989059983049,6.28176288770404,-20.3505335275156));
#67464=CARTESIAN_POINT('Ctrl Pts',(4.72365773778135,6.34686142649266,-20.3463776105699));
#67465=CARTESIAN_POINT('Ctrl Pts',(4.4359436146328,6.55494893129596,-20.3326651142168));
#67466=CARTESIAN_POINT('Ctrl Pts',(4.22910167332117,6.69026482467019,-20.3230504807747));
#67467=CARTESIAN_POINT('Ctrl Pts',(3.99396935792509,6.8288212806999,-20.3121408109388));
#67468=CARTESIAN_POINT('Ctrl Pts',(3.97159925208184,6.84185579288376,-20.3111030356709));
#67469=CARTESIAN_POINT('Ctrl Pts',(3.9378045910166,6.86132552181955,-20.3095350987322));
#67470=CARTESIAN_POINT('Ctrl Pts',(3.92642735072553,6.86784254124089,-20.3090072220809));
#67471=CARTESIAN_POINT('Ctrl Pts',(3.9060239274336,6.87946259459299,-20.3080605583273));
#67472=CARTESIAN_POINT('Ctrl Pts',(3.89700380304837,6.88457623026628,-20.3076420510427));
#67473=CARTESIAN_POINT('Ctrl Pts',(3.87723426966975,6.89573255584849,-20.3067248306139));
#67474=CARTESIAN_POINT('Ctrl Pts',(3.86648073822278,6.90176787232023,-20.3062259314803));
#67475=CARTESIAN_POINT('Ctrl Pts',(3.83766500293938,6.91785194590535,-20.3048891500842));
#67476=CARTESIAN_POINT('Ctrl Pts',(3.8195774915809,6.9278550793475,-20.3040501582207));
#67477=CARTESIAN_POINT('Ctrl Pts',(3.73228232334493,6.97568708976241,-20.3000018330512));
#67478=CARTESIAN_POINT('Ctrl Pts',(3.6625514012252,7.01255008414081,-20.2967707193975));
#67479=CARTESIAN_POINT('Ctrl Pts',(3.46027507998527,7.11564259659308,-20.2874178585725));
#67480=CARTESIAN_POINT('Ctrl Pts',(3.3264059547636,7.17919880802401,-20.2812526839266));
#67481=CARTESIAN_POINT('Ctrl Pts',(2.63290182147522,7.48488591026565,-20.2495636306426));
#67482=CARTESIAN_POINT('Ctrl Pts',(2.04837838062254,7.66549970638557,-20.2238251329256));
#67483=CARTESIAN_POINT('Ctrl Pts',(1.34271351908952,7.79696822633186,-20.1944793584911));
#67484=CARTESIAN_POINT('Ctrl Pts',(1.23610840741245,7.81457801328586,-20.1900859008267));
#67485=CARTESIAN_POINT('Ctrl Pts',(1.08859358208747,7.83585133405766,-20.1840562606589));
#67486=CARTESIAN_POINT('Ctrl Pts',(1.04796696585306,7.84138810265809,-20.1824008193943));
#67487=CARTESIAN_POINT('Ctrl Pts',(0.982714543400365,7.84976480429343,-20.1797497791156));
#67488=CARTESIAN_POINT('Ctrl Pts',(0.958115330509714,7.85280525510726,-20.1787521599428));
#67489=CARTESIAN_POINT('Ctrl Pts',(0.907099737642164,7.85886747558489,-20.1766867855437));
#67490=CARTESIAN_POINT('Ctrl Pts',(0.88068158595198,7.86187177983823,-20.1756192172437));
#67491=CARTESIAN_POINT('Ctrl Pts',(0.818502052832379,7.86862556553225,-20.1731109515746));
#67492=CARTESIAN_POINT('Ctrl Pts',(0.782729220383721,7.87226453328173,-20.1716713548421));
#67493=CARTESIAN_POINT('Ctrl Pts',(0.663198480906921,7.88360090730199,-20.1668718152988));
#67494=CARTESIAN_POINT('Ctrl Pts',(0.579342472025407,7.89020645769767,-20.1635223036657));
#67495=CARTESIAN_POINT('Ctrl Pts',(0.215600419622202,7.91302922943297,-20.1490539038602));
#67496=CARTESIAN_POINT('Ctrl Pts',(-0.0649401045239018,7.91569984903088,
-20.1380206206928));
#67497=CARTESIAN_POINT('Ctrl Pts',(-0.639643343900182,7.89061083529653,
-20.1156667564884));
#67498=CARTESIAN_POINT('Ctrl Pts',(-0.933311067778316,7.86128623828794,
-20.1044037217539));
#67499=CARTESIAN_POINT('Ctrl Pts',(-1.82792646956006,7.72110540766969,-20.0703143704002));
#67500=CARTESIAN_POINT('Ctrl Pts',(-2.41817208514105,7.55705879066635,-20.0483120900414));
#67501=CARTESIAN_POINT('Ctrl Pts',(-3.08885099284436,7.28394307118575,-20.0203255745988));
#67502=CARTESIAN_POINT('Ctrl Pts',(-3.19312895352406,7.23883646009229,-20.0158755225567));
#67503=CARTESIAN_POINT('Ctrl Pts',(-3.31225883538221,7.18423043099901,-20.0106431194425));
#67504=CARTESIAN_POINT('Ctrl Pts',(-3.32809696755596,7.17690713657648,-20.0099444070972));
#67505=CARTESIAN_POINT('Ctrl Pts',(-3.3516006379828,7.16594488976823,-20.0089027850107));
#67506=CARTESIAN_POINT('Ctrl Pts',(-3.35928481703079,7.16234588086196,-20.0085614869611));
#67507=CARTESIAN_POINT('Ctrl Pts',(-3.37295154594217,7.15591801672306,-20.0079531021217));
#67508=CARTESIAN_POINT('Ctrl Pts',(-3.3789363717086,7.15309400112611,-20.007686215285));
#67509=CARTESIAN_POINT('Ctrl Pts',(-3.39138667930302,7.14720005445859,-20.0071300202941));
#67510=CARTESIAN_POINT('Ctrl Pts',(-3.39785155057423,7.14412885289988,-20.0068406588782));
#67511=CARTESIAN_POINT('Ctrl Pts',(-3.41455121985151,7.13616771311956,-20.0060917422371));
#67512=CARTESIAN_POINT('Ctrl Pts',(-3.42477966353301,7.13126453844267,-20.0056316202277));
#67513=CARTESIAN_POINT('Ctrl Pts',(-3.4470461926375,7.1205317530212,-20.0046268153225));
#67514=CARTESIAN_POINT('Ctrl Pts',(-3.45908009589968,7.11469358350185,-20.0040817552548));
#67515=CARTESIAN_POINT('Ctrl Pts',(-3.49381540859763,7.09773301505479,-20.0025024848242));
#67516=CARTESIAN_POINT('Ctrl Pts',(-3.51647824851522,7.08653235149519,-20.0014646998304));
#67517=CARTESIAN_POINT('Ctrl Pts',(-3.59182246232518,7.04884453572608,-19.9979886251268));
#67518=CARTESIAN_POINT('Ctrl Pts',(-3.64425795769325,7.02187877165575,-19.9955260730928));
#67519=CARTESIAN_POINT('Ctrl Pts',(-3.79644369257797,6.94145110721241,-19.9882509253494));
#67520=CARTESIAN_POINT('Ctrl Pts',(-3.89534975611109,6.88643425048212,-19.9833636578857));
#67521=CARTESIAN_POINT('Ctrl Pts',(-4.15843189702593,6.73261256767019,-19.9699904613795));
#67522=CARTESIAN_POINT('Ctrl Pts',(-4.32025233356039,6.62993530937215,-19.9613630088308));
#67523=CARTESIAN_POINT('Ctrl Pts',(-5.20800532617891,6.02033268589059,-19.9122868539698));
#67524=CARTESIAN_POINT('Ctrl Pts',(-5.84873270579262,5.40006087464299,-19.8708966477332));
#67525=CARTESIAN_POINT('Ctrl Pts',(-6.40518822040254,4.6433137385199,-19.832356961059));
#67526=CARTESIAN_POINT('Ctrl Pts',(-6.43652691076983,4.59977391635259,-19.8301721881629));
#67527=CARTESIAN_POINT('Ctrl Pts',(-6.4764374973016,4.54311825549699,-19.8273706722278));
#67528=CARTESIAN_POINT('Ctrl Pts',(-6.48541629094354,4.53029156639412,-19.8267391252944));
#67529=CARTESIAN_POINT('Ctrl Pts',(-6.4996235356568,4.50986695546707,-19.8257377576288));
#67530=CARTESIAN_POINT('Ctrl Pts',(-6.50487685933413,4.5022864310135,-19.8253670355673));
#67531=CARTESIAN_POINT('Ctrl Pts',(-6.51468935099316,4.48807402203607,-19.8246737230017));
#67532=CARTESIAN_POINT('Ctrl Pts',(-6.51925167618946,4.48144433750892,-19.8243510185478));
#67533=CARTESIAN_POINT('Ctrl Pts',(-6.52950041363925,4.46650274497195,-19.8236253104933));
#67534=CARTESIAN_POINT('Ctrl Pts',(-6.53518109112651,4.45818691057923,-19.8232225140185));
#67535=CARTESIAN_POINT('Ctrl Pts',(-6.55185361480285,4.43367998177417,-19.8220386899065));
#67536=CARTESIAN_POINT('Ctrl Pts',(-6.56280131433924,4.41745887199966,-19.8212592504074));
#67537=CARTESIAN_POINT('Ctrl Pts',(-6.6459007821758,4.29334036322256,-19.8153264868713));
#67538=CARTESIAN_POINT('Ctrl Pts',(-6.71544918506046,4.18371997009637,-19.8102668042333));
#67539=CARTESIAN_POINT('Ctrl Pts',(-6.94681541375455,3.79840048862551,-19.7930562095523));
#67540=CARTESIAN_POINT('Ctrl Pts',(-7.09460717086365,3.51463503813587,-19.7813853119961));
#67541=CARTESIAN_POINT('Ctrl Pts',(-7.50517421057323,2.59420017488285,-19.7456294864979));
#67542=CARTESIAN_POINT('Ctrl Pts',(-7.70228771360618,1.93187450202906,-19.7230618850797));
#67543=CARTESIAN_POINT('Ctrl Pts',(-7.81624069148619,1.22119047998754,-19.6963157695708));
#67544=CARTESIAN_POINT('Ctrl Pts',(-7.82106856198937,1.18987867115268,-19.695131962656));
#67545=CARTESIAN_POINT('Ctrl Pts',(-7.84670891033747,1.01668304255297,-19.6885506142617));
#67546=CARTESIAN_POINT('Ctrl Pts',(-7.86384841622122,0.874284321794345,
-19.6830143443933));
#67547=CARTESIAN_POINT('Ctrl Pts',(-7.87855451215898,0.715922114166429,
-19.6766601378556));
#67548=CARTESIAN_POINT('Ctrl Pts',(-7.87995466513111,0.700342876605951,
-19.6760330519743));
#67549=CARTESIAN_POINT('Ctrl Pts',(-7.88193677708997,0.677529564703679,
-19.6751119937283));
#67550=CARTESIAN_POINT('Ctrl Pts',(-7.88255500705428,0.670298612067288,
-19.6748196429958));
#67551=CARTESIAN_POINT('Ctrl Pts',(-7.88363349613805,0.657476517706844,
-19.6743005247235));
#67552=CARTESIAN_POINT('Ctrl Pts',(-7.884097760239,0.651885710478061,-19.6740739330226));
#67553=CARTESIAN_POINT('Ctrl Pts',(-7.88498146399501,0.64110484721572,-19.6736365332979));
#67554=CARTESIAN_POINT('Ctrl Pts',(-7.88540172745599,0.635914859959239,
-19.673425761003));
#67555=CARTESIAN_POINT('Ctrl Pts',(-7.88629143351192,0.624791050197756,
-19.6729735747339));
#67556=CARTESIAN_POINT('Ctrl Pts',(-7.88675930346327,0.618857107622825,
-19.6727320938206));
#67557=CARTESIAN_POINT('Ctrl Pts',(-7.88787011912322,0.604562892913924,
-19.6721497652962));
#67558=CARTESIAN_POINT('Ctrl Pts',(-7.8885064702552,0.596202126489903,-19.6718086410937));
#67559=CARTESIAN_POINT('Ctrl Pts',(-7.89018885139518,0.573623679986948,
-19.6708860596147));
#67560=CARTESIAN_POINT('Ctrl Pts',(-7.89120974098865,0.559404198269232,
-19.6703035712985));
#67561=CARTESIAN_POINT('Ctrl Pts',(-7.90459781270049,0.365595129320806,
-19.6623451071192));
#67562=CARTESIAN_POINT('Ctrl Pts',(-7.91086946006672,0.185645462909779,
-19.6547319091537));
#67563=CARTESIAN_POINT('Ctrl Pts',(-7.91099798332788,0.00564869739125604,
-19.6469874507044));
#67564=CARTESIAN_POINT('',(-7.911,-6.46926956449079E-12,-17.6423315082367));
#67565=CARTESIAN_POINT('Ctrl Pts',(-7.91099783789749,0.00584882734057925,
-19.6423315082367));
#67566=CARTESIAN_POINT('Ctrl Pts',(-7.91113802130119,-0.183760224007458,
-19.6346827876976));
#67567=CARTESIAN_POINT('Ctrl Pts',(-7.90445733796416,-0.373649153007014,
-19.6270340671585));
#67568=CARTESIAN_POINT('Ctrl Pts',(-7.89092201232192,-0.563267960613193,
-19.6193853466194));
#67569=CARTESIAN_POINT('Ctrl Pts',(-7.87739780900031,-0.752730953632383,
-19.6117429112282));
#67570=CARTESIAN_POINT('Ctrl Pts',(-7.85703019670372,-0.941923902422047,
-19.6041004758369));
#67571=CARTESIAN_POINT('Ctrl Pts',(-7.82983741969774,-1.13029508585197,
-19.5964580404456));
#67572=CARTESIAN_POINT('Ctrl Pts',(-7.80266318855097,-1.31853779746571,
-19.5888208173035));
#67573=CARTESIAN_POINT('Ctrl Pts',(-7.76867311292221,-1.50595949675737,
-19.5811835941614));
#67574=CARTESIAN_POINT('Ctrl Pts',(-7.72793739081847,-1.69201202229472,
-19.5735463710194));
#67575=CARTESIAN_POINT('Ctrl Pts',(-7.68721797603965,-1.87799006728208,
-19.5659122052106));
#67576=CARTESIAN_POINT('Ctrl Pts',(-7.63975836785712,-2.06259967049416,
-19.5582780394018));
#67577=CARTESIAN_POINT('Ctrl Pts',(-7.58568014811566,-2.24530124715681,
-19.550643873593));
#67578=CARTESIAN_POINT('Ctrl Pts',(-7.53160837032525,-2.42798105988905,
-19.5430106171877));
#67579=CARTESIAN_POINT('Ctrl Pts',(-7.47091965012036,-2.6087529442751,-19.5353773607825));
#67580=CARTESIAN_POINT('Ctrl Pts',(-7.40378590223481,-2.78709083344427,
-19.5277441043772));
#67581=CARTESIAN_POINT('Ctrl Pts',(-7.36710136042364,-2.88454172748486,
-19.5235729904058));
#67582=CARTESIAN_POINT('Ctrl Pts',(-7.32849322939946,-2.98126610392669,
-19.5194018764345));
#67583=CARTESIAN_POINT('Ctrl Pts',(-7.28799573871105,-3.07718038348901,
-19.5152307624631));
#67584=CARTESIAN_POINT('Ctrl Pts',(-7.20528000829565,-3.27308436559757,
-19.5067113027899));
#67585=CARTESIAN_POINT('Ctrl Pts',(-7.11473925117085,-3.46546708114613,
-19.4981918431167));
#67586=CARTESIAN_POINT('Ctrl Pts',(-7.01670438443082,-3.65373515481204,
-19.4896723834434));
#67587=CARTESIAN_POINT('Ctrl Pts',(-6.91849296434608,-3.84234228497093,
-19.4811375808708));
#67588=CARTESIAN_POINT('Ctrl Pts',(-6.81276057591704,-4.02681974194158,
-19.4726027782982));
#67589=CARTESIAN_POINT('Ctrl Pts',(-6.69988251509191,-4.20660139352016,
-19.4640679757255));
#67590=CARTESIAN_POINT('Ctrl Pts',(-6.58129166582463,-4.39548184192196,
-19.4551012245427));
#67591=CARTESIAN_POINT('Ctrl Pts',(-6.45481338712476,-4.57917861971122,
-19.4461344733599));
#67592=CARTESIAN_POINT('Ctrl Pts',(-6.32093037625521,-4.75707475015205,
-19.4371677221771));
#67593=CARTESIAN_POINT('Ctrl Pts',(-6.19296462642121,-4.9271083606645,-19.4285972767469));
#67594=CARTESIAN_POINT('Ctrl Pts',(-6.05823472329184,-5.09184284991683,
-19.4200268313167));
#67595=CARTESIAN_POINT('Ctrl Pts',(-5.91720073374702,-5.2507767498289,-19.4114563858865));
#67596=CARTESIAN_POINT('Ctrl Pts',(-5.77599050341171,-5.40990925885814,
-19.4028752305411));
#67597=CARTESIAN_POINT('Ctrl Pts',(-5.62846061755716,-5.56322651463609,
-19.3942940751957));
#67598=CARTESIAN_POINT('Ctrl Pts',(-5.47510771234711,-5.71026413909175,
-19.3857129198502));
#67599=CARTESIAN_POINT('Ctrl Pts',(-5.3214996561415,-5.8575464070787,-19.3771174870425));
#67600=CARTESIAN_POINT('Ctrl Pts',(-5.16204939113485,-5.99852798302639,
-19.3685220542347));
#67601=CARTESIAN_POINT('Ctrl Pts',(-4.99728797132674,-6.13278353862527,
-19.3599266214269));
#67602=CARTESIAN_POINT('Ctrl Pts',(-4.97518249240011,-6.15079614957831,
-19.3587734014618));
#67603=CARTESIAN_POINT('Ctrl Pts',(-4.95298145337977,-6.16868775034689,
-19.3576201814967));
#67604=CARTESIAN_POINT('Ctrl Pts',(-4.93068617731446,-6.18645737242568,
-19.3564669615317));
#67605=CARTESIAN_POINT('Ctrl Pts',(-4.77778048606164,-6.30832517703603,
-19.3485579365252));
#67606=CARTESIAN_POINT('Ctrl Pts',(-4.6201590200985,-6.42467610326622,-19.3406489115187));
#67607=CARTESIAN_POINT('Ctrl Pts',(-4.45825686135297,-6.53512561150887,
-19.3327398865122));
#67608=CARTESIAN_POINT('Ctrl Pts',(-4.29651973706778,-6.64546253338993,
-19.3248389235457));
#67609=CARTESIAN_POINT('Ctrl Pts',(-4.13051089421535,-6.74990982709944,
-19.3169379605792));
#67610=CARTESIAN_POINT('Ctrl Pts',(-3.96069883546253,-6.84812278911278,
-19.3090369976126));
#67611=CARTESIAN_POINT('Ctrl Pts',(-3.79102837255323,-6.94625385737073,
-19.3011426227737));
#67612=CARTESIAN_POINT('Ctrl Pts',(-3.61756130816164,-7.03816077831389,
-19.2932482479349));
#67613=CARTESIAN_POINT('Ctrl Pts',(-3.44079574015724,-7.12354165247286,
-19.285353873096));
#67614=CARTESIAN_POINT('Ctrl Pts',(-3.26414478364301,-7.20886716726898,
-19.2774646168222));
#67615=CARTESIAN_POINT('Ctrl Pts',(-3.08419989400257,-7.28767491644094,
-19.2695753605483));
#67616=CARTESIAN_POINT('Ctrl Pts',(-2.90148467407429,-7.35970839681247,
-19.2616861042745));
#67617=CARTESIAN_POINT('Ctrl Pts',(-2.7188540441519,-7.43170852849783,-19.253800500418));
#67618=CARTESIAN_POINT('Ctrl Pts',(-2.53345595980279,-7.49694051474591,
-19.2459148965616));
#67619=CARTESIAN_POINT('Ctrl Pts',(-2.34583521100266,-7.55519544173545,
-19.2380292927051));
#67620=CARTESIAN_POINT('Ctrl Pts',(-2.14846392638771,-7.61647784172909,
-19.2297338788286));
#67621=CARTESIAN_POINT('Ctrl Pts',(-1.94863317336111,-7.67003852780308,
-19.221438464952));
#67622=CARTESIAN_POINT('Ctrl Pts',(-1.74699756297276,-7.71569313250386,
-19.2131430510755));
#67623=CARTESIAN_POINT('Ctrl Pts',(-1.55535481583135,-7.75908513973741,
-19.2052587497812));
#67624=CARTESIAN_POINT('Ctrl Pts',(-1.36208214175197,-7.79533564831999,
-19.1973744484868));
#67625=CARTESIAN_POINT('Ctrl Pts',(-1.16775388967623,-7.82433842910351,
-19.1894901471925));
#67626=CARTESIAN_POINT('Ctrl Pts',(-0.973400300964404,-7.8533449912873,
-19.1816048179381));
#67627=CARTESIAN_POINT('Ctrl Pts',(-0.777991201150984,-7.87510189115162,
-19.1737194886838));
#67628=CARTESIAN_POINT('Ctrl Pts',(-0.582108008285773,-7.88955456706458,
-19.1658341594294));
#67629=CARTESIAN_POINT('Ctrl Pts',(-0.386166365426575,-7.90401155554162,
-19.1579464772552));
#67630=CARTESIAN_POINT('Ctrl Pts',(-0.189750691524313,-7.9111599514527,
-19.1500587950811));
#67631=CARTESIAN_POINT('Ctrl Pts',(0.00655538566710729,-7.91099728396608,
-19.1421711129069));
#67632=CARTESIAN_POINT('Ctrl Pts',(0.202953021448065,-7.91083454061016,
-19.1342797518601));
#67633=CARTESIAN_POINT('Ctrl Pts',(0.399240614178055,-7.90335393913915,
-19.1263883908132));
#67634=CARTESIAN_POINT('Ctrl Pts',(0.594837203384454,-7.88860505422028,
-19.1184970297664));
#67635=CARTESIAN_POINT('Ctrl Pts',(0.79065918549798,-7.87383917363671,-19.1105965752236));
#67636=CARTESIAN_POINT('Ctrl Pts',(0.985788229800109,-7.85178830674623,
-19.1026961206807));
#67637=CARTESIAN_POINT('Ctrl Pts',(1.17965000407716,-7.82255373058445,-19.0947956661379));
#67638=CARTESIAN_POINT('Ctrl Pts',(1.37364143181113,-7.79329960253384,-19.0868899278239));
#67639=CARTESIAN_POINT('Ctrl Pts',(1.56636356226909,-7.75685225133657,-19.07898418951));
#67640=CARTESIAN_POINT('Ctrl Pts',(1.75725460729995,-7.7133635493942,-19.071078451196));
#67641=CARTESIAN_POINT('Ctrl Pts',(1.94840298754163,-7.66981622147343,-19.0631620553636));
#67642=CARTESIAN_POINT('Ctrl Pts',(2.13771502059222,-7.61920867337019,-19.0552456595312));
#67643=CARTESIAN_POINT('Ctrl Pts',(2.32464528458301,-7.5617422133306,-19.0473292636988));
#67644=CARTESIAN_POINT('Ctrl Pts',(2.3906823637629,-7.54144096787786,-19.0445326290221));
#67645=CARTESIAN_POINT('Ctrl Pts',(2.45642238919231,-7.52028416092685,-19.0417359943454));
#67646=CARTESIAN_POINT('Ctrl Pts',(2.5218419829114,-7.49828207079632,-19.0389393596686));
#67647=CARTESIAN_POINT('Ctrl Pts',(2.70340762271942,-7.43721743641755,-19.0311775755376));
#67648=CARTESIAN_POINT('Ctrl Pts',(2.88307273704098,-7.36944680384386,-19.0234157914066));
#67649=CARTESIAN_POINT('Ctrl Pts',(3.06029198926213,-7.29510342219067,-19.0156540072756));
#67650=CARTESIAN_POINT('Ctrl Pts',(3.23729843544195,-7.22084931255816,-19.0079015435459));
#67651=CARTESIAN_POINT('Ctrl Pts',(3.41186453889488,-7.14003830056088,-19.0001490798162));
#67652=CARTESIAN_POINT('Ctrl Pts',(3.58345834686008,-7.05285383914333,-18.9923966160865));
#67653=CARTESIAN_POINT('Ctrl Pts',(3.75488090624852,-6.96575638677996,-18.9846518892232));
#67654=CARTESIAN_POINT('Ctrl Pts',(3.92333675815459,-6.8722983081147,-18.97690716236));
#67655=CARTESIAN_POINT('Ctrl Pts',(4.08831214060738,-6.77271177896729,-18.9691624354968));
#67656=CARTESIAN_POINT('Ctrl Pts',(4.25315629166039,-6.67320446696989,-18.9614238692578));
#67657=CARTESIAN_POINT('Ctrl Pts',(4.41452517995679,-6.56757859470346,-18.9536853030189));
#67658=CARTESIAN_POINT('Ctrl Pts',(4.57192787432426,-6.45611311177065,-18.94594673678));
#67659=CARTESIAN_POINT('Ctrl Pts',(4.72923720705595,-6.34471374333391,-18.9382127605844));
#67660=CARTESIAN_POINT('Ctrl Pts',(4.88258473843477,-6.22748186813724,-18.9304787843889));
#67661=CARTESIAN_POINT('Ctrl Pts',(5.03150679496644,-6.10474081122259,-18.9227448081934));
#67662=CARTESIAN_POINT('Ctrl Pts',(5.18037062940206,-5.9820477407632,-18.9150138556488));
#67663=CARTESIAN_POINT('Ctrl Pts',(5.32481215843983,-5.85385000631522,-18.9072829031041));
#67664=CARTESIAN_POINT('Ctrl Pts',(5.4643991360204,-5.72051248423247,-18.8995519505595));
#67665=CARTESIAN_POINT('Ctrl Pts',(5.60398630974189,-5.58717477479024,-18.8918209871516));
#67666=CARTESIAN_POINT('Ctrl Pts',(5.73871865104356,-5.44869750295523,-18.8840900237438));
#67667=CARTESIAN_POINT('Ctrl Pts',(5.86819898947908,-5.3054841079657,-18.876359060336));
#67668=CARTESIAN_POINT('Ctrl Pts',(5.99768603071206,-5.16226329926077,-18.8686276967201));
#67669=CARTESIAN_POINT('Ctrl Pts',(6.12192028602957,-5.01430614496696,-18.8608963331042));
#67670=CARTESIAN_POINT('Ctrl Pts',(6.24054340776541,-4.86205090222179,-18.8531649694882));
#67671=CARTESIAN_POINT('Ctrl Pts',(6.35919439181006,-4.70975989762404,-18.8454317899224));
#67672=CARTESIAN_POINT('Ctrl Pts',(6.47223139693797,-4.55316907739557,-18.8376986103567));
#67673=CARTESIAN_POINT('Ctrl Pts',(6.57933809314507,-4.39274757482036,-18.8299654307909));
#67674=CARTESIAN_POINT('Ctrl Pts',(6.68648956562127,-4.23225900756459,-18.8222290183467));
#67675=CARTESIAN_POINT('Ctrl Pts',(6.78770559325239,-4.06793686735429,-18.8144926059024));
#67676=CARTESIAN_POINT('Ctrl Pts',(6.88271464792874,-3.90027692288474,-18.8067561934582));
#67677=CARTESIAN_POINT('Ctrl Pts',(6.97783676124531,-3.73241746684855,-18.799010574857));
#67678=CARTESIAN_POINT('Ctrl Pts',(7.06673697369494,-3.56121258662182,-18.7912649562558));
#67679=CARTESIAN_POINT('Ctrl Pts',(7.14919052248813,-3.38718111018084,-18.7835193376546));
#67680=CARTESIAN_POINT('Ctrl Pts',(7.23169768157617,-3.21303648058998,-18.7757686829464));
#67681=CARTESIAN_POINT('Ctrl Pts',(7.30774968655235,-3.03606192241102,-18.7680180282382));
#67682=CARTESIAN_POINT('Ctrl Pts',(7.37717098864852,-2.85679351795727,-18.7602673735299));
#67683=CARTESIAN_POINT('Ctrl Pts',(7.44669775289354,-2.67725277589842,-18.7525049443278));
#67684=CARTESIAN_POINT('Ctrl Pts',(7.50957357984035,-2.49541156571472,-18.7447425151256));
#67685=CARTESIAN_POINT('Ctrl Pts',(7.56567325283131,-2.31181946340817,-18.7369800859235));
#67686=CARTESIAN_POINT('Ctrl Pts',(7.60317775447997,-2.18908202241193,-18.7317906432175));
#67687=CARTESIAN_POINT('Ctrl Pts',(7.63765480311116,-2.06556226457843,-18.7266012005115));
#67688=CARTESIAN_POINT('Ctrl Pts',(7.66907988485672,-1.94142595009081,-18.7214117578056));
#67689=CARTESIAN_POINT('Ctrl Pts',(7.71761344961894,-1.74970718521032,-18.713397072094));
#67690=CARTESIAN_POINT('Ctrl Pts',(7.75901339732821,-1.55593159817677,-18.7053823863825));
#67691=CARTESIAN_POINT('Ctrl Pts',(7.79310652659695,-1.36066589033168,-18.697367700671));
#67692=CARTESIAN_POINT('Ctrl Pts',(7.82716089650987,-1.16562217363877,-18.6893621265916));
#67693=CARTESIAN_POINT('Ctrl Pts',(7.85392494334617,-0.969092038447004,
-18.6813565525123));
#67694=CARTESIAN_POINT('Ctrl Pts',(7.87327554829636,-0.77165610254738,-18.673350978433));
#67695=CARTESIAN_POINT('Ctrl Pts',(7.89260743555861,-0.57441114487542,-18.6653531480826));
#67696=CARTESIAN_POINT('Ctrl Pts',(7.90454013903864,-0.376262463360862,
-18.6573553177321));
#67697=CARTESIAN_POINT('Ctrl Pts',(7.90900171680268,-0.177800010158159,
-18.6493574873816));
#67698=CARTESIAN_POINT('Ctrl Pts',(7.9134597349997,0.0205041043489301,-18.6413660379158));
#67699=CARTESIAN_POINT('Ctrl Pts',(7.9104584999826,0.21912115868565,-18.63337458845));
#67700=CARTESIAN_POINT('Ctrl Pts',(7.89997791425322,0.417456529846294,-18.6253831389842));
#67701=CARTESIAN_POINT('Ctrl Pts',(7.8895039150739,0.615667256651865,-18.6173967117646));
#67702=CARTESIAN_POINT('Ctrl Pts',(7.8715599522246,0.813596320106642,-18.609410284545));
#67703=CARTESIAN_POINT('Ctrl Pts',(7.84617800799023,1.01064913146475,-18.6014238573254));
#67704=CARTESIAN_POINT('Ctrl Pts',(7.82001934766407,1.21373198087282,-18.5931930364344));
#67705=CARTESIAN_POINT('Ctrl Pts',(7.7859602545851,1.41588373550776,-18.5849622155435));
#67706=CARTESIAN_POINT('Ctrl Pts',(7.74409353569296,1.61645795195499,-18.5767313946525));
#67707=CARTESIAN_POINT('Ctrl Pts',(7.70349725826311,1.8109457635541,-18.568750337211));
#67708=CARTESIAN_POINT('Ctrl Pts',(7.6555603371452,2.00395002689001,-18.5607692797695));
#67709=CARTESIAN_POINT('Ctrl Pts',(7.60041950030024,2.19489052561985,-18.5527882223281));
#67710=CARTESIAN_POINT('Ctrl Pts',(7.54528297267458,2.38581610247822,-18.5448077886008));
#67711=CARTESIAN_POINT('Ctrl Pts',(7.48294374411727,2.57467791485703,-18.5368273548736));
#67712=CARTESIAN_POINT('Ctrl Pts',(7.41358873430394,2.76090982804612,-18.5288469211464));
#67713=CARTESIAN_POINT('Ctrl Pts',(7.34422849772688,2.94715577612921,-18.5208658859941));
#67714=CARTESIAN_POINT('Ctrl Pts',(7.26785154308614,3.13077111664938,-18.5128848508418));
#67715=CARTESIAN_POINT('Ctrl Pts',(7.18469349463499,3.31120829730623,-18.5049038156896));
#67716=CARTESIAN_POINT('Ctrl Pts',(7.10151641325563,3.49168677580462,-18.4969209538654));
#67717=CARTESIAN_POINT('Ctrl Pts',(7.01155528492848,3.66898534109895,-18.4889380920412));
#67718=CARTESIAN_POINT('Ctrl Pts',(6.91509253864822,3.84257936572971,-18.4809552302171));
#67719=CARTESIAN_POINT('Ctrl Pts',(6.81855821179896,4.01630220650492,-18.4729664446781));
#67720=CARTESIAN_POINT('Ctrl Pts',(6.71551279225942,4.18631472288134,-18.4649776591392));
#67721=CARTESIAN_POINT('Ctrl Pts',(6.60628357838913,4.35211882672178,-18.4569888736003));
#67722=CARTESIAN_POINT('Ctrl Pts',(6.49700619189741,4.51799605402472,-18.4489965648214));
#67723=CARTESIAN_POINT('Ctrl Pts',(6.38153976407568,4.67966089379926,-18.4410042560424));
#67724=CARTESIAN_POINT('Ctrl Pts',(6.26025338279326,4.8366464190827,-18.4330119472634));
#67725=CARTESIAN_POINT('Ctrl Pts',(6.1388535141161,4.99377883536981,-18.4250121600991));
#67726=CARTESIAN_POINT('Ctrl Pts',(6.011623027214,5.14622293407631,-18.4170123729347));
#67727=CARTESIAN_POINT('Ctrl Pts',(5.8789701684774,5.29354614206326,-18.4090125857704));
#67728=CARTESIAN_POINT('Ctrl Pts',(5.85062354443516,5.3250276768698,-18.4073031091611));
#67729=CARTESIAN_POINT('Ctrl Pts',(5.82202944664807,5.35627551060089,-18.4055936325518));
#67730=CARTESIAN_POINT('Ctrl Pts',(5.79319206789574,5.38728564905091,-18.4038841559425));
#67731=CARTESIAN_POINT('Ctrl Pts',(5.65609027711756,5.53471740941624,-18.3957567770139));
#67732=CARTESIAN_POINT('Ctrl Pts',(5.51324576239915,5.67703248099569,-18.3876293980853));
#67733=CARTESIAN_POINT('Ctrl Pts',(5.36506658550671,5.81377515329578,-18.3795020191568));
#67734=CARTESIAN_POINT('Ctrl Pts',(5.21701325071332,5.95040169602036,-18.3713815424559));
#67735=CARTESIAN_POINT('Ctrl Pts',(5.06363451910478,6.08146505899225,-18.3632610657551));
#67736=CARTESIAN_POINT('Ctrl Pts',(4.90537614374601,6.20654540693674,-18.3551405890542));
#67737=CARTESIAN_POINT('Ctrl Pts',(4.74723227226892,6.33153525612987,-18.3470259877208));
#67738=CARTESIAN_POINT('Ctrl Pts',(4.5842160457718,6.45055052450131,-18.3389113863874));
#67739=CARTESIAN_POINT('Ctrl Pts',(4.41680765496922,6.56321042927966,-18.3307967850539));
#67740=CARTESIAN_POINT('Ctrl Pts',(4.24951786113322,6.67579052250915,-18.3226879323398));
#67741=CARTESIAN_POINT('Ctrl Pts',(4.07784237442878,6.78202405691186,-18.3145790796256));
#67742=CARTESIAN_POINT('Ctrl Pts',(3.90229212802461,6.88157228746143,-18.3064702269115));
#67743=CARTESIAN_POINT('Ctrl Pts',(3.72681706449238,6.98107788450851,-18.2983648469742));
#67744=CARTESIAN_POINT('Ctrl Pts',(3.54747082680692,7.07390372955717,-18.290259467037));
#67745=CARTESIAN_POINT('Ctrl Pts',(3.36479155591205,7.15975549758949,-18.2821540870997));
#67746=CARTESIAN_POINT('Ctrl Pts',(3.18216924970129,7.24558049455566,-18.2740512346545));
#67747=CARTESIAN_POINT('Ctrl Pts',(2.99621627128487,7.32443561632654,-18.2659483822093));
#67748=CARTESIAN_POINT('Ctrl Pts',(2.80749398554382,7.3960731825162,-18.2578455297641));
#67749=CARTESIAN_POINT('Ctrl Pts',(2.70870062513665,7.43357440219186,-18.2536038048464));
#67750=CARTESIAN_POINT('Ctrl Pts',(2.60914873979467,7.46909852772734,-18.2493620799287));
#67751=CARTESIAN_POINT('Ctrl Pts',(2.50892104898112,7.50261528868297,-18.2451203550111));
#67752=CARTESIAN_POINT('Ctrl Pts',(2.31306241344616,7.56811163021332,-18.2368314435541));
#67753=CARTESIAN_POINT('Ctrl Pts',(2.11470623800062,7.62591149242828,-18.2285425320972));
#67754=CARTESIAN_POINT('Ctrl Pts',(1.91447278116729,7.67585271941623,-18.2202536206403));
#67755=CARTESIAN_POINT('Ctrl Pts',(1.71412420047218,7.7258226600218,-18.2119599434888));
#67756=CARTESIAN_POINT('Ctrl Pts',(1.51189646780863,7.76792487583658,-18.2036662663373));
#67757=CARTESIAN_POINT('Ctrl Pts',(1.30842066178171,7.80204821645077,-18.1953725891858));
#67758=CARTESIAN_POINT('Ctrl Pts',(1.10481561220036,7.83619323149357,-18.1870736440649));
#67759=CARTESIAN_POINT('Ctrl Pts',(0.899961195157141,7.86234920667333,-18.178774698944));
#67760=CARTESIAN_POINT('Ctrl Pts',(0.694495091660754,7.88045668522194,-18.1704757538232));
#67761=CARTESIAN_POINT('Ctrl Pts',(0.488790603065375,7.89858517236025,-18.1621671801318));
#67762=CARTESIAN_POINT('Ctrl Pts',(0.282473301148333,7.90864647170555,-18.1538586064405));
#67763=CARTESIAN_POINT('Ctrl Pts',(0.0761841028022858,7.9106331593925,-18.1455500327492));
#67764=CARTESIAN_POINT('Ctrl Pts',(-0.130232059834683,7.9126210698211,-18.137236345401));
#67765=CARTESIAN_POINT('Ctrl Pts',(-0.336619792044605,7.90652445229771,
-18.1289226580528));
#67766=CARTESIAN_POINT('Ctrl Pts',(-0.542340377132606,7.89238797293517,
-18.1206089707047));
#67767=CARTESIAN_POINT('Ctrl Pts',(-0.748284859284791,7.8782361080621,-18.1122862351118));
#67768=CARTESIAN_POINT('Ctrl Pts',(-0.953560451745752,7.85602691891948,
-18.103963499519));
#67769=CARTESIAN_POINT('Ctrl Pts',(-1.157534112256,7.82585687186801,-18.0956407639262));
#67770=CARTESIAN_POINT('Ctrl Pts',(-1.23337993827666,7.81463840310113,-18.0925460273106));
#67771=CARTESIAN_POINT('Ctrl Pts',(-1.3090458505169,7.8023197274721,-18.089451290695));
#67772=CARTESIAN_POINT('Ctrl Pts',(-1.38449969906905,7.78890759884066,-18.0863565540795));
#67773=CARTESIAN_POINT('Ctrl Pts',(-1.59654817636536,7.75121540012354,-18.0776593941658));
#67774=CARTESIAN_POINT('Ctrl Pts',(-1.80710879533676,7.70485031972598,-18.0689622342521));
#67775=CARTESIAN_POINT('Ctrl Pts',(-2.0154962282987,7.64994744777464,-18.0602650743384));
#67776=CARTESIAN_POINT('Ctrl Pts',(-2.22370115450324,7.59509266003351,-18.0515755314409));
#67777=CARTESIAN_POINT('Ctrl Pts',(-2.4297364738889,7.53171506966302,-18.0428859885434));
#67778=CARTESIAN_POINT('Ctrl Pts',(-2.63292905642381,7.46000037425195,-18.0341964456459));
#67779=CARTESIAN_POINT('Ctrl Pts',(-2.84066034756584,7.3866837891397,-18.0253128046044));
#67780=CARTESIAN_POINT('Ctrl Pts',(-3.04542018780775,7.30465333833933,-18.0164291635629));
#67781=CARTESIAN_POINT('Ctrl Pts',(-3.24650425733365,7.21416184370121,-18.0075455225214));
#67782=CARTESIAN_POINT('Ctrl Pts',(-3.44261811569614,7.12590703463398,-17.998881459152));
#67783=CARTESIAN_POINT('Ctrl Pts',(-3.63523550764216,7.02960454536081,-17.9902173957826));
#67784=CARTESIAN_POINT('Ctrl Pts',(-3.82372031978712,6.9255385289555,-17.9815533324132));
#67785=CARTESIAN_POINT('Ctrl Pts',(-4.01937042860175,6.81751641724314,-17.9725599025357));
#67786=CARTESIAN_POINT('Ctrl Pts',(-4.21056738759096,6.70112903845224,-17.9635664726581));
#67787=CARTESIAN_POINT('Ctrl Pts',(-4.39662304927001,6.5767489508592,-17.9545730427806));
#67788=CARTESIAN_POINT('Ctrl Pts',(-4.58267871094901,6.45236886326621,-17.9455796129031));
#67789=CARTESIAN_POINT('Ctrl Pts',(-4.76359280865984,6.31999616555474,-17.9365861830256));
#67790=CARTESIAN_POINT('Ctrl Pts',(-4.93870489993438,6.18005784045458,-17.9275927531481));
#67791=CARTESIAN_POINT('Ctrl Pts',(-5.09081459798682,6.05850154915556,-17.9197806832152));
#67792=CARTESIAN_POINT('Ctrl Pts',(-5.23848061369682,5.9312886315483,-17.9119686132824));
#67793=CARTESIAN_POINT('Ctrl Pts',(-5.3812619697026,5.79878785725366,-17.9041565433495));
#67794=CARTESIAN_POINT('Ctrl Pts',(-5.52403314308139,5.66629653241375,-17.896345030544));
#67795=CARTESIAN_POINT('Ctrl Pts',(-5.66192009263191,5.52851834151829,-17.8885335177385));
#67796=CARTESIAN_POINT('Ctrl Pts',(-5.79451699852455,5.38586053976614,-17.880722004933));
#67797=CARTESIAN_POINT('Ctrl Pts',(-5.92712783037265,5.24318775541558,-17.8729096717253));
#67798=CARTESIAN_POINT('Ctrl Pts',(-6.05444727286243,5.09563459783802,-17.8650973385177));
#67799=CARTESIAN_POINT('Ctrl Pts',(-6.1761081695767,4.94364327977737,-17.8572850053101));
#67800=CARTESIAN_POINT('Ctrl Pts',(-6.29785525627783,4.79154428431124,-17.8494671374984));
#67801=CARTESIAN_POINT('Ctrl Pts',(-6.41393556804186,4.63500112189215,-17.8416492696867));
#67802=CARTESIAN_POINT('Ctrl Pts',(-6.52402334711459,4.47448772110324,-17.833831401875));
#67803=CARTESIAN_POINT('Ctrl Pts',(-6.63415186333711,4.31391492354473,-17.8260106411204));
#67804=CARTESIAN_POINT('Ctrl Pts',(-6.7382832372243,4.14936925564053,-17.8181898803659));
#67805=CARTESIAN_POINT('Ctrl Pts',(-6.83613641550175,3.98135151784552,-17.8103691196113));
#67806=CARTESIAN_POINT('Ctrl Pts',(-6.93409798510463,3.81314766790154,-17.8025396958513));
#67807=CARTESIAN_POINT('Ctrl Pts',(-7.02576729762717,3.64146437372884,-17.7947102720912));
#67808=CARTESIAN_POINT('Ctrl Pts',(-7.110909927966,3.46682578107908,-17.7868808483311));
#67809=CARTESIAN_POINT('Ctrl Pts',(-7.17634624294497,3.3326074005729,-17.7808635496262));
#67810=CARTESIAN_POINT('Ctrl Pts',(-7.2379284054702,3.19664390093214,-17.7748462509213));
#67811=CARTESIAN_POINT('Ctrl Pts',(-7.29556977223707,3.05918006962989,-17.7688289522165));
#67812=CARTESIAN_POINT('Ctrl Pts',(-7.38193387321683,2.85321791304765,-17.7598132292709));
#67813=CARTESIAN_POINT('Ctrl Pts',(-7.45958441345405,2.64356761115758,-17.7507975063253));
#67814=CARTESIAN_POINT('Ctrl Pts',(-7.52824618037755,2.43093201213667,-17.7417817833797));
#67815=CARTESIAN_POINT('Ctrl Pts',(-7.59675969153965,2.21875553984734,-17.7327855273505));
#67816=CARTESIAN_POINT('Ctrl Pts',(-7.65632314523847,2.00360679724776,-17.7237892713212));
#67817=CARTESIAN_POINT('Ctrl Pts',(-7.70671131020899,1.78620317464081,-17.7147930152919));
#67818=CARTESIAN_POINT('Ctrl Pts',(-7.75700744217116,1.56919663554395,-17.7058131907502));
#67819=CARTESIAN_POINT('Ctrl Pts',(-7.79816170520086,1.34994359437431,-17.6968333662085));
#67820=CARTESIAN_POINT('Ctrl Pts',(-7.82999912688721,1.12917433239761,-17.6878535416668));
#67821=CARTESIAN_POINT('Ctrl Pts',(-7.86171708867684,0.909233437538468,
-17.6789074110882));
#67822=CARTESIAN_POINT('Ctrl Pts',(-7.88418794059056,0.687787833739226,
-17.6699612805096));
#67823=CARTESIAN_POINT('Ctrl Pts',(-7.8972882567302,0.465574043639957,-17.661015149931));
#67824=CARTESIAN_POINT('Ctrl Pts',(-7.90640808832236,0.310879124711466,
-17.6547872693662));
#67825=CARTESIAN_POINT('Ctrl Pts',(-7.91098770773955,0.155812222309194,
-17.6485593888015));
#67826=CARTESIAN_POINT('Ctrl Pts',(-7.91099997528238,0.00062536565977314,
-17.6423315082367));
#67827=CARTESIAN_POINT('',(-7.91220373638543,-0.00240967797264085,-15.6423315082368));
#67828=CARTESIAN_POINT('Ctrl Pts',(-7.911,-6.46926956449079E-12,-17.6423315082367));
#67829=CARTESIAN_POINT('Ctrl Pts',(-7.9109999999982,-2.20167589667319,-17.553744072504));
#67830=CARTESIAN_POINT('Ctrl Pts',(-6.94214576672017,-4.38610418339242,
-17.4651566367713));
#67831=CARTESIAN_POINT('Ctrl Pts',(-3.67820201487702,-7.34180684107923,
-17.2879817653058));
#67832=CARTESIAN_POINT('Ctrl Pts',(-1.40868175871105,-8.08992666571447,
-17.1993943295731));
#67833=CARTESIAN_POINT('Ctrl Pts',(2.97309270521869,-7.65454228025025,-17.0222194581077));
#67834=CARTESIAN_POINT('Ctrl Pts',(5.05102072676101,-6.47444880833835,-16.933632022375));
#67835=CARTESIAN_POINT('Ctrl Pts',(7.66951518848094,-2.93425195367123,-16.7564571509095));
#67836=CARTESIAN_POINT('Ctrl Pts',(8.18956872247115,-0.601881960092998,
-16.6678697151768));
#67837=CARTESIAN_POINT('Ctrl Pts',(7.32306689761066,3.71537198232993,-16.4906948437113));
#67838=CARTESIAN_POINT('Ctrl Pts',(5.94329958849784,5.66643518936947,-16.4021074079786));
#67839=CARTESIAN_POINT('Ctrl Pts',(2.16154501637273,7.92205913233153,-16.2249325365132));
#67840=CARTESIAN_POINT('Ctrl Pts',(-0.21081652930626,8.20894963712986,-16.1363451007804));
#67841=CARTESIAN_POINT('Ctrl Pts',(-4.42123908576926,6.91982244717518,-15.959170229315));
#67842=CARTESIAN_POINT('Ctrl Pts',(-6.22631625634562,5.35390358803084,-15.8705827935823));
#67843=CARTESIAN_POINT('Ctrl Pts',(-7.6531728085966,2.31334857513963,-15.7354407413119));
#67844=CARTESIAN_POINT('Ctrl Pts',(-7.91100000000092,1.15702837835916,-15.6888861247743));
#67845=CARTESIAN_POINT('Ctrl Pts',(-7.911,-6.29885033021083E-12,-15.6423315082367));
#67846=CARTESIAN_POINT('',(-7.91330192014884,-0.000633965809683563,-13.6423315453791));
#67847=CARTESIAN_POINT('Ctrl Pts',(-7.91220373638543,-0.00240967797264085,
-15.6423315082368));
#67848=CARTESIAN_POINT('Ctrl Pts',(-7.91556428301706,-0.802155651716782,
-15.6102662518829));
#67849=CARTESIAN_POINT('Ctrl Pts',(-7.41652343406805,-4.23985998589394,
-15.4723584615749));
#67850=CARTESIAN_POINT('Ctrl Pts',(-3.58490407290004,-7.95466169869553,
-15.2815294042895));
#67851=CARTESIAN_POINT('Ctrl Pts',(1.86216543943451,-8.01303484465013,-15.0698443363806));
#67852=CARTESIAN_POINT('Ctrl Pts',(6.70329027487364,-5.57407882739102,-14.8581592684722));
#67853=CARTESIAN_POINT('Ctrl Pts',(9.25305049567197,1.41654005527499,-14.5935529335861));
#67854=CARTESIAN_POINT('Ctrl Pts',(3.7987038621997,8.54783779767953,-14.2760253317233));
#67855=CARTESIAN_POINT('Ctrl Pts',(-3.60029715467979,7.94008165336322,-14.0114189968371));
#67856=CARTESIAN_POINT('Ctrl Pts',(-7.24286590766586,3.91248402646697,-13.8001877347225));
#67857=CARTESIAN_POINT('Ctrl Pts',(-7.91272125770078,1.29905138717317,-13.6947990065622));
#67858=CARTESIAN_POINT('Ctrl Pts',(-7.91330192014884,-0.000633965809683564,
-13.6423315453791));
#67859=CARTESIAN_POINT('',(-7.9129081904216,0.00235452960061844,-11.64233118194));
#67860=CARTESIAN_POINT('Ctrl Pts',(-7.9109999745389,-0.000634701186066671,
-13.6423315082368));
#67861=CARTESIAN_POINT('Ctrl Pts',(-7.91099907293056,-0.011872467354115,
-13.6418777148235));
#67862=CARTESIAN_POINT('Ctrl Pts',(-7.91097422604346,-0.0231101033026613,
-13.6414239214103));
#67863=CARTESIAN_POINT('Ctrl Pts',(-7.91092543559937,-0.0343475237379891,
-13.6409701279972));
#67864=CARTESIAN_POINT('Ctrl Pts',(-7.90999034425114,-0.249717865650979,
-13.6322729680831));
#67865=CARTESIAN_POINT('Ctrl Pts',(-7.90025568575849,-0.46510294259373,
-13.623575808169));
#67866=CARTESIAN_POINT('Ctrl Pts',(-7.881737558672,-0.679804424977677,-13.614878648255));
#67867=CARTESIAN_POINT('Ctrl Pts',(-7.86323564985387,-0.894317870729024,
-13.6061891053571));
#67868=CARTESIAN_POINT('Ctrl Pts',(-7.83596565237483,-1.10814868945514,
-13.5974995624592));
#67869=CARTESIAN_POINT('Ctrl Pts',(-7.799995611737,-1.32060192975913,-13.5888100195613));
#67870=CARTESIAN_POINT('Ctrl Pts',(-7.76322210903109,-1.53780073378222,
-13.57992637852));
#67871=CARTESIAN_POINT('Ctrl Pts',(-7.71735535863239,-1.75355946069846,
-13.5710427374787));
#67872=CARTESIAN_POINT('Ctrl Pts',(-7.66252421961339,-1.96714096694624,
-13.5621590964374));
#67873=CARTESIAN_POINT('Ctrl Pts',(-7.60904834627638,-2.17544336189149,
-13.5534950330676));
#67874=CARTESIAN_POINT('Ctrl Pts',(-7.54704599183567,-2.38167463296328,
-13.5448309696978));
#67875=CARTESIAN_POINT('Ctrl Pts',(-7.47668853165346,-2.58515949230247,
-13.5361669063281));
#67876=CARTESIAN_POINT('Ctrl Pts',(-7.40365641525792,-2.79637987879034,
-13.527173476451));
#67877=CARTESIAN_POINT('Ctrl Pts',(-7.32162155643005,-3.00464072724953,
-13.5181800465739));
#67878=CARTESIAN_POINT('Ctrl Pts',(-7.23083355376838,-3.20920038603035,
-13.5091866166968));
#67879=CARTESIAN_POINT('Ctrl Pts',(-7.14004555110671,-3.41376004481117,
-13.5001931868197));
#67880=CARTESIAN_POINT('Ctrl Pts',(-7.04050445631863,-3.61461823432231,
-13.4911997569426));
#67881=CARTESIAN_POINT('Ctrl Pts',(-6.93251822352143,-3.8110513090935,-13.4822063270655));
#67882=CARTESIAN_POINT('Ctrl Pts',(-6.83871685809038,-3.98168130656698,
-13.4743942571328));
#67883=CARTESIAN_POINT('Ctrl Pts',(-6.73858323730594,-4.14889863996573,
-13.4665821872001));
#67884=CARTESIAN_POINT('Ctrl Pts',(-6.63240542684962,-4.31220584549203,
-13.4587701172674));
#67885=CARTESIAN_POINT('Ctrl Pts',(-6.52623518859451,-4.47550140456403,
-13.4509586044621));
#67886=CARTESIAN_POINT('Ctrl Pts',(-6.41402181117272,-4.63488709610619,
-13.4431470916567));
#67887=CARTESIAN_POINT('Ctrl Pts',(-6.29609728332536,-4.78989352688585,
-13.4353355788514));
#67888=CARTESIAN_POINT('Ctrl Pts',(-6.17816037048478,-4.94491623717606,
-13.427523245644));
#67889=CARTESIAN_POINT('Ctrl Pts',(-6.05451132628634,-5.09555849092362,
-13.4197109124365));
#67890=CARTESIAN_POINT('Ctrl Pts',(-5.92552318486841,-5.24138302221722,
-13.4118985792291));
#67891=CARTESIAN_POINT('Ctrl Pts',(-5.79644366251754,-5.38731086209073,
-13.4040807114175));
#67892=CARTESIAN_POINT('Ctrl Pts',(-5.66201771967842,-5.52841389667778,
-13.396262843606));
#67893=CARTESIAN_POINT('Ctrl Pts',(-5.52265670877546,-5.66429023594461,
-13.3884449757944));
#67894=CARTESIAN_POINT('Ctrl Pts',(-5.38324412838404,-5.8002168552235,-13.38062421504));
#67895=CARTESIAN_POINT('Ctrl Pts',(-5.2388930995787,-5.93091268658528,-13.3728034542856));
#67896=CARTESIAN_POINT('Ctrl Pts',(-5.09004908463706,-6.05601530017762,
-13.3649826935312));
#67897=CARTESIAN_POINT('Ctrl Pts',(-4.94104019615443,-6.18125648911609,
-13.3571532697712));
#67898=CARTESIAN_POINT('Ctrl Pts',(-4.78752865471477,-6.30089186431787,
-13.3493238460113));
#67899=CARTESIAN_POINT('Ctrl Pts',(-4.62999088609122,-6.41460095366128,
-13.3414944222514));
#67900=CARTESIAN_POINT('Ctrl Pts',(-4.50891533311088,-6.50199200275023,
-13.3354771235456));
#67901=CARTESIAN_POINT('Ctrl Pts',(-4.38546225278603,-6.58588343819373,
-13.3294598248398));
#67902=CARTESIAN_POINT('Ctrl Pts',(-4.25985804557763,-6.6661480955292,-13.3234425261341));
#67903=CARTESIAN_POINT('Ctrl Pts',(-4.09041527297058,-6.77442684178735,
-13.3153250609713));
#67904=CARTESIAN_POINT('Ctrl Pts',(-3.91672137263509,-6.87631842405461,
-13.3072075958085));
#67905=CARTESIAN_POINT('Ctrl Pts',(-3.7392868796961,-6.97148869548912,-13.2990901306457));
#67906=CARTESIAN_POINT('Ctrl Pts',(-3.56198186606097,-7.06658951830465,
-13.2909785890423));
#67907=CARTESIAN_POINT('Ctrl Pts',(-3.38094198388653,-7.15497865872263,
-13.2828670474388));
#67908=CARTESIAN_POINT('Ctrl Pts',(-3.19670481719188,-7.23636644399261,
-13.2747555058353));
#67909=CARTESIAN_POINT('Ctrl Pts',(-3.01257592684877,-7.31770639758667,
-13.2666487313922));
#67910=CARTESIAN_POINT('Ctrl Pts',(-2.82525379146581,-7.39205307176465,
-13.2585419569492));
#67911=CARTESIAN_POINT('Ctrl Pts',(-2.63529907242501,-7.45916347849247,
-13.2504351825061));
#67912=CARTESIAN_POINT('Ctrl Pts',(-2.44542903967905,-7.52624396581782,
-13.2423320222543));
#67913=CARTESIAN_POINT('Ctrl Pts',(-2.25292906569277,-7.58609451277635,
-13.2342288620026));
#67914=CARTESIAN_POINT('Ctrl Pts',(-2.05837873744876,-7.63852066654394,
-13.2261257017508));
#67915=CARTESIAN_POINT('Ctrl Pts',(-1.8638875648434,-7.69093087943579,-13.2180250053737));
#67916=CARTESIAN_POINT('Ctrl Pts',(-1.66734759070352,-7.73592111844154,
-13.2099243089965));
#67917=CARTESIAN_POINT('Ctrl Pts',(-1.46935302835809,-7.77334694182981,
-13.2018236126194));
#67918=CARTESIAN_POINT('Ctrl Pts',(-1.26983903390524,-7.8110599751143,-13.1936607506049));
#67919=CARTESIAN_POINT('Ctrl Pts',(-1.06884834867439,-7.84109191182901,
-13.1854978885904));
#67920=CARTESIAN_POINT('Ctrl Pts',(-0.866999753941357,-7.86334740595032,
-13.1773350265759));
#67921=CARTESIAN_POINT('Ctrl Pts',(-0.666689167003725,-7.88543332186132,
-13.1692343623954));
#67922=CARTESIAN_POINT('Ctrl Pts',(-0.465534024469435,-7.8998608814698,
-13.161133698215));
#67923=CARTESIAN_POINT('Ctrl Pts',(-0.26414482943276,-7.90658893006864,
-13.1530330340346));
#67924=CARTESIAN_POINT('Ctrl Pts',(-0.0627284509836759,-7.9133178868161,
-13.1449312764306));
#67925=CARTESIAN_POINT('Ctrl Pts',(0.138921722408625,-7.91234524916927,
-13.1368295188267));
#67926=CARTESIAN_POINT('Ctrl Pts',(0.34019401306695,-7.90368199217766,-13.1287277612227));
#67927=CARTESIAN_POINT('Ctrl Pts',(0.541519438305782,-7.89501644814234,
-13.1206238648072));
#67928=CARTESIAN_POINT('Ctrl Pts',(0.742466461505047,-7.87865624964724,
-13.1125199683917));
#67929=CARTESIAN_POINT('Ctrl Pts',(0.942426801007849,-7.85466439287778,
-13.1044160719762));
#67930=CARTESIAN_POINT('Ctrl Pts',(1.14496643880155,-7.83036306396343,-13.0962076430007));
#67931=CARTESIAN_POINT('Ctrl Pts',(1.34649342566749,-7.79823187326288,-13.0879992140253));
#67932=CARTESIAN_POINT('Ctrl Pts',(1.54638469507451,-7.75838999888761,-13.0797907850499));
#67933=CARTESIAN_POINT('Ctrl Pts',(1.74398657279751,-7.71900444086943,-13.0716763687299));
#67934=CARTESIAN_POINT('Ctrl Pts',(1.93998969892463,-7.67208400233859,-13.0635619524099));
#67935=CARTESIAN_POINT('Ctrl Pts',(2.13380566895088,-7.61779458683109,-13.0554475360899));
#67936=CARTESIAN_POINT('Ctrl Pts',(2.33098993189355,-7.56256168532672,-13.0471921007867));
#67937=CARTESIAN_POINT('Ctrl Pts',(2.52590998779532,-7.49970143399945,-13.0389366654836));
#67938=CARTESIAN_POINT('Ctrl Pts',(2.71796534342915,-7.42944044944961,-13.0306812301804));
#67939=CARTESIAN_POINT('Ctrl Pts',(2.91002069906291,-7.3591794648998,-13.0224257948773));
#67940=CARTESIAN_POINT('Ctrl Pts',(3.09921104666504,-7.28151791046009,-13.0141703595741));
#67941=CARTESIAN_POINT('Ctrl Pts',(3.2849598976723,-7.19673255517286,-13.005914924271));
#67942=CARTESIAN_POINT('Ctrl Pts',(3.46327800417173,-7.11533897490726,-12.9979897415116));
#67943=CARTESIAN_POINT('Ctrl Pts',(3.63880594492515,-7.02720596954404,-12.9900645587522));
#67944=CARTESIAN_POINT('Ctrl Pts',(3.8110004953195,-6.93254615741392,-12.9821393759927));
#67945=CARTESIAN_POINT('Ctrl Pts',(3.98301106040099,-6.83798748678398,-12.974222661081));
#67946=CARTESIAN_POINT('Ctrl Pts',(4.15169503192817,-6.73691606278549,-12.9663059461693));
#67947=CARTESIAN_POINT('Ctrl Pts',(4.3165292516452,-6.62959246256445,-12.9583892312576));
#67948=CARTESIAN_POINT('Ctrl Pts',(4.4812145182245,-6.52236584576732,-12.9504796703187));
#67949=CARTESIAN_POINT('Ctrl Pts',(4.6420566781372,-6.40889849316678,-12.9425701093798));
#67950=CARTESIAN_POINT('Ctrl Pts',(4.79855703300233,-6.28949691159984,-12.9346605484409));
#67951=CARTESIAN_POINT('Ctrl Pts',(4.95491977876746,-6.17020031857552,-12.9267579422949));
#67952=CARTESIAN_POINT('Ctrl Pts',(5.10694805947257,-6.04498010562055,-12.918855336149));
#67953=CARTESIAN_POINT('Ctrl Pts',(5.25417201345454,-5.91418611924168,-12.910952730003));
#67954=CARTESIAN_POINT('Ctrl Pts',(5.40132039303578,-5.78345927327627,-12.903054180498));
#67955=CARTESIAN_POINT('Ctrl Pts',(5.54366910364888,-5.64716458020315,-12.895155630993));
#67956=CARTESIAN_POINT('Ctrl Pts',(5.6807807563017,-5.50569259937678,-12.887257081488));
#67957=CARTESIAN_POINT('Ctrl Pts',(5.81784590906124,-5.36426859720055,-12.8793612106883));
#67958=CARTESIAN_POINT('Ctrl Pts',(5.94967730440633,-5.21767105065525,-12.8714653398886));
#67959=CARTESIAN_POINT('Ctrl Pts',(6.07587366988091,-5.06632807343227,-12.8635694690889));
#67960=CARTESIAN_POINT('Ctrl Pts',(6.16334282995445,-4.96142930672895,-12.8580966871724));
#67961=CARTESIAN_POINT('Ctrl Pts',(6.24810558269317,-4.85425156050755,-12.8526239052559));
#67962=CARTESIAN_POINT('Ctrl Pts',(6.33003929358821,-4.74494715899232,-12.8471511233394));
#67963=CARTESIAN_POINT('Ctrl Pts',(6.45758520287067,-4.57479339532725,-12.8386316636662));
#67964=CARTESIAN_POINT('Ctrl Pts',(6.57814689505413,-4.39965454663752,-12.830112203993));
#67965=CARTESIAN_POINT('Ctrl Pts',(6.69137854313384,-4.22011542407173,-12.8215927443197));
#67966=CARTESIAN_POINT('Ctrl Pts',(6.80481411280608,-4.04025296519124,-12.8130579417471));
#67967=CARTESIAN_POINT('Ctrl Pts',(6.91089312188798,-3.85597460529773,-12.8045231391745));
#67968=CARTESIAN_POINT('Ctrl Pts',(7.00931563572188,-3.66788976372311,-12.7959883366019));
#67969=CARTESIAN_POINT('Ctrl Pts',(7.11271933895107,-3.47028589868759,-12.7870215854191));
#67970=CARTESIAN_POINT('Ctrl Pts',(7.20767140385833,-3.26848062986892,-12.7780548342363));
#67971=CARTESIAN_POINT('Ctrl Pts',(7.29388208941897,-3.06320176704917,-12.7690880830534));
#67972=CARTESIAN_POINT('Ctrl Pts',(7.37628249967098,-2.86699566565453,-12.7605176376233));
#67973=CARTESIAN_POINT('Ctrl Pts',(7.45069749633437,-2.66761661204617,-12.7519471921931));
#67974=CARTESIAN_POINT('Ctrl Pts',(7.51692571238235,-2.46571467013624,-12.743376746763));
#67975=CARTESIAN_POINT('Ctrl Pts',(7.58323668942425,-2.26356042480668,-12.7347955914176));
#67976=CARTESIAN_POINT('Ctrl Pts',(7.64134037487582,-2.05887723087956,-12.7262144360722));
#67977=CARTESIAN_POINT('Ctrl Pts',(7.69108586500686,-1.85232805331335,-12.7176332807268));
#67978=CARTESIAN_POINT('Ctrl Pts',(7.74091412247346,-1.64543521594918,-12.709037847919));
#67979=CARTESIAN_POINT('Ctrl Pts',(7.78235632402971,-1.43667043037062,-12.7004424151112));
#67980=CARTESIAN_POINT('Ctrl Pts',(7.81531263808677,-1.22670671676698,-12.6918469823034));
#67981=CARTESIAN_POINT('Ctrl Pts',(7.81973427457653,-1.19853659992721,-12.6906937623383));
#67982=CARTESIAN_POINT('Ctrl Pts',(7.82400323585118,-1.17034490821894,-12.6895405423731));
#67983=CARTESIAN_POINT('Ctrl Pts',(7.82811935192236,-1.14213327245933,-12.688387322408));
#67984=CARTESIAN_POINT('Ctrl Pts',(7.85634854142691,-0.948651942409426,
-12.6804782974015));
#67985=CARTESIAN_POINT('Ctrl Pts',(7.87743627301376,-0.753876758817094,
-12.672569272395));
#67986=CARTESIAN_POINT('Ctrl Pts',(7.89126959376374,-0.55837729049442,-12.6646602473885));
#67987=CARTESIAN_POINT('Ctrl Pts',(7.90508881356139,-0.363077103944612,
-12.656759284422));
#67988=CARTESIAN_POINT('Ctrl Pts',(7.911668328097,-0.167054444395018,-12.6488583214555));
#67989=CARTESIAN_POINT('Ctrl Pts',(7.91094643343843,0.0291123215807306,
-12.640957358489));
#67990=CARTESIAN_POINT('Ctrl Pts',(7.91022514072346,0.225115516141607,-12.6330629836501));
#67991=CARTESIAN_POINT('Ctrl Pts',(7.90221456866037,0.421262234903514,-12.6251686088112));
#67992=CARTESIAN_POINT('Ctrl Pts',(7.88690489857525,0.616970113400794,-12.6172742339723));
#67993=CARTESIAN_POINT('Ctrl Pts',(7.87160515499402,0.812551098568149,-12.6093849776985));
#67994=CARTESIAN_POINT('Ctrl Pts',(7.84901576942605,1.00769346787065,-12.6014957214247));
#67995=CARTESIAN_POINT('Ctrl Pts',(7.81917898680338,1.20181569815528,-12.5936064651508));
#67996=CARTESIAN_POINT('Ctrl Pts',(7.78935601744504,1.39584805743366,-12.5857208612944));
#67997=CARTESIAN_POINT('Ctrl Pts',(7.75229238934904,1.58886087872405,-12.5778352574379));
#67998=CARTESIAN_POINT('Ctrl Pts',(7.70808212992109,1.78027831486852,-12.5699496535814));
#67999=CARTESIAN_POINT('Ctrl Pts',(7.66157429029105,1.98164359835233,-12.5616542397049));
#68000=CARTESIAN_POINT('Ctrl Pts',(7.60715727742886,2.18124286102403,-12.5533588258284));
#68001=CARTESIAN_POINT('Ctrl Pts',(7.54500165400536,2.37841775999431,-12.5450634119518));
#68002=CARTESIAN_POINT('Ctrl Pts',(7.48592640236596,2.56582086420387,-12.5371791106575));
#68003=CARTESIAN_POINT('Ctrl Pts',(7.41986112155096,2.75103372711868,-12.5292948093632));
#68004=CARTESIAN_POINT('Ctrl Pts',(7.34700343068811,2.93350670520064,-12.5214105080688));
#68005=CARTESIAN_POINT('Ctrl Pts',(7.2741362405951,3.11600347422076,-12.5135251788145));
#68006=CARTESIAN_POINT('Ctrl Pts',(7.19447500312477,3.29575932593703,-12.5056398495601));
#68007=CARTESIAN_POINT('Ctrl Pts',(7.1082655293651,3.47224454266111,-12.4977545203058));
#68008=CARTESIAN_POINT('Ctrl Pts',(7.02203033138084,3.64878242117693,-12.4898668381316));
#68009=CARTESIAN_POINT('Ctrl Pts',(6.92924315475177,3.8220474100577,-12.4819791559574));
#68010=CARTESIAN_POINT('Ctrl Pts',(6.83019591979877,3.99153412827251,-12.4740914737832));
#68011=CARTESIAN_POINT('Ctrl Pts',(6.73110248849132,4.1610998963317,-12.4662001127364));
#68012=CARTESIAN_POINT('Ctrl Pts',(6.62574335448452,4.3268835847316,-12.4583087516896));
#68013=CARTESIAN_POINT('Ctrl Pts',(6.51445405098402,4.48840833900146,-12.4504173906428));
#68014=CARTESIAN_POINT('Ctrl Pts',(6.4030365048607,4.65011922399087,-12.4425169360999));
#68015=CARTESIAN_POINT('Ctrl Pts',(6.28567533592799,4.8075610884601,-12.4346164815571));
#68016=CARTESIAN_POINT('Ctrl Pts',(6.16274739818465,4.96028885309801,-12.4267160270143));
#68017=CARTESIAN_POINT('Ctrl Pts',(6.03973724705966,5.11311876104225,-12.4188102887003));
#68018=CARTESIAN_POINT('Ctrl Pts',(5.91115313047215,5.2612280245565,-12.4109045503864));
#68019=CARTESIAN_POINT('Ctrl Pts',(5.77740928637362,5.40420789179356,-12.4029988120725));
#68020=CARTESIAN_POINT('Ctrl Pts',(5.64348514570665,5.54738050643963,-12.3950824162401));
#68021=CARTESIAN_POINT('Ctrl Pts',(5.50438762924163,5.68540967254575,-12.3871660204077));
#68022=CARTESIAN_POINT('Ctrl Pts',(5.3605654315066,5.81792568313969,-12.3792496245753));
#68023=CARTESIAN_POINT('Ctrl Pts',(5.30975719073765,5.86473977357935,-12.3764529898985));
#68024=CARTESIAN_POINT('Ctrl Pts',(5.25835958554602,5.91086620423005,-12.3736563552217));
#68025=CARTESIAN_POINT('Ctrl Pts',(5.20639327305232,5.95628995989244,-12.370859720545));
#68026=CARTESIAN_POINT('Ctrl Pts',(5.06216589040119,6.0823591203734,-12.3630979364139));
#68027=CARTESIAN_POINT('Ctrl Pts',(4.91310344352879,6.20340786624087,-12.3553361522829));
#68028=CARTESIAN_POINT('Ctrl Pts',(4.7595957947092,6.31903227329838,-12.3475743681518));
#68029=CARTESIAN_POINT('Ctrl Pts',(4.60627247888219,6.43451783780875,-12.3398219044221));
#68030=CARTESIAN_POINT('Ctrl Pts',(4.44851486858131,6.5445918153278,-12.3320694406925));
#68031=CARTESIAN_POINT('Ctrl Pts',(4.2867494487054,6.64888713726018,-12.3243169769628));
#68032=CARTESIAN_POINT('Ctrl Pts',(4.12514546879186,6.75307837370347,-12.3165722500995));
#68033=CARTESIAN_POINT('Ctrl Pts',(3.95954194042255,6.85150224225592,-12.3088275232363));
#68034=CARTESIAN_POINT('Ctrl Pts',(3.7903982699531,6.94383193598006,-12.3010827963731));
#68035=CARTESIAN_POINT('Ctrl Pts',(3.62138914659194,7.03608818508007,-12.2933442301342));
#68036=CARTESIAN_POINT('Ctrl Pts',(3.44884580093232,7.12225973996112,-12.2856056638952));
#68037=CARTESIAN_POINT('Ctrl Pts',(3.27325653934698,7.2020630813415,-12.2778670976563));
#68038=CARTESIAN_POINT('Ctrl Pts',(3.09777142655465,7.28181908826869,-12.2701331214607));
#68039=CARTESIAN_POINT('Ctrl Pts',(2.91924432101981,7.35521425521839,-12.2623991452652));
#68040=CARTESIAN_POINT('Ctrl Pts',(2.73818812701339,7.42201096611174,-12.2546651690697));
#68041=CARTESIAN_POINT('Ctrl Pts',(2.55720271816351,7.48878156237441,-12.246934216525));
#68042=CARTESIAN_POINT('Ctrl Pts',(2.37369052635165,7.54895871655249,-12.2392032639803));
#68043=CARTESIAN_POINT('Ctrl Pts',(2.18818451338544,7.6023528946886,-12.2314723114357));
#68044=CARTESIAN_POINT('Ctrl Pts',(2.00267823975531,7.65574714785158,-12.2237413480278));
#68045=CARTESIAN_POINT('Ctrl Pts',(1.8151784810943,7.70235829576359,-12.21601038462));
#68046=CARTESIAN_POINT('Ctrl Pts',(1.62623383725534,7.7420465321881,-12.2082794212122));
#68047=CARTESIAN_POINT('Ctrl Pts',(1.43727941233524,7.78173682315014,-12.2005480575962));
#68048=CARTESIAN_POINT('Ctrl Pts',(1.24688030463003,7.81450341415753,-12.1928166939803));
#68049=CARTESIAN_POINT('Ctrl Pts',(1.05559562915932,7.84025757661697,-12.1850853303644));
#68050=CARTESIAN_POINT('Ctrl Pts',(0.864266024566849,7.86601778823794,-12.1773521507986));
#68051=CARTESIAN_POINT('Ctrl Pts',(0.672050793867611,7.88476224329706,-12.1696189712328));
#68052=CARTESIAN_POINT('Ctrl Pts',(0.479514552664956,7.89645406456484,-12.161885791667));
#68053=CARTESIAN_POINT('Ctrl Pts',(0.286897821121417,7.90815077363282,-12.1541493792228));
#68054=CARTESIAN_POINT('Ctrl Pts',(0.0939601698556643,7.91278895610964,
-12.1464129667785));
#68055=CARTESIAN_POINT('Ctrl Pts',(-0.0987333508868629,7.91038385449294,
-12.1386765543343));
#68056=CARTESIAN_POINT('Ctrl Pts',(-0.291656172589594,7.90797589085937,
-12.1309309357331));
#68057=CARTESIAN_POINT('Ctrl Pts',(-0.484333924576509,7.89850790921964,
-12.1231853171319));
#68058=CARTESIAN_POINT('Ctrl Pts',(-0.676205200263328,7.8820471660056,-12.1154396985307));
#68059=CARTESIAN_POINT('Ctrl Pts',(-0.868201228321395,7.8655757202164,-12.1076890438225));
#68060=CARTESIAN_POINT('Ctrl Pts',(-1.05938938074976,7.84210249983862,-12.0999383891142));
#68061=CARTESIAN_POINT('Ctrl Pts',(-1.24921814267264,7.81174596566078,-12.0921877344059));
#68062=CARTESIAN_POINT('Ctrl Pts',(-1.43933528508502,7.7813433150141,-12.0844253052038));
#68063=CARTESIAN_POINT('Ctrl Pts',(-1.62808856203291,7.74403653578136,-12.0766628760016));
#68064=CARTESIAN_POINT('Ctrl Pts',(-1.81494016212452,7.69999436414777,-12.0689004467995));
#68065=CARTESIAN_POINT('Ctrl Pts',(-1.93985668605306,7.67055070413076,-12.0637110040936));
#68066=CARTESIAN_POINT('Ctrl Pts',(-2.06392362330912,7.63809777611437,-12.0585215613877));
#68067=CARTESIAN_POINT('Ctrl Pts',(-2.18698543962865,7.60269792158365,-12.0533321186819));
#68068=CARTESIAN_POINT('Ctrl Pts',(-2.37704472668374,7.5480256331746,-12.0453174329703));
#68069=CARTESIAN_POINT('Ctrl Pts',(-2.56528649447441,7.48615503709286,-12.0373027472588));
#68070=CARTESIAN_POINT('Ctrl Pts',(-2.751133962191,7.41722204885895,-12.0292880615473));
#68071=CARTESIAN_POINT('Ctrl Pts',(-2.93677014604261,7.34836742826898,-12.021282487468));
#68072=CARTESIAN_POINT('Ctrl Pts',(-3.12001714278529,7.27246652954982,-12.0132769133886));
#68073=CARTESIAN_POINT('Ctrl Pts',(-3.30031138418942,7.18970554107675,-12.0052713393093));
#68074=CARTESIAN_POINT('Ctrl Pts',(-3.48043122839172,7.10702460665697,-11.9972735089589));
#68075=CARTESIAN_POINT('Ctrl Pts',(-3.65760370705829,7.01749694500259,-11.9892756786084));
#68076=CARTESIAN_POINT('Ctrl Pts',(-3.83128297388375,6.92135765395984,-11.9812778482579));
#68077=CARTESIAN_POINT('Ctrl Pts',(-4.00482367470889,6.82529506543477,-11.9732863987921));
#68078=CARTESIAN_POINT('Ctrl Pts',(-4.17487642696911,6.72263152208037,-11.9652949493263));
#68079=CARTESIAN_POINT('Ctrl Pts',(-4.34091747095585,6.61364925818948,-11.9573034998604));
#68080=CARTESIAN_POINT('Ctrl Pts',(-4.50685416603746,6.50473548447212,-11.9493170726408));
#68081=CARTESIAN_POINT('Ctrl Pts',(-4.66878389953174,6.38951108873213,-11.9413306454211));
#68082=CARTESIAN_POINT('Ctrl Pts',(-4.82620918116694,6.26830327438135,-11.9333442182015));
#68083=CARTESIAN_POINT('Ctrl Pts',(-4.98845185379272,6.14338636434545,-11.9251133973106));
#68084=CARTESIAN_POINT('Ctrl Pts',(-5.14590970040969,6.01211420331347,-11.9168825764196));
#68085=CARTESIAN_POINT('Ctrl Pts',(-5.29807108467227,5.87489266129685,-11.9086517555287));
#68086=CARTESIAN_POINT('Ctrl Pts',(-5.44561514671236,5.74183509346086,-11.9006706980872));
#68087=CARTESIAN_POINT('Ctrl Pts',(-5.58817921861217,5.6031841667586,-11.8926896406457));
#68088=CARTESIAN_POINT('Ctrl Pts',(-5.72533099993576,5.4593503222613,-11.8847085832042));
#68089=CARTESIAN_POINT('Ctrl Pts',(-5.86247206294,5.3155277182821,-11.876728149477));
#68090=CARTESIAN_POINT('Ctrl Pts',(-5.99420144753901,5.1665232457812,-11.8687477157498));
#68091=CARTESIAN_POINT('Ctrl Pts',(-6.12012430553447,5.01278360642131,-11.8607672820226));
#68092=CARTESIAN_POINT('Ctrl Pts',(-6.24605665338571,4.85903238086469,-11.8527862468703));
#68093=CARTESIAN_POINT('Ctrl Pts',(-6.3661813907419,4.70054553614335,-11.844805211718));
#68094=CARTESIAN_POINT('Ctrl Pts',(-6.4801442601237,4.5378024822579,-11.8368241765657));
#68095=CARTESIAN_POINT('Ctrl Pts',(-6.59413321293507,4.375022180302,-11.8288413147416));
#68096=CARTESIAN_POINT('Ctrl Pts',(-6.70195729533414,4.2079840016717,-11.8208584529174));
#68097=CARTESIAN_POINT('Ctrl Pts',(-6.8033056343289,4.03719623574439,-11.8128755910932));
#68098=CARTESIAN_POINT('Ctrl Pts',(-6.90472917926648,3.86628173606806,-11.8048868055543));
#68099=CARTESIAN_POINT('Ctrl Pts',(-6.99966721107912,3.6916123789148,-11.7968980200154));
#68100=CARTESIAN_POINT('Ctrl Pts',(-7.087854388323,3.51372184014763,-11.7889092344765));
#68101=CARTESIAN_POINT('Ctrl Pts',(-7.17608045816177,3.33575284751816,-11.7809169256974));
#68102=CARTESIAN_POINT('Ctrl Pts',(-7.25754959619902,3.15456014368803,-11.7729246169184));
#68103=CARTESIAN_POINT('Ctrl Pts',(-7.33204443313085,2.9706978019642,-11.7649323081394));
#68104=CARTESIAN_POINT('Ctrl Pts',(-7.40660897471381,2.78666342066133,-11.756932520975));
#68105=CARTESIAN_POINT('Ctrl Pts',(-7.47418606501852,2.59995472537995,-11.7489327338107));
#68106=CARTESIAN_POINT('Ctrl Pts',(-7.53460773908747,2.41114230564753,-11.7409329466464));
#68107=CARTESIAN_POINT('Ctrl Pts',(-7.54751926240514,2.37079493034541,-11.7392234700372));
#68108=CARTESIAN_POINT('Ctrl Pts',(-7.56010422833779,2.33035153566343,-11.737513993428));
#68109=CARTESIAN_POINT('Ctrl Pts',(-7.57236129918832,2.28981775575155,-11.7358045168188));
#68110=CARTESIAN_POINT('Ctrl Pts',(-7.63487911187803,2.08307315167448,-11.7270852445103));
#68111=CARTESIAN_POINT('Ctrl Pts',(-7.68895729105136,1.87366285074523,-11.7183659722017));
#68112=CARTESIAN_POINT('Ctrl Pts',(-7.73439168130246,1.66225940219912,-11.7096466998932));
#68113=CARTESIAN_POINT('Ctrl Pts',(-7.77976279339094,1.4511503830867,-11.700939571239));
#68114=CARTESIAN_POINT('Ctrl Pts',(-7.81651409668169,1.23805397237733,-11.6922324425848));
#68115=CARTESIAN_POINT('Ctrl Pts',(-7.84449166760319,1.02365593677963,-11.6835253139307));
#68116=CARTESIAN_POINT('Ctrl Pts',(-7.87240253864888,0.80976903641903,-11.6748389434903));
#68117=CARTESIAN_POINT('Ctrl Pts',(-7.89158139911881,0.594586924409034,
-11.66615257305));
#68118=CARTESIAN_POINT('Ctrl Pts',(-7.90192565665978,0.378803269022262,
-11.6574662026097));
#68119=CARTESIAN_POINT('Ctrl Pts',(-7.90793342777937,0.253479744566416,
-11.6524213044854));
#68120=CARTESIAN_POINT('Ctrl Pts',(-7.91096214797229,0.127953536149312,
-11.6473764063611));
#68121=CARTESIAN_POINT('Ctrl Pts',(-7.91099964736161,0.00236208477935112,
-11.6423315082368));
#68122=CARTESIAN_POINT('',(-7.8964170631581,0.000600145041366463,-9.64211896160294));
#68123=CARTESIAN_POINT('Ctrl Pts',(-7.9129081904216,0.00235452960061844,
-11.64233118194));
#68124=CARTESIAN_POINT('Ctrl Pts',(-7.91061145860717,-0.539573416157087,
-11.6205676932558));
#68125=CARTESIAN_POINT('Ctrl Pts',(-7.71358646751875,-2.40039572256556,
-11.5458829375944));
#68126=CARTESIAN_POINT('Ctrl Pts',(-6.28991713969721,-5.34225823726283,
-11.4182769149559));
#68127=CARTESIAN_POINT('Ctrl Pts',(-2.97255753145148,-7.67959952006296,
-11.2595131140243));
#68128=CARTESIAN_POINT('Ctrl Pts',(2.43982948211447,-8.37481141267956,-11.0478280461155));
#68129=CARTESIAN_POINT('Ctrl Pts',(7.22580432018955,-4.89039179196627,-10.8361429782069));
#68130=CARTESIAN_POINT('Ctrl Pts',(8.21331522541468,0.46673392135825,-10.6244579102983));
#68131=CARTESIAN_POINT('Ctrl Pts',(6.63670966247552,5.65318849316478,-10.4127728423895));
#68132=CARTESIAN_POINT('Ctrl Pts',(0.184060152027318,9.35904114020558,-10.1481665075036));
#68133=CARTESIAN_POINT('Ctrl Pts',(-6.6942692761131,5.76619568406868,-9.87371230712702));
#68134=CARTESIAN_POINT('Ctrl Pts',(-7.89134496298745,1.56412139810797,-9.70510064070473));
#68135=CARTESIAN_POINT('Ctrl Pts',(-7.89604907601277,0.00059194571216748,
-9.64233150823677));
#68136=CARTESIAN_POINT('',(-7.91099369906704,0.00998465430474249,-5.64233150823678));
#68137=CARTESIAN_POINT('Ctrl Pts',(-7.91099994591311,0.000925074479515564,
-9.63369599715849));
#68138=CARTESIAN_POINT('Ctrl Pts',(-7.91111146910358,-0.952792678327162,
-9.59709787947992));
#68139=CARTESIAN_POINT('Ctrl Pts',(-7.7387878457638,-1.89854071997732,-9.56687127556384));
#68140=CARTESIAN_POINT('Ctrl Pts',(-7.33879272140064,-2.95948042625145,
-9.52501737594924));
#68141=CARTESIAN_POINT('Ctrl Pts',(-7.26947854741557,-3.12587321044274,
-9.51815174290647));
#68142=CARTESIAN_POINT('Ctrl Pts',(-7.17967042688255,-3.32227796713343,
-9.50960279053886));
#68143=CARTESIAN_POINT('Ctrl Pts',(-7.16458817198334,-3.35467950857822,
-9.50817883091966));
#68144=CARTESIAN_POINT('Ctrl Pts',(-7.14413446458521,-3.39785352697423,
-9.50626408786518));
#68145=CARTESIAN_POINT('Ctrl Pts',(-7.13895710422596,-3.40871783828617,
-9.50578078410131));
#68146=CARTESIAN_POINT('Ctrl Pts',(-7.13036911345293,-3.42663372168387,
-9.50498138672398));
#68147=CARTESIAN_POINT('Ctrl Pts',(-7.12697275548826,-3.43369213802041,
-9.50466582700147));
#68148=CARTESIAN_POINT('Ctrl Pts',(-7.12033654848942,-3.44743144488754,
-9.50405039629591));
#68149=CARTESIAN_POINT('Ctrl Pts',(-7.11709776494728,-3.45411284336901,
-9.50375056454872));
#68150=CARTESIAN_POINT('Ctrl Pts',(-7.10954582026169,-3.46963629433136,
-9.50305267649529));
#68151=CARTESIAN_POINT('Ctrl Pts',(-7.10522556642992,-3.47847487191732,
-9.50265436538665));
#68152=CARTESIAN_POINT('Ctrl Pts',(-7.09111328332791,-3.50721045533762,
-9.50135632669987));
#68153=CARTESIAN_POINT('Ctrl Pts',(-7.08125411622026,-3.52707427002634,
-9.50045424789244));
#68154=CARTESIAN_POINT('Ctrl Pts',(-6.96437624469295,-3.7600892185885,-9.48981757488879));
#68155=CARTESIAN_POINT('Ctrl Pts',(-6.84785753945099,-3.96833045529407,
-9.4797765537756));
#68156=CARTESIAN_POINT('Ctrl Pts',(-6.52697906365773,-4.48547065495884,
-9.45384182609394));
#68157=CARTESIAN_POINT('Ctrl Pts',(-6.31001385031687,-4.7858781736028,-9.43782713961079));
#68158=CARTESIAN_POINT('Ctrl Pts',(-5.7133783690336,-5.5005257014241,-9.39797255921956));
#68159=CARTESIAN_POINT('Ctrl Pts',(-5.30916730476546,-5.89162610501911,
-9.37456360132866));
#68160=CARTESIAN_POINT('Ctrl Pts',(-4.68714923666404,-6.37703621224692,
-9.34210844832806));
#68161=CARTESIAN_POINT('Ctrl Pts',(-4.50132230734823,-6.50953602426058,
-9.33277714194438));
#68162=CARTESIAN_POINT('Ctrl Pts',(-4.27317163993847,-6.65776665445819,
-9.32176470606153));
#68163=CARTESIAN_POINT('Ctrl Pts',(-4.23611721421675,-6.6814043182343,-9.31998945157181));
#68164=CARTESIAN_POINT('Ctrl Pts',(-4.17768165397452,-6.71799984198844,
-9.31721051371941));
#68165=CARTESIAN_POINT('Ctrl Pts',(-4.15643289274584,-6.73116717160455,
-9.31620425571997));
#68166=CARTESIAN_POINT('Ctrl Pts',(-4.11667792524168,-6.75554231221871,
-9.31432946828467));
#68167=CARTESIAN_POINT('Ctrl Pts',(-4.09818746947109,-6.76677534286162,
-9.31346062835265));
#68168=CARTESIAN_POINT('Ctrl Pts',(-4.05690439505437,-6.79162370831924,
-9.31152774493903));
#68169=CARTESIAN_POINT('Ctrl Pts',(-4.03408882927901,-6.80520045184133,
-9.31046420178991));
#68170=CARTESIAN_POINT('Ctrl Pts',(-3.96923602339953,-6.84335132576966,
-9.30745424132499));
#68171=CARTESIAN_POINT('Ctrl Pts',(-3.92703952985801,-6.86765262277037,
-9.30551136533179));
#68172=CARTESIAN_POINT('Ctrl Pts',(-3.6360741887927,-7.03166333392704,-9.2922183802438));
#68173=CARTESIAN_POINT('Ctrl Pts',(-3.38012623738723,-7.15821750428232,
-9.28105239632895));
#68174=CARTESIAN_POINT('Ctrl Pts',(-2.76318777009988,-7.42278047147471,
-9.25504913786305));
#68175=CARTESIAN_POINT('Ctrl Pts',(-2.3978268911422,-7.54872835165053,-9.24035213959236));
#68176=CARTESIAN_POINT('Ctrl Pts',(-1.87723839538427,-7.68655827718115,
-9.21950849351732));
#68177=CARTESIAN_POINT('Ctrl Pts',(-1.72864208566482,-7.72133390378351,
-9.21356596732958));
#68178=CARTESIAN_POINT('Ctrl Pts',(-1.50262553918261,-7.76737627745208,
-9.20446140734854));
#68179=CARTESIAN_POINT('Ctrl Pts',(-1.42588961765196,-7.78182859290269,
-9.20135882455448));
#68180=CARTESIAN_POINT('Ctrl Pts',(-1.33010383776308,-7.7984043704001,-9.19746264789769));
#68181=CARTESIAN_POINT('Ctrl Pts',(-1.31124274253778,-7.80159787542042,
-9.19669431069833));
#68182=CARTESIAN_POINT('Ctrl Pts',(-1.28061288970092,-7.80666981823595,
-9.1954446332873));
#68183=CARTESIAN_POINT('Ctrl Pts',(-1.26885123748803,-7.80859011346885,
-9.19496431638576));
#68184=CARTESIAN_POINT('Ctrl Pts',(-1.24614426854764,-7.81224476507282,
-9.19403618400884));
#68185=CARTESIAN_POINT('Ctrl Pts',(-1.23519955370831,-7.81398271491793,
-9.19358845170125));
#68186=CARTESIAN_POINT('Ctrl Pts',(-1.21003335909776,-7.81792474880978,
-9.19255810892489));
#68187=CARTESIAN_POINT('Ctrl Pts',(-1.19580945690928,-7.82011303300623,
-9.19197515135805));
#68188=CARTESIAN_POINT('Ctrl Pts',(-1.15778451774657,-7.82585683106444,
-9.1904151709958));
#68189=CARTESIAN_POINT('Ctrl Pts',(-1.13397314961645,-7.82934256608816,
-9.18943668138076));
#68190=CARTESIAN_POINT('Ctrl Pts',(-0.954550820358003,-7.85477243621321,
-9.18205235531685));
#68191=CARTESIAN_POINT('Ctrl Pts',(-0.798335317019516,-7.87218370496563,
-9.17555996198196));
#68192=CARTESIAN_POINT('Ctrl Pts',(-0.266273145815036,-7.91548511512804,
-9.15334200228412));
#68193=CARTESIAN_POINT('Ctrl Pts',(0.110864071114688,-7.91918654777777,
-9.13743517566358));
#68194=CARTESIAN_POINT('Ctrl Pts',(0.820653025232097,-7.8754246270628,-9.10769306838539));
#68195=CARTESIAN_POINT('Ctrl Pts',(1.15284512781218,-7.83369282702711,-9.09385218505519));
#68196=CARTESIAN_POINT('Ctrl Pts',(1.55927161372077,-7.75621535738181,-9.07700635531302));
#68197=CARTESIAN_POINT('Ctrl Pts',(1.6369117362078,-7.74020185540177,-9.073791504617));
#68198=CARTESIAN_POINT('Ctrl Pts',(1.7487387152716,-7.71537934730482,-9.06916342571034));
#68199=CARTESIAN_POINT('Ctrl Pts',(1.78312744624312,-7.70750427124339,-9.06774052700572));
#68200=CARTESIAN_POINT('Ctrl Pts',(1.84323865251974,-7.69331487100634,-9.06525355485945));
#68201=CARTESIAN_POINT('Ctrl Pts',(1.86898419570178,-7.68710091754045,-9.06418846602538));
#68202=CARTESIAN_POINT('Ctrl Pts',(1.91896420495767,-7.67477179178819,-9.06212079117716));
#68203=CARTESIAN_POINT('Ctrl Pts',(1.94320185030642,-7.66867082678095,-9.06111807415116));
#68204=CARTESIAN_POINT('Ctrl Pts',(2.00134680521385,-7.6537415414288,-9.05871241149536));
#68205=CARTESIAN_POINT('Ctrl Pts',(2.03522521057297,-7.64480261172378,-9.05731058516441));
#68206=CARTESIAN_POINT('Ctrl Pts',(2.16103006106165,-7.61071303863791,-9.05210358978585));
#68207=CARTESIAN_POINT('Ctrl Pts',(2.25255951199419,-7.58412682808509,-9.04831247995158));
#68208=CARTESIAN_POINT('Ctrl Pts',(3.13207863067836,-7.3113292492368,-9.01180551888132));
#68209=CARTESIAN_POINT('Ctrl Pts',(3.87747030348066,-6.94483835278237,-8.98059485519494));
#68210=CARTESIAN_POINT('Ctrl Pts',(4.83297567192742,-6.27245956658645,-8.93721530852662));
#68211=CARTESIAN_POINT('Ctrl Pts',(5.10016020297037,-6.05720656316104,-8.92451182116437));
#68212=CARTESIAN_POINT('Ctrl Pts',(5.4377939516108,-5.74697528388434,-8.90679201368324));
#68213=CARTESIAN_POINT('Ctrl Pts',(5.52132325219828,-5.66677299050848,-8.90225547573854));
#68214=CARTESIAN_POINT('Ctrl Pts',(5.61447726244746,-5.57331388302702,-8.89698328906251));
#68215=CARTESIAN_POINT('Ctrl Pts',(5.62585945773153,-5.56182415458531,-8.89633536773506));
#68216=CARTESIAN_POINT('Ctrl Pts',(5.64297820151631,-5.54443736538007,-8.89535512148201));
#68217=CARTESIAN_POINT('Ctrl Pts',(5.64874095275725,-5.53856608965044,-8.89502414333639));
#68218=CARTESIAN_POINT('Ctrl Pts',(5.65906121703248,-5.52801861245821,-8.89442960211954));
#68219=CARTESIAN_POINT('Ctrl Pts',(5.66362212403404,-5.52334573185961,-8.89416621679997));
#68220=CARTESIAN_POINT('Ctrl Pts',(5.67270450997495,-5.51401728874818,-8.89364044255779));
#68221=CARTESIAN_POINT('Ctrl Pts',(5.67722605562234,-5.50936179889564,-8.89337805760678));
#68222=CARTESIAN_POINT('Ctrl Pts',(5.68975540483465,-5.49642948322672,-8.89264919971642));
#68223=CARTESIAN_POINT('Ctrl Pts',(5.6977508521369,-5.48814074674302,-8.89218206456847));
#68224=CARTESIAN_POINT('Ctrl Pts',(5.7293023401077,-5.45528862150533,-8.890330513915));
#68225=CARTESIAN_POINT('Ctrl Pts',(5.7527176425841,-5.43059102882144,-8.88893838678116));
#68226=CARTESIAN_POINT('Ctrl Pts',(6.11739914977545,-5.04093317111175,-8.8669586239689));
#68227=CARTESIAN_POINT('Ctrl Pts',(6.42343458998371,-4.64466216723833,-8.84416370263946));
#68228=CARTESIAN_POINT('Ctrl Pts',(6.91027849575349,-3.87327838870377,-8.80218409360877));
#68229=CARTESIAN_POINT('Ctrl Pts',(7.10290522527286,-3.50756380775889,-8.78313759996896));
#68230=CARTESIAN_POINT('Ctrl Pts',(7.37195554501409,-2.88267457002611,-8.75289874219296));
#68231=CARTESIAN_POINT('Ctrl Pts',(7.4652524482483,-2.6316465691275,-8.74130937809952));
#68232=CARTESIAN_POINT('Ctrl Pts',(7.56936046918252,-2.30107214352001,-8.72681007368894));
#68233=CARTESIAN_POINT('Ctrl Pts',(7.59194230301102,-2.22543556226948,-8.72354229734134));
#68234=CARTESIAN_POINT('Ctrl Pts',(7.62225153439803,-2.11808085663359,-8.71897336166544));
#68235=CARTESIAN_POINT('Ctrl Pts',(7.63092004221935,-2.08663468531716,-8.71764335087714));
#68236=CARTESIAN_POINT('Ctrl Pts',(7.64379618663237,-2.03877120581799,-8.71563147135972));
#68237=CARTESIAN_POINT('Ctrl Pts',(7.64814591941504,-2.02239268497117,-8.71494523734481));
#68238=CARTESIAN_POINT('Ctrl Pts',(7.65514744704342,-1.99568342053183,-8.71382974819836));
#68239=CARTESIAN_POINT('Ctrl Pts',(7.65783102615425,-1.98536110744068,-8.71339951693034));
#68240=CARTESIAN_POINT('Ctrl Pts',(7.66295422846914,-1.96548991957802,-8.71257295958142));
#68241=CARTESIAN_POINT('Ctrl Pts',(7.66539689735125,-1.9559418545863,-8.71217654054457));
#68242=CARTESIAN_POINT('Ctrl Pts',(7.66978175012386,-1.93866767897448,-8.71146067913738));
#68243=CARTESIAN_POINT('Ctrl Pts',(7.67173011643462,-1.93094315946402,-8.711141047445));
#68244=CARTESIAN_POINT('Ctrl Pts',(7.67590186180983,-1.91429781692095,-8.71045331486935));
#68245=CARTESIAN_POINT('Ctrl Pts',(7.67812136586917,-1.90537602999729,-8.7100853331549));
#68246=CARTESIAN_POINT('Ctrl Pts',(7.68404734586532,-1.88137674439763,-8.7090971834772));
#68247=CARTESIAN_POINT('Ctrl Pts',(7.68772500369647,-1.86629213649934,-8.70847789873678));
#68248=CARTESIAN_POINT('Ctrl Pts',(7.70364198513721,-1.80016021042395,-8.70577078060274));
#68249=CARTESIAN_POINT('Ctrl Pts',(7.71541757570812,-1.74900210932304,-8.70369714172563));
#68250=CARTESIAN_POINT('Ctrl Pts',(7.92472111834301,-0.796422965650187,
-8.66545419616806));
#68251=CARTESIAN_POINT('Ctrl Pts',(7.96353066047508,0.132466123893695,-8.63525772346025));
#68252=CARTESIAN_POINT('Ctrl Pts',(7.79578293479666,1.38869152312414,-8.59036027384218));
#68253=CARTESIAN_POINT('Ctrl Pts',(7.72789473335369,1.72694076688382,-8.57773004012213));
#68254=CARTESIAN_POINT('Ctrl Pts',(7.63388346889942,2.07557594455706,-8.56331159461872));
#68255=CARTESIAN_POINT('Ctrl Pts',(7.62954532418908,2.0914661026012,-8.56265148428841));
#68256=CARTESIAN_POINT('Ctrl Pts',(7.62316138052284,2.11456561135005,-8.56168771421622));
#68257=CARTESIAN_POINT('Ctrl Pts',(7.62115489431734,2.12178585970747,-8.56138587363048));
#68258=CARTESIAN_POINT('Ctrl Pts',(7.6176237322187,2.13442295275313,-8.56085655697174));
#68259=CARTESIAN_POINT('Ctrl Pts',(7.61610352783852,2.13984105015289,-8.56062928415217));
#68260=CARTESIAN_POINT('Ctrl Pts',(7.61314633062187,2.15033760238937,-8.56018835073044));
#68261=CARTESIAN_POINT('Ctrl Pts',(7.6117100338266,2.15541625132694,-8.55997472140545));
#68262=CARTESIAN_POINT('Ctrl Pts',(7.60827820997389,2.16750474041263,-8.55946554857952));
#68263=CARTESIAN_POINT('Ctrl Pts',(7.60627807840751,2.17451325897941,-8.55916980157582));
#68264=CARTESIAN_POINT('Ctrl Pts',(7.59913994109129,2.19939514698995,-8.55811791860994));
#68265=CARTESIAN_POINT('Ctrl Pts',(7.5939486232358,2.21725306549521,-8.55735946864107));
#68266=CARTESIAN_POINT('Ctrl Pts',(7.50023256674871,2.53544237721292,-8.54378497258415));
#68267=CARTESIAN_POINT('Ctrl Pts',(7.39402160617019,2.83026155617129,-8.53025709486578));
#68268=CARTESIAN_POINT('Ctrl Pts',(6.9786427361017,3.79885445481074,-8.48410769816022));
#68269=CARTESIAN_POINT('Ctrl Pts',(6.59240937102754,4.43544148713559,-8.45134003963956));
#68270=CARTESIAN_POINT('Ctrl Pts',(6.06599090516504,5.07896134402616,-8.41725403750887));
#68271=CARTESIAN_POINT('Ctrl Pts',(6.00755370971461,5.14795035365396,-8.41357748663019));
#68272=CARTESIAN_POINT('Ctrl Pts',(5.93133379416083,5.23486726252392,-8.40891187106854));
#68273=CARTESIAN_POINT('Ctrl Pts',(5.91463102600849,5.2537315946749,-8.40789716828971));
#68274=CARTESIAN_POINT('Ctrl Pts',(5.88761739846727,5.28394904923023,-8.4062682601092));
#68275=CARTESIAN_POINT('Ctrl Pts',(5.87736318983997,5.29535250216881,-8.40565272745955));
#68276=CARTESIAN_POINT('Ctrl Pts',(5.85778329956495,5.3169998794336,-8.4044826481386));
#68277=CARTESIAN_POINT('Ctrl Pts',(5.84846374719143,5.32724926221128,-8.40392796180242));
#68278=CARTESIAN_POINT('Ctrl Pts',(5.82715316516277,5.35056272195397,-8.40266464361834));
#68279=CARTESIAN_POINT('Ctrl Pts',(5.81514502533279,5.36361107734446,-8.40195640977902));
#68280=CARTESIAN_POINT('Ctrl Pts',(5.78383678146588,5.39740269515026,-8.40011913878099));
#68281=CARTESIAN_POINT('Ctrl Pts',(5.76446889888869,5.41808287969694,-8.39899164335768));
#68282=CARTESIAN_POINT('Ctrl Pts',(5.65498639428042,5.53373197062209,-8.39266794800234));
#68283=CARTESIAN_POINT('Ctrl Pts',(5.56263504826618,5.62655783325126,-8.3875226496088));
#68284=CARTESIAN_POINT('Ctrl Pts',(5.33999579641027,5.83949912457571,-8.37553856295915));
#68285=CARTESIAN_POINT('Ctrl Pts',(5.20789144587378,5.95761481405866,-8.36874747607629));
#68286=CARTESIAN_POINT('Ctrl Pts',(4.67295729417637,6.40450333756107,-8.34235253655104));
#68287=CARTESIAN_POINT('Ctrl Pts',(4.24210855755709,6.69766424664624,-8.32352909040257));
#68288=CARTESIAN_POINT('Ctrl Pts',(3.47680754795278,7.11473248328316,-8.29124734570365));
#68289=CARTESIAN_POINT('Ctrl Pts',(3.15713370250557,7.26223694366356,-8.27802975843393));
#68290=CARTESIAN_POINT('Ctrl Pts',(2.81136341930225,7.39462660592953,-8.26322131561842));
#68291=CARTESIAN_POINT('Ctrl Pts',(2.79397091309997,7.40121567352775,-8.26247508256938));
#68292=CARTESIAN_POINT('Ctrl Pts',(2.76857336190541,7.41073513249896,-8.26138323758826));
#68293=CARTESIAN_POINT('Ctrl Pts',(2.76058648891211,7.41371404228849,-8.26103957099277));
#68294=CARTESIAN_POINT('Ctrl Pts',(2.74656848135597,7.41891662552823,-8.26043582802538));
#68295=CARTESIAN_POINT('Ctrl Pts',(2.74053941337218,7.42114587127686,-8.26017597905425));
#68296=CARTESIAN_POINT('Ctrl Pts',(2.72883499531462,7.42545736731242,-8.25967116257569));
#68297=CARTESIAN_POINT('Ctrl Pts',(2.72315996147496,7.42754046568385,-8.25942623034276));
#68298=CARTESIAN_POINT('Ctrl Pts',(2.70806083691074,7.43306317396299,-8.25877410666161));
#68299=CARTESIAN_POINT('Ctrl Pts',(2.69863260018575,7.43649135900221,-8.25836643857916));
#68300=CARTESIAN_POINT('Ctrl Pts',(2.66505528995629,7.44862808298485,-8.25691285777611));
#68301=CARTESIAN_POINT('Ctrl Pts',(2.64087054654533,7.45723693816457,-8.25586270670017));
#68302=CARTESIAN_POINT('Ctrl Pts',(2.33833843624085,7.56327067084448,-8.24268249784932));
#68303=CARTESIAN_POINT('Ctrl Pts',(2.05485290784931,7.64515567850627,-8.22975886696338));
#68304=CARTESIAN_POINT('Ctrl Pts',(1.36028883474807,7.80436263415105,-8.1976056377951));
#68305=CARTESIAN_POINT('Ctrl Pts',(0.946316264859822,7.86530056050492,-8.17812299066803));
#68306=CARTESIAN_POINT('Ctrl Pts',(0.260351581594936,7.91131381233239,-8.14683361910993));
#68307=CARTESIAN_POINT('Ctrl Pts',(-0.0095215141165007,7.91559178866877,
-8.13476431806485));
#68308=CARTESIAN_POINT('Ctrl Pts',(-0.449815331528298,7.90004856165765,
-8.11566431366983));
#68309=CARTESIAN_POINT('Ctrl Pts',(-0.620296928394362,7.88849400079298,
-8.10841193808687));
#68310=CARTESIAN_POINT('Ctrl Pts',(-0.876808488475988,7.86274066949055,
-8.09772869653342));
#68311=CARTESIAN_POINT('Ctrl Pts',(-0.963191348003113,7.85262676042513,
-8.0941701434276));
#68312=CARTESIAN_POINT('Ctrl Pts',(-1.06581426677893,7.83889249038618,-8.08998843837432));
#68313=CARTESIAN_POINT('Ctrl Pts',(-1.08222982753657,7.83664303971876,-8.08932093046988));
#68314=CARTESIAN_POINT('Ctrl Pts',(-1.10752207628625,7.83309621571392,-8.08829460897441));
#68315=CARTESIAN_POINT('Ctrl Pts',(-1.11640377873893,7.83183529433681,-8.08793460997713));
#68316=CARTESIAN_POINT('Ctrl Pts',(-1.1326062032396,7.82950693978519,-8.08727862262025));
#68317=CARTESIAN_POINT('Ctrl Pts',(-1.13992760303218,7.82844434048065,-8.08698247706419));
#68318=CARTESIAN_POINT('Ctrl Pts',(-1.15589885968758,7.82610345445331,-8.08633705054059));
#68319=CARTESIAN_POINT('Ctrl Pts',(-1.16454811472015,7.82482109334066,-8.08598790301029));
#68320=CARTESIAN_POINT('Ctrl Pts',(-1.18814471920527,7.82128260828196,-8.08503641381896));
#68321=CARTESIAN_POINT('Ctrl Pts',(-1.20308779196449,7.81899797164459,-8.08443500522825));
#68322=CARTESIAN_POINT('Ctrl Pts',(-1.27496247739644,7.80779817604485,-8.08154774296773));
#68323=CARTESIAN_POINT('Ctrl Pts',(-1.33180277900806,7.79830386803138,-8.07928091571683));
#68324=CARTESIAN_POINT('Ctrl Pts',(-2.31141807965984,7.62365091937267,-8.04048609622535));
#68325=CARTESIAN_POINT('Ctrl Pts',(-3.19755127425543,7.29644944788206,-8.01075817549438));
#68326=CARTESIAN_POINT('Ctrl Pts',(-4.24536322075041,6.68116546425609,-7.96878832356702));
#68327=CARTESIAN_POINT('Ctrl Pts',(-4.47730609162477,6.52800046502394,-7.95889938225381));
#68328=CARTESIAN_POINT('Ctrl Pts',(-4.77603497816572,6.30731197842756,-7.94471456086275));
#68329=CARTESIAN_POINT('Ctrl Pts',(-4.85037592285122,6.25032372009586,-7.94105632472342));
#68330=CARTESIAN_POINT('Ctrl Pts',(-4.93197140277605,6.18544187349491,-7.93687592763071));
#68331=CARTESIAN_POINT('Ctrl Pts',(-4.94024482834538,6.17883598439501,-7.93645013072549));
#68332=CARTESIAN_POINT('Ctrl Pts',(-4.95254290076452,6.16897613887925,-7.93581429581939));
#68333=CARTESIAN_POINT('Ctrl Pts',(-4.95657768442432,6.16573478540631,-7.93560522207446));
#68334=CARTESIAN_POINT('Ctrl Pts',(-4.96346831218112,6.16018804783274,-7.93524735992625));
#68335=CARTESIAN_POINT('Ctrl Pts',(-4.96632574377207,6.15788462683106,-7.93509872331718));
#68336=CARTESIAN_POINT('Ctrl Pts',(-4.97216763612319,6.15316867358971,-7.93479435504914));
#68337=CARTESIAN_POINT('Ctrl Pts',(-4.97515194587128,6.15075595701394,-7.93463860902059));
#68338=CARTESIAN_POINT('Ctrl Pts',(-4.98229482630522,6.14497257267629,-7.93426520680609));
#68339=CARTESIAN_POINT('Ctrl Pts',(-4.98645171442332,6.14159986927912,-7.93404738994458));
#68340=CARTESIAN_POINT('Ctrl Pts',(-5.00158286556078,6.12929767670716,-7.93325268036782));
#68341=CARTESIAN_POINT('Ctrl Pts',(-5.01253653709344,6.12034301570558,-7.93267382440147));
#68342=CARTESIAN_POINT('Ctrl Pts',(-5.19136163452159,5.973350866209,-7.92316635459734));
#68343=CARTESIAN_POINT('Ctrl Pts',(-5.35348634995471,5.8284925367666,-7.91372014773208));
#68344=CARTESIAN_POINT('Ctrl Pts',(-5.97856549207776,5.22188103332268,-7.87468207224398));
#68345=CARTESIAN_POINT('Ctrl Pts',(-6.38947296911945,4.71020569644179,-7.84313546437352));
#68346=CARTESIAN_POINT('Ctrl Pts',(-6.83156429926105,3.99362668756256,-7.80517238711811));
#68347=CARTESIAN_POINT('Ctrl Pts',(-6.92461870032747,3.83001135100573,-7.79684959117924));
#68348=CARTESIAN_POINT('Ctrl Pts',(-7.07375450093531,3.54455156760922,-7.78295536721175));
#68349=CARTESIAN_POINT('Ctrl Pts',(-7.13273373678086,3.42431897943836,-7.77728451172786));
#68350=CARTESIAN_POINT('Ctrl Pts',(-7.22794034794548,3.21708931240285,-7.76781757688386));
#68351=CARTESIAN_POINT('Ctrl Pts',(-7.26571626920314,3.1308390695662,-7.76396534641699));
#68352=CARTESIAN_POINT('Ctrl Pts',(-7.30827010206746,3.02875871954841,-7.75950666282897));
#68353=CARTESIAN_POINT('Ctrl Pts',(-7.31454837927487,3.01356487864667,-7.75884560983604));
#68354=CARTESIAN_POINT('Ctrl Pts',(-7.32408409446083,2.99028246302253,-7.75783657059551));
#68355=CARTESIAN_POINT('Ctrl Pts',(-7.32737557747535,2.98220793686286,-7.75748734945598));
#68356=CARTESIAN_POINT('Ctrl Pts',(-7.333347424145,2.96748848281314,-7.75685204649727));
#68357=CARTESIAN_POINT('Ctrl Pts',(-7.33603212043261,2.96084532983361,-7.75656580797129));
#68358=CARTESIAN_POINT('Ctrl Pts',(-7.34180984620272,2.94649252288695,-7.75594842173445));
#68359=CARTESIAN_POINT('Ctrl Pts',(-7.34489976676788,2.9387816220232,-7.75561738665688));
#68360=CARTESIAN_POINT('Ctrl Pts',(-7.35322605953946,2.91790818710773,-7.75472302348134));
#68361=CARTESIAN_POINT('Ctrl Pts',(-7.35843924407603,2.90473640201388,-7.75416053247616));
#68362=CARTESIAN_POINT('Ctrl Pts',(-7.38261656196437,2.84316649289902,-7.75153995106515));
#68363=CARTESIAN_POINT('Ctrl Pts',(-7.40113897744871,2.79459567423399,-7.74949776075982));
#68364=CARTESIAN_POINT('Ctrl Pts',(-7.74561361436762,1.86383675987184,-7.7108281406531));
#68365=CARTESIAN_POINT('Ctrl Pts',(-7.91210823868078,0.93091089069761,-7.68126784400183));
#68366=CARTESIAN_POINT('Ctrl Pts',(-7.91067420643559,-0.279726549592703,
-7.63828233622777));
#68367=CARTESIAN_POINT('Ctrl Pts',(-7.89649511889754,-0.549866780207448,
-7.62830255983803));
#68368=CARTESIAN_POINT('Ctrl Pts',(-7.86685871385677,-0.834693178137426,
-7.61687089892598));
#68369=CARTESIAN_POINT('Ctrl Pts',(-7.86514867750749,-0.850655633416672,
-7.61622717993366));
#68370=CARTESIAN_POINT('Ctrl Pts',(-7.86275367237782,-0.872387205033589,
-7.61534653216811));
#68371=CARTESIAN_POINT('Ctrl Pts',(-7.86211093201363,-0.878160828301624,
-7.61511215409261));
#68372=CARTESIAN_POINT('Ctrl Pts',(-7.86100444735419,-0.888001596550004,
-7.6147119815516));
#68373=CARTESIAN_POINT('Ctrl Pts',(-7.86054390395179,-0.892069106468237,
-7.61454637613297));
#68374=CARTESIAN_POINT('Ctrl Pts',(-7.85964576465246,-0.899946755579525,
-7.61422525684078));
#68375=CARTESIAN_POINT('Ctrl Pts',(-7.85920855454718,-0.903756938963826,
-7.61406976559411));
#68376=CARTESIAN_POINT('Ctrl Pts',(-7.8581626124287,-0.912813921972404,
-7.61369974098891));
#68377=CARTESIAN_POINT('Ctrl Pts',(-7.85755139664994,-0.918060427349082,
-7.61348506319907));
#68378=CARTESIAN_POINT('Ctrl Pts',(-7.85572704962464,-0.933584826776816,
-7.61284886052932));
#68379=CARTESIAN_POINT('Ctrl Pts',(-7.85449900784106,-0.943860922420935,
-7.61242647723079));
#68380=CARTESIAN_POINT('Ctrl Pts',(-7.84468699522595,-1.02462122764104,
-7.60909719439772));
#68381=CARTESIAN_POINT('Ctrl Pts',(-7.83517483661326,-1.09498739903813,
-7.60613799259582));
#68382=CARTESIAN_POINT('Ctrl Pts',(-7.79364284498898,-1.3738856234091,-7.59420221452049));
#68383=CARTESIAN_POINT('Ctrl Pts',(-7.75423548794202,-1.58121826535327,
-7.58486954036107));
#68384=CARTESIAN_POINT('Ctrl Pts',(-7.56013635059216,-2.41842178745667,
-7.54594751398681));
#68385=CARTESIAN_POINT('Ctrl Pts',(-7.33656599118316,-3.02974145159812,
-7.51485800424289));
#68386=CARTESIAN_POINT('Ctrl Pts',(-6.98647935857242,-3.71311946838392,
-7.48035363647049));
#68387=CARTESIAN_POINT('Ctrl Pts',(-6.92969666724075,-3.81804341851617,
-7.47505505358298));
#68388=CARTESIAN_POINT('Ctrl Pts',(-6.72907406849213,-4.16952591649218,
-7.45732453864063));
#68389=CARTESIAN_POINT('Ctrl Pts',(-6.57426815021812,-4.40958103911321,
-7.44525689302093));
#68390=CARTESIAN_POINT('Ctrl Pts',(-6.39204380645067,-4.66115123603427,
-7.43265107135979));
#68391=CARTESIAN_POINT('Ctrl Pts',(-6.37717724909139,-4.68147041191776,
-7.43163312196305));
#68392=CARTESIAN_POINT('Ctrl Pts',(-6.35621640852931,-4.70983394606143,
-7.43021239324831));
#68393=CARTESIAN_POINT('Ctrl Pts',(-6.35020342601233,-4.71793803273492,
-7.42980648574624));
#68394=CARTESIAN_POINT('Ctrl Pts',(-6.33976154478517,-4.73195510681788,
-7.4291044542237));
#68395=CARTESIAN_POINT('Ctrl Pts',(-6.33533984549562,-4.73787342804324,
-7.42880805275665));
#68396=CARTESIAN_POINT('Ctrl Pts',(-6.32614124215157,-4.75014960028148,
-7.42819325871944));
#68397=CARTESIAN_POINT('Ctrl Pts',(-6.32136302722869,-4.75650646159298,
-7.42787491735421));
#68398=CARTESIAN_POINT('Ctrl Pts',(-6.31012278217441,-4.77141345262321,
-7.42712842259818));
#68399=CARTESIAN_POINT('Ctrl Pts',(-6.30365293930875,-4.77995768641166,
-7.42670057258357));
#68400=CARTESIAN_POINT('Ctrl Pts',(-6.28258845217747,-4.80765881991446,
-7.42531348809021));
#68401=CARTESIAN_POINT('Ctrl Pts',(-6.26792362646865,-4.82676231171841,
-7.42435698043247));
#68402=CARTESIAN_POINT('Ctrl Pts',(-6.00637740843168,-5.16426981685921,
-7.40745807197932));
#68403=CARTESIAN_POINT('Ctrl Pts',(-5.73560624594877,-5.46343448781761,
-7.39252106889034));
#68404=CARTESIAN_POINT('Ctrl Pts',(-5.1801956419447,-5.99006260043586,-7.36522659529685));
#68405=CARTESIAN_POINT('Ctrl Pts',(-4.9003651219561,-6.22106923450769,-7.35278293889922));
#68406=CARTESIAN_POINT('Ctrl Pts',(-4.44899597586979,-6.54427195683834,
-7.33347693460576));
#68407=CARTESIAN_POINT('Ctrl Pts',(-4.28826250143942,-6.6507039009242,-7.32673147769319));
#68408=CARTESIAN_POINT('Ctrl Pts',(-3.86881273578883,-6.90691622078107,
-7.30910513803278));
#68409=CARTESIAN_POINT('Ctrl Pts',(-3.6052539477848,-7.04807425490654,-7.29795838794914));
#68410=CARTESIAN_POINT('Ctrl Pts',(-3.31655998018063,-7.1822512402361,-7.28527062250137));
#68411=CARTESIAN_POINT('Ctrl Pts',(-3.29880603938023,-7.19042291430389,
-7.28448906702831));
#68412=CARTESIAN_POINT('Ctrl Pts',(-3.27223103826429,-7.20253555145514,
-7.28331743085811));
#68413=CARTESIAN_POINT('Ctrl Pts',(-3.26343267189909,-7.20652631527845,
-7.28292924126929));
#68414=CARTESIAN_POINT('Ctrl Pts',(-3.24828413876978,-7.21336395747949,
-7.28226040517025));
#68415=CARTESIAN_POINT('Ctrl Pts',(-3.24193747421054,-7.21621859717651,
-7.28198004548194));
#68416=CARTESIAN_POINT('Ctrl Pts',(-3.228846715707,-7.22208587911677,-7.28140148600468));
#68417=CARTESIAN_POINT('Ctrl Pts',(-3.22210215428629,-7.22509745718269,
-7.28110324813216));
#68418=CARTESIAN_POINT('Ctrl Pts',(-3.20642350641933,-7.23207195900676,
-7.28040960679588));
#68419=CARTESIAN_POINT('Ctrl Pts',(-3.19748628207698,-7.23602777757139,
-7.28001395245277));
#68420=CARTESIAN_POINT('Ctrl Pts',(-3.16909208596204,-7.24853281802285,
-7.27875614278746));
#68421=CARTESIAN_POINT('Ctrl Pts',(-3.14960805820633,-7.25702016904315,
-7.27789186470762));
#68422=CARTESIAN_POINT('Ctrl Pts',(-2.72887923290979,-7.4382784517682,-7.25920665431084));
#68423=CARTESIAN_POINT('Ctrl Pts',(-2.3140513120038,-7.57759274281634,-7.24039864737228));
#68424=CARTESIAN_POINT('Ctrl Pts',(-1.62057758538033,-7.74819680808196,
-7.20967601638181));
#68425=CARTESIAN_POINT('Ctrl Pts',(-1.34798951283231,-7.80024061888691,
-7.19776053405291));
#68426=CARTESIAN_POINT('Ctrl Pts',(-0.446219176843177,-7.92371900068378,
-7.15905792973044));
#68427=CARTESIAN_POINT('Ctrl Pts',(0.188846440655802,-7.934028686977,-7.13294710741225));
#68428=CARTESIAN_POINT('Ctrl Pts',(0.894323082355043,-7.86065789268268,
-7.10410376547628));
#68429=CARTESIAN_POINT('Ctrl Pts',(0.970184268632368,-7.85165580628152,
-7.10100765877162));
#68430=CARTESIAN_POINT('Ctrl Pts',(1.0744599350618,-7.83774756032486,-7.09675943684174));
#68431=CARTESIAN_POINT('Ctrl Pts',(1.10299531505903,-7.83378275892561,-7.09559767333884));
#68432=CARTESIAN_POINT('Ctrl Pts',(1.15195926578635,-7.82670670332844,-7.09360549901223));
#68433=CARTESIAN_POINT('Ctrl Pts',(1.17239844178364,-7.82367112464099,-7.09277428874872));
#68434=CARTESIAN_POINT('Ctrl Pts',(1.2145131979512,-7.8172475967819,-7.0910623669303));
#68435=CARTESIAN_POINT('Ctrl Pts',(1.23618705655701,-7.8138494906213,-7.09018177356707));
#68436=CARTESIAN_POINT('Ctrl Pts',(1.28667622021142,-7.80571828931236,-7.08813139075801));
#68437=CARTESIAN_POINT('Ctrl Pts',(1.31548004241416,-7.80091571381796,-7.08696238469085));
#68438=CARTESIAN_POINT('Ctrl Pts',(1.40832849394681,-7.78490585082924,-7.08319630510584));
#68439=CARTESIAN_POINT('Ctrl Pts',(1.47226200528582,-7.77306843743495,-7.08060644036147));
#68440=CARTESIAN_POINT('Ctrl Pts',(1.79559888224548,-7.70906962129087,-7.06752168639807));
#68441=CARTESIAN_POINT('Ctrl Pts',(2.05241796124809,-7.64470505467777,-7.05717840789458));
#68442=CARTESIAN_POINT('Ctrl Pts',(2.64190703786296,-7.46511202571952,-7.03331244957922));
#68443=CARTESIAN_POINT('Ctrl Pts',(2.971072121005,-7.34032014217191,-7.01989729717553));
#68444=CARTESIAN_POINT('Ctrl Pts',(3.51762356168421,-7.09030590046178,-6.99669071652824));
#68445=CARTESIAN_POINT('Ctrl Pts',(3.73936811678915,-6.97590369364318,-6.98698748684759));
#68446=CARTESIAN_POINT('Ctrl Pts',(3.97815201314763,-6.83804956817386,-6.97596592779701));
#68447=CARTESIAN_POINT('Ctrl Pts',(4.00090630676524,-6.82476109876138,-6.97490967479221));
#68448=CARTESIAN_POINT('Ctrl Pts',(4.03500955689731,-6.8046156887428,-6.97331717850109));
#68449=CARTESIAN_POINT('Ctrl Pts',(4.04640836473416,-6.79784349186522,-6.97278331474776));
#68450=CARTESIAN_POINT('Ctrl Pts',(4.06717789657399,-6.78543326211514,-6.97180772352972));
#68451=CARTESIAN_POINT('Ctrl Pts',(4.07655406735528,-6.77980438744584,-6.97136624007879));
#68452=CARTESIAN_POINT('Ctrl Pts',(4.09682851716392,-6.76757559485421,-6.97040932454151));
#68453=CARTESIAN_POINT('Ctrl Pts',(4.1077225798117,-6.76096875728948,-6.96989371483942));
#68454=CARTESIAN_POINT('Ctrl Pts',(4.13782914980523,-6.74261063236277,-6.96846487679374));
#68455=CARTESIAN_POINT('Ctrl Pts',(4.15700746423446,-6.73080360341254,-6.96755026431551));
#68456=CARTESIAN_POINT('Ctrl Pts',(4.26387730647417,-6.6643787566169,-6.96242946575371));
#68457=CARTESIAN_POINT('Ctrl Pts',(4.35054176666697,-6.60812981620152,-6.95818560532621));
#68458=CARTESIAN_POINT('Ctrl Pts',(4.8002581476746,-6.30356247507699,-6.93572780376755));
#68459=CARTESIAN_POINT('Ctrl Pts',(5.14323303337616,-6.02698356156208,-6.91711733154376));
#68460=CARTESIAN_POINT('Ctrl Pts',(5.62035679582944,-5.57169287437059,-6.88953790763791));
#68461=CARTESIAN_POINT('Ctrl Pts',(5.77289124600718,-5.41349253441233,-6.88041017360203));
#68462=CARTESIAN_POINT('Ctrl Pts',(6.02736796030635,-5.12655877909454,-6.86462800436428));
#68463=CARTESIAN_POINT('Ctrl Pts',(6.13225624872269,-5.00062037580189,-6.85793749115287));
#68464=CARTESIAN_POINT('Ctrl Pts',(6.26273054819979,-4.8336769845101,-6.84935359368948));
#68465=CARTESIAN_POINT('Ctrl Pts',(6.29195696899521,-4.79557135753092,-6.84741267676751));
#68466=CARTESIAN_POINT('Ctrl Pts',(6.338307652517,-4.73398578266172,-6.84430446332542));
#68467=CARTESIAN_POINT('Ctrl Pts',(6.35565257611613,-4.7106735853434,-6.84313439116604));
#68468=CARTESIAN_POINT('Ctrl Pts',(6.38688601933766,-4.66820818654298,-6.841014528845));
#68469=CARTESIAN_POINT('Ctrl Pts',(6.40081779391338,-4.64908725128004,-6.84006421447154));
#68470=CARTESIAN_POINT('Ctrl Pts',(6.43372722239032,-4.60349172491967,-6.83780790684811));
#68471=CARTESIAN_POINT('Ctrl Pts',(6.45262756650621,-4.57696182325523,-6.83650285801946));
#68472=CARTESIAN_POINT('Ctrl Pts',(6.50657196257102,-4.50024323757508,-6.83275077888843));
#68473=CARTESIAN_POINT('Ctrl Pts',(6.54119815672911,-4.44976343616691,-6.83030863296799));
#68474=CARTESIAN_POINT('Ctrl Pts',(6.73934823275084,-4.15357864077196,-6.81612608438649));
#68475=CARTESIAN_POINT('Ctrl Pts',(6.88960972709752,-3.89927100359156,-6.80449718637532));
#68476=CARTESIAN_POINT('Ctrl Pts',(7.20120056770127,-3.2974220662573,-6.77811472530825));
#68477=CARTESIAN_POINT('Ctrl Pts',(7.35221888813989,-2.94536503772033,-6.76356602237524));
#68478=CARTESIAN_POINT('Ctrl Pts',(7.62620681516148,-2.15246605789814,-6.73217600937995));
#68479=CARTESIAN_POINT('Ctrl Pts',(7.73763950277963,-1.70910858941191,-6.71550966543826));
#68480=CARTESIAN_POINT('Ctrl Pts',(7.81258143095871,-1.24406995030568,-6.69762218793949));
#68481=CARTESIAN_POINT('Ctrl Pts',(7.81488790120096,-1.22949816859579,-6.69706121136641));
#68482=CARTESIAN_POINT('Ctrl Pts',(7.81921356072185,-1.20166560061616,-6.69598870245183));
#68483=CARTESIAN_POINT('Ctrl Pts',(7.82123981214889,-1.18840595899742,-6.69547730730544));
#68484=CARTESIAN_POINT('Ctrl Pts',(7.8277380122532,-1.14514568797451,-6.69380726468019));
#68485=CARTESIAN_POINT('Ctrl Pts',(7.83207112820847,-1.1151245942258,-6.6926458242466));
#68486=CARTESIAN_POINT('Ctrl Pts',(7.8550890115713,-0.948893947528234,-6.68619817136802));
#68487=CARTESIAN_POINT('Ctrl Pts',(7.87039268466067,-0.812243716793359,
-6.6808366680563));
#68488=CARTESIAN_POINT('Ctrl Pts',(7.88353927771674,-0.658789061602054,
-6.67469009621958));
#68489=CARTESIAN_POINT('Ctrl Pts',(7.88489940862359,-0.642305131528015,
-6.67402821121943));
#68490=CARTESIAN_POINT('Ctrl Pts',(7.886874633313,-0.617414422055768,-6.67302616807881));
#68491=CARTESIAN_POINT('Ctrl Pts',(7.88752800636605,-0.609010671729094,
-6.6726874054418));
#68492=CARTESIAN_POINT('Ctrl Pts',(7.88863901477921,-0.594419038913248,
-6.67209840628921));
#68493=CARTESIAN_POINT('Ctrl Pts',(7.88910280430723,-0.588231622861941,
-6.67184839901681));
#68494=CARTESIAN_POINT('Ctrl Pts',(7.89005320214173,-0.575349050020596,
-6.67132734025234));
#68495=CARTESIAN_POINT('Ctrl Pts',(7.89053856887669,-0.568653809173042,
-6.67105624208396));
#68496=CARTESIAN_POINT('Ctrl Pts',(7.89164978450106,-0.553050116266937,
-6.67042372291975));
#68497=CARTESIAN_POINT('Ctrl Pts',(7.892269070931,-0.544141216501954,-6.67006205013621));
#68498=CARTESIAN_POINT('Ctrl Pts',(7.89418810657139,-0.515841853599745,
-6.66891143278159));
#68499=CARTESIAN_POINT('Ctrl Pts',(7.89543148405543,-0.496447732732629,
-6.66812027695225));
#68500=CARTESIAN_POINT('Ctrl Pts',(7.89815391279287,-0.451383338122713,
-6.66627550041345));
#68501=CARTESIAN_POINT('Ctrl Pts',(7.89957929282201,-0.425710138581909,
-6.66521968041488));
#68502=CARTESIAN_POINT('Ctrl Pts',(7.91256459359305,-0.169241561297714,
-6.65462020418663));
#68503=CARTESIAN_POINT('Ctrl Pts',(7.91413036463311,0.0619164898409031,
-6.64460483783473));
#68504=CARTESIAN_POINT('Ctrl Pts',(7.8923505532015,0.650005682747266,-6.61838909212137));
#68505=CARTESIAN_POINT('Ctrl Pts',(7.85492407844523,1.00591212387657,-6.60185687551704));
#68506=CARTESIAN_POINT('Ctrl Pts',(7.67830094638278,2.0195106240426,-6.55450047506731));
#68507=CARTESIAN_POINT('Ctrl Pts',(7.47928431222842,2.66369992711587,-6.52430445917238));
#68508=CARTESIAN_POINT('Ctrl Pts',(7.18326907162709,3.31458162294114,-6.49506861655921));
#68509=CARTESIAN_POINT('Ctrl Pts',(7.16497043859591,3.35395357444207,-6.49330410123121));
#68510=CARTESIAN_POINT('Ctrl Pts',(7.14017219389706,3.4061810564505,-6.49096848668932));
#68511=CARTESIAN_POINT('Ctrl Pts',(7.1339604270953,3.41917197215601,-6.4903879500562));
#68512=CARTESIAN_POINT('Ctrl Pts',(7.12422191116144,3.43939644707031,-6.48948479890236));
#68513=CARTESIAN_POINT('Ctrl Pts',(7.1207195498117,3.44664167748648,-6.48916138135952));
#68514=CARTESIAN_POINT('Ctrl Pts',(7.11369264876076,3.46112159010717,-6.48851526998474));
#68515=CARTESIAN_POINT('Ctrl Pts',(7.1101681127232,3.46835626368343,-6.48819257654265));
#68516=CARTESIAN_POINT('Ctrl Pts',(7.10220952267399,3.4846294280235,-6.48746701381496));
#68517=CARTESIAN_POINT('Ctrl Pts',(7.09776923861415,3.49366486528267,-6.4870643512981));
#68518=CARTESIAN_POINT('Ctrl Pts',(7.08465418284861,3.52022420402518,-6.48588130511104));
#68519=CARTESIAN_POINT('Ctrl Pts',(7.07593164784833,3.53772450295838,-6.48510250638997));
#68520=CARTESIAN_POINT('Ctrl Pts',(7.00900876765221,3.67075630605786,-6.47918764708619));
#68521=CARTESIAN_POINT('Ctrl Pts',(6.94804598526991,3.78487973336984,-6.47414458428931));
#68522=CARTESIAN_POINT('Ctrl Pts',(6.72663625118153,4.17596860061387,-6.45693300332377));
#68523=CARTESIAN_POINT('Ctrl Pts',(6.55220089327432,4.44466334375616,-6.44524673685178));
#68524=CARTESIAN_POINT('Ctrl Pts',(5.99681230940147,5.19611172136657,-6.41209590930528));
#68525=CARTESIAN_POINT('Ctrl Pts',(5.57538658223575,5.64591251024441,-6.39173290189985));
#68526=CARTESIAN_POINT('Ctrl Pts',(4.91838685278472,6.20111723891688,-6.36051517407707));
#68527=CARTESIAN_POINT('Ctrl Pts',(4.72328127439732,6.35098364469872,-6.35127594927098));
#68528=CARTESIAN_POINT('Ctrl Pts',(4.507418197582,6.50133812660327,-6.34077891523004));
#68529=CARTESIAN_POINT('Ctrl Pts',(4.49328676043122,6.51111283313583,-6.34009067427706));
#68530=CARTESIAN_POINT('Ctrl Pts',(4.47331793050744,6.52482929300462,-6.3391167826426));
#68531=CARTESIAN_POINT('Ctrl Pts',(4.46750687590672,6.52880945682542,-6.338833213155));
#68532=CARTESIAN_POINT('Ctrl Pts',(4.4573848190239,6.53572251260635,-6.33833900535508));
#68533=CARTESIAN_POINT('Ctrl Pts',(4.45307621264733,6.53865891684223,-6.33812855377261));
#68534=CARTESIAN_POINT('Ctrl Pts',(4.44407768582917,6.54477857920941,-6.33768885446171));
#68535=CARTESIAN_POINT('Ctrl Pts',(4.43938724129558,6.54796106052377,-6.3374595662355));
#68536=CARTESIAN_POINT('Ctrl Pts',(4.42841707301928,6.55538714879808,-6.33692308084262));
#68537=CARTESIAN_POINT('Ctrl Pts',(4.42213466940937,6.55962677355026,-6.3366156790331));
#68538=CARTESIAN_POINT('Ctrl Pts',(4.40173506148046,6.57335064448131,-6.33561699790959));
#68539=CARTESIAN_POINT('Ctrl Pts',(4.38759342296387,6.58279835596632,-6.33492388124573));
#68540=CARTESIAN_POINT('Ctrl Pts',(4.35415590536986,6.60498159539983,-6.33328334739964));
#68541=CARTESIAN_POINT('Ctrl Pts',(4.33483450040769,6.6176782456542,-6.33233407602561));
#68542=CARTESIAN_POINT('Ctrl Pts',(4.26701367169305,6.66182079917276,-6.32899817589466));
#68543=CARTESIAN_POINT('Ctrl Pts',(4.21822610840024,6.6928193105453,-6.32659166425935));
#68544=CARTESIAN_POINT('Ctrl Pts',(3.98985622621272,6.83443141243784,-6.31531072553219));
#68545=CARTESIAN_POINT('Ctrl Pts',(3.80624057010353,6.93836667378796,-6.3061968545563));
#68546=CARTESIAN_POINT('Ctrl Pts',(3.31377034648752,7.1916918735842,-6.28200069492805));
#68547=CARTESIAN_POINT('Ctrl Pts',(2.9989650574765,7.32855506027376,-6.26679406440977));
#68548=CARTESIAN_POINT('Ctrl Pts',(2.2191234370551,7.60890288476552,-6.23062978736214));
#68549=CARTESIAN_POINT('Ctrl Pts',(1.74778556160344,7.7307971844164,-6.21004761986399));
#68550=CARTESIAN_POINT('Ctrl Pts',(1.22815964623729,7.815189779488,-6.18870757379603));
#68551=CARTESIAN_POINT('Ctrl Pts',(1.18805882691241,7.82138630083705,-6.18706852957345));
#68552=CARTESIAN_POINT('Ctrl Pts',(1.12979341214207,7.82993123758557,-6.18469781123338));
#68553=CARTESIAN_POINT('Ctrl Pts',(1.11166572885928,7.83252549628893,-6.18396173610088));
#68554=CARTESIAN_POINT('Ctrl Pts',(1.07968299366997,7.83698928695997,-6.18266566509778));
#68555=CARTESIAN_POINT('Ctrl Pts',(1.0658317075291,7.8388850752775,-6.18210520963947));
#68556=CARTESIAN_POINT('Ctrl Pts',(1.03718744258772,7.84272821347573,-6.18094792420604));
#68557=CARTESIAN_POINT('Ctrl Pts',(1.02239383049002,7.84467045060511,-6.18035118484791));
#68558=CARTESIAN_POINT('Ctrl Pts',(0.984455661850834,7.84954217121539,-6.17882322750161));
#68559=CARTESIAN_POINT('Ctrl Pts',(0.961303443864271,7.85241115473449,-6.17789304132472));
#68560=CARTESIAN_POINT('Ctrl Pts',(0.870908014071688,7.86320702261716,-6.17426969528348));
#68561=CARTESIAN_POINT('Ctrl Pts',(0.803576091411761,7.87037299555759,-6.17158888697343));
#68562=CARTESIAN_POINT('Ctrl Pts',(0.423701556982069,7.90587636413933,-6.15656241190318));
#68563=CARTESIAN_POINT('Ctrl Pts',(0.109774555492435,7.91646176373229,-6.14453291973393));
#68564=CARTESIAN_POINT('Ctrl Pts',(-0.72373035540576,7.89496509585911,-6.11320465811824));
#68565=CARTESIAN_POINT('Ctrl Pts',(-1.24089743969202,7.83035244597318,-6.09445532131167));
#68566=CARTESIAN_POINT('Ctrl Pts',(-1.91007313801748,7.67874769603705,-6.0688693420363));
#68567=CARTESIAN_POINT('Ctrl Pts',(-2.07097038843757,7.63692507535028,-6.06260398268898));
#68568=CARTESIAN_POINT('Ctrl Pts',(-2.35358145886287,7.55387663278453,-6.05125959381908));
#68569=CARTESIAN_POINT('Ctrl Pts',(-2.47583373593865,7.51469515203176,-6.04623671087654));
#68570=CARTESIAN_POINT('Ctrl Pts',(-2.6120973979039,7.46733694994792,-6.04046412943302));
#68571=CARTESIAN_POINT('Ctrl Pts',(-2.62710421253011,7.46207058343734,-6.03982599134947));
#68572=CARTESIAN_POINT('Ctrl Pts',(-2.64974614242114,7.45404804589112,-6.03885944194462));
#68573=CARTESIAN_POINT('Ctrl Pts',(-2.65739311282282,7.4513253004438,-6.03853235843499));
#68574=CARTESIAN_POINT('Ctrl Pts',(-2.67066560124264,7.44657652868678,-6.03796351498088));
#68575=CARTESIAN_POINT('Ctrl Pts',(-2.6762930464999,7.44455588200309,-6.03772197284453));
#68576=CARTESIAN_POINT('Ctrl Pts',(-2.68800695926523,7.4403347689571,-6.03721843558106));
#68577=CARTESIAN_POINT('Ctrl Pts',(-2.69409302596184,7.43813321031149,-6.03695639577885));
#68578=CARTESIAN_POINT('Ctrl Pts',(-2.70614892979334,7.43375539985482,-6.03643647257837));
#68579=CARTESIAN_POINT('Ctrl Pts',(-2.71211886053426,7.43157941901413,-6.03617860059287));
#68580=CARTESIAN_POINT('Ctrl Pts',(-2.73235935578889,7.42417432067414,-6.03530289304797));
#68581=CARTESIAN_POINT('Ctrl Pts',(-2.7466174145811,7.41891129253307,-6.03468362599165));
#68582=CARTESIAN_POINT('Ctrl Pts',(-2.85822826901568,7.3773469162973,-6.02981678525168));
#68583=CARTESIAN_POINT('Ctrl Pts',(-2.95486226950634,7.33917603771479,-6.02548504179587));
#68584=CARTESIAN_POINT('Ctrl Pts',(-3.19424323362779,7.23912473227185,-6.01442979544173));
#68585=CARTESIAN_POINT('Ctrl Pts',(-3.33595529210755,7.17492263037374,-6.00760562078298));
#68586=CARTESIAN_POINT('Ctrl Pts',(-3.60462697218734,7.04352122134955,-5.99424858274313));
#68587=CARTESIAN_POINT('Ctrl Pts',(-3.73183466796555,6.97695742594686,-5.98773619813309));
#68588=CARTESIAN_POINT('Ctrl Pts',(-4.34789100008118,6.63292437542874,-5.95548552826682));
#68589=CARTESIAN_POINT('Ctrl Pts',(-4.80807413654674,6.30732654307403,-5.92928534305092));
#68590=CARTESIAN_POINT('Ctrl Pts',(-5.43886368862264,5.75154511367466,-5.89255629731899));
#68591=CARTESIAN_POINT('Ctrl Pts',(-5.637999870792,5.55648160860257,-5.88078665514577));
#68592=CARTESIAN_POINT('Ctrl Pts',(-5.84279391990271,5.33350394575173,-5.86851244551114));
#68593=CARTESIAN_POINT('Ctrl Pts',(-5.85906104673971,5.31562872991664,-5.8675361607289));
#68594=CARTESIAN_POINT('Ctrl Pts',(-5.88172418509079,5.29049479641489,-5.86617411198189));
#68595=CARTESIAN_POINT('Ctrl Pts',(-5.88818910186304,5.2832985607415,-5.86578535335069));
#68596=CARTESIAN_POINT('Ctrl Pts',(-5.89936069479567,5.27081724941683,-5.8651131821257));
#68597=CARTESIAN_POINT('Ctrl Pts',(-5.90407350197084,5.26553769027882,-5.86482950373143));
#68598=CARTESIAN_POINT('Ctrl Pts',(-5.91384140091286,5.25456552383236,-5.86424129516887));
#68599=CARTESIAN_POINT('Ctrl Pts',(-5.91889537404334,5.24887192746876,-5.86393681350339));
#68600=CARTESIAN_POINT('Ctrl Pts',(-5.93073572847056,5.23549422871883,-5.86322315051854));
#68601=CARTESIAN_POINT('Ctrl Pts',(-5.93751541497462,5.22780420424265,-5.86281425851499));
#68602=CARTESIAN_POINT('Ctrl Pts',(-5.95945688594461,5.20281881597365,-5.86149010130662));
#68603=CARTESIAN_POINT('Ctrl Pts',(-5.97455826324583,5.18547042978625,-5.86057743816256));
#68604=CARTESIAN_POINT('Ctrl Pts',(-6.24102363280973,4.87664704009835,-5.84444950590886));
#68605=CARTESIAN_POINT('Ctrl Pts',(-6.4708730901511,4.56726475939106,-5.83019586386764));
#68606=CARTESIAN_POINT('Ctrl Pts',(-6.81468299319699,4.02612020945823,-5.8075519417491));
#68607=CARTESIAN_POINT('Ctrl Pts',(-6.94147973386592,3.80334240948382,-5.79879925262536));
#68608=CARTESIAN_POINT('Ctrl Pts',(-7.10799882641336,3.47460621699002,-5.78634938312584));
#68609=CARTESIAN_POINT('Ctrl Pts',(-7.1566120820879,3.3733424523138,-5.78257397301007));
#68610=CARTESIAN_POINT('Ctrl Pts',(-7.22659820657343,3.21923002309951,-5.77688128262631));
#68611=CARTESIAN_POINT('Ctrl Pts',(-7.24958302592744,3.16712953886381,-5.7749656889427));
#68612=CARTESIAN_POINT('Ctrl Pts',(-7.29710025289357,3.05619238770104,-5.77089856835598));
#68613=CARTESIAN_POINT('Ctrl Pts',(-7.32148803492552,2.99729826849927,-5.76874633273013));
#68614=CARTESIAN_POINT('Ctrl Pts',(-7.51363986592407,2.51692711964419,-5.75120755913347));
#68615=CARTESIAN_POINT('Ctrl Pts',(-7.64556065209967,2.08207034366566,-5.7354574096765));
#68616=CARTESIAN_POINT('Ctrl Pts',(-7.74542488003577,1.61032179897296,-5.71637531943821));
#68617=CARTESIAN_POINT('Ctrl Pts',(-7.75120950260038,1.58224336761794,-5.71523212198671));
#68618=CARTESIAN_POINT('Ctrl Pts',(-7.75839358635542,1.54638688361047,-5.71376209934516));
#68619=CARTESIAN_POINT('Ctrl Pts',(-7.75993425178953,1.5386370077482,-5.71344377097987));
#68620=CARTESIAN_POINT('Ctrl Pts',(-7.76236334877504,1.52632168114289,-5.71293693922529));
#68621=CARTESIAN_POINT('Ctrl Pts',(-7.76325937285701,1.52175771471533,-5.71274889837766));
#68622=CARTESIAN_POINT('Ctrl Pts',(-7.76484569049828,1.51363982165464,-5.7124140490435));
#68623=CARTESIAN_POINT('Ctrl Pts',(-7.76553757106239,1.51008620259842,-5.71226733799124));
#68624=CARTESIAN_POINT('Ctrl Pts',(-7.76712948980867,1.50187980444965,-5.71192823384938));
#68625=CARTESIAN_POINT('Ctrl Pts',(-7.76802778597014,1.49722669454849,-5.71173573316251));
#68626=CARTESIAN_POINT('Ctrl Pts',(-7.77055799879294,1.48405680009977,-5.71119024848579));
#68627=CARTESIAN_POINT('Ctrl Pts',(-7.77218008486971,1.47553818170409,-5.71083665822949));
#68628=CARTESIAN_POINT('Ctrl Pts',(-7.77577285308339,1.45649994290278,-5.71004475959999));
#68629=CARTESIAN_POINT('Ctrl Pts',(-7.77773619732157,1.44597897254671,-5.70960600625238));
#68630=CARTESIAN_POINT('Ctrl Pts',(-7.8664562891401,0.965145930965705,-5.68950341812358));
#68631=CARTESIAN_POINT('Ctrl Pts',(-7.91039819384677,0.487989914473766,
-5.66740103070192));
#68632=CARTESIAN_POINT('Ctrl Pts',(-7.91099386085047,0.00985563728471597,
-5.64509922291617));
#68633=CARTESIAN_POINT('',(-7.8993869982124,-0.00109440781040144,-3.6423308392815));
#68634=CARTESIAN_POINT('Ctrl Pts',(-7.91099369906704,0.00998465430474249,
-5.64233150823678));
#68635=CARTESIAN_POINT('Ctrl Pts',(-7.91123261204234,-0.179309735316508,
-5.63470551807132));
#68636=CARTESIAN_POINT('Ctrl Pts',(-7.90467340181398,-0.368885852312452,
-5.62707952790585));
#68637=CARTESIAN_POINT('Ctrl Pts',(-7.89128247331207,-0.558195240393375,
-5.61945353774039));
#68638=CARTESIAN_POINT('Ctrl Pts',(-7.87790258564991,-0.747348542612155,
-5.61183383521476));
#68639=CARTESIAN_POINT('Ctrl Pts',(-7.85770221405668,-0.936235187822579,
-5.60421413268913));
#68640=CARTESIAN_POINT('Ctrl Pts',(-7.83069978419073,-1.12430506975433,
-5.5965944301635));
#68641=CARTESIAN_POINT('Ctrl Pts',(-7.80371389730901,-1.31225973105197,
-5.58897939583327));
#68642=CARTESIAN_POINT('Ctrl Pts',(-7.76993429822317,-1.49939826089422,
-5.58136436150303));
#68643=CARTESIAN_POINT('Ctrl Pts',(-7.72943137028393,-1.68517408360999,
-5.5737493271728));
#68644=CARTESIAN_POINT('Ctrl Pts',(-7.68765724127902,-1.87678055699289,
-5.56589529185552));
#68645=CARTESIAN_POINT('Ctrl Pts',(-7.63873089817577,-2.06693698902139,
-5.55804125653824));
#68646=CARTESIAN_POINT('Ctrl Pts',(-7.58278696986399,-2.25505271992938,
-5.55018722122097));
#68647=CARTESIAN_POINT('Ctrl Pts',(-7.52856777780362,-2.43736889348865,
-5.54257532369845));
#68648=CARTESIAN_POINT('Ctrl Pts',(-7.46775740041643,-2.61776795328872,
-5.53496342617593));
#68649=CARTESIAN_POINT('Ctrl Pts',(-7.40052952258955,-2.79572598537134,
-5.52735152865341));
#68650=CARTESIAN_POINT('Ctrl Pts',(-7.33329737157989,-2.97369532893992,
-5.51973914729843));
#68651=CARTESIAN_POINT('Ctrl Pts',(-7.25964703846863,-3.14922299010687,
-5.51212676594345));
#68652=CARTESIAN_POINT('Ctrl Pts',(-7.17980084906094,-3.32180384246629,
-5.50451438458848));
#68653=CARTESIAN_POINT('Ctrl Pts',(-7.09993430708423,-3.49442868519939,
-5.49690006285891));
#68654=CARTESIAN_POINT('Ctrl Pts',(-7.0138689212237,-3.66410488922804,-5.48928574112935));
#68655=CARTESIAN_POINT('Ctrl Pts',(-6.92187352593928,-3.83035088352241,
-5.48167141939978));
#68656=CARTESIAN_POINT('Ctrl Pts',(-6.82983705938048,-3.99667109821472,
-5.47405369826206));
#68657=CARTESIAN_POINT('Ctrl Pts',(-6.73186549383551,-4.15955773322744,
-5.46643597712434));
#68658=CARTESIAN_POINT('Ctrl Pts',(-6.62827156178449,-4.31855729419432,
-5.45881825598662));
#68659=CARTESIAN_POINT('Ctrl Pts',(-6.52455768577843,-4.4777409493047,-5.45119171483808));
#68660=CARTESIAN_POINT('Ctrl Pts',(-6.41520865221714,-4.63302823903928,
-5.44356517368953));
#68661=CARTESIAN_POINT('Ctrl Pts',(-6.30057859266597,-4.78399732416724,
-5.43593863254099));
#68662=CARTESIAN_POINT('Ctrl Pts',(-6.1858692800476,-4.93507078648121,-5.42830681854534));
#68663=CARTESIAN_POINT('Ctrl Pts',(-6.0658719063937,-5.08181981811388,-5.42067500454968));
#68664=CARTESIAN_POINT('Ctrl Pts',(-5.94097787625705,-5.22385900210029,
-5.41304319055403));
#68665=CARTESIAN_POINT('Ctrl Pts',(-5.81591352806535,-5.36609188499714,
-5.40540096904959));
#68666=CARTESIAN_POINT('Ctrl Pts',(-5.68593945274347,-5.5036018409918,-5.39775874754515));
#68667=CARTESIAN_POINT('Ctrl Pts',(-5.55148105358028,-5.6360428592887,-5.39011652604071));
#68668=CARTESIAN_POINT('Ctrl Pts',(-5.52295479747683,-5.66414111443715,
-5.38849517721318));
#68669=CARTESIAN_POINT('Ctrl Pts',(-5.49422680642355,-5.69201136762667,
-5.38687382838564));
#68670=CARTESIAN_POINT('Ctrl Pts',(-5.46530130986985,-5.71965056557959,
-5.38525247955811));
#68671=CARTESIAN_POINT('Ctrl Pts',(-5.32231618543271,-5.85627723165268,
-5.3772377938489));
#68672=CARTESIAN_POINT('Ctrl Pts',(-5.17402891933669,-5.98770713879432,
-5.3692231081397));
#68673=CARTESIAN_POINT('Ctrl Pts',(-5.02084751991195,-6.1135105448338,-5.36120842243049));
#68674=CARTESIAN_POINT('Ctrl Pts',(-4.8678402673753,-6.23917092912419,-5.35320284835351));
#68675=CARTESIAN_POINT('Ctrl Pts',(-4.70995022464793,-6.35921734775696,
-5.34519727427653));
#68676=CARTESIAN_POINT('Ctrl Pts',(-4.547622168603,-6.4732568009952,-5.33719170019955));
#68677=CARTESIAN_POINT('Ctrl Pts',(-4.38545113121013,-6.58718594476712,
-5.32919386985141));
#68678=CARTESIAN_POINT('Ctrl Pts',(-4.21885090741432,-6.6951195114049,-5.32119603950328));
#68679=CARTESIAN_POINT('Ctrl Pts',(-4.04829959295944,-6.79670445183874,
-5.31319820915514));
#68680=CARTESIAN_POINT('Ctrl Pts',(-3.87788434894009,-6.89820834506907,
-5.30520675969163));
#68681=CARTESIAN_POINT('Ctrl Pts',(-3.7035245830723,-6.99337353676238,-5.29721531022811));
#68682=CARTESIAN_POINT('Ctrl Pts',(-3.52572797934315,-7.0818898053893,-5.28922386076459));
#68683=CARTESIAN_POINT('Ctrl Pts',(-3.34804311232999,-7.17035044574795,
-5.28123743354728));
#68684=CARTESIAN_POINT('Ctrl Pts',(-3.16692601136339,-7.25217034356515,
-5.27325100632998));
#68685=CARTESIAN_POINT('Ctrl Pts',(-2.98290996906238,-7.32708462599336,
-5.26526457911267));
#68686=CARTESIAN_POINT('Ctrl Pts',(-2.79326282844557,-7.40429136990665,
-5.25703375822027));
#68687=CARTESIAN_POINT('Ctrl Pts',(-2.60053682217364,-7.47416296818509,
-5.24880293732788));
#68688=CARTESIAN_POINT('Ctrl Pts',(-2.40534032221803,-7.53646196396638,
-5.24057211643549));
#68689=CARTESIAN_POINT('Ctrl Pts',(-2.21606704092048,-7.59687050282723,
-5.23259105899629));
#68690=CARTESIAN_POINT('Ctrl Pts',(-2.02447134576737,-7.65015918501625,
-5.22461000155709));
#68691=CARTESIAN_POINT('Ctrl Pts',(-1.83112558464695,-7.69616138690265,
-5.2166289441179));
#68692=CARTESIAN_POINT('Ctrl Pts',(-1.63779493336743,-7.74215999374799,
-5.20864851039296));
#68693=CARTESIAN_POINT('Ctrl Pts',(-1.44271481404433,-7.78087317774757,
-5.20066807666802));
#68694=CARTESIAN_POINT('Ctrl Pts',(-1.24647002645959,-7.81218493592784,
-5.19268764294308));
#68695=CARTESIAN_POINT('Ctrl Pts',(-1.05021044938547,-7.84349905383914,
-5.18470660779305));
#68696=CARTESIAN_POINT('Ctrl Pts',(-0.852786359456356,-7.86741058177904,
-5.17672557264302));
#68697=CARTESIAN_POINT('Ctrl Pts',(-0.654790358630198,-7.88385505867814,
-5.16874453749299));
#68698=CARTESIAN_POINT('Ctrl Pts',(-0.456749041158314,-7.90030329933273,
-5.160761675671));
#68699=CARTESIAN_POINT('Ctrl Pts',(-0.258135885144651,-7.90928105529107,
-5.15277881384901));
#68700=CARTESIAN_POINT('Ctrl Pts',(-0.0595465796660957,-7.91077589145654,
-5.14479595202703));
#68701=CARTESIAN_POINT('Ctrl Pts',(0.139190089805901,-7.91227183687121,
-5.13680716649029));
#68702=CARTESIAN_POINT('Ctrl Pts',(0.337902538740874,-7.90627376810992,
-5.12881838095356));
#68703=CARTESIAN_POINT('Ctrl Pts',(0.535996089866923,-7.89282137081838,
-5.12082959541682));
#68704=CARTESIAN_POINT('Ctrl Pts',(0.73417700485295,-7.87936304070699,-5.11283728664));
#68705=CARTESIAN_POINT('Ctrl Pts',(0.931738145131561,-7.8584438580623,-5.10484497786318));
#68706=CARTESIAN_POINT('Ctrl Pts',(1.12809138442311,-7.83015522377369,-5.09685266908636));
#68707=CARTESIAN_POINT('Ctrl Pts',(1.32462835100054,-7.80184011987339,-5.08885288192413));
#68708=CARTESIAN_POINT('Ctrl Pts',(1.51995483020641,-7.76614184924864,-5.0808530947619));
#68709=CARTESIAN_POINT('Ctrl Pts',(1.71349332094594,-7.7232028096557,-5.07285330759967));
#68710=CARTESIAN_POINT('Ctrl Pts',(1.75485061222708,-7.7140271549268,-5.07114383096486));
#68711=CARTESIAN_POINT('Ctrl Pts',(1.7961263123398,-7.70452104243178,-5.06943435433005));
#68712=CARTESIAN_POINT('Ctrl Pts',(1.83731488053543,-7.69468615537782,-5.06772487769524));
#68713=CARTESIAN_POINT('Ctrl Pts',(2.03313803202395,-7.64792807026323,-5.0595974987479));
#68714=CARTESIAN_POINT('Ctrl Pts',(2.22733455925563,-7.59365244057301,-5.05147011980056));
#68715=CARTESIAN_POINT('Ctrl Pts',(2.41930691256971,-7.53199011303071,-5.04334274085322));
#68716=CARTESIAN_POINT('Ctrl Pts',(2.61111623215242,-7.47038015260884,-5.03522226413369));
#68717=CARTESIAN_POINT('Ctrl Pts',(2.8007048415114,-7.4013960978811,-5.02710178741417));
#68718=CARTESIAN_POINT('Ctrl Pts',(2.98748786274063,-7.32521926429356,-5.01898131069464));
#68719=CARTESIAN_POINT('Ctrl Pts',(3.17413574179092,-7.24909754654689,-5.01086670934275));
#68720=CARTESIAN_POINT('Ctrl Pts',(3.35798178591649,-7.16579354636245,-5.00275210799086));
#68721=CARTESIAN_POINT('Ctrl Pts',(3.53845815631536,-7.07553777998572,-4.99463750663897));
#68722=CARTESIAN_POINT('Ctrl Pts',(3.71880667200424,-6.98534595341901,-4.98652865390669));
#68723=CARTESIAN_POINT('Ctrl Pts',(3.89578999206551,-6.88821232810952,-4.97841980117441));
#68724=CARTESIAN_POINT('Ctrl Pts',(4.06886173436035,-6.78441487430258,-4.97031094844213));
#68725=CARTESIAN_POINT('Ctrl Pts',(4.2418593552487,-6.68066187381404,-4.96220556848688));
#68726=CARTESIAN_POINT('Ctrl Pts',(4.41094846573746,-6.5702508989291,-4.95410018853162));
#68727=CARTESIAN_POINT('Ctrl Pts',(4.57560795403869,-6.4535054699704,-4.94599480857636));
#68728=CARTESIAN_POINT('Ctrl Pts',(4.74021609673627,-6.33679644562211,-4.93789195611363));
#68729=CARTESIAN_POINT('Ctrl Pts',(4.90039711233585,-6.213757090812,-4.9297891036509));
#68730=CARTESIAN_POINT('Ctrl Pts',(5.05565905699076,-6.08475410345129,-4.92168625118817));
#68731=CARTESIAN_POINT('Ctrl Pts',(5.13693641523488,-6.01722292546957,-4.91744452637997));
#68732=CARTESIAN_POINT('Ctrl Pts',(5.21686626674374,-5.9480581972277,-4.91320280157177));
#68733=CARTESIAN_POINT('Ctrl Pts',(5.29538154110007,-5.87731701834916,-4.90896107676356));
#68734=CARTESIAN_POINT('Ctrl Pts',(5.44881114414081,-5.73907906295835,-4.90067216535281));
#68735=CARTESIAN_POINT('Ctrl Pts',(5.59677101776082,-5.59487825941542,-4.89238325394205));
#68736=CARTESIAN_POINT('Ctrl Pts',(5.73881466834484,-5.44517467143067,-4.8840943425313));
#68737=CARTESIAN_POINT('Ctrl Pts',(5.8809399866588,-5.29538501164937,-4.8758006654265));
#68738=CARTESIAN_POINT('Ctrl Pts',(6.01714209097839,-5.1400864644989,-4.86750698832171));
#68739=CARTESIAN_POINT('Ctrl Pts',(6.14701355777908,-4.97977362140893,-4.85921331121692));
#68740=CARTESIAN_POINT('Ctrl Pts',(6.2769675161996,-4.81935895097819,-4.85091436614314));
#68741=CARTESIAN_POINT('Ctrl Pts',(6.40058262654685,-4.65392385420555,-4.84261542106937));
#68742=CARTESIAN_POINT('Ctrl Pts',(6.51749321069374,-4.48399411781071,-4.83431647599559));
#68743=CARTESIAN_POINT('Ctrl Pts',(6.63453943639035,-4.31386722618859,-4.82600790235158));
#68744=CARTESIAN_POINT('Ctrl Pts',(6.74486542128345,-4.13923551257753,-4.81769932870756));
#68745=CARTESIAN_POINT('Ctrl Pts',(6.84814918525661,-3.9606531956824,-4.80939075506355));
#68746=CARTESIAN_POINT('Ctrl Pts',(6.95149651702649,-3.78196096718084,-4.80107706776275));
#68747=CARTESIAN_POINT('Ctrl Pts',(7.04779283552652,-3.59931353819006,-4.79276338046196));
#68748=CARTESIAN_POINT('Ctrl Pts',(7.13676258446991,-3.41328885576806,-4.78444969316117));
#68749=CARTESIAN_POINT('Ctrl Pts',(7.22582916410519,-3.22706171240935,-4.77612695761529));
#68750=CARTESIAN_POINT('Ctrl Pts',(7.30755311650373,-3.0374502357919,-4.76780422206941));
#68751=CARTESIAN_POINT('Ctrl Pts',(7.38170676735722,-2.84505293461346,-4.75948148652353));
#68752=CARTESIAN_POINT('Ctrl Pts',(7.4092801581117,-2.77351166989566,-4.7563867496264));
#68753=CARTESIAN_POINT('Ctrl Pts',(7.43580732530892,-2.7015853846223,-4.75329201272928));
#68754=CARTESIAN_POINT('Ctrl Pts',(7.46127832057214,-2.62930538792285,-4.75019727583216));
#68755=CARTESIAN_POINT('Ctrl Pts',(7.5328596305709,-2.42617642507772,-4.74150011583082));
#68756=CARTESIAN_POINT('Ctrl Pts',(7.59615934173458,-2.22007295003041,-4.73280295582949));
#68757=CARTESIAN_POINT('Ctrl Pts',(7.65095765935272,-2.01165799647753,-4.72410579582815));
#68758=CARTESIAN_POINT('Ctrl Pts',(7.70570798432838,-1.80342557379033,-4.71541625284334));
#68759=CARTESIAN_POINT('Ctrl Pts',(7.7519717245781,-1.59288593608751,-4.70672670985852));
#68760=CARTESIAN_POINT('Ctrl Pts',(7.7895791404599,-1.38071641350137,-4.69803716687371));
#68761=CARTESIAN_POINT('Ctrl Pts',(7.82802659185421,-1.16380766782672,-4.68915352587594));
#68762=CARTESIAN_POINT('Ctrl Pts',(7.85742641042037,-0.945195597718181,
-4.68026988487818));
#68763=CARTESIAN_POINT('Ctrl Pts',(7.87765192902944,-0.725617726532843,
-4.67138624388042));
#68764=CARTESIAN_POINT('Ctrl Pts',(7.89737753215061,-0.511467176185646,
-4.66272218042772));
#68765=CARTESIAN_POINT('Ctrl Pts',(7.90837690929062,-0.296398248404238,
-4.65405811697503));
#68766=CARTESIAN_POINT('Ctrl Pts',(7.91058424242814,-0.0811045217454267,
-4.64539405352233));
#68767=CARTESIAN_POINT('Ctrl Pts',(7.91287548783053,0.142373644274772,-4.63640062375203));
#68768=CARTESIAN_POINT('Ctrl Pts',(7.90569310299304,0.366093807003429,-4.62740719398174));
#68769=CARTESIAN_POINT('Ctrl Pts',(7.88902260448897,0.589273574719011,-4.61841376421144));
#68770=CARTESIAN_POINT('Ctrl Pts',(7.87235210598489,0.812453342434667,-4.60942033444114));
#68771=CARTESIAN_POINT('Ctrl Pts',(7.84619344843791,1.03509243444895,-4.60042690467084));
#68772=CARTESIAN_POINT('Ctrl Pts',(7.81059316005786,1.25640578160776,-4.59143347490053));
#68773=CARTESIAN_POINT('Ctrl Pts',(7.77966925806201,1.44864782708929,-4.5836214050135));
#68774=CARTESIAN_POINT('Ctrl Pts',(7.74163406916984,1.6398066683164,-4.57580933512647));
#68775=CARTESIAN_POINT('Ctrl Pts',(7.69659149203198,1.82931692300185,-4.56799726523944));
#68776=CARTESIAN_POINT('Ctrl Pts',(7.6515521271619,2.01881366252621,-4.56018575247995));
#68777=CARTESIAN_POINT('Ctrl Pts',(7.59950645090055,2.20666170722864,-4.55237423972046));
#68778=CARTESIAN_POINT('Ctrl Pts',(7.54060916867453,2.39230733086315,-4.54456272696097));
#68779=CARTESIAN_POINT('Ctrl Pts',(7.48170570077726,2.57797245187945,-4.53675039379945));
#68780=CARTESIAN_POINT('Ctrl Pts',(7.41594930084795,2.76143435579824,-4.52893806063793));
#68781=CARTESIAN_POINT('Ctrl Pts',(7.34354413609901,2.94215576086071,-4.5211257274764));
#68782=CARTESIAN_POINT('Ctrl Pts',(7.27108767631271,3.12300519700019,-4.51330785971079));
#68783=CARTESIAN_POINT('Ctrl Pts',(7.19197317234486,3.30110992830876,-4.50548999194517));
#68784=CARTESIAN_POINT('Ctrl Pts',(7.10645277805662,3.47595309422486,-4.49767212417955));
#68785=CARTESIAN_POINT('Ctrl Pts',(7.02090073759362,3.65086095953145,-4.48985136347112));
#68786=CARTESIAN_POINT('Ctrl Pts',(6.92893824656883,3.82250454277251,-4.4820306027627));
#68787=CARTESIAN_POINT('Ctrl Pts',(6.83086285658323,3.99039266671234,-4.47420984205427));
#68788=CARTESIAN_POINT('Ctrl Pts',(6.73267882912726,4.15846675923299,-4.46638041834017));
#68789=CARTESIAN_POINT('Ctrl Pts',(6.62836856151648,4.32277678325011,-4.45855099462607));
#68790=CARTESIAN_POINT('Ctrl Pts',(6.51827288047181,4.48286065539693,-4.45072157091198));
#68791=CARTESIAN_POINT('Ctrl Pts',(6.43365890969315,4.60589302098509,-4.44470427193101));
#68792=CARTESIAN_POINT('Ctrl Pts',(6.34562856635552,4.72642972358259,-4.43868697295005));
#68793=CARTESIAN_POINT('Ctrl Pts',(6.25435226710092,4.84427483933453,-4.43266967396909));
#68794=CARTESIAN_POINT('Ctrl Pts',(6.13121858566079,5.00325042292825,-4.42455220884504));
#68795=CARTESIAN_POINT('Ctrl Pts',(6.00193263824056,5.15764151385946,-4.41643474372099));
#68796=CARTESIAN_POINT('Ctrl Pts',(5.86686277145616,5.30696167509261,-4.40831727859694));
#68797=CARTESIAN_POINT('Ctrl Pts',(5.73189146923524,5.45617287289179,-4.40020573703249));
#68798=CARTESIAN_POINT('Ctrl Pts',(5.59114487751525,5.60032028221937,-4.39209419546804));
#68799=CARTESIAN_POINT('Ctrl Pts',(5.44503177828627,5.73895024664377,-4.3839826539036));
#68800=CARTESIAN_POINT('Ctrl Pts',(5.29900454986435,5.87749873810655,-4.37587587949982));
#68801=CARTESIAN_POINT('Ctrl Pts',(5.14761733501422,6.0105360304936,-4.36776910509605));
#68802=CARTESIAN_POINT('Ctrl Pts',(4.99131635487761,6.13764466595544,-4.35966233069228));
#68803=CARTESIAN_POINT('Ctrl Pts',(4.83508505740861,6.26469663338624,-4.35155917047996));
#68804=CARTESIAN_POINT('Ctrl Pts',(4.67394461178193,6.3858250130613,-4.34345601026764));
#68805=CARTESIAN_POINT('Ctrl Pts',(4.50837539117766,6.50065168519462,-4.33535285005532));
#68806=CARTESIAN_POINT('Ctrl Pts',(4.3428565141186,6.61544344273609,-4.32725215371769));
#68807=CARTESIAN_POINT('Ctrl Pts',(4.17291181116822,6.72393713197965,-4.31915145738006));
#68808=CARTESIAN_POINT('Ctrl Pts',(3.99905225549968,6.82579680753705,-4.31105076104244));
#68809=CARTESIAN_POINT('Ctrl Pts',(3.82385848104658,6.92843816628692,-4.30288789900342));
#68810=CARTESIAN_POINT('Ctrl Pts',(3.64468978221517,7.02434306920593,-4.2947250369644));
#68811=CARTESIAN_POINT('Ctrl Pts',(3.46209678621075,7.11321353840226,-4.28656217492539));
#68812=CARTESIAN_POINT('Ctrl Pts',(3.2808950792492,7.20140684849209,-4.27846151078422));
#68813=CARTESIAN_POINT('Ctrl Pts',(3.09632138097202,7.28267243392682,-4.27036084664305));
#68814=CARTESIAN_POINT('Ctrl Pts',(2.90893675580733,7.35676613402337,-4.26226018250188));
#68815=CARTESIAN_POINT('Ctrl Pts',(2.72152683755482,7.43086983525241,-4.25415842493691));
#68816=CARTESIAN_POINT('Ctrl Pts',(2.53130553399829,7.49779960256221,-4.24605666737194));
#68817=CARTESIAN_POINT('Ctrl Pts',(2.33885255485682,7.55735997069345,-4.23795490980697));
#68818=CARTESIAN_POINT('Ctrl Pts',(2.1463487693696,7.6169360623779,-4.22985101343024));
#68819=CARTESIAN_POINT('Ctrl Pts',(1.95161243970321,7.66913878029209,-4.2217471170535));
#68820=CARTESIAN_POINT('Ctrl Pts',(1.75523758018288,7.71382279010309,-4.21364322067677));
#68821=CARTESIAN_POINT('Ctrl Pts',(1.55632966895585,7.75908318177676,-4.20543479162921));
#68822=CARTESIAN_POINT('Ctrl Pts',(1.35574099512005,7.79662948006481,-4.19722636258165));
#68823=CARTESIAN_POINT('Ctrl Pts',(1.15409839849683,7.82636428276802,-4.1890179335341));
#68824=CARTESIAN_POINT('Ctrl Pts',(0.954765254507595,7.85575852688107,-4.18090351725171));
#68825=CARTESIAN_POINT('Ctrl Pts',(0.754402526398841,7.87751926678977,-4.17278910096933));
#68826=CARTESIAN_POINT('Ctrl Pts',(0.553620133605896,7.8916047637769,-4.16467468468694));
#68827=CARTESIAN_POINT('Ctrl Pts',(0.349348375597913,7.90593505037201,-4.1564192492568));
#68828=CARTESIAN_POINT('Ctrl Pts',(0.14464258160877,7.91232085992563,-4.14816381382666));
#68829=CARTESIAN_POINT('Ctrl Pts',(-0.0598555178725263,7.91077355996114,
-4.13990837839652));
#68830=CARTESIAN_POINT('Ctrl Pts',(-0.264353617353823,7.90922625999665,
-4.13165294296637));
#68831=CARTESIAN_POINT('Ctrl Pts',(-0.468643677552347,7.89974590077665,
-4.12339750753623));
#68832=CARTESIAN_POINT('Ctrl Pts',(-0.672089699269375,7.88239915483452,
-4.11514207210609));
#68833=CARTESIAN_POINT('Ctrl Pts',(-0.867397018831502,7.86574635216732,
-4.10721688904244));
#68834=CARTESIAN_POINT('Ctrl Pts',(-1.06234433425082,7.84180827115674,-4.09929170597879));
#68835=CARTESIAN_POINT('Ctrl Pts',(-1.2563485546642,7.81060236532325,-4.09136652291514));
#68836=CARTESIAN_POINT('Ctrl Pts',(-1.45014548666337,7.77942980218056,-4.08344980770145));
#68837=CARTESIAN_POINT('Ctrl Pts',(-1.64300099591074,7.7410049351129,-4.07553309248775));
#68838=CARTESIAN_POINT('Ctrl Pts',(-1.83433475217939,7.69539713185401,-4.06761637727406));
#68839=CARTESIAN_POINT('Ctrl Pts',(-2.02549560883702,7.64983054229206,-4.05970681603574));
#68840=CARTESIAN_POINT('Ctrl Pts',(-2.2151371210944,7.59709402576676,-4.05179725479742));
#68841=CARTESIAN_POINT('Ctrl Pts',(-2.40268653944171,7.53730843160777,-4.04388769355911));
#68842=CARTESIAN_POINT('Ctrl Pts',(-2.59007104747301,7.47757540632003,-4.03598508711838));
#68843=CARTESIAN_POINT('Ctrl Pts',(-2.77536680423015,7.410805763498,-4.02808248067766));
#68844=CARTESIAN_POINT('Ctrl Pts',(-2.95801363401451,7.33717086764267,-4.02017987423693));
#68845=CARTESIAN_POINT('Ctrl Pts',(-3.14056670573212,7.26357377077617,-4.01228132443986));
#68846=CARTESIAN_POINT('Ctrl Pts',(-3.3204732427651,7.18311856880906,-4.00438277464278));
#68847=CARTESIAN_POINT('Ctrl Pts',(-3.49718995100456,7.09602589105992,-3.9964842248457));
#68848=CARTESIAN_POINT('Ctrl Pts',(-3.67384672762452,7.00896274987965,-3.98858835375901));
#68849=CARTESIAN_POINT('Ctrl Pts',(-3.84731552410981,6.91526676854941,-3.98069248267231));
#68850=CARTESIAN_POINT('Ctrl Pts',(-4.01707442205947,6.81520609282181,-3.97279661158562));
#68851=CARTESIAN_POINT('Ctrl Pts',(-4.13473757975116,6.74585211368392,-3.96732383144857));
#68852=CARTESIAN_POINT('Ctrl Pts',(-4.25061888189729,6.67344144305843,-3.96185105131151));
#68853=CARTESIAN_POINT('Ctrl Pts',(-4.36455159383011,6.59807626394202,-3.95637827117446));
#68854=CARTESIAN_POINT('Ctrl Pts',(-4.54191027503512,6.48075553532855,-3.9478588121783));
#68855=CARTESIAN_POINT('Ctrl Pts',(-4.71436916099292,6.35639049379292,-3.93933935318213));
#68856=CARTESIAN_POINT('Ctrl Pts',(-4.88140582515869,6.22541550180442,-3.93081989418597));
#68857=CARTESIAN_POINT('Ctrl Pts',(-5.04874330922775,6.09420463414983,-3.92228509231378));
#68858=CARTESIAN_POINT('Ctrl Pts',(-5.21063885873806,5.95636017846069,-3.91375029044158));
#68859=CARTESIAN_POINT('Ctrl Pts',(-5.36660498450393,5.81235511133805,-3.90521548856939));
#68860=CARTESIAN_POINT('Ctrl Pts',(-5.53046461678876,5.66106189154434,-3.89624873704219));
#68861=CARTESIAN_POINT('Ctrl Pts',(-5.68777890979256,5.5029686325903,-3.88728198551499));
#68862=CARTESIAN_POINT('Ctrl Pts',(-5.83803014074007,5.3386632292935,-3.8783152339878));
#68863=CARTESIAN_POINT('Ctrl Pts',(-5.98164066247767,5.1816196926585,-3.86974478929332));
#68864=CARTESIAN_POINT('Ctrl Pts',(-6.11879886542661,5.01890147419976,-3.86117434459885));
#68865=CARTESIAN_POINT('Ctrl Pts',(-6.24909640662006,4.85105298886419,-3.85260389990438));
#68866=CARTESIAN_POINT('Ctrl Pts',(-6.37955677188634,4.68299475456675,-3.84402274530166));
#68867=CARTESIAN_POINT('Ctrl Pts',(-6.50313919921718,4.50979364545006,-3.83544159069893));
#68868=CARTESIAN_POINT('Ctrl Pts',(-6.61947852636648,4.33202320388211,-3.82686043609621));
#68869=CARTESIAN_POINT('Ctrl Pts',(-6.73601142072992,4.15395698503941,-3.81826500403262));
#68870=CARTESIAN_POINT('Ctrl Pts',(-6.84527698538273,3.97130644314049,-3.80966957196904));
#68871=CARTESIAN_POINT('Ctrl Pts',(-6.94695476963092,3.78467177291536,-3.80107413990545));
#68872=CARTESIAN_POINT('Ctrl Pts',(-6.96059657157506,3.75963156156588,-3.79992091668463));
#68873=CARTESIAN_POINT('Ctrl Pts',(-6.97410185734856,3.73451966479241,-3.79876769346382));
#68874=CARTESIAN_POINT('Ctrl Pts',(-6.98746991817483,3.70933756115587,-3.79761447024301));
#68875=CARTESIAN_POINT('Ctrl Pts',(-7.0819253421148,3.53140702167073,-3.78946607911621));
#68876=CARTESIAN_POINT('Ctrl Pts',(-7.16969060289945,3.34965952500846,-3.78131768798942));
#68877=CARTESIAN_POINT('Ctrl Pts',(-7.25045397823132,3.1646229016345,-3.77316929686262));
#68878=CARTESIAN_POINT('Ctrl Pts',(-7.33111179945917,2.97982811281627,-3.76503155531704));
#68879=CARTESIAN_POINT('Ctrl Pts',(-7.40478585117344,2.79175305277301,-3.75689381377146));
#68880=CARTESIAN_POINT('Ctrl Pts',(-7.47120977818801,2.60095087425884,-3.74875607222588));
#68881=CARTESIAN_POINT('Ctrl Pts',(-7.53755487966607,2.41037512144344,-3.74062798777033));
#68882=CARTESIAN_POINT('Ctrl Pts',(-7.59666690492667,2.21707899775969,-3.73249990331478));
#68883=CARTESIAN_POINT('Ctrl Pts',(-7.64832693960925,2.0216369666306,-3.72437181885923));
#68884=CARTESIAN_POINT('Ctrl Pts',(-7.69991418798707,1.82647030316878,-3.71625518645236));
#68885=CARTESIAN_POINT('Ctrl Pts',(-7.74407031092905,1.62916406731576,-3.7081385540455));
#68886=CARTESIAN_POINT('Ctrl Pts',(-7.78062571210136,1.43030924215263,-3.70002192163863));
#68887=CARTESIAN_POINT('Ctrl Pts',(-7.81715060628764,1.23162036952125,-3.6919120628954));
#68888=CARTESIAN_POINT('Ctrl Pts',(-7.84608736488076,1.03138579234293,-3.68380220415217));
#68889=CARTESIAN_POINT('Ctrl Pts',(-7.86731677212391,0.830209495885109,
-3.67569234540894));
#68890=CARTESIAN_POINT('Ctrl Pts',(-7.8885265146157,0.629219548570451,-3.6675899988093));
#68891=CARTESIAN_POINT('Ctrl Pts',(-7.90204311351956,0.42728993474177,-3.65948765220967));
#68892=CARTESIAN_POINT('Ctrl Pts',(-7.90779875925917,0.225032848844619,
-3.65138530561004));
#68893=CARTESIAN_POINT('Ctrl Pts',(-7.90994260115476,0.149696868479849,
-3.6483673731523));
#68894=CARTESIAN_POINT('Ctrl Pts',(-7.91101021264565,0.0743155299380854,
-3.64534944069455));
#68895=CARTESIAN_POINT('Ctrl Pts',(-7.91099992637351,-0.00107931383712131,
-3.6423315082368));
#68896=CARTESIAN_POINT('',(-7.91472706974257,-0.00545317307574832,-1.6423315082368));
#68897=CARTESIAN_POINT('Ctrl Pts',(-7.89505561641365,-0.00110003754996664,
-3.64233058977502));
#68898=CARTESIAN_POINT('Ctrl Pts',(-7.89694082944445,-1.34945014943438,
-3.58824934930999));
#68899=CARTESIAN_POINT('Ctrl Pts',(-6.93814504690791,-5.33560757785971,
-3.4283255748907));
#68900=CARTESIAN_POINT('Ctrl Pts',(-0.577026428184519,-9.3360978864592,
-3.16255926651691));
#68901=CARTESIAN_POINT('Ctrl Pts',(6.14476370108003,-6.1845707103362,-2.89795293163112));
#68902=CARTESIAN_POINT('Ctrl Pts',(8.15718009137018,-1.12820106384972,-2.6862678637223));
#68903=CARTESIAN_POINT('Ctrl Pts',(7.72063400436892,2.91454907120771,-2.52750406279097));
#68904=CARTESIAN_POINT('Ctrl Pts',(5.38307865781836,6.23175735845454,-2.36874026185935));
#68905=CARTESIAN_POINT('Ctrl Pts',(0.520138418637635,8.70745165738554,-2.15705519395057));
#68906=CARTESIAN_POINT('Ctrl Pts',(-5.15916039566107,7.03642133255631,-1.94537012604193));
#68907=CARTESIAN_POINT('Ctrl Pts',(-7.60147874380101,2.82410070209666,-1.75615514181166));
#68908=CARTESIAN_POINT('Ctrl Pts',(-7.910699221098,0.750269626436475,-1.67278269153563));
#68909=CARTESIAN_POINT('Ctrl Pts',(-7.91472706974257,-0.00545317307574832,
-1.6423315082368));
#68910=CARTESIAN_POINT('',(-7.91099847812363,0.00490704857253402,2.35986635990733));
#68911=CARTESIAN_POINT('Ctrl Pts',(-7.91099806737629,-0.00552973494411184,
-1.64448048805235));
#68912=CARTESIAN_POINT('Ctrl Pts',(-7.91070797338719,-0.420546550464831,
-1.62919126859007));
#68913=CARTESIAN_POINT('Ctrl Pts',(-7.87776006516516,-0.834880730787549,
-1.61380261985671));
#68914=CARTESIAN_POINT('Ctrl Pts',(-7.80961822115242,-1.2625816384502,-1.59654814058759));
#68915=CARTESIAN_POINT('Ctrl Pts',(-7.80670663640616,-1.28046110466453,
-1.59582426432029));
#68916=CARTESIAN_POINT('Ctrl Pts',(-7.80204018361664,-1.30850924782867,
-1.59468447533826));
#68917=CARTESIAN_POINT('Ctrl Pts',(-7.80032677684725,-1.31868481889568,
-1.59427009920818));
#68918=CARTESIAN_POINT('Ctrl Pts',(-7.79740034165437,-1.33585903610092,
-1.5935692111369));
#68919=CARTESIAN_POINT('Ctrl Pts',(-7.79619778471698,-1.34285946901606,
-1.59328309657582));
#68920=CARTESIAN_POINT('Ctrl Pts',(-7.79380471228816,-1.35667867224916,
-1.59271744246618));
#68921=CARTESIAN_POINT('Ctrl Pts',(-7.79261467211045,-1.36349751911817,
-1.59243792144563));
#68922=CARTESIAN_POINT('Ctrl Pts',(-7.79030506680006,-1.3766296076633,-1.59189880576414));
#68923=CARTESIAN_POINT('Ctrl Pts',(-7.78918677252919,-1.3829430692723,-1.59163926102022));
#68924=CARTESIAN_POINT('Ctrl Pts',(-7.78660690665526,-1.39740560501684,
-1.59104388216801));
#68925=CARTESIAN_POINT('Ctrl Pts',(-7.78514021703942,-1.40555374996859,
-1.59070784516098));
#68926=CARTESIAN_POINT('Ctrl Pts',(-7.78048208510383,-1.43120086749349,
-1.58964820311452));
#68927=CARTESIAN_POINT('Ctrl Pts',(-7.77724442717166,-1.44869131035915,
-1.58892273179252));
#68928=CARTESIAN_POINT('Ctrl Pts',(-7.74609651000221,-1.61384418216726,
-1.58204471188636));
#68929=CARTESIAN_POINT('Ctrl Pts',(-7.71404796349201,-1.76067087773591,
-1.57570264336101));
#68930=CARTESIAN_POINT('Ctrl Pts',(-7.63594176891085,-2.07521958455449,
-1.56164255867906));
#68931=CARTESIAN_POINT('Ctrl Pts',(-7.58849780377845,-2.24250734859104,
-1.55388807113807));
#68932=CARTESIAN_POINT('Ctrl Pts',(-7.51907591770018,-2.45974785423633,
-1.5435666628016));
#68933=CARTESIAN_POINT('Ctrl Pts',(-7.50203703623545,-2.51123522946648,
-1.54110150352093));
#68934=CARTESIAN_POINT('Ctrl Pts',(-7.45922759913177,-2.63626960696568,
-1.5350746603938));
#68935=CARTESIAN_POINT('Ctrl Pts',(-7.43289712381474,-2.70961879108291,
-1.53150485168172));
#68936=CARTESIAN_POINT('Ctrl Pts',(-7.36532492957683,-2.88945458350693,
-1.52268421783884));
#68937=CARTESIAN_POINT('Ctrl Pts',(-7.32285296860632,-2.99546046890896,
-1.51742517160671));
#68938=CARTESIAN_POINT('Ctrl Pts',(-7.18565287245346,-3.31752243423368,
-1.50132109060421));
#68939=CARTESIAN_POINT('Ctrl Pts',(-7.08354217897075,-3.53029717590608,
-1.49050810119889));
#68940=CARTESIAN_POINT('Ctrl Pts',(-6.82375730326767,-4.01481952908864,
-1.46576483303475));
#68941=CARTESIAN_POINT('Ctrl Pts',(-6.65910084583029,-4.28238753609946,
-1.45201518061746));
#68942=CARTESIAN_POINT('Ctrl Pts',(-6.40511121052275,-4.64489370772051,
-1.4334397463345));
#68943=CARTESIAN_POINT('Ctrl Pts',(-6.32869156950222,-4.7484894754258,-1.42813554445422));
#68944=CARTESIAN_POINT('Ctrl Pts',(-6.23851566709738,-4.86468709911592,
-1.4221897027533));
#68945=CARTESIAN_POINT('Ctrl Pts',(-6.22720521216287,-4.87915705349189,
-1.42144932952035));
#68946=CARTESIAN_POINT('Ctrl Pts',(-6.21006046937387,-4.90093433908402,
-1.42033513199003));
#68947=CARTESIAN_POINT('Ctrl Pts',(-6.20426348639517,-4.90827087898391,
-1.41995978154105));
#68948=CARTESIAN_POINT('Ctrl Pts',(-6.19423953133169,-4.92091085283253,
-1.41931311369865));
#68949=CARTESIAN_POINT('Ctrl Pts',(-6.19001872832958,-4.92621915227707,
-1.4190415430525));
#68950=CARTESIAN_POINT('Ctrl Pts',(-6.18128269008229,-4.93717708926443,
-1.41848094731223));
#68951=CARTESIAN_POINT('Ctrl Pts',(-6.1767665218171,-4.94282597719233,-1.41819196111892));
#68952=CARTESIAN_POINT('Ctrl Pts',(-6.16451846990933,-4.95810301596886,
-1.41741042693284));
#68953=CARTESIAN_POINT('Ctrl Pts',(-6.15677176433111,-4.96771928822333,
-1.41691849344619));
#68954=CARTESIAN_POINT('Ctrl Pts',(-6.12789659537512,-5.00339181478394,
-1.4150936351285));
#68955=CARTESIAN_POINT('Ctrl Pts',(-6.10662483825247,-5.02933190960061,
-1.41376668592546));
#68956=CARTESIAN_POINT('Ctrl Pts',(-5.7593053323447,-5.44742246665148,-1.39237807758397));
#68957=CARTESIAN_POINT('Ctrl Pts',(-5.39624641578874,-5.80728976398713,
-1.37406020294677));
#68958=CARTESIAN_POINT('Ctrl Pts',(-4.78616714225571,-6.30503123750182,
-1.3470565006893));
#68959=CARTESIAN_POINT('Ctrl Pts',(-4.56223689700481,-6.46891112938595,
-1.33778448707811));
#68960=CARTESIAN_POINT('Ctrl Pts',(-4.18709429947162,-6.71426744763681,
-1.32268488738086));
#68961=CARTESIAN_POINT('Ctrl Pts',(-4.04103041071221,-6.80317701910957,
-1.31690201547228));
#68962=CARTESIAN_POINT('Ctrl Pts',(-3.71554657031063,-6.98711737240301,
-1.30400859775547));
#68963=CARTESIAN_POINT('Ctrl Pts',(-3.5351209785516,-7.0801135735892,-1.29685687576797));
#68964=CARTESIAN_POINT('Ctrl Pts',(-3.24350152532638,-7.21649419617759,
-1.28500652317007));
#68965=CARTESIAN_POINT('Ctrl Pts',(-3.13455401997637,-7.26447929812556,
-1.28051699047033));
#68966=CARTESIAN_POINT('Ctrl Pts',(-2.97088926340818,-7.33219700491838,
-1.27362481377852));
#68967=CARTESIAN_POINT('Ctrl Pts',(-2.91696687728015,-7.35381532568079,
-1.27133060401418));
#68968=CARTESIAN_POINT('Ctrl Pts',(-2.85397638257089,-7.37826738823299,
-1.26861829431712));
#68969=CARTESIAN_POINT('Ctrl Pts',(-2.84513403529233,-7.38168159461096,
-1.26823681565075));
#68970=CARTESIAN_POINT('Ctrl Pts',(-2.83166657786943,-7.38685385493783,
-1.2676546512311));
#68971=CARTESIAN_POINT('Ctrl Pts',(-2.82704589172513,-7.38862348535168,
-1.26745470513146));
#68972=CARTESIAN_POINT('Ctrl Pts',(-2.81866367772374,-7.39182469153875,
-1.26709161307753));
#68973=CARTESIAN_POINT('Ctrl Pts',(-2.81490270832095,-7.39325773533749,
-1.26692856168842));
#68974=CARTESIAN_POINT('Ctrl Pts',(-2.80682114642696,-7.39632999578681,
-1.26657789858199));
#68975=CARTESIAN_POINT('Ctrl Pts',(-2.80250020614774,-7.39796829873965,
-1.26639022741055));
#68976=CARTESIAN_POINT('Ctrl Pts',(-2.79078695822923,-7.40239769196704,
-1.26588098484492));
#68977=CARTESIAN_POINT('Ctrl Pts',(-2.78339193380545,-7.40518148178473,
-1.26555894083732));
#68978=CARTESIAN_POINT('Ctrl Pts',(-2.74826033808485,-7.41834639259286,
-1.26402649227058));
#68979=CARTESIAN_POINT('Ctrl Pts',(-2.72047012891964,-7.42858265868971,
-1.26280684972631));
#68980=CARTESIAN_POINT('Ctrl Pts',(-2.25672778700836,-7.59644664179559,
-1.24233987309187));
#68981=CARTESIAN_POINT('Ctrl Pts',(-1.80784301261029,-7.71559775071775,
-1.22089650925874));
#68982=CARTESIAN_POINT('Ctrl Pts',(-1.01023303491929,-7.85385735937933,
-1.18313489092203));
#68983=CARTESIAN_POINT('Ctrl Pts',(-0.665779263598024,-7.8905261214945,
-1.16692665109964));
#68984=CARTESIAN_POINT('Ctrl Pts',(-0.265874501535279,-7.90671667577206,
-1.14874198714563));
#68985=CARTESIAN_POINT('Ctrl Pts',(-0.211704588242726,-7.90835249162374,
-1.14629152393641));
#68986=CARTESIAN_POINT('Ctrl Pts',(0.0427345111569161,-7.91341981469167,
-1.13484649050152));
#68987=CARTESIAN_POINT('Ctrl Pts',(0.243077960183436,-7.90980152367801,
-1.12602635486139));
#68988=CARTESIAN_POINT('Ctrl Pts',(0.551516011399111,-7.89249940201649,
-1.11278980029884));
#68989=CARTESIAN_POINT('Ctrl Pts',(0.659819631715944,-7.8841839210759,-1.10820674227161));
#68990=CARTESIAN_POINT('Ctrl Pts',(0.861927833652346,-7.86447218643965,
-1.09977622040764));
#68991=CARTESIAN_POINT('Ctrl Pts',(0.955765105246779,-7.85362058545232,
-1.0959114028739));
#68992=CARTESIAN_POINT('Ctrl Pts',(1.06569816945589,-7.83890803611238,-1.09143984305065));
#68993=CARTESIAN_POINT('Ctrl Pts',(1.08200157646206,-7.8366743188745,-1.09077814830186));
#68994=CARTESIAN_POINT('Ctrl Pts',(1.10693709615228,-7.83317862470612,-1.08976830765803));
#68995=CARTESIAN_POINT('Ctrl Pts',(1.11557423733556,-7.83195321890104,-1.08941892415491));
#68996=CARTESIAN_POINT('Ctrl Pts',(1.13061734553261,-7.82979356858565,-1.08881111116596));
#68997=CARTESIAN_POINT('Ctrl Pts',(1.13702421691485,-7.82886574409828,-1.08855246451686));
#68998=CARTESIAN_POINT('Ctrl Pts',(1.15140875222206,-7.82676458729031,-1.08797225298186));
#68999=CARTESIAN_POINT('Ctrl Pts',(1.15938578127427,-7.82558691921988,-1.08765083527731));
#69000=CARTESIAN_POINT('Ctrl Pts',(1.18066045417567,-7.82241284414174,-1.08679452407892));
#69001=CARTESIAN_POINT('Ctrl Pts',(1.19395486002662,-7.82039472193802,-1.08626036677019));
#69002=CARTESIAN_POINT('Ctrl Pts',(1.25075060217756,-7.8116247911155,-1.08398236727343));
#69003=CARTESIAN_POINT('Ctrl Pts',(1.29420072453898,-7.80454377367031,-1.08224969002801));
#69004=CARTESIAN_POINT('Ctrl Pts',(1.99390962814729,-7.68450894480091,-1.05450290009283));
#69005=CARTESIAN_POINT('Ctrl Pts',(2.63342372715673,-7.48949290158658,-1.03169454657));
#69006=CARTESIAN_POINT('Ctrl Pts',(3.54804096151581,-7.07874724116073,-0.997603411465685));
#69007=CARTESIAN_POINT('Ctrl Pts',(3.84601734449962,-6.92137177177645,-0.986165012935075));
#69008=CARTESIAN_POINT('Ctrl Pts',(4.26929569995429,-6.66202429730565,-0.968222392935882));
#69009=CARTESIAN_POINT('Ctrl Pts',(4.40297670666163,-6.57443873215262,-0.962284224711357));
#69010=CARTESIAN_POINT('Ctrl Pts',(4.58794933595095,-6.44507493774083,-0.953539397101558));
#69011=CARTESIAN_POINT('Ctrl Pts',(4.64151544608906,-6.40660627398932,-0.950941890698551));
#69012=CARTESIAN_POINT('Ctrl Pts',(4.70255212323347,-6.36160532519652,-0.947898549032821));
#69013=CARTESIAN_POINT('Ctrl Pts',(4.71050024824058,-6.35572231877995,-0.947500593127752));
#69014=CARTESIAN_POINT('Ctrl Pts',(4.72259587095616,-6.34673428482847,-0.946892459561655));
#69015=CARTESIAN_POINT('Ctrl Pts',(4.72675138046194,-6.3436400614821,-0.94668307933651));
#69016=CARTESIAN_POINT('Ctrl Pts',(4.73429367471911,-6.33801248734628,-0.946302233144981));
#69017=CARTESIAN_POINT('Ctrl Pts',(4.73768147649453,-6.33548049601496,-0.946130866319057));
#69018=CARTESIAN_POINT('Ctrl Pts',(4.74446328711433,-6.3304033926888,-0.945787218853356));
#69019=CARTESIAN_POINT('Ctrl Pts',(4.74785728261048,-6.32785826490852,-0.945614937066853));
#69020=CARTESIAN_POINT('Ctrl Pts',(4.75743391836531,-6.32066478660984,-0.945127972008277));
#69021=CARTESIAN_POINT('Ctrl Pts',(4.76361177588735,-6.31601010766409,-0.944812833507664));
#69022=CARTESIAN_POINT('Ctrl Pts',(4.78921689931841,-6.29665910565342,-0.943502576881805));
#69023=CARTESIAN_POINT('Ctrl Pts',(4.80858287796764,-6.28188228816624,-0.942501742115164));
#69024=CARTESIAN_POINT('Ctrl Pts',(5.14669103442086,-6.02141613817701,-0.924859752744621));
#69025=CARTESIAN_POINT('Ctrl Pts',(5.44626693983657,-5.75186868383697,-0.906612807897746));
#69026=CARTESIAN_POINT('Ctrl Pts',(6.08365513783509,-5.08375134754329,-0.863855741845309));
#69027=CARTESIAN_POINT('Ctrl Pts',(6.40521083473923,-4.67212253638894,-0.839252687477308));
#69028=CARTESIAN_POINT('Ctrl Pts',(6.83377908709746,-3.99522530621722,-0.803341020633583));
#69029=CARTESIAN_POINT('Ctrl Pts',(6.97093574530893,-3.75079153685194,-0.791149445951952));
#69030=CARTESIAN_POINT('Ctrl Pts',(7.14891434369575,-3.38996795678371,-0.774294417744485));
#69031=CARTESIAN_POINT('Ctrl Pts',(7.20043523327538,-3.27911470671699,-0.76926181884632));
#69032=CARTESIAN_POINT('Ctrl Pts',(7.25686990584812,-3.14993829522916,-0.763559020995201));
#69033=CARTESIAN_POINT('Ctrl Pts',(7.26431033023114,-3.13274121601342,-0.762803066681044));
#69034=CARTESIAN_POINT('Ctrl Pts',(7.27549875626116,-3.10662717431008,-0.761660024652058));
#69035=CARTESIAN_POINT('Ctrl Pts',(7.27929159372575,-3.09772956322609,-0.761271423293779));
#69036=CARTESIAN_POINT('Ctrl Pts',(7.28582859548832,-3.08231611988869,-0.760599721328862));
#69037=CARTESIAN_POINT('Ctrl Pts',(7.2885803562698,-3.07580353343402,-0.760316365093108));
#69038=CARTESIAN_POINT('Ctrl Pts',(7.29426881849362,-3.06229016235067,-0.759729352880095));
#69039=CARTESIAN_POINT('Ctrl Pts',(7.29720418124347,-3.05528881982398,-0.759425742083725));
#69040=CARTESIAN_POINT('Ctrl Pts',(7.30431188846066,-3.03826704768689,-0.758688864540792));
#69041=CARTESIAN_POINT('Ctrl Pts',(7.30847370236117,-3.02824222281788,-0.758255951145201));
#69042=CARTESIAN_POINT('Ctrl Pts',(7.32401005144308,-2.99060024919289,-0.756634383527918));
#69043=CARTESIAN_POINT('Ctrl Pts',(7.33524885315496,-2.96292716261822,-0.755450266260491));
#69044=CARTESIAN_POINT('Ctrl Pts',(7.51550318496999,-2.51177833255245,-0.736273666809861));
#69045=CARTESIAN_POINT('Ctrl Pts',(7.64776299826329,-2.07451085555215,-0.719582059124541));
#69046=CARTESIAN_POINT('Ctrl Pts',(7.79292047012449,-1.38435250328366,-0.694699569320171));
#69047=CARTESIAN_POINT('Ctrl Pts',(7.83266473521504,-1.13815920357356,-0.686085388431047));
#69048=CARTESIAN_POINT('Ctrl Pts',(7.91934534706452,-0.373002445267586,
-0.659375255157014));
#69049=CARTESIAN_POINT('Ctrl Pts',(7.92672547430411,0.149034433640475,-0.641213532891909));
#69050=CARTESIAN_POINT('Ctrl Pts',(7.88063527444379,0.692916739309235,-0.619628888839742));
#69051=CARTESIAN_POINT('Ctrl Pts',(7.87840632985506,0.717815868184812,-0.618635786452306));
#69052=CARTESIAN_POINT('Ctrl Pts',(7.87423697717383,0.762030086392197,-0.616863911955863));
#69053=CARTESIAN_POINT('Ctrl Pts',(7.87234341424318,0.781349464499339,-0.616086843472297));
#69054=CARTESIAN_POINT('Ctrl Pts',(7.86942490156779,0.810037990224005,-0.614928849662038));
#69055=CARTESIAN_POINT('Ctrl Pts',(7.8684542765683,0.819412669972078,-0.614549799489582));
#69056=CARTESIAN_POINT('Ctrl Pts',(7.86669658832682,0.836097991930503,-0.613874023862187));
#69057=CARTESIAN_POINT('Ctrl Pts',(7.86591608005126,0.843409322994656,-0.613577519258362));
#69058=CARTESIAN_POINT('Ctrl Pts',(7.86437300180108,0.857675486291132,-0.612998223314184));
#69059=CARTESIAN_POINT('Ctrl Pts',(7.86361139635321,0.864630417012092,-0.612715464047579));
#69060=CARTESIAN_POINT('Ctrl Pts',(7.86154128276495,0.883305573064439,-0.611955293238206));
#69061=CARTESIAN_POINT('Ctrl Pts',(7.86021579430281,0.895023877570837,-0.611477332697259));
#69062=CARTESIAN_POINT('Ctrl Pts',(7.85527834342043,0.937817613733295,-0.60972842908592));
#69063=CARTESIAN_POINT('Ctrl Pts',(7.85150827837333,0.968874324003153,-0.608452542842762));
#69064=CARTESIAN_POINT('Ctrl Pts',(7.84356292826639,1.03123164928963,-0.605878202209843));
#69065=CARTESIAN_POINT('Ctrl Pts',(7.83938424566032,1.06253129201032,-0.604579670384274));
#69066=CARTESIAN_POINT('Ctrl Pts',(7.75261196159212,1.68408862618775,-0.578674569797432));
#69067=CARTESIAN_POINT('Ctrl Pts',(7.60376388218453,2.26316815993202,-0.55261160637913));
#69068=CARTESIAN_POINT('Ctrl Pts',(7.15417413758989,3.44154374197199,-0.498711264590512));
#69069=CARTESIAN_POINT('Ctrl Pts',(6.83959516893831,4.03068441704745,-0.471170276337293));
#69070=CARTESIAN_POINT('Ctrl Pts',(6.4139531919229,4.63143249114936,-0.441142251657658));
#69071=CARTESIAN_POINT('Ctrl Pts',(6.37212654461508,4.68881284209148,-0.438254545741428));
#69072=CARTESIAN_POINT('Ctrl Pts',(6.29692254954123,4.7891171013521,-0.433172184716333));
#69073=CARTESIAN_POINT('Ctrl Pts',(6.26386459953239,4.83227446798347,-0.43097385477294));
#69074=CARTESIAN_POINT('Ctrl Pts',(6.2136318266942,4.8964719726484,-0.427686223426096));
#69075=CARTESIAN_POINT('Ctrl Pts',(6.19678932474537,4.91776985307694,-0.42659258467885));
#69076=CARTESIAN_POINT('Ctrl Pts',(6.16758927180125,4.95430605239585,-0.424711328350378));
#69077=CARTESIAN_POINT('Ctrl Pts',(6.15528408700467,4.96958586777552,-0.423923004641953));
#69078=CARTESIAN_POINT('Ctrl Pts',(6.12786459876445,5.00337561139661,-0.422176206930491));
#69079=CARTESIAN_POINT('Ctrl Pts',(6.11272299731516,5.02186316143138,-0.421218124267794));
#69080=CARTESIAN_POINT('Ctrl Pts',(6.0727212031794,5.07025546564848,-0.418704026470672));
#69081=CARTESIAN_POINT('Ctrl Pts',(6.04772382071143,5.10004606906802,-0.417150003606786));
#69082=CARTESIAN_POINT('Ctrl Pts',(5.94130586239131,5.22498691686365,-0.410605034737791));
#69083=CARTESIAN_POINT('Ctrl Pts',(5.85785097371095,5.31838191993731,-0.405645029565959));
#69084=CARTESIAN_POINT('Ctrl Pts',(5.28910544649948,5.92523363192547,-0.372910332478139));
#69085=CARTESIAN_POINT('Ctrl Pts',(4.73914782770694,6.37365214872079,-0.346545664554225));
#69086=CARTESIAN_POINT('Ctrl Pts',(4.05955766140335,6.79059419927379,-0.315153461703626));
#69087=CARTESIAN_POINT('Ctrl Pts',(3.98129287275165,6.83677442889766,-0.31154927778594));
#69088=CARTESIAN_POINT('Ctrl Pts',(3.88493148963935,6.89141674451312,-0.307111023233599));
#69089=CARTESIAN_POINT('Ctrl Pts',(3.86757498566901,6.90117244776157,-0.306311568841941));
#69090=CARTESIAN_POINT('Ctrl Pts',(3.83976479654112,6.91666606831036,-0.305030404086682));
#69091=CARTESIAN_POINT('Ctrl Pts',(3.82933476459057,6.92244598771006,-0.304549876060715));
#69092=CARTESIAN_POINT('Ctrl Pts',(3.80937824556347,6.93344621290674,-0.303630411447882));
#69093=CARTESIAN_POINT('Ctrl Pts',(3.79985399128274,6.93867052460989,-0.303191580958624));
#69094=CARTESIAN_POINT('Ctrl Pts',(3.77800862509917,6.95059483268709,-0.302185046728234));
#69095=CARTESIAN_POINT('Ctrl Pts',(3.76568040663823,6.95728170859277,-0.301617013265249));
#69096=CARTESIAN_POINT('Ctrl Pts',(3.73337458576308,6.97469349359763,-0.300128547657119));
#69097=CARTESIAN_POINT('Ctrl Pts',(3.71336858364658,6.98536533632033,-0.299206840023063));
#69098=CARTESIAN_POINT('Ctrl Pts',(3.57795223578291,7.0568546174443,-0.292969089914638));
#69099=CARTESIAN_POINT('Ctrl Pts',(3.46110034055326,7.11489442279348,-0.287592067721501));
#69100=CARTESIAN_POINT('Ctrl Pts',(3.11730751590049,7.27518055312138,-0.271843227594982));
#69101=CARTESIAN_POINT('Ctrl Pts',(2.88691136656942,7.36964033663553,-0.261379964145884));
#69102=CARTESIAN_POINT('Ctrl Pts',(2.28903260266111,7.58241716673477,-0.234700740342802));
#69103=CARTESIAN_POINT('Ctrl Pts',(1.91663440211766,7.68500136030606,-0.218537919435358));
#69104=CARTESIAN_POINT('Ctrl Pts',(1.43211994361865,7.78104468231371,-0.198210587883744));
#69105=CARTESIAN_POINT('Ctrl Pts',(1.32558365282905,7.79990078581564,-0.193781397102882));
#69106=CARTESIAN_POINT('Ctrl Pts',(1.1396822247639,7.82888497326154,-0.186118667146628));
#69107=CARTESIAN_POINT('Ctrl Pts',(1.06048844325414,7.84000509733572,-0.182874985068759));
#69108=CARTESIAN_POINT('Ctrl Pts',(0.94650435057953,7.8542516400622,-0.178233557223966));
#69109=CARTESIAN_POINT('Ctrl Pts',(0.911841153463279,7.85835129244421,-0.176825669192673));
#69110=CARTESIAN_POINT('Ctrl Pts',(0.851388987199748,7.8650956624587,-0.174376295178121));
#69111=CARTESIAN_POINT('Ctrl Pts',(0.825612086663567,7.86784326705346,-0.173333764103313));
#69112=CARTESIAN_POINT('Ctrl Pts',(0.775698376311015,7.87291566021252,-0.171318532955375));
#69113=CARTESIAN_POINT('Ctrl Pts',(0.751563469653224,7.87525627006728,-0.170345683737458));
#69114=CARTESIAN_POINT('Ctrl Pts',(0.693938180257213,7.88057747043656,-0.168026485486995));
#69115=CARTESIAN_POINT('Ctrl Pts',(0.660438771445761,7.88345559420831,-0.166681168220933));
#69116=CARTESIAN_POINT('Ctrl Pts',(0.538143229680081,7.89317770837378,-0.161779729055377));
#69117=CARTESIAN_POINT('Ctrl Pts',(0.449251168430254,7.89873572445625,-0.158236103399708));
#69118=CARTESIAN_POINT('Ctrl Pts',(-0.30262101528901,7.9330131444457,-0.128388214473181));
#69119=CARTESIAN_POINT('Ctrl Pts',(-0.966736730704283,7.87970754686613,
-0.102855618202846));
#69120=CARTESIAN_POINT('Ctrl Pts',(-1.9540922700405,7.67362031966792,-0.0652276877533536));
#69121=CARTESIAN_POINT('Ctrl Pts',(-2.28680759055869,7.58112335208946,-0.0525468330231455));
#69122=CARTESIAN_POINT('Ctrl Pts',(-2.7998068750244,7.40164946148996,-0.0321688780311245));
#69123=CARTESIAN_POINT('Ctrl Pts',(-2.98465607916731,7.32906247329563,-0.024642950121644));
#69124=CARTESIAN_POINT('Ctrl Pts',(-3.24550481312258,7.21512566718817,-0.013555465931551));
#69125=CARTESIAN_POINT('Ctrl Pts',(-3.32386677737193,7.17936271035362,-0.0101619727218306));
#69126=CARTESIAN_POINT('Ctrl Pts',(-3.41514486759214,7.13589032284088,-0.00611989928989754));
#69127=CARTESIAN_POINT('Ctrl Pts',(-3.42864392055163,7.12941414343657,-0.00551980286280021));
#69128=CARTESIAN_POINT('Ctrl Pts',(-3.44928301762863,7.11944034854871,-0.00459863848856003));
#69129=CARTESIAN_POINT('Ctrl Pts',(-3.45643634911771,7.11597020624632,-0.00427869598880589));
#69130=CARTESIAN_POINT('Ctrl Pts',(-3.46889405952197,7.1099036478456,-0.00372031236871105));
#69131=CARTESIAN_POINT('Ctrl Pts',(-3.47420079147166,7.10731206139989,-0.00348207349073311));
#69132=CARTESIAN_POINT('Ctrl Pts',(-3.48612209820756,7.10147365065413,-0.00294602020970374));
#69133=CARTESIAN_POINT('Ctrl Pts',(-3.49273504356157,7.09822352490751,-0.00264806555199162));
#69134=CARTESIAN_POINT('Ctrl Pts',(-3.51038891211625,7.08951637046142,-0.00185102932588452));
#69135=CARTESIAN_POINT('Ctrl Pts',(-3.52142162238392,7.08404280312358,-0.00135123093661767));
#69136=CARTESIAN_POINT('Ctrl Pts',(-3.56873522819477,7.0604316544988,0.000799598868601299));
#69137=CARTESIAN_POINT('Ctrl Pts',(-3.604888685537,7.04204116392354,0.00246194632964015));
#69138=CARTESIAN_POINT('Ctrl Pts',(-4.42321899247683,6.6178208658783,0.0405517306117198));
#69139=CARTESIAN_POINT('Ctrl Pts',(-5.13222291348374,6.08445269227029,0.0833100832995876));
#69140=CARTESIAN_POINT('Ctrl Pts',(-6.01696175696256,5.15203959842608,0.140699852691159));
#69141=CARTESIAN_POINT('Ctrl Pts',(-6.27234988840713,4.83787424741975,0.158048075558377));
#69142=CARTESIAN_POINT('Ctrl Pts',(-6.51612066530618,4.48605105140301,0.175413745633794));
#69143=CARTESIAN_POINT('Ctrl Pts',(-6.52952938742779,4.46651189985413,0.176372000855372));
#69144=CARTESIAN_POINT('Ctrl Pts',(-6.54895316415056,4.43793322739295,0.177764649949383));
#69145=CARTESIAN_POINT('Ctrl Pts',(-6.55503766567519,4.42894119172777,0.178201553671758));
#69146=CARTESIAN_POINT('Ctrl Pts',(-6.5656764029701,4.41314868974018,0.178966640012359));
#69147=CARTESIAN_POINT('Ctrl Pts',(-6.57023862568318,4.40635363859298,0.179295110308285));
#69148=CARTESIAN_POINT('Ctrl Pts',(-6.57907100052883,4.39315433580018,0.179931759899439));
#69149=CARTESIAN_POINT('Ctrl Pts',(-6.5833423662229,4.38675090900764,0.180239982664855));
#69150=CARTESIAN_POINT('Ctrl Pts',(-6.593508171665,4.3714625328864,0.180974358684691));
#69151=CARTESIAN_POINT('Ctrl Pts',(-6.59939401452939,4.36257187084997,0.181400203239108));
#69152=CARTESIAN_POINT('Ctrl Pts',(-6.61710444506986,4.33570211496103,0.182683552246976));
#69153=CARTESIAN_POINT('Ctrl Pts',(-6.62887370779771,4.31768658446259,0.183539077684414));
#69154=CARTESIAN_POINT('Ctrl Pts',(-6.74800299509092,4.1336969031297,0.192226736964433));
#69155=CARTESIAN_POINT('Ctrl Pts',(-6.84918358459858,3.96379679945411,0.199836259942572));
#69156=CARTESIAN_POINT('Ctrl Pts',(-7.26177346692412,3.20792015919807,0.232134480405514));
#69157=CARTESIAN_POINT('Ctrl Pts',(-7.50511823228193,2.58791694293089,0.254454982516534));
#69158=CARTESIAN_POINT('Ctrl Pts',(-7.77669296721741,1.51711918286306,0.29294060734452));
#69159=CARTESIAN_POINT('Ctrl Pts',(-7.84918681734211,1.08112487855704,0.308685458497038));
#69160=CARTESIAN_POINT('Ctrl Pts',(-7.8863038062427,0.624827576467823,0.326964441133551));
#69161=CARTESIAN_POINT('Ctrl Pts',(-7.88759907778965,0.608258173998842,
0.327630519167729));
#69162=CARTESIAN_POINT('Ctrl Pts',(-7.889397511442,0.584279940193138,0.328597658169758));
#69163=CARTESIAN_POINT('Ctrl Pts',(-7.88994247683504,0.576874209623265,
0.328896806957226));
#69164=CARTESIAN_POINT('Ctrl Pts',(-7.89087448147038,0.563960464715188,
0.329419211895097));
#69165=CARTESIAN_POINT('Ctrl Pts',(-7.89126618336089,0.558452783327961,
0.329642258651101));
#69166=CARTESIAN_POINT('Ctrl Pts',(-7.89201132765303,0.547818049938513,
0.330073399551271));
#69167=CARTESIAN_POINT('Ctrl Pts',(-7.89236554094427,0.542691053542111,
0.330281459459491));
#69168=CARTESIAN_POINT('Ctrl Pts',(-7.89319281065941,0.530544765385646,
0.330774856047037));
#69169=CARTESIAN_POINT('Ctrl Pts',(-7.89366149960529,0.523525188965229,
0.331060383232331));
#69170=CARTESIAN_POINT('Ctrl Pts',(-7.89503201352728,0.502578630475558,
0.33191352820109));
#69171=CARTESIAN_POINT('Ctrl Pts',(-7.89590634595267,0.488649922588824,
0.332482323923043));
#69172=CARTESIAN_POINT('Ctrl Pts',(-7.90387826652317,0.356040506440882,
0.337911262116892));
#69173=CARTESIAN_POINT('Ctrl Pts',(-7.90833619723854,0.237219840392893,
0.342879684112651));
#69174=CARTESIAN_POINT('Ctrl Pts',(-7.91067802142328,0.080697658441547,
0.349523829075627));
#69175=CARTESIAN_POINT('Ctrl Pts',(-7.91097250897623,0.0430440070615793,
0.351129753580282));
#69176=CARTESIAN_POINT('Ctrl Pts',(-7.91113408027291,-0.194096696370491,
0.361286214600696));
#69177=CARTESIAN_POINT('Ctrl Pts',(-7.90372443035215,-0.39351272728581,
0.370013797739556));
#69178=CARTESIAN_POINT('Ctrl Pts',(-7.86327959725429,-0.932075543662419,
0.393795777188776));
#69179=CARTESIAN_POINT('Ctrl Pts',(-7.81586396527105,-1.26972848142478,
0.408917764487408));
#69180=CARTESIAN_POINT('Ctrl Pts',(-7.66021932085351,-2.02178451207977,
0.442337527682981));
#69181=CARTESIAN_POINT('Ctrl Pts',(-7.53983025666885,-2.43260784721639,
0.460384148701842));
#69182=CARTESIAN_POINT('Ctrl Pts',(-7.37323433896409,-2.86719013982119,
0.479250342479628));
#69183=CARTESIAN_POINT('Ctrl Pts',(-7.35938209004656,-2.90256080052845,
0.480784677243386));
#69184=CARTESIAN_POINT('Ctrl Pts',(-7.33955573220331,-2.95213141400793,
0.482933725846532));
#69185=CARTESIAN_POINT('Ctrl Pts',(-7.33379415562166,-2.96641560082236,
0.483552844624101));
#69186=CARTESIAN_POINT('Ctrl Pts',(-7.32313780372092,-2.99261417751219,
0.484688136423428));
#69187=CARTESIAN_POINT('Ctrl Pts',(-7.31825557981575,-3.00453360398302,
0.485204565716377));
#69188=CARTESIAN_POINT('Ctrl Pts',(-7.30828851683016,-3.02869869158878,
0.486251406362699));
#69189=CARTESIAN_POINT('Ctrl Pts',(-7.30320195745272,-3.04094360020834,
0.48678178062176));
#69190=CARTESIAN_POINT('Ctrl Pts',(-7.2905666746271,-3.07114604279159,0.488089805146977));
#69191=CARTESIAN_POINT('Ctrl Pts',(-7.28298235371228,-3.08908861850425,
0.488866732386426));
#69192=CARTESIAN_POINT('Ctrl Pts',(-7.25499059363136,-3.15463388500575,
0.491704564453053));
#69193=CARTESIAN_POINT('Ctrl Pts',(-7.23418190737374,-3.20206428257444,
0.493757565627394));
#69194=CARTESIAN_POINT('Ctrl Pts',(-7.1158391955095,-3.46476658125485,0.505128828410783));
#69195=CARTESIAN_POINT('Ctrl Pts',(-7.0091601478767,-3.67579319138934,0.514257890867353));
#69196=CARTESIAN_POINT('Ctrl Pts',(-6.72152872753648,-4.18656960944573,
0.536478714487409));
#69197=CARTESIAN_POINT('Ctrl Pts',(-6.52983221270056,-4.47968921005404,
0.549331851355685));
#69198=CARTESIAN_POINT('Ctrl Pts',(-6.0109180945819,-5.16871926905778,0.580807858824923));
#69199=CARTESIAN_POINT('Ctrl Pts',(-5.66341238307279,-5.5472953081069,0.59922546479623));
#69200=CARTESIAN_POINT('Ctrl Pts',(-5.22679142747073,-5.93885713485855,
0.622136843487409));
#69201=CARTESIAN_POINT('Ctrl Pts',(-5.17113611814522,-5.98738035444429,
0.625054929994005));
#69202=CARTESIAN_POINT('Ctrl Pts',(-5.10496151252808,-6.04346387813062,
0.6285308288425));
#69203=CARTESIAN_POINT('Ctrl Pts',(-5.09509172781592,-6.0517871718369,0.629049412596094));
#69204=CARTESIAN_POINT('Ctrl Pts',(-5.07923919828449,-6.06508950883681,
0.629882670596337));
#69205=CARTESIAN_POINT('Ctrl Pts',(-5.07326937940912,-6.07008396869089,
0.630196536410737));
#69206=CARTESIAN_POINT('Ctrl Pts',(-5.06267466904515,-6.07892115030153,
0.630753704546092));
#69207=CARTESIAN_POINT('Ctrl Pts',(-5.05805274330983,-6.08276742953376,
0.630996817583994));
#69208=CARTESIAN_POINT('Ctrl Pts',(-5.04844293474478,-6.09074600435306,
0.631502404111061));
#69209=CARTESIAN_POINT('Ctrl Pts',(-5.04345435446418,-6.09487744987591,
0.631764922866609));
#69210=CARTESIAN_POINT('Ctrl Pts',(-5.03057657313571,-6.10551594241911,
0.632442775909948));
#69211=CARTESIAN_POINT('Ctrl Pts',(-5.02267983443925,-6.11201381384533,
0.63285860724703));
#69212=CARTESIAN_POINT('Ctrl Pts',(-4.98967655326645,-6.1390635779207,0.634597299212861));
#69213=CARTESIAN_POINT('Ctrl Pts',(-4.96445654791544,-6.15947602129014,
0.635927839550689));
#69214=CARTESIAN_POINT('Ctrl Pts',(-4.52838240647946,-6.5080055099179,0.658977828626436));
#69215=CARTESIAN_POINT('Ctrl Pts',(-4.08603059740957,-6.79444747358901,
0.683308073093284));
#69216=CARTESIAN_POINT('Ctrl Pts',(-3.19496179601415,-7.25280305552963,
0.729680837587388));
#69217=CARTESIAN_POINT('Ctrl Pts',(-2.75241107654865,-7.43204171326891,
0.751598835914133));
#69218=CARTESIAN_POINT('Ctrl Pts',(-2.06504167107419,-7.64054781812181,
0.782743862105871));
#69219=CARTESIAN_POINT('Ctrl Pts',(-1.83058633857419,-7.70008674145379,
0.792903000473528));
#69220=CARTESIAN_POINT('Ctrl Pts',(-1.57112006888485,-7.75345321823026,
0.803635496280399));
#69221=CARTESIAN_POINT('Ctrl Pts',(-1.54846335417354,-7.75800981768439,
0.804568504197486));
#69222=CARTESIAN_POINT('Ctrl Pts',(-1.51655999575588,-7.76428072674086,
0.805876484469635));
#69223=CARTESIAN_POINT('Ctrl Pts',(-1.50732987950346,-7.76607790712419,
0.806254220020084));
#69224=CARTESIAN_POINT('Ctrl Pts',(-1.49128717428575,-7.76917187711368,
0.806909573807847));
#69225=CARTESIAN_POINT('Ctrl Pts',(-1.48447605323501,-7.77047617202754,
0.807187442230658));
#69226=CARTESIAN_POINT('Ctrl Pts',(-1.47028193034725,-7.77317493037592,
0.807765741329133));
#69227=CARTESIAN_POINT('Ctrl Pts',(-1.46289863695209,-7.77456783566554,
0.808066119789815));
#69228=CARTESIAN_POINT('Ctrl Pts',(-1.44547582574641,-7.77782906209976,
0.808773923495439));
#69229=CARTESIAN_POINT('Ctrl Pts',(-1.43543464129414,-7.77968846893555,
0.809181051015383));
#69230=CARTESIAN_POINT('Ctrl Pts',(-1.40245943380679,-7.78572873811413,
0.81051545232933));
#69231=CARTESIAN_POINT('Ctrl Pts',(-1.3795104257884,-7.78982769030095,0.8114399931544));
#69232=CARTESIAN_POINT('Ctrl Pts',(-0.978932484073002,-7.85954973204209,
0.827506727321981));
#69233=CARTESIAN_POINT('Ctrl Pts',(-0.597028528464808,-7.8977484596977,
0.84168419610726));
#69234=CARTESIAN_POINT('Ctrl Pts',(0.301190809625515,-7.92203506861667,
0.873400238837709));
#69235=CARTESIAN_POINT('Ctrl Pts',(0.81631598619467,-7.88561832759274,0.890304356520257));
#69236=CARTESIAN_POINT('Ctrl Pts',(1.61982881854081,-7.74919126816101,0.918117963333181));
#69237=CARTESIAN_POINT('Ctrl Pts',(1.91230550033713,-7.68224420467472,0.928581740609763));
#69238=CARTESIAN_POINT('Ctrl Pts',(2.2418608423217,-7.58682127191102,0.941428481064208));
#69239=CARTESIAN_POINT('Ctrl Pts',(2.28336503064313,-7.57443338318042,0.943066079640623));
#69240=CARTESIAN_POINT('Ctrl Pts',(2.41171215342113,-7.53497444466144,0.948197036242251));
#69241=CARTESIAN_POINT('Ctrl Pts',(2.49818886956554,-7.50674673645679,0.951749500546143));
#69242=CARTESIAN_POINT('Ctrl Pts',(2.59410636589023,-7.47359645612732,0.955815888665348));
#69243=CARTESIAN_POINT('Ctrl Pts',(2.60404937473593,-7.47013779514324,0.956238941930233));
#69244=CARTESIAN_POINT('Ctrl Pts',(2.61895953425925,-7.46491793205423,0.956875663367475));
#69245=CARTESIAN_POINT('Ctrl Pts',(2.62393188039337,-7.46317159532852,0.957088391231943));
#69246=CARTESIAN_POINT('Ctrl Pts',(2.63255876116346,-7.4601320629529,0.95745814621254));
#69247=CARTESIAN_POINT('Ctrl Pts',(2.6362140586181,-7.45884116097915,0.957615026163655));
#69248=CARTESIAN_POINT('Ctrl Pts',(2.64382959650188,-7.45614536620189,0.957942311150955));
#69249=CARTESIAN_POINT('Ctrl Pts',(2.64778966820685,-7.45474000419017,0.958112745672993));
#69250=CARTESIAN_POINT('Ctrl Pts',(2.65713077838812,-7.45141662108601,0.95851534931639));
#69251=CARTESIAN_POINT('Ctrl Pts',(2.66251085660703,-7.4494959274147,0.958747685145861));
#69252=CARTESIAN_POINT('Ctrl Pts',(2.68016674107373,-7.44317118783274,0.959511622120159));
#69253=CARTESIAN_POINT('Ctrl Pts',(2.69243368049453,-7.43874263323731,0.960044735265224));
#69254=CARTESIAN_POINT('Ctrl Pts',(3.01165668557476,-7.32260513465293,0.973977959528962));
#69255=CARTESIAN_POINT('Ctrl Pts',(3.31138566483445,-7.19203077666982,0.988497039594466));
#69256=CARTESIAN_POINT('Ctrl Pts',(3.78865342200688,-6.94794253030611,1.01298277459154));
#69257=CARTESIAN_POINT('Ctrl Pts',(3.97128725472937,-6.84519357638455,1.02270760994379));
#69258=CARTESIAN_POINT('Ctrl Pts',(4.34780607817477,-6.6132206446582,1.04323951818558));
#69259=CARTESIAN_POINT('Ctrl Pts',(4.54050589649925,-6.48243131828122,1.05403563300145));
#69260=CARTESIAN_POINT('Ctrl Pts',(5.11866494297116,-6.05157720954975,1.08693784811189));
#69261=CARTESIAN_POINT('Ctrl Pts',(5.48235588577568,-5.72417726992167,1.10830267994569));
#69262=CARTESIAN_POINT('Ctrl Pts',(5.83549947986606,-5.34152711247806,1.12946528710456));
#69263=CARTESIAN_POINT('Ctrl Pts',(5.85727857190797,-5.31763611366062,1.13077276203441));
#69264=CARTESIAN_POINT('Ctrl Pts',(5.8870596111589,-5.28456227489341,1.13256398865709));
#69265=CARTESIAN_POINT('Ctrl Pts',(5.89518755413347,-5.27549362675442,1.13305320598128));
#69266=CARTESIAN_POINT('Ctrl Pts',(5.90809544553832,-5.26102473054823,1.13383069403956));
#69267=CARTESIAN_POINT('Ctrl Pts',(5.9128889893362,-5.25563667020221,1.13411955155512));
#69268=CARTESIAN_POINT('Ctrl Pts',(5.92219769285639,-5.24514460467396,1.13468073806562));
#69269=CARTESIAN_POINT('Ctrl Pts',(5.92671363823681,-5.24004130593262,1.13495310080827));
#69270=CARTESIAN_POINT('Ctrl Pts',(5.93749464532129,-5.22782633255479,1.13560359237155));
#69271=CARTESIAN_POINT('Ctrl Pts',(5.94375353854363,-5.22070921431547,1.13598145644064));
#69272=CARTESIAN_POINT('Ctrl Pts',(5.96246377845384,-5.19935615123396,1.13711171506887));
#69273=CARTESIAN_POINT('Ctrl Pts',(5.97487692086391,-5.18508673830982,1.13786247747011));
#69274=CARTESIAN_POINT('Ctrl Pts',(6.082045867785,-5.0609957958204,1.14435229051958));
#69275=CARTESIAN_POINT('Ctrl Pts',(6.17381847618985,-4.94862895776917,1.14996415952195));
#69276=CARTESIAN_POINT('Ctrl Pts',(6.39930133272391,-4.65650345354465,1.16394163762249));
#69277=CARTESIAN_POINT('Ctrl Pts',(6.52856351607667,-4.47347159755049,1.17213566413985));
#69278=CARTESIAN_POINT('Ctrl Pts',(6.8853248807192,-3.91983877512422,1.19563993270673));
#69279=CARTESIAN_POINT('Ctrl Pts',(7.09025293168861,-3.5356965918727,1.21031707315098));
#69280=CARTESIAN_POINT('Ctrl Pts',(7.4028938548105,-2.81181516262591,1.23755131853022));
#69281=CARTESIAN_POINT('Ctrl Pts',(7.52123541730029,-2.4779272566285,1.2499838263971));
#69282=CARTESIAN_POINT('Ctrl Pts',(7.64235820823402,-2.04626861047108,1.26711097783196));
#69283=CARTESIAN_POINT('Ctrl Pts',(7.66625918263362,-1.95482047471425,1.27079840807742));
#69284=CARTESIAN_POINT('Ctrl Pts',(7.6914005157306,-1.85106164863855,1.27507067218087));
#69285=CARTESIAN_POINT('Ctrl Pts',(7.69425811604767,-1.83914740096191,1.27556255849954));
#69286=CARTESIAN_POINT('Ctrl Pts',(7.69841653386357,-1.82163030066871,1.27628771891884));
#69287=CARTESIAN_POINT('Ctrl Pts',(7.69973889644629,-1.81603276606096,1.27651973258855));
#69288=CARTESIAN_POINT('Ctrl Pts',(7.702083840748,-1.80605805982674,1.27693368862337));
#69289=CARTESIAN_POINT('Ctrl Pts',(7.70310879968537,-1.80168144393878,1.27711549613169));
#69290=CARTESIAN_POINT('Ctrl Pts',(7.70524164793555,-1.79253900584068,1.27749564183167));
#69291=CARTESIAN_POINT('Ctrl Pts',(7.70634884675568,-1.78777302598855,1.27769401868533));
#69292=CARTESIAN_POINT('Ctrl Pts',(7.70921700132435,-1.77537477147594,1.27821060709812));
#69293=CARTESIAN_POINT('Ctrl Pts',(7.71097104119072,-1.76774091818448,1.2785292024733));
#69294=CARTESIAN_POINT('Ctrl Pts',(7.71843976117335,-1.73501325952487,1.27989727257737));
#69295=CARTESIAN_POINT('Ctrl Pts',(7.72404325284918,-1.7098944874602,1.28095280910065));
#69296=CARTESIAN_POINT('Ctrl Pts',(7.80280442489478,-1.34854312837109,1.2962123110058));
#69297=CARTESIAN_POINT('Ctrl Pts',(7.85406543932431,-1.00793969377509,1.31151386769961));
#69298=CARTESIAN_POINT('Ctrl Pts',(7.92949326281809,-0.113963894222885,
1.35225740440064));
#69299=CARTESIAN_POINT('Ctrl Pts',(7.91806835812111,0.440600274355359,1.37799794823071));
#69300=CARTESIAN_POINT('Ctrl Pts',(7.83210139939867,1.12254467519836,1.40818862001701));
#69301=CARTESIAN_POINT('Ctrl Pts',(7.81193879079907,1.25520247804307,1.41399988141834));
#69302=CARTESIAN_POINT('Ctrl Pts',(7.76443214114257,1.52191099476298,1.42554434086491));
#69303=CARTESIAN_POINT('Ctrl Pts',(7.73696559959172,1.65589408415447,1.43127189912038));
#69304=CARTESIAN_POINT('Ctrl Pts',(7.69155541436089,1.85148527022574,1.43952691416695));
#69305=CARTESIAN_POINT('Ctrl Pts',(7.67631485624526,1.91369090229151,1.44213648360352));
#69306=CARTESIAN_POINT('Ctrl Pts',(7.65622013014844,1.99160334154202,1.44538568792651));
#69307=CARTESIAN_POINT('Ctrl Pts',(7.65207037315818,2.00748837098475,1.44604713615625));
#69308=CARTESIAN_POINT('Ctrl Pts',(7.64546084737434,2.03247096976761,1.44708583474866));
#69309=CARTESIAN_POINT('Ctrl Pts',(7.64303423244067,2.04157721729774,1.4474641152804));
#69310=CARTESIAN_POINT('Ctrl Pts',(7.63872294567616,2.05764056914736,1.44813082337534));
#69311=CARTESIAN_POINT('Ctrl Pts',(7.63684502910415,2.06459946584801,1.44841946083274));
#69312=CARTESIAN_POINT('Ctrl Pts',(7.63252722730391,2.08051322192979,1.44907908909235));
#69313=CARTESIAN_POINT('Ctrl Pts',(7.6300810864038,2.08946638111303,1.44944988448129));
#69314=CARTESIAN_POINT('Ctrl Pts',(7.62340214184059,2.11374396206957,1.45045449464372));
#69315=CARTESIAN_POINT('Ctrl Pts',(7.61913888065585,2.1290599978215,1.45108735842495));
#69316=CARTESIAN_POINT('Ctrl Pts',(7.5969978138326,2.20768494960582,1.45433153583404));
#69317=CARTESIAN_POINT('Ctrl Pts',(7.57837677796811,2.27078274681001,1.45691956027937));
#69318=CARTESIAN_POINT('Ctrl Pts',(7.52483261717145,2.44421927038467,1.46399406323524));
#69319=CARTESIAN_POINT('Ctrl Pts',(7.48827164313876,2.55403657479191,1.46842920652532));
#69320=CARTESIAN_POINT('Ctrl Pts',(7.35250329062869,2.93382453463047,1.48364750039816));
#69321=CARTESIAN_POINT('Ctrl Pts',(7.24099469376575,3.19916239604902,1.49405608761019));
#69322=CARTESIAN_POINT('Ctrl Pts',(6.98303509029311,3.72997058145068,1.51492775467666));
#69323=CARTESIAN_POINT('Ctrl Pts',(6.83528780563502,3.99428364284762,1.5253484602029));
#69324=CARTESIAN_POINT('Ctrl Pts',(6.42659214822958,4.6360394260103,1.55183257787725));
#69325=CARTESIAN_POINT('Ctrl Pts',(6.14731621122736,5.00043674921337,1.56797806795701));
#69326=CARTESIAN_POINT('Ctrl Pts',(5.81940161360902,5.359034860021,1.58723247941226));
#69327=CARTESIAN_POINT('Ctrl Pts',(5.80058357072736,5.37939773367214,1.58833846278712));
#69328=CARTESIAN_POINT('Ctrl Pts',(5.77592680644698,5.40579883625361,1.58978955651309));
#69329=CARTESIAN_POINT('Ctrl Pts',(5.7701847865595,5.41192748098696,1.59012762127));
#69330=CARTESIAN_POINT('Ctrl Pts',(5.76133851614269,5.42133931036578,1.59064868102908));
#69331=CARTESIAN_POINT('Ctrl Pts',(5.75824117996673,5.42462901301864,1.59083116248052));
#69332=CARTESIAN_POINT('Ctrl Pts',(5.75211708184382,5.43112230584879,1.59119205698398));
#69333=CARTESIAN_POINT('Ctrl Pts',(5.74909045730042,5.43432602426156,1.59137045974044));
#69334=CARTESIAN_POINT('Ctrl Pts',(5.74238107431875,5.44141610832319,1.59176604027809));
#69335=CARTESIAN_POINT('Ctrl Pts',(5.73869704725166,5.4453012649639,1.59198331422795));
#69336=CARTESIAN_POINT('Ctrl Pts',(5.72816199187676,5.45638891644689,1.59260484223571));
#69337=CARTESIAN_POINT('Ctrl Pts',(5.7213014216135,5.46358214500764,1.59300983283677));
#69338=CARTESIAN_POINT('Ctrl Pts',(5.6733740144914,5.51364421215869,1.59584082693093));
#69339=CARTESIAN_POINT('Ctrl Pts',(5.63184040106756,5.55606142519326,1.59830291972939));
#69340=CARTESIAN_POINT('Ctrl Pts',(5.52249352897605,5.66524867711007,1.60479696528814));
#69341=CARTESIAN_POINT('Ctrl Pts',(5.45394699079058,5.73126847812177,1.60887958943954));
#69342=CARTESIAN_POINT('Ctrl Pts',(5.14181593027705,6.02122280938211,1.62744910633205));
#69343=CARTESIAN_POINT('Ctrl Pts',(4.8855256183909,6.23097211184154,1.64262759848161));
#69344=CARTESIAN_POINT('Ctrl Pts',(4.34967110798423,6.61608313900535,1.67307017565107));
#69345=CARTESIAN_POINT('Ctrl Pts',(4.07073868440935,6.79126613214633,1.68830113079214));
#69346=CARTESIAN_POINT('Ctrl Pts',(3.40527424525268,7.15343944058758,1.72243051756395));
#69347=CARTESIAN_POINT('Ctrl Pts',(3.01279290394992,7.32739678014616,1.74096206394387));
#69348=CARTESIAN_POINT('Ctrl Pts',(2.58265222392357,7.47760358057917,1.75943742532252));
#69349=CARTESIAN_POINT('Ctrl Pts',(2.55715446717307,7.48636152403647,1.76052622264357));
#69350=CARTESIAN_POINT('Ctrl Pts',(2.52199475121543,7.49823756122175,1.76201890289129));
#69351=CARTESIAN_POINT('Ctrl Pts',(2.51237096836658,7.50146760094104,1.76242657931731));
#69352=CARTESIAN_POINT('Ctrl Pts',(2.49589586770674,7.50696189440581,1.76312296303653));
#69353=CARTESIAN_POINT('Ctrl Pts',(2.48904763154708,7.50923531092091,1.7634119804516));
#69354=CARTESIAN_POINT('Ctrl Pts',(2.47572727428686,7.51363706078377,1.76397327034386));
#69355=CARTESIAN_POINT('Ctrl Pts',(2.46925549594348,7.51576640895075,1.76424557700168));
#69356=CARTESIAN_POINT('Ctrl Pts',(2.45378398475232,7.52083471354659,1.7648956047355));
#69357=CARTESIAN_POINT('Ctrl Pts',(2.44478170159639,7.52376588316435,1.76527306228048));
#69358=CARTESIAN_POINT('Ctrl Pts',(2.41818662800142,7.53237254444137,1.76638590942943));
#69359=CARTESIAN_POINT('Ctrl Pts',(2.4005791260392,7.53800255915434,1.76711976290587));
#69360=CARTESIAN_POINT('Ctrl Pts',(2.25588156018059,7.583711329935,1.77312681150086));
#69361=CARTESIAN_POINT('Ctrl Pts',(2.12781383138726,7.62063577498225,1.77829291440644));
#69362=CARTESIAN_POINT('Ctrl Pts',(1.81277731687962,7.70290540083898,1.79066719239981));
#69363=CARTESIAN_POINT('Ctrl Pts',(1.62496848516576,7.74470115482851,1.79776015246552));
#69364=CARTESIAN_POINT('Ctrl Pts',(1.15238130106175,7.83192248198373,1.81506245537962));
#69365=CARTESIAN_POINT('Ctrl Pts',(0.866293443997138,7.86870617413613,1.82504378371942));
#69366=CARTESIAN_POINT('Ctrl Pts',(-0.0524261159683648,7.93610743082871,
1.85658204200696));
#69367=CARTESIAN_POINT('Ctrl Pts',(-0.686871950875746,7.90648721083647,
1.87747032809366));
#69368=CARTESIAN_POINT('Ctrl Pts',(-1.34816033135247,7.7953711819752,1.90387280606141));
#69369=CARTESIAN_POINT('Ctrl Pts',(-1.38536970957351,7.78884451128901,1.90537474700557));
#69370=CARTESIAN_POINT('Ctrl Pts',(-1.43048245795619,7.78059806743851,1.90721709088383));
#69371=CARTESIAN_POINT('Ctrl Pts',(-1.43843233814451,7.77913226248515,1.90754256108662));
#69372=CARTESIAN_POINT('Ctrl Pts',(-1.45148191255063,7.77670548420166,1.90807816134065));
#69373=CARTESIAN_POINT('Ctrl Pts',(-1.45658294707071,7.77575167096252,1.9082878638964));
#69374=CARTESIAN_POINT('Ctrl Pts',(-1.465738948893,7.77403031674311,1.90866487862788));
#69375=CARTESIAN_POINT('Ctrl Pts',(-1.46979426541629,7.7732646197826,1.90883207960772));
#69376=CARTESIAN_POINT('Ctrl Pts',(-1.47840429542076,7.77163195451163,1.90918753416234));
#69377=CARTESIAN_POINT('Ctrl Pts',(-1.48295884755782,7.77076415504748,1.90937583817795));
#69378=CARTESIAN_POINT('Ctrl Pts',(-1.49522619049994,7.76841562476377,1.9098837678716));
#69379=CARTESIAN_POINT('Ctrl Pts',(-1.50293750640738,7.76692741888601,1.91020385210367));
#69380=CARTESIAN_POINT('Ctrl Pts',(-1.54136074899968,7.75945275801042,1.91180266677277));
#69381=CARTESIAN_POINT('Ctrl Pts',(-1.57203879797313,7.75329568796154,1.91309171154383));
#69382=CARTESIAN_POINT('Ctrl Pts',(-1.83549708248724,7.69879182440814,1.92426448270721));
#69383=CARTESIAN_POINT('Ctrl Pts',(-2.06600781666357,7.6401595897593,1.93472808542587));
#69384=CARTESIAN_POINT('Ctrl Pts',(-2.52469654079835,7.50121195800753,1.95645562050984));
#69385=CARTESIAN_POINT('Ctrl Pts',(-2.75254864587117,7.42062948669689,1.96771748595835));
#69386=CARTESIAN_POINT('Ctrl Pts',(-3.18833776494563,7.24367121757269,1.98975947015524));
#69387=CARTESIAN_POINT('Ctrl Pts',(-3.39649559556496,7.14843272975139,2.00052344681072));
#69388=CARTESIAN_POINT('Ctrl Pts',(-3.61059264032584,7.03901108946279,2.01170154648894));
#69389=CARTESIAN_POINT('Ctrl Pts',(-3.62093970458779,7.03369404995895,2.01224205106997));
#69390=CARTESIAN_POINT('Ctrl Pts',(-3.96544901597128,6.85569959776057,2.03024720333538));
#69391=CARTESIAN_POINT('Ctrl Pts',(-4.28690767162199,6.65941980550538,2.04729133160068));
#69392=CARTESIAN_POINT('Ctrl Pts',(-4.76585900725941,6.31786970092608,2.0726408058102));
#69393=CARTESIAN_POINT('Ctrl Pts',(-4.93350029482871,6.18784891863283,2.08151139185494));
#69394=CARTESIAN_POINT('Ctrl Pts',(-5.11145106485326,6.03799732800331,2.09093429012564));
#69395=CARTESIAN_POINT('Ctrl Pts',(-5.12712624877658,6.02469253648826,2.09176442033273));
#69396=CARTESIAN_POINT('Ctrl Pts',(-5.15031389465427,6.0048552760769,2.09299257989854));
#69397=CARTESIAN_POINT('Ctrl Pts',(-5.15786611694894,5.99836954685847,2.09339262077767));
#69398=CARTESIAN_POINT('Ctrl Pts',(-5.17076850775989,5.98724679336051,2.09407611574168));
#69399=CARTESIAN_POINT('Ctrl Pts',(-5.17612472163907,5.98261681807077,2.09435987391054));
#69400=CARTESIAN_POINT('Ctrl Pts',(-5.18652834594398,5.97359937078779,2.0949110655382));
#69401=CARTESIAN_POINT('Ctrl Pts',(-5.19157642193942,5.96921267684744,2.09517853232561));
#69402=CARTESIAN_POINT('Ctrl Pts',(-5.20362936303686,5.95871201691534,2.09581718544443));
#69403=CARTESIAN_POINT('Ctrl Pts',(-5.21062903145754,5.95259208628538,2.09618811251325));
#69404=CARTESIAN_POINT('Ctrl Pts',(-5.23155346318051,5.93423230700284,2.09729705197242));
#69405=CARTESIAN_POINT('Ctrl Pts',(-5.24544605218195,5.92195579445637,2.09803346861905));
#69406=CARTESIAN_POINT('Ctrl Pts',(-5.36488350044488,5.81566203810158,2.10436610445773));
#69407=CARTESIAN_POINT('Ctrl Pts',(-5.46793717313559,5.71887800009418,2.10983959434883));
#69408=CARTESIAN_POINT('Ctrl Pts',(-5.78893962350264,5.40079090319609,2.12697558305169));
#69409=CARTESIAN_POINT('Ctrl Pts',(-5.99647920700682,5.16939260293312,2.13817683724625));
#69410=CARTESIAN_POINT('Ctrl Pts',(-6.22360909018243,4.88400894421965,2.15096342024755));
#69411=CARTESIAN_POINT('Ctrl Pts',(-6.25689534504864,4.84129261450204,2.15285242656162));
#69412=CARTESIAN_POINT('Ctrl Pts',(-6.31320851777073,4.76747483548044,2.15607831746115));
#69413=CARTESIAN_POINT('Ctrl Pts',(-6.33645053399966,4.7365401660442,2.15741881856307));
#69414=CARTESIAN_POINT('Ctrl Pts',(-6.43409090880158,4.60457779256147,2.16309290320925));
#69415=CARTESIAN_POINT('Ctrl Pts',(-6.50630752206593,4.50195793057714,2.16739587818395));
#69416=CARTESIAN_POINT('Ctrl Pts',(-6.89647201577676,3.91852483104086,2.19143871543941));
#69417=CARTESIAN_POINT('Ctrl Pts',(-7.16356297767803,3.40580563186794,2.21093928248211));
#69418=CARTESIAN_POINT('Ctrl Pts',(-7.38551731810349,2.83537117864144,2.23513968744872));
#69419=CARTESIAN_POINT('Ctrl Pts',(-7.39823855945185,2.80201033778206,2.2365624603226));
#69420=CARTESIAN_POINT('Ctrl Pts',(-7.41460145233,2.75821109906044,2.23843922483164));
#69421=CARTESIAN_POINT('Ctrl Pts',(-7.41844780933309,2.74784920662286,2.23888386768796));
#69422=CARTESIAN_POINT('Ctrl Pts',(-7.42434668166966,2.7318552821801,2.2395711485841));
#69423=CARTESIAN_POINT('Ctrl Pts',(-7.42641454175537,2.7262288946686,2.23981310510466));
#69424=CARTESIAN_POINT('Ctrl Pts',(-7.43049858028765,2.71507761175493,2.2402930093324));
#69425=CARTESIAN_POINT('Ctrl Pts',(-7.43251499669349,2.70955280686344,2.24053094643773));
#69426=CARTESIAN_POINT('Ctrl Pts',(-7.43698316688266,2.69726789284315,2.24106039858926));
#69427=CARTESIAN_POINT('Ctrl Pts',(-7.43943186637629,2.69050668375757,2.24135204496635));
#69428=CARTESIAN_POINT('Ctrl Pts',(-7.44643682110039,2.6710823245341,2.24219063071053));
#69429=CARTESIAN_POINT('Ctrl Pts',(-7.45096997327485,2.65841091057888,2.24273854646207));
#69430=CARTESIAN_POINT('Ctrl Pts',(-7.48049409382297,2.57521406887332,2.24634144595223));
#69431=CARTESIAN_POINT('Ctrl Pts',(-7.50451529450351,2.50435004019854,2.24943586494628));
#69432=CARTESIAN_POINT('Ctrl Pts',(-7.57745191539672,2.27870398008065,2.25935047053162));
#69433=CARTESIAN_POINT('Ctrl Pts',(-7.62260959672493,2.12275504683166,2.26629273175166));
#69434=CARTESIAN_POINT('Ctrl Pts',(-7.82724748024627,1.32494236079879,2.30197280470235));
#69435=CARTESIAN_POINT('Ctrl Pts',(-7.91058737473885,0.666279616503375,
2.33170392820332));
#69436=CARTESIAN_POINT('Ctrl Pts',(-7.91099847169151,0.00491740731324478,
2.35986591881366));
#69437=CARTESIAN_POINT('',(-7.92581838649827,-0.00396439408934276,6.35738248087998));
#69438=CARTESIAN_POINT('Ctrl Pts',(-7.91099847812363,0.00490704857253402,
2.35986635990733));
#69439=CARTESIAN_POINT('Ctrl Pts',(-7.91117119108635,-0.273535678266459,
2.37172294511405));
#69440=CARTESIAN_POINT('Ctrl Pts',(-7.89664345732018,-0.551807601433357,
2.38331463608623));
#69441=CARTESIAN_POINT('Ctrl Pts',(-7.86391655216152,-0.862489658471575,
2.39600992918712));
#69442=CARTESIAN_POINT('Ctrl Pts',(-7.86014551404695,-0.896205594465593,
2.39738452163096));
#69443=CARTESIAN_POINT('Ctrl Pts',(-7.85384577448809,-0.949428459081086,
2.39954968758841));
#69444=CARTESIAN_POINT('Ctrl Pts',(-7.85146101062526,-0.968951934492959,
2.40034290928089));
#69445=CARTESIAN_POINT('Ctrl Pts',(-7.84728274747829,-1.00212979760632,
2.4016891634594));
#69446=CARTESIAN_POINT('Ctrl Pts',(-7.84552636178184,-1.01578873700424,
2.40224290064964));
#69447=CARTESIAN_POINT('Ctrl Pts',(-7.84219237196741,-1.04119172589804,
2.4032718138032));
#69448=CARTESIAN_POINT('Ctrl Pts',(-7.84062403131142,-1.05293694474951,
2.40374716712783));
#69449=CARTESIAN_POINT('Ctrl Pts',(-7.83732090476096,-1.07725724708036,
2.40473069278164));
#69450=CARTESIAN_POINT('Ctrl Pts',(-7.8355822280402,-1.08983177115391,2.40523878776886));
#69451=CARTESIAN_POINT('Ctrl Pts',(-7.8315399552441,-1.1185566900726,2.40639849673642));
#69452=CARTESIAN_POINT('Ctrl Pts',(-7.82921665080356,-1.13470426845318,
2.40704972023831));
#69453=CARTESIAN_POINT('Ctrl Pts',(-7.82193230767062,-1.18424476577751,
2.40904551913824));
#69454=CARTESIAN_POINT('Ctrl Pts',(-7.81680743576341,-1.21761333199256,
2.41038681807528));
#69455=CARTESIAN_POINT('Ctrl Pts',(-7.77454789171875,-1.48150044693227,
2.42097083009402));
#69456=CARTESIAN_POINT('Ctrl Pts',(-7.7274369826424,-1.71031090341293,2.43000152228597));
#69457=CARTESIAN_POINT('Ctrl Pts',(-7.65363108968939,-2.00261644581014,
2.44141846896412));
#69458=CARTESIAN_POINT('Ctrl Pts',(-7.63614130903436,-2.06830547756909,
2.44397665093341));
#69459=CARTESIAN_POINT('Ctrl Pts',(-7.58519352139753,-2.25019572634655,
2.45104585456814));
#69460=CARTESIAN_POINT('Ctrl Pts',(-7.54991457310734,-2.3658681696567,2.45552489361593));
#69461=CARTESIAN_POINT('Ctrl Pts',(-7.30324896783043,-3.11281883083619,
2.48445052846274));
#69462=CARTESIAN_POINT('Ctrl Pts',(-7.01557423291366,-3.71599447268652,
2.50754428369342));
#69463=CARTESIAN_POINT('Ctrl Pts',(-6.62879385889571,-4.31804530076434,
2.53567959958025));
#69464=CARTESIAN_POINT('Ctrl Pts',(-6.6013581777931,-4.3598730826848,2.53766455655686));
#69465=CARTESIAN_POINT('Ctrl Pts',(-6.56729567507356,-4.41074528848481,
2.54011935719801));
#69466=CARTESIAN_POINT('Ctrl Pts',(-6.56104351334651,-4.42004010138089,
2.5405695473902));
#69467=CARTESIAN_POINT('Ctrl Pts',(-6.55122760858426,-4.43456625697984,
2.54127579131269));
#69468=CARTESIAN_POINT('Ctrl Pts',(-6.54767727673166,-4.43980667895011,
2.54153112095232));
#69469=CARTESIAN_POINT('Ctrl Pts',(-6.54138019229956,-4.4490774288657,2.54198379958337));
#69470=CARTESIAN_POINT('Ctrl Pts',(-6.5386359919988,-4.45310949250267,2.54218100851659));
#69471=CARTESIAN_POINT('Ctrl Pts',(-6.53279198570338,-4.46167906391326,
2.542600852415));
#69472=CARTESIAN_POINT('Ctrl Pts',(-6.52969117829312,-4.46621588301787,
2.5428235429785));
#69473=CARTESIAN_POINT('Ctrl Pts',(-6.52082061427943,-4.47916550060539,
2.54346039102214));
#69474=CARTESIAN_POINT('Ctrl Pts',(-6.5150393240681,-4.48757035262232,2.54387519790678));
#69475=CARTESIAN_POINT('Ctrl Pts',(-6.49003457069698,-4.52377215214289,
2.54566830743923));
#69476=CARTESIAN_POINT('Ctrl Pts',(-6.47064960212792,-4.55145657290654,
2.54705601557109));
#69477=CARTESIAN_POINT('Ctrl Pts',(-6.12238390190193,-5.04210618191876,
2.57195565846574));
#69478=CARTESIAN_POINT('Ctrl Pts',(-5.74479645450918,-5.46842162690606,
2.59831288653491));
#69479=CARTESIAN_POINT('Ctrl Pts',(-5.19479843158625,-5.96899708172098,
2.63260082061013));
#69480=CARTESIAN_POINT('Ctrl Pts',(-5.06080746830011,-6.08301622487178,
2.6406920219968));
#69481=CARTESIAN_POINT('Ctrl Pts',(-4.76965145577883,-6.31449031398618,
2.65763138149675));
#69482=CARTESIAN_POINT('Ctrl Pts',(-4.61168972765105,-6.43076090356348,
2.66645361315393));
#69483=CARTESIAN_POINT('Ctrl Pts',(-4.16858514620309,-6.73218410544912,
2.69010467797355));
#69484=CARTESIAN_POINT('Ctrl Pts',(-3.87556336288559,-6.90503073090581,
2.70455630689548));
#69485=CARTESIAN_POINT('Ctrl Pts',(-3.55156860830657,-7.06900429112808,
2.71928683854302));
#69486=CARTESIAN_POINT('Ctrl Pts',(-3.53078381537044,-7.07940865526012,
2.72022664447055));
#69487=CARTESIAN_POINT('Ctrl Pts',(-3.50030023416997,-7.09450035538991,
2.72159747573838));
#69488=CARTESIAN_POINT('Ctrl Pts',(-3.49063733640822,-7.09925968033115,
2.72203091100409));
#69489=CARTESIAN_POINT('Ctrl Pts',(-3.47362699271886,-7.10759476091169,
2.72279199413157));
#69490=CARTESIAN_POINT('Ctrl Pts',(-3.46628368133205,-7.1111788903741,2.72311992155211));
#69491=CARTESIAN_POINT('Ctrl Pts',(-3.4519892222961,-7.11812833914228,2.72375704314912));
#69492=CARTESIAN_POINT('Ctrl Pts',(-3.44503867496338,-7.12149486918206,
2.72406627749625));
#69493=CARTESIAN_POINT('Ctrl Pts',(-3.4283935381111,-7.12952694782317,2.72480549479299));
#69494=CARTESIAN_POINT('Ctrl Pts',(-3.41869432778078,-7.13418291370693,
2.72523515829234));
#69495=CARTESIAN_POINT('Ctrl Pts',(-3.38374378761735,-7.15087277340537,
2.72677954923168));
#69496=CARTESIAN_POINT('Ctrl Pts',(-3.35843804304892,-7.16279256800083,
2.72789048431469));
#69497=CARTESIAN_POINT('Ctrl Pts',(-2.94919511069632,-7.35291317448888,
2.74574083558877));
#69498=CARTESIAN_POINT('Ctrl Pts',(-2.55161309007714,-7.5001602409424,2.76139689896681));
#69499=CARTESIAN_POINT('Ctrl Pts',(-1.93604453840895,-7.67348566024924,
2.78411063902228));
#69500=CARTESIAN_POINT('Ctrl Pts',(-1.72564832041538,-7.72352195122062,
2.79162663923935));
#69501=CARTESIAN_POINT('Ctrl Pts',(-1.15139415152783,-7.83545070034438,
2.81184979276966));
#69502=CARTESIAN_POINT('Ctrl Pts',(-0.784841921303233,-7.88060937406926,
2.82443900279151));
#69503=CARTESIAN_POINT('Ctrl Pts',(-0.14942285776977,-7.91410873902272,
2.84721744480106));
#69504=CARTESIAN_POINT('Ctrl Pts',(0.118183083009651,-7.91463671372961,
2.8571117548681));
#69505=CARTESIAN_POINT('Ctrl Pts',(0.427350238322998,-7.8995610819512,2.86930421417937));
#69506=CARTESIAN_POINT('Ctrl Pts',(0.469383939686272,-7.89717494674567,
2.87097695038183));
#69507=CARTESIAN_POINT('Ctrl Pts',(0.523325906304419,-7.89368063168055,
2.87314133026004));
#69508=CARTESIAN_POINT('Ctrl Pts',(0.535253974643467,-7.89288078586238,
2.87362105059203));
#69509=CARTESIAN_POINT('Ctrl Pts',(0.55445036392076,-7.89154984170729,2.87439483770193));
#69510=CARTESIAN_POINT('Ctrl Pts',(0.561719870444779,-7.89103573030265,
2.87468826854016));
#69511=CARTESIAN_POINT('Ctrl Pts',(0.575550766760856,-7.89003837761832,
2.8752473048616));
#69512=CARTESIAN_POINT('Ctrl Pts',(0.58211228760229,-7.88955699451595,2.87551284199279));
#69513=CARTESIAN_POINT('Ctrl Pts',(0.597052117007533,-7.8884422015333,2.87611816805273));
#69514=CARTESIAN_POINT('Ctrl Pts',(0.605430025316074,-7.88780362846049,
2.87645814265024));
#69515=CARTESIAN_POINT('Ctrl Pts',(0.627126312571109,-7.88611514434115,
2.87733990274209));
#69516=CARTESIAN_POINT('Ctrl Pts',(0.640443050246937,-7.88504484315655,
2.87788240465538));
#69517=CARTESIAN_POINT('Ctrl Pts',(0.721412953104962,-7.87833060732248,
2.88118863598486));
#69518=CARTESIAN_POINT('Ctrl Pts',(0.788992885828264,-7.87184982946218,
2.88398058120636));
#69519=CARTESIAN_POINT('Ctrl Pts',(1.63904736994006,-7.77927502567528,2.91944875299837));
#69520=CARTESIAN_POINT('Ctrl Pts',(2.40455097742003,-7.57772491893492,2.95443807846174));
#69521=CARTESIAN_POINT('Ctrl Pts',(3.39534916642152,-7.15125324548186,2.99980583738341));
#69522=CARTESIAN_POINT('Ctrl Pts',(3.6564173292753,-7.02135588881491,3.01185295123205));
#69523=CARTESIAN_POINT('Ctrl Pts',(4.0943334926834,-6.77240329330084,3.03248126314873));
#69524=CARTESIAN_POINT('Ctrl Pts',(4.27464074163336,-6.66006471556015,3.04113002341403));
#69525=CARTESIAN_POINT('Ctrl Pts',(4.49076480480736,-6.51301455204948,3.05170349413296));
#69526=CARTESIAN_POINT('Ctrl Pts',(4.53106222637471,-6.48504450390937,3.05368393037118));
#69527=CARTESIAN_POINT('Ctrl Pts',(4.59426448330008,-6.44029972930029,3.05680433801208));
#69528=CARTESIAN_POINT('Ctrl Pts',(4.61734353629094,-6.42377345643984,3.0579468470729));
#69529=CARTESIAN_POINT('Ctrl Pts',(4.65979178282747,-6.39303048522686,3.06005391324991));
#69530=CARTESIAN_POINT('Ctrl Pts',(4.67918611056879,-6.37884908041973,3.06101883902535));
#69531=CARTESIAN_POINT('Ctrl Pts',(4.72298911172012,-6.34651244576885,3.06320325951784));
#69532=CARTESIAN_POINT('Ctrl Pts',(4.7473582963467,-6.32830432166698,3.06442214377139));
#69533=CARTESIAN_POINT('Ctrl Pts',(4.81667963656603,-6.27588316017457,3.06789992083251));
#69534=CARTESIAN_POINT('Ctrl Pts',(4.86137129216246,-6.24132849415861,3.07015477446153));
#69535=CARTESIAN_POINT('Ctrl Pts',(5.2359751824811,-5.94522762080542,3.08916682101756));
#69536=CARTESIAN_POINT('Ctrl Pts',(5.54489849507036,-5.65820485443976,3.10555008502351));
#69537=CARTESIAN_POINT('Ctrl Pts',(6.12811823599195,-5.02246891966692,3.13890647479704));
#69538=CARTESIAN_POINT('Ctrl Pts',(6.398926856496,-4.67255186088155,3.15581394655312));
#69539=CARTESIAN_POINT('Ctrl Pts',(6.66018457722227,-4.26935178765177,3.17489461780981));
#69540=CARTESIAN_POINT('Ctrl Pts',(6.68102188037722,-4.236669669806,3.17643881478327));
#69541=CARTESIAN_POINT('Ctrl Pts',(6.71670740825333,-4.17978096574632,3.17912396493538));
#69542=CARTESIAN_POINT('Ctrl Pts',(6.73166707402852,-4.15564504259226,3.18026232398707));
#69543=CARTESIAN_POINT('Ctrl Pts',(6.75387975371021,-4.11937242215445,3.18197230549185));
#69544=CARTESIAN_POINT('Ctrl Pts',(6.7612307551626,-4.10729589311127,3.18254149137813));
#69545=CARTESIAN_POINT('Ctrl Pts',(6.77420219959194,-4.08585667969533,3.18355179338039));
#69546=CARTESIAN_POINT('Ctrl Pts',(6.77983571035995,-4.07650193028374,3.18399257238239));
#69547=CARTESIAN_POINT('Ctrl Pts',(6.7907480937362,-4.05829613687344,3.18485032715158));
#69548=CARTESIAN_POINT('Ctrl Pts',(6.79602907689711,-4.04944638096903,3.18526724613924));
#69549=CARTESIAN_POINT('Ctrl Pts',(6.8086795705797,-4.0281525133272,3.18627037838236));
#69550=CARTESIAN_POINT('Ctrl Pts',(6.81603223810991,-4.01569853108739,3.1868570499081));
#69551=CARTESIAN_POINT('Ctrl Pts',(6.84526434029541,-3.96587347398827,3.18920411243838));
#69552=CARTESIAN_POINT('Ctrl Pts',(6.86687073859161,-3.92834348108647,3.19097178729382));
#69553=CARTESIAN_POINT('Ctrl Pts',(7.05554687711995,-3.59430243083595,3.20669557740396));
#69554=CARTESIAN_POINT('Ctrl Pts',(7.2036254157549,-3.28747981349787,3.22105585821392));
#69555=CARTESIAN_POINT('Ctrl Pts',(7.50810465608365,-2.53639610702728,3.25524742932266));
#69556=CARTESIAN_POINT('Ctrl Pts',(7.64554453932837,-2.08581413408517,3.27497262594183));
#69557=CARTESIAN_POINT('Ctrl Pts',(7.75433998029619,-1.56768772902354,3.29658720617295));
#69558=CARTESIAN_POINT('Ctrl Pts',(7.76586669750839,-1.50955220488174,3.29899875893063));
#69559=CARTESIAN_POINT('Ctrl Pts',(7.78299812064975,-1.41775360174582,3.30278608454479));
#69560=CARTESIAN_POINT('Ctrl Pts',(7.78904009666747,-1.38417463074033,3.30416712400916));
#69561=CARTESIAN_POINT('Ctrl Pts',(7.79891723108562,-1.32716785757236,3.30650461162907));
#69562=CARTESIAN_POINT('Ctrl Pts',(7.80286449363473,-1.30376002328595,3.30746239696744));
#69563=CARTESIAN_POINT('Ctrl Pts',(7.81038090660719,-1.25792948567564,3.30933380841486));
#69564=CARTESIAN_POINT('Ctrl Pts',(7.81395900206547,-1.23550848456939,3.31024753259054));
#69565=CARTESIAN_POINT('Ctrl Pts',(7.82071315614648,-1.19198247552003,3.31201796040784));
#69566=CARTESIAN_POINT('Ctrl Pts',(7.82390042775347,-1.17087940996271,3.31287478834747));
#69567=CARTESIAN_POINT('Ctrl Pts',(7.83110730764892,-1.1218186621085,3.31486327872281));
#69568=CARTESIAN_POINT('Ctrl Pts',(7.83506266749147,-1.09385180840138,3.31599418864444));
#69569=CARTESIAN_POINT('Ctrl Pts',(7.84523147749112,-1.01906558960532,3.31901166697977));
#69570=CARTESIAN_POINT('Ctrl Pts',(7.85117558632553,-0.972210655273763,
3.32089517302241));
#69571=CARTESIAN_POINT('Ctrl Pts',(7.89477883026822,-0.601978622556918,
3.3357275431221));
#69572=CARTESIAN_POINT('Ctrl Pts',(7.91286345269262,-0.276602854153996,
3.34847621657132));
#69573=CARTESIAN_POINT('Ctrl Pts',(7.91001956246774,0.182893264006606,3.36634124389311));
#69574=CARTESIAN_POINT('Ctrl Pts',(7.90578954108794,0.316783449614114,3.37152171445215));
#69575=CARTESIAN_POINT('Ctrl Pts',(7.86686859743088,0.999140972472912,3.39780256674687));
#69576=CARTESIAN_POINT('Ctrl Pts',(7.77849572381311,1.54302082852759,3.41820712580402));
#69577=CARTESIAN_POINT('Ctrl Pts',(7.54549753889202,2.40096629918483,3.4515399777985));
#69578=CARTESIAN_POINT('Ctrl Pts',(7.43553052472111,2.72250565524463,3.46434922331243));
#69579=CARTESIAN_POINT('Ctrl Pts',(7.29351948429944,3.06421773268418,3.47898153986713));
#69580=CARTESIAN_POINT('Ctrl Pts',(7.28161621806224,3.09239745321008,3.48019613629088));
#69581=CARTESIAN_POINT('Ctrl Pts',(7.26065538980941,3.14122790785675,3.48231552431692));
#69582=CARTESIAN_POINT('Ctrl Pts',(7.25167238465197,3.16191035188239,3.48321781660625));
#69583=CARTESIAN_POINT('Ctrl Pts',(7.23857690169577,3.19171200169049,3.48452492194868));
#69584=CARTESIAN_POINT('Ctrl Pts',(7.23453532058555,3.20086234594562,3.48492721076003));
#69585=CARTESIAN_POINT('Ctrl Pts',(7.22746816379373,3.21678098495243,3.48562875691541));
#69586=CARTESIAN_POINT('Ctrl Pts',(7.22445040397407,3.22355274874229,3.48592772833631));
#69587=CARTESIAN_POINT('Ctrl Pts',(7.21861380171799,3.23660054937353,3.48650483155131));
#69588=CARTESIAN_POINT('Ctrl Pts',(7.21579628196911,3.24287717178979,3.48678291385445));
#69589=CARTESIAN_POINT('Ctrl Pts',(7.20911473914521,3.2577099035395,3.48744119121204));
#69590=CARTESIAN_POINT('Ctrl Pts',(7.20524367080158,3.26626281570605,3.48782165341119));
#69591=CARTESIAN_POINT('Ctrl Pts',(7.19167390179325,3.29610295677496,3.48915218547146));
#69592=CARTESIAN_POINT('Ctrl Pts',(7.18189606841672,3.31735392435872,3.49010532991368));
#69593=CARTESIAN_POINT('Ctrl Pts',(7.01714768936195,3.67127267413449,3.50607684616359));
#69594=CARTESIAN_POINT('Ctrl Pts',(6.83934332957474,3.99272791060968,3.52225070098082));
#69595=CARTESIAN_POINT('Ctrl Pts',(6.35551397120063,4.73973229419203,3.56259390955272));
#69596=CARTESIAN_POINT('Ctrl Pts',(6.02822946432228,5.14957519898245,3.58694305838343));
#69597=CARTESIAN_POINT('Ctrl Pts',(5.40996110519929,5.78337530592687,3.62617854477727));
#69598=CARTESIAN_POINT('Ctrl Pts',(5.13952089636872,6.02498777118756,3.6416487917214));
#69599=CARTESIAN_POINT('Ctrl Pts',(4.83367092808728,6.26260118485098,3.65735972996765));
#69600=CARTESIAN_POINT('Ctrl Pts',(4.81382034473135,6.27787240591909,3.65837201047308));
#69601=CARTESIAN_POINT('Ctrl Pts',(4.78523467972665,6.29964829588114,3.65981919486222));
#69602=CARTESIAN_POINT('Ctrl Pts',(4.77655826305,6.30622951951161,3.66025706519359));
#69603=CARTESIAN_POINT('Ctrl Pts',(4.76149894632268,6.31760338212437,3.66101467053474));
#69604=CARTESIAN_POINT('Ctrl Pts',(4.75512234191113,6.32240430719077,3.66133472583254));
#69605=CARTESIAN_POINT('Ctrl Pts',(4.74286348276394,6.33160492621358,3.6619486082152));
#69606=CARTESIAN_POINT('Ctrl Pts',(4.73698234716823,6.3360060922281,3.66224249198448));
#69607=CARTESIAN_POINT('Ctrl Pts',(4.72313814712758,6.34633639257582,3.66293283218992));
#69608=CARTESIAN_POINT('Ctrl Pts',(4.71517002566562,6.35225874745336,3.66332902717017));
#69609=CARTESIAN_POINT('Ctrl Pts',(4.6877075603652,6.37259024883434,3.66469063914138));
#69610=CARTESIAN_POINT('Ctrl Pts',(4.66815805874853,6.38692484712394,3.66565318897203));
#69611=CARTESIAN_POINT('Ctrl Pts',(4.45010041231214,6.54527877384177,3.67631554406752));
#69612=CARTESIAN_POINT('Ctrl Pts',(4.24505636357455,6.68008807100873,3.68565616258135));
#69613=CARTESIAN_POINT('Ctrl Pts',(3.91670519074361,6.87473314761765,3.69971916906134));
#69614=CARTESIAN_POINT('Ctrl Pts',(3.79755961984533,6.9412591075866,3.70465048431178));
#69615=CARTESIAN_POINT('Ctrl Pts',(3.1580822444697,7.27692060455967,3.730353911298));
#69616=CARTESIAN_POINT('Ctrl Pts',(2.61081017483483,7.49070724770031,3.74958215182077));
#69617=CARTESIAN_POINT('Ctrl Pts',(1.85476871750775,7.69301762122654,3.77688909637846));
#69618=CARTESIAN_POINT('Ctrl Pts',(1.6627428849949,7.73679307335058,3.78390077453241));
#69619=CARTESIAN_POINT('Ctrl Pts',(1.35524022414728,7.79491614191002,3.79549970454625));
#69620=CARTESIAN_POINT('Ctrl Pts',(1.24073119804129,7.81396044405406,3.79989968273087));
#69621=CARTESIAN_POINT('Ctrl Pts',(1.06962068979217,7.83856234077358,3.80664443465385));
#69622=CARTESIAN_POINT('Ctrl Pts',(1.01330811241883,7.84604068105439,3.80889137889274));
#69623=CARTESIAN_POINT('Ctrl Pts',(0.947221135914901,7.85409374831722,3.81156486221682));
#69624=CARTESIAN_POINT('Ctrl Pts',(0.937518966538457,7.85525777256611,3.81195827497018));
#69625=CARTESIAN_POINT('Ctrl Pts',(0.922689783331571,7.85700904892436,3.81256102073576));
#69626=CARTESIAN_POINT('Ctrl Pts',(0.917564281063219,7.85760926879306,3.81276961387849));
#69627=CARTESIAN_POINT('Ctrl Pts',(0.908643596861281,7.85864507450734,3.81313312171755));
#69628=CARTESIAN_POINT('Ctrl Pts',(0.904848674809405,7.85908292797527,3.81328790590078));
#69629=CARTESIAN_POINT('Ctrl Pts',(0.896932264124252,7.85999050386975,3.81361109973172));
#69630=CARTESIAN_POINT('Ctrl Pts',(0.892810721160892,7.86045973359108,3.81377953785291));
#69631=CARTESIAN_POINT('Ctrl Pts',(0.882719046163696,7.86160061178409,3.8141923885795));
#69632=CARTESIAN_POINT('Ctrl Pts',(0.876748523155292,7.86226870059873,3.81443700851683));
#69633=CARTESIAN_POINT('Ctrl Pts',(0.853447245596857,7.86484919192799,3.81539313651795));
#69634=CARTESIAN_POINT('Ctrl Pts',(0.836111262273416,7.86671106313678,3.81610763240073));
#69635=CARTESIAN_POINT('Ctrl Pts',(0.528966353275871,7.89867145949238,3.82882045732331));
#69636=CARTESIAN_POINT('Ctrl Pts',(0.237742187972288,7.91279119943711,3.84171714842958));
#69637=CARTESIAN_POINT('Ctrl Pts',(-0.560954793583377,7.90738293822852,
3.87808166650427));
#69638=CARTESIAN_POINT('Ctrl Pts',(-1.06684049781057,7.85514270765737,3.90213283668487));
#69639=CARTESIAN_POINT('Ctrl Pts',(-1.84139764805392,7.69890288191097,3.93796218045429));
#69640=CARTESIAN_POINT('Ctrl Pts',(-2.11535357974377,7.62818138055529,3.95045526521643));
#69641=CARTESIAN_POINT('Ctrl Pts',(-2.49314758242171,7.50872906595663,3.96728829589015));
#69642=CARTESIAN_POINT('Ctrl Pts',(-2.60059523152472,7.47219532704595,3.97203117891056));
#69643=CARTESIAN_POINT('Ctrl Pts',(-2.76672409838413,7.41169135421003,3.97929440108609));
#69644=CARTESIAN_POINT('Ctrl Pts',(-2.82596367574222,7.38930717540576,3.9818703630484));
#69645=CARTESIAN_POINT('Ctrl Pts',(-2.89852969435713,7.36088717201735,3.98500910521081));
#69646=CARTESIAN_POINT('Ctrl Pts',(-2.91211554745962,7.35552291748696,3.98559601842834));
#69647=CARTESIAN_POINT('Ctrl Pts',(-2.93341837757752,7.34704341048817,3.98651518390495));
#69648=CARTESIAN_POINT('Ctrl Pts',(-2.94114539283368,7.34395356959053,3.98684835329543));
#69649=CARTESIAN_POINT('Ctrl Pts',(-2.95484863078439,7.33844889028748,3.98743879252541));
#69650=CARTESIAN_POINT('Ctrl Pts',(-2.96082679824562,7.33603893237216,3.98769623861385));
#69651=CARTESIAN_POINT('Ctrl Pts',(-2.97459135014448,7.33047051034533,3.98828868307784));
#69652=CARTESIAN_POINT('Ctrl Pts',(-2.98237566784237,7.3273069391053,3.98862349606506));
#69653=CARTESIAN_POINT('Ctrl Pts',(-3.00364808128175,7.31862224837698,3.98953781295383));
#69654=CARTESIAN_POINT('Ctrl Pts',(-3.01712601561208,7.31307623505106,3.99011641295266));
#69655=CARTESIAN_POINT('Ctrl Pts',(-3.08237844998437,7.28601452129017,3.99291432300602));
#69656=CARTESIAN_POINT('Ctrl Pts',(-3.13393918473677,7.26398581181785,3.99511493160931));
#69657=CARTESIAN_POINT('Ctrl Pts',(-3.28196079343056,7.1988758967759,4.00140515101398));
#69658=CARTESIAN_POINT('Ctrl Pts',(-3.37779989801451,7.1544077162641,4.00544389789004));
#69659=CARTESIAN_POINT('Ctrl Pts',(-4.15028569256747,6.77699967275721,4.03777872328744));
#69660=CARTESIAN_POINT('Ctrl Pts',(-4.77695807943907,6.350841928595,4.06211737850159));
#69661=CARTESIAN_POINT('Ctrl Pts',(-5.48188780997847,5.70727705391847,4.09501733817585));
#69662=CARTESIAN_POINT('Ctrl Pts',(-5.62473551899532,5.56654732875783,4.10206445045347));
#69663=CARTESIAN_POINT('Ctrl Pts',(-5.87231430093308,5.30336961937923,4.11531729681671));
#69664=CARTESIAN_POINT('Ctrl Pts',(-5.97894410927416,5.18285886469941,4.12141195755589));
#69665=CARTESIAN_POINT('Ctrl Pts',(-6.09782029081979,5.03995383940207,4.1287843580056));
#69666=CARTESIAN_POINT('Ctrl Pts',(-6.11372941587572,5.02064334560323,4.12978354440819));
#69667=CARTESIAN_POINT('Ctrl Pts',(-6.13408375182362,4.99569705203258,4.13107864072407));
#69668=CARTESIAN_POINT('Ctrl Pts',(-6.1386134300646,4.9901300249205,4.13136792868201));
#69669=CARTESIAN_POINT('Ctrl Pts',(-6.14592138157936,4.98112345969848,4.13183640693174));
#69670=CARTESIAN_POINT('Ctrl Pts',(-6.14870436679462,4.9776877321599,4.13201522404845));
#69671=CARTESIAN_POINT('Ctrl Pts',(-6.15403751286836,4.97109241280141,4.13235868854814));
#69672=CARTESIAN_POINT('Ctrl Pts',(-6.15658812591725,4.96793318534904,4.13252330045944));
#69673=CARTESIAN_POINT('Ctrl Pts',(-6.16239561906418,4.96072859632745,4.13289889576014));
#69674=CARTESIAN_POINT('Ctrl Pts',(-6.16565094701837,4.95668199217514,4.13310999953099));
#69675=CARTESIAN_POINT('Ctrl Pts',(-6.17576442127482,4.94408484545787,4.13376760538043));
#69676=CARTESIAN_POINT('Ctrl Pts',(-6.18260875644006,4.93552328619168,4.13421516667474));
#69677=CARTESIAN_POINT('Ctrl Pts',(-6.23458928152608,4.87022320149393,4.13763332837882));
#69678=CARTESIAN_POINT('Ctrl Pts',(-6.27896000081939,4.81288252428012,4.14066097469018));
#69679=CARTESIAN_POINT('Ctrl Pts',(-6.42172617847592,4.62304968210538,4.15074557537173));
#69680=CARTESIAN_POINT('Ctrl Pts',(-6.51676080179441,4.48809291980044,4.15801036155191));
#69681=CARTESIAN_POINT('Ctrl Pts',(-6.65584212091184,4.27684636632203,4.16940102319782));
#69682=CARTESIAN_POINT('Ctrl Pts',(-6.70295579040209,4.20262206405166,4.17340685674299));
#69683=CARTESIAN_POINT('Ctrl Pts',(-7.06433040015784,3.61176169014668,4.20523372057327));
#69684=CARTESIAN_POINT('Ctrl Pts',(-7.31966226481008,3.0614092505138,4.23432343874945));
#69685=CARTESIAN_POINT('Ctrl Pts',(-7.57006758041437,2.30536906055945,4.27035471830639));
#69686=CARTESIAN_POINT('Ctrl Pts',(-7.62369492804355,2.12130426988319,4.27885786594408));
#69687=CARTESIAN_POINT('Ctrl Pts',(-7.72172097485857,1.73280983378444,4.29619840651706));
#69688=CARTESIAN_POINT('Ctrl Pts',(-7.76480657157006,1.52819923012435,4.30498895881389));
#69689=CARTESIAN_POINT('Ctrl Pts',(-7.80615474789803,1.28426722346424,4.31507579345122));
#69690=CARTESIAN_POINT('Ctrl Pts',(-7.81229398093943,1.24637757565016,4.31663156101586));
#69691=CARTESIAN_POINT('Ctrl Pts',(-7.82007779944335,1.19601934785357,4.31868495208943));
#69692=CARTESIAN_POINT('Ctrl Pts',(-7.82196870671538,1.18358971899486,4.31919062124964));
#69693=CARTESIAN_POINT('Ctrl Pts',(-7.82502694811659,1.16315933311269,4.32001989338746));
#69694=CARTESIAN_POINT('Ctrl Pts',(-7.82621165830959,1.1551612237325,4.32034406262532));
#69695=CARTESIAN_POINT('Ctrl Pts',(-7.82848502417897,1.13964944876765,4.32097184944036));
#69696=CARTESIAN_POINT('Ctrl Pts',(-7.8295751291473,1.13213600655403,4.3212755138998));
#69697=CARTESIAN_POINT('Ctrl Pts',(-7.83206894597459,1.11477174082932,4.32197635227435));
#69698=CARTESIAN_POINT('Ctrl Pts',(-7.83346489322489,1.10491980533502,4.32237327340145));
#69699=CARTESIAN_POINT('Ctrl Pts',(-7.83788198838691,1.07331689932008,4.32364424171172));
#69700=CARTESIAN_POINT('Ctrl Pts',(-7.8408311715568,1.05155588514363,4.32451595357579));
#69701=CARTESIAN_POINT('Ctrl Pts',(-7.86672410431421,0.854333578555812,
4.332385623939));
#69702=CARTESIAN_POINT('Ctrl Pts',(-7.88386606828014,0.67815533263219,4.33919367111561));
#69703=CARTESIAN_POINT('Ctrl Pts',(-7.90579533365887,0.332953684635162,
4.35217546162546));
#69704=CARTESIAN_POINT('Ctrl Pts',(-7.91110266801687,0.164060522392913,
4.3583607118558));
#69705=CARTESIAN_POINT('Ctrl Pts',(-7.91074839564088,-0.410472873522453,
4.37900619817625));
#69706=CARTESIAN_POINT('Ctrl Pts',(-7.87930631962955,-0.815455084703749,
4.39285851388627));
#69707=CARTESIAN_POINT('Ctrl Pts',(-7.74419887009957,-1.68381264150579,
4.42327619276572));
#69708=CARTESIAN_POINT('Ctrl Pts',(-7.62964143285399,-2.14392825483457,
4.43989634087291));
#69709=CARTESIAN_POINT('Ctrl Pts',(-7.46527634657199,-2.6180888647318,4.45980631812643));
#69710=CARTESIAN_POINT('Ctrl Pts',(-7.45575524147669,-2.64508109214738,
4.46094852808306));
#69711=CARTESIAN_POINT('Ctrl Pts',(-7.44201401661616,-2.68337359665407,
4.46258097425397));
#69712=CARTESIAN_POINT('Ctrl Pts',(-7.43791413720657,-2.69471701077335,
4.46306606348556));
#69713=CARTESIAN_POINT('Ctrl Pts',(-7.43133644876903,-2.71278656834385,
4.46384115545806));
#69714=CARTESIAN_POINT('Ctrl Pts',(-7.428875402385,-2.71951882427602,4.46413045957101));
#69715=CARTESIAN_POINT('Ctrl Pts',(-7.42443488239403,-2.73161497411448,
4.46465119934292));
#69716=CARTESIAN_POINT('Ctrl Pts',(-7.42245873525908,-2.73698008996829,
4.4648824985253));
#69717=CARTESIAN_POINT('Ctrl Pts',(-7.41782130634378,-2.74952845935181,
4.46542424765462));
#69718=CARTESIAN_POINT('Ctrl Pts',(-7.41515540646165,-2.75670999184286,
4.46573488431364));
#69719=CARTESIAN_POINT('Ctrl Pts',(-7.40748146960362,-2.77729074771746,
4.46662677539982));
#69720=CARTESIAN_POINT('Ctrl Pts',(-7.40244752962748,-2.79068023744827,
4.46720905898022));
#69721=CARTESIAN_POINT('Ctrl Pts',(-7.36940067298264,-2.87786111852038,
4.4710133907859));
#69722=CARTESIAN_POINT('Ctrl Pts',(-7.34032157618289,-2.95124203637413,
4.4742762891005));
#69723=CARTESIAN_POINT('Ctrl Pts',(-7.24418216528634,-3.18363392541702,
4.48478263843739));
#69724=CARTESIAN_POINT('Ctrl Pts',(-7.17301626018948,-3.34088827172534,
4.49215241876972));
#69725=CARTESIAN_POINT('Ctrl Pts',(-6.78413671106209,-4.13037251404046,
4.5301734889989));
#69726=CARTESIAN_POINT('Ctrl Pts',(-6.3877302182522,-4.72033205108303,4.56166780993951));
#69727=CARTESIAN_POINT('Ctrl Pts',(-5.77330113470282,-5.41300017162005,
4.60047854676485));
#69728=CARTESIAN_POINT('Ctrl Pts',(-5.62173591794911,-5.57024844453724,
4.60946947752466));
#69729=CARTESIAN_POINT('Ctrl Pts',(-5.43682942528658,-5.74684291485599,
4.61982008260452));
#69730=CARTESIAN_POINT('Ctrl Pts',(-5.40961998548378,-5.77246302107295,
4.62132849454857));
#69731=CARTESIAN_POINT('Ctrl Pts',(-5.36907920851549,-5.81009736821291,
4.62355441143365));
#69732=CARTESIAN_POINT('Ctrl Pts',(-5.35588694928053,-5.82226055454719,
4.62427540043048));
#69733=CARTESIAN_POINT('Ctrl Pts',(-5.3324179890581,-5.84375153492287,4.62555212364906));
#69734=CARTESIAN_POINT('Ctrl Pts',(-5.32215792297588,-5.85309735578473,
4.62610828829591));
#69735=CARTESIAN_POINT('Ctrl Pts',(-5.30059161979503,-5.87263835511359,
4.62727316623914));
#69736=CARTESIAN_POINT('Ctrl Pts',(-5.28928043528483,-5.88282799753943,
4.62788174433197));
#69737=CARTESIAN_POINT('Ctrl Pts',(-5.25954296079113,-5.90946180096811,
4.629475486206));
#69738=CARTESIAN_POINT('Ctrl Pts',(-5.24106892020545,-5.9258524716276,4.63045934234861));
#69739=CARTESIAN_POINT('Ctrl Pts',(-5.15835423109427,-5.99854981454305,
4.63483674545658));
#69740=CARTESIAN_POINT('Ctrl Pts',(-5.09328018615468,-6.05390085373992,
4.63820656783975));
#69741=CARTESIAN_POINT('Ctrl Pts',(-4.45247477792675,-6.58131340308698,
4.67069153614563));
#69742=CARTESIAN_POINT('Ctrl Pts',(-3.81376255761221,-6.97089665206033,
4.69714850013192));
#69743=CARTESIAN_POINT('Ctrl Pts',(-2.84025291126275,-7.39029335677249,
4.73610917112075));
#69744=CARTESIAN_POINT('Ctrl Pts',(-2.54328992862581,-7.49767448158712,
4.74791489070535));
#69745=CARTESIAN_POINT('Ctrl Pts',(-2.22289051899876,-7.59230036683773,
4.76124404717879));
#69746=CARTESIAN_POINT('Ctrl Pts',(-2.20502967632595,-7.59750690937414,
4.76198903270666));
#69747=CARTESIAN_POINT('Ctrl Pts',(-2.18014531588567,-7.60466570857732,
4.7630298759672));
#69748=CARTESIAN_POINT('Ctrl Pts',(-2.17313712339672,-7.60667136006428,
4.76332332897935));
#69749=CARTESIAN_POINT('Ctrl Pts',(-2.16104972016486,-7.61011254622313,
4.76383002930704));
#69750=CARTESIAN_POINT('Ctrl Pts',(-2.15597181943808,-7.61155269132217,
4.76404306552176));
#69751=CARTESIAN_POINT('Ctrl Pts',(-2.14547728904073,-7.61451770418703,
4.76448371122279));
#69752=CARTESIAN_POINT('Ctrl Pts',(-2.1400604677349,-7.61604187615527,4.76471135271007));
#69753=CARTESIAN_POINT('Ctrl Pts',(-2.12742715727273,-7.61958206417113,
4.76524274044985));
#69754=CARTESIAN_POINT('Ctrl Pts',(-2.12020942934569,-7.6215936074593,4.76554669586726));
#69755=CARTESIAN_POINT('Ctrl Pts',(-2.09712116476968,-7.6279928517625,4.76652017849778));
#69756=CARTESIAN_POINT('Ctrl Pts',(-2.08123985773627,-7.63234123807238,
4.76719157448971));
#69757=CARTESIAN_POINT('Ctrl Pts',(-1.73261972908868,-7.72662627781598,
4.78197110650287));
#69758=CARTESIAN_POINT('Ctrl Pts',(-1.39441808818264,-7.79475795519613,
4.79720071794645));
#69759=CARTESIAN_POINT('Ctrl Pts',(-0.139062961115238,-7.96333819606989,
4.8546936661156));
#69760=CARTESIAN_POINT('Ctrl Pts',(0.789506630207529,-7.92536897953664,
4.89811185553703));
#69761=CARTESIAN_POINT('Ctrl Pts',(1.74228601220451,-7.71693961788635,4.93812188301683));
#69762=CARTESIAN_POINT('Ctrl Pts',(1.7938333232978,-7.70512035978467,4.94027548742045));
#69763=CARTESIAN_POINT('Ctrl Pts',(1.86040006586186,-7.68915307695565,4.94304273199312));
#69764=CARTESIAN_POINT('Ctrl Pts',(1.87553054069765,-7.68547647451182,4.94367079124955));
#69765=CARTESIAN_POINT('Ctrl Pts',(1.89958692028265,-7.67955566662255,4.94466789870903));
#69766=CARTESIAN_POINT('Ctrl Pts',(1.90851989756494,-7.67734052297875,4.94503783840902));
#69767=CARTESIAN_POINT('Ctrl Pts',(1.92454564794662,-7.67333685918713,4.94570093737707));
#69768=CARTESIAN_POINT('Ctrl Pts',(1.93163983721816,-7.67155408279231,4.94599427276674));
#69769=CARTESIAN_POINT('Ctrl Pts',(1.94819637669238,-7.66736898711918,4.94667839624049));
#69770=CARTESIAN_POINT('Ctrl Pts',(1.95765678214055,-7.66495898429893,4.94706894741789));
#69771=CARTESIAN_POINT('Ctrl Pts',(1.98465771530557,-7.65802734827585,4.94818260874155));
#69772=CARTESIAN_POINT('Ctrl Pts',(2.00218725630916,-7.65346296194613,4.9489044008849));
#69773=CARTESIAN_POINT('Ctrl Pts',(2.11347435530932,-7.62407723592029,4.9534791217359));
#69774=CARTESIAN_POINT('Ctrl Pts',(2.20678620744848,-7.59759323582987,4.95728042920969));
#69775=CARTESIAN_POINT('Ctrl Pts',(2.48212956667434,-7.51394370660503,4.96840754023745));
#69776=CARTESIAN_POINT('Ctrl Pts',(2.662609237899,-7.45190139793182,4.9755818999431));
#69777=CARTESIAN_POINT('Ctrl Pts',(3.09726108354482,-7.28467403485139,4.99269328139777));
#69778=CARTESIAN_POINT('Ctrl Pts',(3.34853240814211,-7.17264539450853,5.00243780354241));
#69779=CARTESIAN_POINT('Ctrl Pts',(4.24356083883718,-6.71629375586315,5.03747526303579));
#69780=CARTESIAN_POINT('Ctrl Pts',(4.84463319251512,-6.29649356921655,5.0614962856532));
#69781=CARTESIAN_POINT('Ctrl Pts',(5.41042146742667,-5.7717438363351,5.09188247036127));
#69782=CARTESIAN_POINT('Ctrl Pts',(5.44100778586675,-5.74291925339349,5.09355171564732));
#69783=CARTESIAN_POINT('Ctrl Pts',(5.48040985294967,-5.70518937025563,5.09573521223236));
#69784=CARTESIAN_POINT('Ctrl Pts',(5.48943652183164,-5.69650459293307,5.0962377173195));
#69785=CARTESIAN_POINT('Ctrl Pts',(5.50379088947734,-5.68262810525776,5.09704040874343));
#69786=CARTESIAN_POINT('Ctrl Pts',(5.5091319795083,-5.6774502348903,5.09733987891205));
#69787=CARTESIAN_POINT('Ctrl Pts',(5.5191472233807,-5.66771360926592,5.09790291298832));
#69788=CARTESIAN_POINT('Ctrl Pts',(5.52382305509085,-5.6631565831918,5.09816638896673));
#69789=CARTESIAN_POINT('Ctrl Pts',(5.53437447764849,-5.65284775551494,5.09876231842716));
#69790=CARTESIAN_POINT('Ctrl Pts',(5.54024674906531,-5.64709257625073,5.09909494088358));
#69791=CARTESIAN_POINT('Ctrl Pts',(5.55762765089376,-5.63000504130767,5.1000822835887));
#69792=CARTESIAN_POINT('Ctrl Pts',(5.56911052508693,-5.6186466187212,5.1007382818236));
#69793=CARTESIAN_POINT('Ctrl Pts',(5.66215685978641,-5.52604325342921,5.10608349094295));
#69794=CARTESIAN_POINT('Ctrl Pts',(5.74197095106509,-5.44306371720488,5.11085401342704));
#69795=CARTESIAN_POINT('Ctrl Pts',(6.04915225041551,-5.10942188123228,5.12987305247875));
#69796=CARTESIAN_POINT('Ctrl Pts',(6.26214694578054,-4.84602337905215,5.14451897909836));
#69797=CARTESIAN_POINT('Ctrl Pts',(6.7636711562799,-4.13731648081782,5.18202184418714));
#69798=CARTESIAN_POINT('Ctrl Pts',(7.02551888685204,-3.67515602344842,5.20464840308578));
#69799=CARTESIAN_POINT('Ctrl Pts',(7.31864840013873,-3.0100029401262,5.23478538434852));
#69800=CARTESIAN_POINT('Ctrl Pts',(7.39133397209335,-2.82682084189524,5.24287017474098));
#69801=CARTESIAN_POINT('Ctrl Pts',(7.51671099857692,-2.47282258723944,5.25820774134906));
#69802=CARTESIAN_POINT('Ctrl Pts',(7.57060228220667,-2.30255904770196,5.26547125232975));
#69803=CARTESIAN_POINT('Ctrl Pts',(7.63165973204635,-2.08422908957248,5.27463824237077));
#69804=CARTESIAN_POINT('Ctrl Pts',(7.6442086187375,-2.03772318632278,5.27658253525373));
#69805=CARTESIAN_POINT('Ctrl Pts',(7.66364703086753,-1.96297730195073,5.27969418683678));
#69806=CARTESIAN_POINT('Ctrl Pts',(7.67080698517684,-1.93480900974373,5.28086381816623));
#69807=CARTESIAN_POINT('Ctrl Pts',(7.68414892181248,-1.88108154932852,5.28308906408046));
#69808=CARTESIAN_POINT('Ctrl Pts',(7.69035901209496,-1.85552976740456,5.28414491299281));
#69809=CARTESIAN_POINT('Ctrl Pts',(7.70428922004837,-1.7969417288493,5.28656036385985));
#69810=CARTESIAN_POINT('Ctrl Pts',(7.71192446116997,-1.76388578961946,5.28791917680736));
#69811=CARTESIAN_POINT('Ctrl Pts',(7.73505880636972,-1.66070580088093,5.2921482787337));
#69812=CARTESIAN_POINT('Ctrl Pts',(7.749815892315,-1.59041888584172,5.29501154222261));
#69813=CARTESIAN_POINT('Ctrl Pts',(7.81668704688395,-1.2488516680876,5.30884517877739));
#69814=CARTESIAN_POINT('Ctrl Pts',(7.85552568122707,-0.975165635290019,
5.31967730011351));
#69815=CARTESIAN_POINT('Ctrl Pts',(7.91131647906015,-0.347127784117426,
5.34420503526885));
#69816=CARTESIAN_POINT('Ctrl Pts',(7.9189247760439,0.00745533517541197,
5.35781155369968));
#69817=CARTESIAN_POINT('Ctrl Pts',(7.89153099412876,0.606556623570824,5.38109845982058));
#69818=CARTESIAN_POINT('Ctrl Pts',(7.86891303796264,0.851101749908046,5.39069342226176));
#69819=CARTESIAN_POINT('Ctrl Pts',(7.83102340598378,1.12241044308791,5.40164958931195));
#69820=CARTESIAN_POINT('Ctrl Pts',(7.82693021591501,1.15060686984834,5.40279205113136));
#69821=CARTESIAN_POINT('Ctrl Pts',(7.82057075989004,1.19280982656045,5.40450823146574));
#69822=CARTESIAN_POINT('Ctrl Pts',(7.81841897574612,1.20683346432946,5.40507952936244));
#69823=CARTESIAN_POINT('Ctrl Pts',(7.81452906453894,1.23173775941384,5.40609598372799));
#69824=CARTESIAN_POINT('Ctrl Pts',(7.81280590639158,1.24262072920156,5.40654081045102));
#69825=CARTESIAN_POINT('Ctrl Pts',(7.80913871762963,1.26547244881944,5.40747623797684));
#69826=CARTESIAN_POINT('Ctrl Pts',(7.80718989539551,1.27744039622054,5.40796694606765));
#69827=CARTESIAN_POINT('Ctrl Pts',(7.80192180217572,1.30933001295187,5.40927669168564));
#69828=CARTESIAN_POINT('Ctrl Pts',(7.79855377105532,1.32924337940081,5.4100968918124));
#69829=CARTESIAN_POINT('Ctrl Pts',(7.77912988947296,1.44147108001134,5.41473238358788));
#69830=CARTESIAN_POINT('Ctrl Pts',(7.76151139590888,1.53350613787863,5.41858307090073));
#69831=CARTESIAN_POINT('Ctrl Pts',(7.59421099140825,2.3305031632011,5.45228414745399));
#69832=CARTESIAN_POINT('Ctrl Pts',(7.35047704466483,3.01228631617945,5.48319147548354));
#69833=CARTESIAN_POINT('Ctrl Pts',(6.96719498926358,3.74888385590859,5.5172037358831));
#69834=CARTESIAN_POINT('Ctrl Pts',(6.91458227867885,3.84506028301337,5.5216662472084));
#69835=CARTESIAN_POINT('Ctrl Pts',(6.84156086658007,3.9721951987542,5.5275989093398));
#69836=CARTESIAN_POINT('Ctrl Pts',(6.82290936848958,4.00414754422264,5.52909286787867));
#69837=CARTESIAN_POINT('Ctrl Pts',(6.79325287620942,4.05414392504598,5.53143540538389));
#69838=CARTESIAN_POINT('Ctrl Pts',(6.7823985932055,4.07227662755972,5.53228602304595));
#69839=CARTESIAN_POINT('Ctrl Pts',(6.76135490576954,4.10711379062192,5.53392231565219));
#69840=CARTESIAN_POINT('Ctrl Pts',(6.75117593148488,4.1238243652781,5.53470812495331));
#69841=CARTESIAN_POINT('Ctrl Pts',(6.72695763458914,4.16325295683886,5.536564498572));
#69842=CARTESIAN_POINT('Ctrl Pts',(6.7128650506098,4.18593800945797,5.53763433592764));
#69843=CARTESIAN_POINT('Ctrl Pts',(6.6709384789533,4.25267160409983,5.54078707604022));
#69844=CARTESIAN_POINT('Ctrl Pts',(6.64278379238153,4.29651713555425,5.54286567926148));
#69845=CARTESIAN_POINT('Ctrl Pts',(6.38996135009806,4.6818135086468,5.56120248707517));
#69846=CARTESIAN_POINT('Ctrl Pts',(6.1395688481963,5.00566609815102,5.57716985458573));
#69847=CARTESIAN_POINT('Ctrl Pts',(5.43621167111037,5.78276201186043,5.61766462165159));
#69848=CARTESIAN_POINT('Ctrl Pts',(4.9512693118493,6.20303670041,5.64133322261512));
#69849=CARTESIAN_POINT('Ctrl Pts',(4.20769704034764,6.7041328506683,5.67502867288368));
#69850=CARTESIAN_POINT('Ctrl Pts',(3.98746554895735,6.83741339066503,5.68477307302276));
#69851=CARTESIAN_POINT('Ctrl Pts',(3.70277068015722,6.99126686776119,5.69741633349765));
#69852=CARTESIAN_POINT('Ctrl Pts',(3.64400662985024,7.02207509011529,5.70002878484663));
#69853=CARTESIAN_POINT('Ctrl Pts',(3.55780442068837,7.06589485180721,5.70387265113061));
#69854=CARTESIAN_POINT('Ctrl Pts',(3.53066724667832,7.0794937050405,5.70508439183675));
#69855=CARTESIAN_POINT('Ctrl Pts',(3.49321144664688,7.09799445339141,5.70675987416452));
#69856=CARTESIAN_POINT('Ctrl Pts',(3.48295929886775,7.10303076104196,5.70721878269879));
#69857=CARTESIAN_POINT('Ctrl Pts',(3.46583519250046,7.11139689017797,5.70798585320047));
#69858=CARTESIAN_POINT('Ctrl Pts',(3.4589692395527,7.11473900509223,5.70829356135694));
#69859=CARTESIAN_POINT('Ctrl Pts',(3.44541676830162,7.12131163750869,5.708901246944));
#69860=CARTESIAN_POINT('Ctrl Pts',(3.43873051822722,7.12454269187827,5.70920120379815));
#69861=CARTESIAN_POINT('Ctrl Pts',(3.42301394984646,7.132110266346,5.70990664439253));
#69862=CARTESIAN_POINT('Ctrl Pts',(3.41397993541542,7.13643905261351,5.71031242233383));
#69863=CARTESIAN_POINT('Ctrl Pts',(3.384566760328,7.15046419295984,5.71163455235557));
#69864=CARTESIAN_POINT('Ctrl Pts',(3.36415442775782,7.16009045356691,5.71255363186411));
#69865=CARTESIAN_POINT('Ctrl Pts',(2.86166095835166,7.39443842791785,5.73522192258381));
#69866=CARTESIAN_POINT('Ctrl Pts',(2.35829510538361,7.570006128427,5.7594334516651));
#69867=CARTESIAN_POINT('Ctrl Pts',(1.59472603826666,7.75274364326049,5.79541604440773));
#69868=CARTESIAN_POINT('Ctrl Pts',(1.34548551814666,7.79986275922093,5.80703781460866));
#69869=CARTESIAN_POINT('Ctrl Pts',(0.637617840821994,7.89874002508715,5.83925560321977));
#69870=CARTESIAN_POINT('Ctrl Pts',(0.176082918226642,7.92248280954953,5.85928803879936));
#69871=CARTESIAN_POINT('Ctrl Pts',(-0.315086690177379,7.90478028737376,
5.87927124828294));
#69872=CARTESIAN_POINT('Ctrl Pts',(-0.345227301746537,7.90352131331452,
5.8804924710024));
#69873=CARTESIAN_POINT('Ctrl Pts',(-0.386248435682548,7.90157275276713,
5.8821477474101));
#69874=CARTESIAN_POINT('Ctrl Pts',(-0.397135624726235,7.90103304119698,
5.88258641302048));
#69875=CARTESIAN_POINT('Ctrl Pts',(-0.415616436023386,7.90007859530998,
5.88332993837988));
#69876=CARTESIAN_POINT('Ctrl Pts',(-0.423210625524627,7.89967541110753,
5.88363515410429));
#69877=CARTESIAN_POINT('Ctrl Pts',(-0.437860912850174,7.89887642426437,
5.88422335192427));
#69878=CARTESIAN_POINT('Ctrl Pts',(-0.44491708321792,7.89848211583716,5.88450637988196));
#69879=CARTESIAN_POINT('Ctrl Pts',(-0.461602087948332,7.89752730546941,
5.8851749864428));
#69880=CARTESIAN_POINT('Ctrl Pts',(-0.471230454278757,7.8969586479883,5.88556031254988));
#69881=CARTESIAN_POINT('Ctrl Pts',(-0.499428925545599,7.89524147286145,
5.88668734125412));
#69882=CARTESIAN_POINT('Ctrl Pts',(-0.517996104394526,7.89404504726751,
5.88742756017706));
#69883=CARTESIAN_POINT('Ctrl Pts',(-0.655086522677808,7.88472550908008,
5.89287929798806));
#69884=CARTESIAN_POINT('Ctrl Pts',(-0.773420350430547,7.87399880435287,
5.89750940817328));
#69885=CARTESIAN_POINT('Ctrl Pts',(-1.15755434499525,7.83043420750406,5.91231764890264));
#69886=CARTESIAN_POINT('Ctrl Pts',(-1.42194396437552,7.78676575283191,5.92215572795283));
#69887=CARTESIAN_POINT('Ctrl Pts',(-2.10950521061917,7.6370078620693,5.94722612192232));
#69888=CARTESIAN_POINT('Ctrl Pts',(-2.52700115225641,7.50920602060341,5.96189690810108));
#69889=CARTESIAN_POINT('Ctrl Pts',(-3.13746701447804,7.26562014724769,5.98433122219344));
#69890=CARTESIAN_POINT('Ctrl Pts',(-3.33955422127151,7.17497791687253,5.99194135161082));
#69891=CARTESIAN_POINT('Ctrl Pts',(-3.79798889690992,6.94578800764415,6.01012358242564));
#69892=CARTESIAN_POINT('Ctrl Pts',(-4.05100283669737,6.80132621315834,6.02085977275839));
#69893=CARTESIAN_POINT('Ctrl Pts',(-4.30995323735038,6.63389192585832,6.03316864472254));
#69894=CARTESIAN_POINT('Ctrl Pts',(-4.32441856068365,6.62447153329727,6.03386077978817));
#69895=CARTESIAN_POINT('Ctrl Pts',(-4.34435638105539,6.61139410067184,6.03482120650253));
#69896=CARTESIAN_POINT('Ctrl Pts',(-4.34985540959995,6.60777740508074,6.03508678045295));
#69897=CARTESIAN_POINT('Ctrl Pts',(-4.3590305620555,6.60172651647461,6.03553103794525));
#69898=CARTESIAN_POINT('Ctrl Pts',(-4.36270918469568,6.59929609950054,6.03570946377086));
#69899=CARTESIAN_POINT('Ctrl Pts',(-4.36989708083729,6.59453851559377,6.03605870804953));
#69900=CARTESIAN_POINT('Ctrl Pts',(-4.3734065323073,6.5922116193123,6.03622950786512));
#69901=CARTESIAN_POINT('Ctrl Pts',(-4.38171789636009,6.58669131909051,6.03663468485052));
#69902=CARTESIAN_POINT('Ctrl Pts',(-4.38651817235953,6.58349546817502,6.03686923187691));
#69903=CARTESIAN_POINT('Ctrl Pts',(-4.40208258957126,6.57310865964512,6.03763147702867));
#69904=CARTESIAN_POINT('Ctrl Pts',(-4.41283236573116,6.56589667011022,6.0381606646453));
#69905=CARTESIAN_POINT('Ctrl Pts',(-4.66405224746038,6.39645845956242,6.05059138130058));
#69906=CARTESIAN_POINT('Ctrl Pts',(-4.89541685187881,6.22116769284531,6.06339832303223));
#69907=CARTESIAN_POINT('Ctrl Pts',(-5.64766672541784,5.58324390055841,6.10823586258162));
#69908=CARTESIAN_POINT('Ctrl Pts',(-6.11704678303744,5.06465489144723,6.14153870453736));
#69909=CARTESIAN_POINT('Ctrl Pts',(-6.66273704585592,4.2733976523693,6.18349748480281));
#69910=CARTESIAN_POINT('Ctrl Pts',(-6.80199705355515,4.0480671484131,6.19465738866081));
#69911=CARTESIAN_POINT('Ctrl Pts',(-6.94090056341677,3.79583440262743,6.20630739188017));
#69912=CARTESIAN_POINT('Ctrl Pts',(-6.95200462835084,3.77545905866299,6.20724276820934));
#69913=CARTESIAN_POINT('Ctrl Pts',(-6.9674239703305,3.74686673673796,6.2085474350096));
#69914=CARTESIAN_POINT('Ctrl Pts',(-6.97181462226908,3.73869067973158,6.20891960461373));
#69915=CARTESIAN_POINT('Ctrl Pts',(-6.97939114585035,3.72452229022356,6.20956298307715));
#69916=CARTESIAN_POINT('Ctrl Pts',(-6.98258370784065,3.71853355779991,6.2098344469564));
#69917=CARTESIAN_POINT('Ctrl Pts',(-6.98919340766281,3.70609629803709,6.2103972212356));
#69918=CARTESIAN_POINT('Ctrl Pts',(-6.99260933750081,3.6996471336524,6.2106884854944));
#69919=CARTESIAN_POINT('Ctrl Pts',(-7.00060184668952,3.68450692265038,6.21137096790856));
#69920=CARTESIAN_POINT('Ctrl Pts',(-7.00517117852559,3.67581205170315,6.21176191032794));
#69921=CARTESIAN_POINT('Ctrl Pts',(-7.01992905276472,3.6476021896075,6.21302706549719));
#69922=CARTESIAN_POINT('Ctrl Pts',(-7.03005237677896,3.62805309084041,6.21389880416742));
#69923=CARTESIAN_POINT('Ctrl Pts',(-7.21418835136842,3.26880457517399,6.22982780551063));
#69924=CARTESIAN_POINT('Ctrl Pts',(-7.36348162021659,2.91698089216684,6.24390563404368));
#69925=CARTESIAN_POINT('Ctrl Pts',(-7.76822058489126,1.73132607939897,6.28804145891455));
#69926=CARTESIAN_POINT('Ctrl Pts',(-7.91147119677858,0.866368619473638,
6.31458488693133));
#69927=CARTESIAN_POINT('Ctrl Pts',(-7.91099883573547,-0.00429196832219148,
6.34885622675283));
#69928=CARTESIAN_POINT('',(-7.90785232982224,0.00748026227384232,8.35766849176316));
#69929=CARTESIAN_POINT('Ctrl Pts',(-7.92631550431099,-0.00395340570050814,
6.35766849176318));
#69930=CARTESIAN_POINT('Ctrl Pts',(-7.92638474181553,-0.0501225147052013,
6.35953525763348));
#69931=CARTESIAN_POINT('Ctrl Pts',(-7.92601146905589,-0.0962875653539168,
6.36140202350379));
#69932=CARTESIAN_POINT('Ctrl Pts',(-7.9251921263217,-0.14244181639041,6.3632687893741));
#69933=CARTESIAN_POINT('Ctrl Pts',(-7.87873674991768,-2.75931143039582,
6.46911132332844));
#69934=CARTESIAN_POINT('Ctrl Pts',(-5.65808046510112,-6.63253954498222,
6.62787512426005));
#69935=CARTESIAN_POINT('Ctrl Pts',(-0.472789767622867,-8.21296885635869,
6.83956019216859));
#69936=CARTESIAN_POINT('Ctrl Pts',(4.88506260381215,-7.22940821924057,7.05124526007741));
#69937=CARTESIAN_POINT('Ctrl Pts',(8.37301016309629,-2.44600387829248,7.26293032798607));
#69938=CARTESIAN_POINT('Ctrl Pts',(7.68178920747253,2.96689427180967,7.47461539589462));
#69939=CARTESIAN_POINT('Ctrl Pts',(5.34689457404341,6.2859763852109,7.63337919682633));
#69940=CARTESIAN_POINT('Ctrl Pts',(1.68801954593999,8.05996376630325,7.79214299775764));
#69941=CARTESIAN_POINT('Ctrl Pts',(-3.75079024074277,7.87010856532681,8.00382806566654));
#69942=CARTESIAN_POINT('Ctrl Pts',(-7.47900960997268,4.11875362579123,8.19233656366825));
#69943=CARTESIAN_POINT('Ctrl Pts',(-7.91308753929871,0.751099506788409,
8.32792379469287));
#69944=CARTESIAN_POINT('Ctrl Pts',(-7.90669357492867,0.0102339785243165,
8.35766849176316));
#69945=CARTESIAN_POINT('',(-7.911,-4.08117983852208E-12,10.3576684917632));
#69946=CARTESIAN_POINT('Ctrl Pts',(-7.911,-4.02677891031544E-12,8.35766849176316));
#69947=CARTESIAN_POINT('Ctrl Pts',(-7.91099999999888,-2.20167589667082,
8.44625592749589));
#69948=CARTESIAN_POINT('Ctrl Pts',(-6.94214576672145,-4.38610418339042,
8.53484336322862));
#69949=CARTESIAN_POINT('Ctrl Pts',(-3.67820201487902,-7.34180684107825,
8.71201823469407));
#69950=CARTESIAN_POINT('Ctrl Pts',(-1.40868175871317,-8.08992666571412,
8.8006056704268));
#69951=CARTESIAN_POINT('Ctrl Pts',(2.97309270521684,-7.65454228025099,8.97778054189226));
#69952=CARTESIAN_POINT('Ctrl Pts',(5.05102072675952,-6.47444880833954,9.06636797762498));
#69953=CARTESIAN_POINT('Ctrl Pts',(7.66951518848033,-2.93425195367289,9.24354284909043));
#69954=CARTESIAN_POINT('Ctrl Pts',(8.18956872247105,-0.601881960094668,
9.33213028482316));
#69955=CARTESIAN_POINT('Ctrl Pts',(7.32306689761137,3.71537198232857,9.50930515628861));
#69956=CARTESIAN_POINT('Ctrl Pts',(5.94329958849885,5.66643518936844,9.59789259202134));
#69957=CARTESIAN_POINT('Ctrl Pts',(2.16154501637399,7.92205913233121,9.77506746348679));
#69958=CARTESIAN_POINT('Ctrl Pts',(-0.210816529305054,8.20894963712991,
9.86365489921953));
#69959=CARTESIAN_POINT('Ctrl Pts',(-4.42123908576837,6.91982244717576,10.040829770685));
#69960=CARTESIAN_POINT('Ctrl Pts',(-6.226316256345,5.35390358803159,10.1294172064177));
#69961=CARTESIAN_POINT('Ctrl Pts',(-7.65317280859616,2.31334857514088,10.264559258688));
#69962=CARTESIAN_POINT('Ctrl Pts',(-7.9110000000006,1.15702837836093,10.3111138752256));
#69963=CARTESIAN_POINT('Ctrl Pts',(-7.911,-4.08117983852208E-12,10.3576684917632));
#69964=CARTESIAN_POINT('',(-7.90990495318262,0.00414520974019739,14.3576684917631));
#69965=CARTESIAN_POINT('Ctrl Pts',(-7.91099906521622,-0.00384579616109687,
10.3649678417381));
#69966=CARTESIAN_POINT('Ctrl Pts',(-7.91057198107668,-0.88237967762714,
10.3971597508701));
#69967=CARTESIAN_POINT('Ctrl Pts',(-7.76382265767731,-1.75459616253359,
10.4245499411469));
#69968=CARTESIAN_POINT('Ctrl Pts',(-7.42063542251528,-2.74729858307459,
10.4631505107621));
#69969=CARTESIAN_POINT('Ctrl Pts',(-7.35918199542276,-2.90790531779804,
10.4696709074192));
#69970=CARTESIAN_POINT('Ctrl Pts',(-7.28217855326639,-3.09103743038594,
10.4775539654887));
#69971=CARTESIAN_POINT('Ctrl Pts',(-7.27168279065158,-3.11564860632312,
10.478622896393));
#69972=CARTESIAN_POINT('Ctrl Pts',(-7.2580098789783,-3.14726432605392,10.4800088752525));
#69973=CARTESIAN_POINT('Ctrl Pts',(-7.25494697983428,-3.15431838285341,
10.4803189375722));
#69974=CARTESIAN_POINT('Ctrl Pts',(-7.24999433227957,-3.16567927971392,
10.4808196533531));
#69975=CARTESIAN_POINT('Ctrl Pts',(-7.24811101415213,-3.16998893475049,
10.4810099079065));
#69976=CARTESIAN_POINT('Ctrl Pts',(-7.24451681547553,-3.17819370230368,
10.4813727162146));
#69977=CARTESIAN_POINT('Ctrl Pts',(-7.24280663323189,-3.18208912077373,
10.4815452262445));
#69978=CARTESIAN_POINT('Ctrl Pts',(-7.2389013680173,-3.19096499628663,10.4819388890561));
#69979=CARTESIAN_POINT('Ctrl Pts',(-7.23670428791175,-3.19594456654695,
10.4821601677828));
#69980=CARTESIAN_POINT('Ctrl Pts',(-7.22997348399945,-3.2111570637923,10.4828374799755));
#69981=CARTESIAN_POINT('Ctrl Pts',(-7.22542326095984,-3.22138246183518,
10.4832945694224));
#69982=CARTESIAN_POINT('Ctrl Pts',(-7.18917239218993,-3.30238328913814,
10.4869298822154));
#69983=CARTESIAN_POINT('Ctrl Pts',(-7.15645535268782,-3.37269640978962,
10.4901727994694));
#69984=CARTESIAN_POINT('Ctrl Pts',(-6.96388570389769,-3.77113128654321,
10.5089958458147));
#69985=CARTESIAN_POINT('Ctrl Pts',(-6.78251942879694,-4.088340361109,10.525708802195));
#69986=CARTESIAN_POINT('Ctrl Pts',(-6.49586472584326,-4.51780793709011,
10.5496412318384));
#69987=CARTESIAN_POINT('Ctrl Pts',(-6.40820777726173,-4.64130586388238,
10.5566921658941));
#69988=CARTESIAN_POINT('Ctrl Pts',(-6.09263619212748,-5.05991069205952,
10.5810253734471));
#69989=CARTESIAN_POINT('Ctrl Pts',(-5.84743392889067,-5.34139178205895,
10.598133917764));
#69990=CARTESIAN_POINT('Ctrl Pts',(-5.45962329474864,-5.72773073201286,
10.6221563188856));
#69991=CARTESIAN_POINT('Ctrl Pts',(-5.33192165571878,-5.8467942188939,10.629651844648));
#69992=CARTESIAN_POINT('Ctrl Pts',(-5.14016721926627,-6.01406570574888,
10.6403050544507));
#69993=CARTESIAN_POINT('Ctrl Pts',(-5.0791613997734,-6.06567600184165,10.6436106207689));
#69994=CARTESIAN_POINT('Ctrl Pts',(-4.99270644395592,-6.13659694391542,
10.648180050761));
#69995=CARTESIAN_POINT('Ctrl Pts',(-4.96790757188951,-6.15669018859719,
10.6494778069736));
#69996=CARTESIAN_POINT('Ctrl Pts',(-4.9303876047021,-6.18671637474069,10.651421976789));
#69997=CARTESIAN_POINT('Ctrl Pts',(-4.9177567639647,-6.19676123865373,10.6520732079638));
#69998=CARTESIAN_POINT('Ctrl Pts',(-4.89731755057989,-6.21291397663385,
10.6531217966822));
#69999=CARTESIAN_POINT('Ctrl Pts',(-4.88952831309075,-6.21904591949265,
10.6535201861312));
#70000=CARTESIAN_POINT('Ctrl Pts',(-4.87458935844933,-6.23076093865924,
10.6542819280721));
#70001=CARTESIAN_POINT('Ctrl Pts',(-4.86744152739758,-6.23634638761809,
10.6546453818307));
#70002=CARTESIAN_POINT('Ctrl Pts',(-4.85469826742705,-6.24626895442537,
10.6552915495564));
#70003=CARTESIAN_POINT('Ctrl Pts',(-4.84910660079537,-6.25061087360696,
10.6555744681356));
#70004=CARTESIAN_POINT('Ctrl Pts',(-4.83802525529555,-6.25919169970944,
10.6561339291831));
#70005=CARTESIAN_POINT('Ctrl Pts',(-4.83253581552,-6.26343090459634,10.6564104842418));
#70006=CARTESIAN_POINT('Ctrl Pts',(-4.81765418072823,-6.27489199615742,
10.6571586229789));
#70007=CARTESIAN_POINT('Ctrl Pts',(-4.8082513075627,-6.28210002575037,10.6576296184672));
#70008=CARTESIAN_POINT('Ctrl Pts',(-4.77321890196462,-6.30883034346367,
10.6593780798998));
#70009=CARTESIAN_POINT('Ctrl Pts',(-4.74748620720042,-6.32821726354204,
10.6606498240613));
#70010=CARTESIAN_POINT('Ctrl Pts',(-4.3821600137862,-6.5999701845109,10.6785298478837));
#70011=CARTESIAN_POINT('Ctrl Pts',(-4.02295612873389,-6.82486696335122,
10.6939285093056));
#70012=CARTESIAN_POINT('Ctrl Pts',(-3.45335361420601,-7.12082281742278,
10.7162598821874));
#70013=CARTESIAN_POINT('Ctrl Pts',(-3.255147461332,-7.21358347489035,10.723690514822));
#70014=CARTESIAN_POINT('Ctrl Pts',(-2.64675924382396,-7.46812155108779,
10.7459884338386));
#70015=CARTESIAN_POINT('Ctrl Pts',(-2.22669151838874,-7.60394421978643,
10.7606793946627));
#70016=CARTESIAN_POINT('Ctrl Pts',(-1.63530614273069,-7.74192777876334,
10.7828948287936));
#70017=CARTESIAN_POINT('Ctrl Pts',(-1.47193143421454,-7.77464361101532,
10.7891929564004));
#70018=CARTESIAN_POINT('Ctrl Pts',(-1.28245416720249,-7.80640027732479,
10.7968099077025));
#70019=CARTESIAN_POINT('Ctrl Pts',(-1.25723216285564,-7.81050198383651,
10.7978301772157));
#70020=CARTESIAN_POINT('Ctrl Pts',(-1.22484812179071,-7.815607485517,10.7991488245032));
#70021=CARTESIAN_POINT('Ctrl Pts',(-1.21770370712999,-7.81672380029247,
10.7994402785277));
#70022=CARTESIAN_POINT('Ctrl Pts',(-1.20617701075306,-7.81850866023468,
10.7999113924637));
#70023=CARTESIAN_POINT('Ctrl Pts',(-1.20179566649169,-7.81918332226885,
10.8000906712723));
#70024=CARTESIAN_POINT('Ctrl Pts',(-1.19340369004479,-7.82046834213657,
10.8004344520695));
#70025=CARTESIAN_POINT('Ctrl Pts',(-1.18939314801595,-7.82107929873497,
10.8005989170863));
#70026=CARTESIAN_POINT('Ctrl Pts',(-1.18018520979318,-7.82247476819439,
10.8009769085944));
#70027=CARTESIAN_POINT('Ctrl Pts',(-1.17498750318287,-7.82325718582399,
10.8011905633478));
#70028=CARTESIAN_POINT('Ctrl Pts',(-1.15891472086327,-7.82566026376077,
10.8018521191351));
#70029=CARTESIAN_POINT('Ctrl Pts',(-1.14803708549907,-7.82726342612241,
10.8023010804277));
#70030=CARTESIAN_POINT('Ctrl Pts',(-1.06466752194235,-7.83937303223978,
10.8057513466935));
#70031=CARTESIAN_POINT('Ctrl Pts',(-0.992038362476137,-7.8488945515213,
10.8088108938967));
#70032=CARTESIAN_POINT('Ctrl Pts',(-0.103821166611422,-7.95281294854144,
10.8467927485948));
#70033=CARTESIAN_POINT('Ctrl Pts',(0.721532118973731,-7.92070372895431,
10.8873515855274));
#70034=CARTESIAN_POINT('Ctrl Pts',(1.80897967830843,-7.70674926601612,10.9378394405189));
#70035=CARTESIAN_POINT('Ctrl Pts',(2.08754287887858,-7.6360054188718,10.9505639761255));
#70036=CARTESIAN_POINT('Ctrl Pts',(2.47394692210884,-7.51514132093443,10.9678101210924));
#70037=CARTESIAN_POINT('Ctrl Pts',(2.58543741558046,-7.4775181356851,10.972738937587));
#70038=CARTESIAN_POINT('Ctrl Pts',(2.73661868904119,-7.42271521514538,10.9793596680852));
#70039=CARTESIAN_POINT('Ctrl Pts',(2.77706600975968,-7.40767760317586,10.9811248052535));
#70040=CARTESIAN_POINT('Ctrl Pts',(2.84523319138744,-7.38169743488428,10.9840895319938));
#70041=CARTESIAN_POINT('Ctrl Pts',(2.87301768329552,-7.3709279165727,10.9852950742376));
#70042=CARTESIAN_POINT('Ctrl Pts',(2.91149917241148,-7.35576150295803,10.9869608980344));
#70043=CARTESIAN_POINT('Ctrl Pts',(2.92224819315074,-7.35149782143082,10.9874257934812));
#70044=CARTESIAN_POINT('Ctrl Pts',(2.9394884951408,-7.34461553653067,10.9881707743588));
#70045=CARTESIAN_POINT('Ctrl Pts',(2.94598569698152,-7.3420118677396,10.9884513774215));
#70046=CARTESIAN_POINT('Ctrl Pts',(2.95950352296517,-7.33657394288449,10.9890348769518));
#70047=CARTESIAN_POINT('Ctrl Pts',(2.96652355291728,-7.33373822359823,10.9893377222511));
#70048=CARTESIAN_POINT('Ctrl Pts',(2.98264084566769,-7.32720076484524,10.9900326256078));
#70049=CARTESIAN_POINT('Ctrl Pts',(2.99173531592787,-7.32349214944242,10.9904244444667));
#70050=CARTESIAN_POINT('Ctrl Pts',(3.02050447388234,-7.31169790078577,10.9916629976298));
#70051=CARTESIAN_POINT('Ctrl Pts',(3.04015354553766,-7.30354981484479,10.992507562343));
#70052=CARTESIAN_POINT('Ctrl Pts',(3.20534463079779,-7.23426615245253,10.9995968274794));
#70053=CARTESIAN_POINT('Ctrl Pts',(3.34906382947605,-7.16886433954886,11.0056911959243));
#70054=CARTESIAN_POINT('Ctrl Pts',(3.97418435713948,-6.86148755777984,11.0319862738834));
#70055=CARTESIAN_POINT('Ctrl Pts',(4.43210578649819,-6.5750001461634,11.0505615150084));
#70056=CARTESIAN_POINT('Ctrl Pts',(5.2604983339992,-5.93059435755964,11.0867961756885));
#70057=CARTESIAN_POINT('Ctrl Pts',(5.63231715549257,-5.5786895005302,11.1044371889084));
#70058=CARTESIAN_POINT('Ctrl Pts',(5.9984953533835,-5.15792482240521,11.1263939660171));
#70059=CARTESIAN_POINT('Ctrl Pts',(6.02906695479708,-5.12215643060492,11.1282648486462));
#70060=CARTESIAN_POINT('Ctrl Pts',(6.06715026846275,-5.07678609570064,11.130641491682));
#70061=CARTESIAN_POINT('Ctrl Pts',(6.0749617568578,-5.06743614583681,11.1311314585084));
#70062=CARTESIAN_POINT('Ctrl Pts',(6.08735237463813,-5.05253538795189,11.1319125593831));
#70063=CARTESIAN_POINT('Ctrl Pts',(6.09194560259897,-5.04699629027516,11.132202975701));
#70064=CARTESIAN_POINT('Ctrl Pts',(6.10057877144233,-5.0365563625102,11.1327504382646));
#70065=CARTESIAN_POINT('Ctrl Pts',(6.10462038261891,-5.03165691627802,11.1330074008693));
#70066=CARTESIAN_POINT('Ctrl Pts',(6.11368695668513,-5.02063895159478,11.1335853424039));
#70067=CARTESIAN_POINT('Ctrl Pts',(6.11870863940272,-5.01451775070527,11.1339064815764));
#70068=CARTESIAN_POINT('Ctrl Pts',(6.13145362880036,-4.99893454418843,11.1347241509884));
#70069=CARTESIAN_POINT('Ctrl Pts',(6.13916421242646,-4.98946219045832,11.1352212897778));
#70070=CARTESIAN_POINT('Ctrl Pts',(6.18178447069619,-4.93685537835804,11.1379827412921));
#70071=CARTESIAN_POINT('Ctrl Pts',(6.21626101838585,-4.89337297184899,11.1402670132772));
#70072=CARTESIAN_POINT('Ctrl Pts',(6.72723971401613,-4.23480258149033,11.1748544908382));
#70073=CARTESIAN_POINT('Ctrl Pts',(7.11092020475321,-3.55305999768354,11.2100684648503));
#70074=CARTESIAN_POINT('Ctrl Pts',(7.49911171463348,-2.53818489126325,11.2564450684829));
#70075=CARTESIAN_POINT('Ctrl Pts',(7.59236722520927,-2.24388830013566,11.2693215400156));
#70076=CARTESIAN_POINT('Ctrl Pts',(7.68378649476927,-1.88344469292061,11.2844644648059));
#70077=CARTESIAN_POINT('Ctrl Pts',(7.6986308353565,-1.82181837246644,11.2870324566008));
#70078=CARTESIAN_POINT('Ctrl Pts',(7.71773763324199,-1.73808884760496,11.2904944817907));
#70079=CARTESIAN_POINT('Ctrl Pts',(7.72264868039951,-1.71613646976979,11.2913996361497));
#70080=CARTESIAN_POINT('Ctrl Pts',(7.73062230238228,-1.67976695906232,11.2928950521766));
#70081=CARTESIAN_POINT('Ctrl Pts',(7.73373833035206,-1.66536171993156,11.2934862699581));
#70082=CARTESIAN_POINT('Ctrl Pts',(7.73969588991651,-1.63744289052289,11.2946300039706));
#70083=CARTESIAN_POINT('Ctrl Pts',(7.74254232975586,-1.62393040537018,11.2951826077042));
#70084=CARTESIAN_POINT('Ctrl Pts',(7.74864596436921,-1.59457465622449,11.2963810626688));
#70085=CARTESIAN_POINT('Ctrl Pts',(7.75188998181096,-1.57872870615324,11.2970266688636));
#70086=CARTESIAN_POINT('Ctrl Pts',(7.7620978026828,-1.52807677961243,11.2990861891692));
#70087=CARTESIAN_POINT('Ctrl Pts',(7.76887598438157,-1.49323370811335,11.3004966262842));
#70088=CARTESIAN_POINT('Ctrl Pts',(7.82076704947028,-1.21656768287698,11.3116464343408));
#70089=CARTESIAN_POINT('Ctrl Pts',(7.85481398576106,-0.972799779315094,
11.3211640080145));
#70090=CARTESIAN_POINT('Ctrl Pts',(7.93735418621054,-0.0794542015955126,
11.3551489064448));
#70091=CARTESIAN_POINT('Ctrl Pts',(7.91698191507798,0.573790600533551,11.3780373641599));
#70092=CARTESIAN_POINT('Ctrl Pts',(7.7916441161491,1.37875264098124,11.4084106170939));
#70093=CARTESIAN_POINT('Ctrl Pts',(7.76147214170448,1.5395530377404,11.4146063532321));
#70094=CARTESIAN_POINT('Ctrl Pts',(7.71048244740145,1.77139228805234,11.4238564857108));
#70095=CARTESIAN_POINT('Ctrl Pts',(7.69361804883746,1.84326098592666,11.4267689169675));
#70096=CARTESIAN_POINT('Ctrl Pts',(7.67266439806903,1.92725312723281,11.430235853212));
#70097=CARTESIAN_POINT('Ctrl Pts',(7.66954814545796,1.939617184811,11.4307478179174));
#70098=CARTESIAN_POINT('Ctrl Pts',(7.66473624434677,1.95851598979028,11.4315329119258));
#70099=CARTESIAN_POINT('Ctrl Pts',(7.66306209036361,1.96505622730898,11.4318050725991));
#70100=CARTESIAN_POINT('Ctrl Pts',(7.65999841307298,1.97696131073191,11.4323013437489));
#70101=CARTESIAN_POINT('Ctrl Pts',(7.65861161919257,1.98232685966465,11.4325253291397));
#70102=CARTESIAN_POINT('Ctrl Pts',(7.65581652179868,1.99309446594069,11.4329754721483));
#70103=CARTESIAN_POINT('Ctrl Pts',(7.6544081359219,1.99849649839561,11.4332016334942));
#70104=CARTESIAN_POINT('Ctrl Pts',(7.65039507508952,2.01382260060149,11.4338442171972));
#70105=CARTESIAN_POINT('Ctrl Pts',(7.64777681667737,2.02374307470288,11.4342612779022));
#70106=CARTESIAN_POINT('Ctrl Pts',(7.63666411512549,2.06551909346673,11.4360223865732));
#70107=CARTESIAN_POINT('Ctrl Pts',(7.62798991759016,2.09732633233515,11.4373751142866));
#70108=CARTESIAN_POINT('Ctrl Pts',(7.47348647456869,2.65023211936364,11.4611093242326));
#70109=CARTESIAN_POINT('Ctrl Pts',(7.27478073763207,3.15502775450272,11.486080446767));
#70110=CARTESIAN_POINT('Ctrl Pts',(6.81583682560413,4.04199488327738,11.5321143910098));
#70111=CARTESIAN_POINT('Ctrl Pts',(6.57063887336521,4.42946025006581,11.5530960249361));
#70112=CARTESIAN_POINT('Ctrl Pts',(6.1759529603678,4.94762879171046,11.5814992826194));
#70113=CARTESIAN_POINT('Ctrl Pts',(6.05298461998006,5.09733355109033,11.5897607923683));
#70114=CARTESIAN_POINT('Ctrl Pts',(5.85944317081221,5.31606305274151,11.6019061868513));
#70115=CARTESIAN_POINT('Ctrl Pts',(5.79287604273786,5.38852379458448,11.6059433428859));
#70116=CARTESIAN_POINT('Ctrl Pts',(5.71242087999194,5.47288767321996,11.6106620901336));
#70117=CARTESIAN_POINT('Ctrl Pts',(5.69982332502911,5.48600636736837,11.6113964067281));
#70118=CARTESIAN_POINT('Ctrl Pts',(5.6803833857919,5.50611126014726,11.6125226422606));
#70119=CARTESIAN_POINT('Ctrl Pts',(5.67357314077606,5.51312837106187,11.6129158903508));
#70120=CARTESIAN_POINT('Ctrl Pts',(5.66164470997077,5.52537362597298,11.6136024223074));
#70121=CARTESIAN_POINT('Ctrl Pts',(5.65653225593739,5.53060732347208,11.6138959439219));
#70122=CARTESIAN_POINT('Ctrl Pts',(5.64498045529267,5.54240030567731,11.6145575445469));
#70123=CARTESIAN_POINT('Ctrl Pts',(5.63853691769707,5.54895547986091,11.6149254479938));
#70124=CARTESIAN_POINT('Ctrl Pts',(5.62118455127312,5.56654704857579,11.6159131712153));
#70125=CARTESIAN_POINT('Ctrl Pts',(5.61025462628477,5.5775626249371,11.6165321058928));
#70126=CARTESIAN_POINT('Ctrl Pts',(5.56226147264403,5.62564806545191,11.6192358736856));
#70127=CARTESIAN_POINT('Ctrl Pts',(5.52486235894881,5.66238155624846,11.6213065051225));
#70128=CARTESIAN_POINT('Ctrl Pts',(4.85920827364071,6.3033144930139,11.6575382885572));
#70129=CARTESIAN_POINT('Ctrl Pts',(4.13578890552273,6.79991876020181,11.6864662867405));
#70130=CARTESIAN_POINT('Ctrl Pts',(3.1660099092786,7.25256796548579,11.723969375297));
#70131=CARTESIAN_POINT('Ctrl Pts',(2.98295922726337,7.32975511855154,11.7310347468575));
#70132=CARTESIAN_POINT('Ctrl Pts',(2.6237870063464,7.46552299979584,11.7451569221899));
#70133=CARTESIAN_POINT('Ctrl Pts',(2.44812134767194,7.52495808925122,11.7521852291177));
#70134=CARTESIAN_POINT('Ctrl Pts',(2.23744172255077,7.58808067783243,11.7608815521763));
#70135=CARTESIAN_POINT('Ctrl Pts',(2.20429311554061,7.59777636195549,11.7622566101809));
#70136=CARTESIAN_POINT('Ctrl Pts',(2.16036174754652,7.61031421259078,11.7640869759373));
#70137=CARTESIAN_POINT('Ctrl Pts',(2.14963463567596,7.61335118237301,11.7645345434598));
#70138=CARTESIAN_POINT('Ctrl Pts',(2.13203533252269,7.61829358835381,11.765269836125));
#70139=CARTESIAN_POINT('Ctrl Pts',(2.12516690018039,7.62021243164845,11.7655570453459));
#70140=CARTESIAN_POINT('Ctrl Pts',(2.11186875887065,7.62390817388876,11.7661135876519));
#70141=CARTESIAN_POINT('Ctrl Pts',(2.10543937640416,7.62568623341806,11.7663828767579));
#70142=CARTESIAN_POINT('Ctrl Pts',(2.09061122007195,7.62976680951593,11.7670044191273));
#70143=CARTESIAN_POINT('Ctrl Pts',(2.08221088544915,7.6320635917742,11.7673568837643));
#70144=CARTESIAN_POINT('Ctrl Pts',(2.05970137190924,7.63817811410851,11.7683022642162));
#70145=CARTESIAN_POINT('Ctrl Pts',(2.04558540991467,7.64197062096955,11.7688960868105));
#70146=CARTESIAN_POINT('Ctrl Pts',(1.94567850599283,7.66851575747277,11.7731053806426));
#70147=CARTESIAN_POINT('Ctrl Pts',(1.85952206105141,7.68986188733611,11.7767689295909));
#70148=CARTESIAN_POINT('Ctrl Pts',(1.75646751673716,7.71356153581915,11.781178443165));
#70149=CARTESIAN_POINT('Ctrl Pts',(1.73989628461707,7.71731628347817,11.7818883391061));
#70150=CARTESIAN_POINT('Ctrl Pts',(1.19662365178015,7.83857346934994,11.8051869973082));
#70151=CARTESIAN_POINT('Ctrl Pts',(0.659287836616959,7.90192992536936,11.8288601208207));
#70152=CARTESIAN_POINT('Ctrl Pts',(-0.193433763272482,7.91483235956703,
11.8653841944395));
#70153=CARTESIAN_POINT('Ctrl Pts',(-0.506566162748853,7.90097395295921,
11.878608853835));
#70154=CARTESIAN_POINT('Ctrl Pts',(-1.18639068096993,7.83029574412889,11.90701524613));
#70155=CARTESIAN_POINT('Ctrl Pts',(-1.5515856657425,7.76618602852799,11.9221207739951));
#70156=CARTESIAN_POINT('Ctrl Pts',(-1.97461207186458,7.66088327830881,11.9397847546885));
#70157=CARTESIAN_POINT('Ctrl Pts',(-2.03807805662243,7.64424380431644,11.9424372272892));
#70158=CARTESIAN_POINT('Ctrl Pts',(-2.13281889971316,7.618140938867,11.9464003764097));
#70159=CARTESIAN_POINT('Ctrl Pts',(-2.16425388325388,7.6092701989806,11.9477159477078));
#70160=CARTESIAN_POINT('Ctrl Pts',(-2.21837236470394,7.59363584063085,11.9499819163305));
#70161=CARTESIAN_POINT('Ctrl Pts',(-2.2410820753947,7.58696463438578,11.950933113499));
#70162=CARTESIAN_POINT('Ctrl Pts',(-2.29155339858204,7.57189179107308,11.953047875865));
#70163=CARTESIAN_POINT('Ctrl Pts',(-2.3192994555088,7.56343918574742,11.954210962553));
#70164=CARTESIAN_POINT('Ctrl Pts',(-2.39263055412286,7.540658013955,11.9572864034181));
#70165=CARTESIAN_POINT('Ctrl Pts',(-2.43813342565547,7.52606867365385,11.9591962642178));
#70166=CARTESIAN_POINT('Ctrl Pts',(-2.63688177368224,7.46035340928852,11.9675458226683));
#70167=CARTESIAN_POINT('Ctrl Pts',(-2.78867415734696,7.40495213052502,11.9739419401032));
#70168=CARTESIAN_POINT('Ctrl Pts',(-3.44855094367339,7.14093954473215,12.0018995022386));
#70169=CARTESIAN_POINT('Ctrl Pts',(-3.93580363057525,6.88440027061463,12.0228549884201));
#70170=CARTESIAN_POINT('Ctrl Pts',(-4.56677976971644,6.4631517682881,12.052395624773));
#70171=CARTESIAN_POINT('Ctrl Pts',(-4.73631930609016,6.33995929165136,12.0606159343692));
#70172=CARTESIAN_POINT('Ctrl Pts',(-4.92173374058754,6.19363959813403,12.0700683409608));
#70173=CARTESIAN_POINT('Ctrl Pts',(-4.94261813161492,6.17698635890976,12.0711399214685));
#70174=CARTESIAN_POINT('Ctrl Pts',(-4.97403329337885,6.15167453987365,12.0727626973159));
#70175=CARTESIAN_POINT('Ctrl Pts',(-4.98462674283243,6.14309393393588,12.0733117912938));
#70176=CARTESIAN_POINT('Ctrl Pts',(-5.00288523790929,6.12822638076048,12.0742615070649));
#70177=CARTESIAN_POINT('Ctrl Pts',(-5.01056075394301,6.12195231996527,12.0746617667322));
#70178=CARTESIAN_POINT('Ctrl Pts',(-5.02759280759495,6.10797662248854,12.0755522430866));
#70179=CARTESIAN_POINT('Ctrl Pts',(-5.03694347586652,6.10026788588286,12.0760426643604));
#70180=CARTESIAN_POINT('Ctrl Pts',(-5.06180135993526,6.07967880477147,12.077350596979));
#70181=CARTESIAN_POINT('Ctrl Pts',(-5.07727700003152,6.06676071996899,12.0781692647516));
#70182=CARTESIAN_POINT('Ctrl Pts',(-5.15280988895577,6.00321920634209,12.0821864400853));
#70183=CARTESIAN_POINT('Ctrl Pts',(-5.21215960622338,5.95176297700436,12.0854093566284));
#70184=CARTESIAN_POINT('Ctrl Pts',(-5.31910344464904,5.8562160927036,12.0913304058303));
#70185=CARTESIAN_POINT('Ctrl Pts',(-5.36694070752205,5.81240704824798,12.0940219602861));
#70186=CARTESIAN_POINT('Ctrl Pts',(-5.56876835864034,5.62295851015435,12.1055521658863));
#70187=CARTESIAN_POINT('Ctrl Pts',(-5.71740995080261,5.47175156197472,12.114483056172));
#70188=CARTESIAN_POINT('Ctrl Pts',(-6.04007051853839,5.11600158583701,12.1347400885826));
#70189=CARTESIAN_POINT('Ctrl Pts',(-6.21011521253505,4.90819686212203,12.1460554319916));
#70190=CARTESIAN_POINT('Ctrl Pts',(-6.52007920837321,4.48744213779018,12.1678586904135));
#70191=CARTESIAN_POINT('Ctrl Pts',(-6.66093216206234,4.27557695239898,12.1783468107694));
#70192=CARTESIAN_POINT('Ctrl Pts',(-6.82398314142684,4.00265238843444,12.191276675271));
#70193=CARTESIAN_POINT('Ctrl Pts',(-6.85596565550101,3.94762043292549,12.1938559182505));
#70194=CARTESIAN_POINT('Ctrl Pts',(-6.90152585455357,3.86700144580556,12.197595282332));
#70195=CARTESIAN_POINT('Ctrl Pts',(-6.91563249153241,3.84171661549174,12.1987625543951));
#70196=CARTESIAN_POINT('Ctrl Pts',(-6.94016521726196,3.79717097338337,12.2008095087994));
#70197=CARTESIAN_POINT('Ctrl Pts',(-6.95065070835634,3.77794327354758,12.2016899748308));
#70198=CARTESIAN_POINT('Ctrl Pts',(-6.97090900099191,3.74042494120677,12.2034021008175));
#70199=CARTESIAN_POINT('Ctrl Pts',(-6.98068999305033,3.72213893681264,12.2042338621265));
#70200=CARTESIAN_POINT('Ctrl Pts',(-7.00401924416201,3.67810844697983,12.2062302492886));
#70201=CARTESIAN_POINT('Ctrl Pts',(-7.01749763227976,3.65232724568943,12.2073939691314));
#70202=CARTESIAN_POINT('Ctrl Pts',(-7.06685203017204,3.55664126362344,12.2116942605815));
#70203=CARTESIAN_POINT('Ctrl Pts',(-7.10182837993177,3.48627717017877,12.2148195260181));
#70204=CARTESIAN_POINT('Ctrl Pts',(-7.48134210319676,2.6933648350003,12.2496590140817));
#70205=CARTESIAN_POINT('Ctrl Pts',(-7.71536966193981,1.92299114742071,12.2802299309106));
#70206=CARTESIAN_POINT('Ctrl Pts',(-7.88398953567299,0.755288528951129,
12.3243985687035));
#70207=CARTESIAN_POINT('Ctrl Pts',(-7.91112897766017,0.376530074955401,
12.3384731604433));
#70208=CARTESIAN_POINT('Ctrl Pts',(-7.91094292353554,-0.168573338039825,
12.3593972147587));
#70209=CARTESIAN_POINT('Ctrl Pts',(-7.9056694122443,-0.334398991950649,
12.3658561422641));
#70210=CARTESIAN_POINT('Ctrl Pts',(-7.89389772941376,-0.520304129314716,
12.3732917211989));
#70211=CARTESIAN_POINT('Ctrl Pts',(-7.89252880157451,-0.540672597338497,
12.3741090324915));
#70212=CARTESIAN_POINT('Ctrl Pts',(-7.89039630589137,-0.570666596264693,
12.3753167054481));
#70213=CARTESIAN_POINT('Ctrl Pts',(-7.88969392519024,-0.580296470804183,
12.3757050676165));
#70214=CARTESIAN_POINT('Ctrl Pts',(-7.88842254330443,-0.597298459763331,
12.3763918755042));
#70215=CARTESIAN_POINT('Ctrl Pts',(-7.88786083240934,-0.604671117117169,
12.3766900769387));
#70216=CARTESIAN_POINT('Ctrl Pts',(-7.88667732202812,-0.619922804888298,
12.3773077579349));
#70217=CARTESIAN_POINT('Ctrl Pts',(-7.88605404986315,-0.62780171067851,
12.3776272873688));
#70218=CARTESIAN_POINT('Ctrl Pts',(-7.88442622267742,-0.647994427748542,
12.3784473563314));
#70219=CARTESIAN_POINT('Ctrl Pts',(-7.88340462880942,-0.660306819336622,
12.3789484872272));
#70220=CARTESIAN_POINT('Ctrl Pts',(-7.87909898430925,-0.710764403442265,
12.3810068301706));
#70221=CARTESIAN_POINT('Ctrl Pts',(-7.87556691566925,-0.748887530610363,
12.3825729055543));
#70222=CARTESIAN_POINT('Ctrl Pts',(-7.81998220310333,-1.3048707935045,12.4055873459321));
#70223=CARTESIAN_POINT('Ctrl Pts',(-7.71723551499487,-1.81627550322845,
12.429366737792));
#70224=CARTESIAN_POINT('Ctrl Pts',(-7.49214956433761,-2.55221191251773,
12.4646396354337));
#70225=CARTESIAN_POINT('Ctrl Pts',(-7.40799074989495,-2.78707175986403,
12.4760624524673));
#70226=CARTESIAN_POINT('Ctrl Pts',(-7.13891279354165,-3.43916453018471,
12.5078365070028));
#70227=CARTESIAN_POINT('Ctrl Pts',(-6.92880049308469,-3.84496267450702,
12.527628013733));
#70228=CARTESIAN_POINT('Ctrl Pts',(-6.66888418691902,-4.25567824466761,
12.5473877997429));
#70229=CARTESIAN_POINT('Ctrl Pts',(-6.65276449799541,-4.28083381831811,
12.548597206193));
#70230=CARTESIAN_POINT('Ctrl Pts',(-6.6305936048464,-4.31500490212036,12.5502389688052));
#70231=CARTESIAN_POINT('Ctrl Pts',(-6.62466587966553,-4.32410000369459,
12.5506758412599));
#70232=CARTESIAN_POINT('Ctrl Pts',(-6.61456062214397,-4.33953527747424,
12.5514170826851));
#70233=CARTESIAN_POINT('Ctrl Pts',(-6.61039265800405,-4.3458816776194,12.5517218030335));
#70234=CARTESIAN_POINT('Ctrl Pts',(-6.60232570275485,-4.3581264675895,12.5523096380675));
#70235=CARTESIAN_POINT('Ctrl Pts',(-6.59842792876036,-4.36402564864764,
12.5525927972494));
#70236=CARTESIAN_POINT('Ctrl Pts',(-6.58917934580003,-4.37798242395774,
12.5532626204084));
#70237=CARTESIAN_POINT('Ctrl Pts',(-6.58382165223542,-4.38603545448579,
12.5536490290804));
#70238=CARTESIAN_POINT('Ctrl Pts',(-6.56804246605141,-4.4096587399761,12.5547823240929));
#70239=CARTESIAN_POINT('Ctrl Pts',(-6.5575803808945,-4.42520187032525,12.5555277012866));
#70240=CARTESIAN_POINT('Ctrl Pts',(-6.47849450338701,-4.54180045354959,
12.5611172555531));
#70241=CARTESIAN_POINT('Ctrl Pts',(-6.40759196883169,-4.64129391263505,
12.5658752410872));
#70242=CARTESIAN_POINT('Ctrl Pts',(-6.16678465574467,-4.96316303609849,
12.5812565634968));
#70243=CARTESIAN_POINT('Ctrl Pts',(-5.98738170385845,-5.1781749519126,12.5915054056492));
#70244=CARTESIAN_POINT('Ctrl Pts',(-5.58494692041342,-5.61153772323387,
12.6125009678628));
#70245=CARTESIAN_POINT('Ctrl Pts',(-5.35963578123574,-5.82711761938126,
12.6231523282668));
#70246=CARTESIAN_POINT('Ctrl Pts',(-5.01219605947817,-6.12230720410174,
12.6386752315774));
#70247=CARTESIAN_POINT('Ctrl Pts',(-4.89966060832409,-6.21273534339769,
12.6435798729402));
#70248=CARTESIAN_POINT('Ctrl Pts',(-4.64617666636072,-6.40524993083205,
12.6544782755039));
#70249=CARTESIAN_POINT('Ctrl Pts',(-4.50420823607487,-6.50586581502865,
12.6604857838361));
#70250=CARTESIAN_POINT('Ctrl Pts',(-4.10722463127369,-6.76798974426168,
12.6773082800426));
#70251=CARTESIAN_POINT('Ctrl Pts',(-3.84612065961206,-6.91970404113166,
12.6883973511577));
#70252=CARTESIAN_POINT('Ctrl Pts',(-3.56092790012047,-7.0642790755253,12.7011535073613));
#70253=CARTESIAN_POINT('Ctrl Pts',(-3.54481145964228,-7.07237994401317,
12.7018764823961));
#70254=CARTESIAN_POINT('Ctrl Pts',(-3.52254522154923,-7.08347675616798,
12.702878422273));
#70255=CARTESIAN_POINT('Ctrl Pts',(-3.51641892892075,-7.08651999988749,
12.7031544156759));
#70256=CARTESIAN_POINT('Ctrl Pts',(-3.50664698823074,-7.09135843216561,
12.7035951709909));
#70257=CARTESIAN_POINT('Ctrl Pts',(-3.5030038790084,-7.09315877004391,12.7037596061665));
#70258=CARTESIAN_POINT('Ctrl Pts',(-3.4959088763605,-7.09665815229578,12.7040800738716));
#70259=CARTESIAN_POINT('Ctrl Pts',(-3.49245712767554,-7.09835748702438,
12.7042360877296));
#70260=CARTESIAN_POINT('Ctrl Pts',(-3.48419173287023,-7.10241914564412,
12.7046099252819));
#70261=CARTESIAN_POINT('Ctrl Pts',(-3.47937692708046,-7.10477909233291,
12.7048279014368));
#70262=CARTESIAN_POINT('Ctrl Pts',(-3.46487486402493,-7.11186890989261,
12.705485069899));
#70263=CARTESIAN_POINT('Ctrl Pts',(-3.45518049500035,-7.11658379844696,
12.7059252266967));
#70264=CARTESIAN_POINT('Ctrl Pts',(-3.35452710587119,-7.16528275858591,
12.7105041082501));
#70265=CARTESIAN_POINT('Ctrl Pts',(-3.26274681950491,-7.20753845690531,
12.7147537572039));
#70266=CARTESIAN_POINT('Ctrl Pts',(-2.99872330643792,-7.3230187430057,12.7271290693311));
#70267=CARTESIAN_POINT('Ctrl Pts',(-2.82466134133931,-7.39190272322281,
12.73546609378));
#70268=CARTESIAN_POINT('Ctrl Pts',(-2.04211206372408,-7.66991422459173,
12.773180158934));
#70269=CARTESIAN_POINT('Ctrl Pts',(-1.41178166387862,-7.81055909177022,
12.803908750693));
#70270=CARTESIAN_POINT('Ctrl Pts',(-0.511743733597448,-7.8987405318854,
12.8439323632822));
#70271=CARTESIAN_POINT('Ctrl Pts',(-0.250985591616078,-7.91132149617307,
12.8551236232527));
#70272=CARTESIAN_POINT('Ctrl Pts',(0.0831678784627014,-7.91090177594154,
12.8689047692178));
#70273=CARTESIAN_POINT('Ctrl Pts',(0.156395476740914,-7.90979295973493,
12.8718910202751));
#70274=CARTESIAN_POINT('Ctrl Pts',(0.244206198407208,-7.90724338156028,
12.8754322832596));
#70275=CARTESIAN_POINT('Ctrl Pts',(0.25881267319208,-7.90677877305069,12.8760200224908));
#70276=CARTESIAN_POINT('Ctrl Pts',(0.282618152018711,-7.90595552272274,
12.8769757827018));
#70277=CARTESIAN_POINT('Ctrl Pts',(0.291817931135807,-7.90562129392657,
12.8773446234972));
#70278=CARTESIAN_POINT('Ctrl Pts',(0.308219602131311,-7.90499675064557,
12.8780012842433));
#70279=CARTESIAN_POINT('Ctrl Pts',(0.315421711564824,-7.90471265101458,
12.8782893127928));
#70280=CARTESIAN_POINT('Ctrl Pts',(0.330598305899951,-7.9040932095109,12.8788955942288));
#70281=CARTESIAN_POINT('Ctrl Pts',(0.338572694712872,-7.90375564117537,
12.8792137719128));
#70282=CARTESIAN_POINT('Ctrl Pts',(0.359617582645859,-7.90283287017822,
12.8800524454896));
#70283=CARTESIAN_POINT('Ctrl Pts',(0.372687190791276,-7.90222730879096,
12.880572256141));
#70284=CARTESIAN_POINT('Ctrl Pts',(0.431599913346708,-7.89935119199268,
12.8829107320863));
#70285=CARTESIAN_POINT('Ctrl Pts',(0.477424700038748,-7.89671409458951,
12.8847170513157));
#70286=CARTESIAN_POINT('Ctrl Pts',(0.80845729397981,-7.87477193400816,12.8976772563508));
#70287=CARTESIAN_POINT('Ctrl Pts',(1.09246692385802,-7.84041907516085,12.9083098943244));
#70288=CARTESIAN_POINT('Ctrl Pts',(1.90866642295981,-7.69647050323325,12.9379890495746));
#70289=CARTESIAN_POINT('Ctrl Pts',(2.43216735476726,-7.54739815922646,12.955831510622));
#70290=CARTESIAN_POINT('Ctrl Pts',(3.14643934839447,-7.2618911314956,12.9821345141041));
#70291=CARTESIAN_POINT('Ctrl Pts',(3.35288634969586,-7.16891122001979,12.9900062118686));
#70292=CARTESIAN_POINT('Ctrl Pts',(3.7271766991155,-6.98063019661283,13.0052637446836));
#70293=CARTESIAN_POINT('Ctrl Pts',(3.89606783157521,-6.88779278415899,13.0125437376599));
#70294=CARTESIAN_POINT('Ctrl Pts',(4.07318536589359,-6.78183388975971,13.0207941242038));
#70295=CARTESIAN_POINT('Ctrl Pts',(4.08496252187106,-6.77474657262915,13.0213457126258));
#70296=CARTESIAN_POINT('Ctrl Pts',(4.10124360262773,-6.76489097177664,13.0221124810346));
#70297=CARTESIAN_POINT('Ctrl Pts',(4.10576338174277,-6.76214877100989,13.0223257965578));
#70298=CARTESIAN_POINT('Ctrl Pts',(4.1135450087943,-6.7574168924967,13.0226938454136));
#70299=CARTESIAN_POINT('Ctrl Pts',(4.11680815829377,-6.75542938576662,13.0228484215376));
#70300=CARTESIAN_POINT('Ctrl Pts',(4.12355977958542,-6.75131042515161,13.0231687389019));
#70301=CARTESIAN_POINT('Ctrl Pts',(4.12704804072541,-6.74917863017348,13.0233345045565));
#70302=CARTESIAN_POINT('Ctrl Pts',(4.13519525631529,-6.74419091176789,13.0237223011931));
#70303=CARTESIAN_POINT('Ctrl Pts',(4.13985290210613,-6.741332866047,13.0239444830674));
#70304=CARTESIAN_POINT('Ctrl Pts',(4.15480392247154,-6.7321372152446,13.0246592318724));
#70305=CARTESIAN_POINT('Ctrl Pts',(4.16508568870247,-6.72578087076789,13.0251531189568));
#70306=CARTESIAN_POINT('Ctrl Pts',(4.36799340736201,-6.59969652094499,13.0349458197738));
#70307=CARTESIAN_POINT('Ctrl Pts',(4.55538192507872,-6.47177247722091,13.0448083376605));
#70308=CARTESIAN_POINT('Ctrl Pts',(5.2003773730214,-5.9895519752051,13.0809877119812));
#70309=CARTESIAN_POINT('Ctrl Pts',(5.6243494887328,-5.5933328140834,13.1088561423947));
#70310=CARTESIAN_POINT('Ctrl Pts',(6.34581639885618,-4.75332357639945,13.1599965414283));
#70311=CARTESIAN_POINT('Ctrl Pts',(6.64926751996135,-4.31866419020705,13.1833288148501));
#70312=CARTESIAN_POINT('Ctrl Pts',(6.92370875687746,-3.82718399292746,13.2062462508969));
#70313=CARTESIAN_POINT('Ctrl Pts',(6.94011649178461,-3.79734952118029,13.2076252764666));
#70314=CARTESIAN_POINT('Ctrl Pts',(6.96224822833813,-3.75648439130198,13.2094978426363));
#70315=CARTESIAN_POINT('Ctrl Pts',(6.96813947927014,-3.74554503035532,13.2099975310944));
#70316=CARTESIAN_POINT('Ctrl Pts',(6.97742625535198,-3.72820283452315,13.210787191168));
#70317=CARTESIAN_POINT('Ctrl Pts',(6.98083878334621,-3.72180915758926,13.2110777851002));
#70318=CARTESIAN_POINT('Ctrl Pts',(6.98742534323375,-3.70942771868935,13.2116394907264));
#70319=CARTESIAN_POINT('Ctrl Pts',(6.9906004758436,-3.70344055101387,13.2119106424804));
#70320=CARTESIAN_POINT('Ctrl Pts',(6.99812114837816,-3.68921511233897,13.2125537918746));
#70321=CARTESIAN_POINT('Ctrl Pts',(7.00245984484999,-3.68097322382787,13.2129255400676));
#70322=CARTESIAN_POINT('Ctrl Pts',(7.01522912263288,-3.65661212862132,13.2140217621512));
#70323=CARTESIAN_POINT('Ctrl Pts',(7.02361870030412,-3.64047143386169,13.2147447476181));
#70324=CARTESIAN_POINT('Ctrl Pts',(7.08860692581546,-3.51437980706251,13.2203670509686));
#70325=CARTESIAN_POINT('Ctrl Pts',(7.14267749232969,-3.40314171565699,13.2251747264478));
#70326=CARTESIAN_POINT('Ctrl Pts',(7.32373600397322,-3.00730947563662,13.2417938038197));
#70327=CARTESIAN_POINT('Ctrl Pts',(7.43650200595465,-2.71651907479519,13.2531180230539));
#70328=CARTESIAN_POINT('Ctrl Pts',(7.68074788304711,-1.95629004921626,13.2813300127674));
#70329=CARTESIAN_POINT('Ctrl Pts',(7.78655714297726,-1.48002151445437,13.29766845675));
#70330=CARTESIAN_POINT('Ctrl Pts',(7.88800319004038,-0.68153548830664,13.3262218467346));
#70331=CARTESIAN_POINT('Ctrl Pts',(7.90902565384798,-0.363878220777233,
13.3379312660078));
#70332=CARTESIAN_POINT('Ctrl Pts',(7.91100511558555,-0.0220198555669485,
13.3515476374036));
#70333=CARTESIAN_POINT('Ctrl Pts',(7.91103556269699,0.00176689301103428,
13.3524995600894));
#70334=CARTESIAN_POINT('Ctrl Pts',(7.91093050328304,0.034291954984522,13.3538070446172));
#70335=CARTESIAN_POINT('Ctrl Pts',(7.91088779676659,0.0430305951357745,
13.3541589105356));
#70336=CARTESIAN_POINT('Ctrl Pts',(7.91079040641116,0.0579127981321211,
13.35475911931));
#70337=CARTESIAN_POINT('Ctrl Pts',(7.91074304487798,0.0640564126838488,
13.3550071764854));
#70338=CARTESIAN_POINT('Ctrl Pts',(7.91063754482319,0.0759449968300303,
13.355487732757));
#70339=CARTESIAN_POINT('Ctrl Pts',(7.91058030465561,0.0816899717049817,
13.3557201971834));
#70340=CARTESIAN_POINT('Ctrl Pts',(7.91042951927387,0.0953320152892803,
13.3562727788523));
#70341=CARTESIAN_POINT('Ctrl Pts',(7.9103304067409,0.103229008297088,13.3565931067895));
#70342=CARTESIAN_POINT('Ctrl Pts',(7.91000276441198,0.126551425152569,13.3575404605473));
#70343=CARTESIAN_POINT('Ctrl Pts',(7.90974093909563,0.141976295464001,13.3581687223974));
#70344=CARTESIAN_POINT('Ctrl Pts',(7.90736403277617,0.261416929245609,13.3630463935562));
#70345=CARTESIAN_POINT('Ctrl Pts',(7.90324243665916,0.365380144076104,13.3673670887883));
#70346=CARTESIAN_POINT('Ctrl Pts',(7.88085197158054,0.742209174616122,13.3832446307259));
#70347=CARTESIAN_POINT('Ctrl Pts',(7.85048909334578,1.01415669672764,13.3951102836394));
#70348=CARTESIAN_POINT('Ctrl Pts',(7.75621939416736,1.5872825190564,13.4204932609149));
#70349=CARTESIAN_POINT('Ctrl Pts',(7.68869444826428,1.88742870221137,13.4340077710592));
#70350=CARTESIAN_POINT('Ctrl Pts',(7.55643929391266,2.34812723892847,13.4547945815904));
#70351=CARTESIAN_POINT('Ctrl Pts',(7.50362768984153,2.51178223856262,13.4621902346964));
#70352=CARTESIAN_POINT('Ctrl Pts',(7.34003922498173,2.96735030229902,13.4827742878316));
#70353=CARTESIAN_POINT('Ctrl Pts',(7.21725733351476,3.25462080078784,13.4957402822217));
#70354=CARTESIAN_POINT('Ctrl Pts',(7.06130130625612,3.56697515752773,13.5098862036261));
#70355=CARTESIAN_POINT('Ctrl Pts',(7.04455398198891,3.59993710111737,13.5113798331956));
#70356=CARTESIAN_POINT('Ctrl Pts',(7.01917349858612,3.64903538236361,13.513606109142));
#70357=CARTESIAN_POINT('Ctrl Pts',(7.01071444890233,3.66526107449348,13.5143420626276));
#70358=CARTESIAN_POINT('Ctrl Pts',(6.9960767480636,3.69310224928894,13.5156052464317));
#70359=CARTESIAN_POINT('Ctrl Pts',(6.98992528675756,3.7047319167885,13.5161330124327));
#70360=CARTESIAN_POINT('Ctrl Pts',(6.97718613108572,3.72867129371056,13.5172196417223));
#70361=CARTESIAN_POINT('Ctrl Pts',(6.97059480183289,3.7409790208575,13.5177784295066));
#70362=CARTESIAN_POINT('Ctrl Pts',(6.95536350046394,3.76923980696297,13.5190618047613));
#70363=CARTESIAN_POINT('Ctrl Pts',(6.94670115424453,3.78518073846935,13.5197859303597));
#70364=CARTESIAN_POINT('Ctrl Pts',(6.91928725453774,3.83521825656811,13.5220596027478));
#70365=CARTESIAN_POINT('Ctrl Pts',(6.90033884811351,3.86920650784861,13.5236050155179));
#70366=CARTESIAN_POINT('Ctrl Pts',(6.85600984341112,3.9473591855416,13.5271609944496));
#70367=CARTESIAN_POINT('Ctrl Pts',(6.83045186110074,3.99142117049217,13.5291676551678));
#70368=CARTESIAN_POINT('Ctrl Pts',(6.42445478118277,4.67603951395493,13.5603788505829));
#70369=CARTESIAN_POINT('Ctrl Pts',(5.95585745240629,5.25991456050197,13.5869036925496));
#70370=CARTESIAN_POINT('Ctrl Pts',(5.17560209973628,5.99187707791571,13.6261808213525));
#70371=CARTESIAN_POINT('Ctrl Pts',(4.92523381000498,6.19931379996694,13.6383121588653));
#70372=CARTESIAN_POINT('Ctrl Pts',(4.6477968454869,6.40173824060358,13.6520143020839));
#70373=CARTESIAN_POINT('Ctrl Pts',(4.63270956515399,6.41266482008458,13.6527602464552));
#70374=CARTESIAN_POINT('Ctrl Pts',(4.61166170459041,6.42779515222198,13.653802216833));
#70375=CARTESIAN_POINT('Ctrl Pts',(4.60573361396373,6.43204415977029,13.6540958312776));
#70376=CARTESIAN_POINT('Ctrl Pts',(4.59550455780423,6.43935452739607,13.6546027351572));
#70377=CARTESIAN_POINT('Ctrl Pts',(4.59120638237387,6.44241979573845,13.6548158130943));
#70378=CARTESIAN_POINT('Ctrl Pts',(4.58232091980058,6.44874310591347,13.6552564745998));
#70379=CARTESIAN_POINT('Ctrl Pts',(4.57773322008242,6.45200055979598,13.6554840900156));
#70380=CARTESIAN_POINT('Ctrl Pts',(4.56703116388776,6.45958229554746,13.6560152958301));
#70381=CARTESIAN_POINT('Ctrl Pts',(4.56091414147107,6.4639027899879,13.6563190949626));
#70382=CARTESIAN_POINT('Ctrl Pts',(4.54134477863286,6.4776831550029,13.6572915888545));
#70383=CARTESIAN_POINT('Ctrl Pts',(4.5278691348644,6.48710972206702,13.6579621470252));
#70384=CARTESIAN_POINT('Ctrl Pts',(4.49676662714164,6.50872261767476,13.6595121082597));
#70385=CARTESIAN_POINT('Ctrl Pts',(4.47911943699744,6.52087948676193,13.6603932216758));
#70386=CARTESIAN_POINT('Ctrl Pts',(4.4187223680554,6.56212521401816,13.6634152104931));
#70387=CARTESIAN_POINT('Ctrl Pts',(4.3757376535872,6.5908659881499,13.6655765939995));
#70388=CARTESIAN_POINT('Ctrl Pts',(4.16637816783898,6.72789872996754,13.6761440554093));
#70389=CARTESIAN_POINT('Ctrl Pts',(3.9962567659548,6.83031855292808,13.6848521688649));
#70390=CARTESIAN_POINT('Ctrl Pts',(3.52119675655663,7.09249662130454,13.7091634006234));
#70391=CARTESIAN_POINT('Ctrl Pts',(3.20939841942565,7.23892856657625,13.7251013611657));
#70392=CARTESIAN_POINT('Ctrl Pts',(2.27195763366182,7.60667854130153,13.7714745325932));
#70393=CARTESIAN_POINT('Ctrl Pts',(1.62677800316817,7.77027657844395,13.8012503850251));
#70394=CARTESIAN_POINT('Ctrl Pts',(0.92677360516341,7.85664016368797,13.8300788304247));
#70395=CARTESIAN_POINT('Ctrl Pts',(0.884824922468746,7.86147498264042,13.8317946270485));
#70396=CARTESIAN_POINT('Ctrl Pts',(0.828681361628141,7.86749076545296,13.8340755264006));
#70397=CARTESIAN_POINT('Ctrl Pts',(0.814519481856601,7.86896954879795,13.8346495533726));
#70398=CARTESIAN_POINT('Ctrl Pts',(0.792379770655545,7.87122096876801,13.8355449044463));
#70399=CARTESIAN_POINT('Ctrl Pts',(0.784404658984386,7.87201972631806,13.8358670114656));
#70400=CARTESIAN_POINT('Ctrl Pts',(0.769146049729517,7.87352455394798,13.8364825029414));
#70401=CARTESIAN_POINT('Ctrl Pts',(0.761862761907683,7.87423264069644,13.8367759475751));
#70402=CARTESIAN_POINT('Ctrl Pts',(0.744830788677803,7.8758646500763,13.8374613675367));
#70403=CARTESIAN_POINT('Ctrl Pts',(0.735081339892921,7.87678058058522,13.8378531028979));
#70404=CARTESIAN_POINT('Ctrl Pts',(0.707154712912288,7.87935189978771,13.8389734560641));
#70405=CARTESIAN_POINT('Ctrl Pts',(0.688973421235429,7.88096249064679,13.8397007306963));
#70406=CARTESIAN_POINT('Ctrl Pts',(0.571513940217959,7.89095806939856,13.8443857330652));
#70407=CARTESIAN_POINT('Ctrl Pts',(0.472088540911872,7.89753003822413,13.8482888984392));
#70408=CARTESIAN_POINT('Ctrl Pts',(0.176714189488021,7.91145594826203,13.8597134977731));
#70409=CARTESIAN_POINT('Ctrl Pts',(-0.019416305734166,7.91340582274937,
13.8670749875113));
#70410=CARTESIAN_POINT('Ctrl Pts',(-0.347925794187607,7.90445686131532,
13.8791255750927));
#70411=CARTESIAN_POINT('Ctrl Pts',(-0.480317729926491,7.89751776345304,
13.8839063631969));
#70412=CARTESIAN_POINT('Ctrl Pts',(-0.84892559843332,7.86889396315792,13.8970742118697));
#70413=CARTESIAN_POINT('Ctrl Pts',(-1.08443423228592,7.83990898624841,13.9053203770593));
#70414=CARTESIAN_POINT('Ctrl Pts',(-1.50263648320707,7.76923160068669,13.9199857568496));
#70415=CARTESIAN_POINT('Ctrl Pts',(-1.68582187551429,7.73155095242213,13.926418659946));
#70416=CARTESIAN_POINT('Ctrl Pts',(-2.30228634592221,7.58179362510882,13.9484616739566));
#70417=CARTESIAN_POINT('Ctrl Pts',(-2.72732533387491,7.439476070655,13.9643341635458));
#70418=CARTESIAN_POINT('Ctrl Pts',(-3.1702944621503,7.24806101527795,13.9834022714797));
#70419=CARTESIAN_POINT('Ctrl Pts',(-3.20245338658352,7.23390957313716,13.9848004020707));
#70420=CARTESIAN_POINT('Ctrl Pts',(-3.24516269989113,7.21477485026682,13.9866747013566));
#70421=CARTESIAN_POINT('Ctrl Pts',(-3.25579817876838,7.20998164395142,13.9871428911578));
#70422=CARTESIAN_POINT('Ctrl Pts',(-3.27236107149047,7.20247294514798,13.9878742390647));
#70423=CARTESIAN_POINT('Ctrl Pts',(-3.2782958212829,7.19977360863918,13.9881367388999));
#70424=CARTESIAN_POINT('Ctrl Pts',(-3.29021997117679,7.19433227845172,13.9886650441898));
#70425=CARTESIAN_POINT('Ctrl Pts',(-3.29620929665295,7.19159013458303,13.9889308555334));
#70426=CARTESIAN_POINT('Ctrl Pts',(-3.30964356169433,7.18541910253192,13.9895280827967));
#70427=CARTESIAN_POINT('Ctrl Pts',(-3.31708660623242,7.18198612019348,13.9898596597143));
#70428=CARTESIAN_POINT('Ctrl Pts',(-3.33906716957666,7.17180648749431,13.9908408840315));
#70429=CARTESIAN_POINT('Ctrl Pts',(-3.35358949291768,7.16502724109791,13.9914917859102));
#70430=CARTESIAN_POINT('Ctrl Pts',(-3.46699352433759,7.11166817130854,13.9965946310388));
#70431=CARTESIAN_POINT('Ctrl Pts',(-3.56491873156037,7.06308867132844,14.0011198256364));
#70432=CARTESIAN_POINT('Ctrl Pts',(-3.92791176111297,6.87354005795813,14.0182716057813));
#70433=CARTESIAN_POINT('Ctrl Pts',(-4.18588943512417,6.71955101106894,14.0312174971903));
#70434=CARTESIAN_POINT('Ctrl Pts',(-4.62733864500261,6.42073915520068,14.0542418758444));
#70435=CARTESIAN_POINT('Ctrl Pts',(-4.81433589561284,6.28174547402739,14.0643044833392));
#70436=CARTESIAN_POINT('Ctrl Pts',(-5.2929588896299,5.89204644265265,14.0907438012491));
#70437=CARTESIAN_POINT('Ctrl Pts',(-5.57291658280146,5.62798768354655,14.106909344237));
#70438=CARTESIAN_POINT('Ctrl Pts',(-6.03317027384588,5.12571294755363,14.1350405623342));
#70439=CARTESIAN_POINT('Ctrl Pts',(-6.22128262891421,4.89568423554769,14.1471474375716));
#70440=CARTESIAN_POINT('Ctrl Pts',(-6.43660198069764,4.59987296973472,14.1619778642588));
#70441=CARTESIAN_POINT('Ctrl Pts',(-6.47645402657645,4.54359105927815,14.1647665498412));
#70442=CARTESIAN_POINT('Ctrl Pts',(-6.53445206264249,4.45936836077071,14.1688911910025));
#70443=CARTESIAN_POINT('Ctrl Pts',(-6.55316552531535,4.43182259834525,14.1702326423048));
#70444=CARTESIAN_POINT('Ctrl Pts',(-6.58630364509432,4.38237526675871,14.1726272915516));
#70445=CARTESIAN_POINT('Ctrl Pts',(-6.60079436457796,4.36051859821404,14.1736811482571));
#70446=CARTESIAN_POINT('Ctrl Pts',(-6.6285553272511,4.31819064185481,14.1757132065426));
#70447=CARTESIAN_POINT('Ctrl Pts',(-6.64184007920961,4.2977292273864,14.1766915496187));
#70448=CARTESIAN_POINT('Ctrl Pts',(-6.67053604489903,4.2530803414051,14.1788178566927));
#70449=CARTESIAN_POINT('Ctrl Pts',(-6.68591081478279,4.22886983719592,14.1799654227316));
#70450=CARTESIAN_POINT('Ctrl Pts',(-6.74606033479842,4.13300496208066,14.18448828381));
#70451=CARTESIAN_POINT('Ctrl Pts',(-6.78981779721852,4.06071847143417,14.187852450383));
#70452=CARTESIAN_POINT('Ctrl Pts',(-6.9518038119753,3.78317944427748,14.2006008887999));
#70453=CARTESIAN_POINT('Ctrl Pts',(-7.06195251964445,3.5733531414311,14.2098917535242));
#70454=CARTESIAN_POINT('Ctrl Pts',(-7.25126217980454,3.16966882281385,14.2272552711131));
#70455=CARTESIAN_POINT('Ctrl Pts',(-7.33246878775492,2.9769961361698,14.2353365447301));
#70456=CARTESIAN_POINT('Ctrl Pts',(-7.43576586967369,2.70194349037944,14.2466936980983));
#70457=CARTESIAN_POINT('Ctrl Pts',(-7.46430252799417,2.62207941174306,14.2499709647801));
#70458=CARTESIAN_POINT('Ctrl Pts',(-7.59569624133899,2.23481316966507,14.2657946939803));
#70459=CARTESIAN_POINT('Ctrl Pts',(-7.68087562455405,1.92175157049473,14.2783729672968));
#70460=CARTESIAN_POINT('Ctrl Pts',(-7.75232917856588,1.57673995305073,14.2924655405697));
#70461=CARTESIAN_POINT('Ctrl Pts',(-7.75790158680702,1.54908990318224,14.2935966034708));
#70462=CARTESIAN_POINT('Ctrl Pts',(-7.76604301512412,1.50754651239229,14.29529893697));
#70463=CARTESIAN_POINT('Ctrl Pts',(-7.76872289889706,1.49367503765232,14.2958678434983));
#70464=CARTESIAN_POINT('Ctrl Pts',(-7.7734253348885,1.46897951394598,14.2968816187653));
#70465=CARTESIAN_POINT('Ctrl Pts',(-7.77546247579389,1.45815826853639,14.297326163986));
#70466=CARTESIAN_POINT('Ctrl Pts',(-7.77934118168447,1.43731541513366,14.2981830619638));
#70467=CARTESIAN_POINT('Ctrl Pts',(-7.78118599136153,1.42729443028998,14.2985953400622));
#70468=CARTESIAN_POINT('Ctrl Pts',(-7.78512765935432,1.40564855573744,14.2994865465338));
#70469=CARTESIAN_POINT('Ctrl Pts',(-7.78721784540623,1.39402251145441,14.2999656296989));
#70470=CARTESIAN_POINT('Ctrl Pts',(-7.79225814712182,1.36562221892125,14.3011369976424));
#70471=CARTESIAN_POINT('Ctrl Pts',(-7.79518013244954,1.34884312483217,14.3018299367363));
#70472=CARTESIAN_POINT('Ctrl Pts',(-7.80934752160713,1.2659051096327,14.3052592022005));
#70473=CARTESIAN_POINT('Ctrl Pts',(-7.81980486559591,1.19961499648297,14.3080130139937));
#70474=CARTESIAN_POINT('Ctrl Pts',(-7.88353766025106,0.759277547792316,
14.326369812278));
#70475=CARTESIAN_POINT('Ctrl Pts',(-7.91079964517495,0.381969395142818,
14.3423822839279));
#70476=CARTESIAN_POINT('Ctrl Pts',(-7.9109988997264,0.00417235277290443,
14.3582990582019));
#70477=CARTESIAN_POINT('',(-7.90819530369822,-0.000235767854399078,16.3575721401914));
#70478=CARTESIAN_POINT('Ctrl Pts',(-7.90990495318262,0.00414520974019739,
14.3576684917631));
#70479=CARTESIAN_POINT('Ctrl Pts',(-7.90763939544643,-0.844290181882231,
14.3918532068026));
#70480=CARTESIAN_POINT('Ctrl Pts',(-7.55560401264065,-3.01018261765953,
14.4789591888192));
#70481=CARTESIAN_POINT('Ctrl Pts',(-4.90838355554223,-7.20519306720496,
14.6719077047901));
#70482=CARTESIAN_POINT('Ctrl Pts',(2.27684130052813,-9.07257823005059,14.9365140396761));
#70483=CARTESIAN_POINT('Ctrl Pts',(8.87314431977926,-2.98208636427268,15.2540416415389));
#70484=CARTESIAN_POINT('Ctrl Pts',(7.55975124971049,4.34219026825647,15.518647976425));
#70485=CARTESIAN_POINT('Ctrl Pts',(3.20850006480449,7.5750851400838,15.7303330443335));
#70486=CARTESIAN_POINT('Ctrl Pts',(-2.16791332744556,8.4515283681303,15.9420181122423));
#70487=CARTESIAN_POINT('Ctrl Pts',(-7.00166927530617,5.16152017814356,16.1510978108616));
#70488=CARTESIAN_POINT('Ctrl Pts',(-7.91003961585176,1.25389860036366,16.3072562425037));
#70489=CARTESIAN_POINT('Ctrl Pts',(-7.90819530369822,-0.000235767854399078,
16.3575721401914));
#70490=CARTESIAN_POINT('',(-7.91099999795386,-0.000179927557964477,20.3534744230576));
#70491=CARTESIAN_POINT('Ctrl Pts',(-7.91099999818148,-0.000169625007045761,
16.3591892934433));
#70492=CARTESIAN_POINT('Ctrl Pts',(-7.91099702810346,-0.138688629851337,
16.3648599814544));
#70493=CARTESIAN_POINT('Ctrl Pts',(-7.90735590079701,-0.277186163552383,
16.3705089826685));
#70494=CARTESIAN_POINT('Ctrl Pts',(-7.89566147356344,-0.499527941317111,
16.3795600850917));
#70495=CARTESIAN_POINT('Ctrl Pts',(-7.88990300868537,-0.583462861242157,
16.3829714920976));
#70496=CARTESIAN_POINT('Ctrl Pts',(-7.87986244070676,-0.702073691726116,
16.387784110266));
#70497=CARTESIAN_POINT('Ctrl Pts',(-7.87668778112999,-0.736837269673295,
16.3891936542688));
#70498=CARTESIAN_POINT('Ctrl Pts',(-7.87072527718944,-0.797679381472114,
16.391658891131));
#70499=CARTESIAN_POINT('Ctrl Pts',(-7.86803764990721,-0.823767156926277,
16.3927153825496));
#70500=CARTESIAN_POINT('Ctrl Pts',(-7.86252930117675,-0.874746540085974,
16.3947788755023));
#70501=CARTESIAN_POINT('Ctrl Pts',(-7.859719973982,-0.899639069822063,16.395785961393));
#70502=CARTESIAN_POINT('Ctrl Pts',(-7.85391791030823,-0.948946510252506,
16.397779873353));
#70503=CARTESIAN_POINT('Ctrl Pts',(-7.85092944394953,-0.973361644653989,
16.39876672544));
#70504=CARTESIAN_POINT('Ctrl Pts',(-7.84360537018038,-1.03096860616319,
16.4010941542709));
#70505=CARTESIAN_POINT('Ctrl Pts',(-7.83917286517155,-1.06414767311025,
16.4024338441374));
#70506=CARTESIAN_POINT('Ctrl Pts',(-7.82282553032091,-1.18086502861993,
16.4071440094059));
#70507=CARTESIAN_POINT('Ctrl Pts',(-7.8097847811458,-1.26424021908153,16.4105038977454));
#70508=CARTESIAN_POINT('Ctrl Pts',(-7.76685881046335,-1.51259098135986,
16.4205026969115));
#70509=CARTESIAN_POINT('Ctrl Pts',(-7.73306062228825,-1.67684282546261,
16.427102509766));
#70510=CARTESIAN_POINT('Ctrl Pts',(-7.56912444529879,-2.36238953531032,
16.4546830847381));
#70511=CARTESIAN_POINT('Ctrl Pts',(-7.39128540198393,-2.87078667416051,
16.475140701656));
#70512=CARTESIAN_POINT('Ctrl Pts',(-7.09711954390062,-3.49844828073813,
16.5022715884294));
#70513=CARTESIAN_POINT('Ctrl Pts',(-7.02677112315478,-3.63768223284488,
16.5084248019897));
#70514=CARTESIAN_POINT('Ctrl Pts',(-6.94373720427147,-3.79061483349588,
16.5153920383527));
#70515=CARTESIAN_POINT('Ctrl Pts',(-6.93506536196415,-3.80645709283556,
16.5161163256904));
#70516=CARTESIAN_POINT('Ctrl Pts',(-6.92037229639406,-3.83308241562713,
16.5173380451424));
#70517=CARTESIAN_POINT('Ctrl Pts',(-6.91437992174831,-3.84388134861235,
16.517834797546));
#70518=CARTESIAN_POINT('Ctrl Pts',(-6.90331006903885,-3.8637208235337,16.5187497427036));
#70519=CARTESIAN_POINT('Ctrl Pts',(-6.89824005400551,-3.8727655064668,16.5191677526948));
#70520=CARTESIAN_POINT('Ctrl Pts',(-6.88832730817703,-3.89036818134578,
16.5199830515246));
#70521=CARTESIAN_POINT('Ctrl Pts',(-6.88348637337637,-3.89892716499044,
16.5203802946748));
#70522=CARTESIAN_POINT('Ctrl Pts',(-6.87215987251667,-3.91886606705995,
16.5213076503013));
#70523=CARTESIAN_POINT('Ctrl Pts',(-6.86566198309094,-3.93023893641888,
16.5218380807621));
#70524=CARTESIAN_POINT('Ctrl Pts',(-6.84687391321031,-3.96293379858266,
16.5233673273332));
#70525=CARTESIAN_POINT('Ctrl Pts',(-6.83451252399377,-3.98421450451254,
16.5243680892133));
#70526=CARTESIAN_POINT('Ctrl Pts',(-6.73564155043303,-4.15261134221547,
16.532329031178));
#70527=CARTESIAN_POINT('Ctrl Pts',(-6.6444927364507,-4.29694797612673,16.5394052933685));
#70528=CARTESIAN_POINT('Ctrl Pts',(-6.31328910573177,-4.78565053455505,
16.564088017228));
#70529=CARTESIAN_POINT('Ctrl Pts',(-6.0505532695961,-5.11379327346394,16.5819190240991));
#70530=CARTESIAN_POINT('Ctrl Pts',(-5.62491406399624,-5.56640879857414,
16.6078912520514));
#70531=CARTESIAN_POINT('Ctrl Pts',(-5.4812367991102,-5.7079427972747,16.6162505186416));
#70532=CARTESIAN_POINT('Ctrl Pts',(-5.27246869853824,-5.89843680842886,
16.6278437875401));
#70533=CARTESIAN_POINT('Ctrl Pts',(-5.21179429089689,-5.95211587797516,
16.6311520188961));
#70534=CARTESIAN_POINT('Ctrl Pts',(-5.10385257482604,-6.0446964530064,16.6369335892106));
#70535=CARTESIAN_POINT('Ctrl Pts',(-5.05693840622139,-6.08399871420263,
16.6394130929294));
#70536=CARTESIAN_POINT('Ctrl Pts',(-4.98761386913091,-6.14071932874993,
16.6430298534107));
#70537=CARTESIAN_POINT('Ctrl Pts',(-4.96555852829936,-6.15856756821716,
16.6441736540967));
#70538=CARTESIAN_POINT('Ctrl Pts',(-4.92730165749428,-6.18918774583637,
16.6461460400135));
#70539=CARTESIAN_POINT('Ctrl Pts',(-4.91114533206358,-6.2020156487724,16.6469754561016));
#70540=CARTESIAN_POINT('Ctrl Pts',(-4.87883630728768,-6.22746316244811,
16.6486271330586));
#70541=CARTESIAN_POINT('Ctrl Pts',(-4.86268436924029,-6.24008348350396,
16.6494493994557));
#70542=CARTESIAN_POINT('Ctrl Pts',(-4.81988491349509,-6.27325776307819,
16.6516192904687));
#70543=CARTESIAN_POINT('Ctrl Pts',(-4.79315493287898,-6.29370473915348,
16.6529653660239));
#70544=CARTESIAN_POINT('Ctrl Pts',(-4.6966830559512,-6.36652939223119,16.6577916797023));
#70545=CARTESIAN_POINT('Ctrl Pts',(-4.62620618402064,-6.41792371226835,
16.6612581834255));
#70546=CARTESIAN_POINT('Ctrl Pts',(-3.88575563128781,-6.93935213906297,
16.6971122496134));
#70547=CARTESIAN_POINT('Ctrl Pts',(-3.14749277660903,-7.30391137957557,
16.728279656686));
#70548=CARTESIAN_POINT('Ctrl Pts',(-2.00280354864637,-7.66276491964995,
16.7731609227091));
#70549=CARTESIAN_POINT('Ctrl Pts',(-1.63136414884033,-7.75034328118297,
16.7873270927641));
#70550=CARTESIAN_POINT('Ctrl Pts',(-1.11848195793934,-7.83275549591297,
16.8073858368042));
#70551=CARTESIAN_POINT('Ctrl Pts',(-0.981339535757896,-7.85111655824607,
16.812800484503));
#70552=CARTESIAN_POINT('Ctrl Pts',(-0.825697836469471,-7.86781260507817,
16.8190559927588));
#70553=CARTESIAN_POINT('Ctrl Pts',(-0.807598761753455,-7.86969099393013,
16.8197851165736));
#70554=CARTESIAN_POINT('Ctrl Pts',(-0.780366014791391,-7.87242237377243,
16.8208849029204));
#70555=CARTESIAN_POINT('Ctrl Pts',(-0.771237016371916,-7.8733219553073,
16.8212540327628));
#70556=CARTESIAN_POINT('Ctrl Pts',(-0.755519377502438,-7.87484318998133,
16.8218903866215));
#70557=CARTESIAN_POINT('Ctrl Pts',(-0.748931473157895,-7.87547245851339,
16.8221573543464));
#70558=CARTESIAN_POINT('Ctrl Pts',(-0.735347293658637,-7.87675280363303,
16.8227083566559));
#70559=CARTESIAN_POINT('Ctrl Pts',(-0.728350927388893,-7.8774028269485,
16.8229924269215));
#70560=CARTESIAN_POINT('Ctrl Pts',(-0.709474536288181,-7.87913124528543,
16.8237596381439));
#70561=CARTESIAN_POINT('Ctrl Pts',(-0.697592948207542,-7.8801920899717,
16.8242433879757));
#70562=CARTESIAN_POINT('Ctrl Pts',(-0.653834811043981,-7.88399928319668,
16.8260281606536));
#70563=CARTESIAN_POINT('Ctrl Pts',(-0.621944335365847,-7.88657909766544,
16.8273351214225));
#70564=CARTESIAN_POINT('Ctrl Pts',(-0.0903071567596755,-7.92634183716924,
16.8492374933701));
#70565=CARTESIAN_POINT('Ctrl Pts',(0.411734134838231,-7.91614184292397,
16.872006878316));
#70566=CARTESIAN_POINT('Ctrl Pts',(1.24217752392004,-7.82005078107087,16.9103094987087));
#70567=CARTESIAN_POINT('Ctrl Pts',(1.57226479924577,-7.76042510119439,16.9256856146406));
#70568=CARTESIAN_POINT('Ctrl Pts',(2.28209549621272,-7.58504030034019,16.9583254813782));
#70569=CARTESIAN_POINT('Ctrl Pts',(2.65895724579031,-7.46128669114439,16.9753637315994));
#70570=CARTESIAN_POINT('Ctrl Pts',(3.05365971936996,-7.29794803104929,16.992733206555));
#70571=CARTESIAN_POINT('Ctrl Pts',(3.08225116141491,-7.28591867589262,16.9939888831089));
#70572=CARTESIAN_POINT('Ctrl Pts',(3.12169079924542,-7.26905142348819,16.9957175600027));
#70573=CARTESIAN_POINT('Ctrl Pts',(3.13259977252125,-7.26435686831149,16.9961953464088));
#70574=CARTESIAN_POINT('Ctrl Pts',(3.15099891434594,-7.25638984977537,16.9970005751208));
#70575=CARTESIAN_POINT('Ctrl Pts',(3.15849464116724,-7.25313031817039,16.9973284506703));
#70576=CARTESIAN_POINT('Ctrl Pts',(3.17331759029196,-7.24665719390785,16.9979764953645));
#70577=CARTESIAN_POINT('Ctrl Pts',(3.18064501428476,-7.24344409162011,16.9982966804312));
#70578=CARTESIAN_POINT('Ctrl Pts',(3.19678381663278,-7.23633795681649,16.9990015390025));
#70579=CARTESIAN_POINT('Ctrl Pts',(3.20559299097138,-7.23243993218401,16.9993860436491));
#70580=CARTESIAN_POINT('Ctrl Pts',(3.23633073649572,-7.21877141119608,17.0007268822206));
#70581=CARTESIAN_POINT('Ctrl Pts',(3.25822203453082,-7.20891715236306,17.001680381894));
#70582=CARTESIAN_POINT('Ctrl Pts',(3.47876496686351,-7.10843103539184,17.0112722642425));
#70583=CARTESIAN_POINT('Ctrl Pts',(3.67363570175245,-7.00970805591823,17.0196280194292));
#70584=CARTESIAN_POINT('Ctrl Pts',(4.1872412039892,-6.72220222693817,17.04148233463));
#70585=CARTESIAN_POINT('Ctrl Pts',(4.49721821290795,-6.51889893336964,17.0544703233563));
#70586=CARTESIAN_POINT('Ctrl Pts',(5.20527690965082,-5.9798841755385,17.0850167760022));
#70587=CARTESIAN_POINT('Ctrl Pts',(5.58668393047818,-5.62519541838529,17.1022049095917));
#70588=CARTESIAN_POINT('Ctrl Pts',(6.03743088833185,-5.11462943019445,17.1269185787962));
#70589=CARTESIAN_POINT('Ctrl Pts',(6.14058355596565,-4.99031408046956,17.1329406386608));
#70590=CARTESIAN_POINT('Ctrl Pts',(6.28155261096253,-4.80943025078405,17.1418374071634));
#70591=CARTESIAN_POINT('Ctrl Pts',(6.32255993577157,-4.75539250875926,17.1445115868247));
#70592=CARTESIAN_POINT('Ctrl Pts',(6.36894726810647,-4.69260443965641,17.1476451825453));
#70593=CARTESIAN_POINT('Ctrl Pts',(6.37501235210579,-4.68436156158629,17.1480570809009));
#70594=CARTESIAN_POINT('Ctrl Pts',(6.38416935597897,-4.67186582437189,17.1486823119456));
#70595=CARTESIAN_POINT('Ctrl Pts',(6.38727307773992,-4.66762158672706,17.1488948168666));
#70596=CARTESIAN_POINT('Ctrl Pts',(6.39284633457129,-4.65998437266837,17.1492774659704));
#70597=CARTESIAN_POINT('Ctrl Pts',(6.39531740808339,-4.65659251606692,17.1494475013763));
#70598=CARTESIAN_POINT('Ctrl Pts',(6.4006107549468,-4.64931457642787,17.1498125495163));
#70599=CARTESIAN_POINT('Ctrl Pts',(6.40343218919807,-4.64542788826497,17.1500076216993));
#70600=CARTESIAN_POINT('Ctrl Pts',(6.41102302813513,-4.63495101490992,17.1505337916938));
#70601=CARTESIAN_POINT('Ctrl Pts',(6.41578580199248,-4.62835604940675,17.1508653636647));
#70602=CARTESIAN_POINT('Ctrl Pts',(6.43756895737701,-4.59809489915312,17.1523884874238));
#70603=CARTESIAN_POINT('Ctrl Pts',(6.45446841460836,-4.57434238152234,17.1535887605723));
#70604=CARTESIAN_POINT('Ctrl Pts',(6.73467368021476,-4.17586408957423,17.1737952787741));
#70605=CARTESIAN_POINT('Ctrl Pts',(6.96506024633229,-3.77909177602197,17.1949036364035));
#70606=CARTESIAN_POINT('Ctrl Pts',(7.28429701470246,-3.0997744242288,17.2297629008882));
#70607=CARTESIAN_POINT('Ctrl Pts',(7.39398690718939,-2.82817096907393,17.2434048336608));
#70608=CARTESIAN_POINT('Ctrl Pts',(7.58545761683625,-2.26613914600669,17.2704729157486));
#70609=CARTESIAN_POINT('Ctrl Pts',(7.66619988865757,-1.97584361723614,17.2838583388304));
#70610=CARTESIAN_POINT('Ctrl Pts',(7.76536433583358,-1.51999954895285,17.3037604201321));
#70611=CARTESIAN_POINT('Ctrl Pts',(7.79544894919056,-1.35729962154772,17.3106524319193));
#70612=CARTESIAN_POINT('Ctrl Pts',(7.8236939273539,-1.17226595175835,17.3182540366684));
#70613=CARTESIAN_POINT('Ctrl Pts',(7.82688755578149,-1.15074989912175,17.3191343941096));
#70614=CARTESIAN_POINT('Ctrl Pts',(7.8324640516627,-1.11208259908737,17.320710150935));
#70615=CARTESIAN_POINT('Ctrl Pts',(7.83487941760931,-1.09493622856667,17.3214066493033));
#70616=CARTESIAN_POINT('Ctrl Pts',(7.83845155346,-1.06896095636231,17.3224584086927));
#70617=CARTESIAN_POINT('Ctrl Pts',(7.8396497368357,-1.06013786208114,17.3228150736291));
#70618=CARTESIAN_POINT('Ctrl Pts',(7.84169604593879,-1.04487621126205,17.3234309960499));
#70619=CARTESIAN_POINT('Ctrl Pts',(7.84255114299337,-1.03843860846858,17.3236904896607));
#70620=CARTESIAN_POINT('Ctrl Pts',(7.84430618695515,-1.02509993644775,17.324227514181));
#70621=CARTESIAN_POINT('Ctrl Pts',(7.84520495632541,-1.01819871732988,17.3245050049444));
#70622=CARTESIAN_POINT('Ctrl Pts',(7.84736355331006,-1.00145134463913,17.3251775352615));
#70623=CARTESIAN_POINT('Ctrl Pts',(7.84861395983336,-0.991603975401235,
17.3255722553875));
#70624=CARTESIAN_POINT('Ctrl Pts',(7.85321706983824,-0.954798732396256,
17.3270448574326));
#70625=CARTESIAN_POINT('Ctrl Pts',(7.85644946406174,-0.92782584786468,17.3281186641683));
#70626=CARTESIAN_POINT('Ctrl Pts',(7.90865925038612,-0.472310356602522,
17.3461633498642));
#70627=CARTESIAN_POINT('Ctrl Pts',(7.9226502100186,-0.0404622924064998,
17.3618699252433));
#70628=CARTESIAN_POINT('Ctrl Pts',(7.87595141836899,0.904661507713193,17.3947809663055));
#70629=CARTESIAN_POINT('Ctrl Pts',(7.80040147377598,1.41517678471952,17.4115913930652));
#70630=CARTESIAN_POINT('Ctrl Pts',(7.63061198213414,2.09583566924965,17.4360565856003));
#70631=CARTESIAN_POINT('Ctrl Pts',(7.57903745982945,2.27529150654023,17.4427206575297));
#70632=CARTESIAN_POINT('Ctrl Pts',(7.48150276259319,2.5743744947767,17.4544438171782));
#70633=CARTESIAN_POINT('Ctrl Pts',(7.43889570300004,2.69501673808782,17.4593467960221));
#70634=CARTESIAN_POINT('Ctrl Pts',(7.38565548057392,2.83486967331362,17.4652951046804));
#70635=CARTESIAN_POINT('Ctrl Pts',(7.37784293489364,2.85514037341621,17.4661638555165));
#70636=CARTESIAN_POINT('Ctrl Pts',(7.36747092639055,2.88172510143414,17.4673122021937));
#70637=CARTESIAN_POINT('Ctrl Pts',(7.36498658808689,2.8880685532803,17.4675868865842));
#70638=CARTESIAN_POINT('Ctrl Pts',(7.36090454050823,2.89845203859809,17.4680376301149));
#70639=CARTESIAN_POINT('Ctrl Pts',(7.35931169140283,2.90249397986553,17.4682133667684));
#70640=CARTESIAN_POINT('Ctrl Pts',(7.35621362150004,2.91033655535251,17.4685548839712));
#70641=CARTESIAN_POINT('Ctrl Pts',(7.35470878239149,2.91413734004587,17.4687206394324));
#70642=CARTESIAN_POINT('Ctrl Pts',(7.35122063214955,2.92292747852222,17.4691045473338));
#70643=CARTESIAN_POINT('Ctrl Pts',(7.34923518834108,2.92791597785922,17.4693228388062));
#70644=CARTESIAN_POINT('Ctrl Pts',(7.34300010021262,2.94353556254634,17.4700076409165));
#70645=CARTESIAN_POINT('Ctrl Pts',(7.33873247227389,2.954159402831,17.4704753129156));
#70646=CARTESIAN_POINT('Ctrl Pts',(7.30150956009607,3.04624375538912,17.4745451732579));
#70647=CARTESIAN_POINT('Ctrl Pts',(7.26722336194286,3.12715626855057,17.4782314601976));
#70648=CARTESIAN_POINT('Ctrl Pts',(7.22334557379982,3.22608338243671,17.4828594515673));
#70649=CARTESIAN_POINT('Ctrl Pts',(7.21502159476869,3.24465693763958,17.4837336669822));
#70650=CARTESIAN_POINT('Ctrl Pts',(7.19415050125701,3.29074980925187,17.4859159926649));
#70651=CARTESIAN_POINT('Ctrl Pts',(7.18151714380436,3.31822953011595,17.4872284779585));
#70652=CARTESIAN_POINT('Ctrl Pts',(7.00721425272674,3.69171004288188,17.505215827643));
#70653=CARTESIAN_POINT('Ctrl Pts',(6.82086301693795,4.02561370088062,17.5230257312923));
#70654=CARTESIAN_POINT('Ctrl Pts',(6.35137969424957,4.74000152318988,17.5631520154991));
#70655=CARTESIAN_POINT('Ctrl Pts',(6.05666676107285,5.11121240409239,17.5854105581209));
#70656=CARTESIAN_POINT('Ctrl Pts',(5.48321881064938,5.7137491525905,17.6225408925745));
#70657=CARTESIAN_POINT('Ctrl Pts',(5.21849290152389,5.95650873577452,17.6378732339556));
#70658=CARTESIAN_POINT('Ctrl Pts',(4.92105304906423,6.19416161396239,17.6532903018575));
#70659=CARTESIAN_POINT('Ctrl Pts',(4.90387605468125,6.20776939506738,17.6541747285777));
#70660=CARTESIAN_POINT('Ctrl Pts',(4.87873881765007,6.22751391500264,17.6554604979247));
#70661=CARTESIAN_POINT('Ctrl Pts',(4.8708231464093,6.23370707442999,17.655864159489));
#70662=CARTESIAN_POINT('Ctrl Pts',(4.8569165970475,6.24454478973123,17.6565711888736));
#70663=CARTESIAN_POINT('Ctrl Pts',(4.85093081432213,6.24919584400352,17.6568748224422));
#70664=CARTESIAN_POINT('Ctrl Pts',(4.83930040894617,6.25820608608209,17.6574634451409));
#70665=CARTESIAN_POINT('Ctrl Pts',(4.83365656032202,6.26256625682203,17.6577484742177));
#70666=CARTESIAN_POINT('Ctrl Pts',(4.82017742648523,6.27295052253683,17.6584277557478));
#70667=CARTESIAN_POINT('Ctrl Pts',(4.81233672380333,6.27896758541555,17.6588217224322));
#70668=CARTESIAN_POINT('Ctrl Pts',(4.78862743881198,6.29709191996949,17.6600095252908));
#70669=CARTESIAN_POINT('Ctrl Pts',(4.77272423632373,6.30915388684902,17.6608015302592));
#70670=CARTESIAN_POINT('Ctrl Pts',(4.61018975181843,6.43146380920138,17.6688483969515));
#70671=CARTESIAN_POINT('Ctrl Pts',(4.45980660161947,6.53664338324402,17.6758982292768));
#70672=CARTESIAN_POINT('Ctrl Pts',(4.15740369424774,6.73284840960087,17.6894011334408));
#70673=CARTESIAN_POINT('Ctrl Pts',(4.0057161314352,6.82418457566719,17.6958627333373));
#70674=CARTESIAN_POINT('Ctrl Pts',(3.37278812031355,7.17691032472051,17.7218145940418));
#70675=CARTESIAN_POINT('Ctrl Pts',(2.8681323167152,7.39307311013705,17.7400876528261));
#70676=CARTESIAN_POINT('Ctrl Pts',(2.05715598890869,7.64480224006212,17.7701564873003));
#70677=CARTESIAN_POINT('Ctrl Pts',(1.76422260143587,7.71766881886595,17.7811900259877));
#70678=CARTESIAN_POINT('Ctrl Pts',(1.42487295648765,7.78174597191026,17.7948069529935));
#70679=CARTESIAN_POINT('Ctrl Pts',(1.38183633622384,7.78950329269495,17.7965472355436));
#70680=CARTESIAN_POINT('Ctrl Pts',(1.32703189787337,7.79891328456964,17.7987787778896));
#70681=CARTESIAN_POINT('Ctrl Pts',(1.31532109862832,7.80089690251622,17.7992565139291));
#70682=CARTESIAN_POINT('Ctrl Pts',(1.29657599491621,7.80402860634351,17.8000225991004));
#70683=CARTESIAN_POINT('Ctrl Pts',(1.289544501767,7.80519357714808,17.8003102783273));
#70684=CARTESIAN_POINT('Ctrl Pts',(1.27623398435503,7.80738037292326,17.8008554320334));
#70685=CARTESIAN_POINT('Ctrl Pts',(1.26995527982548,7.80840412999174,17.8011128310155));
#70686=CARTESIAN_POINT('Ctrl Pts',(1.25575353898104,7.81070217379605,17.8016955836962));
#70687=CARTESIAN_POINT('Ctrl Pts',(1.24782979135952,7.81197197957118,17.8020211088937));
#70688=CARTESIAN_POINT('Ctrl Pts',(1.22749853342217,7.81519840601153,17.8028573254095));
#70689=CARTESIAN_POINT('Ctrl Pts',(1.21508829568487,7.81713753277578,17.8033686731912));
#70690=CARTESIAN_POINT('Ctrl Pts',(1.14330075726487,7.82817941188841,17.806331737665));
#70691=CARTESIAN_POINT('Ctrl Pts',(1.08382678987283,7.83663504259709,17.8088069136173));
#70692=CARTESIAN_POINT('Ctrl Pts',(0.335215391968185,7.93438298243581,17.8401798896467));
#70693=CARTESIAN_POINT('Ctrl Pts',(-0.36268576712055,7.9331773453036,17.8714463155295));
#70694=CARTESIAN_POINT('Ctrl Pts',(-1.42384920662199,7.79087618750982,17.9175715109498));
#70695=CARTESIAN_POINT('Ctrl Pts',(-1.79223564925196,7.71446808135062,17.9333744887431));
#70696=CARTESIAN_POINT('Ctrl Pts',(-2.22245126700878,7.59274124496653,17.9516120691243));
#70697=CARTESIAN_POINT('Ctrl Pts',(-2.29082339836031,7.57239312040085,17.9545048388973));
#70698=CARTESIAN_POINT('Ctrl Pts',(-2.38146509711709,7.54407736541356,17.9583343337344));
#70699=CARTESIAN_POINT('Ctrl Pts',(-2.40398707191292,7.5369307724812,17.9592853832973));
#70700=CARTESIAN_POINT('Ctrl Pts',(-2.44074081429855,7.52508670181965,17.9608366093582));
#70701=CARTESIAN_POINT('Ctrl Pts',(-2.45499180498145,7.5204495099541,17.961437889352));
#70702=CARTESIAN_POINT('Ctrl Pts',(-2.48248703952698,7.51141623334938,17.9625975896548));
#70703=CARTESIAN_POINT('Ctrl Pts',(-2.49573299446361,7.50702554637102,17.96315610853));
#70704=CARTESIAN_POINT('Ctrl Pts',(-2.52618374703081,7.49684241734209,17.9644396745417));
#70705=CARTESIAN_POINT('Ctrl Pts',(-2.5433803798618,7.49102575091314,17.9651642577805));
#70706=CARTESIAN_POINT('Ctrl Pts',(-2.59813354089362,7.47229552044047,17.9674703621151));
#70707=CARTESIAN_POINT('Ctrl Pts',(-2.635613070304,7.45915826482264,17.9690475305864));
#70708=CARTESIAN_POINT('Ctrl Pts',(-3.03496554567734,7.31579223334455,17.9858381527423));
#70709=CARTESIAN_POINT('Ctrl Pts',(-3.38699055211238,7.15961963885377,18.0004715540782));
#70710=CARTESIAN_POINT('Ctrl Pts',(-4.13058380294964,6.76256384061525,18.0317019445917));
#70711=CARTESIAN_POINT('Ctrl Pts',(-4.51535159556521,6.51195652307564,18.048062185909));
#70712=CARTESIAN_POINT('Ctrl Pts',(-5.07640921246084,6.07277544297216,18.0743971781));
#70713=CARTESIAN_POINT('Ctrl Pts',(-5.2688895764366,5.90654900197727,18.0839712595894));
#70714=CARTESIAN_POINT('Ctrl Pts',(-5.47928471007736,5.7063713520879,18.0954598621463));
#70715=CARTESIAN_POINT('Ctrl Pts',(-5.5053735585937,5.68120558186405,18.0969035748097));
#70716=CARTESIAN_POINT('Ctrl Pts',(-5.53857482387999,5.64873559267836,18.0987669027846));
#70717=CARTESIAN_POINT('Ctrl Pts',(-5.54584761259681,5.64159544208592,18.0991766846171));
#70718=CARTESIAN_POINT('Ctrl Pts',(-5.55751462251857,5.63009684868889,18.0998366985648));
#70719=CARTESIAN_POINT('Ctrl Pts',(-5.56191757774558,5.62574725375826,18.1000863852519));
#70720=CARTESIAN_POINT('Ctrl Pts',(-5.57027409329137,5.61747261339971,18.1005614393047));
#70721=CARTESIAN_POINT('Ctrl Pts',(-5.57422862230835,5.61354854817251,18.1007867452334));
#70722=CARTESIAN_POINT('Ctrl Pts',(-5.58320722387668,5.60462027070444,18.1012994342072));
#70723=CARTESIAN_POINT('Ctrl Pts',(-5.58822871493128,5.59961347886257,18.1015869814342));
#70724=CARTESIAN_POINT('Ctrl Pts',(-5.60342206173172,5.58442381593077,18.1024594967923));
#70725=CARTESIAN_POINT('Ctrl Pts',(-5.61357282601606,5.5742199705936,18.10304582524));
#70726=CARTESIAN_POINT('Ctrl Pts',(-5.69468263256046,5.4922397755936,18.1077587137666));
#70727=CARTESIAN_POINT('Ctrl Pts',(-5.76428331940084,5.41914595231678,18.111979302164));
#70728=CARTESIAN_POINT('Ctrl Pts',(-6.41124964062997,4.71314268091962,18.1528039455147));
#70729=CARTESIAN_POINT('Ctrl Pts',(-6.88362467736341,3.99171133190357,18.1942800854542));
#70730=CARTESIAN_POINT('Ctrl Pts',(-7.37241183897025,2.8901229520899,18.2475761987917));
#70731=CARTESIAN_POINT('Ctrl Pts',(-7.49251825864636,2.56270861303139,18.2624197972734));
#70732=CARTESIAN_POINT('Ctrl Pts',(-7.59790735582282,2.20372119393185,18.2776139991284));
#70733=CARTESIAN_POINT('Ctrl Pts',(-7.60503602920081,2.1789929551116,18.2786553749989));
#70734=CARTESIAN_POINT('Ctrl Pts',(-7.6151111784191,2.14339208114612,18.2801471563036));
#70735=CARTESIAN_POINT('Ctrl Pts',(-7.61815526079389,2.13254737273164,18.2806005873791));
#70736=CARTESIAN_POINT('Ctrl Pts',(-7.62339806484694,2.11371511300971,18.2813862715456));
#70737=CARTESIAN_POINT('Ctrl Pts',(-7.62560741630043,2.10573055423663,18.2817188535643));
#70738=CARTESIAN_POINT('Ctrl Pts',(-7.62983134776988,2.09037150900919,18.2823575819921));
#70739=CARTESIAN_POINT('Ctrl Pts',(-7.63184778804856,2.08299754717225,18.2826637856598));
#70740=CARTESIAN_POINT('Ctrl Pts',(-7.63657262885299,2.06562021836922,18.283384315082));
#70741=CARTESIAN_POINT('Ctrl Pts',(-7.63927207055801,2.05561441795856,18.2837983634969));
#70742=CARTESIAN_POINT('Ctrl Pts',(-7.64853548242268,2.02100822291067,18.2852275440433));
#70743=CARTESIAN_POINT('Ctrl Pts',(-7.65500037772436,1.99638135003596,18.286239615371));
#70744=CARTESIAN_POINT('Ctrl Pts',(-7.72842126909674,1.71109649157515,18.2979069587214));
#70745=CARTESIAN_POINT('Ctrl Pts',(-7.78215622093737,1.44720632931898,18.3081436475568));
#70746=CARTESIAN_POINT('Ctrl Pts',(-7.88136205928372,0.790159333628197,
18.3325973940439));
#70747=CARTESIAN_POINT('Ctrl Pts',(-7.91100066395141,0.395357546547743,
18.3463792010137));
#70748=CARTESIAN_POINT('Ctrl Pts',(-7.91099895747553,-0.620768414657839,
18.3814975743519));
#70749=CARTESIAN_POINT('Ctrl Pts',(-7.83793470667573,-1.23935196704252,
18.4025337088538));
#70750=CARTESIAN_POINT('Ctrl Pts',(-7.68456469624239,-1.87957482020434,
18.4285148712731));
#70751=CARTESIAN_POINT('Ctrl Pts',(-7.67554038797965,-1.91609388168929,
18.4300107443672));
#70752=CARTESIAN_POINT('Ctrl Pts',(-7.66329653234707,-1.96416675474369,
18.4319970305218));
#70753=CARTESIAN_POINT('Ctrl Pts',(-7.66031058841938,-1.97577996499985,
18.4324781920922));
#70754=CARTESIAN_POINT('Ctrl Pts',(-7.65564393055039,-1.99376036024174,
18.4332251693793));
#70755=CARTESIAN_POINT('Ctrl Pts',(-7.65398164291206,-2.00013233939653,
18.4334902781251));
#70756=CARTESIAN_POINT('Ctrl Pts',(-7.65064297576142,-2.01286520378321,
18.434020807257));
#70757=CARTESIAN_POINT('Ctrl Pts',(-7.64896661480329,-2.01922608849729,
18.4342862267831));
#70758=CARTESIAN_POINT('Ctrl Pts',(-7.64521507037805,-2.03338946417253,
18.434878069516));
#70759=CARTESIAN_POINT('Ctrl Pts',(-7.64313587341957,-2.04119087917306,
18.4352046410989));
#70760=CARTESIAN_POINT('Ctrl Pts',(-7.63704606022468,-2.06390087579453,
18.4361569451007));
#70761=CARTESIAN_POINT('Ctrl Pts',(-7.6330037517108,-2.07880087396382,18.4367838240967));
#70762=CARTESIAN_POINT('Ctrl Pts',(-7.60364017823742,-2.18579494184249,
18.4412998184791));
#70763=CARTESIAN_POINT('Ctrl Pts',(-7.57669702925659,-2.27743382700996,
18.4452448418068));
#70764=CARTESIAN_POINT('Ctrl Pts',(-7.47936647338979,-2.58760577567366,
18.4588174027484));
#70765=CARTESIAN_POINT('Ctrl Pts',(-7.40113003448595,-2.80355051812288,
18.4686379817823));
#70766=CARTESIAN_POINT('Ctrl Pts',(-7.10545968553398,-3.52058524759278,
18.5020390327163));
#70767=CARTESIAN_POINT('Ctrl Pts',(-6.84558342480646,-4.00251392977768,
18.5256957681537));
#70768=CARTESIAN_POINT('Ctrl Pts',(-6.43888024955435,-4.59954643588493,
18.5559918399502));
#70769=CARTESIAN_POINT('Ctrl Pts',(-6.33477430618393,-4.74190284477679,
18.5633148542309));
#70770=CARTESIAN_POINT('Ctrl Pts',(-6.05189693576716,-5.10275410166161,
18.5822156708884));
#70771=CARTESIAN_POINT('Ctrl Pts',(-5.86603368768708,-5.31537478333532,
18.5937198703796));
#70772=CARTESIAN_POINT('Ctrl Pts',(-5.62382342421901,-5.56423986047458,
18.6077917217352));
#70773=CARTESIAN_POINT('Ctrl Pts',(-5.57786576639218,-5.61030914376227,
18.6104225724697));
#70774=CARTESIAN_POINT('Ctrl Pts',(-5.50776425937407,-5.67886799850951,
18.6143772501603));
#70775=CARTESIAN_POINT('Ctrl Pts',(-5.48403966757122,-5.70178198591922,
18.6157058252478));
#70776=CARTESIAN_POINT('Ctrl Pts',(-5.4412190988007,-5.74262498876983,18.6180863191342));
#70777=CARTESIAN_POINT('Ctrl Pts',(-5.42217608013372,-5.76060878757986,
18.6191388662858));
#70778=CARTESIAN_POINT('Ctrl Pts',(-5.3814100504924,-5.79872607438953,18.6213792009594));
#70779=CARTESIAN_POINT('Ctrl Pts',(-5.3596625628735,-5.81883282424091,18.6225666557676));
#70780=CARTESIAN_POINT('Ctrl Pts',(-5.30045254546596,-5.87296217717641,
18.6257790029644));
#70781=CARTESIAN_POINT('Ctrl Pts',(-5.26277556191809,-5.90674828833299,
18.6278009787152));
#70782=CARTESIAN_POINT('Ctrl Pts',(-5.0573190287319,-6.08746103216223,18.6387098973539));
#70783=CARTESIAN_POINT('Ctrl Pts',(-4.88370570197996,-6.22760620491813,
18.6475080789913));
#70784=CARTESIAN_POINT('Ctrl Pts',(-4.35866848654732,-6.61595463538525,
18.6730628800961));
#70785=CARTESIAN_POINT('Ctrl Pts',(-3.9926617600959,-6.84306214523772,18.6895562191977));
#70786=CARTESIAN_POINT('Ctrl Pts',(-3.38035122590235,-7.15707793102041,
18.7162559178597));
#70787=CARTESIAN_POINT('Ctrl Pts',(-3.14506579476865,-7.26354551726059,
18.726332984537));
#70788=CARTESIAN_POINT('Ctrl Pts',(-2.87843585220965,-7.36880885804074,
18.7377974326141));
#70789=CARTESIAN_POINT('Ctrl Pts',(-2.85181025247576,-7.37915409862963,
18.7389427961303));
#70790=CARTESIAN_POINT('Ctrl Pts',(-2.81186263547759,-7.39442704009274,
18.7406625114606));
#70791=CARTESIAN_POINT('Ctrl Pts',(-2.7985823400193,-7.39946346813889,18.7412344282876));
#70792=CARTESIAN_POINT('Ctrl Pts',(-2.77497344036099,-7.40834427272926,
18.7422515913481));
#70793=CARTESIAN_POINT('Ctrl Pts',(-2.76465021860639,-7.41220288617679,
18.7426965062654));
#70794=CARTESIAN_POINT('Ctrl Pts',(-2.74295896261043,-7.42025902381596,
18.7436317213732));
#70795=CARTESIAN_POINT('Ctrl Pts',(-2.73158928291619,-7.42445202283006,
18.7441221278759));
#70796=CARTESIAN_POINT('Ctrl Pts',(-2.70128219938187,-7.43554986406698,
18.7454299701171));
#70797=CARTESIAN_POINT('Ctrl Pts',(-2.68232810889937,-7.44240842803317,
18.7462485619804));
#70798=CARTESIAN_POINT('Ctrl Pts',(-2.57571836695739,-7.48052514631642,
18.7508564175114));
#70799=CARTESIAN_POINT('Ctrl Pts',(-2.48754383602839,-7.51030670182811,
18.7546805902781));
#70800=CARTESIAN_POINT('Ctrl Pts',(-1.71414275115884,-7.75641390476471,
18.7882642415646));
#70801=CARTESIAN_POINT('Ctrl Pts',(-1.00290549535961,-7.88000742256015,
18.819081944281));
#70802=CARTESIAN_POINT('Ctrl Pts',(-0.172974304941317,-7.90989956029704,
18.8531094984428));
#70803=CARTESIAN_POINT('Ctrl Pts',(-0.0611240664904855,-7.91155455823628,
18.8576638600065));
#70804=CARTESIAN_POINT('Ctrl Pts',(0.0880060991340752,-7.91059832630897,
18.8636988889013));
#70805=CARTESIAN_POINT('Ctrl Pts',(0.125285382710805,-7.91009573553948,
18.8652044268233));
#70806=CARTESIAN_POINT('Ctrl Pts',(0.183744452697223,-7.90889423075326,
18.8675607828463));
#70807=CARTESIAN_POINT('Ctrl Pts',(0.204927264084802,-7.90837371379046,
18.8684136815279));
#70808=CARTESIAN_POINT('Ctrl Pts',(0.245652796800963,-7.90720924371385,
18.8700517252497));
#70809=CARTESIAN_POINT('Ctrl Pts',(0.265195719170338,-7.90657792939589,
18.8708370110468));
#70810=CARTESIAN_POINT('Ctrl Pts',(0.311306212102885,-7.90491722455827,
18.8726881371742));
#70811=CARTESIAN_POINT('Ctrl Pts',(0.337871357212215,-7.90382634154128,
18.873753263055));
#70812=CARTESIAN_POINT('Ctrl Pts',(0.415896568159029,-7.90022818832662,
18.8768779993726));
#70813=CARTESIAN_POINT('Ctrl Pts',(0.467338373483844,-7.89735210512718,
18.8789334255746));
#70814=CARTESIAN_POINT('Ctrl Pts',(0.913984744327948,-7.86800095702388,
18.8967455356701));
#70815=CARTESIAN_POINT('Ctrl Pts',(1.30672606453444,-7.81238038356054,18.9122247141363));
#70816=CARTESIAN_POINT('Ctrl Pts',(2.30741323347474,-7.59306058693808,18.9518486290778));
#70817=CARTESIAN_POINT('Ctrl Pts',(2.90296219211652,-7.38590149261466,18.9751741379433));
#70818=CARTESIAN_POINT('Ctrl Pts',(3.65812523151308,-7.01761487599907,19.0066976603031));
#70819=CARTESIAN_POINT('Ctrl Pts',(3.84472186169952,-6.91714601369213,19.0146879414807));
#70820=CARTESIAN_POINT('Ctrl Pts',(4.15748119652173,-6.73217878418793,19.028674304431));
#70821=CARTESIAN_POINT('Ctrl Pts',(4.2856590217366,-6.65131605084177,19.0345883297743));
#70822=CARTESIAN_POINT('Ctrl Pts',(4.42822708541558,-6.55554233222859,19.0414454075995));
#70823=CARTESIAN_POINT('Ctrl Pts',(4.44497913926222,-6.54419520133423,19.0422556136045));
#70824=CARTESIAN_POINT('Ctrl Pts',(4.46951303763605,-6.52743931512137,19.0434490137914));
#70825=CARTESIAN_POINT('Ctrl Pts',(4.47732905250439,-6.52208060061623,19.0438302303607));
#70826=CARTESIAN_POINT('Ctrl Pts',(4.49120313822218,-6.51253173725278,19.0445087705006));
#70827=CARTESIAN_POINT('Ctrl Pts',(4.49726502838217,-6.50834714206152,19.0448058686449));
#70828=CARTESIAN_POINT('Ctrl Pts',(4.50988344543191,-6.49961045127315,19.0454256354309));
#70829=CARTESIAN_POINT('Ctrl Pts',(4.51643894314147,-6.49505688828202,19.0457483646651));
#70830=CARTESIAN_POINT('Ctrl Pts',(4.53341299362928,-6.48322829319567,19.0465859712395));
#70831=CARTESIAN_POINT('Ctrl Pts',(4.54382090749996,-6.47593808114644,19.0471014903024));
#70832=CARTESIAN_POINT('Ctrl Pts',(4.58795866855565,-6.44486304565221,19.0492960635452));
#70833=CARTESIAN_POINT('Ctrl Pts',(4.62151930947078,-6.42083979022933,19.0509855410284));
#70834=CARTESIAN_POINT('Ctrl Pts',(5.10456540682449,-6.06931833160826,19.0756251430737));
#70835=CARTESIAN_POINT('Ctrl Pts',(5.51838944790545,-5.6956422967183,19.10122066532));
#70836=CARTESIAN_POINT('Ctrl Pts',(6.32431783895333,-4.79697637723482,19.1565291787788));
#70837=CARTESIAN_POINT('Ctrl Pts',(6.69763130678205,-4.26027672490204,19.1857740695928));
#70838=CARTESIAN_POINT('Ctrl Pts',(7.02029585313811,-3.647066273651,19.2140679424585));
#70839=CARTESIAN_POINT('Ctrl Pts',(7.03934800413248,-3.61015595430483,19.2157539641006));
#70840=CARTESIAN_POINT('Ctrl Pts',(7.06435345568218,-3.56076149331376,19.2179877962457));
#70841=CARTESIAN_POINT('Ctrl Pts',(7.07056581696743,-3.54840967047123,19.2185445410687));
#70842=CARTESIAN_POINT('Ctrl Pts',(7.08020488044858,-3.52911883346136,19.2194111693633));
#70843=CARTESIAN_POINT('Ctrl Pts',(7.08365382150165,-3.5221909981392,19.2197218191441));
#70844=CARTESIAN_POINT('Ctrl Pts',(7.090220431135,-3.50895209243333,19.2203143604352));
#70845=CARTESIAN_POINT('Ctrl Pts',(7.09333985184895,-3.50264190227501,19.2205963121248));
#70846=CARTESIAN_POINT('Ctrl Pts',(7.10059678348885,-3.48791260187965,19.2212533361912));
#70847=CARTESIAN_POINT('Ctrl Pts',(7.10472775378018,-3.47949027092903,19.2216281832074));
#70848=CARTESIAN_POINT('Ctrl Pts',(7.11646149836042,-3.45545918461187,19.2226953197855));
#70849=CARTESIAN_POINT('Ctrl Pts',(7.12402790446088,-3.43983267841626,19.2233863584308));
#70850=CARTESIAN_POINT('Ctrl Pts',(7.17133596099948,-3.34130418368985,19.2277255090623));
#70851=CARTESIAN_POINT('Ctrl Pts',(7.2096821264332,-3.25773808857364,19.2313255735565));
#70852=CARTESIAN_POINT('Ctrl Pts',(7.31835108781493,-3.00959836498081,19.2417910353267));
#70853=CARTESIAN_POINT('Ctrl Pts',(7.3845578131383,-2.84328251513537,19.2485178402016));
#70854=CARTESIAN_POINT('Ctrl Pts',(7.5610823503117,-2.35195267370947,19.2676789580178));
#70855=CARTESIAN_POINT('Ctrl Pts',(7.65596893332244,-2.02183201718658,19.2796532809663));
#70856=CARTESIAN_POINT('Ctrl Pts',(7.83930168108754,-1.18167051899068,19.3091241765175));
#70857=CARTESIAN_POINT('Ctrl Pts',(7.89973172729658,-0.667211031505966,
19.3262456895624));
#70858=CARTESIAN_POINT('Ctrl Pts',(7.91356201733813,0.0592879994883373,
19.3527252606395));
#70859=CARTESIAN_POINT('Ctrl Pts',(7.90920299650626,0.269211687218983,19.3606560268355));
#70860=CARTESIAN_POINT('Ctrl Pts',(7.89560757777464,0.493478709939184,19.3696403493004));
#70861=CARTESIAN_POINT('Ctrl Pts',(7.89467008425227,0.508256347393159,19.3702347394251));
#70862=CARTESIAN_POINT('Ctrl Pts',(7.89331662608523,0.528683008859509,19.371059742036));
#70863=CARTESIAN_POINT('Ctrl Pts',(7.89293606985189,0.534334427503551,19.3712883539665));
#70864=CARTESIAN_POINT('Ctrl Pts',(7.89227270679021,0.544030292583091,19.3716811959742));
#70865=CARTESIAN_POINT('Ctrl Pts',(7.89199285931805,0.548074945553286,19.3718452571678));
#70866=CARTESIAN_POINT('Ctrl Pts',(7.89144112073751,0.555961212584904,19.3721655097354));
#70867=CARTESIAN_POINT('Ctrl Pts',(7.89116953342111,0.559802846234865,19.3723216835727));
#70868=CARTESIAN_POINT('Ctrl Pts',(7.89052177283564,0.568871351135959,19.3726907479961));
#70869=CARTESIAN_POINT('Ctrl Pts',(7.89014321138746,0.574098045016697,19.372903776637));
#70870=CARTESIAN_POINT('Ctrl Pts',(7.88904902098002,0.588999713081414,19.3735120456783));
#70871=CARTESIAN_POINT('Ctrl Pts',(7.88832079838922,0.598673616091708,19.3739080199639));
#70872=CARTESIAN_POINT('Ctrl Pts',(7.88659820821451,0.621008032109794,19.3748247680247));
#70873=CARTESIAN_POINT('Ctrl Pts',(7.88559116133486,0.633667346763451,19.3753462712858));
#70874=CARTESIAN_POINT('Ctrl Pts',(7.84234861705062,1.16118621118185,19.3971542762921));
#70875=CARTESIAN_POINT('Ctrl Pts',(7.7498176529061,1.67063603797218,19.4211839647866));
#70876=CARTESIAN_POINT('Ctrl Pts',(7.53924714487542,2.40981738083116,19.4569099173629));
#70877=CARTESIAN_POINT('Ctrl Pts',(7.45863336832276,2.6488227644166,19.4686175784548));
#70878=CARTESIAN_POINT('Ctrl Pts',(7.19801475742954,3.31463166133814,19.501189047015));
#70879=CARTESIAN_POINT('Ctrl Pts',(6.99176350902266,3.73008623819,19.5213991651837));
#70880=CARTESIAN_POINT('Ctrl Pts',(6.734131664389,4.15166911621944,19.5414574533513));
#70881=CARTESIAN_POINT('Ctrl Pts',(6.71777945401352,4.17807670609057,19.5427122763766));
#70882=CARTESIAN_POINT('Ctrl Pts',(6.69507077161803,4.21427152802927,19.5444300426139));
#70883=CARTESIAN_POINT('Ctrl Pts',(6.68884765430728,4.22414183095521,19.5448982580326));
#70884=CARTESIAN_POINT('Ctrl Pts',(6.67890955150117,4.23982733365198,19.5456419875196));
#70885=CARTESIAN_POINT('Ctrl Pts',(6.67520876808631,4.24565148347183,19.5459180652106));
#70886=CARTESIAN_POINT('Ctrl Pts',(6.6679996673331,4.25696416104126,19.5464541676916));
#70887=CARTESIAN_POINT('Ctrl Pts',(6.66449218238999,4.26245321183774,19.5467142253226));
#70888=CARTESIAN_POINT('Ctrl Pts',(6.65609583050655,4.27555741235422,19.5473349144811));
#70889=CARTESIAN_POINT('Ctrl Pts',(6.6512006638116,4.28316852594872,19.5476952942952));
#70890=CARTESIAN_POINT('Ctrl Pts',(6.63651890719506,4.3059101829803,19.5487717241254));
#70891=CARTESIAN_POINT('Ctrl Pts',(6.6266936370525,4.3210157551202,19.5494862263836));
#70892=CARTESIAN_POINT('Ctrl Pts',(6.54216857955549,4.44999995920475,19.5555832488658));
#70893=CARTESIAN_POINT('Ctrl Pts',(6.46458914370474,4.56196876072596,19.5608485454711));
#70894=CARTESIAN_POINT('Ctrl Pts',(6.1796861519972,4.95129034598981,19.5791068605381));
#70895=CARTESIAN_POINT('Ctrl Pts',(5.95708724142328,5.21698516489592,19.5914542449298));
#70896=CARTESIAN_POINT('Ctrl Pts',(5.39997727330915,5.79962376245188,19.6192894662721));
#70897=CARTESIAN_POINT('Ctrl Pts',(5.05381080760213,6.10363539631836,19.6344037552009));
#70898=CARTESIAN_POINT('Ctrl Pts',(4.41555495422948,6.57244888613843,19.6618989951938));
#70899=CARTESIAN_POINT('Ctrl Pts',(4.13581138685182,6.75197982226366,19.673867548586));
#70900=CARTESIAN_POINT('Ctrl Pts',(3.82669028774661,6.92393190887077,19.6879239888571));
#70901=CARTESIAN_POINT('Ctrl Pts',(3.80768873970237,6.93439961929832,19.6887912713313));
#70902=CARTESIAN_POINT('Ctrl Pts',(3.78241985451737,6.94818475018462,19.6899492304948));
#70903=CARTESIAN_POINT('Ctrl Pts',(3.7761906016219,6.95157218319537,19.6902350601175));
#70904=CARTESIAN_POINT('Ctrl Pts',(3.76647330309772,6.95683948050068,19.6906815304173));
#70905=CARTESIAN_POINT('Ctrl Pts',(3.76298837329954,6.95872511331611,19.6908417671113));
#70906=CARTESIAN_POINT('Ctrl Pts',(3.75630755653767,6.96233349691772,19.6911491747973));
#70907=CARTESIAN_POINT('Ctrl Pts',(3.75311189632321,6.96405666800563,19.6912963165729));
#70908=CARTESIAN_POINT('Ctrl Pts',(3.74562059721355,6.96808948914809,19.6916414759559));
#70909=CARTESIAN_POINT('Ctrl Pts',(3.74132401081695,6.970397365496,19.6918396155207));
#70910=CARTESIAN_POINT('Ctrl Pts',(3.72912582057772,6.97693499615886,19.6924026339749));
#70911=CARTESIAN_POINT('Ctrl Pts',(3.72121918197264,6.98115528581892,19.6927681570472));
#70912=CARTESIAN_POINT('Ctrl Pts',(3.67130342042662,7.00768969663006,19.69507935826));
#70913=CARTESIAN_POINT('Ctrl Pts',(3.62910177127783,7.02963753208244,19.6970494455339));
#70914=CARTESIAN_POINT('Ctrl Pts',(3.50101031292845,7.0947932735981,19.7030712814589));
#70915=CARTESIAN_POINT('Ctrl Pts',(3.41453057215005,7.13681612435584,19.7071936075786));
#70916=CARTESIAN_POINT('Ctrl Pts',(3.15177246381048,7.25862845346571,19.7198387525893));
#70917=CARTESIAN_POINT('Ctrl Pts',(2.97331724045881,7.33353486026401,19.7285857498669));
#70918=CARTESIAN_POINT('Ctrl Pts',(2.60528294164501,7.47237427417238,19.7466900795438));
#70919=CARTESIAN_POINT('Ctrl Pts',(2.41565646611307,7.53581297432056,19.7560512933824));
#70920=CARTESIAN_POINT('Ctrl Pts',(1.9515705563846,7.67175220281575,19.7787592119042));
#70921=CARTESIAN_POINT('Ctrl Pts',(1.67520536201082,7.73680195171031,19.7921094744262));
#70922=CARTESIAN_POINT('Ctrl Pts',(0.885752837641893,7.87832578089778,19.8290932648749));
#70923=CARTESIAN_POINT('Ctrl Pts',(0.367761812392883,7.91943596649023,19.8519229113806));
#70924=CARTESIAN_POINT('Ctrl Pts',(-0.18410591415826,7.90892845039262,19.8743899595941));
#70925=CARTESIAN_POINT('Ctrl Pts',(-0.217610215226007,7.90807751941728,
19.8757471966372));
#70926=CARTESIAN_POINT('Ctrl Pts',(-0.263445723050402,7.9066218901948,19.8775948964575));
#70927=CARTESIAN_POINT('Ctrl Pts',(-0.275782167516644,7.90620120926819,
19.8780912988361));
#70928=CARTESIAN_POINT('Ctrl Pts',(-0.295344110721614,7.90548829281707,
19.8788770322433));
#70929=CARTESIAN_POINT('Ctrl Pts',(-0.302570254724032,7.90521502129598,
19.8791669747076));
#70930=CARTESIAN_POINT('Ctrl Pts',(-0.316572948043356,7.90466625264866,
19.879728230175));
#70931=CARTESIAN_POINT('Ctrl Pts',(-0.323349536571749,7.90439194844929,
19.8799995813946));
#70932=CARTESIAN_POINT('Ctrl Pts',(-0.339470304493258,7.9037186428237,19.8806444625774));
#70933=CARTESIAN_POINT('Ctrl Pts',(-0.348814155299892,7.90331178420844,
19.8810177391247));
#70934=CARTESIAN_POINT('Ctrl Pts',(-0.376515413210523,7.90205636886534,
19.8821228820909));
#70935=CARTESIAN_POINT('Ctrl Pts',(-0.394870667695896,7.90116041318558,
19.88285322299));
#70936=CARTESIAN_POINT('Ctrl Pts',(-0.542089644753295,7.89346007374551,
19.8886955956486));
#70937=CARTESIAN_POINT('Ctrl Pts',(-0.670775665315519,7.88356740775545,
19.8937076395799));
#70938=CARTESIAN_POINT('Ctrl Pts',(-1.11271523487854,7.83869328851252,19.9106394730681));
#70939=CARTESIAN_POINT('Ctrl Pts',(-1.4240937000983,7.78814635790689,19.9220683836599));
#70940=CARTESIAN_POINT('Ctrl Pts',(-1.88544910206653,7.68465028393059,19.9387463941926));
#70941=CARTESIAN_POINT('Ctrl Pts',(-2.03819271530998,7.64555686964193,19.9442279785561));
#70942=CARTESIAN_POINT('Ctrl Pts',(-2.24087854721437,7.58717499844503,19.9515265993637));
#70943=CARTESIAN_POINT('Ctrl Pts',(-2.29193893746326,7.57190709409158,19.953367479697));
#70944=CARTESIAN_POINT('Ctrl Pts',(-2.38702620974348,7.54242446938941,19.9568045636771));
#70945=CARTESIAN_POINT('Ctrl Pts',(-2.43109018994791,7.52833723278806,19.9584009320506));
#70946=CARTESIAN_POINT('Ctrl Pts',(-2.51369859096942,7.50112645250372,19.9614037631316));
#70947=CARTESIAN_POINT('Ctrl Pts',(-2.5522701671939,7.48809025386366,19.9628100046962));
#70948=CARTESIAN_POINT('Ctrl Pts',(-2.62499849376896,7.4628827267102,19.9654717306857));
#70949=CARTESIAN_POINT('Ctrl Pts',(-2.65917554562323,7.45077318766046,19.966726839643));
#70950=CARTESIAN_POINT('Ctrl Pts',(-3.02216606235357,7.31934345248576,19.980112487768));
#70951=CARTESIAN_POINT('Ctrl Pts',(-3.34278391400817,7.17858207328368,19.9924081500867));
#70952=CARTESIAN_POINT('Ctrl Pts',(-3.68391828357103,7.00099144196255,20.0070001626933));
#70953=CARTESIAN_POINT('Ctrl Pts',(-3.71471786544114,6.98469800471286,20.0083317955208));
#70954=CARTESIAN_POINT('Ctrl Pts',(-3.80275645685197,6.93737726200084,20.012181682755));
#70955=CARTESIAN_POINT('Ctrl Pts',(-3.85971793100382,6.90584801050679,20.0147272284603));
#70956=CARTESIAN_POINT('Ctrl Pts',(-3.9444610210877,6.85756516644299,20.0185938111878));
#70957=CARTESIAN_POINT('Ctrl Pts',(-3.97253988025756,6.84133756042702,20.0198880713221));
#70958=CARTESIAN_POINT('Ctrl Pts',(-4.01005361096654,6.81934844466994,20.0216341749185));
#70959=CARTESIAN_POINT('Ctrl Pts',(-4.01957759258095,6.81373899912817,20.0220789497719));
#70960=CARTESIAN_POINT('Ctrl Pts',(-4.03446581458019,6.80492803896768,20.0227765168939));
#70961=CARTESIAN_POINT('Ctrl Pts',(-4.03983809386328,6.80174008615711,20.0230286934172));
#70962=CARTESIAN_POINT('Ctrl Pts',(-4.05058892675396,6.79534322697834,20.023534267309));
#70963=CARTESIAN_POINT('Ctrl Pts',(-4.05596745680672,6.79213429011894,20.0237876659624));
#70964=CARTESIAN_POINT('Ctrl Pts',(-4.06801317310468,6.78492816855124,20.0243562112798));
#70965=CARTESIAN_POINT('Ctrl Pts',(-4.07467828516519,6.78092753985872,20.0246715099846));
#70966=CARTESIAN_POINT('Ctrl Pts',(-4.09415790210251,6.76919611546709,20.0255950753167));
#70967=CARTESIAN_POINT('Ctrl Pts',(-4.10695634035251,6.76143879597122,20.0262044931457));
#70968=CARTESIAN_POINT('Ctrl Pts',(-4.13604812709682,6.74369276712165,20.0275956106835));
#70969=CARTESIAN_POINT('Ctrl Pts',(-4.15232741701016,6.73368125629367,20.0283782659263));
#70970=CARTESIAN_POINT('Ctrl Pts',(-4.20466911568278,6.70122993698245,20.0309079578919));
#70971=CARTESIAN_POINT('Ctrl Pts',(-4.24058683784758,6.67855884409813,20.0326642625336));
#70972=CARTESIAN_POINT('Ctrl Pts',(-4.38444532617381,6.58612766993456,20.0397768806848));
#70973=CARTESIAN_POINT('Ctrl Pts',(-4.49085920574644,6.51403257822305,20.0452167592483));
#70974=CARTESIAN_POINT('Ctrl Pts',(-4.75244729291475,6.32735009177143,20.0589745419437));
#70975=CARTESIAN_POINT('Ctrl Pts',(-4.90527605067203,6.20961984429675,20.0673643380829));
#70976=CARTESIAN_POINT('Ctrl Pts',(-5.35371286729974,5.83727628879885,20.0928428194602));
#70977=CARTESIAN_POINT('Ctrl Pts',(-5.63495209810417,5.56627032365979,20.1099954908831));
#70978=CARTESIAN_POINT('Ctrl Pts',(-6.15760899631907,4.98224617347384,20.1436809414318));
#70979=CARTESIAN_POINT('Ctrl Pts',(-6.39790479730613,4.66966510344618,20.1601579924094));
#70980=CARTESIAN_POINT('Ctrl Pts',(-6.63751823856307,4.30454637233406,20.1778613672382));
#70981=CARTESIAN_POINT('Ctrl Pts',(-6.66080398296911,4.26842572607273,20.1795974791336));
#70982=CARTESIAN_POINT('Ctrl Pts',(-6.69296906445738,4.21762732222437,20.1820180834329));
#70983=CARTESIAN_POINT('Ctrl Pts',(-6.7020966813757,4.20310780293963,20.1827075694078));
#70984=CARTESIAN_POINT('Ctrl Pts',(-6.71866786701452,4.17655638779867,20.1839640587366));
#70985=CARTESIAN_POINT('Ctrl Pts',(-6.7261265052807,4.16453399604354,20.1845313728532));
#70986=CARTESIAN_POINT('Ctrl Pts',(-6.74110506156459,4.14024522934447,20.1856742496819));
#70987=CARTESIAN_POINT('Ctrl Pts',(-6.74862384836337,4.12797821761278,20.1862497871313));
#70988=CARTESIAN_POINT('Ctrl Pts',(-6.76694653524783,4.09790062426173,20.1876568680118));
#70989=CARTESIAN_POINT('Ctrl Pts',(-6.77771364887792,4.08006772444066,20.1884876292816));
#70990=CARTESIAN_POINT('Ctrl Pts',(-6.8163418458834,4.01551537966389,20.1914822859254));
#70991=CARTESIAN_POINT('Ctrl Pts',(-6.84379149191096,3.96855112473484,20.1936373171496));
#70992=CARTESIAN_POINT('Ctrl Pts',(-6.99647324467392,3.70102837043541,20.2057807290713));
#70993=CARTESIAN_POINT('Ctrl Pts',(-7.1115288525968,3.47482586168494,20.2155362286519));
#70994=CARTESIAN_POINT('Ctrl Pts',(-7.46083915781616,2.69774145944402,20.2476265767177));
#70995=CARTESIAN_POINT('Ctrl Pts',(-7.64343776973488,2.12596944621827,20.2687624682831));
#70996=CARTESIAN_POINT('Ctrl Pts',(-7.76749778782643,1.50048291702491,20.2924514456719));
#70997=CARTESIAN_POINT('Ctrl Pts',(-7.77486857067629,1.46181036484864,20.29391921236));
#70998=CARTESIAN_POINT('Ctrl Pts',(-7.80725199715692,1.28472587417353,20.3006598962358));
#70999=CARTESIAN_POINT('Ctrl Pts',(-7.82885854493788,1.14572069482018,20.3060055377072));
#71000=CARTESIAN_POINT('Ctrl Pts',(-7.84966453041497,0.983470247404358,
20.3123748030812));
#71001=CARTESIAN_POINT('Ctrl Pts',(-7.85248260576773,0.96071009200969,20.3132712356937));
#71002=CARTESIAN_POINT('Ctrl Pts',(-7.86159573620695,0.884387919116747,
20.3162880714843));
#71003=CARTESIAN_POINT('Ctrl Pts',(-7.8674419583904,0.830774551294097,20.3184250975977));
#71004=CARTESIAN_POINT('Ctrl Pts',(-7.87382942149011,0.766064201971669,
20.32103006895));
#71005=CARTESIAN_POINT('Ctrl Pts',(-7.87489615293663,0.755019667917537,
20.3214755751515));
#71006=CARTESIAN_POINT('Ctrl Pts',(-7.87660287823664,0.736951719146519,
20.3222059064409));
#71007=CARTESIAN_POINT('Ctrl Pts',(-7.8772567248818,0.729929604573375,20.3224901252637));
#71008=CARTESIAN_POINT('Ctrl Pts',(-7.87840986522335,0.717363216146676,
20.3229994331137));
#71009=CARTESIAN_POINT('Ctrl Pts',(-7.8789126991669,0.711819265684822,20.3232243646281));
#71010=CARTESIAN_POINT('Ctrl Pts',(-7.87987278277401,0.701108290196049,
20.3236594034014));
#71011=CARTESIAN_POINT('Ctrl Pts',(-7.88033080297295,0.69594133575079,20.3238694758583));
#71012=CARTESIAN_POINT('Ctrl Pts',(-7.88131334914259,0.684731830895633,
20.3243256833692));
#71013=CARTESIAN_POINT('Ctrl Pts',(-7.88183600821365,0.678689123916538,
20.3245719032586));
#71014=CARTESIAN_POINT('Ctrl Pts',(-7.88308805129682,0.664017147319941,
20.3251704581343));
#71015=CARTESIAN_POINT('Ctrl Pts',(-7.88381021490033,0.655387283169653,
20.3255231259719));
#71016=CARTESIAN_POINT('Ctrl Pts',(-7.88572999626808,0.631983488466599,
20.3264812269822));
#71017=CARTESIAN_POINT('Ctrl Pts',(-7.88690026056012,0.617207403467188,
20.3270879451169));
#71018=CARTESIAN_POINT('Ctrl Pts',(-7.90334433779482,0.401893183150274,
20.3359564659492));
#71019=CARTESIAN_POINT('Ctrl Pts',(-7.91100527114318,0.200868484566958,
20.3445978728846));
#71020=CARTESIAN_POINT('Ctrl Pts',(-7.91099999727893,-0.000207491421311337,
20.3534756400368));
#71021=CARTESIAN_POINT('',(-7.91099868333906,-0.00456423132557518,24.3648581729618));
#71022=CARTESIAN_POINT('Ctrl Pts',(-7.91099999795386,-0.000179927557964477,
20.3534744230576));
#71023=CARTESIAN_POINT('Ctrl Pts',(-7.91098172587622,-0.80356106444437,
20.388944664795));
#71024=CARTESIAN_POINT('Ctrl Pts',(-7.78859805973727,-1.6023406876584,20.4274466847679));
#71025=CARTESIAN_POINT('Ctrl Pts',(-7.48828697629528,-2.5591306577211,20.471266686629));
#71026=CARTESIAN_POINT('Ctrl Pts',(-7.42148272694363,-2.7468514261103,20.4797783367217));
#71027=CARTESIAN_POINT('Ctrl Pts',(-7.3097870754086,-3.02677677424593,20.4923253103193));
#71028=CARTESIAN_POINT('Ctrl Pts',(-7.270076738684,-3.12095336833719,20.4965213640672));
#71029=CARTESIAN_POINT('Ctrl Pts',(-7.22108293721243,-3.23113294702392,
20.5014026443798));
#71030=CARTESIAN_POINT('Ctrl Pts',(-7.21355544809895,-3.24790343303585,
20.5021448633821));
#71031=CARTESIAN_POINT('Ctrl Pts',(-7.20191703467251,-3.2735925924565,20.5032806550884));
#71032=CARTESIAN_POINT('Ctrl Pts',(-7.19784786627995,-3.28253005019517,
20.5036755925323));
#71033=CARTESIAN_POINT('Ctrl Pts',(-7.19071636593886,-3.29811654302511,
20.5043639768595));
#71034=CARTESIAN_POINT('Ctrl Pts',(-7.18766143114841,-3.30476893871632,
20.504657665782));
#71035=CARTESIAN_POINT('Ctrl Pts',(-7.18076252454994,-3.31973711216809,
20.5053182175351));
#71036=CARTESIAN_POINT('Ctrl Pts',(-7.17691332969104,-3.32805047838612,
20.5056849083068));
#71037=CARTESIAN_POINT('Ctrl Pts',(-7.16656291403311,-3.35030350538055,
20.5066659780709));
#71038=CARTESIAN_POINT('Ctrl Pts',(-7.16003545182479,-3.36423095385105,
20.5072794926979));
#71039=CARTESIAN_POINT('Ctrl Pts',(-7.1315869688662,-3.42447278390364,20.5099310581098));
#71040=CARTESIAN_POINT('Ctrl Pts',(-7.1092566698663,-3.47059307083007,20.5119555769473));
#71041=CARTESIAN_POINT('Ctrl Pts',(-6.64564081022046,-4.40487722587664,
20.5528671247981));
#71042=CARTESIAN_POINT('Ctrl Pts',(-6.04177901096497,-5.20231919269601,
20.5846798560224));
#71043=CARTESIAN_POINT('Ctrl Pts',(-5.17252924212299,-5.9884389260997,20.6267740073886));
#71044=CARTESIAN_POINT('Ctrl Pts',(-5.03464761291745,-6.10481593453984,
20.6334020493709));
#71045=CARTESIAN_POINT('Ctrl Pts',(-4.80503883200239,-6.28554128561496,
20.6445460924391));
#71046=CARTESIAN_POINT('Ctrl Pts',(-4.71571585455712,-6.35283003132572,
20.6489127200964));
#71047=CARTESIAN_POINT('Ctrl Pts',(-4.61229549057141,-6.42735530960186,
20.6540038254323));
#71048=CARTESIAN_POINT('Ctrl Pts',(-4.59957036958959,-6.4364678496016,20.654630727467));
#71049=CARTESIAN_POINT('Ctrl Pts',(-4.58018642294146,-6.45026197815132,
20.6555863059638));
#71050=CARTESIAN_POINT('Ctrl Pts',(-4.57354723237446,-6.45497118260902,
20.6559137127795));
#71051=CARTESIAN_POINT('Ctrl Pts',(-4.56166962846795,-6.46336849048662,
20.6564996320999));
#71052=CARTESIAN_POINT('Ctrl Pts',(-4.55643397458303,-6.4670604974821,20.6567579693477));
#71053=CARTESIAN_POINT('Ctrl Pts',(-4.54593646372188,-6.47444391291601,
20.6572760557511));
#71054=CARTESIAN_POINT('Ctrl Pts',(-4.54067458146822,-6.47813527634243,
20.6575358065459));
#71055=CARTESIAN_POINT('Ctrl Pts',(-4.52624362056184,-6.48823279470624,
20.6582483372506));
#71056=CARTESIAN_POINT('Ctrl Pts',(-4.51706546237797,-6.49462591055676,
20.6587016777658));
#71057=CARTESIAN_POINT('Ctrl Pts',(-4.48177952571629,-6.51909361725839,
20.6604451275905));
#71058=CARTESIAN_POINT('Ctrl Pts',(-4.45557674666313,-6.53703029899564,
20.6617409525715));
#71059=CARTESIAN_POINT('Ctrl Pts',(-4.30764676436469,-6.63699071216031,
20.6690603704238));
#71060=CARTESIAN_POINT('Ctrl Pts',(-4.18376596376306,-6.71576997496561,
20.6752032922685));
#71061=CARTESIAN_POINT('Ctrl Pts',(-4.03960840254393,-6.80190653624829,
20.6823162670694));
#71062=CARTESIAN_POINT('Ctrl Pts',(-4.02140406465349,-6.81268507398716,
20.6832138820106));
#71063=CARTESIAN_POINT('Ctrl Pts',(-3.52751132096905,-7.10244279766773,
20.7075467832909));
#71064=CARTESIAN_POINT('Ctrl Pts',(-3.02398591932898,-7.33100100829271,
20.7316868105654));
#71065=CARTESIAN_POINT('Ctrl Pts',(-2.18333850272882,-7.61110404665538,
20.76932522613));
#71066=CARTESIAN_POINT('Ctrl Pts',(-1.85950886494569,-7.69662983954183,
20.7832767490004));
#71067=CARTESIAN_POINT('Ctrl Pts',(-1.28476040294153,-7.81002063025915,
20.8073648427572));
#71068=CARTESIAN_POINT('Ctrl Pts',(-1.03611105453133,-7.84687890968481,
20.8176044074162));
#71069=CARTESIAN_POINT('Ctrl Pts',(-0.720252426499742,-7.8784224680025,
20.830467372978));
#71070=CARTESIAN_POINT('Ctrl Pts',(-0.654294576333215,-7.88417420011935,
20.8331441119363));
#71071=CARTESIAN_POINT('Ctrl Pts',(-0.555585418267175,-7.89153471766616,
20.8371360895608));
#71072=CARTESIAN_POINT('Ctrl Pts',(-0.522883880347012,-7.89376892325486,
20.8384563277763));
#71073=CARTESIAN_POINT('Ctrl Pts',(-0.466530782709033,-7.89726730986283,
20.8407275691585));
#71074=CARTESIAN_POINT('Ctrl Pts',(-0.442885723285561,-7.89862862617552,
20.8416793828187));
#71075=CARTESIAN_POINT('Ctrl Pts',(-0.393941093099465,-7.90122604360499,
20.8436472198839));
#71076=CARTESIAN_POINT('Ctrl Pts',(-0.368640972180599,-7.90244686252048,
20.8446630992689));
#71077=CARTESIAN_POINT('Ctrl Pts',(-0.29951822442489,-7.90544960136094,
20.8474350525814));
#71078=CARTESIAN_POINT('Ctrl Pts',(-0.255685867429983,-7.90698863833048,
20.8491889230253));
#71079=CARTESIAN_POINT('Ctrl Pts',(-0.0838622507045206,-7.91159142715724,
20.8560495436711));
#71080=CARTESIAN_POINT('Ctrl Pts',(0.0441837431742176,-7.91191254734126,
20.861130213061));
#71081=CARTESIAN_POINT('Ctrl Pts',(0.688460287949695,-7.89788660717095,
20.8865674217526));
#71082=CARTESIAN_POINT('Ctrl Pts',(1.20239718353165,-7.83612388225894,20.9063722790975));
#71083=CARTESIAN_POINT('Ctrl Pts',(1.89891798392786,-7.68223961041667,20.9340179828592));
#71084=CARTESIAN_POINT('Ctrl Pts',(2.08953662122669,-7.63259650565974,20.9416804405368));
#71085=CARTESIAN_POINT('Ctrl Pts',(2.36888426145028,-7.54859557502793,20.9531920657983));
#71086=CARTESIAN_POINT('Ctrl Pts',(2.45916826291393,-7.5196674668373,20.9569574865461));
#71087=CARTESIAN_POINT('Ctrl Pts',(2.56967751196085,-7.48205585129312,20.9616362704421));
#71088=CARTESIAN_POINT('Ctrl Pts',(2.59041607784389,-7.47490112405543,20.9625173665108));
#71089=CARTESIAN_POINT('Ctrl Pts',(2.62303035973587,-7.46349729085645,20.9639080694315));
#71090=CARTESIAN_POINT('Ctrl Pts',(2.63492617962997,-7.45930587288788,20.9644163809634));
#71091=CARTESIAN_POINT('Ctrl Pts',(2.65634803820866,-7.45170037645811,20.9653337109129));
#71092=CARTESIAN_POINT('Ctrl Pts',(2.66587765497354,-7.44829643130626,20.9657424931357));
#71093=CARTESIAN_POINT('Ctrl Pts',(2.68733066257378,-7.44058704766428,20.9666643600721));
#71094=CARTESIAN_POINT('Ctrl Pts',(2.69925027871608,-7.43627121851401,20.9671776921112));
#71095=CARTESIAN_POINT('Ctrl Pts',(2.73326697543591,-7.42386196161241,20.9686459704829));
#71096=CARTESIAN_POINT('Ctrl Pts',(2.75533823405328,-7.41569861746346,20.9696026788189));
#71097=CARTESIAN_POINT('Ctrl Pts',(2.90914325702542,-7.35803037651737,20.9762969798641));
#71098=CARTESIAN_POINT('Ctrl Pts',(3.03956979444996,-7.30511735096004,20.9821137401974));
#71099=CARTESIAN_POINT('Ctrl Pts',(3.55496082049081,-7.07983409478263,21.0055532422737));
#71100=CARTESIAN_POINT('Ctrl Pts',(3.92728162067759,-6.8802804842894,21.0234814595417));
#71101=CARTESIAN_POINT('Ctrl Pts',(4.46793977866948,-6.53225668660148,21.0504155080742));
#71102=CARTESIAN_POINT('Ctrl Pts',(4.64885941082402,-6.40476173729586,21.0596070787767));
#71103=CARTESIAN_POINT('Ctrl Pts',(4.89253544780301,-6.21727047351181,21.0722327717848));
#71104=CARTESIAN_POINT('Ctrl Pts',(4.96000697041814,-6.16357739768896,21.0757568598084));
#71105=CARTESIAN_POINT('Ctrl Pts',(5.07657521382355,-6.06765981811501,21.0818974506092));
#71106=CARTESIAN_POINT('Ctrl Pts',(5.12605614234644,-6.02591570594786,21.0845210426706));
#71107=CARTESIAN_POINT('Ctrl Pts',(5.19706757293003,-5.96449992726538,21.0883124607802));
#71108=CARTESIAN_POINT('Ctrl Pts',(5.21901020269072,-5.94530934881373,21.0894877241172));
#71109=CARTESIAN_POINT('Ctrl Pts',(5.25727418922191,-5.91146936488328,21.0915438779844));
#71110=CARTESIAN_POINT('Ctrl Pts',(5.27364160612686,-5.89687257505842,21.0924255746682));
#71111=CARTESIAN_POINT('Ctrl Pts',(5.30532332439834,-5.86838078250689,21.0941365740435));
#71112=CARTESIAN_POINT('Ctrl Pts',(5.32064425812621,-5.85449342526256,21.0949659863577));
#71113=CARTESIAN_POINT('Ctrl Pts',(5.35722187000292,-5.82107619641557,21.0969510379614));
#71114=CARTESIAN_POINT('Ctrl Pts',(5.37842647296293,-5.80148971661407,21.0981057939752));
#71115=CARTESIAN_POINT('Ctrl Pts',(5.45566595402274,-5.72935694033224,21.1023272283551));
#71116=CARTESIAN_POINT('Ctrl Pts',(5.5110421269326,-5.67611106023804,21.1053831487359));
#71117=CARTESIAN_POINT('Ctrl Pts',(6.02482459224143,-5.16748577357066,21.1340423214596));
#71118=CARTESIAN_POINT('Ctrl Pts',(6.4266274589081,-4.65832184857035,21.1590072098058));
#71119=CARTESIAN_POINT('Ctrl Pts',(6.90124393906994,-3.87668754684734,21.1935195477238));
#71120=CARTESIAN_POINT('Ctrl Pts',(7.02871502931433,-3.64047255180341,21.2035306392816));
#71121=CARTESIAN_POINT('Ctrl Pts',(7.32508974723458,-3.01741931310199,21.2293476475888));
#71122=CARTESIAN_POINT('Ctrl Pts',(7.4754882053651,-2.62274555077706,21.2451277900368));
#71123=CARTESIAN_POINT('Ctrl Pts',(7.5991415943857,-2.19939617874741,21.2626752941814));
#71124=CARTESIAN_POINT('Ctrl Pts',(7.60450630480875,-2.18077517776791,21.2634484269859));
#71125=CARTESIAN_POINT('Ctrl Pts',(7.61404109434782,-2.14721673936626,21.2648443453518));
#71126=CARTESIAN_POINT('Ctrl Pts',(7.6182357779132,-2.13228636461093,21.2654663200664));
#71127=CARTESIAN_POINT('Ctrl Pts',(7.62458246582442,-2.10943844159508,21.2664196407676));
#71128=CARTESIAN_POINT('Ctrl Pts',(7.62676611189578,-2.10152967880901,21.2667499077475));
#71129=CARTESIAN_POINT('Ctrl Pts',(7.63082851190424,-2.08672669077147,21.2673686123297));
#71130=CARTESIAN_POINT('Ctrl Pts',(7.6327102373227,-2.07983328485176,21.267656946361));
#71131=CARTESIAN_POINT('Ctrl Pts',(7.63649313982912,-2.06590093822609,21.2682401554886));
#71132=CARTESIAN_POINT('Ctrl Pts',(7.63839393026194,-2.05886190088904,21.2685350438691));
#71133=CARTESIAN_POINT('Ctrl Pts',(7.64372270878547,-2.03901933117859,21.2693669933348));
#71134=CARTESIAN_POINT('Ctrl Pts',(7.64712824574418,-2.02620982929596,21.2699048598986));
#71135=CARTESIAN_POINT('Ctrl Pts',(7.66104809578373,-1.97331707863493,21.2721292744339));
#71136=CARTESIAN_POINT('Ctrl Pts',(7.67127946166076,-1.93316050981997,21.2738262696188));
#71137=CARTESIAN_POINT('Ctrl Pts',(7.8786236470392,-1.09179051453554,21.3095821042463));
#71138=CARTESIAN_POINT('Ctrl Pts',(7.94948169478973,-0.264825296249611,
21.3491856437994));
#71139=CARTESIAN_POINT('Ctrl Pts',(7.86336667347681,0.952964761167712,21.4036851468227));
#71140=CARTESIAN_POINT('Ctrl Pts',(7.80582868617316,1.34527775489399,21.4207178947119));
#71141=CARTESIAN_POINT('Ctrl Pts',(7.71230866792631,1.76215553761376,21.4380919002179));
#71142=CARTESIAN_POINT('Ctrl Pts',(7.70528916941435,1.7926003382245,21.4393567376548));
#71143=CARTESIAN_POINT('Ctrl Pts',(7.69534481036431,1.83459290001176,21.4410958870381));
#71144=CARTESIAN_POINT('Ctrl Pts',(7.69257399662633,1.84617663488404,21.4415750617184));
#71145=CARTESIAN_POINT('Ctrl Pts',(7.68785590217273,1.86570618097345,21.4423819634324));
#71146=CARTESIAN_POINT('Ctrl Pts',(7.68592244139155,1.87365529159508,21.4427101277936));
#71147=CARTESIAN_POINT('Ctrl Pts',(7.68207506802009,1.88936697584728,21.4433582267641));
#71148=CARTESIAN_POINT('Ctrl Pts',(7.68016171189104,1.89712967394649,21.4436781785292));
#71149=CARTESIAN_POINT('Ctrl Pts',(7.67592249946423,1.91421710942443,21.4443819040726));
#71150=CARTESIAN_POINT('Ctrl Pts',(7.67359141078608,1.92354054310399,21.4447655109902));
#71151=CARTESIAN_POINT('Ctrl Pts',(7.66541147506815,1.95600553602064,21.4460999912667));
#71152=CARTESIAN_POINT('Ctrl Pts',(7.65947486133289,1.97912495822983,21.4470480664334));
#71153=CARTESIAN_POINT('Ctrl Pts',(7.59935015440447,2.20895039186463,21.4564506782376));
#71154=CARTESIAN_POINT('Ctrl Pts',(7.53691063332288,2.41341480076733,21.4646348472004));
#71155=CARTESIAN_POINT('Ctrl Pts',(7.32886485941783,3.00739542832371,21.4880345009394));
#71156=CARTESIAN_POINT('Ctrl Pts',(7.16075669613831,3.38825621791586,21.5025162340452));
#71157=CARTESIAN_POINT('Ctrl Pts',(6.78560033245285,4.08412465583359,21.5295450543203));
#71158=CARTESIAN_POINT('Ctrl Pts',(6.58448455573352,4.40102198453725,21.5421212676687));
#71159=CARTESIAN_POINT('Ctrl Pts',(6.16678675370185,4.96609991279743,21.5668432395028));
#71160=CARTESIAN_POINT('Ctrl Pts',(5.95572189139081,5.21735033538304,21.5788313592145));
#71161=CARTESIAN_POINT('Ctrl Pts',(5.72013504507011,5.46481186311343,21.5925063006117));
#71162=CARTESIAN_POINT('Ctrl Pts',(5.71053871461802,5.47483892159157,21.5930638101822));
#71163=CARTESIAN_POINT('Ctrl Pts',(5.69678658009283,5.48913282193774,21.5938635200462));
#71164=CARTESIAN_POINT('Ctrl Pts',(5.69265222112983,5.49342035210292,21.5941040382163));
#71165=CARTESIAN_POINT('Ctrl Pts',(5.68550084226022,5.50081993524719,21.5945202502279));
#71166=CARTESIAN_POINT('Ctrl Pts',(5.68248609441766,5.50393419055534,21.5946957635984));
#71167=CARTESIAN_POINT('Ctrl Pts',(5.6767078096007,5.5098933905579,21.5950322725535));
#71168=CARTESIAN_POINT('Ctrl Pts',(5.67394468846056,5.5127387388738,21.5951932348163));
#71169=CARTESIAN_POINT('Ctrl Pts',(5.66746640929436,5.51939977365708,21.5955707319528));
#71170=CARTESIAN_POINT('Ctrl Pts',(5.66374953996047,5.52321378458636,21.5957874051983));
#71171=CARTESIAN_POINT('Ctrl Pts',(5.65097619436663,5.53629451373348,21.5965323305311));
#71172=CARTESIAN_POINT('Ctrl Pts',(5.64190097851535,5.54554255541434,21.5970621311982));
#71173=CARTESIAN_POINT('Ctrl Pts',(5.53181953112572,5.65717045554271,21.6034949151164));
#71174=CARTESIAN_POINT('Ctrl Pts',(5.42806769394745,5.75679436526213,21.6096211480092));
#71175=CARTESIAN_POINT('Ctrl Pts',(4.80755521091041,6.32092570902297,21.6462706226067));
#71176=CARTESIAN_POINT('Ctrl Pts',(4.23411022750957,6.71856488375504,21.6798465459883));
#71177=CARTESIAN_POINT('Ctrl Pts',(3.34644969566059,7.17475296938914,21.7248370762101));
#71178=CARTESIAN_POINT('Ctrl Pts',(3.0690878847468,7.29770733949958,21.7380916626012));
#71179=CARTESIAN_POINT('Ctrl Pts',(2.67447344759015,7.44614941148397,21.755728411644));
#71180=CARTESIAN_POINT('Ctrl Pts',(2.56269079358081,7.48535683176492,21.7605954224736));
#71181=CARTESIAN_POINT('Ctrl Pts',(2.43348273002804,7.5274422609158,21.7660767897983));
#71182=CARTESIAN_POINT('Ctrl Pts',(2.41688135166986,7.53278897395631,21.7667783670003));
#71183=CARTESIAN_POINT('Ctrl Pts',(2.39175316816391,7.54079024572829,21.7678362332365));
#71184=CARTESIAN_POINT('Ctrl Pts',(2.38323938310447,7.54348532119207,21.7681939509841));
#71185=CARTESIAN_POINT('Ctrl Pts',(2.36852315922854,7.54811640490491,21.7688110633448));
#71186=CARTESIAN_POINT('Ctrl Pts',(2.36232287468557,7.55005919538418,21.7690706967667));
#71187=CARTESIAN_POINT('Ctrl Pts',(2.34948719790915,7.55406375310155,21.7696074194585));
#71188=CARTESIAN_POINT('Ctrl Pts',(2.34285146706557,7.55612442212799,21.7698844699015));
#71189=CARTESIAN_POINT('Ctrl Pts',(2.32483302084007,7.56169387786597,21.7706356215995));
#71190=CARTESIAN_POINT('Ctrl Pts',(2.31344505984468,7.56518571048549,21.7711091261618));
#71191=CARTESIAN_POINT('Ctrl Pts',(2.27082619529148,7.57814848460779,21.7728765967029));
#71192=CARTESIAN_POINT('Ctrl Pts',(2.23954445640299,7.58745192581547,21.7741646778632));
#71193=CARTESIAN_POINT('Ctrl Pts',(1.73687607224747,7.73357003688371,21.7947176048506));
#71194=CARTESIAN_POINT('Ctrl Pts',(1.25379314513056,7.82642431393164,21.8123206757606));
#71195=CARTESIAN_POINT('Ctrl Pts',(0.495492891238331,7.90011568418972,21.8384921888617));
#71196=CARTESIAN_POINT('Ctrl Pts',(0.224631824181886,7.91245111358229,21.847580094274));
#71197=CARTESIAN_POINT('Ctrl Pts',(-0.536758470382203,7.90799233933541,
21.8733683806937));
#71198=CARTESIAN_POINT('Ctrl Pts',(-1.02580444749758,7.85952028132506,21.8901880399758));
#71199=CARTESIAN_POINT('Ctrl Pts',(-1.5294978563163,7.7617701496894,21.9105685716016));
#71200=CARTESIAN_POINT('Ctrl Pts',(-1.551833396365,7.75733540835425,21.9114788074538));
#71201=CARTESIAN_POINT('Ctrl Pts',(-1.58094381607892,7.75142475418711,21.912673989271));
#71202=CARTESIAN_POINT('Ctrl Pts',(-1.58773655305818,7.75003623908245,21.9129535071313));
#71203=CARTESIAN_POINT('Ctrl Pts',(-1.5988076513715,7.74775801054076,21.913410117321));
#71204=CARTESIAN_POINT('Ctrl Pts',(-1.60308712165481,7.74687367756892,21.9135868706715));
#71205=CARTESIAN_POINT('Ctrl Pts',(-1.61135829544614,7.74515733020936,21.9139289784644));
#71206=CARTESIAN_POINT('Ctrl Pts',(-1.61535009395602,7.74432577438658,21.9140943042724));
#71207=CARTESIAN_POINT('Ctrl Pts',(-1.6245353210695,7.74240493315269,21.9144752246521));
#71208=CARTESIAN_POINT('Ctrl Pts',(-1.6297282949823,7.74131350886696,21.9146909515765));
#71209=CARTESIAN_POINT('Ctrl Pts',(-1.64581697443108,7.73791519241831,21.9153604442928));
#71210=CARTESIAN_POINT('Ctrl Pts',(-1.65670886653204,7.73559052480158,21.9158152994355));
#71211=CARTESIAN_POINT('Ctrl Pts',(-1.745679926237,7.71640481395985,21.9195437970396));
#71212=CARTESIAN_POINT('Ctrl Pts',(-1.8235019587745,7.69838563539463,21.9228868436706));
#71213=CARTESIAN_POINT('Ctrl Pts',(-2.15548700202678,7.61620052755629,21.9374584631671));
#71214=CARTESIAN_POINT('Ctrl Pts',(-2.4066332077301,7.54060547228964,21.9492618771522));
#71215=CARTESIAN_POINT('Ctrl Pts',(-3.31127806423235,7.21850519785562,21.9935252897246));
#71216=CARTESIAN_POINT('Ctrl Pts',(-3.93523849053538,6.89822453043655,22.0271712160521));
#71217=CARTESIAN_POINT('Ctrl Pts',(-4.68656063589212,6.37704844730224,22.0675613583843));
#71218=CARTESIAN_POINT('Ctrl Pts',(-4.85896833464568,6.24668186226148,22.0768522775412));
#71219=CARTESIAN_POINT('Ctrl Pts',(-5.10607804207177,6.04340011844219,22.090190143348));
#71220=CARTESIAN_POINT('Ctrl Pts',(-5.18501675166131,5.97581127363246,22.0944550180567));
#71221=CARTESIAN_POINT('Ctrl Pts',(-5.27560044008503,5.89510508982503,22.0993572111415));
#71222=CARTESIAN_POINT('Ctrl Pts',(-5.28855946199602,5.88348220407366,22.1000587306561));
#71223=CARTESIAN_POINT('Ctrl Pts',(-5.30827149163427,5.86568482728106,22.101126159855));
#71224=CARTESIAN_POINT('Ctrl Pts',(-5.31505228381499,5.85954127410598,22.1014934102048));
#71225=CARTESIAN_POINT('Ctrl Pts',(-5.32682207678129,5.84884033134909,22.1021309812048));
#71226=CARTESIAN_POINT('Ctrl Pts',(-5.33181591829319,5.84428829482554,22.1024015341109));
#71227=CARTESIAN_POINT('Ctrl Pts',(-5.34220910495313,5.834790184338,22.1029646867348));
#71228=CARTESIAN_POINT('Ctrl Pts',(-5.34760742826367,5.82984300044389,22.1032572375904));
#71229=CARTESIAN_POINT('Ctrl Pts',(-5.36079099456491,5.81772746932402,22.1039718049777));
#71230=CARTESIAN_POINT('Ctrl Pts',(-5.36856874798952,5.81055097164049,22.1043934652861));
#71231=CARTESIAN_POINT('Ctrl Pts',(-5.3982254406198,5.78307649831113,22.1060016482041));
#71232=CARTESIAN_POINT('Ctrl Pts',(-5.42000398666191,5.76267025805648,22.1071834289799));
#71233=CARTESIAN_POINT('Ctrl Pts',(-5.77178270156673,5.42929939907984,22.1262874451495));
#71234=CARTESIAN_POINT('Ctrl Pts',(-6.07432386215653,5.08855708464409,22.1428666797978));
#71235=CARTESIAN_POINT('Ctrl Pts',(-6.49490231894895,4.52354009847755,22.1675967687351));
#71236=CARTESIAN_POINT('Ctrl Pts',(-6.63432902944382,4.31646280750821,22.1761747300734));
#71237=CARTESIAN_POINT('Ctrl Pts',(-7.02478769757883,3.67281966465503,22.20218167004));
#71238=CARTESIAN_POINT('Ctrl Pts',(-7.24417883742072,3.21855988807715,22.219679622657));
#71239=CARTESIAN_POINT('Ctrl Pts',(-7.43134308939176,2.71299479324775,22.2410221629067));
#71240=CARTESIAN_POINT('Ctrl Pts',(-7.44353565794962,2.67936143727599,22.24244898413));
#71241=CARTESIAN_POINT('Ctrl Pts',(-7.45919326751457,2.63523789994686,22.2443290573173));
#71242=CARTESIAN_POINT('Ctrl Pts',(-7.46286518274943,2.6248211851347,22.244773504281));
#71243=CARTESIAN_POINT('Ctrl Pts',(-7.46880911285582,2.60784578033238,22.2454987300479));
#71244=CARTESIAN_POINT('Ctrl Pts',(-7.47109433925842,2.6012917083211,22.245778962155));
#71245=CARTESIAN_POINT('Ctrl Pts',(-7.47547218254493,2.58868261676965,22.2463185174433));
#71246=CARTESIAN_POINT('Ctrl Pts',(-7.47756607655164,2.58262804384704,22.2465777884844));
#71247=CARTESIAN_POINT('Ctrl Pts',(-7.48233682719779,2.56877880069575,22.2471712711227));
#71248=CARTESIAN_POINT('Ctrl Pts',(-7.48500886010623,2.56098248452242,22.2475056750852));
#71249=CARTESIAN_POINT('Ctrl Pts',(-7.49204625026789,2.54034406332725,22.2483917025645));
#71250=CARTESIAN_POINT('Ctrl Pts',(-7.4963907609046,2.52749491260642,22.2489441402271));
#71251=CARTESIAN_POINT('Ctrl Pts',(-7.52464776918806,2.44320934869856,22.2525729998191));
#71252=CARTESIAN_POINT('Ctrl Pts',(-7.5475714637052,2.37144692942415,22.2556865353714));
#71253=CARTESIAN_POINT('Ctrl Pts',(-7.68148761241604,1.93059835245026,22.2749224573472));
#71254=CARTESIAN_POINT('Ctrl Pts',(-7.76640663932383,1.5541459584239,22.2917880522237));
#71255=CARTESIAN_POINT('Ctrl Pts',(-7.88151128349742,0.786447781953037,
22.3257917354479));
#71256=CARTESIAN_POINT('Ctrl Pts',(-7.91074265904272,0.396095247116501,
22.3428783831706));
#71257=CARTESIAN_POINT('Ctrl Pts',(-7.91120615143957,-0.312646158696349,
22.3730416757368));
#71258=CARTESIAN_POINT('Ctrl Pts',(-7.89226171799543,-0.630200445195317,
22.3862510241615));
#71259=CARTESIAN_POINT('Ctrl Pts',(-7.84982478831273,-0.982623972669835,
22.4006343752917));
#71260=CARTESIAN_POINT('Ctrl Pts',(-7.84512736365174,-1.01944874916272,
22.4021341353553));
#71261=CARTESIAN_POINT('Ctrl Pts',(-7.83772256119207,-1.07441254576667,
22.404368102185));
#71262=CARTESIAN_POINT('Ctrl Pts',(-7.83521103564284,-1.09257736336207,
22.4051056463718));
#71263=CARTESIAN_POINT('Ctrl Pts',(-7.83078771632382,-1.12376959544013,
22.4063708386694));
#71264=CARTESIAN_POINT('Ctrl Pts',(-7.82890651893481,-1.13680124945904,
22.4068990262957));
#71265=CARTESIAN_POINT('Ctrl Pts',(-7.82496433168676,-1.16363610356916,
22.4079858651169));
#71266=CARTESIAN_POINT('Ctrl Pts',(-7.82289933143595,-1.17743867160734,
22.4085444422408));
#71267=CARTESIAN_POINT('Ctrl Pts',(-7.8180151827501,-1.20950448228181,22.4098410896835));
#71268=CARTESIAN_POINT('Ctrl Pts',(-7.81516854225128,-1.22776347479674,
22.4105786553262));
#71269=CARTESIAN_POINT('Ctrl Pts',(-7.8058959287635,-1.28590097808107,22.412924634599));
#71270=CARTESIAN_POINT('Ctrl Pts',(-7.79922847262497,-1.32574048918317,
22.4145285459894));
#71271=CARTESIAN_POINT('Ctrl Pts',(-7.70505704204403,-1.86312106482157,
22.4361138129765));
#71272=CARTESIAN_POINT('Ctrl Pts',(-7.57039667832971,-2.35122629731901,
22.455029107944));
#71273=CARTESIAN_POINT('Ctrl Pts',(-7.19506049946698,-3.3337244033677,22.4934923418002));
#71274=CARTESIAN_POINT('Ctrl Pts',(-6.94765886811018,-3.82263745751245,
22.5128668109563));
#71275=CARTESIAN_POINT('Ctrl Pts',(-6.64766207167355,-4.28865603963787,
22.5344447536521));
#71276=CARTESIAN_POINT('Ctrl Pts',(-6.64343714282686,-4.2951978504266,22.534748344715));
#71277=CARTESIAN_POINT('Ctrl Pts',(-6.60238204916128,-4.35856139672346,
22.5376956753082));
#71278=CARTESIAN_POINT('Ctrl Pts',(-6.56483412584911,-4.41491321661571,
22.5403696674405));
#71279=CARTESIAN_POINT('Ctrl Pts',(-6.51979758087205,-4.48065888443176,
22.5435601010937));
#71280=CARTESIAN_POINT('Ctrl Pts',(-6.51300453306289,-4.49052741715739,
22.5440408877308));
#71281=CARTESIAN_POINT('Ctrl Pts',(-6.50206871376163,-4.50633730467339,
22.5448142428635));
#71282=CARTESIAN_POINT('Ctrl Pts',(-6.49794013760245,-4.51228849139713,
22.5451060603173));
#71283=CARTESIAN_POINT('Ctrl Pts',(-6.49060067728028,-4.52283708462651,
22.5456245878453));
#71284=CARTESIAN_POINT('Ctrl Pts',(-6.48739306292013,-4.52743676851696,
22.5458511216128));
#71285=CARTESIAN_POINT('Ctrl Pts',(-6.480713082694,-4.53699411236018,22.5463227251958));
#71286=CARTESIAN_POINT('Ctrl Pts',(-6.47723991338176,-4.54195120405089,
22.546567838919));
#71287=CARTESIAN_POINT('Ctrl Pts',(-6.46825378552984,-4.55474541322106,
22.5472018010601));
#71288=CARTESIAN_POINT('Ctrl Pts',(-6.46273228247843,-4.56257649328165,
22.5475911239951));
#71289=CARTESIAN_POINT('Ctrl Pts',(-6.43951067083552,-4.59538469246332,
22.5492276774471));
#71290=CARTESIAN_POINT('Ctrl Pts',(-6.42168000652413,-4.62026882514597,
22.5504823370517));
#71291=CARTESIAN_POINT('Ctrl Pts',(-6.29440415596683,-4.79573244779552,
22.5594289322657));
#71292=CARTESIAN_POINT('Ctrl Pts',(-6.17982464696088,-4.94250264721055,
22.5674335341006));
#71293=CARTESIAN_POINT('Ctrl Pts',(-5.9183359451113,-5.25413345182559,22.5853756527728));
#71294=CARTESIAN_POINT('Ctrl Pts',(-5.7694824073621,-5.41716570056153,22.5953874800186));
#71295=CARTESIAN_POINT('Ctrl Pts',(-5.4777200974479,-5.71103542410882,22.6143657890295));
#71296=CARTESIAN_POINT('Ctrl Pts',(-5.33643600819178,-5.84326905712422,
22.623302822943));
#71297=CARTESIAN_POINT('Ctrl Pts',(-4.69199355000562,-6.40354348810939,
22.6626228591802));
#71298=CARTESIAN_POINT('Ctrl Pts',(-4.14115851632649,-6.77283036320718,
22.6922714304811));
#71299=CARTESIAN_POINT('Ctrl Pts',(-3.51383773837286,-7.0879173770017,22.7209555663216));
#71300=CARTESIAN_POINT('Ctrl Pts',(-3.47676801136364,-7.10617426290782,
22.7226342739608));
#71301=CARTESIAN_POINT('Ctrl Pts',(-3.42684509289811,-7.1302772004995,22.724873489262));
#71302=CARTESIAN_POINT('Ctrl Pts',(-3.41411715504994,-7.13638033605583,
22.7254425143634));
#71303=CARTESIAN_POINT('Ctrl Pts',(-3.39415893121352,-7.14588482928227,
22.7263318754924));
#71304=CARTESIAN_POINT('Ctrl Pts',(-3.38693973970159,-7.14930934033406,
22.7266529769068));
#71305=CARTESIAN_POINT('Ctrl Pts',(-3.37309506086123,-7.15585105518575,
22.7272676381245));
#71306=CARTESIAN_POINT('Ctrl Pts',(-3.36647041187674,-7.15897000831293,
22.7275612554895));
#71307=CARTESIAN_POINT('Ctrl Pts',(-3.35093419820725,-7.16625828435632,
22.7282486904962));
#71308=CARTESIAN_POINT('Ctrl Pts',(-3.34201915807507,-7.1704201931791,22.7286422634024));
#71309=CARTESIAN_POINT('Ctrl Pts',(-3.31634690120914,-7.18234678388407,
22.729773060101));
#71310=CARTESIAN_POINT('Ctrl Pts',(-3.29957017925254,-7.19006945244487,
22.7305089009041));
#71311=CARTESIAN_POINT('Ctrl Pts',(-3.18819468969066,-7.24086596140615,
22.7353733627831));
#71312=CARTESIAN_POINT('Ctrl Pts',(-3.09278004232527,-7.28213140727594,
22.7394424475358));
#71313=CARTESIAN_POINT('Ctrl Pts',(-2.81291659814369,-7.39667513556913,
22.7511103199443));
#71314=CARTESIAN_POINT('Ctrl Pts',(-2.62648667654647,-7.46490966636221,
22.7585490165663));
#71315=CARTESIAN_POINT('Ctrl Pts',(-1.88210020738159,-7.70601530284374,
22.7871918872537));
#71316=CARTESIAN_POINT('Ctrl Pts',(-1.30831987783538,-7.82389123765218,
22.8068494484479));
#71317=CARTESIAN_POINT('Ctrl Pts',(-0.58686246957568,-7.8904537389032,22.8321243279684));
#71318=CARTESIAN_POINT('Ctrl Pts',(-0.446616737987543,-7.89963289652462,
22.8370706997292));
#71319=CARTESIAN_POINT('Ctrl Pts',(-0.0189262071950909,-7.91619952801481,
22.852411181903));
#71320=CARTESIAN_POINT('Ctrl Pts',(0.268741777340459,-7.91165939057682,
22.8630985646318));
#71321=CARTESIAN_POINT('Ctrl Pts',(0.579585591892116,-7.88977712288962,
22.8754830065679));
#71322=CARTESIAN_POINT('Ctrl Pts',(0.603632484769886,-7.88797377746221,
22.8764458327305));
#71323=CARTESIAN_POINT('Ctrl Pts',(0.636617338469257,-7.88534843338616,
22.8777727512764));
#71324=CARTESIAN_POINT('Ctrl Pts',(0.645562854808283,-7.88462111652887,
22.8781332408271));
#71325=CARTESIAN_POINT('Ctrl Pts',(0.6608338028638,-7.88335334665052,22.8787496874603));
#71326=CARTESIAN_POINT('Ctrl Pts',(0.667159869008805,-7.88282049853148,
22.8790053620629));
#71327=CARTESIAN_POINT('Ctrl Pts',(0.67943143400787,-7.88177197979014,22.8795019207765));
#71328=CARTESIAN_POINT('Ctrl Pts',(0.685377005224254,-7.88125719510468,
22.8797427724058));
#71329=CARTESIAN_POINT('Ctrl Pts',(0.69954380828997,-7.88001444027691,22.8803172942931));
#71330=CARTESIAN_POINT('Ctrl Pts',(0.707764486543604,-7.87928033196305,
22.8806511845306));
#71331=CARTESIAN_POINT('Ctrl Pts',(0.732219032594326,-7.87705795598791,
22.8816459128797));
#71332=CARTESIAN_POINT('Ctrl Pts',(0.748449415066305,-7.87553237706649,
22.8823080574863));
#71333=CARTESIAN_POINT('Ctrl Pts',(0.884049307936662,-7.86236366932037,
22.8878557804203));
#71334=CARTESIAN_POINT('Ctrl Pts',(1.00314182887592,-7.84805776294403,22.8928296052281));
#71335=CARTESIAN_POINT('Ctrl Pts',(1.48948692221074,-7.77838499562673,22.913454715745));
#71336=CARTESIAN_POINT('Ctrl Pts',(1.85294383724109,-7.69989846061144,22.9295734938286));
#71337=CARTESIAN_POINT('Ctrl Pts',(2.9791241347201,-7.37232104929163,22.9802036375432));
#71338=CARTESIAN_POINT('Ctrl Pts',(3.71027367737872,-7.032801364994,23.0135445544));
#71339=CARTESIAN_POINT('Ctrl Pts',(4.45185123773458,-6.54009342820564,23.0497055887872));
#71340=CARTESIAN_POINT('Ctrl Pts',(4.52495942948383,-6.48972601968616,23.0533011167772));
#71341=CARTESIAN_POINT('Ctrl Pts',(4.62493759251298,-6.41833580659422,23.0582606765467));
#71342=CARTESIAN_POINT('Ctrl Pts',(4.65254221462104,-6.39835394550075,23.059634636335));
#71343=CARTESIAN_POINT('Ctrl Pts',(4.69996937625198,-6.36355414034355,23.0620032232721));
#71344=CARTESIAN_POINT('Ctrl Pts',(4.71985305385803,-6.34882040923402,23.0629987025124));
#71345=CARTESIAN_POINT('Ctrl Pts',(4.76098952569798,-6.3180383777337,23.0650633557095));
#71346=CARTESIAN_POINT('Ctrl Pts',(4.78223108706012,-6.30197556654246,23.0661323590951));
#71347=CARTESIAN_POINT('Ctrl Pts',(4.83214612017109,-6.26383225795724,23.0686512693773));
#71348=CARTESIAN_POINT('Ctrl Pts',(4.86075001927093,-6.24166163337496,23.0701001451148));
#71349=CARTESIAN_POINT('Ctrl Pts',(4.95568937871483,-6.16702655618315,23.0749275480354));
#71350=CARTESIAN_POINT('Ctrl Pts',(5.02133581461236,-6.11369451041662,23.078295764278));
#71351=CARTESIAN_POINT('Ctrl Pts',(5.17463438154379,-5.98501767205325,23.0862376702482));
#71352=CARTESIAN_POINT('Ctrl Pts',(5.26151570867085,-5.90878417028714,23.0907996989384));
#71353=CARTESIAN_POINT('Ctrl Pts',(5.58861721896062,-5.60883386968437,23.1082384850568));
#71354=CARTESIAN_POINT('Ctrl Pts',(5.81649884194595,-5.37215092027798,23.1209394018081));
#71355=CARTESIAN_POINT('Ctrl Pts',(6.28173242759376,-4.82453174847245,23.148715823079));
#71356=CARTESIAN_POINT('Ctrl Pts',(6.51207663856423,-4.50878141877307,23.1637448717277));
#71357=CARTESIAN_POINT('Ctrl Pts',(6.74145640679847,-4.13988302276304,23.181047900546));
#71358=CARTESIAN_POINT('Ctrl Pts',(6.76443000200072,-4.10223751447841,23.1828111039054));
#71359=CARTESIAN_POINT('Ctrl Pts',(6.79505207899578,-4.05110214243058,23.185204316452));
#71360=CARTESIAN_POINT('Ctrl Pts',(6.8029775572945,-4.03777880489369,23.1858277038117));
#71361=CARTESIAN_POINT('Ctrl Pts',(6.81631523438678,-4.01520640323484,23.1868836569137));
#71362=CARTESIAN_POINT('Ctrl Pts',(6.82174790513662,-4.00596946481896,23.1873157139473));
#71363=CARTESIAN_POINT('Ctrl Pts',(6.8321624762226,-3.98817939335677,23.1881477736466));
#71364=CARTESIAN_POINT('Ctrl Pts',(6.83714712648454,-3.97962789029868,23.1885477053694));
#71365=CARTESIAN_POINT('Ctrl Pts',(6.84885669347463,-3.95945240325309,23.1894912208817));
#71366=CARTESIAN_POINT('Ctrl Pts',(6.85556808000964,-3.94782061902841,23.1900351552152));
#71367=CARTESIAN_POINT('Ctrl Pts',(6.87585782351141,-3.91244785221126,23.1916892939209));
#71368=CARTESIAN_POINT('Ctrl Pts',(6.8893426270714,-3.88865364248772,23.1928020380197));
#71369=CARTESIAN_POINT('Ctrl Pts',(6.92057543881955,-3.83287031746905,23.195410397647));
#71370=CARTESIAN_POINT('Ctrl Pts',(6.93822546948616,-3.80082709137985,23.1969084117865));
#71371=CARTESIAN_POINT('Ctrl Pts',(7.15928429260873,-3.39282869953811,23.215972058358));
#71372=CARTESIAN_POINT('Ctrl Pts',(7.33211758677791,-3.00111346891349,23.2341256964937));
#71373=CARTESIAN_POINT('Ctrl Pts',(7.61086672054827,-2.199169079531,23.2698653959958));
#71374=CARTESIAN_POINT('Ctrl Pts',(7.71723037376971,-1.79053539711598,23.2873958969421));
#71375=CARTESIAN_POINT('Ctrl Pts',(7.79926621871597,-1.3258562245647,23.3065452459883));
#71376=CARTESIAN_POINT('Ctrl Pts',(7.80753418056874,-1.27626734831667,23.3085795977167));
#71377=CARTESIAN_POINT('Ctrl Pts',(7.81941077848575,-1.20059532227504,23.3116706741806));
#71378=CARTESIAN_POINT('Ctrl Pts',(7.82336277393056,-1.1745675649381,23.3127314729844));
#71379=CARTESIAN_POINT('Ctrl Pts',(7.83033237691482,-1.1270696141196,23.3146630986422));
#71380=CARTESIAN_POINT('Ctrl Pts',(7.83339178068934,-1.10560583476223,23.3155344092165));
#71381=CARTESIAN_POINT('Ctrl Pts',(7.83972868879752,-1.05980106500253,23.3173905825955));
#71382=CARTESIAN_POINT('Ctrl Pts',(7.84298115345093,-1.03545682820167,23.3183751458748));
#71383=CARTESIAN_POINT('Ctrl Pts',(7.85148000659213,-0.969505716347193,
23.3210373443951));
#71384=CARTESIAN_POINT('Ctrl Pts',(7.85650902451848,-0.927871542886805,
23.3227124818463));
#71385=CARTESIAN_POINT('Ctrl Pts',(7.88210177274179,-0.70084596653946,23.3318191407429));
#71386=CARTESIAN_POINT('Ctrl Pts',(7.89643501282665,-0.514809836578552,
23.33917984715));
#71387=CARTESIAN_POINT('Ctrl Pts',(7.92877855106349,0.26356654612102,23.3697480910059));
#71388=CARTESIAN_POINT('Ctrl Pts',(7.88679135747681,0.856487282413173,23.3924787464047));
#71389=CARTESIAN_POINT('Ctrl Pts',(7.68394771174086,1.95290454328115,23.4343579205409));
#71390=CARTESIAN_POINT('Ctrl Pts',(7.53824744648573,2.45594445503094,23.4535460998312));
#71391=CARTESIAN_POINT('Ctrl Pts',(7.30465067374258,3.03928051752987,23.4779753859744));
#71392=CARTESIAN_POINT('Ctrl Pts',(7.26329039781512,3.13683904001587,23.482142496315));
#71393=CARTESIAN_POINT('Ctrl Pts',(7.2132233632447,3.24863098935327,23.4870371636609));
#71394=CARTESIAN_POINT('Ctrl Pts',(7.20641525223859,3.26370553220862,23.487699729943));
#71395=CARTESIAN_POINT('Ctrl Pts',(7.19551888031526,3.28763199144062,23.488755549197));
#71396=CARTESIAN_POINT('Ctrl Pts',(7.19146142702185,3.29649793126628,23.4891476994164));
#71397=CARTESIAN_POINT('Ctrl Pts',(7.18429162999197,3.31208841689563,23.4898389292233));
#71398=CARTESIAN_POINT('Ctrl Pts',(7.18118620551502,3.31881614245334,23.490137754466));
#71399=CARTESIAN_POINT('Ctrl Pts',(7.17476479296949,3.33267655746222,23.4907545229749));
#71400=CARTESIAN_POINT('Ctrl Pts',(7.17144761078337,3.33980868260003,23.4910725107582));
#71401=CARTESIAN_POINT('Ctrl Pts',(7.16296508547,3.3579756749499,23.4918840922758));
#71402=CARTESIAN_POINT('Ctrl Pts',(7.15778488647676,3.36900355686768,23.4923782535389));
#71403=CARTESIAN_POINT('Ctrl Pts',(7.13680999380535,3.41338927325529,23.4943734072684));
#71404=CARTESIAN_POINT('Ctrl Pts',(7.12080756971057,3.44664804055914,23.4958825856642));
#71405=CARTESIAN_POINT('Ctrl Pts',(7.02106126503938,3.65029661103432,23.5052169252257));
#71406=CARTESIAN_POINT('Ctrl Pts',(6.93145261984057,3.81771075567021,23.5133305183864));
#71407=CARTESIAN_POINT('Ctrl Pts',(6.77862428799867,4.08008952507064,23.5266739473422));
#71408=CARTESIAN_POINT('Ctrl Pts',(6.71921808174932,4.17719821268043,23.5317505649124));
#71409=CARTESIAN_POINT('Ctrl Pts',(6.61147894941804,4.34506642757134,23.5407318260381));
#71410=CARTESIAN_POINT('Ctrl Pts',(6.56405207665741,4.41638722957821,23.5446149554398));
#71411=CARTESIAN_POINT('Ctrl Pts',(6.12904193172172,5.04806702939568,23.5795370095158));
#71412=CARTESIAN_POINT('Ctrl Pts',(5.67166590504446,5.55702874414432,23.6111498576263));
#71413=CARTESIAN_POINT('Ctrl Pts',(5.02672858974368,6.11100476619619,23.6472191217833));
#71414=CARTESIAN_POINT('Ctrl Pts',(4.89527196509317,6.2168075786396,23.6542203536619));
#71415=CARTESIAN_POINT('Ctrl Pts',(4.74268081558628,6.3317769210229,23.6619615610662));
#71416=CARTESIAN_POINT('Ctrl Pts',(4.724777457135,6.34514761744716,23.6628640245789));
#71417=CARTESIAN_POINT('Ctrl Pts',(4.69855409812888,6.3645593791199,23.6641774652524));
#71418=CARTESIAN_POINT('Ctrl Pts',(4.69027866588356,6.37066030649616,23.6645907381541));
#71419=CARTESIAN_POINT('Ctrl Pts',(4.67561495802314,6.38142682643755,23.6653208961907));
#71420=CARTESIAN_POINT('Ctrl Pts',(4.66923154197052,6.38609899585017,23.6656380329438));
#71421=CARTESIAN_POINT('Ctrl Pts',(4.65612110420082,6.39566466144694,23.6662879122424));
#71422=CARTESIAN_POINT('Ctrl Pts',(4.64939334922257,6.40055713851608,23.6666206156598));
#71423=CARTESIAN_POINT('Ctrl Pts',(4.63222486269812,6.41300084598711,23.667467633827));
#71424=CARTESIAN_POINT('Ctrl Pts',(4.62177335841787,6.42053720919399,23.6679813810798));
#71425=CARTESIAN_POINT('Ctrl Pts',(4.59909572836672,6.43680551232517,23.6690920474437));
#71426=CARTESIAN_POINT('Ctrl Pts',(4.58686303558996,6.44552823421536,23.6696886154088));
#71427=CARTESIAN_POINT('Ctrl Pts',(4.55173524446504,6.47042603516095,23.6713944951618));
#71428=CARTESIAN_POINT('Ctrl Pts',(4.52877882227899,6.48651441155713,23.6725005250598));
#71429=CARTESIAN_POINT('Ctrl Pts',(4.45217889305156,6.53959248698265,23.6761622605801));
#71430=CARTESIAN_POINT('Ctrl Pts',(4.39816335931221,6.57604182653211,23.6786977051158));
#71431=CARTESIAN_POINT('Ctrl Pts',(4.18747564078016,6.71445527622746,23.6884131467903));
#71432=CARTESIAN_POINT('Ctrl Pts',(4.02765516701556,6.81152412512922,23.6954139551315));
#71433=CARTESIAN_POINT('Ctrl Pts',(3.6346555170252,7.03154396873902,23.7118728288845));
#71434=CARTESIAN_POINT('Ctrl Pts',(3.39847963177191,7.14868355680275,23.7211496677));
#71435=CARTESIAN_POINT('Ctrl Pts',(2.70858062390757,7.44893018829526,23.7471397187575));
#71436=CARTESIAN_POINT('Ctrl Pts',(2.243169230144,7.60204761736952,23.7633231211076));
#71437=CARTESIAN_POINT('Ctrl Pts',(1.53560572187946,7.76414878679049,23.7890273418242));
#71438=CARTESIAN_POINT('Ctrl Pts',(1.30233994350359,7.80666305662586,23.7976844718643));
#71439=CARTESIAN_POINT('Ctrl Pts',(0.998277790035399,7.8480728742975,23.8095687776602));
#71440=CARTESIAN_POINT('Ctrl Pts',(0.928901479797764,7.85658627503436,23.812320486009));
#71441=CARTESIAN_POINT('Ctrl Pts',(0.848270607176247,7.86539788230396,23.8155736477568));
#71442=CARTESIAN_POINT('Ctrl Pts',(0.837115302974101,7.86659296246253,23.8160249442697));
#71443=CARTESIAN_POINT('Ctrl Pts',(0.820528641148601,7.86833422948586,23.8166978300939));
#71444=CARTESIAN_POINT('Ctrl Pts',(0.815099158920377,7.86889853528994,23.8169183887842));
#71445=CARTESIAN_POINT('Ctrl Pts',(0.805435194367477,7.86989283684836,23.8173114954916));
#71446=CARTESIAN_POINT('Ctrl Pts',(0.80120093591569,7.87032503623294,23.8174839169804));
#71447=CARTESIAN_POINT('Ctrl Pts',(0.792295569322927,7.87122676401817,23.8178469351468));
#71448=CARTESIAN_POINT('Ctrl Pts',(0.78762438966661,7.87169555180985,23.8180375745378));
#71449=CARTESIAN_POINT('Ctrl Pts',(0.775338199530305,7.87291751716785,23.8185395901324));
#71450=CARTESIAN_POINT('Ctrl Pts',(0.767722525272494,7.87366380277699,23.8188513674404));
#71451=CARTESIAN_POINT('Ctrl Pts',(0.732536457642459,7.87706026950344,23.8202946608434));
#71452=CARTESIAN_POINT('Ctrl Pts',(0.704953759796035,7.87957665736916,23.8214340766096));
#71453=CARTESIAN_POINT('Ctrl Pts',(0.488827753901776,7.89815009389373,23.8304212661561));
#71454=CARTESIAN_POINT('Ctrl Pts',(0.299787799166418,7.90758150313049,23.8386338580007));
#71455=CARTESIAN_POINT('Ctrl Pts',(-0.120729563006223,7.91346142537141,
23.8573852362886));
#71456=CARTESIAN_POINT('Ctrl Pts',(-0.352087218733693,7.90654628231055,
23.8680241801041));
#71457=CARTESIAN_POINT('Ctrl Pts',(-0.65105880425389,7.88446118747239,23.881918907157));
#71458=CARTESIAN_POINT('Ctrl Pts',(-0.71924979366994,7.87853320517207,23.8850983236977));
#71459=CARTESIAN_POINT('Ctrl Pts',(-1.09604502441676,7.84084492532695,23.9026977017609));
#71460=CARTESIAN_POINT('Ctrl Pts',(-1.4026630453346,7.79183636428385,23.917120256516));
#71461=CARTESIAN_POINT('Ctrl Pts',(-2.11664858668259,7.63419290565653,23.9502008801544));
#71462=CARTESIAN_POINT('Ctrl Pts',(-2.51981349726183,7.51077348649919,23.9684536193038));
#71463=CARTESIAN_POINT('Ctrl Pts',(-2.94036906228805,7.34432631318953,23.9868175858454));
#71464=CARTESIAN_POINT('Ctrl Pts',(-2.96938237553174,7.33264396765908,23.9880812258696));
#71465=CARTESIAN_POINT('Ctrl Pts',(-3.00915499015354,7.3163545694439,23.9898090959107));
#71466=CARTESIAN_POINT('Ctrl Pts',(-3.01997427489917,7.31189533029402,23.9902786789134));
#71467=CARTESIAN_POINT('Ctrl Pts',(-3.03716377430616,7.30476590427185,23.9910240407974));
#71468=CARTESIAN_POINT('Ctrl Pts',(-3.0435404331586,7.30211136180672,23.9913003877579));
#71469=CARTESIAN_POINT('Ctrl Pts',(-3.05631996584912,7.29677171580894,23.9918539102653));
#71470=CARTESIAN_POINT('Ctrl Pts',(-3.06272279800345,7.29408652740122,23.9921310824059));
#71471=CARTESIAN_POINT('Ctrl Pts',(-3.0774821986731,7.28787394177867,23.9927696467572));
#71472=CARTESIAN_POINT('Ctrl Pts',(-3.08583625987789,7.2843405914596,23.9931308215867));
#71473=CARTESIAN_POINT('Ctrl Pts',(-3.11105452801021,7.27362335649574,23.9942203069956));
#71474=CARTESIAN_POINT('Ctrl Pts',(-3.12789991788475,7.26639519420163,23.9949470003055));
#71475=CARTESIAN_POINT('Ctrl Pts',(-3.16633395964868,7.2497451739042,23.9966026228445));
#71476=CARTESIAN_POINT('Ctrl Pts',(-3.18790600519988,7.24028529449018,23.9975301561475));
#71477=CARTESIAN_POINT('Ctrl Pts',(-3.25800683985186,7.20917029763962,24.0005388355236));
#71478=CARTESIAN_POINT('Ctrl Pts',(-3.30636020693329,7.18712232237946,24.0026055864361));
#71479=CARTESIAN_POINT('Ctrl Pts',(-3.49663728033995,7.09803385163271,24.0107076555686));
#71480=CARTESIAN_POINT('Ctrl Pts',(-3.63677803213146,7.0272616109383,24.0166054729994));
#71481=CARTESIAN_POINT('Ctrl Pts',(-3.94385852656225,6.86053492260607,24.0294363261122));
#71482=CARTESIAN_POINT('Ctrl Pts',(-4.10958850413554,6.76256212043791,24.0362967993362));
#71483=CARTESIAN_POINT('Ctrl Pts',(-4.63589686827892,6.42492986833089,24.0581297817026));
#71484=CARTESIAN_POINT('Ctrl Pts',(-4.98040439427615,6.16172309248277,24.0724535638952));
#71485=CARTESIAN_POINT('Ctrl Pts',(-5.52756918400236,5.66767561438524,24.0976380874301));
#71486=CARTESIAN_POINT('Ctrl Pts',(-5.74150971493769,5.45083571940355,24.1082604598443));
#71487=CARTESIAN_POINT('Ctrl Pts',(-6.02353300551831,5.12991937375214,24.1243069739131));
#71488=CARTESIAN_POINT('Ctrl Pts',(-6.10248894611335,5.03573712885225,24.1290532292525));
#71489=CARTESIAN_POINT('Ctrl Pts',(-6.18703868328447,4.92997264760374,24.1344726365829));
#71490=CARTESIAN_POINT('Ctrl Pts',(-6.19483866167622,4.92016787587154,24.1349758653105));
#71491=CARTESIAN_POINT('Ctrl Pts',(-6.20568060660859,4.90647262275271,24.135679993006));
#71492=CARTESIAN_POINT('Ctrl Pts',(-6.20874230601726,4.90259771616207,24.1358793535303));
#71493=CARTESIAN_POINT('Ctrl Pts',(-6.21434610689373,4.8954918409712,24.1362451970532));
#71494=CARTESIAN_POINT('Ctrl Pts',(-6.21688930762985,4.89226177118805,24.1364115909687));
#71495=CARTESIAN_POINT('Ctrl Pts',(-6.2220413309239,4.88570778196178,24.1367494030047));
#71496=CARTESIAN_POINT('Ctrl Pts',(-6.22465001032928,4.88238375214546,24.1369208320856));
#71497=CARTESIAN_POINT('Ctrl Pts',(-6.23107045755304,4.87418918434719,24.1373436873592));
#71498=CARTESIAN_POINT('Ctrl Pts',(-6.23487917345583,4.86931627066528,24.1375953471596));
#71499=CARTESIAN_POINT('Ctrl Pts',(-6.2487650879767,4.85150747322559,24.1385158189377));
#71500=CARTESIAN_POINT('Ctrl Pts',(-6.25880771009156,4.8385448150794,24.1391872407626));
#71501=CARTESIAN_POINT('Ctrl Pts',(-6.47597989011398,4.55641929758985,24.1538295358105));
#71502=CARTESIAN_POINT('Ctrl Pts',(-6.66558337008851,4.27425115991201,24.1690395234084));
#71503=CARTESIAN_POINT('Ctrl Pts',(-7.18503379951001,3.38217198963414,24.2166621385544));
#71504=CARTESIAN_POINT('Ctrl Pts',(-7.45353448312411,2.74022632557994,24.2500217232447));
#71505=CARTESIAN_POINT('Ctrl Pts',(-7.6457392424917,2.03181794326608,24.2824492078524));
#71506=CARTESIAN_POINT('Ctrl Pts',(-7.65619972334459,1.99203879997181,24.2842573851819));
#71507=CARTESIAN_POINT('Ctrl Pts',(-7.73259036098254,1.69204725906104,24.2977966740719));
#71508=CARTESIAN_POINT('Ctrl Pts',(-7.78555191866778,1.42869818541259,24.3091257566545));
#71509=CARTESIAN_POINT('Ctrl Pts',(-7.82856292048183,1.13934309435532,24.320985714229));
#71510=CARTESIAN_POINT('Ctrl Pts',(-7.8319924517737,1.11552424257621,24.3219577645945));
#71511=CARTESIAN_POINT('Ctrl Pts',(-7.83664570468078,1.08212676226932,24.323314872601));
#71512=CARTESIAN_POINT('Ctrl Pts',(-7.83796063480691,1.07256110240004,24.3237029022796));
#71513=CARTESIAN_POINT('Ctrl Pts',(-7.8402083464816,1.05598489611933,24.3243741572717));
#71514=CARTESIAN_POINT('Ctrl Pts',(-7.84114924464035,1.0489754719331,24.3246576464972));
#71515=CARTESIAN_POINT('Ctrl Pts',(-7.84302304457943,1.03487279720169,24.3252272980427));
#71516=CARTESIAN_POINT('Ctrl Pts',(-7.84395572626761,1.02777952349394,24.3255134529837));
#71517=CARTESIAN_POINT('Ctrl Pts',(-7.84583429129169,1.0133410677833,24.326095186239));
#71518=CARTESIAN_POINT('Ctrl Pts',(-7.84677948536533,1.00599580243136,24.3263907419387));
#71519=CARTESIAN_POINT('Ctrl Pts',(-7.84893635826412,0.989046384850755,
24.3270718522219));
#71520=CARTESIAN_POINT('Ctrl Pts',(-7.85014072725494,0.979441305353303,
24.3274571697809));
#71521=CARTESIAN_POINT('Ctrl Pts',(-7.85319884954731,0.954684162242196,
24.3284486346545));
#71522=CARTESIAN_POINT('Ctrl Pts',(-7.85502638631633,0.939528868030736,
24.3290539347043));
#71523=CARTESIAN_POINT('Ctrl Pts',(-7.89308436335134,0.616049266785744,
24.3419391860885));
#71524=CARTESIAN_POINT('Ctrl Pts',(-7.91117986940194,0.305855064022118,
24.3536116502532));
#71525=CARTESIAN_POINT('Ctrl Pts',(-7.91099865242614,-0.00461750059333042,
24.3648601029169));
#71526=CARTESIAN_POINT('',(-7.911,-2.54574139546548E-12,28.3576684917631));
#71527=CARTESIAN_POINT('Ctrl Pts',(-7.91099868333906,-0.00456423132557518,
24.3648581729618));
#71528=CARTESIAN_POINT('Ctrl Pts',(-7.91057280418394,-0.74272345138825,
24.3916018705913));
#71529=CARTESIAN_POINT('Ctrl Pts',(-7.80684320026678,-1.4771488358149,24.4154648676329));
#71530=CARTESIAN_POINT('Ctrl Pts',(-7.56811091958988,-2.30724848110784,
24.447304034168));
#71531=CARTESIAN_POINT('Ctrl Pts',(-7.53052499884332,-2.42711544366794,
24.4520358224672));
#71532=CARTESIAN_POINT('Ctrl Pts',(-7.46568562111904,-2.61786464781053,
24.4598522725625));
#71533=CARTESIAN_POINT('Ctrl Pts',(-7.44023716408572,-2.68933955186086,
24.4628475646539));
#71534=CARTESIAN_POINT('Ctrl Pts',(-7.40882571863918,-2.77370201921998,
24.466454506756));
#71535=CARTESIAN_POINT('Ctrl Pts',(-7.40385024548674,-2.78695585891665,
24.4670232896717));
#71536=CARTESIAN_POINT('Ctrl Pts',(-7.39613871846185,-2.8073316984716,24.4679008983619));
#71537=CARTESIAN_POINT('Ctrl Pts',(-7.39342787799656,-2.81446325616779,
24.4682086643088));
#71538=CARTESIAN_POINT('Ctrl Pts',(-7.38866736450488,-2.82693266111981,
24.4687478307165));
#71539=CARTESIAN_POINT('Ctrl Pts',(-7.38662221030384,-2.83227223547321,
24.4689790443924));
#71540=CARTESIAN_POINT('Ctrl Pts',(-7.38231899087612,-2.84347089747421,
24.4694646652473));
#71541=CARTESIAN_POINT('Ctrl Pts',(-7.38005973579183,-2.84932952177866,
24.4697191208459));
#71542=CARTESIAN_POINT('Ctrl Pts',(-7.37375230336661,-2.86562791465739,
24.4704281102938));
#71543=CARTESIAN_POINT('Ctrl Pts',(-7.36968894157625,-2.87606176558802,
24.470883254155));
#71544=CARTESIAN_POINT('Ctrl Pts',(-7.35335451956991,-2.91774318610118,
24.4727064574208));
#71545=CARTESIAN_POINT('Ctrl Pts',(-7.34090686230723,-2.94892088541314,
24.4740814241713));
#71546=CARTESIAN_POINT('Ctrl Pts',(-7.02618161225528,-3.72287217082697,
24.5084798205973));
#71547=CARTESIAN_POINT('Ctrl Pts',(-6.61290490762547,-4.41549731126929,
24.5448642602979));
#71548=CARTESIAN_POINT('Ctrl Pts',(-5.90484596763496,-5.27382606389827,
24.5923710786458));
#71549=CARTESIAN_POINT('Ctrl Pts',(-5.6931873058509,-5.50164353888001,24.6053443713055));
#71550=CARTESIAN_POINT('Ctrl Pts',(-5.42266693281738,-5.76043897508899,
24.6205907434687));
#71551=CARTESIAN_POINT('Ctrl Pts',(-5.37613535644784,-5.80389029820227,
24.623170000312));
#71552=CARTESIAN_POINT('Ctrl Pts',(-5.31242847210986,-5.86195637962692,
24.6266448495277));
#71553=CARTESIAN_POINT('Ctrl Pts',(-5.29570802569502,-5.8770660520855,24.6275516671449));
#71554=CARTESIAN_POINT('Ctrl Pts',(-5.26793945656868,-5.90194479501025,
24.6290491025975));
#71555=CARTESIAN_POINT('Ctrl Pts',(-5.25692820328638,-5.91175476052918,
24.6296406817606));
#71556=CARTESIAN_POINT('Ctrl Pts',(-5.23560056281896,-5.93064892687557,
24.6307822485686));
#71557=CARTESIAN_POINT('Ctrl Pts',(-5.22528780580952,-5.93973714023708,
24.6313323304907));
#71558=CARTESIAN_POINT('Ctrl Pts',(-5.20118048409164,-5.96087056947665,
24.6326137666886));
#71559=CARTESIAN_POINT('Ctrl Pts',(-5.18736766212209,-5.97289486894715,
24.6333446170841));
#71560=CARTESIAN_POINT('Ctrl Pts',(-5.14396246651794,-6.01041570216597,
24.6356306867513));
#71561=CARTESIAN_POINT('Ctrl Pts',(-5.11422281464742,-6.03574119766234,
24.6371817506539));
#71562=CARTESIAN_POINT('Ctrl Pts',(-4.78273737141377,-6.31381631427511,
24.65430281125));
#71563=CARTESIAN_POINT('Ctrl Pts',(-4.46271148451399,-6.54393516552441,
24.6692622136227));
#71564=CARTESIAN_POINT('Ctrl Pts',(-3.54124720150995,-7.10736674454685,
24.7092287078701));
#71565=CARTESIAN_POINT('Ctrl Pts',(-2.91159064066481,-7.38766060745645,
24.7330569426243));
#71566=CARTESIAN_POINT('Ctrl Pts',(-2.20447659406172,-7.59781857764282,
24.7620519783176));
#71567=CARTESIAN_POINT('Ctrl Pts',(-2.15505423245597,-7.61198431975259,
24.7640914166593));
#71568=CARTESIAN_POINT('Ctrl Pts',(-2.09444467739586,-7.628719026526,24.7666118803012));
#71569=CARTESIAN_POINT('Ctrl Pts',(-2.08338467545342,-7.63174690254177,
24.7670725997542));
#71570=CARTESIAN_POINT('Ctrl Pts',(-2.06607118397764,-7.63644634386728,
24.7677950992663));
#71571=CARTESIAN_POINT('Ctrl Pts',(-2.05982213117272,-7.63813430672697,
24.7680561360051));
#71572=CARTESIAN_POINT('Ctrl Pts',(-2.04875728857251,-7.64110852029014,
24.7685188116157));
#71573=CARTESIAN_POINT('Ctrl Pts',(-2.04394233644181,-7.64239789408099,
24.7687203068061));
#71574=CARTESIAN_POINT('Ctrl Pts',(-2.03288457655398,-7.64534780297848,
24.7691834195844));
#71575=CARTESIAN_POINT('Ctrl Pts',(-2.02664095278821,-7.64700524245969,
24.7694451807607));
#71576=CARTESIAN_POINT('Ctrl Pts',(-2.00965764677336,-7.65149138961377,
24.7701579500033));
#71577=CARTESIAN_POINT('Ctrl Pts',(-1.99891405493644,-7.65430512467304,
24.7706096625556));
#71578=CARTESIAN_POINT('Ctrl Pts',(-1.94694966130662,-7.66779767665567,
24.772798592575));
#71579=CARTESIAN_POINT('Ctrl Pts',(-1.90565114741246,-7.67816565644995,
24.7745509536764));
#71580=CARTESIAN_POINT('Ctrl Pts',(-1.14061337383398,-7.86367545737623,
24.8072617473561));
#71581=CARTESIAN_POINT('Ctrl Pts',(-0.395833514475741,-7.9360988753032,
24.8428048346375));
#71582=CARTESIAN_POINT('Ctrl Pts',(0.580362777294007,-7.89310941372685,
24.8872368707984));
#71583=CARTESIAN_POINT('Ctrl Pts',(0.812124855088617,-7.87263991554324,
24.8976542536977));
#71584=CARTESIAN_POINT('Ctrl Pts',(1.24019296708237,-7.81572467997065,24.916528247909));
#71585=CARTESIAN_POINT('Ctrl Pts',(1.43667267779269,-7.78200549687933,24.9250461319951));
#71586=CARTESIAN_POINT('Ctrl Pts',(1.69777864429009,-7.72696784047774,24.9361576998387));
#71587=CARTESIAN_POINT('Ctrl Pts',(1.76369840599539,-7.71218857071168,24.9389452366668));
#71588=CARTESIAN_POINT('Ctrl Pts',(1.85768236901427,-7.6898492180152,24.9428946964361));
#71589=CARTESIAN_POINT('Ctrl Pts',(1.88590586808909,-7.68297623705975,24.9440775099758));
#71590=CARTESIAN_POINT('Ctrl Pts',(1.93563880087852,-7.67057472479855,24.9461561788123));
#71591=CARTESIAN_POINT('Ctrl Pts',(1.95716392549673,-7.66511079860863,24.9470540059836));
#71592=CARTESIAN_POINT('Ctrl Pts',(1.98890646314267,-7.65691086201822,24.9483753185498));
#71593=CARTESIAN_POINT('Ctrl Pts',(1.99914176747386,-7.6542449047991,24.9488009589429));
#71594=CARTESIAN_POINT('Ctrl Pts',(2.01731033406585,-7.64947366711465,24.9495557796115));
#71595=CARTESIAN_POINT('Ctrl Pts',(2.02524571390958,-7.64737655451795,24.9498852111278));
#71596=CARTESIAN_POINT('Ctrl Pts',(2.04068906644963,-7.64326955843328,24.9505258528143));
#71597=CARTESIAN_POINT('Ctrl Pts',(2.04819736802509,-7.6412609529352,24.9508371019934));
#71598=CARTESIAN_POINT('Ctrl Pts',(2.06618157076311,-7.63642144427841,24.9515820953173));
#71599=CARTESIAN_POINT('Ctrl Pts',(2.07665464327614,-7.63358004161279,24.952015514621));
#71600=CARTESIAN_POINT('Ctrl Pts',(2.10850720898211,-7.62486786090342,24.9533324220028));
#71601=CARTESIAN_POINT('Ctrl Pts',(2.1298679767266,-7.61892872771783,24.9542137952552));
#71602=CARTESIAN_POINT('Ctrl Pts',(2.3609904755439,-7.55361963892546,24.9637315555435));
#71603=CARTESIAN_POINT('Ctrl Pts',(2.56824481651057,-7.48569119055802,24.9720962281796));
#71604=CARTESIAN_POINT('Ctrl Pts',(3.18927518032591,-7.25331133215228,24.9968311235325));
#71605=CARTESIAN_POINT('Ctrl Pts',(3.59222096964228,-7.0624343638207,25.0123821974582));
#71606=CARTESIAN_POINT('Ctrl Pts',(4.26880091771409,-6.66897414393222,25.0394358086205));
#71607=CARTESIAN_POINT('Ctrl Pts',(4.54944875954921,-6.48077018322996,25.0509985159481));
#71608=CARTESIAN_POINT('Ctrl Pts',(5.06113495334599,-6.08797150006487,25.0740260343391));
#71609=CARTESIAN_POINT('Ctrl Pts',(5.29393425210766,-5.88665853749663,25.0854177797673));
#71610=CARTESIAN_POINT('Ctrl Pts',(5.53019444191725,-5.65697391424798,25.0985318157757));
#71611=CARTESIAN_POINT('Ctrl Pts',(5.54589543263123,-5.64158207152078,25.0994105434988));
#71612=CARTESIAN_POINT('Ctrl Pts',(5.5681651846667,-5.61956799686196,25.1006669696907));
#71613=CARTESIAN_POINT('Ctrl Pts',(5.57478680053978,-5.61299920921923,25.1010418289023));
#71614=CARTESIAN_POINT('Ctrl Pts',(5.58618134954588,-5.60165551516449,25.1016890739585));
#71615=CARTESIAN_POINT('Ctrl Pts',(5.59095982426596,-5.59688617212325,25.1019611706111));
#71616=CARTESIAN_POINT('Ctrl Pts',(5.60008495211548,-5.58775513483806,25.1024820381891));
#71617=CARTESIAN_POINT('Ctrl Pts',(5.60443263074964,-5.58339446975902,25.102730756456));
#71618=CARTESIAN_POINT('Ctrl Pts',(5.61458719454918,-5.57318576349309,25.103312949429));
#71619=CARTESIAN_POINT('Ctrl Pts',(5.62039003650966,-5.56733372059712,25.1036466257482));
#71620=CARTESIAN_POINT('Ctrl Pts',(5.64094662244933,-5.54653794642556,25.1048321302628));
#71621=CARTESIAN_POINT('Ctrl Pts',(5.65564993067959,-5.53154461615034,25.1056864069206));
#71622=CARTESIAN_POINT('Ctrl Pts',(5.90146310147021,-5.27887815383104,25.1200726748901));
#71623=CARTESIAN_POINT('Ctrl Pts',(6.11746049448109,-5.0269753881479,25.134249044076));
#71624=CARTESIAN_POINT('Ctrl Pts',(6.55917400858412,-4.44105678080844,25.1658737865343));
#71625=CARTESIAN_POINT('Ctrl Pts',(6.77649152296901,-4.10181989985027,25.1833100046639));
#71626=CARTESIAN_POINT('Ctrl Pts',(7.23703448889201,-3.24561948833542,25.2246095169069));
#71627=CARTESIAN_POINT('Ctrl Pts',(7.45198461487632,-2.71600323355572,25.2479730860838));
#71628=CARTESIAN_POINT('Ctrl Pts',(7.62939279128401,-2.0933911265076,25.2742362256997));
#71629=CARTESIAN_POINT('Ctrl Pts',(7.64952386379584,-2.01858998718013,25.2773705458916));
#71630=CARTESIAN_POINT('Ctrl Pts',(7.67711152940006,-1.90973640188646,25.2819013974262));
#71631=CARTESIAN_POINT('Ctrl Pts',(7.6854466510456,-1.87591160350011,25.2833050894432));
#71632=CARTESIAN_POINT('Ctrl Pts',(7.69970888978824,-1.81634297718084,25.2857697823978));
#71633=CARTESIAN_POINT('Ctrl Pts',(7.70573097929015,-1.79062248334811,25.286831589573));
#71634=CARTESIAN_POINT('Ctrl Pts',(7.71781795265164,-1.73780835204953,25.2890070242199));
#71635=CARTESIAN_POINT('Ctrl Pts',(7.72386926207246,-1.71071197075203,25.290120516651));
#71636=CARTESIAN_POINT('Ctrl Pts',(7.73901764214081,-1.64116177599236,25.2929719740408));
#71637=CARTESIAN_POINT('Ctrl Pts',(7.74790810464243,-1.59866383731985,25.2947080161914));
#71638=CARTESIAN_POINT('Ctrl Pts',(7.78224438332102,-1.4275125808803,25.3016748788065));
#71639=CARTESIAN_POINT('Ctrl Pts',(7.80483935090458,-1.29830779536354,25.3068780602028));
#71640=CARTESIAN_POINT('Ctrl Pts',(7.9000304207093,-0.660968121277869,25.3323056701324));
#71641=CARTESIAN_POINT('Ctrl Pts',(7.92626698574461,-0.147163008991056,
25.3519894929041));
#71642=CARTESIAN_POINT('Ctrl Pts',(7.88986299150046,0.639812488650948,25.3825238973486));
#71643=CARTESIAN_POINT('Ctrl Pts',(7.86290839865452,0.913215186299687,25.3932212701483));
#71644=CARTESIAN_POINT('Ctrl Pts',(7.81702505766936,1.21616441837616,25.4054654802047));
#71645=CARTESIAN_POINT('Ctrl Pts',(7.81206238070383,1.24764497564341,25.4067426317572));
#71646=CARTESIAN_POINT('Ctrl Pts',(7.80454175468626,1.29354685884412,25.4086125362271));
#71647=CARTESIAN_POINT('Ctrl Pts',(7.80213374443213,1.30799254914851,25.40920212347));
#71648=CARTESIAN_POINT('Ctrl Pts',(7.79783296193881,1.33335851563333,25.4102394459991));
#71649=CARTESIAN_POINT('Ctrl Pts',(7.79595732560442,1.34428167061491,25.4106868039568));
#71650=CARTESIAN_POINT('Ctrl Pts',(7.7922671195098,1.36550485945748,25.411557327662));
#71651=CARTESIAN_POINT('Ctrl Pts',(7.79045506577337,1.37580530976172,25.4119804356678));
#71652=CARTESIAN_POINT('Ctrl Pts',(7.78606071856236,1.40049751067626,25.412996207441));
#71653=CARTESIAN_POINT('Ctrl Pts',(7.78345895449406,1.41488568199054,25.4135893266697));
#71654=CARTESIAN_POINT('Ctrl Pts',(7.77293131128146,1.47219736053309,25.4159568607082));
#71655=CARTESIAN_POINT('Ctrl Pts',(7.76469020079339,1.51506180355613,25.4177386432284));
#71656=CARTESIAN_POINT('Ctrl Pts',(7.66879175300856,1.99251137683444,25.4376988104559));
#71657=CARTESIAN_POINT('Ctrl Pts',(7.54510701946391,2.41905347451808,25.4565372503823));
#71658=CARTESIAN_POINT('Ctrl Pts',(7.23598835250862,3.22501008889486,25.4928701956944));
#71659=CARTESIAN_POINT('Ctrl Pts',(7.05465115731419,3.60446099832577,25.510325987878));
#71660=CARTESIAN_POINT('Ctrl Pts',(6.81874135146916,4.01138797281012,25.5294115341544));
#71661=CARTESIAN_POINT('Ctrl Pts',(6.79301674932022,4.0547984631937,25.5314531073103));
#71662=CARTESIAN_POINT('Ctrl Pts',(6.75320840415856,4.12053317739695,25.5345537597579));
#71663=CARTESIAN_POINT('Ctrl Pts',(6.73942543881044,4.14303779578966,25.5356169445171));
#71664=CARTESIAN_POINT('Ctrl Pts',(6.7152406250969,4.18208634784794,25.5374647443686));
#71665=CARTESIAN_POINT('Ctrl Pts',(6.7048896191626,4.19866146185758,25.5382500461887));
#71666=CARTESIAN_POINT('Ctrl Pts',(6.68183351577716,4.23527861660687,25.5399871075836));
#71667=CARTESIAN_POINT('Ctrl Pts',(6.66909943421595,4.25530220243095,25.5409384642154));
#71668=CARTESIAN_POINT('Ctrl Pts',(6.6353576046144,4.30783572760024,25.5434384723009));
#71669=CARTESIAN_POINT('Ctrl Pts',(6.61420098189177,4.34024936928514,25.5449850999709));
#71670=CARTESIAN_POINT('Ctrl Pts',(6.51813209980344,4.48510075313238,25.5519166294206));
#71671=CARTESIAN_POINT('Ctrl Pts',(6.44058417768881,4.59576446092332,25.5572660407516));
#71672=CARTESIAN_POINT('Ctrl Pts',(6.13337057256121,5.0111110997588,25.5776164835313));
#71673=CARTESIAN_POINT('Ctrl Pts',(5.88460119207482,5.30103324847743,25.5924719500433));
#71674=CARTESIAN_POINT('Ctrl Pts',(5.22796585240134,5.9628550767811,25.6282232313017));
#71675=CARTESIAN_POINT('Ctrl Pts',(4.80028440682766,6.31225283562574,25.6486142711579));
#71676=CARTESIAN_POINT('Ctrl Pts',(4.05968869489079,6.7981672170229,25.6818946297322));
#71677=CARTESIAN_POINT('Ctrl Pts',(3.7682122321413,6.963957491497,25.6945983223048));
#71678=CARTESIAN_POINT('Ctrl Pts',(3.44501995440808,7.12154219710119,25.7089268363617));
#71679=CARTESIAN_POINT('Ctrl Pts',(3.42286582245018,7.13221671703125,25.7099102854397));
#71680=CARTESIAN_POINT('Ctrl Pts',(3.39129602995836,7.14724701208313,25.7113138881344));
#71681=CARTESIAN_POINT('Ctrl Pts',(3.38192091051453,7.15168788248264,25.71173098123));
#71682=CARTESIAN_POINT('Ctrl Pts',(3.36576229710609,7.15930312611876,25.7124503723698));
#71683=CARTESIAN_POINT('Ctrl Pts',(3.35898296806823,7.16248633590961,25.7127523447949));
#71684=CARTESIAN_POINT('Ctrl Pts',(3.34602781139467,7.16854694521082,25.7133297142549));
#71685=CARTESIAN_POINT('Ctrl Pts',(3.33985276539943,7.17142600362154,25.7136050488055));
#71686=CARTESIAN_POINT('Ctrl Pts',(3.32542838405404,7.17812856762465,25.7142485304757));
#71687=CARTESIAN_POINT('Ctrl Pts',(3.31717616987855,7.18194583159784,25.714616914209));
#71688=CARTESIAN_POINT('Ctrl Pts',(3.28881776321003,7.19500440455749,25.7158837459417));
#71689=CARTESIAN_POINT('Ctrl Pts',(3.26867949085281,7.20417552778718,25.7167849099572));
#71690=CARTESIAN_POINT('Ctrl Pts',(3.05438306416182,7.30068423842469,25.7263929948997));
#71691=CARTESIAN_POINT('Ctrl Pts',(2.85684972978158,7.38021924102636,25.7354619489356));
#71692=CARTESIAN_POINT('Ctrl Pts',(1.95177791181698,7.70285663117788,25.7777250487018));
#71693=CARTESIAN_POINT('Ctrl Pts',(1.21511682068751,7.85284145258832,25.8132825514916));
#71694=CARTESIAN_POINT('Ctrl Pts',(0.270104089451477,7.90887993498538,25.8546754203215));
#71695=CARTESIAN_POINT('Ctrl Pts',(0.0715352027644414,7.91316799886341,
25.8631696524825));
#71696=CARTESIAN_POINT('Ctrl Pts',(-0.233581190075055,7.90826937787337,
25.8758843356522));
#71697=CARTESIAN_POINT('Ctrl Pts',(-0.340125199037607,7.90440388130973,
25.8802614385258));
#71698=CARTESIAN_POINT('Ctrl Pts',(-0.464618989283191,7.89736521347536,
25.8853038913444));
#71699=CARTESIAN_POINT('Ctrl Pts',(-0.482673137310035,7.8962823384366,25.8860333809009));
#71700=CARTESIAN_POINT('Ctrl Pts',(-0.510240055474146,7.89453399606832,
25.8871445574995));
#71701=CARTESIAN_POINT('Ctrl Pts',(-0.519755542450827,7.89391323148379,
25.8875276226282));
#71702=CARTESIAN_POINT('Ctrl Pts',(-0.537059063589122,7.89275297383559,
25.8882233265403));
#71703=CARTESIAN_POINT('Ctrl Pts',(-0.544847458766876,7.89221915502193,
25.8885361401978));
#71704=CARTESIAN_POINT('Ctrl Pts',(-0.561631446853583,7.89104381242936,
25.8892095537734));
#71705=CARTESIAN_POINT('Ctrl Pts',(-0.570626763352512,7.89039843286804,
25.8895700339791));
#71706=CARTESIAN_POINT('Ctrl Pts',(-0.594882220657005,7.88861650140046,
25.8905408892103));
#71707=CARTESIAN_POINT('Ctrl Pts',(-0.610140234161235,7.88745104964955,
25.8911503685201));
#71708=CARTESIAN_POINT('Ctrl Pts',(-0.680635822924575,7.88186060744194,
25.8939606162287));
#71709=CARTESIAN_POINT('Ctrl Pts',(-0.735829935505321,7.87689953095941,
25.8961447212129));
#71710=CARTESIAN_POINT('Ctrl Pts',(-1.78588003306379,7.77138330028402,25.9374008925704));
#71711=CARTESIAN_POINT('Ctrl Pts',(-2.7526205253803,7.48374815716393,25.9688847971152));
#71712=CARTESIAN_POINT('Ctrl Pts',(-3.78194210678685,6.95027410426895,26.0100509519456));
#71713=CARTESIAN_POINT('Ctrl Pts',(-3.92138991922525,6.87256091035423,26.0158439381851));
#71714=CARTESIAN_POINT('Ctrl Pts',(-4.16382189973761,6.72767385463727,26.0264549272363));
#71715=CARTESIAN_POINT('Ctrl Pts',(-4.26777135806214,6.66221684887756,26.031188742951));
#71716=CARTESIAN_POINT('Ctrl Pts',(-4.38828534924573,6.58235110095856,26.0369437252511));
#71717=CARTESIAN_POINT('Ctrl Pts',(-4.40637065471377,6.57025813486448,26.0378145866603));
#71718=CARTESIAN_POINT('Ctrl Pts',(-4.43030877898876,6.55410831691033,26.0389771864212));
#71719=CARTESIAN_POINT('Ctrl Pts',(-4.43620647782245,6.55011784569408,26.0392644211135));
#71720=CARTESIAN_POINT('Ctrl Pts',(-4.44588536927462,6.54354989468009,26.0397371419005));
#71721=CARTESIAN_POINT('Ctrl Pts',(-4.44966973808012,6.54097708012681,26.0399223069392));
#71722=CARTESIAN_POINT('Ctrl Pts',(-4.45700080282973,6.53598372715914,26.0402816616937));
#71723=CARTESIAN_POINT('Ctrl Pts',(-4.46054776543342,6.53356358125187,26.0404558241495));
#71724=CARTESIAN_POINT('Ctrl Pts',(-4.46873435970091,6.52796797114192,26.0408584916684));
#71725=CARTESIAN_POINT('Ctrl Pts',(-4.47337257519347,6.52479044973977,26.0410871408061));
#71726=CARTESIAN_POINT('Ctrl Pts',(-4.48829626878186,6.51454322080528,26.0418244960686));
#71727=CARTESIAN_POINT('Ctrl Pts',(-4.49856820769432,6.50745425244984,26.042334577621));
#71728=CARTESIAN_POINT('Ctrl Pts',(-4.60315689471571,6.43490853250688,26.0475542894979));
#71729=CARTESIAN_POINT('Ctrl Pts',(-4.69605068602707,6.36743329219995,26.0524061847));
#71730=CARTESIAN_POINT('Ctrl Pts',(-5.4374867102003,5.80382581272292,26.092660597372));
#71731=CARTESIAN_POINT('Ctrl Pts',(-6.00714946539273,5.21201776450046,26.1326284383752));
#71732=CARTESIAN_POINT('Ctrl Pts',(-6.60671485938683,4.35739302211068,26.1788141193332));
#71733=CARTESIAN_POINT('Ctrl Pts',(-6.72914848508708,4.16582855848665,26.1885994188836));
#71734=CARTESIAN_POINT('Ctrl Pts',(-6.89543128386307,3.87914900211362,26.202400558143));
#71735=CARTESIAN_POINT('Ctrl Pts',(-6.94590735121461,3.78802611003953,26.2066698760701));
#71736=CARTESIAN_POINT('Ctrl Pts',(-7.00246025467444,3.68099939710884,26.2115512320661));
#71737=CARTESIAN_POINT('Ctrl Pts',(-7.01030200112158,3.66604310365004,26.2122303973224));
#71738=CARTESIAN_POINT('Ctrl Pts',(-7.02216380753612,3.64324225834743,26.2132612873442));
#71739=CARTESIAN_POINT('Ctrl Pts',(-7.0262187213448,3.6354159560361,26.2136143329046));
#71740=CARTESIAN_POINT('Ctrl Pts',(-7.03354861794924,3.62121060642831,26.2142536861538));
#71741=CARTESIAN_POINT('Ctrl Pts',(-7.03682802073475,3.61483385844223,26.214540160911));
#71742=CARTESIAN_POINT('Ctrl Pts',(-7.04336963570848,3.60207115378337,26.2151124684279));
#71743=CARTESIAN_POINT('Ctrl Pts',(-7.04663184402713,3.59568520274753,26.2153983008876));
#71744=CARTESIAN_POINT('Ctrl Pts',(-7.05579354022095,3.57769032873201,26.2162022629613));
#71745=CARTESIAN_POINT('Ctrl Pts',(-7.06167306730886,3.56607123641736,26.2167196394454));
#71746=CARTESIAN_POINT('Ctrl Pts',(-7.08577345631355,3.51815083593836,26.218846349131));
#71747=CARTESIAN_POINT('Ctrl Pts',(-7.10374346000765,3.48172366793042,26.2204462442268));
#71748=CARTESIAN_POINT('Ctrl Pts',(-7.39310689150369,2.88358526952599,26.2464485099742));
#71749=CARTESIAN_POINT('Ctrl Pts',(-7.5974179773813,2.29181619010096,26.2680574152853));
#71750=CARTESIAN_POINT('Ctrl Pts',(-7.81390931877673,1.29697653796323,26.3024931912484));
#71751=CARTESIAN_POINT('Ctrl Pts',(-7.86882056065629,0.906068509209754,
26.3156481182655));
#71752=CARTESIAN_POINT('Ctrl Pts',(-7.90556323740453,0.340339599843021,
26.3359660510946));
#71753=CARTESIAN_POINT('Ctrl Pts',(-7.91110921672639,0.167647964647231,
26.3423427371046));
#71754=CARTESIAN_POINT('Ctrl Pts',(-7.91095488487696,-0.0728388390359211,
26.351635775486));
#71755=CARTESIAN_POINT('Ctrl Pts',(-7.91004077470606,-0.140595545078708,
26.3542997823184));
#71756=CARTESIAN_POINT('Ctrl Pts',(-7.90797765089617,-0.21891214830021,
26.3574405856538));
#71757=CARTESIAN_POINT('Ctrl Pts',(-7.90767764832572,-0.229493493853941,
26.3578662402143));
#71758=CARTESIAN_POINT('Ctrl Pts',(-7.90720084075094,-0.245198172506846,
26.3584999647099));
#71759=CARTESIAN_POINT('Ctrl Pts',(-7.90704029201898,-0.250321992406321,
26.358707036841));
#71760=CARTESIAN_POINT('Ctrl Pts',(-7.9067443280252,-0.259483041069016,
26.3590778275356));
#71761=CARTESIAN_POINT('Ctrl Pts',(-7.90661080158455,-0.263520301882438,
26.3592414283301));
#71762=CARTESIAN_POINT('Ctrl Pts',(-7.90632170207179,-0.272063356188622,
26.3595880237614));
#71763=CARTESIAN_POINT('Ctrl Pts',(-7.90616536936308,-0.276569120736856,
26.3597710645546));
#71764=CARTESIAN_POINT('Ctrl Pts',(-7.90573976665904,-0.288540375032233,
26.360258014082));
#71765=CARTESIAN_POINT('Ctrl Pts',(-7.9054637743304,-0.296005604907943,
26.3605623280983));
#71766=CARTESIAN_POINT('Ctrl Pts',(-7.90414217693727,-0.330432228911968,
26.3619686816774));
#71767=CARTESIAN_POINT('Ctrl Pts',(-7.90296922761689,-0.357388252526246,
26.363078286255));
#71768=CARTESIAN_POINT('Ctrl Pts',(-7.89294376396666,-0.563503467131169,
26.3716243655331));
#71769=CARTESIAN_POINT('Ctrl Pts',(-7.87813841968225,-0.742309813567676,
26.3793939771249));
#71770=CARTESIAN_POINT('Ctrl Pts',(-7.83461280456575,-1.11386087706274,
26.3960620371927));
#71771=CARTESIAN_POINT('Ctrl Pts',(-7.80482193228937,-1.30636599472182,
26.4049941176159));
#71772=CARTESIAN_POINT('Ctrl Pts',(-7.6255875677926,-2.2360644086917,26.4489870421113));
#71773=CARTESIAN_POINT('Ctrl Pts',(-7.37858777193132,-2.95065617169274,
26.4849685297941));
#71774=CARTESIAN_POINT('Ctrl Pts',(-6.94056586629228,-3.80190626710509,
26.5261272453434));
#71775=CARTESIAN_POINT('Ctrl Pts',(-6.83971592156793,-3.98048246356251,
26.5346912163795));
#71776=CARTESIAN_POINT('Ctrl Pts',(-6.72000931531388,-4.17443651374091,
26.5439248243107));
#71777=CARTESIAN_POINT('Ctrl Pts',(-6.7078974000297,-4.19387146771705,26.5448493269086));
#71778=CARTESIAN_POINT('Ctrl Pts',(-6.69079612143912,-4.22104881343413,
26.5461411475077));
#71779=CARTESIAN_POINT('Ctrl Pts',(-6.68587742581563,-4.2288354037215,26.5465111541231));
#71780=CARTESIAN_POINT('Ctrl Pts',(-6.6768441846859,-4.24308041089931,26.5471878525473));
#71781=CARTESIAN_POINT('Ctrl Pts',(-6.67273384116231,-4.2495414723716,26.5474947040863));
#71782=CARTESIAN_POINT('Ctrl Pts',(-6.66440107022578,-4.26259788184021,
26.5481146339475));
#71783=CARTESIAN_POINT('Ctrl Pts',(-6.66017821767725,-4.26919294906439,
26.5484276955192));
#71784=CARTESIAN_POINT('Ctrl Pts',(-6.64978792483477,-4.28536711970946,
26.5491952813481));
#71785=CARTESIAN_POINT('Ctrl Pts',(-6.6436095626985,-4.29493920513681,26.5496493875526));
#71786=CARTESIAN_POINT('Ctrl Pts',(-6.62117757717204,-4.32952867388575,
26.5512897757357));
#71787=CARTESIAN_POINT('Ctrl Pts',(-6.60480305178352,-4.35446755861476,
26.5524714267361));
#71788=CARTESIAN_POINT('Ctrl Pts',(-6.37316371728363,-4.70294834648023,
26.5689699783768));
#71789=CARTESIAN_POINT('Ctrl Pts',(-6.13447511987585,-5.01030873932337,
26.583324661585));
#71790=CARTESIAN_POINT('Ctrl Pts',(-5.38878599826297,-5.83694910472618,
26.6228787741273));
#71791=CARTESIAN_POINT('Ctrl Pts',(-4.83187460590466,-6.3056919513229,26.6463418048821));
#71792=CARTESIAN_POINT('Ctrl Pts',(-4.11649365350646,-6.75670754013949,
26.6784377683842));
#71793=CARTESIAN_POINT('Ctrl Pts',(-4.01248728966773,-6.81898522664786,
26.683163292731));
#71794=CARTESIAN_POINT('Ctrl Pts',(-3.89224918264555,-6.88727874699043,
26.6886937144669));
#71795=CARTESIAN_POINT('Ctrl Pts',(-3.87738287971627,-6.8956590864508,26.6893785124154));
#71796=CARTESIAN_POINT('Ctrl Pts',(-3.85538512701272,-6.90796589415586,
26.6903931987763));
#71797=CARTESIAN_POINT('Ctrl Pts',(-3.84827448522773,-6.91192959730584,
26.6907214033687));
#71798=CARTESIAN_POINT('Ctrl Pts',(-3.83556976521688,-6.91898593973979,
26.6913081792572));
#71799=CARTESIAN_POINT('Ctrl Pts',(-3.82997802610118,-6.92208279186529,
26.691566563871));
#71800=CARTESIAN_POINT('Ctrl Pts',(-3.81826416955449,-6.92855169444655,
26.6921080975798));
#71801=CARTESIAN_POINT('Ctrl Pts',(-3.8121413260167,-6.93192241453992,26.6923913042075));
#71802=CARTESIAN_POINT('Ctrl Pts',(-3.79614147610415,-6.94070296981067,
26.6931317321994));
#71803=CARTESIAN_POINT('Ctrl Pts',(-3.78625739007331,-6.94609982624964,
26.6935895067553));
#71804=CARTESIAN_POINT('Ctrl Pts',(-3.74321334568618,-6.96948333467801,
26.6955845666008));
#71805=CARTESIAN_POINT('Ctrl Pts',(-3.70993679490908,-6.98725361093644,
26.6971307866421));
#71806=CARTESIAN_POINT('Ctrl Pts',(-3.45521964523936,-7.12094457416614,
26.7089900778491));
#71807=CARTESIAN_POINT('Ctrl Pts',(-3.22853244460029,-7.22654565123714,
26.7196761825378));
#71808=CARTESIAN_POINT('Ctrl Pts',(-2.5753882025136,-7.49393623537764,26.7502793793018));
#71809=CARTESIAN_POINT('Ctrl Pts',(-2.13939733916224,-7.62985577825859,
26.7704470921711));
#71810=CARTESIAN_POINT('Ctrl Pts',(-1.2745741393656,-7.81945412227201,26.8086540803558));
#71811=CARTESIAN_POINT('Ctrl Pts',(-0.848212687349006,-7.87711744554902,
26.8266892207419));
#71812=CARTESIAN_POINT('Ctrl Pts',(-0.380152875301321,-7.90195786298712,
26.8456919894774));
#71813=CARTESIAN_POINT('Ctrl Pts',(-0.341035719444665,-7.90374271743369,
26.8472745359449));
#71814=CARTESIAN_POINT('Ctrl Pts',(-0.28305752755332,-7.9059569471026,26.8496121382941));
#71815=CARTESIAN_POINT('Ctrl Pts',(-0.264205692785964,-7.90660939776337,
26.8503709543125));
#71816=CARTESIAN_POINT('Ctrl Pts',(-0.232050711490708,-7.9076071319199,
26.8516630767828));
#71817=CARTESIAN_POINT('Ctrl Pts',(-0.218748721954937,-7.90798628497822,
26.8521969747193));
#71818=CARTESIAN_POINT('Ctrl Pts',(-0.191557219965009,-7.90869267671559,
26.8532870577256));
#71819=CARTESIAN_POINT('Ctrl Pts',(-0.177667672550743,-7.90901689357426,
26.8538431872197));
#71820=CARTESIAN_POINT('Ctrl Pts',(-0.145734794371737,-7.90967812505064,
26.8551201738712));
#71821=CARTESIAN_POINT('Ctrl Pts',(-0.127691002476367,-7.90998999261756,
26.8558405748922));
#71822=CARTESIAN_POINT('Ctrl Pts',(-0.0715457219873636,-7.91076823951385,
26.8580785617733));
#71823=CARTESIAN_POINT('Ctrl Pts',(-0.0334416744985713,-7.91102108547707,
26.8595922215144));
#71824=CARTESIAN_POINT('Ctrl Pts',(0.586326756623952,-7.91065578024007,
26.8841284243866));
#71825=CARTESIAN_POINT('Ctrl Pts',(1.16618008228814,-7.84616678562703,26.9056770765643));
#71826=CARTESIAN_POINT('Ctrl Pts',(2.14257718764931,-7.62685101651237,26.9421203250294));
#71827=CARTESIAN_POINT('Ctrl Pts',(2.54344147141739,-7.5026904420863,26.9571931032407));
#71828=CARTESIAN_POINT('Ctrl Pts',(2.9512712745099,-7.33991311900215,26.9739988393092));
#71829=CARTESIAN_POINT('Ctrl Pts',(2.96995028088422,-7.33237492577289,26.9747719970411));
#71830=CARTESIAN_POINT('Ctrl Pts',(3.08735006738658,-7.28447427612128,26.9796541415517));
#71831=CARTESIAN_POINT('Ctrl Pts',(3.18527228683115,-7.24219131542487,26.9838276918068));
#71832=CARTESIAN_POINT('Ctrl Pts',(3.29619598237155,-7.19160942155647,26.9887023216859));
#71833=CARTESIAN_POINT('Ctrl Pts',(3.31006682856318,-7.18523566852529,26.9893145470748));
#71834=CARTESIAN_POINT('Ctrl Pts',(3.33043989449225,-7.17580258551042,26.9902177986928));
#71835=CARTESIAN_POINT('Ctrl Pts',(3.33695658599247,-7.17277445482206,26.9905073286058));
#71836=CARTESIAN_POINT('Ctrl Pts',(3.34854354544349,-7.1673710991995,26.9910232236695));
#71837=CARTESIAN_POINT('Ctrl Pts',(3.35361544072023,-7.16499935972748,26.9912494185789));
#71838=CARTESIAN_POINT('Ctrl Pts',(3.36418890859571,-7.16004126691194,26.9917217618622));
#71839=CARTESIAN_POINT('Ctrl Pts',(3.36969002466698,-7.1574539533237,26.9919679576968));
#71840=CARTESIAN_POINT('Ctrl Pts',(3.38396148675098,-7.15072162487563,26.992607834387));
#71841=CARTESIAN_POINT('Ctrl Pts',(3.39272718239887,-7.14656682364324,26.9930020068059));
#71842=CARTESIAN_POINT('Ctrl Pts',(3.43005914486989,-7.12878789923668,26.9946857422024));
#71843=CARTESIAN_POINT('Ctrl Pts',(3.45855102336243,-7.11500860502383,26.9959832928563));
#71844=CARTESIAN_POINT('Ctrl Pts',(3.66437279006198,-7.01394027753768,27.0054526731039));
#71845=CARTESIAN_POINT('Ctrl Pts',(3.83844834247212,-6.92020886319932,27.0139762750983));
#71846=CARTESIAN_POINT('Ctrl Pts',(4.52528286671108,-6.51648893309566,27.0492316629394));
#71847=CARTESIAN_POINT('Ctrl Pts',(5.005590012512,-6.1552339574266,27.0775318515316));
#71848=CARTESIAN_POINT('Ctrl Pts',(5.78600072616481,-5.41595592669741,27.1261681463026));
#71849=CARTESIAN_POINT('Ctrl Pts',(6.10127615309793,-5.05815265024049,27.1468686914432));
#71850=CARTESIAN_POINT('Ctrl Pts',(6.40111423180907,-4.64872559077335,27.1675295849248));
#71851=CARTESIAN_POINT('Ctrl Pts',(6.41957181548765,-4.62320351719952,27.1688062771329));
#71852=CARTESIAN_POINT('Ctrl Pts',(6.44447182745346,-4.58833658849288,27.1705353325365));
#71853=CARTESIAN_POINT('Ctrl Pts',(6.45104717048535,-4.57908726600077,27.170992573409));
#71854=CARTESIAN_POINT('Ctrl Pts',(6.46217047747764,-4.56336895839991,27.1717671866105));
#71855=CARTESIAN_POINT('Ctrl Pts',(6.46672867670651,-4.55690725742493,27.1720849333047));
#71856=CARTESIAN_POINT('Ctrl Pts',(6.47549969374818,-4.54443380464932,27.1726969708252));
#71857=CARTESIAN_POINT('Ctrl Pts',(6.47971384625439,-4.53842300359883,27.1729913102356));
#71858=CARTESIAN_POINT('Ctrl Pts',(6.48965299322679,-4.52420436885574,27.1736861754239));
#71859=CARTESIAN_POINT('Ctrl Pts',(6.49537079816818,-4.51599151226919,27.1740864390894));
#71860=CARTESIAN_POINT('Ctrl Pts',(6.51205040392488,-4.49193629480981,27.1752555997163));
#71861=CARTESIAN_POINT('Ctrl Pts',(6.52296997119519,-4.47606466678041,27.176022962576));
#71862=CARTESIAN_POINT('Ctrl Pts',(6.60256070058121,-4.35946947670472,27.1816307189061));
#71863=CARTESIAN_POINT('Ctrl Pts',(6.66895509352743,-4.25720817427779,27.1863884991745));
#71864=CARTESIAN_POINT('Ctrl Pts',(6.87725908736984,-3.9195364537011,27.2016145316846));
#71865=CARTESIAN_POINT('Ctrl Pts',(7.00927433155034,-3.67825305314022,27.2117419649909));
#71866=CARTESIAN_POINT('Ctrl Pts',(7.34363108223795,-2.98348588499039,27.2393666218784));
#71867=CARTESIAN_POINT('Ctrl Pts',(7.51625138875095,-2.51715483521127,27.2561246702818));
#71868=CARTESIAN_POINT('Ctrl Pts',(7.75124985886786,-1.63561426779284,27.2879858265191));
#71869=CARTESIAN_POINT('Ctrl Pts',(7.82654812954041,-1.22566580896864,27.3029281031745));
#71870=CARTESIAN_POINT('Ctrl Pts',(7.87201465904843,-0.784877867924856,
27.3205124360066));
#71871=CARTESIAN_POINT('Ctrl Pts',(7.87464410623256,-0.758042371290732,
27.3215880472976));
#71872=CARTESIAN_POINT('Ctrl Pts',(7.87810306337385,-0.720779113916123,
27.3230881917766));
#71873=CARTESIAN_POINT('Ctrl Pts',(7.87904918045207,-0.710362174464526,
27.3235082692306));
#71874=CARTESIAN_POINT('Ctrl Pts',(7.88053034281201,-0.693687224063578,
27.3241818193112));
#71875=CARTESIAN_POINT('Ctrl Pts',(7.88107860148629,-0.687430378834518,
27.324434801578));
#71876=CARTESIAN_POINT('Ctrl Pts',(7.8821931309302,-0.674534538549685,27.3249567243227));
#71877=CARTESIAN_POINT('Ctrl Pts',(7.88275846634275,-0.667895469320237,
27.3252256986466));
#71878=CARTESIAN_POINT('Ctrl Pts',(7.88405184871841,-0.65247610716855,27.3258510280238));
#71879=CARTESIAN_POINT('Ctrl Pts',(7.88477361616578,-0.643695304304122,
27.3262076072471));
#71880=CARTESIAN_POINT('Ctrl Pts',(7.88701594725224,-0.615846056928081,
27.3273400086753));
#71881=CARTESIAN_POINT('Ctrl Pts',(7.88848201236248,-0.596773366852653,
27.3281177278352));
#71882=CARTESIAN_POINT('Ctrl Pts',(7.91824595772938,-0.190272250907117,
27.3447377228723));
#71883=CARTESIAN_POINT('Ctrl Pts',(7.91803756237773,0.198702011401427,27.3614604442978));
#71884=CARTESIAN_POINT('Ctrl Pts',(7.86779346753827,0.875055143247997,27.390746074619));
#71885=CARTESIAN_POINT('Ctrl Pts',(7.83046276168631,1.16264920682545,27.403273493816));
#71886=CARTESIAN_POINT('Ctrl Pts',(7.66673512481276,2.04233063562632,27.4414812843643));
#71887=CARTESIAN_POINT('Ctrl Pts',(7.48816939195346,2.6224617220409,27.4663716334106));
#71888=CARTESIAN_POINT('Ctrl Pts',(7.20830468508872,3.26078498540832,27.4946869329944));
#71889=CARTESIAN_POINT('Ctrl Pts',(7.16991911557229,3.34434376269594,27.4984117712935));
#71890=CARTESIAN_POINT('Ctrl Pts',(7.11512265567787,3.45834404167846,27.5035185721234));
#71891=CARTESIAN_POINT('Ctrl Pts',(7.09995605531491,3.48937500690739,27.5049112384976));
#71892=CARTESIAN_POINT('Ctrl Pts',(7.07352213701872,3.54257305297703,27.5073032703575));
#71893=CARTESIAN_POINT('Ctrl Pts',(7.06235264134946,3.56478813280392,27.5083035274183));
#71894=CARTESIAN_POINT('Ctrl Pts',(7.04021607465496,3.60830328124302,27.5102655551532));
#71895=CARTESIAN_POINT('Ctrl Pts',(7.02925661297004,3.62960692361107,27.5112273877182));
#71896=CARTESIAN_POINT('Ctrl Pts',(7.00277848447357,3.68050692818033,27.5135285883812));
#71897=CARTESIAN_POINT('Ctrl Pts',(6.98716870822562,3.71005541790068,27.5148670302288));
#71898=CARTESIAN_POINT('Ctrl Pts',(6.95407896189088,3.77174299054988,27.5176667487735));
#71899=CARTESIAN_POINT('Ctrl Pts',(6.93656231989072,3.8038615367437,27.519127614949));
#71900=CARTESIAN_POINT('Ctrl Pts',(6.88953814026436,3.88868011972685,27.5229941422977));
#71901=CARTESIAN_POINT('Ctrl Pts',(6.85964873048598,3.94116584462289,27.5253956921561));
#71902=CARTESIAN_POINT('Ctrl Pts',(6.61559558811418,4.35853403788827,27.5445701313407));
#71903=CARTESIAN_POINT('Ctrl Pts',(6.37307310690725,4.70604659744921,27.5609746508008));
#71904=CARTESIAN_POINT('Ctrl Pts',(5.84569406806699,5.34570487104086,27.5930251169877));
#71905=CARTESIAN_POINT('Ctrl Pts',(5.56374962610629,5.63856108874527,27.6086357763255));
#71906=CARTESIAN_POINT('Ctrl Pts',(5.22824375308421,5.93727749384892,27.6265323920733));
#71907=CARTESIAN_POINT('Ctrl Pts',(5.195660901891,5.9658113049236,27.6282641942437));
#71908=CARTESIAN_POINT('Ctrl Pts',(5.15118902371042,6.00411603163212,27.6306210384783));
#71909=CARTESIAN_POINT('Ctrl Pts',(5.13950321394401,6.01412207980838,27.6312397082363));
#71910=CARTESIAN_POINT('Ctrl Pts',(5.11965295485321,6.03101888246819,27.6322896339148));
#71911=CARTESIAN_POINT('Ctrl Pts',(5.111503584499,6.03792731354662,27.6327203928369));
#71912=CARTESIAN_POINT('Ctrl Pts',(5.095770812557,6.05120971054573,27.6335514893774));
#71913=CARTESIAN_POINT('Ctrl Pts',(5.08818938170897,6.05758598373248,27.6339517595927));
#71914=CARTESIAN_POINT('Ctrl Pts',(5.0725899856437,6.07065572468458,27.6347749140902));
#71915=CARTESIAN_POINT('Ctrl Pts',(5.06457070269689,6.07734758646254,27.6351978443987));
#71916=CARTESIAN_POINT('Ctrl Pts',(5.04025274747567,6.09755866371282,27.6364796948681));
#71917=CARTESIAN_POINT('Ctrl Pts',(5.02391314593244,6.11102823648242,27.637340131315));
#71918=CARTESIAN_POINT('Ctrl Pts',(4.91169089049873,6.20278452641663,27.6432434062733));
#71919=CARTESIAN_POINT('Ctrl Pts',(4.81403784051086,6.27887584736698,27.6483483071909));
#71920=CARTESIAN_POINT('Ctrl Pts',(4.44698457214418,6.55128601602659,27.6673494806297));
#71921=CARTESIAN_POINT('Ctrl Pts',(4.16704309101618,6.7328128719612,27.681467129918));
#71922=CARTESIAN_POINT('Ctrl Pts',(3.49486788187357,7.11065919210472,27.7139452771799));
#71923=CARTESIAN_POINT('Ctrl Pts',(3.0960837087615,7.29313848138394,27.7321690558418));
#71924=CARTESIAN_POINT('Ctrl Pts',(2.64101898084673,7.45728174067475,27.7518004601329));
#71925=CARTESIAN_POINT('Ctrl Pts',(2.59766161522202,7.47249532521434,27.7536602150912));
#71926=CARTESIAN_POINT('Ctrl Pts',(2.52773453797921,7.49634974497479,27.7566430681176));
#71927=CARTESIAN_POINT('Ctrl Pts',(2.50124743346664,7.50522902234875,27.7577691215931));
#71928=CARTESIAN_POINT('Ctrl Pts',(2.4544968154364,7.5206262667146,27.7597501206918));
#71929=CARTESIAN_POINT('Ctrl Pts',(2.43425301666154,7.52720308712821,27.7606057812059));
#71930=CARTESIAN_POINT('Ctrl Pts',(2.41387195962422,7.5337336809916,27.7614651323739));
#71931=CARTESIAN_POINT('Ctrl Pts',(2.41376107979313,7.53376920692567,27.7614698074712));
#71932=CARTESIAN_POINT('Ctrl Pts',(2.41354279685651,7.53383913953905,27.7614790109518));
#71933=CARTESIAN_POINT('Ctrl Pts',(2.41343539770515,7.53387354511677,27.7614835391717));
#71934=CARTESIAN_POINT('Ctrl Pts',(2.41322400948941,7.53394125885882,27.761492451718));
#71935=CARTESIAN_POINT('Ctrl Pts',(2.41311996890431,7.53397458368491,27.7614968382206));
#71936=CARTESIAN_POINT('Ctrl Pts',(2.41291516925222,7.5340401775665,27.7615054727627));
#71937=CARTESIAN_POINT('Ctrl Pts',(2.41281441009642,7.53407244679959,27.7615097208098));
#71938=CARTESIAN_POINT('Ctrl Pts',(2.41261604714609,7.53413597033904,27.7615180837707));
#71939=CARTESIAN_POINT('Ctrl Pts',(2.41251844356679,7.53416722471391,27.7615221986787));
#71940=CARTESIAN_POINT('Ctrl Pts',(2.41232628704227,7.53422875248035,27.7615302997861));
#71941=CARTESIAN_POINT('Ctrl Pts',(2.41223173403143,7.53425902602164,27.7615342859913));
#71942=CARTESIAN_POINT('Ctrl Pts',(2.41206413926481,7.53431268225275,27.7615413514405));
#71943=CARTESIAN_POINT('Ctrl Pts',(2.41199111416306,7.53433606040207,27.7615444300006));
#71944=CARTESIAN_POINT('Ctrl Pts',(2.41184560964406,7.53438263967457,27.7615505640623));
#71945=CARTESIAN_POINT('Ctrl Pts',(2.4117731312072,7.534405840501,27.7615536195227));
#71946=CARTESIAN_POINT('Ctrl Pts',(2.41162872010481,7.5344520651516,27.7615597073823));
#71947=CARTESIAN_POINT('Ctrl Pts',(2.41155678815637,7.53447508876354,27.7615627397516));
#71948=CARTESIAN_POINT('Ctrl Pts',(2.41141346480107,7.53452096071091,27.7615687816505));
#71949=CARTESIAN_POINT('Ctrl Pts',(2.4113420743052,7.53454380877178,27.7615717911421));
#71950=CARTESIAN_POINT('Ctrl Pts',(2.41119982871127,7.53458933131424,27.7615777875037));
#71951=CARTESIAN_POINT('Ctrl Pts',(2.41112897444595,7.53461200554604,27.761580774339));
#71952=CARTESIAN_POINT('Ctrl Pts',(2.41098779612116,7.53465718214196,27.7615867256079));
#71953=CARTESIAN_POINT('Ctrl Pts',(2.41091747310987,7.5346796841871,27.7615896899978));
#71954=CARTESIAN_POINT('Ctrl Pts',(2.41077735230251,7.53472451805588,27.7615955965875));
#71955=CARTESIAN_POINT('Ctrl Pts',(2.41070755540548,7.53474684960801,27.7615985387497));
#71956=CARTESIAN_POINT('Ctrl Pts',(2.41056848181816,7.53479134414165,27.7616044010965));
#71957=CARTESIAN_POINT('Ctrl Pts',(2.41049920617094,7.53481350680533,27.7616073212373));
#71958=CARTESIAN_POINT('Ctrl Pts',(2.41036117026654,7.53485766515065,27.7616131397453));
#71959=CARTESIAN_POINT('Ctrl Pts',(2.41029241084389,7.53487966058094,27.7616160380777));
#71960=CARTESIAN_POINT('Ctrl Pts',(2.41015540235864,7.53492348611532,27.7616218131818));
#71961=CARTESIAN_POINT('Ctrl Pts',(2.41008715450086,7.53494531584937,27.7616246899032));
#71962=CARTESIAN_POINT('Ctrl Pts',(2.40995116431534,7.53498881158225,27.76163042199));
#71963=CARTESIAN_POINT('Ctrl Pts',(2.40988342305291,7.53501047725542,27.7616332773109));
#71964=CARTESIAN_POINT('Ctrl Pts',(2.40974844132029,7.53505364642708,27.7616389667975));
#71965=CARTESIAN_POINT('Ctrl Pts',(2.40968120197208,7.53507514958157,27.7616418009163));
#71966=CARTESIAN_POINT('Ctrl Pts',(2.40954721931298,7.53511799528097,27.7616474482002));
#71967=CARTESIAN_POINT('Ctrl Pts',(2.4094804771886,7.53513933746103,27.7616502613156));
#71968=CARTESIAN_POINT('Ctrl Pts',(2.40934748432725,7.53518186274223,27.7616558667898));
#71969=CARTESIAN_POINT('Ctrl Pts',(2.40928123475648,7.5352030454848,27.7616586590997));
#71970=CARTESIAN_POINT('Ctrl Pts',(2.40914922245572,7.53524525338779,27.7616642231555));
#71971=CARTESIAN_POINT('Ctrl Pts',(2.40908346083661,7.53526627820712,27.7616669948548));
#71972=CARTESIAN_POINT('Ctrl Pts',(2.40895241984852,7.53530817177361,27.761672517884));
#71973=CARTESIAN_POINT('Ctrl Pts',(2.40888714169459,7.53532904014618,27.7616752691629));
#71974=CARTESIAN_POINT('Ctrl Pts',(2.40875706307799,7.53537062231813,27.7616807515442));
#71975=CARTESIAN_POINT('Ctrl Pts',(2.4086922638823,7.53539133572613,27.7616834825935));
#71976=CARTESIAN_POINT('Ctrl Pts',(2.38653437342672,7.54247390840601,27.7626173494076));
#71977=CARTESIAN_POINT('Ctrl Pts',(2.36441028851278,7.54943858617563,27.7635473069478));
#71978=CARTESIAN_POINT('Ctrl Pts',(2.3057135131476,7.5676330409355,27.7660081373301));
#71979=CARTESIAN_POINT('Ctrl Pts',(2.26908937636123,7.57869501086796,27.7675370059045));
#71980=CARTESIAN_POINT('Ctrl Pts',(2.18800566083259,7.60254511881239,27.7709079917402));
#71981=CARTESIAN_POINT('Ctrl Pts',(2.14351119295588,7.61520983638117,27.7727486686793));
#71982=CARTESIAN_POINT('Ctrl Pts',(2.0090515927684,7.6522100255411,27.7782853861594));
#71983=CARTESIAN_POINT('Ctrl Pts',(1.91876469890791,7.67534682114395,27.7819685960052));
#71984=CARTESIAN_POINT('Ctrl Pts',(1.56587088631675,7.75916276083621,27.7962530929716));
#71985=CARTESIAN_POINT('Ctrl Pts',(1.30063353999508,7.80800328896239,27.8067786896681));
#71986=CARTESIAN_POINT('Ctrl Pts',(0.678545703696835,7.88996956763789,27.8310670562652));
#71987=CARTESIAN_POINT('Ctrl Pts',(0.320900900958636,7.91258977232274,27.8446775408132));
#71988=CARTESIAN_POINT('Ctrl Pts',(-0.610028097376528,7.90822958728728,
27.8796771442475));
#71989=CARTESIAN_POINT('Ctrl Pts',(-1.18098042953533,7.84330529232685,27.900633179886));
#71990=CARTESIAN_POINT('Ctrl Pts',(-1.75903284846369,7.71298323588363,27.923847265959));
#71991=CARTESIAN_POINT('Ctrl Pts',(-1.77818143760208,7.7085911636356,27.9246187549463));
#71992=CARTESIAN_POINT('Ctrl Pts',(-1.82791316106835,7.69698913746483,27.9266292755805));
#71993=CARTESIAN_POINT('Ctrl Pts',(-1.85846992711701,7.68966825100608,27.9278713497798));
#71994=CARTESIAN_POINT('Ctrl Pts',(-1.9213884683283,7.67419709322354,27.9304439553221));
#71995=CARTESIAN_POINT('Ctrl Pts',(-1.95374388393988,7.66602370680407,27.9317751645656));
#71996=CARTESIAN_POINT('Ctrl Pts',(-1.99778133478408,7.6546023875245,27.9335992328));
#71997=CARTESIAN_POINT('Ctrl Pts',(-2.00950926511531,7.65153190441981,27.9340861987137));
#71998=CARTESIAN_POINT('Ctrl Pts',(-2.0280649634662,7.6466282427248,27.9348585967848));
#71999=CARTESIAN_POINT('Ctrl Pts',(-2.03489743565709,7.6448128429998,27.9351434196245));
#72000=CARTESIAN_POINT('Ctrl Pts',(-2.04811319234573,7.64128242109991,27.935695156109));
#72001=CARTESIAN_POINT('Ctrl Pts',(-2.05449677989012,7.639568552528,27.9359620293122));
#72002=CARTESIAN_POINT('Ctrl Pts',(-2.06964832810854,7.63548029353204,27.9365963459412));
#72003=CARTESIAN_POINT('Ctrl Pts',(-2.07841435164152,7.63309880042477,27.9369640410639));
#72004=CARTESIAN_POINT('Ctrl Pts',(-2.1043069575169,7.62601656473729,27.9380522520825));
#72005=CARTESIAN_POINT('Ctrl Pts',(-2.12142177177624,7.62127325826567,27.9387743116736));
#72006=CARTESIAN_POINT('Ctrl Pts',(-2.2597644476746,7.58242999626432,27.9446340948373));
#72007=CARTESIAN_POINT('Ctrl Pts',(-2.38016438947108,7.54550176332656,27.9498832347025));
#72008=CARTESIAN_POINT('Ctrl Pts',(-2.640698181632,7.45873564586007,27.9616174203887));
#72009=CARTESIAN_POINT('Ctrl Pts',(-2.78039584289463,7.40779453023576,27.9681359323521));
#72010=CARTESIAN_POINT('Ctrl Pts',(-3.09682941297819,7.2821941488284,27.9833048501267));
#72011=CARTESIAN_POINT('Ctrl Pts',(-3.27245325530868,7.2049809219385,27.9920195523561));
#72012=CARTESIAN_POINT('Ctrl Pts',(-3.61536808775942,7.0390918117813,28.0094330581364));
#72013=CARTESIAN_POINT('Ctrl Pts',(-3.78263441217647,6.95063861221565,28.0181248111665));
#72014=CARTESIAN_POINT('Ctrl Pts',(-4.4573263159712,6.56227634423336,28.0536943887056));
#72015=CARTESIAN_POINT('Ctrl Pts',(-4.93369485062658,6.21209029757279,28.0798603743371));
#72016=CARTESIAN_POINT('Ctrl Pts',(-5.39382914491411,5.78721720954648,28.1053893570867));
#72017=CARTESIAN_POINT('Ctrl Pts',(-5.42069795320241,5.76205775936328,28.1068818759532));
#72018=CARTESIAN_POINT('Ctrl Pts',(-5.45693447104418,5.72764876718623,28.1088973339125));
#72019=CARTESIAN_POINT('Ctrl Pts',(-5.466455915722,5.71856222709284,28.1094271568823));
#72020=CARTESIAN_POINT('Ctrl Pts',(-5.48144378012906,5.70418731563782,28.1102615556022));
#72021=CARTESIAN_POINT('Ctrl Pts',(-5.48692530482257,5.69891476917314,28.1105668049021));
#72022=CARTESIAN_POINT('Ctrl Pts',(-5.49748538664941,5.68872792153926,28.1111550277991));
#72023=CARTESIAN_POINT('Ctrl Pts',(-5.50256497797338,5.68381470539292,28.1114380473471));
#72024=CARTESIAN_POINT('Ctrl Pts',(-5.51456041234048,5.67218101367929,28.1121065734927));
#72025=CARTESIAN_POINT('Ctrl Pts',(-5.52147057140741,5.66545467930172,28.112491827781));
#72026=CARTESIAN_POINT('Ctrl Pts',(-5.54167072923172,5.64571982770468,28.1136184404968));
#72027=CARTESIAN_POINT('Ctrl Pts',(-5.55492721844101,5.63267702322526,28.1143583169358));
#72028=CARTESIAN_POINT('Ctrl Pts',(-5.65237284011208,5.53612356066904,28.1198010591183));
#72029=CARTESIAN_POINT('Ctrl Pts',(-5.734722754409,5.45077418613406,28.1244228233983));
#72030=CARTESIAN_POINT('Ctrl Pts',(-6.03296525320804,5.12742487426509,28.1412735924021));
#72031=CARTESIAN_POINT('Ctrl Pts',(-6.23622395794494,4.87818493035999,28.1529707174204));
#72032=CARTESIAN_POINT('Ctrl Pts',(-6.4855866561619,4.53125853418781,28.1680159066556));
#72033=CARTESIAN_POINT('Ctrl Pts',(-6.54566914125742,4.44402454730085,28.1717041496508));
#72034=CARTESIAN_POINT('Ctrl Pts',(-6.66328984415847,4.26568783480336,28.1790864355487));
#72035=CARTESIAN_POINT('Ctrl Pts',(-6.72075463821378,4.17456364898016,28.182778718532));
#72036=CARTESIAN_POINT('Ctrl Pts',(-7.09225404166409,3.55789891216932,28.2073618737278));
#72037=CARTESIAN_POINT('Ctrl Pts',(-7.3461939045247,2.99866356383236,28.2276039530862));
#72038=CARTESIAN_POINT('Ctrl Pts',(-7.5570054777368,2.34130619710707,28.2542257774296));
#72039=CARTESIAN_POINT('Ctrl Pts',(-7.57979793510687,2.26643090042485,28.2572991335334));
#72040=CARTESIAN_POINT('Ctrl Pts',(-7.60469059143986,2.18007724130886,28.2609024469297));
#72041=CARTESIAN_POINT('Ctrl Pts',(-7.60788155081493,2.1689154146039,28.261369322989));
#72042=CARTESIAN_POINT('Ctrl Pts',(-7.61254159247629,2.15247798892071,28.2620585665311));
#72043=CARTESIAN_POINT('Ctrl Pts',(-7.61402979607196,2.14720778086619,28.2622798104047));
#72044=CARTESIAN_POINT('Ctrl Pts',(-7.61666889814576,2.13782462727274,28.2626741795955));
#72045=CARTESIAN_POINT('Ctrl Pts',(-7.61782194185423,2.13371228215564,28.2628471777023));
#72046=CARTESIAN_POINT('Ctrl Pts',(-7.62022077929459,2.12513006815882,28.2632085479972));
#72047=CARTESIAN_POINT('Ctrl Pts',(-7.62146597121516,2.12066003433308,28.2633969559858));
#72048=CARTESIAN_POINT('Ctrl Pts',(-7.62468914498746,2.10904986578274,28.263886810072));
#72049=CARTESIAN_POINT('Ctrl Pts',(-7.6266610262553,2.10190805791161,28.264188622482));
#72050=CARTESIAN_POINT('Ctrl Pts',(-7.63529858816319,2.0704521432846,28.2655201277558));
#72051=CARTESIAN_POINT('Ctrl Pts',(-7.64185794446066,2.04610941125025,28.2665562984237));
#72052=CARTESIAN_POINT('Ctrl Pts',(-7.68959802676401,1.86550695766192,28.2742840129058));
#72053=CARTESIAN_POINT('Ctrl Pts',(-7.72609642892959,1.70805789823672,28.2812430857041));
#72054=CARTESIAN_POINT('Ctrl Pts',(-7.85916345205061,1.0418910141892,28.3112600394506));
#72055=CARTESIAN_POINT('Ctrl Pts',(-7.9104895321659,0.525463859223298,28.3358246275417));
#72056=CARTESIAN_POINT('Ctrl Pts',(-7.91099621143461,0.00774226499310415,
28.3596644754603));
#72057=CARTESIAN_POINT('',(-7.911,-2.37587727269783E-12,30.3576684917631));
#72058=CARTESIAN_POINT('Ctrl Pts',(-7.911,-2.54574139546548E-12,28.3576684917631));
#72059=CARTESIAN_POINT('Ctrl Pts',(-7.91099999999929,-2.20167589666934,
28.4462559274958));
#72060=CARTESIAN_POINT('Ctrl Pts',(-6.94214576672227,-4.38610418338912,
28.5348433632286));
#72061=CARTESIAN_POINT('Ctrl Pts',(-3.67820201488039,-7.34180684107757,
28.712018234694));
#72062=CARTESIAN_POINT('Ctrl Pts',(-1.40868175871468,-8.08992666571385,
28.8006056704267));
#72063=CARTESIAN_POINT('Ctrl Pts',(2.9730927052154,-7.65454228025154,28.9777805418922));
#72064=CARTESIAN_POINT('Ctrl Pts',(5.05102072675831,-6.47444880834048,29.0663679776249));
#72065=CARTESIAN_POINT('Ctrl Pts',(7.66951518847978,-2.93425195367432,29.2435428490904));
#72066=CARTESIAN_POINT('Ctrl Pts',(8.18956872247094,-0.601881960096201,
29.3321302848231));
#72067=CARTESIAN_POINT('Ctrl Pts',(7.32306689761206,3.7153719823272,29.5093051562886));
#72068=CARTESIAN_POINT('Ctrl Pts',(5.94329958849991,5.66643518936733,29.5978925920213));
#72069=CARTESIAN_POINT('Ctrl Pts',(2.16154501637547,7.9220591323308,29.7750674634867));
#72070=CARTESIAN_POINT('Ctrl Pts',(-0.210816529303517,8.20894963712995,
29.8636548992195));
#72071=CARTESIAN_POINT('Ctrl Pts',(-4.42123908576708,6.91982244717659,30.0408297706849));
#72072=CARTESIAN_POINT('Ctrl Pts',(-6.226316256344,5.35390358803276,30.1294172064176));
#72073=CARTESIAN_POINT('Ctrl Pts',(-7.65317280859569,2.31334857514238,30.264559258688));
#72074=CARTESIAN_POINT('Ctrl Pts',(-7.91100000000035,1.15702837836256,30.3111138752255));
#72075=CARTESIAN_POINT('Ctrl Pts',(-7.911,-2.37587727269783E-12,30.3576684917631));
#72076=CARTESIAN_POINT('',(-7.91024367631032,0.00400354093750647,34.3576684917631));
#72077=CARTESIAN_POINT('Ctrl Pts',(-7.91099920125805,-0.00355495352692831,
30.3653171807264));
#72078=CARTESIAN_POINT('Ctrl Pts',(-7.91060312412407,-0.884963350813036,
30.3979267782199));
#72079=CARTESIAN_POINT('Ctrl Pts',(-7.76292703746049,-1.76000380474951,
30.4255138963057));
#72080=CARTESIAN_POINT('Ctrl Pts',(-7.42189359812388,-2.74313434757834,
30.463310969466));
#72081=CARTESIAN_POINT('Ctrl Pts',(-7.3651632720638,-2.89199859532217,30.4692547066593));
#72082=CARTESIAN_POINT('Ctrl Pts',(-7.27814038175919,-3.1011479366229,30.4780455188782));
#72083=CARTESIAN_POINT('Ctrl Pts',(-7.2515088280524,-3.16292035659979,30.4806977990225));
#72084=CARTESIAN_POINT('Ctrl Pts',(-7.21993112783547,-3.23366971154254,
30.4838078375857));
#72085=CARTESIAN_POINT('Ctrl Pts',(-7.21575073109272,-3.24298730786078,
30.4842188811017));
#72086=CARTESIAN_POINT('Ctrl Pts',(-7.20939252565837,-3.25708581571384,
30.4848430744588));
#72087=CARTESIAN_POINT('Ctrl Pts',(-7.2072279639431,-3.26187272520651,30.4850554007007));
#72088=CARTESIAN_POINT('Ctrl Pts',(-7.20347653105907,-3.27014702216382,
30.4854230956453));
#72089=CARTESIAN_POINT('Ctrl Pts',(-7.20189188935338,-3.27363542473126,
30.485578324346));
#72090=CARTESIAN_POINT('Ctrl Pts',(-7.19860399699981,-3.28085939197745,
30.485900218467));
#72091=CARTESIAN_POINT('Ctrl Pts',(-7.19690037164981,-3.28459478413672,
30.486066907572));
#72092=CARTESIAN_POINT('Ctrl Pts',(-7.19276087050353,-3.29365242848827,
30.4864716916494));
#72093=CARTESIAN_POINT('Ctrl Pts',(-7.19032199768044,-3.29897329926115,
30.4867099775843));
#72094=CARTESIAN_POINT('Ctrl Pts',(-7.181043549368,-3.31915685402946,30.4876157681417));
#72095=CARTESIAN_POINT('Ctrl Pts',(-7.17416390688409,-3.33400073494111,
30.4882858742115));
#72096=CARTESIAN_POINT('Ctrl Pts',(-7.05147293841193,-3.59658714502922,
30.50020870706));
#72097=CARTESIAN_POINT('Ctrl Pts',(-6.92294710521461,-3.83816193688928,
30.5122567648152));
#72098=CARTESIAN_POINT('Ctrl Pts',(-6.69062791188648,-4.22505042662448,
30.5327246761899));
#72099=CARTESIAN_POINT('Ctrl Pts',(-6.59395503197211,-4.3743922075168,30.5409362172563));
#72100=CARTESIAN_POINT('Ctrl Pts',(-6.25394976808366,-4.86272386638663,
30.5685435971015));
#72101=CARTESIAN_POINT('Ctrl Pts',(-5.9888401199099,-5.18573073278105,30.5880340152787));
#72102=CARTESIAN_POINT('Ctrl Pts',(-5.46211515191264,-5.73291971264871,
30.6220384897984));
#72103=CARTESIAN_POINT('Ctrl Pts',(-5.20897968555213,-5.9638612999378,30.6367919632479));
#72104=CARTESIAN_POINT('Ctrl Pts',(-4.9156159914246,-6.19852823031809,30.6521557821943));
#72105=CARTESIAN_POINT('Ctrl Pts',(-4.88944631697091,-6.21919187266309,
30.6535123647288));
#72106=CARTESIAN_POINT('Ctrl Pts',(-4.85000181318907,-6.24993449193625,
30.655536371107));
#72107=CARTESIAN_POINT('Ctrl Pts',(-4.83682467927748,-6.26013783938651,
30.6562090932728));
#72108=CARTESIAN_POINT('Ctrl Pts',(-4.81558327261646,-6.27647842644345,
30.657288026596));
#72109=CARTESIAN_POINT('Ctrl Pts',(-4.80753931514613,-6.28264191463366,
30.6576953516203));
#72110=CARTESIAN_POINT('Ctrl Pts',(-4.7921505523098,-6.29438632241335,30.6584722030826));
#72111=CARTESIAN_POINT('Ctrl Pts',(-4.78480778885031,-6.29996988217775,
30.6588418410599));
#72112=CARTESIAN_POINT('Ctrl Pts',(-4.77179391518922,-6.30982997239186,
30.6594951356247));
#72113=CARTESIAN_POINT('Ctrl Pts',(-4.7661267875593,-6.31411172650571,30.6597790125707));
#72114=CARTESIAN_POINT('Ctrl Pts',(-4.75496090660317,-6.32252442283372,
30.6603371311269));
#72115=CARTESIAN_POINT('Ctrl Pts',(-4.74946251900478,-6.32665583713298,
30.6606113925113));
#72116=CARTESIAN_POINT('Ctrl Pts',(-4.73625625671035,-6.33655192618142,
30.6612687577214));
#72117=CARTESIAN_POINT('Ctrl Pts',(-4.72854322573208,-6.34230972168188,
30.6616515724326));
#72118=CARTESIAN_POINT('Ctrl Pts',(-4.70054433966655,-6.36313148914015,
30.6630371933592));
#72119=CARTESIAN_POINT('Ctrl Pts',(-4.68019674598859,-6.37811240668014,
30.6640365212823));
#72120=CARTESIAN_POINT('Ctrl Pts',(-4.35089928347479,-6.61813336331553,
30.6800874699453));
#72121=CARTESIAN_POINT('Ctrl Pts',(-4.02609970597036,-6.82059945136334,
30.6941588217865));
#72122=CARTESIAN_POINT('Ctrl Pts',(-3.50426161557939,-7.09557323358911,
30.7149094042061));
#72123=CARTESIAN_POINT('Ctrl Pts',(-3.31687961446773,-7.18507633364875,
30.7220279541172));
#72124=CARTESIAN_POINT('Ctrl Pts',(-2.7866794233017,-7.41315979245692,30.7416262099554));
#72125=CARTESIAN_POINT('Ctrl Pts',(-2.43736177314507,-7.53523537258662,
30.7539137988252));
#72126=CARTESIAN_POINT('Ctrl Pts',(-1.77539942391532,-7.71570356526808,
30.7779107272071));
#72127=CARTESIAN_POINT('Ctrl Pts',(-1.46530143179927,-7.78055123014887,
30.7894383335952));
#72128=CARTESIAN_POINT('Ctrl Pts',(-1.14011820973023,-7.82842259364277,
30.8025971405579));
#72129=CARTESIAN_POINT('Ctrl Pts',(-1.12804440008767,-7.83017149651902,
30.8030872413475));
#72130=CARTESIAN_POINT('Ctrl Pts',(-1.11059275765077,-7.83265818173073,
30.803797905035));
#72131=CARTESIAN_POINT('Ctrl Pts',(-1.10521811742434,-7.83341837118187,
30.8040170814458));
#72132=CARTESIAN_POINT('Ctrl Pts',(-1.09580323035483,-7.83474013091302,
30.8044015653175));
#72133=CARTESIAN_POINT('Ctrl Pts',(-1.0917633699312,-7.83530410274844,30.804566720435));
#72134=CARTESIAN_POINT('Ctrl Pts',(-1.08392166453407,-7.83639263656369,
30.8048876390319));
#72135=CARTESIAN_POINT('Ctrl Pts',(-1.08011986964507,-7.83691755707138,
30.8050433804356));
#72136=CARTESIAN_POINT('Ctrl Pts',(-1.07104908786558,-7.83816324996986,
30.8054153330873));
#72137=CARTESIAN_POINT('Ctrl Pts',(-1.06577975970749,-7.83888147539604,
30.8056316994712));
#72138=CARTESIAN_POINT('Ctrl Pts',(-1.04986684595157,-7.84103411224908,
30.8062859877939));
#72139=CARTESIAN_POINT('Ctrl Pts',(-1.03922109876303,-7.84245215792203,
30.8067248962862));
#72140=CARTESIAN_POINT('Ctrl Pts',(-0.932363279012059,-7.85646454226463,
30.8111421826469));
#72141=CARTESIAN_POINT('Ctrl Pts',(-0.83593389435246,-7.86730890289019,
30.8152234589616));
#72142=CARTESIAN_POINT('Ctrl Pts',(-0.589066249673858,-7.8904816816879,
30.825870624684));
#72143=CARTESIAN_POINT('Ctrl Pts',(-0.438433075831382,-7.90028304646046,
30.8325548575094));
#72144=CARTESIAN_POINT('Ctrl Pts',(0.472141298527506,-7.93341064097906,
30.8737208893049));
#72145=CARTESIAN_POINT('Ctrl Pts',(1.23195256747041,-7.85139931491644,30.910799115841));
#72146=CARTESIAN_POINT('Ctrl Pts',(2.20185962885061,-7.60222349820075,30.9553548133858));
#72147=CARTESIAN_POINT('Ctrl Pts',(2.43240155306293,-7.53162827794695,30.9657728874423));
#72148=CARTESIAN_POINT('Ctrl Pts',(2.72732737222575,-7.42635927286325,30.9788503146075));
#72149=CARTESIAN_POINT('Ctrl Pts',(2.79494487333692,-7.40117627003489,30.9818315289005));
#72150=CARTESIAN_POINT('Ctrl Pts',(2.89011392967679,-7.36424187520213,30.9860043232094));
#72151=CARTESIAN_POINT('Ctrl Pts',(2.91795668595226,-7.35325409113056,30.9872222962018));
#72152=CARTESIAN_POINT('Ctrl Pts',(2.96019326116399,-7.33630830137857,30.9890657459639));
#72153=CARTESIAN_POINT('Ctrl Pts',(2.97463279217727,-7.33046542804557,30.9896952257405));
#72154=CARTESIAN_POINT('Ctrl Pts',(3.00112624968517,-7.31965383158318,30.9908488408604));
#72155=CARTESIAN_POINT('Ctrl Pts',(3.01318531350744,-7.31469789187549,30.9913734195874));
#72156=CARTESIAN_POINT('Ctrl Pts',(3.03279621646187,-7.30658163064384,30.9922256858691));
#72157=CARTESIAN_POINT('Ctrl Pts',(3.04035547449334,-7.30343936820892,30.9925540025439));
#72158=CARTESIAN_POINT('Ctrl Pts',(3.05484172840246,-7.29739127641125,30.9931827965578));
#72159=CARTESIAN_POINT('Ctrl Pts',(3.06176948716682,-7.29448730443067,30.9934833382366));
#72160=CARTESIAN_POINT('Ctrl Pts',(3.07749529313766,-7.28786902475474,30.9941651848802));
#72161=CARTESIAN_POINT('Ctrl Pts',(3.08629077944693,-7.28414864118051,30.9945462772635));
#72162=CARTESIAN_POINT('Ctrl Pts',(3.10895269339301,-7.27451451295729,30.9955274994458));
#72163=CARTESIAN_POINT('Ctrl Pts',(3.12280902241621,-7.26857703142814,30.9961267998536));
#72164=CARTESIAN_POINT('Ctrl Pts',(3.20463617693524,-7.23323665602835,30.999662125855));
#72165=CARTESIAN_POINT('Ctrl Pts',(3.27220943062045,-7.20291964207612,31.0025661082263));
#72166=CARTESIAN_POINT('Ctrl Pts',(3.84491603132704,-6.93624952811896,31.027064766771));
#72167=CARTESIAN_POINT('Ctrl Pts',(4.32419932658879,-6.64802971885325,31.0466563131154));
#72168=CARTESIAN_POINT('Ctrl Pts',(5.06994459708018,-6.08454387233539,31.0789532875692));
#72169=CARTESIAN_POINT('Ctrl Pts',(5.35405536947215,-5.83610152476604,31.0918362443326));
#72170=CARTESIAN_POINT('Ctrl Pts',(5.73842597110009,-5.44821092649485,31.1116499078771));
#72171=CARTESIAN_POINT('Ctrl Pts',(5.8536015138051,-5.32427262605735,31.1179455178552));
#72172=CARTESIAN_POINT('Ctrl Pts',(6.01711679478501,-5.13659332998736,31.1275841946935));
#72173=CARTESIAN_POINT('Ctrl Pts',(6.06860768793099,-5.07565612653685,31.1307307844488));
#72174=CARTESIAN_POINT('Ctrl Pts',(6.12826319842071,-5.00285090648096,31.1345016672797));
#72175=CARTESIAN_POINT('Ctrl Pts',(6.13733007459012,-4.99172380781719,31.135078291832));
#72176=CARTESIAN_POINT('Ctrl Pts',(6.15119639623407,-4.97461181878337,31.1359654656859));
#72177=CARTESIAN_POINT('Ctrl Pts',(6.15601753073699,-4.96864448449911,31.1362749178635));
#72178=CARTESIAN_POINT('Ctrl Pts',(6.16480419856887,-4.95773641188236,31.1368407096842));
#72179=CARTESIAN_POINT('Ctrl Pts',(6.16877249515417,-4.95279790008913,31.137096912204));
#72180=CARTESIAN_POINT('Ctrl Pts',(6.17735149161495,-4.94209510578575,31.1376522493715));
#72181=CARTESIAN_POINT('Ctrl Pts',(6.18196006238769,-4.93632912923834,31.1379514871591));
#72182=CARTESIAN_POINT('Ctrl Pts',(6.19446434434433,-4.92063952221115,31.1387658745215));
#72183=CARTESIAN_POINT('Ctrl Pts',(6.20234425614442,-4.91070336579804,31.1392817756522));
#72184=CARTESIAN_POINT('Ctrl Pts',(6.23974344267957,-4.86331133093884,31.1417430354073));
#72185=CARTESIAN_POINT('Ctrl Pts',(6.26894717859584,-4.82560840612285,31.1437028445916));
#72186=CARTESIAN_POINT('Ctrl Pts',(6.59752545899825,-4.39338688429603,31.1661722291948));
#72187=CARTESIAN_POINT('Ctrl Pts',(6.85954967461005,-3.97186851748783,31.1880379696263));
#72188=CARTESIAN_POINT('Ctrl Pts',(7.24213491691667,-3.20418789103403,31.2255722810119));
#72189=CARTESIAN_POINT('Ctrl Pts',(7.38134480055917,-2.86899050018733,31.2413027165437));
#72190=CARTESIAN_POINT('Ctrl Pts',(7.57607418417918,-2.29090732904578,31.2670837268361));
#72191=CARTESIAN_POINT('Ctrl Pts',(7.64402531897234,-2.05281308150819,31.2773444918702));
#72192=CARTESIAN_POINT('Ctrl Pts',(7.71343001058933,-1.75784089072636,31.2896636448816));
#72193=CARTESIAN_POINT('Ctrl Pts',(7.72558385120725,-1.70363181445123,31.2919119648223));
#72194=CARTESIAN_POINT('Ctrl Pts',(7.74160035335889,-1.62849544674163,31.2950075332478));
#72195=CARTESIAN_POINT('Ctrl Pts',(7.74595103764545,-1.60767408969779,31.2958631477727));
#72196=CARTESIAN_POINT('Ctrl Pts',(7.75312173895509,-1.57265187065761,31.2972985925961));
#72197=CARTESIAN_POINT('Ctrl Pts',(7.75598683743078,-1.55846038915843,31.2978792279422));
#72198=CARTESIAN_POINT('Ctrl Pts',(7.76154234292019,-1.53054792786461,31.2990192289511));
#72199=CARTESIAN_POINT('Ctrl Pts',(7.76423536262972,-1.51682752335679,31.2995786402218));
#72200=CARTESIAN_POINT('Ctrl Pts',(7.77008979712634,-1.48657620296027,31.3008099435709));
#72201=CARTESIAN_POINT('Ctrl Pts',(7.77323486412581,-1.47004218047487,31.301481532466));
#72202=CARTESIAN_POINT('Ctrl Pts',(7.78349876186327,-1.41512953856948,31.3037074112258));
#72203=CARTESIAN_POINT('Ctrl Pts',(7.79038634373476,-1.37670811553079,31.3052573731454));
#72204=CARTESIAN_POINT('Ctrl Pts',(7.86357900991018,-0.950264665550267,
31.3223786946493));
#72205=CARTESIAN_POINT('Ctrl Pts',(7.90112051485106,-0.55785341012628,31.337339355633));
#72206=CARTESIAN_POINT('Ctrl Pts',(7.92354632733192,0.521992051633251,31.3773062121688));
#72207=CARTESIAN_POINT('Ctrl Pts',(7.84842631290132,1.2070882678104,31.4011337169805));
#72208=CARTESIAN_POINT('Ctrl Pts',(7.67369595031647,1.92378736809428,31.4301286983926));
#72209=CARTESIAN_POINT('Ctrl Pts',(7.66102409454298,1.97364562030095,31.4321693483615));
#72210=CARTESIAN_POINT('Ctrl Pts',(7.64493362965968,2.03446364935185,31.4346911359885));
#72211=CARTESIAN_POINT('Ctrl Pts',(7.64197608579264,2.04554492608356,31.4351519426416));
#72212=CARTESIAN_POINT('Ctrl Pts',(7.63731155154349,2.06287061419628,31.435874548951));
#72213=CARTESIAN_POINT('Ctrl Pts',(7.63562096875154,2.0691194570294,31.4361356049262));
#72214=CARTESIAN_POINT('Ctrl Pts',(7.63261505783495,2.08017624864531,31.4365983004786));
#72215=CARTESIAN_POINT('Ctrl Pts',(7.6313028506043,2.0849850475955,31.4367997963202));
#72216=CARTESIAN_POINT('Ctrl Pts',(7.62850343743843,2.09520591046973,31.4372286270021));
#72217=CARTESIAN_POINT('Ctrl Pts',(7.62701501562688,2.1006176361813,31.437456018396));
#72218=CARTESIAN_POINT('Ctrl Pts',(7.62274968208299,2.11606158730045,31.4381059140786));
#72219=CARTESIAN_POINT('Ctrl Pts',(7.6199587342022,2.12608989565351,31.4385290805968));
#72220=CARTESIAN_POINT('Ctrl Pts',(7.60789738701082,2.16909936319313,31.4403490754998));
#72221=CARTESIAN_POINT('Ctrl Pts',(7.59843265055139,2.20202542030444,31.4417553434923));
#72222=CARTESIAN_POINT('Ctrl Pts',(7.43808248871584,2.74650789195676,31.4652381138569));
#72223=CARTESIAN_POINT('Ctrl Pts',(7.23607042515302,3.2415379525862,31.4898234140032));
#72224=CARTESIAN_POINT('Ctrl Pts',(6.7730884959596,4.11274909002927,31.5353007538303));
#72225=CARTESIAN_POINT('Ctrl Pts',(6.5263190051239,4.49406820842912,31.5561060003558));
#72226=CARTESIAN_POINT('Ctrl Pts',(6.12598075308176,5.00959163936947,31.5846327269059));
#72227=CARTESIAN_POINT('Ctrl Pts',(5.99781986367865,5.16234564288104,31.5931520905564));
#72228=CARTESIAN_POINT('Ctrl Pts',(5.79500322495911,5.38631885309384,31.6057333777597));
#72229=CARTESIAN_POINT('Ctrl Pts',(5.72450579927918,5.46118371065252,31.6099555797658));
#72230=CARTESIAN_POINT('Ctrl Pts',(5.63968493583025,5.5478116297034,31.6148635568323));
#72231=CARTESIAN_POINT('Ctrl Pts',(5.62675667922351,5.56092342445259,31.6156070418903));
#72232=CARTESIAN_POINT('Ctrl Pts',(5.60685884741494,5.58096330679199,31.6167443639161));
#72233=CARTESIAN_POINT('Ctrl Pts',(5.59992198550004,5.58792370418223,31.6171395713646));
#72234=CARTESIAN_POINT('Ctrl Pts',(5.58779458074353,5.60004699264239,31.6178282526309));
#72235=CARTESIAN_POINT('Ctrl Pts',(5.58260981364795,5.60521563058168,31.6181219691736));
#72236=CARTESIAN_POINT('Ctrl Pts',(5.57092425387647,5.61683254136234,31.6187823579931));
#72237=CARTESIAN_POINT('Ctrl Pts',(5.5644194210303,5.6232767447185,31.6191488587621));
#72238=CARTESIAN_POINT('Ctrl Pts',(5.54697296076758,5.64050067753201,31.6201288864096));
#72239=CARTESIAN_POINT('Ctrl Pts',(5.53601107903679,5.65125988225382,31.6207415521513));
#72240=CARTESIAN_POINT('Ctrl Pts',(5.48847565737654,5.69764537363359,31.6233850214464));
#72241=CARTESIAN_POINT('Ctrl Pts',(5.45158867668825,5.73294940352518,31.6254023953576));
#72242=CARTESIAN_POINT('Ctrl Pts',(4.78542844629761,6.35827860027531,31.6612439170891));
#72243=CARTESIAN_POINT('Ctrl Pts',(4.06423647782678,6.84178294074071,31.6899550832066));
#72244=CARTESIAN_POINT('Ctrl Pts',(3.09555083545373,7.28300916836281,31.7271947743833));
#72245=CARTESIAN_POINT('Ctrl Pts',(2.90874531298586,7.35960957936124,31.7343587395591));
#72246=CARTESIAN_POINT('Ctrl Pts',(2.53903534427114,7.49493412840622,31.7488039591175));
#72247=CARTESIAN_POINT('Ctrl Pts',(2.35651177215115,7.5543094178956,31.7560637534897));
#72248=CARTESIAN_POINT('Ctrl Pts',(2.13810348886371,7.61667103095306,31.7650416944534));
#72249=CARTESIAN_POINT('Ctrl Pts',(2.10413647357246,7.62612442664081,31.7664451572457));
#72250=CARTESIAN_POINT('Ctrl Pts',(2.05926331342329,7.63829050592086,31.7683077613857));
#72251=CARTESIAN_POINT('Ctrl Pts',(2.04841263815998,7.64120755568485,31.768758808325));
#72252=CARTESIAN_POINT('Ctrl Pts',(2.0306462938027,7.64594322259052,31.7694983627328));
#72253=CARTESIAN_POINT('Ctrl Pts',(2.02373428693343,7.64777560268952,31.769786342373));
#72254=CARTESIAN_POINT('Ctrl Pts',(2.01037672776945,7.65129732865811,31.7703433494751));
#72255=CARTESIAN_POINT('Ctrl Pts',(2.00393150459491,7.65298790823911,31.7706123303634));
#72256=CARTESIAN_POINT('Ctrl Pts',(1.98910231173995,7.65685758212376,31.7712316895764));
#72257=CARTESIAN_POINT('Ctrl Pts',(1.98071689096315,7.65903105076917,31.7715822745833));
#72258=CARTESIAN_POINT('Ctrl Pts',(1.95832500515489,7.66479570843899,31.7725193808405));
#72259=CARTESIAN_POINT('Ctrl Pts',(1.94431226855425,7.66836226824856,31.7731067844201));
#72260=CARTESIAN_POINT('Ctrl Pts',(1.8471461879325,7.69280978946205,31.7771862787486));
#72261=CARTESIAN_POINT('Ctrl Pts',(1.76366943639669,7.71237583659046,31.7807232189715));
#72262=CARTESIAN_POINT('Ctrl Pts',(1.01545829949418,7.87496576646416,31.8126274012644));
#72263=CARTESIAN_POINT('Ctrl Pts',(0.33516685241311,7.93309448014955,31.8426732427994));
#72264=CARTESIAN_POINT('Ctrl Pts',(-0.891156915128255,7.87968897134275,
31.8946998603581));
#72265=CARTESIAN_POINT('Ctrl Pts',(-1.43418032141702,7.7991548035678,31.9171259763563));
#72266=CARTESIAN_POINT('Ctrl Pts',(-2.03869730178635,7.64418046461702,31.942440576106));
#72267=CARTESIAN_POINT('Ctrl Pts',(-2.11257467746494,7.6240940445047,31.9455381509962));
#72268=CARTESIAN_POINT('Ctrl Pts',(-2.21947736928432,7.59335524080166,31.9500260566281));
#72269=CARTESIAN_POINT('Ctrl Pts',(-2.25274225757413,7.58355298901857,31.9514233615065));
#72270=CARTESIAN_POINT('Ctrl Pts',(-2.31120932181367,7.56590570184017,31.9538807624126));
#72271=CARTESIAN_POINT('Ctrl Pts',(-2.33643867256069,7.55815268121473,31.9549416494663));
#72272=CARTESIAN_POINT('Ctrl Pts',(-2.385640580848,7.54276295489301,31.9570115632458));
#72273=CARTESIAN_POINT('Ctrl Pts',(-2.40961644236547,7.53513786069259,31.9580206827517));
#72274=CARTESIAN_POINT('Ctrl Pts',(-2.47444476902372,7.5141793137717,31.9607505525043));
#72275=CARTESIAN_POINT('Ctrl Pts',(-2.51522570396413,7.50062713073175,31.9624692181688));
#72276=CARTESIAN_POINT('Ctrl Pts',(-2.67127926982586,7.44735210782456,31.9690519517231));
#72277=CARTESIAN_POINT('Ctrl Pts',(-2.7857390612271,7.40529842300519,31.9738926154428));
#72278=CARTESIAN_POINT('Ctrl Pts',(-2.91948193524314,7.35262009395263,31.9795703692867));
#72279=CARTESIAN_POINT('Ctrl Pts',(-2.93974868782772,7.34454046699756,31.9804313485876));
#72280=CARTESIAN_POINT('Ctrl Pts',(-3.25019002610646,7.21928781226467,31.9936295162194));
#72281=CARTESIAN_POINT('Ctrl Pts',(-3.53319775953302,7.08508082954811,32.0057828777964));
#72282=CARTESIAN_POINT('Ctrl Pts',(-4.11811764360785,6.76391806199331,32.0315991691729));
#72283=CARTESIAN_POINT('Ctrl Pts',(-4.4169069248435,6.57270157253297,32.0452182432583));
#72284=CARTESIAN_POINT('Ctrl Pts',(-4.75404129853829,6.32354502005252,32.0616923866786));
#72285=CARTESIAN_POINT('Ctrl Pts',(-4.80574097283294,6.28434434700464,32.0642520867674));
#72286=CARTESIAN_POINT('Ctrl Pts',(-4.89204668846952,6.21721617027423,32.0685880094399));
#72287=CARTESIAN_POINT('Ctrl Pts',(-4.92691021719911,6.18962465542846,32.0703572048615));
#72288=CARTESIAN_POINT('Ctrl Pts',(-4.98696103557478,6.1412707099657,32.0734375063217));
#72289=CARTESIAN_POINT('Ctrl Pts',(-5.0122559267398,6.1206434961833,32.0747453141198));
#72290=CARTESIAN_POINT('Ctrl Pts',(-5.04882466951977,6.09044408380105,32.0766517651363));
#72291=CARTESIAN_POINT('Ctrl Pts',(-5.0602005705987,6.08099579548292,32.0772470665321));
#72292=CARTESIAN_POINT('Ctrl Pts',(-5.08007291976968,6.06439638022556,32.0782909941949));
#72293=CARTESIAN_POINT('Ctrl Pts',(-5.08858093800096,6.05725914611251,32.0787392281378));
#72294=CARTESIAN_POINT('Ctrl Pts',(-5.1050404257405,6.043392405207,32.0796089239101));
#72295=CARTESIAN_POINT('Ctrl Pts',(-5.11299368937797,6.0366650597293,32.0800303222729));
#72296=CARTESIAN_POINT('Ctrl Pts',(-5.13195044569499,6.0205659642021,32.0810375442143));
#72297=CARTESIAN_POINT('Ctrl Pts',(-5.14294153451239,6.01117977421789,32.0816238048612));
#72298=CARTESIAN_POINT('Ctrl Pts',(-5.18571486044419,5.97444894677131,32.0839143156753));
#72299=CARTESIAN_POINT('Ctrl Pts',(-5.21730497889847,5.94688216961574,32.0856253221289));
#72300=CARTESIAN_POINT('Ctrl Pts',(-5.5613355735828,5.64181637249005,32.1044639872128));
#72301=CARTESIAN_POINT('Ctrl Pts',(-5.85153305396377,5.34023373139806,32.1221893502809));
#72302=CARTESIAN_POINT('Ctrl Pts',(-6.40005430444207,4.67151645782309,32.1586285919391));
#72303=CARTESIAN_POINT('Ctrl Pts',(-6.65376687824803,4.30246170590275,32.177247847855));
#72304=CARTESIAN_POINT('Ctrl Pts',(-6.90005081578642,3.86985701182146,32.1974475367171));
#72305=CARTESIAN_POINT('Ctrl Pts',(-6.92472489354689,3.8255299958124,32.1995001637835));
#72306=CARTESIAN_POINT('Ctrl Pts',(-6.96161043211629,3.75773875726609,32.2026140904936));
#72307=CARTESIAN_POINT('Ctrl Pts',(-6.97413332039988,3.73444571688238,32.2036795503167));
#72308=CARTESIAN_POINT('Ctrl Pts',(-6.99570902834766,3.69382705265076,32.2055298663076));
#72309=CARTESIAN_POINT('Ctrl Pts',(-7.00481485312628,3.67652988295461,32.2063154152573));
#72310=CARTESIAN_POINT('Ctrl Pts',(-7.02369699876184,3.6403370834715,32.2079541854236));
#72311=CARTESIAN_POINT('Ctrl Pts',(-7.03346139822558,3.62143540253318,32.2088072465828));
#72312=CARTESIAN_POINT('Ctrl Pts',(-7.06031016518923,3.56894403113251,32.2111686843905));
#72313=CARTESIAN_POINT('Ctrl Pts',(-7.07723098431855,3.53527123974191,32.2126749659109));
#72314=CARTESIAN_POINT('Ctrl Pts',(-7.14568308991905,3.39658894112014,32.2188447821186));
#72315=CARTESIAN_POINT('Ctrl Pts',(-7.19512327348996,3.29056299154068,32.2234823651031));
#72316=CARTESIAN_POINT('Ctrl Pts',(-7.52041560277533,2.55054540145986,32.255380138994));
#72317=CARTESIAN_POINT('Ctrl Pts',(-7.71448142923748,1.88382536400206,32.2819063898042));
#72318=CARTESIAN_POINT('Ctrl Pts',(-7.88052359178331,0.802212600736091,
32.322963547461));
#72319=CARTESIAN_POINT('Ctrl Pts',(-7.91114475720133,0.39996457160148,32.3378710197299));
#72320=CARTESIAN_POINT('Ctrl Pts',(-7.91092746979535,-0.202542422171511,
32.3608634280321));
#72321=CARTESIAN_POINT('Ctrl Pts',(-7.90329461465925,-0.402151086599798,
32.3685972740227));
#72322=CARTESIAN_POINT('Ctrl Pts',(-7.88648412906036,-0.622697182523359,
32.3774230150704));
#72323=CARTESIAN_POINT('Ctrl Pts',(-7.88476183717319,-0.644138541417185,
32.3782840166816));
#72324=CARTESIAN_POINT('Ctrl Pts',(-7.88213466579698,-0.675254409781156,
32.3795380883945));
#72325=CARTESIAN_POINT('Ctrl Pts',(-7.88129936918853,-0.684934785212657,
32.379928883228));
#72326=CARTESIAN_POINT('Ctrl Pts',(-7.87979613395171,-0.701989108547733,
32.3806185279854));
#72327=CARTESIAN_POINT('Ctrl Pts',(-7.87913567232502,-0.70936371336394,
32.3809171271696));
#72328=CARTESIAN_POINT('Ctrl Pts',(-7.87775101888295,-0.724583993489366,
32.3815342078939));
#72329=CARTESIAN_POINT('Ctrl Pts',(-7.87702545738826,-0.732429533999852,
32.3818527358431));
#72330=CARTESIAN_POINT('Ctrl Pts',(-7.87514245282453,-0.752464125736244,
32.3826672946928));
#72331=CARTESIAN_POINT('Ctrl Pts',(-7.87396843283787,-0.764651573912543,
32.3831639014454));
#72332=CARTESIAN_POINT('Ctrl Pts',(-7.86909484946609,-0.814042400135809,
32.3851810266616));
#72333=CARTESIAN_POINT('Ctrl Pts',(-7.86515990484144,-0.851221704328809,
32.3867099632953));
#72334=CARTESIAN_POINT('Ctrl Pts',(-7.802336490884,-1.40712939915158,32.4097435337132));
#72335=CARTESIAN_POINT('Ctrl Pts',(-7.69251757597306,-1.9186998064338,32.4335955396737));
#72336=CARTESIAN_POINT('Ctrl Pts',(-7.45709899350262,-2.65286046525554,
32.4689324038717));
#72337=CARTESIAN_POINT('Ctrl Pts',(-7.3698562800263,-2.88638487778127,32.4803459503612));
#72338=CARTESIAN_POINT('Ctrl Pts',(-7.09222532820695,-3.53440924607822,
32.5120992708572));
#72339=CARTESIAN_POINT('Ctrl Pts',(-6.87682040595874,-3.93714814281155,
32.5318794963912));
#72340=CARTESIAN_POINT('Ctrl Pts',(-6.61159463846393,-4.34414882566462,
32.5516287223159));
#72341=CARTESIAN_POINT('Ctrl Pts',(-6.59514990729964,-4.36907431937963,
32.5528374884528));
#72342=CARTESIAN_POINT('Ctrl Pts',(-6.5725359186241,-4.40293202355548,32.5544785183539));
#72343=CARTESIAN_POINT('Ctrl Pts',(-6.56648892917775,-4.41194537022426,
32.5549152932547));
#72344=CARTESIAN_POINT('Ctrl Pts',(-6.55618071892211,-4.42724214598884,
32.5556564104499));
#72345=CARTESIAN_POINT('Ctrl Pts',(-6.55192897587351,-4.43353192543998,
32.5559611038756));
#72346=CARTESIAN_POINT('Ctrl Pts',(-6.54369993036841,-4.44566780323547,
32.5565489193596));
#72347=CARTESIAN_POINT('Ctrl Pts',(-6.53972383237845,-4.45151470760091,
32.5568320858398));
#72348=CARTESIAN_POINT('Ctrl Pts',(-6.53028924513555,-4.46534847010777,
32.5575019759469));
#72349=CARTESIAN_POINT('Ctrl Pts',(-6.52482392854366,-4.47333067042677,
32.5578884441143));
#72350=CARTESIAN_POINT('Ctrl Pts',(-6.50872660006217,-4.49674886487872,
32.5590220840116));
#72351=CARTESIAN_POINT('Ctrl Pts',(-6.49805432296485,-4.51215717036431,
32.5597677451865));
#72352=CARTESIAN_POINT('Ctrl Pts',(-6.41731051402919,-4.62785199998683,
32.565365025458));
#72353=CARTESIAN_POINT('Ctrl Pts',(-6.34497418135968,-4.72654129832449,
32.5701301805974));
#72354=CARTESIAN_POINT('Ctrl Pts',(-6.09935222264076,-5.04583991640927,
32.5855435842295));
#72355=CARTESIAN_POINT('Ctrl Pts',(-5.91661894577559,-5.2589194258272,32.5958153598227));
#72356=CARTESIAN_POINT('Ctrl Pts',(-5.51204586957432,-5.68283211459569,
32.6166146085642));
#72357=CARTESIAN_POINT('Ctrl Pts',(-5.28852230219091,-5.89141492735127,
32.6270648963156));
#72358=CARTESIAN_POINT('Ctrl Pts',(-4.94467863795966,-6.17689868608441,
32.6422835533191));
#72359=CARTESIAN_POINT('Ctrl Pts',(-4.83346049647168,-6.26431030384937,
32.6470888467411));
#72360=CARTESIAN_POINT('Ctrl Pts',(-4.58378590122663,-6.44993180667817,
32.6577325583592));
#72361=CARTESIAN_POINT('Ctrl Pts',(-4.4443928367037,-6.54676131071564,32.6635826566439));
#72362=CARTESIAN_POINT('Ctrl Pts',(-4.15758219764344,-6.73261048534774,
32.6756289955966));
#72363=CARTESIAN_POINT('Ctrl Pts',(-4.01015760936008,-6.82144890002884,
32.6818259065695));
#72364=CARTESIAN_POINT('Ctrl Pts',(-3.84268395291629,-6.91506274367206,
32.6889897886896));
#72365=CARTESIAN_POINT('Ctrl Pts',(-3.82537197536631,-6.92465464495434,
32.6897317813967));
#72366=CARTESIAN_POINT('Ctrl Pts',(-3.69480966097545,-6.99635517220981,
32.6953398531934));
#72367=CARTESIAN_POINT('Ctrl Pts',(-3.58009453882149,-7.05574405244669,
32.7003358825635));
#72368=CARTESIAN_POINT('Ctrl Pts',(-3.45196991285036,-7.11814605464429,
32.7060420340481));
#72369=CARTESIAN_POINT('Ctrl Pts',(-3.43994251061171,-7.12396624459321,
32.7065788945651));
#72370=CARTESIAN_POINT('Ctrl Pts',(-3.42314300200417,-7.13204324534366,
32.7073305211416));
#72371=CARTESIAN_POINT('Ctrl Pts',(-3.41838323693154,-7.1343258203449,32.707543673969));
#72372=CARTESIAN_POINT('Ctrl Pts',(-3.41005336029733,-7.13831021474073,
32.7079170529731));
#72373=CARTESIAN_POINT('Ctrl Pts',(-3.40648424608221,-7.14001412624842,
32.708077147049));
#72374=CARTESIAN_POINT('Ctrl Pts',(-3.39899078941399,-7.14358463925437,
32.7084135065499));
#72375=CARTESIAN_POINT('Ctrl Pts',(-3.39506618512975,-7.14545068439722,
32.708589807174));
#72376=CARTESIAN_POINT('Ctrl Pts',(-3.38570383838536,-7.14989277709013,
32.7090107111318));
#72377=CARTESIAN_POINT('Ctrl Pts',(-3.38026469768572,-7.15246585300009,
32.7092555040833));
#72378=CARTESIAN_POINT('Ctrl Pts',(-3.36178210175921,-7.16118356061889,
32.7100882436872));
#72379=CARTESIAN_POINT('Ctrl Pts',(-3.34872504734232,-7.16729861492442,
32.7106780990421));
#72380=CARTESIAN_POINT('Ctrl Pts',(-3.04431071796018,-7.30885257951498,
32.7244656720448));
#72381=CARTESIAN_POINT('Ctrl Pts',(-2.74501220678494,-7.42644079699674,
32.7387657857388));
#72382=CARTESIAN_POINT('Ctrl Pts',(-1.85378484549011,-7.71533664684171,
32.7816133063665));
#72383=CARTESIAN_POINT('Ctrl Pts',(-1.24789317764472,-7.83618801848575,
32.8108759286724));
#72384=CARTESIAN_POINT('Ctrl Pts',(-0.494159383322317,-7.8967994722947,
32.844259128784));
#72385=CARTESIAN_POINT('Ctrl Pts',(-0.353924144084563,-7.90432639673571,
32.8503561218869));
#72386=CARTESIAN_POINT('Ctrl Pts',(-0.038728035658005,-7.91283823084119,
32.8637851127222));
#72387=CARTESIAN_POINT('Ctrl Pts',(0.136216875681287,-7.91176081747751,
32.871048403724));
#72388=CARTESIAN_POINT('Ctrl Pts',(0.33011189978663,-7.90413267275771,32.8788903677481));
#72389=CARTESIAN_POINT('Ctrl Pts',(0.349230106061316,-7.90331104760243,
32.8796613652996));
#72390=CARTESIAN_POINT('Ctrl Pts',(0.377810927396445,-7.90197884691433,
32.8808106689884));
#72391=CARTESIAN_POINT('Ctrl Pts',(0.387275838177037,-7.90152062706566,
32.881190734362));
#72392=CARTESIAN_POINT('Ctrl Pts',(0.4035690881239,-7.90070248434555,32.8818440651301));
#72393=CARTESIAN_POINT('Ctrl Pts',(0.410397815562013,-7.90035071299772,
32.8821176044655));
#72394=CARTESIAN_POINT('Ctrl Pts',(0.424483458704019,-7.8996068009482,32.8826812582192));
#72395=CARTESIAN_POINT('Ctrl Pts',(0.431740309144017,-7.89921351288598,
32.8829713337696));
#72396=CARTESIAN_POINT('Ctrl Pts',(0.448616688980382,-7.89827556482687,
32.8836451955218));
#72397=CARTESIAN_POINT('Ctrl Pts',(0.458235795639389,-7.89772332942059,
32.884028726405));
#72398=CARTESIAN_POINT('Ctrl Pts',(0.488820830509399,-7.89591136925101,
32.8852464569668));
#72399=CARTESIAN_POINT('Ctrl Pts',(0.509782846475794,-7.89458571517036,
32.8860784364723));
#72400=CARTESIAN_POINT('Ctrl Pts',(0.872144802056555,-7.87022039384877,
32.9004159330345));
#72401=CARTESIAN_POINT('Ctrl Pts',(1.21171525168398,-7.82513794470721,32.9131420424039));
#72402=CARTESIAN_POINT('Ctrl Pts',(2.06823688875544,-7.6543096548038,32.9442245502106));
#72403=CARTESIAN_POINT('Ctrl Pts',(2.57733356105756,-7.49822645377081,32.9616640397618));
#72404=CARTESIAN_POINT('Ctrl Pts',(3.27934925793857,-7.20297734330344,32.9877571751242));
#72405=CARTESIAN_POINT('Ctrl Pts',(3.4877355277662,-7.10441451813099,32.9958010248579));
#72406=CARTESIAN_POINT('Ctrl Pts',(3.73131165764893,-6.97590561727908,33.005894993658));
#72407=CARTESIAN_POINT('Ctrl Pts',(3.77093031525983,-6.9545690245547,33.0075594850674));
#72408=CARTESIAN_POINT('Ctrl Pts',(3.84041224238881,-6.91638130974689,33.0105225476616));
#72409=CARTESIAN_POINT('Ctrl Pts',(3.87035221868428,-6.8996717503794,33.0118138853848));
#72410=CARTESIAN_POINT('Ctrl Pts',(3.98758141852602,-6.83324277457977,33.0169312516423));
#72411=CARTESIAN_POINT('Ctrl Pts',(4.07402583230292,-6.78205900000284,33.0208388597984));
#72412=CARTESIAN_POINT('Ctrl Pts',(4.16956192988194,-6.72300640420817,33.0253365249781));
#72413=CARTESIAN_POINT('Ctrl Pts',(4.17964113122038,-6.71674488195535,33.0258132968662));
#72414=CARTESIAN_POINT('Ctrl Pts',(4.19420996980241,-6.70764876248092,33.0265057770203));
#72415=CARTESIAN_POINT('Ctrl Pts',(4.19871091421087,-6.70483227607867,33.026720176992));
#72416=CARTESIAN_POINT('Ctrl Pts',(4.20666146061695,-6.69984604024579,33.0270997178114));
#72417=CARTESIAN_POINT('Ctrl Pts',(4.21011219121537,-6.6976781756434,33.0272647210103));
#72418=CARTESIAN_POINT('Ctrl Pts',(4.21726489075554,-6.69317689820336,33.0276073051194));
#72419=CARTESIAN_POINT('Ctrl Pts',(4.22096660083447,-6.69084307871034,33.0277849153057));
#72420=CARTESIAN_POINT('Ctrl Pts',(4.23048157194049,-6.68483313011628,33.0282422527284));
#72421=CARTESIAN_POINT('Ctrl Pts',(4.23629196767401,-6.68115249579342,33.0285223019758));
#72422=CARTESIAN_POINT('Ctrl Pts',(4.2602835399118,-6.6659109931913,33.029681815876));
#72423=CARTESIAN_POINT('Ctrl Pts',(4.27842209132177,-6.6542835527151,33.0305659838422));
#72424=CARTESIAN_POINT('Ctrl Pts',(4.40093364158854,-6.57504141243854,33.0365876888371));
#72425=CARTESIAN_POINT('Ctrl Pts',(4.50374235145094,-6.50505097909369,33.0418867505677));
#72426=CARTESIAN_POINT('Ctrl Pts',(4.75278299010074,-6.32677421678128,33.0552499474867));
#72427=CARTESIAN_POINT('Ctrl Pts',(4.8970087338744,-6.21581185361765,33.0634538502892));
#72428=CARTESIAN_POINT('Ctrl Pts',(5.42327710420013,-5.78122740691778,33.0947884990583));
#72429=CARTESIAN_POINT('Ctrl Pts',(5.77815545307308,-5.42655225955305,33.1187426847549));
#72430=CARTESIAN_POINT('Ctrl Pts',(6.4252785009965,-4.64380472094178,33.165551983905));
#72431=CARTESIAN_POINT('Ctrl Pts',(6.71390762270889,-4.215768901284,33.1882220692318));
#72432=CARTESIAN_POINT('Ctrl Pts',(6.97483644424306,-3.73318888403737,33.2105520296715));
#72433=CARTESIAN_POINT('Ctrl Pts',(6.99057855220665,-3.7036271695444,33.2119083201034));
#72434=CARTESIAN_POINT('Ctrl Pts',(7.01186344541045,-3.66303757813,33.2137549386503));
#72435=CARTESIAN_POINT('Ctrl Pts',(7.01756873799708,-3.65209560187206,33.2142511973975));
#72436=CARTESIAN_POINT('Ctrl Pts',(7.02657639642081,-3.63472109338896,33.2150367592113));
#72437=CARTESIAN_POINT('Ctrl Pts',(7.0298955737428,-3.62829732851342,33.2153266732395));
#72438=CARTESIAN_POINT('Ctrl Pts',(7.03631109045922,-3.61583921636753,33.2158879093494));
#72439=CARTESIAN_POINT('Ctrl Pts',(7.03940848528146,-3.60980542107245,33.2161592695666));
#72440=CARTESIAN_POINT('Ctrl Pts',(7.04675940902331,-3.59544021448345,33.2168042277656));
#72441=CARTESIAN_POINT('Ctrl Pts',(7.05100593216663,-3.58710521868658,33.2171775721551));
#72442=CARTESIAN_POINT('Ctrl Pts',(7.06355475934116,-3.56236623321961,33.2182831119125));
#72443=CARTESIAN_POINT('Ctrl Pts',(7.07181470002205,-3.54594075984663,33.2190137801));
#72444=CARTESIAN_POINT('Ctrl Pts',(7.13769979304879,-3.41377774057424,33.2248662260409));
#72445=CARTESIAN_POINT('Ctrl Pts',(7.1925385244288,-3.29666927826247,33.2298876247549));
#72446=CARTESIAN_POINT('Ctrl Pts',(7.37148054601365,-2.88879191306712,33.2468635717766));
#72447=CARTESIAN_POINT('Ctrl Pts',(7.48101792558783,-2.59195562700374,33.2583240696627));
#72448=CARTESIAN_POINT('Ctrl Pts',(7.71345115790378,-1.82313281118756,33.2866493364581));
#72449=CARTESIAN_POINT('Ctrl Pts',(7.81103761279837,-1.34491930664794,33.3029901075963));
#72450=CARTESIAN_POINT('Ctrl Pts',(7.89740189708789,-0.555904175066547,
33.3312170301369));
#72451=CARTESIAN_POINT('Ctrl Pts',(7.91301602063158,-0.249342549770843,
33.3425395217143));
#72452=CARTESIAN_POINT('Ctrl Pts',(7.91061575368542,0.0816723465747907,
33.3557202794264));
#72453=CARTESIAN_POINT('Ctrl Pts',(7.91032743184258,0.105980554140972,33.3566929646156));
#72454=CARTESIAN_POINT('Ctrl Pts',(7.90978182354199,0.139105320911063,33.3580246285723));
#72455=CARTESIAN_POINT('Ctrl Pts',(7.90962182541215,0.1479235088808,33.3583797302412));
#72456=CARTESIAN_POINT('Ctrl Pts',(7.90932491281167,0.162906242805148,33.3589840719565));
#72457=CARTESIAN_POINT('Ctrl Pts',(7.90919553662948,0.169070942098553,33.3592330177593));
#72458=CARTESIAN_POINT('Ctrl Pts',(7.90893183622479,0.180972767746121,33.3597141909425));
#72459=CARTESIAN_POINT('Ctrl Pts',(7.90879847643914,0.186709912872769,33.3599463810995));
#72460=CARTESIAN_POINT('Ctrl Pts',(7.90846800053546,0.20029091218076,33.3604965984255));
#72461=CARTESIAN_POINT('Ctrl Pts',(7.90826545737063,0.208134620350179,33.3608148310837));
#72462=CARTESIAN_POINT('Ctrl Pts',(7.9076451260912,0.230848098739798,33.3617376519985));
#72463=CARTESIAN_POINT('Ctrl Pts',(7.90719706688842,0.245716964344987,33.3623433648009));
#72464=CARTESIAN_POINT('Ctrl Pts',(7.90365603834653,0.353159596492445,33.3667315418744));
#72465=CARTESIAN_POINT('Ctrl Pts',(7.89897943712547,0.44567200733777,33.3705704429663));
#72466=CARTESIAN_POINT('Ctrl Pts',(7.8785872811178,0.744789499577517,33.3831431884445));
#72467=CARTESIAN_POINT('Ctrl Pts',(7.85638002390072,0.950860974038948,33.3920517516341));
#72468=CARTESIAN_POINT('Ctrl Pts',(7.70495458107232,1.97617346788039,33.437082553918));
#72469=CARTESIAN_POINT('Ctrl Pts',(7.45553304126914,2.77252951500953,33.4736766693005));
#72470=CARTESIAN_POINT('Ctrl Pts',(7.05576612426643,3.57840826362952,33.5103731881086));
#72471=CARTESIAN_POINT('Ctrl Pts',(7.02375981884731,3.64082950274119,33.5132182490646));
#72472=CARTESIAN_POINT('Ctrl Pts',(6.97951017615574,3.72437292666064,33.5170316258426));
#72473=CARTESIAN_POINT('Ctrl Pts',(6.96799335069341,3.74587568777321,33.5180136157243));
#72474=CARTESIAN_POINT('Ctrl Pts',(6.94987979088404,3.77932243258408,33.5195418035732));
#72475=CARTESIAN_POINT('Ctrl Pts',(6.94335132264555,3.79130314916276,33.5200893535031));
#72476=CARTESIAN_POINT('Ctrl Pts',(6.93081893556965,3.81416101381399,33.521134299543));
#72477=CARTESIAN_POINT('Ctrl Pts',(6.92482032554711,3.82504102159432,33.5216318011316));
#72478=CARTESIAN_POINT('Ctrl Pts',(6.91090935455271,3.85013213435724,33.5227794052549));
#72479=CARTESIAN_POINT('Ctrl Pts',(6.90297873923738,3.86433307141723,33.5234291301266));
#72480=CARTESIAN_POINT('Ctrl Pts',(6.88044162310628,3.90439833744,33.5252628015691));
#72481=CARTESIAN_POINT('Ctrl Pts',(6.86573312908299,3.93020507367409,33.5264446038895));
#72482=CARTESIAN_POINT('Ctrl Pts',(6.83254580805027,3.98767889855076,33.5290781898424));
#72483=CARTESIAN_POINT('Ctrl Pts',(6.81399144879621,4.01930165332891,33.530528319358));
#72484=CARTESIAN_POINT('Ctrl Pts',(6.66453174568438,4.27002067971258,33.5420349097794));
#72485=CARTESIAN_POINT('Ctrl Pts',(6.52331018001215,4.48279967952675,33.5518495252379));
#72486=CARTESIAN_POINT('Ctrl Pts',(6.0969138581944,5.0623201048706,33.5789408476289));
#72487=CARTESIAN_POINT('Ctrl Pts',(5.78940794619793,5.41130319298667,33.5956393611481));
#72488=CARTESIAN_POINT('Ctrl Pts',(5.29002954128316,5.88643834552112,33.6208133917479));
#72489=CARTESIAN_POINT('Ctrl Pts',(5.12044501474955,6.03453444817852,33.6290957261962));
#72490=CARTESIAN_POINT('Ctrl Pts',(4.86088141644757,6.24237986006729,33.6417089373373));
#72491=CARTESIAN_POINT('Ctrl Pts',(4.7756202609987,6.30784625938431,33.6458432449112));
#72492=CARTESIAN_POINT('Ctrl Pts',(4.67281650537838,6.38350322025479,33.6508489310775));
#72493=CARTESIAN_POINT('Ctrl Pts',(4.65653341917434,6.39539083737836,33.6516423913928));
#72494=CARTESIAN_POINT('Ctrl Pts',(4.60893800954172,6.42986017087523,33.653963967118));
#72495=CARTESIAN_POINT('Ctrl Pts',(4.5775058843503,6.45227488571555,33.6555000176022));
#72496=CARTESIAN_POINT('Ctrl Pts',(4.53709129367659,6.4806511815563,33.6574803187621));
#72497=CARTESIAN_POINT('Ctrl Pts',(4.52825863548561,6.48682594746188,33.6579134366595));
#72498=CARTESIAN_POINT('Ctrl Pts',(4.51417522042669,6.49662864965488,33.6586045848618));
#72499=CARTESIAN_POINT('Ctrl Pts',(4.50893262291727,6.50026832783638,33.6588619889915));
#72500=CARTESIAN_POINT('Ctrl Pts',(4.49912731577516,6.50705810162583,33.6593436543037));
#72501=CARTESIAN_POINT('Ctrl Pts',(4.49456568504792,6.51020975422795,33.6595678311992));
#72502=CARTESIAN_POINT('Ctrl Pts',(4.48440398107736,6.51721475353447,33.6600674409286));
#72503=CARTESIAN_POINT('Ctrl Pts',(4.47880225136634,6.52106567992592,33.660343005504));
#72504=CARTESIAN_POINT('Ctrl Pts',(4.46249786542099,6.53224326155335,33.6611455205228));
#72505=CARTESIAN_POINT('Ctrl Pts',(4.45178218190412,6.539550797169,33.6616735269393));
#72506=CARTESIAN_POINT('Ctrl Pts',(4.42778463883018,6.55582954956543,33.6628573726563));
#72507=CARTESIAN_POINT('Ctrl Pts',(4.41449341682578,6.56478680213562,33.6635140001783));
#72508=CARTESIAN_POINT('Ctrl Pts',(4.37261852432178,6.59282255622585,33.6655860107285));
#72509=CARTESIAN_POINT('Ctrl Pts',(4.34393860727937,6.61175462886298,33.6670100884214));
#72510=CARTESIAN_POINT('Ctrl Pts',(4.22872894021534,6.68673321991033,33.6727486263584));
#72511=CARTESIAN_POINT('Ctrl Pts',(4.14123306790011,6.74127115710724,33.6771463052817));
#72512=CARTESIAN_POINT('Ctrl Pts',(3.93383020899701,6.86498787279223,33.6876214062948));
#72513=CARTESIAN_POINT('Ctrl Pts',(3.81312434203901,6.93275982156251,33.693756190696));
#72514=CARTESIAN_POINT('Ctrl Pts',(3.40508924640276,7.14797598555145,33.7144870309655));
#72515=CARTESIAN_POINT('Ctrl Pts',(3.11052127233813,7.28099188248554,33.7294311511076));
#72516=CARTESIAN_POINT('Ctrl Pts',(2.18396243818395,7.63287336895979,33.7750829708796));
#72517=CARTESIAN_POINT('Ctrl Pts',(1.53163360906138,7.79004538863906,33.8051315388421));
#72518=CARTESIAN_POINT('Ctrl Pts',(0.824430612135664,7.86804233170642,33.8342211784226));
#72519=CARTESIAN_POINT('Ctrl Pts',(0.781582599764353,7.87241415837215,33.8359715889673));
#72520=CARTESIAN_POINT('Ctrl Pts',(0.724410171690338,7.87777614022145,33.8382913512211));
#72521=CARTESIAN_POINT('Ctrl Pts',(0.710116086697029,7.87907749412359,33.8388700149798));
#72522=CARTESIAN_POINT('Ctrl Pts',(0.68781166301903,7.88104693079272,33.8397709196889));
#72523=CARTESIAN_POINT('Ctrl Pts',(0.679803746825926,7.88174171585242,33.8400939599521));
#72524=CARTESIAN_POINT('Ctrl Pts',(0.664507366012739,7.88304537932679,33.8407102381162));
#72525=CARTESIAN_POINT('Ctrl Pts',(0.657219091346626,7.8836563571945,33.841003538594));
#72526=CARTESIAN_POINT('Ctrl Pts',(0.640211983875246,7.88505831916638,33.8416871667047));
#72527=CARTESIAN_POINT('Ctrl Pts',(0.630492505690202,7.88584144413706,33.8420772586367));
#72528=CARTESIAN_POINT('Ctrl Pts',(0.602767593339027,7.88802373096866,33.8431883033816));
#72529=CARTESIAN_POINT('Ctrl Pts',(0.584758731872752,7.88937921402568,33.8439079480389));
#72530=CARTESIAN_POINT('Ctrl Pts',(0.471023307754614,7.89754822804403,33.8484401433245));
#72531=CARTESIAN_POINT('Ctrl Pts',(0.37518228839042,7.90268118992016,33.8522021853134));
#72532=CARTESIAN_POINT('Ctrl Pts',(0.0908909016374918,7.91272333794625,
33.8632051251299));
#72533=CARTESIAN_POINT('Ctrl Pts',(-0.0976708626531418,7.9126428708132,
33.8702983174578));
#72534=CARTESIAN_POINT('Ctrl Pts',(-0.422168451783075,7.90090155498634,
33.8822389789408));
#72535=CARTESIAN_POINT('Ctrl Pts',(-0.558132440884234,7.89246230388878,
33.8871618897826));
#72536=CARTESIAN_POINT('Ctrl Pts',(-0.971901495377524,7.85603340520139,
33.9019783943688));
#72537=CARTESIAN_POINT('Ctrl Pts',(-1.24850317948589,7.8168470856265,33.9116496690037));
#72538=CARTESIAN_POINT('Ctrl Pts',(-1.69135065204,7.72999844234706,33.9272355686748));
#72539=CARTESIAN_POINT('Ctrl Pts',(-1.85911683229895,7.69137353691499,33.9331662196671));
#72540=CARTESIAN_POINT('Ctrl Pts',(-2.44421628413267,7.53640237963433,33.9542424173627));
#72541=CARTESIAN_POINT('Ctrl Pts',(-2.8531273054934,7.39129329290249,33.9696933264443));
#72542=CARTESIAN_POINT('Ctrl Pts',(-3.27659728510231,7.20061165459805,33.9880813290809));
#72543=CARTESIAN_POINT('Ctrl Pts',(-3.30502116806719,7.18760968688966,33.9893265322627));
#72544=CARTESIAN_POINT('Ctrl Pts',(-3.3434544803934,7.16975291495953,33.9910244601922));
#72545=CARTESIAN_POINT('Ctrl Pts',(-3.35353205478074,7.16504483447363,33.9914710055822));
#72546=CARTESIAN_POINT('Ctrl Pts',(-3.36940245665855,7.15758962140184,33.9921763032658));
#72547=CARTESIAN_POINT('Ctrl Pts',(-3.37520195330211,7.15485666365741,33.9924344752722));
#72548=CARTESIAN_POINT('Ctrl Pts',(-3.38637632447907,7.14957423754186,33.992932749767));
#72549=CARTESIAN_POINT('Ctrl Pts',(-3.39175165927738,7.14702574996537,33.9931728126738));
#72550=CARTESIAN_POINT('Ctrl Pts',(-3.40444567435204,7.14098987364071,33.993740600473));
#72551=CARTESIAN_POINT('Ctrl Pts',(-3.41176187155182,7.13749729641193,33.9940685308334));
#72552=CARTESIAN_POINT('Ctrl Pts',(-3.43313804780068,7.12725244545341,33.9950286464845));
#72553=CARTESIAN_POINT('Ctrl Pts',(-3.44718340122695,7.1204698490191,33.9956620070491));
#72554=CARTESIAN_POINT('Ctrl Pts',(-3.5490867058006,7.07088787668999,34.0002750594893));
#72555=CARTESIAN_POINT('Ctrl Pts',(-3.63616321820791,7.02650610407864,34.0043132648407));
#72556=CARTESIAN_POINT('Ctrl Pts',(-3.92946913765471,6.87009950938167,34.0181989876576));
#72557=CARTESIAN_POINT('Ctrl Pts',(-4.13152446440245,6.75051814337375,34.0282458813579));
#72558=CARTESIAN_POINT('Ctrl Pts',(-4.54237363692547,6.48200380283279,34.0493914998326));
#72559=CARTESIAN_POINT('Ctrl Pts',(-4.74985718774298,6.33153927368154,34.0604884284565));
#72560=CARTESIAN_POINT('Ctrl Pts',(-5.2430600967325,5.93596555342014,34.0876701552954));
#72561=CARTESIAN_POINT('Ctrl Pts',(-5.51929944106448,5.68002803141701,34.1036017923442));
#72562=CARTESIAN_POINT('Ctrl Pts',(-5.830612021902,5.34735493135501,34.1225275990923));
#72563=CARTESIAN_POINT('Ctrl Pts',(-5.88405500723007,5.28849110266729,34.1258167620943));
#72564=CARTESIAN_POINT('Ctrl Pts',(-6.12448351607916,5.01551837361121,34.1408151998826));
#72565=CARTESIAN_POINT('Ctrl Pts',(-6.3007356924843,4.79222882067065,34.1524037587994));
#72566=CARTESIAN_POINT('Ctrl Pts',(-6.50234455584356,4.50640956742863,34.1665773693545));
#72567=CARTESIAN_POINT('Ctrl Pts',(-6.53943582214714,4.45241407624802,34.1692258945061));
#72568=CARTESIAN_POINT('Ctrl Pts',(-6.59423784021253,4.37047389157929,34.1732017612311));
#72569=CARTESIAN_POINT('Ctrl Pts',(-6.61245081372409,4.342868749517,34.1745339257333));
#72570=CARTESIAN_POINT('Ctrl Pts',(-6.64478173051477,4.29319033305393,34.1769183518695));
#72571=CARTESIAN_POINT('Ctrl Pts',(-6.65896411453266,4.27115960929814,34.177971250334));
#72572=CARTESIAN_POINT('Ctrl Pts',(-6.6861494671716,4.2284657169355,34.1800030343796));
#72573=CARTESIAN_POINT('Ctrl Pts',(-6.69916674489275,4.20781201394333,34.180982058088));
#72574=CARTESIAN_POINT('Ctrl Pts',(-6.72733808212606,4.16265221945933,34.1831143356069));
#72575=CARTESIAN_POINT('Ctrl Pts',(-6.74245429776418,4.13812291026708,34.1842671797409));
#72576=CARTESIAN_POINT('Ctrl Pts',(-6.80213400458153,4.04008457750123,34.1888538344518));
#72577=CARTESIAN_POINT('Ctrl Pts',(-6.84563229667065,3.96593356520003,34.1922760810727));
#72578=CARTESIAN_POINT('Ctrl Pts',(-7.0146035680123,3.66682453631923,34.20590217578));
#72579=CARTESIAN_POINT('Ctrl Pts',(-7.13026669950786,3.436504920471,34.2159925132599));
#72580=CARTESIAN_POINT('Ctrl Pts',(-7.32003420274299,3.00761012587288,34.2342321611224));
#72581=CARTESIAN_POINT('Ctrl Pts',(-7.39779439043106,2.81091768888644,34.2423991442973));
#72582=CARTESIAN_POINT('Ctrl Pts',(-7.58604461796744,2.27258461749701,34.2644442599387));
#72583=CARTESIAN_POINT('Ctrl Pts',(-7.68131474043748,1.92616303313631,34.2782982588775));
#72584=CARTESIAN_POINT('Ctrl Pts',(-7.76172219545577,1.53023789837007,34.2943869398474));
#72585=CARTESIAN_POINT('Ctrl Pts',(-7.77032902953044,1.48591594130574,34.2961917417176));
#72586=CARTESIAN_POINT('Ctrl Pts',(-7.78172185144996,1.42443950271301,34.2987020253555));
#72587=CARTESIAN_POINT('Ctrl Pts',(-7.78483147791202,1.40734563181627,34.2994007659));
#72588=CARTESIAN_POINT('Ctrl Pts',(-7.78972120681561,1.37995424720859,34.3005217401465));
#72589=CARTESIAN_POINT('Ctrl Pts',(-7.79153726661345,1.36966317995263,34.3009431900185));
#72590=CARTESIAN_POINT('Ctrl Pts',(-7.79512934678877,1.34906959151864,34.3017871805859));
#72591=CARTESIAN_POINT('Ctrl Pts',(-7.79690534630222,1.33876708801416,34.30220972082));
#72592=CARTESIAN_POINT('Ctrl Pts',(-7.80045395369489,1.31793517542846,34.3030647686239));
#72593=CARTESIAN_POINT('Ctrl Pts',(-7.80222567643297,1.30740563846673,34.3034972955494));
#72594=CARTESIAN_POINT('Ctrl Pts',(-7.80623665932681,1.28326940848313,34.3044895724062));
#72595=CARTESIAN_POINT('Ctrl Pts',(-7.80846166197171,1.26966043754333,34.3050496646688));
#72596=CARTESIAN_POINT('Ctrl Pts',(-7.81423166667276,1.23377998232336,34.3065279158373));
#72597=CARTESIAN_POINT('Ctrl Pts',(-7.81771702853883,1.21149908755133,34.3074474389253));
#72598=CARTESIAN_POINT('Ctrl Pts',(-7.82805901666214,1.14348231499749,34.310258854645));
#72599=CARTESIAN_POINT('Ctrl Pts',(-7.83460987114422,1.0977011798412,34.3121572264864));
#72600=CARTESIAN_POINT('Ctrl Pts',(-7.8873571986243,0.70451493309922,34.3285041600686));
#72601=CARTESIAN_POINT('Ctrl Pts',(-7.91082079892818,0.354462731269747,
34.3433274249038));
#72602=CARTESIAN_POINT('Ctrl Pts',(-7.91099897745234,0.00402228145511663,
34.3581038380725));
#72603=CARTESIAN_POINT('',(-7.90835677968835,8.74328140329327E-7,36.3575767704668));
#72604=CARTESIAN_POINT('Ctrl Pts',(-7.91024367631032,0.00400354093750647,
34.3576684917631));
#72605=CARTESIAN_POINT('Ctrl Pts',(-7.90782998290103,-0.879334447994197,
34.3932661792596));
#72606=CARTESIAN_POINT('Ctrl Pts',(-7.53464189968267,-3.08007093248513,
34.4817851337331));
#72607=CARTESIAN_POINT('Ctrl Pts',(-4.8119999607783,-7.26991696249447,34.6761466221616));
#72608=CARTESIAN_POINT('Ctrl Pts',(2.39745492945816,-9.04145408158046,34.940752957047));
#72609=CARTESIAN_POINT('Ctrl Pts',(8.91206867060443,-2.8636622032058,35.2582805589104));
#72610=CARTESIAN_POINT('Ctrl Pts',(7.50125790307925,4.4424751158228,35.522886893796));
#72611=CARTESIAN_POINT('Ctrl Pts',(3.10734150823604,7.61713964008732,35.7345719617049));
#72612=CARTESIAN_POINT('Ctrl Pts',(-2.28026636838621,8.42190983339057,35.9462570296132));
#72613=CARTESIAN_POINT('Ctrl Pts',(-7.03744966258467,5.09046671418386,36.1539252992009));
#72614=CARTESIAN_POINT('Ctrl Pts',(-7.91033516654623,1.2191874091852,36.308672301811));
#72615=CARTESIAN_POINT('Ctrl Pts',(-7.90835677968835,8.74328140328812E-7,
36.3575767704668));
#72616=CARTESIAN_POINT('',(-7.91892560419408,-0.000477670393038393,40.3576684917631));
#72617=CARTESIAN_POINT('Ctrl Pts',(-7.91099999974567,6.34350998739673E-5,
36.3591007772358));
#72618=CARTESIAN_POINT('Ctrl Pts',(-7.91100128680852,-0.160446349449327,
36.3656875025832));
#72619=CARTESIAN_POINT('Ctrl Pts',(-7.90611756750387,-0.320921897579779,
36.3722377272791));
#72620=CARTESIAN_POINT('Ctrl Pts',(-7.8904555431557,-0.577963795836673,
36.3827140688806));
#72621=CARTESIAN_POINT('Ctrl Pts',(-7.88277542261335,-0.674672258868436,
36.3866495373655));
#72622=CARTESIAN_POINT('Ctrl Pts',(-7.86990544413694,-0.806061535681041,
36.3919871907642));
#72623=CARTESIAN_POINT('Ctrl Pts',(-7.86626086167125,-0.840884632690744,
36.3934010063988));
#72624=CARTESIAN_POINT('Ctrl Pts',(-7.859478196455,-0.901783336511438,36.3958719992469));
#72625=CARTESIAN_POINT('Ctrl Pts',(-7.8564412223582,-0.927869619495753,
36.3969299829559));
#72626=CARTESIAN_POINT('Ctrl Pts',(-7.85025643312285,-0.978785641192203,
36.3989940772854));
#72627=CARTESIAN_POINT('Ctrl Pts',(-7.8471205724269,-1.00361652192462,36.4000002771073));
#72628=CARTESIAN_POINT('Ctrl Pts',(-7.84067389521036,-1.05278542288196,
36.4019918977854));
#72629=CARTESIAN_POINT('Ctrl Pts',(-7.83736746181006,-1.07712373949573,
36.4029773457103));
#72630=CARTESIAN_POINT('Ctrl Pts',(-7.82840941896887,-1.14083709459794,
36.4055560983881));
#72631=CARTESIAN_POINT('Ctrl Pts',(-7.82257407345061,-1.18018565910166,
36.4071477262376));
#72632=CARTESIAN_POINT('Ctrl Pts',(-7.80106401981511,-1.31805663613217,
36.4127215177653));
#72633=CARTESIAN_POINT('Ctrl Pts',(-7.78382266736936,-1.41632556054869,
36.4166887825074));
#72634=CARTESIAN_POINT('Ctrl Pts',(-7.73289634930477,-1.67746530858593,
36.427224340502));
#72635=CARTESIAN_POINT('Ctrl Pts',(-7.69592638373383,-1.83964508464265,
36.4337594446801));
#72636=CARTESIAN_POINT('Ctrl Pts',(-7.49705272225421,-2.60051619191154,
36.4644865102498));
#72637=CARTESIAN_POINT('Ctrl Pts',(-7.27023661998133,-3.17995251326264,
36.4879439620504));
#72638=CARTESIAN_POINT('Ctrl Pts',(-6.9479831059587,-3.78332395732732,36.5150820373445));
#72639=CARTESIAN_POINT('Ctrl Pts',(-6.91717783344546,-3.83935672767541,
36.517631449933));
#72640=CARTESIAN_POINT('Ctrl Pts',(-6.8786142825756,-3.90753035701743,36.520773659593));
#72641=CARTESIAN_POINT('Ctrl Pts',(-6.87149746033779,-3.92003196290222,
36.5213515560707));
#72642=CARTESIAN_POINT('Ctrl Pts',(-6.85891286492553,-3.9419988327894,36.5223700289469));
#72643=CARTESIAN_POINT('Ctrl Pts',(-6.85345949214589,-3.95147231737965,
36.5228102560313));
#72644=CARTESIAN_POINT('Ctrl Pts',(-6.84243450288904,-3.97053321794282,
36.5236980545097));
#72645=CARTESIAN_POINT('Ctrl Pts',(-6.83686232852009,-3.98012028223527,
36.5241456391603));
#72646=CARTESIAN_POINT('Ctrl Pts',(-6.82600117466787,-3.99871705816677,
36.5250159303589));
#72647=CARTESIAN_POINT('Ctrl Pts',(-6.82071446710367,-4.00772807277308,
36.5254385776426));
#72648=CARTESIAN_POINT('Ctrl Pts',(-6.80800891639722,-4.02928629732271,
36.5264520492108));
#72649=CARTESIAN_POINT('Ctrl Pts',(-6.80057325177522,-4.04182346443603,
36.5270433239849));
#72650=CARTESIAN_POINT('Ctrl Pts',(-6.77097861931579,-4.09140968127563,
36.5293894988432));
#72651=CARTESIAN_POINT('Ctrl Pts',(-6.74855138255254,-4.12829732779608,
36.5311515938725));
#72652=CARTESIAN_POINT('Ctrl Pts',(-6.5425058423051,-4.4610287029693,36.5471907051692));
#72653=CARTESIAN_POINT('Ctrl Pts',(-6.33984747248848,-4.74462691636221,
36.5618887958264));
#72654=CARTESIAN_POINT('Ctrl Pts',(-5.94180798011561,-5.23040656238268,
36.5883789342644));
#72655=CARTESIAN_POINT('Ctrl Pts',(-5.75307970086982,-5.43730754710313,
36.6001599706305));
#72656=CARTESIAN_POINT('Ctrl Pts',(-5.4397540626069,-5.74618441616636,36.6184551663497));
#72657=CARTESIAN_POINT('Ctrl Pts',(-5.32233713101884,-5.85510789717026,
36.6250638843976));
#72658=CARTESIAN_POINT('Ctrl Pts',(-5.14962157520898,-6.00583843649464,
36.6344438203726));
#72659=CARTESIAN_POINT('Ctrl Pts',(-5.09695560693799,-6.05059842956173,
36.6372609594777));
#72660=CARTESIAN_POINT('Ctrl Pts',(-5.00221372162009,-6.12900318537022,
36.6422543882455));
#72661=CARTESIAN_POINT('Ctrl Pts',(-4.96036807312028,-6.16291901613924,
36.6444347844668));
#72662=CARTESIAN_POINT('Ctrl Pts',(-4.89706276917497,-6.21316538043723,
36.6476967960334));
#72663=CARTESIAN_POINT('Ctrl Pts',(-4.87586083302529,-6.22981773039324,
36.6487832435795));
#72664=CARTESIAN_POINT('Ctrl Pts',(-4.83795351385324,-6.25927870439202,
36.65071513245));
#72665=CARTESIAN_POINT('Ctrl Pts',(-4.82128136953312,-6.27212962721198,
36.6515611920964));
#72666=CARTESIAN_POINT('Ctrl Pts',(-4.78778191385402,-6.29773858292842,
36.6532540584411));
#72667=CARTESIAN_POINT('Ctrl Pts',(-4.77095441421748,-6.31049608939397,
36.6541008521693));
#72668=CARTESIAN_POINT('Ctrl Pts',(-4.72459897977821,-6.34534833879061,
36.6564239019418));
#72669=CARTESIAN_POINT('Ctrl Pts',(-4.69496725366666,-6.36730426194092,
36.6578981769453));
#72670=CARTESIAN_POINT('Ctrl Pts',(-4.57583330360917,-6.45429395243304,
36.663784022659));
#72671=CARTESIAN_POINT('Ctrl Pts',(-4.4851241895155,-6.51765465868862,36.6681725628441));
#72672=CARTESIAN_POINT('Ctrl Pts',(-3.74574367023264,-7.01136771515209,
36.7032782935725));
#72673=CARTESIAN_POINT('Ctrl Pts',(-3.03806676371634,-7.34575600187266,
36.732945549065));
#72674=CARTESIAN_POINT('Ctrl Pts',(-1.90166291890524,-7.68991409795436,
36.777376187884));
#72675=CARTESIAN_POINT('Ctrl Pts',(-1.50175405456209,-7.77790532378213,
36.7925499150258));
#72676=CARTESIAN_POINT('Ctrl Pts',(-0.977021751312561,-7.85136875372685,
36.8130868687108));
#72677=CARTESIAN_POINT('Ctrl Pts',(-0.856820687275151,-7.86539380505291,
36.8178363282465));
#72678=CARTESIAN_POINT('Ctrl Pts',(-0.7187680762016,-7.87829964037159,36.8233787458573));
#72679=CARTESIAN_POINT('Ctrl Pts',(-0.701182318152164,-7.8798842708637,
36.8240863926316));
#72680=CARTESIAN_POINT('Ctrl Pts',(-0.674563346213154,-7.88219305855269,
36.8251601533033));
#72681=CARTESIAN_POINT('Ctrl Pts',(-0.665533894843102,-7.88296059576792,
36.8255248407219));
#72682=CARTESIAN_POINT('Ctrl Pts',(-0.649923053382483,-7.88426056284363,
36.8261561537298));
#72683=CARTESIAN_POINT('Ctrl Pts',(-0.643342268852679,-7.8848002715951,
36.8264225344935));
#72684=CARTESIAN_POINT('Ctrl Pts',(-0.629711658359943,-7.88590097846509,
36.8269748098343));
#72685=CARTESIAN_POINT('Ctrl Pts',(-0.622661742816073,-7.88646076313511,
36.827260745538));
#72686=CARTESIAN_POINT('Ctrl Pts',(-0.603487885387555,-7.8879573553563,
36.8280392260134));
#72687=CARTESIAN_POINT('Ctrl Pts',(-0.591362545437713,-7.88887566169215,
36.8285324123451));
#72688=CARTESIAN_POINT('Ctrl Pts',(-0.545793449416968,-7.89222116311333,
36.8303893394664));
#72689=CARTESIAN_POINT('Ctrl Pts',(-0.51233676863031,-7.89446365303272,
36.8317596663563));
#72690=CARTESIAN_POINT('Ctrl Pts',(0.0139043092441738,-7.92637649912327,
36.8534346627102));
#72691=CARTESIAN_POINT('Ctrl Pts',(0.508282527678121,-7.91006149081741,
36.8758468277803));
#72692=CARTESIAN_POINT('Ctrl Pts',(1.33548105221676,-7.80488833396626,36.9140470880228));
#72693=CARTESIAN_POINT('Ctrl Pts',(1.67004954912004,-7.74020295352098,36.9296744609613));
#72694=CARTESIAN_POINT('Ctrl Pts',(2.38254560718237,-7.55408498922569,36.9625481662131));
#72695=CARTESIAN_POINT('Ctrl Pts',(2.75764563159093,-7.42537343382496,36.9795830537459));
#72696=CARTESIAN_POINT('Ctrl Pts',(3.15019087989054,-7.25680294962654,36.9969552640543));
#72697=CARTESIAN_POINT('Ctrl Pts',(3.1787452105361,-7.24434058727828,36.9982165067383));
#72698=CARTESIAN_POINT('Ctrl Pts',(3.21810086301006,-7.22688656163997,36.9999515476662));
#72699=CARTESIAN_POINT('Ctrl Pts',(3.22896547211706,-7.22203880637441,37.0004301784889));
#72700=CARTESIAN_POINT('Ctrl Pts',(3.24727994271609,-7.21381735659886,37.0012364247012));
#72701=CARTESIAN_POINT('Ctrl Pts',(3.2547355669171,-7.21045659238659,37.0015644758173));
#72702=CARTESIAN_POINT('Ctrl Pts',(3.26947169811863,-7.20378648852256,37.0022125528971));
#72703=CARTESIAN_POINT('Ctrl Pts',(3.2767524233374,-7.20047765871258,37.0025325955344));
#72704=CARTESIAN_POINT('Ctrl Pts',(3.2927793837052,-7.19316463456151,37.0032367629342));
#72705=CARTESIAN_POINT('Ctrl Pts',(3.30152336496803,-7.1891555137647,37.0036207200573));
#72706=CARTESIAN_POINT('Ctrl Pts',(3.33198780519098,-7.17512024751193,37.0049576784032));
#72707=CARTESIAN_POINT('Ctrl Pts',(3.35367017867262,-7.16501148956461,37.005907867409));
#72708=CARTESIAN_POINT('Ctrl Pts',(3.57019680227172,-7.06286422342636,37.0153835412734));
#72709=CARTESIAN_POINT('Ctrl Pts',(3.76125634517662,-6.96299615427769,37.0236339609932));
#72710=CARTESIAN_POINT('Ctrl Pts',(4.26268021305892,-6.67422921724155,37.0451360617842));
#72711=CARTESIAN_POINT('Ctrl Pts',(4.56451194854539,-6.47155557089894,37.0578994980821));
#72712=CARTESIAN_POINT('Ctrl Pts',(5.17079297006981,-6.00086292009092,37.0842777138259));
#72713=CARTESIAN_POINT('Ctrl Pts',(5.47072712262579,-5.72875079511461,37.097785527289));
#72714=CARTESIAN_POINT('Ctrl Pts',(5.9356987084977,-5.23694767772726,37.1214768117619));
#72715=CARTESIAN_POINT('Ctrl Pts',(6.11249873253866,-5.02946118450261,37.1313008642115));
#72716=CARTESIAN_POINT('Ctrl Pts',(6.327701727509,-4.74876011100447,37.1449308537782));
#72717=CARTESIAN_POINT('Ctrl Pts',(6.37617175245921,-4.68347784265528,37.1481233235664));
#72718=CARTESIAN_POINT('Ctrl Pts',(6.42986051378105,-4.60878822328366,37.1518142236186));
#72719=CARTESIAN_POINT('Ctrl Pts',(6.43607797466473,-4.60010167449692,37.1522440617405));
#72720=CARTESIAN_POINT('Ctrl Pts',(6.44538314027623,-4.58704543285931,37.1528910338218));
#72721=CARTESIAN_POINT('Ctrl Pts',(6.44848405801431,-4.58268512788451,37.1531072502198));
#72722=CARTESIAN_POINT('Ctrl Pts',(6.45380562261194,-4.57518620034406,37.153479368757));
#72723=CARTESIAN_POINT('Ctrl Pts',(6.45602841310377,-4.57204909328216,37.1536351209302));
#72724=CARTESIAN_POINT('Ctrl Pts',(6.46059745470107,-4.565590658881,37.1539559381918));
#72725=CARTESIAN_POINT('Ctrl Pts',(6.46294343310752,-4.56226914117113,37.1541210223437));
#72726=CARTESIAN_POINT('Ctrl Pts',(6.46924034916175,-4.55333914504494,37.1545651029844));
#72727=CARTESIAN_POINT('Ctrl Pts',(6.47318654608231,-4.54772734495588,37.1548444343671));
#72728=CARTESIAN_POINT('Ctrl Pts',(6.48784316130739,-4.52682676658602,37.1558857742386));
#72729=CARTESIAN_POINT('Ctrl Pts',(6.49850656925911,-4.51150549233775,37.1566511454344));
#72730=CARTESIAN_POINT('Ctrl Pts',(6.67752892654667,-4.25233308400209,37.1696298435719));
#72731=CARTESIAN_POINT('Ctrl Pts',(6.83209651678353,-3.99926930485025,37.1827682456569));
#72732=CARTESIAN_POINT('Ctrl Pts',(6.97219703407295,-3.73796596650605,37.1962838440715));
#72733=CARTESIAN_POINT('Ctrl Pts',(6.97230129610631,-3.73777148646186,37.1962939032933));
#72734=CARTESIAN_POINT('Ctrl Pts',(6.97262284963992,-3.73717163216025,37.196324929889));
#72735=CARTESIAN_POINT('Ctrl Pts',(6.97284011393855,-3.73676624329022,37.1963458979422));
#72736=CARTESIAN_POINT('Ctrl Pts',(6.97349023387072,-3.7355529441025,37.1964086534861));
#72737=CARTESIAN_POINT('Ctrl Pts',(6.97392298441589,-3.73474497757456,37.1964504435833));
#72738=CARTESIAN_POINT('Ctrl Pts',(6.97515070243164,-3.73245181029339,37.1965690508874));
#72739=CARTESIAN_POINT('Ctrl Pts',(6.975945335761,-3.73096643113628,37.1966458763341));
#72740=CARTESIAN_POINT('Ctrl Pts',(6.97803306342754,-3.72706091912252,37.1968478698159));
#72741=CARTESIAN_POINT('Ctrl Pts',(6.97932537277535,-3.72464036788215,37.1969730570357));
#72742=CARTESIAN_POINT('Ctrl Pts',(6.98244828661375,-3.71878368326225,37.197275945453));
#72743=CARTESIAN_POINT('Ctrl Pts',(6.98427761372055,-3.71534687109722,37.1974536774068));
#72744=CARTESIAN_POINT('Ctrl Pts',(6.98840760384156,-3.70757390457266,37.1978556282583));
#72745=CARTESIAN_POINT('Ctrl Pts',(6.99070676893085,-3.70323695785707,37.1980798824442));
#72746=CARTESIAN_POINT('Ctrl Pts',(6.9956737490153,-3.69384656583093,37.1985654018961));
#72747=CARTESIAN_POINT('Ctrl Pts',(6.99834012750028,-3.68879236529416,37.1988267000539));
#72748=CARTESIAN_POINT('Ctrl Pts',(7.09853760436693,-3.4983653709777,37.2086706214829));
#72749=CARTESIAN_POINT('Ctrl Pts',(7.18867207167391,-3.30919744495289,37.2184108638924));
#72750=CARTESIAN_POINT('Ctrl Pts',(7.42387594751548,-2.76046832297191,37.2461611695393));
#72751=CARTESIAN_POINT('Ctrl Pts',(7.5501873876328,-2.39349687376259,37.2640956791124));
#72752=CARTESIAN_POINT('Ctrl Pts',(7.72519746143205,-1.73037139967677,37.2944864047326));
#72753=CARTESIAN_POINT('Ctrl Pts',(7.78493765322533,-1.43792689906373,37.3072370785531));
#72754=CARTESIAN_POINT('Ctrl Pts',(7.83472255011574,-1.09690173597895,37.3213121931983));
#72755=CARTESIAN_POINT('Ctrl Pts',(7.84101700906523,-1.05096299749347,37.3231921233004));
#72756=CARTESIAN_POINT('Ctrl Pts',(7.84862397292639,-0.991567114696946,
37.325602277619));
#72757=CARTESIAN_POINT('Ctrl Pts',(7.85030629853086,-0.97815879749513,37.3261450131621));
#72758=CARTESIAN_POINT('Ctrl Pts',(7.85293935211318,-0.956728688156941,
37.3270103149777));
#72759=CARTESIAN_POINT('Ctrl Pts',(7.85391216011091,-0.948709667132181,
37.3273336283052));
#72760=CARTESIAN_POINT('Ctrl Pts',(7.85572758983231,-0.933550600741194,
37.3279439169007));
#72761=CARTESIAN_POINT('Ctrl Pts',(7.85657276328813,-0.926410872849657,
37.3282309782548));
#72762=CARTESIAN_POINT('Ctrl Pts',(7.85845877543905,-0.910290290740692,
37.3288782778832));
#72763=CARTESIAN_POINT('Ctrl Pts',(7.85949395493788,-0.90130877713249,37.3292383243573));
#72764=CARTESIAN_POINT('Ctrl Pts',(7.86210176090017,-0.878336560303134,
37.3301577117613));
#72765=CARTESIAN_POINT('Ctrl Pts',(7.86365244365131,-0.864343369377637,
37.3307163101667));
#72766=CARTESIAN_POINT('Ctrl Pts',(7.87224717002346,-0.784847561057308,
37.333881650503));
#72767=CARTESIAN_POINT('Ctrl Pts',(7.87851022866422,-0.719262162811634,
37.3364619464332));
#72768=CARTESIAN_POINT('Ctrl Pts',(7.90622274111874,-0.384986669870525,
37.3494614982831));
#72769=CARTESIAN_POINT('Ctrl Pts',(7.91475029820828,-0.115395698033488,
37.3594383910394));
#72770=CARTESIAN_POINT('Ctrl Pts',(7.90730889460935,0.266494716771104,37.3730861339757));
#72771=CARTESIAN_POINT('Ctrl Pts',(7.902724692449,0.378809513161197,37.3770418158233));
#72772=CARTESIAN_POINT('Ctrl Pts',(7.86503777196913,0.984863040936311,37.3981674873349));
#72773=CARTESIAN_POINT('Ctrl Pts',(7.78806062932387,1.47474085886958,37.4143735496396));
#72774=CARTESIAN_POINT('Ctrl Pts',(7.61829376074975,2.14069080753604,37.4382137105358));
#72775=CARTESIAN_POINT('Ctrl Pts',(7.56396759940108,2.3253698243664,37.4450375592331));
#72776=CARTESIAN_POINT('Ctrl Pts',(7.46876937846004,2.61018017457105,37.4561509423528));
#72777=CARTESIAN_POINT('Ctrl Pts',(7.43248632296349,2.71177098691488,37.4602354730277));
#72778=CARTESIAN_POINT('Ctrl Pts',(7.3751840495486,2.86241571094123,37.466518585957));
#72779=CARTESIAN_POINT('Ctrl Pts',(7.35572630425045,2.91205318346399,37.4686261773634));
#72780=CARTESIAN_POINT('Ctrl Pts',(7.33235245901648,2.9699514643652,37.4711327028303));
#72781=CARTESIAN_POINT('Ctrl Pts',(7.32892150652308,2.97840793608622,37.471500009864));
#72782=CARTESIAN_POINT('Ctrl Pts',(7.32365096332777,2.99133430620729,37.4720633483097));
#72783=CARTESIAN_POINT('Ctrl Pts',(7.32182189549999,2.99580848759161,37.4722586816354));
#72784=CARTESIAN_POINT('Ctrl Pts',(7.31847889903726,3.00396462247884,37.4726153907883));
#72785=CARTESIAN_POINT('Ctrl Pts',(7.31696629110291,3.0076471108665,37.4727766786994));
#72786=CARTESIAN_POINT('Ctrl Pts',(7.31366084912057,3.0156770547789,37.4731288871527));
#72787=CARTESIAN_POINT('Ctrl Pts',(7.31186691807611,3.02002405401504,37.4733198797862));
#72788=CARTESIAN_POINT('Ctrl Pts',(7.30696380538713,3.03187515003108,37.4738414588666));
#72789=CARTESIAN_POINT('Ctrl Pts',(7.3038469483573,3.03937604330163,37.4741725456504));
#72790=CARTESIAN_POINT('Ctrl Pts',(7.28883813553353,3.07533919333979,37.4757645286633));
#72791=CARTESIAN_POINT('Ctrl Pts',(7.27679148092318,3.10373616961389,37.4770353625158));
#72792=CARTESIAN_POINT('Ctrl Pts',(7.07535160434235,3.57096068311142,37.4981635576092));
#72793=CARTESIAN_POINT('Ctrl Pts',(6.84675556793272,3.99176758181895,37.5203402564296));
#72794=CARTESIAN_POINT('Ctrl Pts',(6.3350477932549,4.75905313849894,37.5636009822948));
#72795=CARTESIAN_POINT('Ctrl Pts',(6.05774103805619,5.1073709989602,37.5845651512568));
#72796=CARTESIAN_POINT('Ctrl Pts',(5.62558359873539,5.56515836500273,37.6129417402302));
#72797=CARTESIAN_POINT('Ctrl Pts',(5.49383972766374,5.69525323599682,37.6211234290596));
#72798=CARTESIAN_POINT('Ctrl Pts',(5.21152947102894,5.95510883183441,37.6376769920443));
#72799=CARTESIAN_POINT('Ctrl Pts',(5.06039269599592,6.08406067721272,37.6460129329371));
#72800=CARTESIAN_POINT('Ctrl Pts',(4.87539563984146,6.23023429828023,37.655620932466));
#72801=CARTESIAN_POINT('Ctrl Pts',(4.8460745922381,6.25306829916386,37.6571268088175));
#72802=CARTESIAN_POINT('Ctrl Pts',(4.80674229040214,6.28325582515507,37.6591246006389));
#72803=CARTESIAN_POINT('Ctrl Pts',(4.79687330466832,6.29079340874685,37.6596240213283));
#72804=CARTESIAN_POINT('Ctrl Pts',(4.78057658281538,6.30317962294404,37.660445684369));
#72805=CARTESIAN_POINT('Ctrl Pts',(4.77415913811843,6.30804172050976,37.6607684727417));
#72806=CARTESIAN_POINT('Ctrl Pts',(4.76166388616725,6.31747860329622,37.6613954702727));
#72807=CARTESIAN_POINT('Ctrl Pts',(4.75558688224872,6.32205443457652,37.6616997215624));
#72808=CARTESIAN_POINT('Ctrl Pts',(4.741475206544,6.33264831157299,37.6624046519201));
#72809=CARTESIAN_POINT('Ctrl Pts',(4.73343565318888,6.33865984971924,37.6628050688354));
#72810=CARTESIAN_POINT('Ctrl Pts',(4.70738845261501,6.35805933180136,37.6640985472136));
#72811=CARTESIAN_POINT('Ctrl Pts',(4.68933520595172,6.37138602249232,37.6649891545291));
#72812=CARTESIAN_POINT('Ctrl Pts',(4.5165353143801,6.49781253596613,37.6734581690479));
#72813=CARTESIAN_POINT('Ctrl Pts',(4.35777801693759,6.60533389271473,37.6808129086014));
#72814=CARTESIAN_POINT('Ctrl Pts',(4.02580875454984,6.81298283822459,37.6954447855455));
#72815=CARTESIAN_POINT('Ctrl Pts',(3.85239241672874,6.91252117236997,37.7026996592549));
#72816=CARTESIAN_POINT('Ctrl Pts',(3.1690638887644,7.27103044348587,37.7301567660788));
#72817=CARTESIAN_POINT('Ctrl Pts',(2.63546796499408,7.4809829268591,37.7491358755223));
#72818=CARTESIAN_POINT('Ctrl Pts',(1.84284387199572,7.69742191377548,37.7786343112821));
#72819=CARTESIAN_POINT('Ctrl Pts',(1.59877442321255,7.75179336408153,37.7879179371882));
#72820=CARTESIAN_POINT('Ctrl Pts',(1.31271264063229,7.80143193160307,37.7993850180541));
#72821=CARTESIAN_POINT('Ctrl Pts',(1.27283731290128,7.80803686924428,37.8009949538998));
#72822=CARTESIAN_POINT('Ctrl Pts',(1.22150517506652,7.81613584198696,37.8030809497118));
#72823=CARTESIAN_POINT('Ctrl Pts',(1.21009281712895,7.81791083123741,37.8035455727699));
#72824=CARTESIAN_POINT('Ctrl Pts',(1.19170420479502,7.82072962361312,37.8042955578566));
#72825=CARTESIAN_POINT('Ctrl Pts',(1.18473034454057,7.82178910273695,37.8045802997195));
#72826=CARTESIAN_POINT('Ctrl Pts',(1.17145011824583,7.82378848603372,37.8051231117874));
#72827=CARTESIAN_POINT('Ctrl Pts',(1.16514401170046,7.82473009665043,37.8053811154658));
#72828=CARTESIAN_POINT('Ctrl Pts',(1.15077189851091,7.82685834203353,37.8059696865679));
#72829=CARTESIAN_POINT('Ctrl Pts',(1.14270518907462,7.82804013268324,37.8063004389156));
#72830=CARTESIAN_POINT('Ctrl Pts',(1.11812834011462,7.83160189644056,37.8073093428725));
#72831=CARTESIAN_POINT('Ctrl Pts',(1.10161254513154,7.83394211393584,37.8079889821348));
#72832=CARTESIAN_POINT('Ctrl Pts',(0.981284226205531,7.85060408025789,37.8129521209237));
#72833=CARTESIAN_POINT('Ctrl Pts',(0.877206057646947,7.86291368243202,37.8173073258085));
#72834=CARTESIAN_POINT('Ctrl Pts',(0.165300409073685,7.9328023279853,37.8474142774084));
#72835=CARTESIAN_POINT('Ctrl Pts',(-0.447177677043078,7.92191436211371,
37.8747144257888));
#72836=CARTESIAN_POINT('Ctrl Pts',(-1.45498545193957,7.78665596903055,37.9186810360124));
#72837=CARTESIAN_POINT('Ctrl Pts',(-1.85292262537028,7.70166909409274,37.935827409712));
#72838=CARTESIAN_POINT('Ctrl Pts',(-2.31424785378348,7.56529983021761,37.9554636589941));
#72839=CARTESIAN_POINT('Ctrl Pts',(-2.38560331190508,7.54310292125155,37.9584952241123));
#72840=CARTESIAN_POINT('Ctrl Pts',(-2.47952628870685,7.51241974066353,37.9624804137584));
#72841=CARTESIAN_POINT('Ctrl Pts',(-2.50238419490923,7.50483672871961,37.9634498564228));
#72842=CARTESIAN_POINT('Ctrl Pts',(-2.53950473785945,7.49233370169141,37.9650234837776));
#72843=CARTESIAN_POINT('Ctrl Pts',(-2.5537885076299,7.48747706983161,37.965628833108));
#72844=CARTESIAN_POINT('Ctrl Pts',(-2.5812243836107,7.47806094149906,37.9667912346238));
#72845=CARTESIAN_POINT('Ctrl Pts',(-2.59437851638697,7.47350753518694,37.9673483987745));
#72846=CARTESIAN_POINT('Ctrl Pts',(-2.62444733879125,7.4630100228967,37.9686216682976));
#72847=CARTESIAN_POINT('Ctrl Pts',(-2.64135399337032,7.4570430815986,37.9693373344421));
#72848=CARTESIAN_POINT('Ctrl Pts',(-2.6945126484634,7.43807809402771,37.971586781919));
#72849=CARTESIAN_POINT('Ctrl Pts',(-2.73069024673419,7.42487272307073,37.9731165129498));
#72850=CARTESIAN_POINT('Ctrl Pts',(-3.06857350668557,7.29873665335821,37.9873931792002));
#72851=CARTESIAN_POINT('Ctrl Pts',(-3.36322139417798,7.16773735584352,37.9997455489935));
#72852=CARTESIAN_POINT('Ctrl Pts',(-4.01889341894382,6.8268694930818,38.0273770435127));
#72853=CARTESIAN_POINT('Ctrl Pts',(-4.3729357496788,6.60568592943777,38.0423877387682));
#72854=CARTESIAN_POINT('Ctrl Pts',(-4.81192342978387,6.28061038744971,38.0623321942736));
#72855=CARTESIAN_POINT('Ctrl Pts',(-4.91403457858747,6.20104324498531,38.0670794218106));
#72856=CARTESIAN_POINT('Ctrl Pts',(-5.19402001982697,5.9716125917231,38.0805124594735));
#72857=CARTESIAN_POINT('Ctrl Pts',(-5.367298804267,5.81636430251224,38.089314051897));
#72858=CARTESIAN_POINT('Ctrl Pts',(-5.54980628846175,5.63773830033998,38.0994248920202));
#72859=CARTESIAN_POINT('Ctrl Pts',(-5.56606478973794,5.62168708880586,38.100333339442));
#72860=CARTESIAN_POINT('Ctrl Pts',(-5.59429185564068,5.59357741334053,38.1019245335957));
#72861=CARTESIAN_POINT('Ctrl Pts',(-5.60629157875211,5.58155035566258,38.1026054321085));
#72862=CARTESIAN_POINT('Ctrl Pts',(-5.62359539843265,5.56409502004858,38.1035939305795));
#72863=CARTESIAN_POINT('Ctrl Pts',(-5.62893062517671,5.55869756451686,38.1038996284192));
#72864=CARTESIAN_POINT('Ctrl Pts',(-5.6382192634132,5.54927350026747,38.1044334679941));
#72865=CARTESIAN_POINT('Ctrl Pts',(-5.64217615507197,5.54525031698269,38.1046613939001));
#72866=CARTESIAN_POINT('Ctrl Pts',(-5.64980555553745,5.53747647755059,38.1051018659463));
#72867=CARTESIAN_POINT('Ctrl Pts',(-5.6534786442269,5.53372639131168,38.1053143756318));
#72868=CARTESIAN_POINT('Ctrl Pts',(-5.66216759438751,5.52483761735602,38.1058181552082));
#72869=CARTESIAN_POINT('Ctrl Pts',(-5.66718019036322,5.5196957574207,38.1061096309926));
#72870=CARTESIAN_POINT('Ctrl Pts',(-5.68208549734059,5.50436436779795,38.1069789106145));
#72871=CARTESIAN_POINT('Ctrl Pts',(-5.69195774024892,5.49415505529739,38.1075580232018));
#72872=CARTESIAN_POINT('Ctrl Pts',(-5.80536627073424,5.37624065898127,38.114250229616));
#72873=CARTESIAN_POINT('Ctrl Pts',(-5.90584783122677,5.26566175736592,38.1205733151838));
#72874=CARTESIAN_POINT('Ctrl Pts',(-6.00725855969204,5.14750481089611,38.1273280416066));
#72875=CARTESIAN_POINT('Ctrl Pts',(-6.01138117532429,5.14268971899392,38.1276033021788));
#72876=CARTESIAN_POINT('Ctrl Pts',(-6.54229996296318,4.52108171887196,38.1631370246617));
#72877=CARTESIAN_POINT('Ctrl Pts',(-6.97113206028465,3.82692971621161,38.2021659090481));
#72878=CARTESIAN_POINT('Ctrl Pts',(-7.37820212491066,2.86373938765046,38.2483028712294));
#72879=CARTESIAN_POINT('Ctrl Pts',(-7.45981795345878,2.64386030629179,38.2583949191294));
#72880=CARTESIAN_POINT('Ctrl Pts',(-7.56606917200836,2.31327539743514,38.272894775682));
#72881=CARTESIAN_POINT('Ctrl Pts',(-7.5982857282647,2.20515330447075,38.2775342975795));
#72882=CARTESIAN_POINT('Ctrl Pts',(-7.63318322867374,2.07817017892457,38.2828665581275));
#72883=CARTESIAN_POINT('Ctrl Pts',(-7.63812144861313,2.05994617343988,38.2836290445919));
#72884=CARTESIAN_POINT('Ctrl Pts',(-7.64555621822489,2.03211457481,38.2847893109544));
#72885=CARTESIAN_POINT('Ctrl Pts',(-7.64809999080462,2.02251973111002,38.2851885488024));
#72886=CARTESIAN_POINT('Ctrl Pts',(-7.65249116304121,2.00582994042879,38.2858816897108));
#72887=CARTESIAN_POINT('Ctrl Pts',(-7.654346768445,1.99873717609292,38.2861758457201));
#72888=CARTESIAN_POINT('Ctrl Pts',(-7.6581929341286,1.98395189469187,38.2867881747528));
#72889=CARTESIAN_POINT('Ctrl Pts',(-7.66018177058015,1.97625893519164,38.2871062943631));
#72890=CARTESIAN_POINT('Ctrl Pts',(-7.66561639185071,1.95510597598861,38.2879796914495));
#72891=CARTESIAN_POINT('Ctrl Pts',(-7.66903831985326,1.94163984698425,38.288534233441));
#72892=CARTESIAN_POINT('Ctrl Pts',(-7.68211621208046,1.88960116864405,38.2906715810454));
#72893=CARTESIAN_POINT('Ctrl Pts',(-7.69151685916195,1.85096475753186,38.2922465283114));
#72894=CARTESIAN_POINT('Ctrl Pts',(-7.84039088122147,1.21837123857555,38.3178426403182));
#72895=CARTESIAN_POINT('Ctrl Pts',(-7.91099079599388,0.610306051304702,
38.3395066691258));
#72896=CARTESIAN_POINT('Ctrl Pts',(-7.91100981824995,-0.65091673621086,
38.3831754832856));
#72897=CARTESIAN_POINT('Ctrl Pts',(-7.83065472643843,-1.29943978580713,
38.4050395380097));
#72898=CARTESIAN_POINT('Ctrl Pts',(-7.66160866396208,-1.97114432808144,
38.4323189790172));
#72899=CARTESIAN_POINT('Ctrl Pts',(-7.6511201427678,-2.01147153957299,38.4339741085834));
#72900=CARTESIAN_POINT('Ctrl Pts',(-7.63707579532795,-2.06377085953423,
38.4361416128402));
#72901=CARTESIAN_POINT('Ctrl Pts',(-7.63380940543998,-2.07582051811485,
38.436642456131));
#72902=CARTESIAN_POINT('Ctrl Pts',(-7.62855366735773,-2.09502867411696,
38.437443112728));
#72903=CARTESIAN_POINT('Ctrl Pts',(-7.62658272644618,-2.10219221703006,
38.4377422163453));
#72904=CARTESIAN_POINT('Ctrl Pts',(-7.62301986472479,-2.11507076418925,
38.4382808376318));
#72905=CARTESIAN_POINT('Ctrl Pts',(-7.62143159967058,-2.12078678014625,
38.4385202170476));
#72906=CARTESIAN_POINT('Ctrl Pts',(-7.61769773513827,-2.13416624191905,
38.4390812678936));
#72907=CARTESIAN_POINT('Ctrl Pts',(-7.61554700086746,-2.14182823986773,
38.4394031300336));
#72908=CARTESIAN_POINT('Ctrl Pts',(-7.60933793479913,-2.1638204684871,38.4403285732887));
#72909=CARTESIAN_POINT('Ctrl Pts',(-7.60525070176967,-2.17814246218283,
38.4409332049806));
#72910=CARTESIAN_POINT('Ctrl Pts',(-7.5780187615719,-2.27255422395595,38.444931552894));
#72911=CARTESIAN_POINT('Ctrl Pts',(-7.55365013972952,-2.35228401521999,
38.4483677745479));
#72912=CARTESIAN_POINT('Ctrl Pts',(-7.46994773376024,-2.61141824179472,
38.4597034060154));
#72913=CARTESIAN_POINT('Ctrl Pts',(-7.40544689783887,-2.78908175963155,
38.4677380148503));
#72914=CARTESIAN_POINT('Ctrl Pts',(-7.07771495103241,-3.60000882275987,
38.5052547123691));
#72915=CARTESIAN_POINT('Ctrl Pts',(-6.73918001943477,-4.19972462246992,
38.5350422230333));
#72916=CARTESIAN_POINT('Ctrl Pts',(-6.3101459695669,-4.77145896535504,38.5647594968143));
#72917=CARTESIAN_POINT('Ctrl Pts',(-6.29260390016519,-4.79456973868993,
38.5659639729351));
#72918=CARTESIAN_POINT('Ctrl Pts',(-6.13163730855142,-5.00422980959778,
38.5769217729587));
#72919=CARTESIAN_POINT('Ctrl Pts',(-5.98008222606419,-5.18439110800345,
38.5865565243785));
#72920=CARTESIAN_POINT('Ctrl Pts',(-5.76715154438655,-5.41573087583818,
38.5993752439367));
#72921=CARTESIAN_POINT('Ctrl Pts',(-5.71271275145341,-5.47312442421492,
38.6025942331002));
#72922=CARTESIAN_POINT('Ctrl Pts',(-5.59876785020851,-5.58970133406722,
38.6092122347445));
#72923=CARTESIAN_POINT('Ctrl Pts',(-5.53916212488614,-5.64877380785448,
38.61260986032));
#72924=CARTESIAN_POINT('Ctrl Pts',(-5.45461804362853,-5.72993636330983,
38.6173404197055));
#72925=CARTESIAN_POINT('Ctrl Pts',(-5.43046318661462,-5.75283393794001,
38.6186821565142));
#72926=CARTESIAN_POINT('Ctrl Pts',(-5.38824152429984,-5.79235504464503,
38.6210105346445));
#72927=CARTESIAN_POINT('Ctrl Pts',(-5.3702405230033,-5.80904815063089,38.6219979609916));
#72928=CARTESIAN_POINT('Ctrl Pts',(-5.33244069181307,-5.84377570419608,
38.6240604986701));
#72929=CARTESIAN_POINT('Ctrl Pts',(-5.31262739089202,-5.86179395947277,
38.6251354101817));
#72930=CARTESIAN_POINT('Ctrl Pts',(-5.26518294675502,-5.90450188944251,
38.6276947288119));
#72931=CARTESIAN_POINT('Ctrl Pts',(-5.23746904751534,-5.9290987523724,38.6291780093822));
#72932=CARTESIAN_POINT('Ctrl Pts',(-5.14197421867869,-6.01266107032881,
38.6342494938536));
#72933=CARTESIAN_POINT('Ctrl Pts',(-5.07336189055058,-6.07066646584998,
38.6378258484435));
#72934=CARTESIAN_POINT('Ctrl Pts',(-4.66993674814903,-6.40010784396557,
38.6584800837229));
#72935=CARTESIAN_POINT('Ctrl Pts',(-4.31437351420493,-6.6449892785218,38.6751810864711));
#72936=CARTESIAN_POINT('Ctrl Pts',(-3.59709648633883,-7.05703758469521,
38.7071584296001));
#72937=CARTESIAN_POINT('Ctrl Pts',(-3.23923220006731,-7.22829439386741,
38.7224061508348));
#72938=CARTESIAN_POINT('Ctrl Pts',(-2.82921270399289,-7.38792244027133,
38.7399332964247));
#72939=CARTESIAN_POINT('Ctrl Pts',(-2.78823298177557,-7.40348561816221,
38.741685928633));
#72940=CARTESIAN_POINT('Ctrl Pts',(-2.73262559852371,-7.42407687466456,
38.744066908039));
#72941=CARTESIAN_POINT('Ctrl Pts',(-2.71810921980288,-7.42940390404958,
38.7446887179512));
#72942=CARTESIAN_POINT('Ctrl Pts',(-2.69351667987478,-7.43834682553775,
38.745742655039));
#72943=CARTESIAN_POINT('Ctrl Pts',(-2.68344860948487,-7.44198489391061,
38.7461742774308));
#72944=CARTESIAN_POINT('Ctrl Pts',(-2.66405480154881,-7.44894831780974,
38.7470060113369));
#72945=CARTESIAN_POINT('Ctrl Pts',(-2.65473014235097,-7.45227662514535,
38.7474060530876));
#72946=CARTESIAN_POINT('Ctrl Pts',(-2.63272172823744,-7.46008567351715,
38.7483506071761));
#72947=CARTESIAN_POINT('Ctrl Pts',(-2.62003275830467,-7.46455158052007,
38.7488954724963));
#72948=CARTESIAN_POINT('Ctrl Pts',(-2.58138292288528,-7.47804377127799,
38.7505560620547));
#72949=CARTESIAN_POINT('Ctrl Pts',(-2.55538651510466,-7.48696708801213,
38.7516743561389));
#72950=CARTESIAN_POINT('Ctrl Pts',(-2.49446155000433,-7.50752542002795,
38.7542978521915));
#72951=CARTESIAN_POINT('Ctrl Pts',(-2.45949725145354,-7.51905243999628,
38.7558054904453));
#72952=CARTESIAN_POINT('Ctrl Pts',(-2.03578699504226,-7.65546948224984,
38.7740938095676));
#72953=CARTESIAN_POINT('Ctrl Pts',(-1.63802077000728,-7.75032395030728,
38.7914140914641));
#72954=CARTESIAN_POINT('Ctrl Pts',(-0.799431495454176,-7.88283181723932,
38.8271765843557));
#72955=CARTESIAN_POINT('Ctrl Pts',(-0.359141497706395,-7.91512309858168,
38.8455247451218));
#72956=CARTESIAN_POINT('Ctrl Pts',(0.127468642125678,-7.91010625107164,
38.8652725906629));
#72957=CARTESIAN_POINT('Ctrl Pts',(0.173376079523153,-7.90923320736555,
38.8671309885941));
#72958=CARTESIAN_POINT('Ctrl Pts',(0.247188518586936,-7.90718652134299,
38.87011209305));
#72959=CARTESIAN_POINT('Ctrl Pts',(0.27509930536438,-7.90626468233021,38.8712377493657));
#72960=CARTESIAN_POINT('Ctrl Pts',(0.324810799355717,-7.90435924976712,
38.8732399593243));
#72961=CARTESIAN_POINT('Ctrl Pts',(0.346613392718665,-7.90343320111091,
38.8741171750243));
#72962=CARTESIAN_POINT('Ctrl Pts',(0.392247566746003,-7.90130572876317,
38.8759514151218));
#72963=CARTESIAN_POINT('Ctrl Pts',(0.416078115186704,-7.90008666913056,
38.8769082272354));
#72964=CARTESIAN_POINT('Ctrl Pts',(0.478584092498757,-7.89660554587436,
38.8794153169725));
#72965=CARTESIAN_POINT('Ctrl Pts',(0.517249127963761,-7.89416716568477,
38.8809635752767));
#72966=CARTESIAN_POINT('Ctrl Pts',(0.697259648302866,-7.88148673556538,
38.8881611271639));
#72967=CARTESIAN_POINT('Ctrl Pts',(0.838332627271029,-7.86773178126254,
38.8937709018608));
#72968=CARTESIAN_POINT('Ctrl Pts',(1.62086629443244,-7.77014564311123,38.9248228976185));
#72969=CARTESIAN_POINT('Ctrl Pts',(2.25056849685423,-7.61166110748908,38.9496646258324));
#72970=CARTESIAN_POINT('Ctrl Pts',(3.31629040743672,-7.19943698053501,38.9925746549227));
#72971=CARTESIAN_POINT('Ctrl Pts',(3.76078971416224,-6.97754230099519,39.0108153383814));
#72972=CARTESIAN_POINT('Ctrl Pts',(4.27592054176512,-6.65678418947294,39.0342895664285));
#72973=CARTESIAN_POINT('Ctrl Pts',(4.36901202842072,-6.5960598147054,39.0386371732951));
#72974=CARTESIAN_POINT('Ctrl Pts',(4.48590999772952,-6.51624566575718,39.0442635493966));
#72975=CARTESIAN_POINT('Ctrl Pts',(4.51092946896942,-6.4989507910021,39.0454777228118));
#72976=CARTESIAN_POINT('Ctrl Pts',(4.54540417469726,-6.47482493360941,39.0471653183678));
#72977=CARTESIAN_POINT('Ctrl Pts',(4.55494512125043,-6.46811657076956,39.0476339187399));
#72978=CARTESIAN_POINT('Ctrl Pts',(4.57017156110797,-6.45736026657286,39.04838429675));
#72979=CARTESIAN_POINT('Ctrl Pts',(4.57586661147937,-6.4533258451668,39.0486655251054));
#72980=CARTESIAN_POINT('Ctrl Pts',(4.58757192078579,-6.44501042061869,39.0492447323563));
#72981=CARTESIAN_POINT('Ctrl Pts',(4.59358154196227,-6.44072853543507,39.0495427476473));
#72982=CARTESIAN_POINT('Ctrl Pts',(4.60749773194266,-6.43078379608512,39.0502343605096));
#72983=CARTESIAN_POINT('Ctrl Pts',(4.61539985797929,-6.42511476409802,39.0506282189203));
#72984=CARTESIAN_POINT('Ctrl Pts',(4.64032673271211,-6.40716236233438,39.0518742716282));
#72985=CARTESIAN_POINT('Ctrl Pts',(4.65731297294972,-6.39482584480044,39.0527287701526));
#72986=CARTESIAN_POINT('Ctrl Pts',(5.06805475228453,-6.09401375459001,39.0735265391759));
#72987=CARTESIAN_POINT('Ctrl Pts',(5.43422506600703,-5.76984843082238,39.095541584117));
#72988=CARTESIAN_POINT('Ctrl Pts',(6.27603840056216,-4.87299267831161,39.1518462263429));
#72989=CARTESIAN_POINT('Ctrl Pts',(6.7053796374883,-4.26297575916533,39.1857209588094));
#72990=CARTESIAN_POINT('Ctrl Pts',(7.06390711950271,-3.56190465030219,39.2179138693967));
#72991=CARTESIAN_POINT('Ctrl Pts',(7.08406663873472,-3.52164002632757,39.219743014043));
#72992=CARTESIAN_POINT('Ctrl Pts',(7.11016576216679,-3.4683811466781,39.2221367142375));
#72993=CARTESIAN_POINT('Ctrl Pts',(7.11641530227057,-3.45554021716885,39.2227118875952));
#72994=CARTESIAN_POINT('Ctrl Pts',(7.12603771020939,-3.43563223722311,39.2236005934681));
#72995=CARTESIAN_POINT('Ctrl Pts',(7.12943489874847,-3.42857701411655,39.2239149585747));
#72996=CARTESIAN_POINT('Ctrl Pts',(7.1361987940855,-3.41447634986946,39.2245420880664));
#72997=CARTESIAN_POINT('Ctrl Pts',(7.1395655560033,-3.40743094493573,39.2248548541176));
#72998=CARTESIAN_POINT('Ctrl Pts',(7.14703424237991,-3.39174204113685,39.2255500443789));
#72999=CARTESIAN_POINT('Ctrl Pts',(7.15113093226423,-3.38309605624769,39.2259322892975));
#73000=CARTESIAN_POINT('Ctrl Pts',(7.16299062105289,-3.35794861834376,39.2270415649767));
#73001=CARTESIAN_POINT('Ctrl Pts',(7.17071228216737,-3.3414276788144,39.2277671830755));
#73002=CARTESIAN_POINT('Ctrl Pts',(7.22457569450785,-3.22513720968939,39.2328529280268));
#73003=CARTESIAN_POINT('Ctrl Pts',(7.2686917478937,-3.12444002289568,39.2371436477149));
#73004=CARTESIAN_POINT('Ctrl Pts',(7.39980491508323,-2.80734608739438,39.2503238604886));
#73005=CARTESIAN_POINT('Ctrl Pts',(7.47934402141128,-2.5879967734711,39.2589641881539));
#73006=CARTESIAN_POINT('Ctrl Pts',(7.77487786782445,-1.64482940394179,39.2945515432749));
#73007=CARTESIAN_POINT('Ctrl Pts',(7.89631324499339,-0.895688255920419,
39.3186354178186));
#73008=CARTESIAN_POINT('Ctrl Pts',(7.91113426286729,-0.0628401258798168,
39.3486620262958));
#73009=CARTESIAN_POINT('Ctrl Pts',(7.91136941031116,0.0150931128500409,
39.3515068206282));
#73010=CARTESIAN_POINT('Ctrl Pts',(7.90914645800753,0.204142758367049,39.3585170221932));
#73011=CARTESIAN_POINT('Ctrl Pts',(7.90549825472322,0.315226201816551,39.3627277977289));
#73012=CARTESIAN_POINT('Ctrl Pts',(7.89757202801532,0.46213966515205,39.3684572545262));
#73013=CARTESIAN_POINT('Ctrl Pts',(7.89538725358157,0.498073340249719,39.3698713652257));
#73014=CARTESIAN_POINT('Ctrl Pts',(7.89109160886784,0.561567634263152,39.3723943908811));
#73015=CARTESIAN_POINT('Ctrl Pts',(7.88908139998445,0.589134633937439,39.3734979116748));
#73016=CARTESIAN_POINT('Ctrl Pts',(7.88629302747159,0.62479547187006,39.3749365247286));
#73017=CARTESIAN_POINT('Ctrl Pts',(7.88564677399291,0.632899716942392,39.375264204287));
#73018=CARTESIAN_POINT('Ctrl Pts',(7.8846378211372,0.645310863453291,39.3757671792674));
#73019=CARTESIAN_POINT('Ctrl Pts',(7.88428408135613,0.649618507527592,39.3759419641523));
#73020=CARTESIAN_POINT('Ctrl Pts',(7.88361246630713,0.657715700628144,39.3762709156675));
#73021=CARTESIAN_POINT('Ctrl Pts',(7.88329538817588,0.661505317019026,39.3764250365274));
#73022=CARTESIAN_POINT('Ctrl Pts',(7.88257593252306,0.670030037517674,39.376772107259));
#73023=CARTESIAN_POINT('Ctrl Pts',(7.88217202098633,0.674765006913782,39.3769651456983));
#73024=CARTESIAN_POINT('Ctrl Pts',(7.88106023655268,0.687661000316005,39.3774916169928));
#73025=CARTESIAN_POINT('Ctrl Pts',(7.88034395449867,0.695821285819502,39.3778255399807));
#73026=CARTESIAN_POINT('Ctrl Pts',(7.8765539268322,0.73824286118144,39.3795655905216));
#73027=CARTESIAN_POINT('Ctrl Pts',(7.87326946013208,0.772484446792259,39.3809841316718));
#73028=CARTESIAN_POINT('Ctrl Pts',(7.83713095376385,1.12503233668865,39.3957251190699));
#73029=CARTESIAN_POINT('Ctrl Pts',(7.78521805078241,1.44106340421453,39.4100707466557));
#73030=CARTESIAN_POINT('Ctrl Pts',(7.5223260687658,2.59792238958884,39.464524897215));
#73031=CARTESIAN_POINT('Ctrl Pts',(7.19275528358834,3.40581461046731,39.5055529444607));
#73032=CARTESIAN_POINT('Ctrl Pts',(6.71077311124079,4.18954426720153,39.5432300339242));
#73033=CARTESIAN_POINT('Ctrl Pts',(6.68241863323018,4.23462374758903,39.545392731348));
#73034=CARTESIAN_POINT('Ctrl Pts',(6.64587770808624,4.29143738712001,39.5481130923226));
#73035=CARTESIAN_POINT('Ctrl Pts',(6.63811208384724,4.30343970838252,39.5486874884755));
#73036=CARTESIAN_POINT('Ctrl Pts',(6.62576606730168,4.32240841766777,39.5495948113172));
#73037=CARTESIAN_POINT('Ctrl Pts',(6.62120714166934,4.32938869766044,39.5499285963988));
#73038=CARTESIAN_POINT('Ctrl Pts',(6.61271057487117,4.34235318326565,39.5505483533919));
#73039=CARTESIAN_POINT('Ctrl Pts',(6.60877582624161,4.34833926851263,39.5508344408915));
#73040=CARTESIAN_POINT('Ctrl Pts',(6.60005359349936,4.36156955246328,39.5514665857459));
#73041=CARTESIAN_POINT('Ctrl Pts',(6.59526229891212,4.36881123502164,39.551812489324));
#73042=CARTESIAN_POINT('Ctrl Pts',(6.58145961970992,4.38959849654459,39.5528051104522));
#73043=CARTESIAN_POINT('Ctrl Pts',(6.57241833435402,4.4031242236997,39.5534506213828));
#73044=CARTESIAN_POINT('Ctrl Pts',(6.51272632871377,4.49182972058001,39.5576817870158));
#73045=CARTESIAN_POINT('Ctrl Pts',(6.46082734931513,4.56616350572395,39.5612165434991));
#73046=CARTESIAN_POINT('Ctrl Pts',(6.30558089509436,4.78057178786957,39.5713907791924));
#73047=CARTESIAN_POINT('Ctrl Pts',(6.19887275518761,4.91814986443986,39.5778906434871));
#73048=CARTESIAN_POINT('Ctrl Pts',(6.01702912271833,5.13726878629127,39.5882628498776));
#73049=CARTESIAN_POINT('Ctrl Pts',(5.94456923086756,5.22094508997288,39.5922292224447));
#73050=CARTESIAN_POINT('Ctrl Pts',(5.81646868286776,5.36274930153257,39.5989861327818));
#73051=CARTESIAN_POINT('Ctrl Pts',(5.76165398796227,5.42159862186811,39.6018013091954));
#73052=CARTESIAN_POINT('Ctrl Pts',(5.35593444996822,5.84407739244176,39.6221418083102));
#73053=CARTESIAN_POINT('Ctrl Pts',(4.97182155525041,6.17415844202331,39.6386593473583));
#73054=CARTESIAN_POINT('Ctrl Pts',(4.35320216799812,6.61036154238549,39.6650441185029));
#73055=CARTESIAN_POINT('Ctrl Pts',(4.14074875590315,6.74547490770903,39.6740908337311));
#73056=CARTESIAN_POINT('Ctrl Pts',(3.85337036410591,6.90954020288023,39.6867981478361));
#73057=CARTESIAN_POINT('Ctrl Pts',(3.78392091849768,6.94781624956217,39.6899038310327));
#73058=CARTESIAN_POINT('Ctrl Pts',(3.70424046642362,6.99018193638044,39.6935200671318));
#73059=CARTESIAN_POINT('Ctrl Pts',(3.69456013274496,6.99530316425914,39.6939602836247));
#73060=CARTESIAN_POINT('Ctrl Pts',(3.68025209831515,7.0028346201805,39.6946122945205));
#73061=CARTESIAN_POINT('Ctrl Pts',(3.67563259059131,7.00526040083783,39.6948230111966));
#73062=CARTESIAN_POINT('Ctrl Pts',(3.66741284780572,7.00956635607492,39.6951983216982));
#73063=CARTESIAN_POINT('Ctrl Pts',(3.66381359176345,7.01144831408973,39.6953627881956));
#73064=CARTESIAN_POINT('Ctrl Pts',(3.6562974809123,7.01537092655476,39.6957064934848));
#73065=CARTESIAN_POINT('Ctrl Pts',(3.65238036448886,7.01741107382281,39.6958857669346));
#73066=CARTESIAN_POINT('Ctrl Pts',(3.6423227292759,7.0226386780009,39.6963464447277));
#73067=CARTESIAN_POINT('Ctrl Pts',(3.63617974540995,7.02582135585667,39.696628173266));
#73068=CARTESIAN_POINT('Ctrl Pts',(3.61066492203174,7.03899815116564,39.6977997830988));
#73069=CARTESIAN_POINT('Ctrl Pts',(3.59125616343564,7.04892015142095,39.6986944826849));
#73070=CARTESIAN_POINT('Ctrl Pts',(3.54126602492629,7.07421568141801,39.7010073182057));
#73071=CARTESIAN_POINT('Ctrl Pts',(3.51062568772735,7.08947105061343,39.7024329640918));
#73072=CARTESIAN_POINT('Ctrl Pts',(3.38406902279584,7.15146011751771,39.7083513555607));
#73073=CARTESIAN_POINT('Ctrl Pts',(3.28731438915655,7.19644823614337,39.7129463705618));
#73074=CARTESIAN_POINT('Ctrl Pts',(2.90152686785163,7.36642493136792,39.7314548387959));
#73075=CARTESIAN_POINT('Ctrl Pts',(2.60606280460498,7.47606096161805,39.7460290344763));
#73076=CARTESIAN_POINT('Ctrl Pts',(1.67352074052255,7.76007921745206,39.7916666038562));
#73077=CARTESIAN_POINT('Ctrl Pts',(1.02047861694388,7.87263359857287,39.822867946901));
#73078=CARTESIAN_POINT('Ctrl Pts',(0.140654800042331,7.91282452431211,39.8608984824239));
#73079=CARTESIAN_POINT('Ctrl Pts',(-0.080028247656927,7.91367058139126,
39.8701365449494));
#73080=CARTESIAN_POINT('Ctrl Pts',(-0.32147299899154,7.90449351925316,39.8799270859024));
#73081=CARTESIAN_POINT('Ctrl Pts',(-0.342470980685254,7.90361159986924,
39.8807759610251));
#73082=CARTESIAN_POINT('Ctrl Pts',(-0.37360047820906,7.90217986517778,39.8820306278958));
#73083=CARTESIAN_POINT('Ctrl Pts',(-0.383734765081152,7.90169422149441,
39.8824384921223));
#73084=CARTESIAN_POINT('Ctrl Pts',(-0.401061400542074,7.90083050222642,
39.8831348076947));
#73085=CARTESIAN_POINT('Ctrl Pts',(-0.408254206519649,7.90046209883756,
39.8834235709902));
#73086=CARTESIAN_POINT('Ctrl Pts',(-0.422229421657502,7.89972717570526,
39.8839840453006));
#73087=CARTESIAN_POINT('Ctrl Pts',(-0.429011880851549,7.89936174266642,
39.8842557911373));
#73088=CARTESIAN_POINT('Ctrl Pts',(-0.445205350891899,7.89846833513182,
39.8849039714005));
#73089=CARTESIAN_POINT('Ctrl Pts',(-0.454615915161151,7.89793227471796,
39.8852801448721));
#73090=CARTESIAN_POINT('Ctrl Pts',(-0.482725710398447,7.89628063032873,
39.8864022930131));
#73091=CARTESIAN_POINT('Ctrl Pts',(-0.50142202161738,7.8951154435487,39.8871466701851));
#73092=CARTESIAN_POINT('Ctrl Pts',(-0.660017048269538,7.88466589658636,
39.8934444269884));
#73093=CARTESIAN_POINT('Ctrl Pts',(-0.799654037753729,7.87173009599693,
39.8988793234973));
#73094=CARTESIAN_POINT('Ctrl Pts',(-1.29594959264021,7.81241045480591,39.9178655120552));
#73095=CARTESIAN_POINT('Ctrl Pts',(-1.64970937858002,7.74543260241374,39.9307648251475));
#73096=CARTESIAN_POINT('Ctrl Pts',(-2.06719586534866,7.63647698437656,39.9458506606912));
#73097=CARTESIAN_POINT('Ctrl Pts',(-2.13644083943982,7.61739457547457,39.9483491978771));
#73098=CARTESIAN_POINT('Ctrl Pts',(-2.26330029100403,7.58056895227552,39.9529303291083));
#73099=CARTESIAN_POINT('Ctrl Pts',(-2.32099010376022,7.56310510427093,39.9550150525149));
#73100=CARTESIAN_POINT('Ctrl Pts',(-2.42793927787715,7.52939052916617,39.9588891968728));
#73101=CARTESIAN_POINT('Ctrl Pts',(-2.47724921620078,7.5133113341546,39.9606791450338));
#73102=CARTESIAN_POINT('Ctrl Pts',(-2.56941876738174,7.48225027809897,39.9640364348168));
#73103=CARTESIAN_POINT('Ctrl Pts',(-2.61231441930413,7.46738209783918,39.9656036477097));
#73104=CARTESIAN_POINT('Ctrl Pts',(-2.69302041430844,7.43862784895288,39.9685644075401));
#73105=CARTESIAN_POINT('Ctrl Pts',(-2.73085730750169,7.42482064315305,39.9699575570814));
#73106=CARTESIAN_POINT('Ctrl Pts',(-2.80250055328276,7.39805530521667,39.9726074176593));
#73107=CARTESIAN_POINT('Ctrl Pts',(-2.83632661821765,7.38515287272247,39.9738636446431));
#73108=CARTESIAN_POINT('Ctrl Pts',(-3.22675793843371,7.23315075950918,39.9884331377066));
#73109=CARTESIAN_POINT('Ctrl Pts',(-3.57288412273344,7.06858542733107,40.0020100056435));
#73110=CARTESIAN_POINT('Ctrl Pts',(-3.96260347854693,6.84733336084427,40.0194769653508));
#73111=CARTESIAN_POINT('Ctrl Pts',(-4.01908862889808,6.8143324478534,40.0220645152471));
#73112=CARTESIAN_POINT('Ctrl Pts',(-4.0862775477239,6.7739519591715,40.0252048793601));
#73113=CARTESIAN_POINT('Ctrl Pts',(-4.09738183142048,6.76724105282791,40.0257259528498));
#73114=CARTESIAN_POINT('Ctrl Pts',(-4.11544395846612,6.75626439923794,40.0265768461123));
#73115=CARTESIAN_POINT('Ctrl Pts',(-4.12241182559444,6.75201513233165,40.0269059046806));
#73116=CARTESIAN_POINT('Ctrl Pts',(-4.13481246030258,6.74442640890183,40.027492952359));
#73117=CARTESIAN_POINT('Ctrl Pts',(-4.14024779589585,6.74109114722834,40.0277507510214));
#73118=CARTESIAN_POINT('Ctrl Pts',(-4.15156223827328,6.7341294683586,40.0282884084115));
#73119=CARTESIAN_POINT('Ctrl Pts',(-4.15744063867017,6.73050191667929,40.0285683178254));
#73120=CARTESIAN_POINT('Ctrl Pts',(-4.17276437549087,6.72101792729627,40.0292994588515));
#73121=CARTESIAN_POINT('Ctrl Pts',(-4.18220211739188,6.71514928799971,40.0297512280887));
#73122=CARTESIAN_POINT('Ctrl Pts',(-4.20285800854994,6.7022444684399,40.0307431666832));
#73123=CARTESIAN_POINT('Ctrl Pts',(-4.21407091010389,6.69519997586373,40.0312836929362));
#73124=CARTESIAN_POINT('Ctrl Pts',(-4.24697253341932,6.67441417092408,40.032875705267));
#73125=CARTESIAN_POINT('Ctrl Pts',(-4.26861200189376,6.66059545265817,40.0339304175673));
#73126=CARTESIAN_POINT('Ctrl Pts',(-4.34366651095584,6.61215051031579,40.037614434611));
#73127=CARTESIAN_POINT('Ctrl Pts',(-4.39672995577182,6.57698552383581,40.040264820952));
#73128=CARTESIAN_POINT('Ctrl Pts',(-4.60177473636943,6.43751253821415,40.050672428993));
#73129=CARTESIAN_POINT('Ctrl Pts',(-4.75051304195258,6.32854804558949,40.0585814619191));
#73130=CARTESIAN_POINT('Ctrl Pts',(-5.2521752520448,5.93337663253643,40.0862706967208));
#73131=CARTESIAN_POINT('Ctrl Pts',(-5.5841705389251,5.62204211675794,40.1063700147992));
#73132=CARTESIAN_POINT('Ctrl Pts',(-6.09332178049453,5.05472091788597,40.1392739320605));
#73133=CARTESIAN_POINT('Ctrl Pts',(-6.28547614589442,4.81368657991219,40.1523293518545));
#73134=CARTESIAN_POINT('Ctrl Pts',(-6.47508990065234,4.54505934433498,40.1659285153721));
#73135=CARTESIAN_POINT('Ctrl Pts',(-6.48701799195423,4.52801846750245,40.1667873749137));
#73136=CARTESIAN_POINT('Ctrl Pts',(-6.56904353959225,4.40984460804113,40.1727170855935));
#73137=CARTESIAN_POINT('Ctrl Pts',(-6.63684131314007,4.30713371889715,40.1777381154848));
#73138=CARTESIAN_POINT('Ctrl Pts',(-6.71694103290499,4.17940094962973,40.1838310159566));
#73139=CARTESIAN_POINT('Ctrl Pts',(-6.73154193568581,4.15584315369801,40.1849485897316));
#73140=CARTESIAN_POINT('Ctrl Pts',(-6.75518160095659,4.11725032742334,40.1867693960527));
#73141=CARTESIAN_POINT('Ctrl Pts',(-6.76429466236532,4.10226113797595,40.187474132729));
#73142=CARTESIAN_POINT('Ctrl Pts',(-6.78050365021546,4.07539967935176,40.1887326768995));
#73143=CARTESIAN_POINT('Ctrl Pts',(-6.78761843187343,4.06353889138136,40.1892868718717));
#73144=CARTESIAN_POINT('Ctrl Pts',(-6.80261145565194,4.0383953346864,40.1904584890285));
#73145=CARTESIAN_POINT('Ctrl Pts',(-6.81048198537449,4.02510802646178,40.1910757485691));
#73146=CARTESIAN_POINT('Ctrl Pts',(-6.83133596730885,3.9896653153138,40.1927172077337));
#73147=CARTESIAN_POINT('Ctrl Pts',(-6.84425056567696,3.96746954998603,40.1937399508534));
#73148=CARTESIAN_POINT('Ctrl Pts',(-6.90468869961299,3.86242378662305,40.1985558008823));
#73149=CARTESIAN_POINT('Ctrl Pts',(-6.95081788858602,3.77877952729895,40.2023187916375));
#73150=CARTESIAN_POINT('Ctrl Pts',(-7.22342233810574,3.26258616503966,40.2251173770489));
#73151=CARTESIAN_POINT('Ctrl Pts',(-7.41096919416746,2.81067056843982,40.2431829927566));
#73152=CARTESIAN_POINT('Ctrl Pts',(-7.6606742474745,2.0058822105014,40.2738934044646));
#73153=CARTESIAN_POINT('Ctrl Pts',(-7.74282301829315,1.66077419386668,40.2866601413561));
#73154=CARTESIAN_POINT('Ctrl Pts',(-7.80776906374627,1.27438878554553,40.3013395267461));
#73155=CARTESIAN_POINT('Ctrl Pts',(-7.81371652344107,1.23739992954977,40.3027488926121));
#73156=CARTESIAN_POINT('Ctrl Pts',(-7.82365348426069,1.17266901230708,40.3052242941165));
#73157=CARTESIAN_POINT('Ctrl Pts',(-7.82775872736925,1.14494530162478,40.3062873651171));
#73158=CARTESIAN_POINT('Ctrl Pts',(-7.83595384321674,1.08749650566718,40.3084971332476));
#73159=CARTESIAN_POINT('Ctrl Pts',(-7.8400220911903,1.05776881672722,40.3096444161343));
#73160=CARTESIAN_POINT('Ctrl Pts',(-7.84592396866892,1.01273670555742,40.3113889521385));
#73161=CARTESIAN_POINT('Ctrl Pts',(-7.84788216963856,0.997448748038592,
40.3119823562326));
#73162=CARTESIAN_POINT('Ctrl Pts',(-7.86215888453117,0.883343266028346,
40.3164205382333));
#73163=CARTESIAN_POINT('Ctrl Pts',(-7.87265492056882,0.784309288593359,
40.3203236668393));
#73164=CARTESIAN_POINT('Ctrl Pts',(-7.88257497961383,0.67019163305026,40.3249046720238));
#73165=CARTESIAN_POINT('Ctrl Pts',(-7.88382915718263,0.65527318748757,40.3255051784838));
#73166=CARTESIAN_POINT('Ctrl Pts',(-7.88562425964197,0.633168983982901,
40.3263974670674));
#73167=CARTESIAN_POINT('Ctrl Pts',(-7.88619773057843,0.625985846685082,
40.3266878280719));
#73168=CARTESIAN_POINT('Ctrl Pts',(-7.88719826268721,0.613233853971028,
40.3272040154966));
#73169=CARTESIAN_POINT('Ctrl Pts',(-7.8876292428401,0.607665304134125,40.3274296678775));
#73170=CARTESIAN_POINT('Ctrl Pts',(-7.88844853387981,0.596931785115121,
40.3278650948511));
#73171=CARTESIAN_POINT('Ctrl Pts',(-7.88883767020609,0.591766880364478,
40.3280748322352));
#73172=CARTESIAN_POINT('Ctrl Pts',(-7.88966549891312,0.5806333884767,40.3285274079213));
#73173=CARTESIAN_POINT('Ctrl Pts',(-7.89010249109803,0.57466468154663,40.3287703233468));
#73174=CARTESIAN_POINT('Ctrl Pts',(-7.89114115045964,0.560253497163474,
40.3293575387927));
#73175=CARTESIAN_POINT('Ctrl Pts',(-7.89173604169649,0.551810551625998,
40.3297021506095));
#73176=CARTESIAN_POINT('Ctrl Pts',(-7.89330297783959,0.529051045923306,
40.3306327295443));
#73177=CARTESIAN_POINT('Ctrl Pts',(-7.8942496179195,0.514732818828182,40.3312198875157));
#73178=CARTESIAN_POINT('Ctrl Pts',(-7.90572984560547,0.333605723165124,
40.3386701185946));
#73179=CARTESIAN_POINT('Ctrl Pts',(-7.9110123521574,0.166522693952854,40.3457953989745));
#73180=CARTESIAN_POINT('Ctrl Pts',(-7.91099997831229,-0.000585784094123132,
40.3531019614398));
#73181=CARTESIAN_POINT('',(-7.90825726396148,0.00539299807561528,42.3576680289075));
#73182=CARTESIAN_POINT('Ctrl Pts',(-7.91892560419408,-0.000477670393038393,
40.3576684917631));
#73183=CARTESIAN_POINT('Ctrl Pts',(-7.9047553262244,-2.46403417491885,40.4571955913693));
#73184=CARTESIAN_POINT('Ctrl Pts',(-6.01794529465323,-6.22621325369113,
40.6096439579526));
#73185=CARTESIAN_POINT('Ctrl Pts',(-1.09061100011871,-8.16228612049071,
40.8150135915134));
#73186=CARTESIAN_POINT('Ctrl Pts',(2.94220442931933,-7.7101370801012,40.9737773924446));
#73187=CARTESIAN_POINT('Ctrl Pts',(6.25649344662756,-5.35431747772407,41.1325411933765));
#73188=CARTESIAN_POINT('Ctrl Pts',(8.70421013023098,-0.493722870432395,
41.3442262612849));
#73189=CARTESIAN_POINT('Ctrl Pts',(6.60205231354672,6.62635550641215,41.608832596171));
#73190=CARTESIAN_POINT('Ctrl Pts',(-2.01662681621539,9.14104728615634,41.9263601980336));
#73191=CARTESIAN_POINT('Ctrl Pts',(-7.29947900301956,4.51893018671728,42.1759720089462));
#73192=CARTESIAN_POINT('Ctrl Pts',(-7.91185655759119,0.949470213429403,
42.319741285904));
#73193=CARTESIAN_POINT('Ctrl Pts',(-7.90825726396148,0.00539299807561528,
42.3576680289075));
#73194=CARTESIAN_POINT('',(-7.91099872614571,-0.004489423238615,44.3576684917631));
#73195=CARTESIAN_POINT('Ctrl Pts',(-7.91099816834962,0.00538334179892528,
42.3576684917631));
#73196=CARTESIAN_POINT('Ctrl Pts',(-7.91113024696707,-0.18871053886295,
42.3654632149619));
#73197=CARTESIAN_POINT('Ctrl Pts',(-7.9041150552579,-0.382973778850431,
42.3732579381608));
#73198=CARTESIAN_POINT('Ctrl Pts',(-7.8899419111821,-0.576834151357323,
42.3810526613597));
#73199=CARTESIAN_POINT('Ctrl Pts',(-7.87685079500157,-0.755894538080088,
42.3882523078493));
#73200=CARTESIAN_POINT('Ctrl Pts',(-7.85765347124877,-0.934610951447137,
42.3954519543389));
#73201=CARTESIAN_POINT('Ctrl Pts',(-7.83238104679367,-1.11253230866672,
42.4026516008285));
#73202=CARTESIAN_POINT('Ctrl Pts',(-7.80466487664022,-1.3076579729809,42.4105474252875));
#73203=CARTESIAN_POINT('Ctrl Pts',(-7.76965417934316,-1.50173723265223,
42.4184432497465));
#73204=CARTESIAN_POINT('Ctrl Pts',(-7.72745945464938,-1.69419342955575,
42.4263390742055));
#73205=CARTESIAN_POINT('Ctrl Pts',(-7.68525522192022,-1.88669299397369,
42.4342366778864));
#73206=CARTESIAN_POINT('Ctrl Pts',(-7.63586380877042,-2.07756843230082,
42.4421342815673));
#73207=CARTESIAN_POINT('Ctrl Pts',(-7.57944638287488,-2.26625539803548,
42.4500318852482));
#73208=CARTESIAN_POINT('Ctrl Pts',(-7.52300695240184,-2.45501595764461,
42.4579325692439));
#73209=CARTESIAN_POINT('Ctrl Pts',(-7.45953614592364,-2.64158601582986,
42.4658332532396));
#73210=CARTESIAN_POINT('Ctrl Pts',(-7.38924442052067,-2.82541818034147,
42.4737339372353));
#73211=CARTESIAN_POINT('Ctrl Pts',(-7.31887553032036,-3.00945215198811,
42.481643294438));
#73212=CARTESIAN_POINT('Ctrl Pts',(-7.24167088411708,-3.19074190532464,
42.4895526516406));
#73213=CARTESIAN_POINT('Ctrl Pts',(-7.15788884657419,-3.36876064155481,
42.4974620088432));
#73214=CARTESIAN_POINT('Ctrl Pts',(-7.07405692569699,-3.5468853690976,42.5053760752308));
#73215=CARTESIAN_POINT('Ctrl Pts',(-6.98363996176963,-3.72173489275421,
42.5132901416184));
#73216=CARTESIAN_POINT('Ctrl Pts',(-6.88694154181228,-3.89280839493293,
42.521204208006));
#73217=CARTESIAN_POINT('Ctrl Pts',(-6.79010815352162,-4.06412067563019,
42.5291293205756));
#73218=CARTESIAN_POINT('Ctrl Pts',(-6.68697596968834,-4.23164611266594,
42.5370544331452));
#73219=CARTESIAN_POINT('Ctrl Pts',(-6.57789179660735,-4.39491302668503,
42.5449795457148));
#73220=CARTESIAN_POINT('Ctrl Pts',(-6.50248206794155,-4.50777920459647,
42.5504581643966));
#73221=CARTESIAN_POINT('Ctrl Pts',(-6.42422879901295,-4.61861091326156,
42.5559367830783));
#73222=CARTESIAN_POINT('Ctrl Pts',(-6.34325741845261,-4.72726203242912,
42.56141540176));
#73223=CARTESIAN_POINT('Ctrl Pts',(-6.22317456187274,-4.88839472733875,
42.5695403488321));
#73224=CARTESIAN_POINT('Ctrl Pts',(-6.09684859963159,-5.04508340046696,
42.5776652959043));
#73225=CARTESIAN_POINT('Ctrl Pts',(-5.96463392833433,-5.19683202547118,
42.5857902429765));
#73226=CARTESIAN_POINT('Ctrl Pts',(-5.83253577703048,-5.34844691532628,
42.5939080295817));
#73227=CARTESIAN_POINT('Ctrl Pts',(-5.69455947321675,-5.49513019650033,
42.6020258161869));
#73228=CARTESIAN_POINT('Ctrl Pts',(-5.55110078110194,-5.63641740097816,
42.6101436027922));
#73229=CARTESIAN_POINT('Ctrl Pts',(-5.40774811398311,-5.77760018532595,
42.6182553898426));
#73230=CARTESIAN_POINT('Ctrl Pts',(-5.25892136528683,-5.91339462065451,
42.6263671768929));
#73231=CARTESIAN_POINT('Ctrl Pts',(-5.10505477600203,-6.04337130532444,
42.6344789639433));
#73232=CARTESIAN_POINT('Ctrl Pts',(-4.95128004829302,-6.17327039119191,
42.642585908087));
#73233=CARTESIAN_POINT('Ctrl Pts',(-4.79247172446257,-6.29735844626082,
42.6506928522306));
#73234=CARTESIAN_POINT('Ctrl Pts',(-4.62909933209039,-6.4152443736494,42.6587997963743));
#73235=CARTESIAN_POINT('Ctrl Pts',(-4.46580129601439,-6.53307664716902,
42.6669030507737));
#73236=CARTESIAN_POINT('Ctrl Pts',(-4.2979435938005,-6.6447122353955,42.6750063051732));
#73237=CARTESIAN_POINT('Ctrl Pts',(-4.12602757531319,-6.74980128950143,
42.6831095595726));
#73238=CARTESIAN_POINT('Ctrl Pts',(-3.95291345593058,-6.8556227203278,42.691269286408));
#73239=CARTESIAN_POINT('Ctrl Pts',(-3.77568449598357,-6.95480581642194,
42.6994290132435));
#73240=CARTESIAN_POINT('Ctrl Pts',(-3.5948819093796,-7.04703803435282,42.7075887400789));
#73241=CARTESIAN_POINT('Ctrl Pts',(-3.41539852283936,-7.13859729317367,
42.7156889306413));
#73242=CARTESIAN_POINT('Ctrl Pts',(-3.23239378349034,-7.22330663852351,
42.7237891212037));
#73243=CARTESIAN_POINT('Ctrl Pts',(-3.04642167655107,-7.30090651690869,
42.7318893117661));
#73244=CARTESIAN_POINT('Ctrl Pts',(-2.86045067859473,-7.37850593255275,
42.7399894540257));
#73245=CARTESIAN_POINT('Ctrl Pts',(-2.67151264429676,-7.4489958424245,42.7480895962853));
#73246=CARTESIAN_POINT('Ctrl Pts',(-2.48018164408593,-7.51216480199544,
42.7561897385449));
#73247=CARTESIAN_POINT('Ctrl Pts',(-2.28882710835914,-7.57534153194366,
42.7642908771983));
#73248=CARTESIAN_POINT('Ctrl Pts',(-2.09507932430806,-7.6311954156024,42.7723920158517));
#73249=CARTESIAN_POINT('Ctrl Pts',(-1.89952815504884,-7.67956468741404,
42.7804931545052));
#73250=CARTESIAN_POINT('Ctrl Pts',(-1.70149032427789,-7.72854903100981,
42.7886973085983));
#73251=CARTESIAN_POINT('Ctrl Pts',(-1.50160325697955,-7.76985702428737,
42.7969014626915));
#73252=CARTESIAN_POINT('Ctrl Pts',(-1.30049100326436,-7.8033738953371,42.8051056167846));
#73253=CARTESIAN_POINT('Ctrl Pts',(-1.10171483656257,-7.83650143990004,
42.813214472767));
#73254=CARTESIAN_POINT('Ctrl Pts',(-0.901742118956392,-7.86201788206749,
42.8213233287494));
#73255=CARTESIAN_POINT('Ctrl Pts',(-0.701181595934555,-7.87986455273964,
42.8294321847318));
#73256=CARTESIAN_POINT('Ctrl Pts',(-0.497085486823625,-7.89802583388256,
42.8376839878803));
#73257=CARTESIAN_POINT('Ctrl Pts',(-0.292381002291157,-7.90824438756082,
42.8459357910288));
#73258=CARTESIAN_POINT('Ctrl Pts',(-0.0877110389684923,-7.91051374903319,
42.8541875941774));
#73259=CARTESIAN_POINT('Ctrl Pts',(0.116958924354173,-7.91278311050555,
42.8624393973259));
#73260=CARTESIAN_POINT('Ctrl Pts',(0.321594019388287,-7.90710331561421,
42.8706912004744));
#73261=CARTESIAN_POINT('Ctrl Pts',(0.525555155170245,-7.89352347047084,
42.878943003623));
#73262=CARTESIAN_POINT('Ctrl Pts',(0.719080167925258,-7.88063846816632,
42.8867725849962));
#73263=CARTESIAN_POINT('Ctrl Pts',(0.912368204998893,-7.86061641127412,
42.8946021663694));
#73264=CARTESIAN_POINT('Ctrl Pts',(1.10484707557039,-7.83346883185244,42.9024317477426));
#73265=CARTESIAN_POINT('Ctrl Pts',(1.29716368498403,-7.80634413804753,42.9102547287189));
#73266=CARTESIAN_POINT('Ctrl Pts',(1.48867213996247,-7.77210593107621,42.9180777096951));
#73267=CARTESIAN_POINT('Ctrl Pts',(1.6788026931358,-7.73081771338065,42.9259006906714));
#73268=CARTESIAN_POINT('Ctrl Pts',(1.86880650906592,-7.68955701758938,42.9337184570043));
#73269=CARTESIAN_POINT('Ctrl Pts',(2.05743390983847,-7.64125574449681,42.9415362233372));
#73270=CARTESIAN_POINT('Ctrl Pts',(2.24412254296994,-7.58602893562463,42.94935398967));
#73271=CARTESIAN_POINT('Ctrl Pts',(2.43072169798444,-7.53082859644576,42.9571680090205));
#73272=CARTESIAN_POINT('Ctrl Pts',(2.61538359950324,-7.46870943292098,42.964982028371));
#73273=CARTESIAN_POINT('Ctrl Pts',(2.79755815857188,-7.3998371164106,42.9727960477216));
#73274=CARTESIAN_POINT('Ctrl Pts',(2.97967965849695,-7.33098485926607,42.9806077912045));
#73275=CARTESIAN_POINT('Ctrl Pts',(3.15931493044627,-7.25538349241912,42.9884195346874));
#73276=CARTESIAN_POINT('Ctrl Pts',(3.33593090555019,-7.1732479389322,42.9962312781704));
#73277=CARTESIAN_POINT('Ctrl Pts',(3.51255675900827,-7.09110779150023,43.0040434585739));
#73278=CARTESIAN_POINT('Ctrl Pts',(3.68616265629164,-7.00243286991442,43.0118556389775));
#73279=CARTESIAN_POINT('Ctrl Pts',(3.85623690647469,-6.90748564393315,43.0196678193811));
#73280=CARTESIAN_POINT('Ctrl Pts',(3.98714218169645,-6.83440525266143,43.025680814439));
#73281=CARTESIAN_POINT('Ctrl Pts',(4.11595559747919,-6.75760994234814,43.0316938094968));
#73282=CARTESIAN_POINT('Ctrl Pts',(4.24245425707339,-6.67723766812593,43.0377068045546));
#73283=CARTESIAN_POINT('Ctrl Pts',(4.42421058285637,-6.56175684560724,43.0463464209123));
#73284=CARTESIAN_POINT('Ctrl Pts',(4.60110107446976,-6.43894548806574,43.0549860372701));
#73285=CARTESIAN_POINT('Ctrl Pts',(4.77257691221894,-6.30923375830653,43.0636256536278));
#73286=CARTESIAN_POINT('Ctrl Pts',(4.9443366844956,-6.17930724820753,43.0722795757059));
#73287=CARTESIAN_POINT('Ctrl Pts',(5.11066369807891,-6.04245766591505,43.0809334977841));
#73288=CARTESIAN_POINT('Ctrl Pts',(5.27104270752504,-5.89915500520601,43.0895874198622));
#73289=CARTESIAN_POINT('Ctrl Pts',(5.43611063166046,-5.75166268181521,43.0984943519975));
#73290=CARTESIAN_POINT('Ctrl Pts',(5.59487731685527,-5.59733445716044,43.1074012841328));
#73291=CARTESIAN_POINT('Ctrl Pts',(5.74682357947842,-5.43672141518681,43.1163082162681));
#73292=CARTESIAN_POINT('Ctrl Pts',(5.89494638410779,-5.28014991532575,43.1249910212661));
#73293=CARTESIAN_POINT('Ctrl Pts',(6.0365877411356,-5.11760625487598,43.133673826264));
#73294=CARTESIAN_POINT('Ctrl Pts',(6.17130825003054,-4.94963387364207,43.142356631262));
#73295=CARTESIAN_POINT('Ctrl Pts',(6.3112450206072,-4.77515774696507,43.151375626966));
#73296=CARTESIAN_POINT('Ctrl Pts',(6.44371419150937,-4.59482438808266,43.16039462267));
#73297=CARTESIAN_POINT('Ctrl Pts',(6.56827233633681,-4.40927652973962,43.169413618374));
#73298=CARTESIAN_POINT('Ctrl Pts',(6.69283048116424,-4.22372867139657,43.1784326140779));
#73299=CARTESIAN_POINT('Ctrl Pts',(6.80947747298286,-4.03296655902076,43.1874516097819));
#73300=CARTESIAN_POINT('Ctrl Pts',(6.91782181590263,-3.83766365428521,43.1964706054859));
#73301=CARTESIAN_POINT('Ctrl Pts',(7.01779401935553,-3.65745247573178,43.2047926724177));
#73302=CARTESIAN_POINT('Ctrl Pts',(7.11078183195034,-3.47322237723703,43.2131147393495));
#73303=CARTESIAN_POINT('Ctrl Pts',(7.1964719594793,-3.28553075414432,43.2214368062813));
#73304=CARTESIAN_POINT('Ctrl Pts',(7.28208606784707,-3.09800563984513,43.2297514903726));
#73305=CARTESIAN_POINT('Ctrl Pts',(7.36041528523218,-2.9070253920006,43.2380661744638));
#73306=CARTESIAN_POINT('Ctrl Pts',(7.43119251262743,-2.71317136212772,43.2463808585551));
#73307=CARTESIAN_POINT('Ctrl Pts',(7.5019112625629,-2.51947749805468,43.2546886728999));
#73308=CARTESIAN_POINT('Ctrl Pts',(7.56509037036864,-2.32291486264367,43.2629964872447));
#73309=CARTESIAN_POINT('Ctrl Pts',(7.62051076398834,-2.12408490789278,43.2713043015896));
#73310=CARTESIAN_POINT('Ctrl Pts',(7.6758754314067,-1.92545488023311,43.2796037622779));
#73311=CARTESIAN_POINT('Ctrl Pts',(7.72349687879767,-1.72456236487494,43.2879032229661));
#73312=CARTESIAN_POINT('Ctrl Pts',(7.76320568484589,-1.52202447246304,43.2962026836544));
#73313=CARTESIAN_POINT('Ctrl Pts',(7.80288919504733,-1.31961560350977,43.3044968573067));
#73314=CARTESIAN_POINT('Ctrl Pts',(7.83467006217641,-1.11556373440944,43.312791030959));
#73315=CARTESIAN_POINT('Ctrl Pts',(7.8584295011605,-0.910498091865268,43.3210852046113));
#73316=CARTESIAN_POINT('Ctrl Pts',(7.88217139453547,-0.705583883940912,
43.3293732532735));
#73317=CARTESIAN_POINT('Ctrl Pts',(7.89790364856776,-0.499657686565649,
43.3376613019357));
#73318=CARTESIAN_POINT('Ctrl Pts',(7.90555899679994,-0.29335635005154,43.3459493505979));
#73319=CARTESIAN_POINT('Ctrl Pts',(7.90841774512349,-0.216316928457862,
43.3490443692045));
#73320=CARTESIAN_POINT('Ctrl Pts',(7.91015067683777,-0.139225261458094,
43.3521393878111));
#73321=CARTESIAN_POINT('Ctrl Pts',(7.91075614355395,-0.0621147102014839,
43.3552344064177));
#73322=CARTESIAN_POINT('Ctrl Pts',(7.9123413244539,0.139769505344386,43.3633375180322));
#73323=CARTESIAN_POINT('Ctrl Pts',(7.9061938450066,0.341698587564988,43.3714406296467));
#73324=CARTESIAN_POINT('Ctrl Pts',(7.89233854919701,0.543059135692251,43.3795437412613));
#73325=CARTESIAN_POINT('Ctrl Pts',(7.87848019615452,0.744464114923822,43.3876486408636));
#73326=CARTESIAN_POINT('Ctrl Pts',(7.85691065662277,0.945299991786688,43.3957535404659));
#73327=CARTESIAN_POINT('Ctrl Pts',(7.82770671799616,1.14495787566083,43.4038584400682));
#73328=CARTESIAN_POINT('Ctrl Pts',(7.7984926778759,1.34468482018025,43.411966143114));
#73329=CARTESIAN_POINT('Ctrl Pts',(7.76163901810054,1.54323264372335,43.4200738461598));
#73330=CARTESIAN_POINT('Ctrl Pts',(7.71727386240876,1.74000147487945,43.4281815492056));
#73331=CARTESIAN_POINT('Ctrl Pts',(7.67286879729545,1.936947312745,43.436296545672));
#73332=CARTESIAN_POINT('Ctrl Pts',(7.62093880373944,2.13211064900299,43.4444115421383));
#73333=CARTESIAN_POINT('Ctrl Pts',(7.5616625759656,2.32490431786801,43.4525265386047));
#73334=CARTESIAN_POINT('Ctrl Pts',(7.50235740918861,2.51779210973645,43.4606454968601));
#73335=CARTESIAN_POINT('Ctrl Pts',(7.43569895437681,2.70830762408483,43.4687644551155));
#73336=CARTESIAN_POINT('Ctrl Pts',(7.3619148464566,2.89588169536014,43.4768834133708));
#73337=CARTESIAN_POINT('Ctrl Pts',(7.28805172311064,3.08365663977086,43.4850110662213));
#73338=CARTESIAN_POINT('Ctrl Pts',(7.20704782178509,3.26848355272822,43.4931387190718));
#73339=CARTESIAN_POINT('Ctrl Pts',(7.11917829022251,3.44981470111432,43.5012663719223));
#73340=CARTESIAN_POINT('Ctrl Pts',(7.07329622826837,3.54449879509452,43.5055103170645));
#73341=CARTESIAN_POINT('Ctrl Pts',(7.02554299595123,3.63823017154937,43.5097542622068));
#73342=CARTESIAN_POINT('Ctrl Pts',(6.97596260869761,3.73093375471247,43.513998207349));
#73343=CARTESIAN_POINT('Ctrl Pts',(6.88251635233599,3.90565612534637,43.5219969505561));
#73344=CARTESIAN_POINT('Ctrl Pts',(6.78241523949474,4.07702803553045,43.5299956937631));
#73345=CARTESIAN_POINT('Ctrl Pts',(6.67592567899843,4.244518503728,43.5379944369702));
#73346=CARTESIAN_POINT('Ctrl Pts',(6.56952285386751,4.41187255153944,43.5459866652296));
#73347=CARTESIAN_POINT('Ctrl Pts',(6.45674212935142,4.57535117686935,43.553978893489));
#73348=CARTESIAN_POINT('Ctrl Pts',(6.3378956964629,4.7344481347626,43.5619711217483));
#73349=CARTESIAN_POINT('Ctrl Pts',(6.21912593332849,4.89344245663771,43.5699581940921));
#73350=CARTESIAN_POINT('Ctrl Pts',(6.09429846048844,5.04806047787279,43.5779452664359));
#73351=CARTESIAN_POINT('Ctrl Pts',(5.96376885304586,5.19782474381736,43.5859323387797));
#73352=CARTESIAN_POINT('Ctrl Pts',(5.83330135281578,5.34751775051837,43.5939156107995));
#73353=CARTESIAN_POINT('Ctrl Pts',(5.69713734546972,5.49236135384377,43.6018988828193));
#73354=CARTESIAN_POINT('Ctrl Pts',(5.555673029076,5.63191070543537,43.6098821548391));
#73355=CARTESIAN_POINT('Ctrl Pts',(5.41425207984176,5.77141727691717,43.617862979515));
#73356=CARTESIAN_POINT('Ctrl Pts',(5.26753429878308,5.9056325977337,43.6258438041909));
#73357=CARTESIAN_POINT('Ctrl Pts',(5.11595340638602,6.03414797164333,43.6338246288668));
#73358=CARTESIAN_POINT('Ctrl Pts',(4.95949651042153,6.16679738521814,43.6420621780479));
#73359=CARTESIAN_POINT('Ctrl Pts',(4.79785868252293,6.29337377059787,43.6502997272289));
#73360=CARTESIAN_POINT('Ctrl Pts',(4.63155514665626,6.41347159684066,43.65853727641));
#73361=CARTESIAN_POINT('Ctrl Pts',(4.47041249070389,6.52984244003419,43.6665191906048));
#73362=CARTESIAN_POINT('Ctrl Pts',(4.30488966491796,6.64013060880149,43.6745011047995));
#73363=CARTESIAN_POINT('Ctrl Pts',(4.13548618829145,6.74401030444428,43.6824830189943));
#73364=CARTESIAN_POINT('Ctrl Pts',(3.96604504855562,6.84791309543559,43.6904667077908));
#73365=CARTESIAN_POINT('Ctrl Pts',(3.79272182307201,6.94540439762522,43.6984503965873));
#73366=CARTESIAN_POINT('Ctrl Pts',(3.61604241025721,7.03620340007459,43.7064340853838));
#73367=CARTESIAN_POINT('Ctrl Pts',(3.43929658853721,7.12703653135793,43.7144207750282));
#73368=CARTESIAN_POINT('Ctrl Pts',(3.25919236202255,7.2111721951554,43.7224074646725));
#73369=CARTESIAN_POINT('Ctrl Pts',(3.07627780477868,7.28837676494746,43.7303941543169));
#73370=CARTESIAN_POINT('Ctrl Pts',(2.8932664045596,7.36562221021905,43.7383850724644));
#73371=CARTESIAN_POINT('Ctrl Pts',(2.70744201509281,7.4359291156739,43.7463759906119));
#73372=CARTESIAN_POINT('Ctrl Pts',(2.51937049646888,7.49911283429728,43.7543669087594));
#73373=CARTESIAN_POINT('Ctrl Pts',(2.33107685659861,7.562371175843,43.7623672645545));
#73374=CARTESIAN_POINT('Ctrl Pts',(2.14053110304867,7.61848941838521,43.7703676203495));
#73375=CARTESIAN_POINT('Ctrl Pts',(1.94831321245926,7.66733308433621,43.7783679761445));
#73376=CARTESIAN_POINT('Ctrl Pts',(1.75596099349397,7.71621088389621,43.7863739228593));
#73377=CARTESIAN_POINT('Ctrl Pts',(1.56193463296585,7.75780389781041,43.7943798695741));
#73378=CARTESIAN_POINT('Ctrl Pts',(1.36682248332548,7.79202908741208,43.8023858162889));
#73379=CARTESIAN_POINT('Ctrl Pts',(1.17145718371103,7.82629868278693,43.8104021503896));
#73380=CARTESIAN_POINT('Ctrl Pts',(0.975003611245265,7.85318131420356,43.8184184844903));
#73381=CARTESIAN_POINT('Ctrl Pts',(0.778054559532989,7.87264581334572,43.8264348185911));
#73382=CARTESIAN_POINT('Ctrl Pts',(0.73636194532399,7.87676629956513,43.8281318154648));
#73383=CARTESIAN_POINT('Ctrl Pts',(0.694647124162059,7.88055453808428,43.8298288123385));
#73384=CARTESIAN_POINT('Ctrl Pts',(0.652915709971441,7.88401053244302,43.8315258092121));
#73385=CARTESIAN_POINT('Ctrl Pts',(0.462030253411381,7.89981874488519,43.8392881156017));
#73386=CARTESIAN_POINT('Ctrl Pts',(0.270232650410157,7.90871816315991,43.8470504219912));
#73387=CARTESIAN_POINT('Ctrl Pts',(0.0780762746324438,7.91061471033317,
43.8548127283807));
#73388=CARTESIAN_POINT('Ctrl Pts',(-0.113847326598659,7.91250896006557,
43.8625656316612));
#73389=CARTESIAN_POINT('Ctrl Pts',(-0.306128481512187,7.90741722029475,
43.8703185349417));
#73390=CARTESIAN_POINT('Ctrl Pts',(-0.49820617021761,7.89529680328467,43.8780714382222));
#73391=CARTESIAN_POINT('Ctrl Pts',(-0.690090140167289,7.88318861024562,
43.8858165223604));
#73392=CARTESIAN_POINT('Ctrl Pts',(-0.881770697586988,7.86406587377253,
43.8935616064987));
#73393=CARTESIAN_POINT('Ctrl Pts',(-1.07268417604572,7.83793784476894,43.9013066906369));
#73394=CARTESIAN_POINT('Ctrl Pts',(-1.26344377770638,7.81183087502986,43.9090455322156));
#73395=CARTESIAN_POINT('Ctrl Pts',(-1.45343717791831,7.7787299026399,43.9167843737943));
#73396=CARTESIAN_POINT('Ctrl Pts',(-1.642103096099,7.73869617065963,43.9245232153731));
#73397=CARTESIAN_POINT('Ctrl Pts',(-1.83065512200523,7.69868660591018,43.9322573852322));
#73398=CARTESIAN_POINT('Ctrl Pts',(-2.01788091174332,7.65175268949037,43.9399915550913));
#73399=CARTESIAN_POINT('Ctrl Pts',(-2.20322658576623,7.59800721319563,43.9477257249504));
#73400=CARTESIAN_POINT('Ctrl Pts',(-2.38849784653986,7.54428331482845,43.9554567896672));
#73401=CARTESIAN_POINT('Ctrl Pts',(-2.5718901508525,7.48375340309149,43.9631878543839));
#73402=CARTESIAN_POINT('Ctrl Pts',(-2.75286196847964,7.41658088221914,43.9709189191006));
#73403=CARTESIAN_POINT('Ctrl Pts',(-2.9338311581051,7.34940933679976,43.9786498715498));
#73404=CARTESIAN_POINT('Ctrl Pts',(-3.1123795908031,7.27559548889696,43.9863808239991));
#73405=CARTESIAN_POINT('Ctrl Pts',(-3.28798262899866,7.19535205750233,43.9941117764483));
#73406=CARTESIAN_POINT('Ctrl Pts',(-3.46359303313458,7.11510526017318,44.0018430531843));
#73407=CARTESIAN_POINT('Ctrl Pts',(-3.63625746961744,7.02842849068314,44.0095743299202));
#73408=CARTESIAN_POINT('Ctrl Pts',(-3.80547310961163,6.93558183658897,44.0173056066562));
#73409=CARTESIAN_POINT('Ctrl Pts',(-3.97472683290778,6.84271428662983,44.0250386233764));
#73410=CARTESIAN_POINT('Ctrl Pts',(-4.14052989917433,6.74367425952843,44.0327716400966));
#73411=CARTESIAN_POINT('Ctrl Pts',(-4.30240578570369,6.63876686253881,44.0405046568168));
#73412=CARTESIAN_POINT('Ctrl Pts',(-4.46434775407009,6.53381663969255,44.0482408303503));
#73413=CARTESIAN_POINT('Ctrl Pts',(-4.62235904934568,6.42299447252852,44.0559770038838));
#73414=CARTESIAN_POINT('Ctrl Pts',(-4.77599369422241,6.30664770165163,44.0637131774173));
#73415=CARTESIAN_POINT('Ctrl Pts',(-4.92980885450255,6.19016422733589,44.0714584406876));
#73416=CARTESIAN_POINT('Ctrl Pts',(-5.07923680822337,6.06814340245827,44.079203703958));
#73417=CARTESIAN_POINT('Ctrl Pts',(-5.2238653520194,5.94097229281295,44.0869489672283));
#73418=CARTESIAN_POINT('Ctrl Pts',(-5.36858671047325,5.81371957173246,44.0946992009832));
#73419=CARTESIAN_POINT('Ctrl Pts',(-5.50850226408887,5.68131022788748,44.1024494347382));
#73420=CARTESIAN_POINT('Ctrl Pts',(-5.64323812714229,5.54416670387603,44.1101996684932));
#73421=CARTESIAN_POINT('Ctrl Pts',(-5.77817690296244,5.4068166411505,44.1179615741323));
#73422=CARTESIAN_POINT('Ctrl Pts',(-5.90792016806836,5.26471842297204,44.1257234797713));
#73423=CARTESIAN_POINT('Ctrl Pts',(-6.03213487910658,5.11832685555211,44.1334853854103));
#73424=CARTESIAN_POINT('Ctrl Pts',(-6.11518054251764,5.02045451231224,44.1386747272986));
#73425=CARTESIAN_POINT('Ctrl Pts',(-6.1957559387252,4.92066375303239,44.1438640691869));
#73426=CARTESIAN_POINT('Ctrl Pts',(-6.27377276627098,4.81909703961195,44.1490534110751));
#73427=CARTESIAN_POINT('Ctrl Pts',(-6.39474680077887,4.66160620743258,44.157100080549));
#73428=CARTESIAN_POINT('Ctrl Pts',(-6.50994226304667,4.49935561946676,44.165146750023));
#73429=CARTESIAN_POINT('Ctrl Pts',(-6.61897066961584,4.33279912698076,44.1731934194969));
#73430=CARTESIAN_POINT('Ctrl Pts',(-6.72781079660562,4.16653025849421,44.1812261932936));
#73431=CARTESIAN_POINT('Ctrl Pts',(-6.83050492667977,3.9959705883102,44.1892589670903));
#73432=CARTESIAN_POINT('Ctrl Pts',(-6.9267053946297,3.82160612517929,44.197291740887));
#73433=CARTESIAN_POINT('Ctrl Pts',(-7.02280644779102,3.64742185250496,44.205316213513));
#73434=CARTESIAN_POINT('Ctrl Pts',(-7.11242705224154,3.46944090855861,44.2133406861389));
#73435=CARTESIAN_POINT('Ctrl Pts',(-7.19526256081308,3.28817847462111,44.2213651587649));
#73436=CARTESIAN_POINT('Ctrl Pts',(-7.278024651545,3.10707669517265,44.2293825192302));
#73437=CARTESIAN_POINT('Ctrl Pts',(-7.3540134943608,2.92269952047661,44.2373998796956));
#73438=CARTESIAN_POINT('Ctrl Pts',(-7.42296995277387,2.73558733734024,44.2454172401609));
#73439=CARTESIAN_POINT('Ctrl Pts',(-7.49187543070865,2.54861348886911,44.253428673279));
#73440=CARTESIAN_POINT('Ctrl Pts',(-7.55375877312745,2.35890897085495,44.2614401063971));
#73441=CARTESIAN_POINT('Ctrl Pts',(-7.60840847115289,2.16703519493545,44.2694515395153));
#73442=CARTESIAN_POINT('Ctrl Pts',(-7.66302119601303,1.97529123091046,44.2774575525112));
#73443=CARTESIAN_POINT('Ctrl Pts',(-7.710409946119,1.78138125261382,44.2854635655071));
#73444=CARTESIAN_POINT('Ctrl Pts',(-7.75041260210287,1.58588319152611,44.2934695785031));
#73445=CARTESIAN_POINT('Ctrl Pts',(-7.79039910156847,1.39046408939542,44.3014723579813));
#73446=CARTESIAN_POINT('Ctrl Pts',(-7.82300538715269,1.19345850598231,44.3094751374596));
#73447=CARTESIAN_POINT('Ctrl Pts',(-7.84811997459449,0.995456610993642,
44.3174779169379));
#73448=CARTESIAN_POINT('Ctrl Pts',(-7.87322921456482,0.797496875148093,
44.3254789924409));
#73449=CARTESIAN_POINT('Ctrl Pts',(-7.890849893012,0.598541577754206,44.3334800679439));
#73450=CARTESIAN_POINT('Ctrl Pts',(-7.90092206350628,0.399188610057576,
44.3414811434469));
#73451=CARTESIAN_POINT('Ctrl Pts',(-7.90771455584179,0.264748520316231,
44.346876926219));
#73452=CARTESIAN_POINT('Ctrl Pts',(-7.91107512021797,0.130127737187862,
44.352272708991));
#73453=CARTESIAN_POINT('Ctrl Pts',(-7.91099872614571,-0.004489423238615,
44.3576684917631));
#73454=CARTESIAN_POINT('',(-7.911,-3.90243393155743E-13,48.357668491763));
#73455=CARTESIAN_POINT('Ctrl Pts',(-7.91099884597975,-0.00427304422863289,
44.3652531274272));
#73456=CARTESIAN_POINT('Ctrl Pts',(-7.91057750947961,-0.784324077631529,
44.3937615432355));
#73457=CARTESIAN_POINT('Ctrl Pts',(-7.79479648296751,-1.55994847174528,
44.4188079269021));
#73458=CARTESIAN_POINT('Ctrl Pts',(-7.53183115076875,-2.42288181788949,
44.4521374585171));
#73459=CARTESIAN_POINT('Ctrl Pts',(-7.49353088856122,-2.53886381240998,
44.4567476485824));
#73460=CARTESIAN_POINT('Ctrl Pts',(-7.42801957037524,-2.72282917360768,
44.4643344212046));
#73461=CARTESIAN_POINT('Ctrl Pts',(-7.40252214680675,-2.79140444063471,
44.4672246802999));
#73462=CARTESIAN_POINT('Ctrl Pts',(-7.37101319255404,-2.87267851311738,
44.4707176672332));
#73463=CARTESIAN_POINT('Ctrl Pts',(-7.36591370256768,-2.88572913620001,
44.4712806453262));
#73464=CARTESIAN_POINT('Ctrl Pts',(-7.35799548059657,-2.90583572118567,
44.4721511683454));
#73465=CARTESIAN_POINT('Ctrl Pts',(-7.35520119375882,-2.91290132510785,
44.4724576806694));
#73466=CARTESIAN_POINT('Ctrl Pts',(-7.35028727784135,-2.92527444794868,
44.4729954858059));
#73467=CARTESIAN_POINT('Ctrl Pts',(-7.34817206561477,-2.93058372283022,
44.4732265951265));
#73468=CARTESIAN_POINT('Ctrl Pts',(-7.34371418790866,-2.9417380200731,44.4737128406693));
#73469=CARTESIAN_POINT('Ctrl Pts',(-7.34137029384775,-2.94758254519611,
44.4739680271478));
#73470=CARTESIAN_POINT('Ctrl Pts',(-7.3348060491135,-2.9638941602868,44.4746813626376));
#73471=CARTESIAN_POINT('Ctrl Pts',(-7.33057028327148,-2.9743550043453,44.475140134089));
#73472=CARTESIAN_POINT('Ctrl Pts',(-7.31340104920725,-3.01649748804308,
44.4769935023396));
#73473=CARTESIAN_POINT('Ctrl Pts',(-7.30028456869861,-3.04810386544434,
44.4783952928077));
#73474=CARTESIAN_POINT('Ctrl Pts',(-6.97504697922301,-3.81767657319244,
44.5128016805283));
#73475=CARTESIAN_POINT('Ctrl Pts',(-6.55281067395682,-4.50407920316199,
44.5491531708751));
#73476=CARTESIAN_POINT('Ctrl Pts',(-5.83385442278534,-5.35224280756966,
44.596624521268));
#73477=CARTESIAN_POINT('Ctrl Pts',(-5.61926957148779,-5.577112696885,44.6095917821584));
#73478=CARTESIAN_POINT('Ctrl Pts',(-5.3454394939657,-5.83217354700291,44.6248317119176));
#73479=CARTESIAN_POINT('Ctrl Pts',(-5.29834588890316,-5.87498958483114,
44.6274102680671));
#73480=CARTESIAN_POINT('Ctrl Pts',(-5.2338860360916,-5.93218894794574,44.6308843197901));
#73481=CARTESIAN_POINT('Ctrl Pts',(-5.21696775593485,-5.94707290963484,
44.6317910341077));
#73482=CARTESIAN_POINT('Ctrl Pts',(-5.18887266315499,-5.97157759312106,
44.6332883441317));
#73483=CARTESIAN_POINT('Ctrl Pts',(-5.17773215972628,-5.9812396832901,44.6338799008416));
#73484=CARTESIAN_POINT('Ctrl Pts',(-5.15615500485754,-5.99984795811422,
44.6350214557659));
#73485=CARTESIAN_POINT('Ctrl Pts',(-5.14572192689813,-6.00879819989468,
44.6355715481778));
#73486=CARTESIAN_POINT('Ctrl Pts',(-5.12133392988368,-6.02960987202533,
44.6368530556845));
#73487=CARTESIAN_POINT('Ctrl Pts',(-5.10736102775537,-6.04145013765289,
44.6375839667308));
#73488=CARTESIAN_POINT('Ctrl Pts',(-5.06345296196222,-6.07839546823662,
44.6398703999343));
#73489=CARTESIAN_POINT('Ctrl Pts',(-5.03337274525318,-6.1033274700671,44.6414217648199));
#73490=CARTESIAN_POINT('Ctrl Pts',(-4.69798878060645,-6.37714481812217,
44.6585542160999));
#73491=CARTESIAN_POINT('Ctrl Pts',(-4.37468245957252,-6.6031247201412,44.6735237484585));
#73492=CARTESIAN_POINT('Ctrl Pts',(-3.44505815631026,-7.15453450261184,
44.7135178874886));
#73493=CARTESIAN_POINT('Ctrl Pts',(-2.81119746222818,-7.42648994964344,
44.7373621636362));
#73494=CARTESIAN_POINT('Ctrl Pts',(-2.10147999290365,-7.62694394025388,
44.7663576576294));
#73495=CARTESIAN_POINT('Ctrl Pts',(-2.05255302192354,-7.6402564069175,44.7683694233245));
#73496=CARTESIAN_POINT('Ctrl Pts',(-1.99245766300421,-7.65598875414102,
44.7708596372374));
#73497=CARTESIAN_POINT('Ctrl Pts',(-1.98140689082546,-7.65885618571279,
44.7713183499096));
#73498=CARTESIAN_POINT('Ctrl Pts',(-1.9640916811857,-7.66330911712793,44.772038391414));
#73499=CARTESIAN_POINT('Ctrl Pts',(-1.95783141404456,-7.6649108873217,44.7722989852096));
#73500=CARTESIAN_POINT('Ctrl Pts',(-1.94673904786902,-7.66773453646699,
44.7727612024936));
#73501=CARTESIAN_POINT('Ctrl Pts',(-1.94190773832127,-7.66895952381403,
44.7729626834628));
#73502=CARTESIAN_POINT('Ctrl Pts',(-1.93080147429702,-7.67176436929156,
44.7734262263224));
#73503=CARTESIAN_POINT('Ctrl Pts',(-1.92452573846798,-7.67334109450874,
44.7736884330451));
#73504=CARTESIAN_POINT('Ctrl Pts',(-1.90742808587944,-7.67761443959303,
44.7744035585324));
#73505=CARTESIAN_POINT('Ctrl Pts',(-1.89660241848049,-7.68029586995761,
44.7748571896351));
#73506=CARTESIAN_POINT('Ctrl Pts',(-1.84388756178559,-7.69323466295953,
44.7770703413092));
#73507=CARTESIAN_POINT('Ctrl Pts',(-1.80192284738801,-7.70317174381062,
44.7788454302143));
#73508=CARTESIAN_POINT('Ctrl Pts',(-0.988963526297145,-7.88867053920941,
44.8135040554103));
#73509=CARTESIAN_POINT('Ctrl Pts',(-0.196051153149005,-7.94800232516257,
44.8514891451777));
#73510=CARTESIAN_POINT('Ctrl Pts',(0.883121294802134,-7.86695484367695,
44.9004001482116));
#73511=CARTESIAN_POINT('Ctrl Pts',(1.17236899251804,-7.82907737292079,44.913281142439));
#73512=CARTESIAN_POINT('Ctrl Pts',(1.58524286892673,-7.75160982274104,44.9311997949603));
#73513=CARTESIAN_POINT('Ctrl Pts',(1.71100887160302,-7.72482364752583,44.9365960407663));
#73514=CARTESIAN_POINT('Ctrl Pts',(1.88169869122541,-7.68409601329739,44.9438352685631));
#73515=CARTESIAN_POINT('Ctrl Pts',(1.92723007394158,-7.67280299783028,44.9457580833418));
#73516=CARTESIAN_POINT('Ctrl Pts',(2.00433036105135,-7.65295043731689,44.9490003694468));
#73517=CARTESIAN_POINT('Ctrl Pts',(2.03595125761321,-7.64459894964962,44.9503261874252));
#73518=CARTESIAN_POINT('Ctrl Pts',(2.0794739064918,-7.63281485767463,44.9521457259189));
#73519=CARTESIAN_POINT('Ctrl Pts',(2.0914205325787,-7.6295500874534,44.9526446227682));
#73520=CARTESIAN_POINT('Ctrl Pts',(2.11068269853752,-7.62423748680386,44.9534481378551));
#73521=CARTESIAN_POINT('Ctrl Pts',(2.11800301975766,-7.62220715526593,44.9537532968507));
#73522=CARTESIAN_POINT('Ctrl Pts',(2.13325371764232,-7.61795362346454,44.9543886196733));
#73523=CARTESIAN_POINT('Ctrl Pts',(2.1411835719791,-7.61572857609072,44.9547187258455));
#73524=CARTESIAN_POINT('Ctrl Pts',(2.15949118577555,-7.61056076617832,44.9554802888589));
#73525=CARTESIAN_POINT('Ctrl Pts',(2.16986644029136,-7.6076091506837,44.9559114706419));
#73526=CARTESIAN_POINT('Ctrl Pts',(2.2030933487687,-7.5980830553634,44.9572910374755));
#73527=CARTESIAN_POINT('Ctrl Pts',(2.22592150374738,-7.59142673618077,44.9582368806852));
#73528=CARTESIAN_POINT('Ctrl Pts',(2.43203929044306,-7.53031646773791,44.9667596176839));
#73529=CARTESIAN_POINT('Ctrl Pts',(2.61333443357915,-7.46933531870476,44.9741294552133));
#73530=CARTESIAN_POINT('Ctrl Pts',(3.25443007485733,-7.22749024658638,44.9998800116175));
#73531=CARTESIAN_POINT('Ctrl Pts',(3.69928297843251,-7.01022631594068,45.0170936213973));
#73532=CARTESIAN_POINT('Ctrl Pts',(4.45682287358665,-6.54793486118525,45.0477478049317));
#73533=CARTESIAN_POINT('Ctrl Pts',(4.77690049979974,-6.31822108393,45.0612294004367));
#73534=CARTESIAN_POINT('Ctrl Pts',(5.18873190136544,-5.97341057495099,45.0808055496746));
#73535=CARTESIAN_POINT('Ctrl Pts',(5.2963792373924,-5.8781746008102,45.0861559128048));
#73536=CARTESIAN_POINT('Ctrl Pts',(5.47242929088031,-5.71365887831471,45.0954032313498));
#73537=CARTESIAN_POINT('Ctrl Pts',(5.54225199798967,-5.64595617263282,45.0992149271494));
#73538=CARTESIAN_POINT('Ctrl Pts',(5.62167455715504,-5.56605189793051,45.1037157614456));
#73539=CARTESIAN_POINT('Ctrl Pts',(5.63250809413296,-5.55508875917418,45.1043332594447));
#73540=CARTESIAN_POINT('Ctrl Pts',(5.64896399507179,-5.53833836851867,45.1052765837661));
#73541=CARTESIAN_POINT('Ctrl Pts',(5.65460969395091,-5.53257402212637,45.1056011867686));
#73542=CARTESIAN_POINT('Ctrl Pts',(5.66484192080888,-5.52209473652575,45.1061912372581));
#73543=CARTESIAN_POINT('Ctrl Pts',(5.66943141038547,-5.51738269014867,45.1064565331326));
#73544=CARTESIAN_POINT('Ctrl Pts',(5.67860965313612,-5.50793580960032,45.1069883539893));
#73545=CARTESIAN_POINT('Ctrl Pts',(5.68319837414563,-5.50320095173255,45.1072548801758));
#73546=CARTESIAN_POINT('Ctrl Pts',(5.69612969468175,-5.48982438513567,45.1080077609376));
#73547=CARTESIAN_POINT('Ctrl Pts',(5.70445852188799,-5.48116942344234,45.1084947882875));
#73548=CARTESIAN_POINT('Ctrl Pts',(5.73899546914147,-5.44511611822613,45.1105230116991));
#73549=CARTESIAN_POINT('Ctrl Pts',(5.76502594871138,-5.41754873463898,45.1120725337521));
#73550=CARTESIAN_POINT('Ctrl Pts',(6.15642395459617,-4.997026313365,45.1356768960343));
#73551=CARTESIAN_POINT('Ctrl Pts',(6.48107897072506,-4.56808906303766,45.1591835217404));
#73552=CARTESIAN_POINT('Ctrl Pts',(6.98709097378206,-3.73575908485551,45.2011100414992));
#73553=CARTESIAN_POINT('Ctrl Pts',(7.18297181307584,-3.3436927505341,45.2196238680416));
#73554=CARTESIAN_POINT('Ctrl Pts',(7.46803712816953,-2.63084878797105,45.2513904451755));
#73555=CARTESIAN_POINT('Ctrl Pts',(7.57132706747662,-2.31688522985853,45.2648523101606));
#73556=CARTESIAN_POINT('Ctrl Pts',(7.6703520681745,-1.93738620675107,45.2807381815993));
#73557=CARTESIAN_POINT('Ctrl Pts',(7.68530238979467,-1.87720361117908,45.2832444217188));
#73558=CARTESIAN_POINT('Ctrl Pts',(7.70688268338584,-1.78574955733624,45.2870333111725));
#73559=CARTESIAN_POINT('Ctrl Pts',(7.71403320866772,-1.75460361360804,45.2883202449156));
#73560=CARTESIAN_POINT('Ctrl Pts',(7.72613323009837,-1.70039485045857,45.2905542209848));
#73561=CARTESIAN_POINT('Ctrl Pts',(7.73116865279933,-1.67735166322344,45.2915019979227));
#73562=CARTESIAN_POINT('Ctrl Pts',(7.74225919391443,-1.62548787914591,45.2936310651142));
#73563=CARTESIAN_POINT('Ctrl Pts',(7.74825659186675,-1.59665527414665,45.294811826373));
#73564=CARTESIAN_POINT('Ctrl Pts',(7.76355875227602,-1.52097269661544,45.2979038414637));
#73565=CARTESIAN_POINT('Ctrl Pts',(7.77260047261892,-1.47407067904797,45.2998126457242));
#73566=CARTESIAN_POINT('Ctrl Pts',(7.81205309372857,-1.25895494761477,45.3085346807306));
#73567=CARTESIAN_POINT('Ctrl Pts',(7.83743199013671,-1.08986340055955,45.3152984140403));
#73568=CARTESIAN_POINT('Ctrl Pts',(7.85974497082825,-0.899314810687137,
45.3228382244148));
#73569=CARTESIAN_POINT('Ctrl Pts',(7.86209429946939,-0.878539335303452,
45.3236592123933));
#73570=CARTESIAN_POINT('Ctrl Pts',(7.8980939122556,-0.548475345758534,45.336686065598));
#73571=CARTESIAN_POINT('Ctrl Pts',(7.9135531057463,-0.237473332399331,45.3487219677521));
#73572=CARTESIAN_POINT('Ctrl Pts',(7.90786946442744,0.373143235492292,45.3723265695618));
#73573=CARTESIAN_POINT('Ctrl Pts',(7.88807395794214,0.672249371242181,45.3838788109277));
#73574=CARTESIAN_POINT('Ctrl Pts',(7.84361225533363,1.03231428757976,45.3981413553201));
#73575=CARTESIAN_POINT('Ctrl Pts',(7.83510323439984,1.095026572812,45.4006389706971));
#73576=CARTESIAN_POINT('Ctrl Pts',(7.81944606970038,1.20087261763275,45.4048829994601));
#73577=CARTESIAN_POINT('Ctrl Pts',(7.81269110979921,1.24406167817418,45.4066227908376));
#73578=CARTESIAN_POINT('Ctrl Pts',(7.80033762180236,1.31897365781012,45.4096564982795));
#73579=CARTESIAN_POINT('Ctrl Pts',(7.79490262952818,1.35072258445195,45.4109472478512));
#73580=CARTESIAN_POINT('Ctrl Pts',(7.78670360178222,1.39691959761215,45.4128333726759));
#73581=CARTESIAN_POINT('Ctrl Pts',(7.78409290620811,1.41139468954072,45.4134255046806));
#73582=CARTESIAN_POINT('Ctrl Pts',(7.7794425172241,1.43677352833108,45.4144657641333));
#73583=CARTESIAN_POINT('Ctrl Pts',(7.77742022784319,1.44768043750186,45.4149135075829));
#73584=CARTESIAN_POINT('Ctrl Pts',(7.77345019920226,1.46884375882291,45.4157836438063));
#73585=CARTESIAN_POINT('Ctrl Pts',(7.77150508436882,1.47910064233368,45.416205976267));
#73586=CARTESIAN_POINT('Ctrl Pts',(7.76680128790469,1.5036390277085,45.4172178744757));
#73587=CARTESIAN_POINT('Ctrl Pts',(7.76402352401531,1.51791675954302,45.4178078873223));
#73588=CARTESIAN_POINT('Ctrl Pts',(7.75290048785266,1.57425987593919,45.420141194224));
#73589=CARTESIAN_POINT('Ctrl Pts',(7.74425266900614,1.61626442066841,45.4218915821549));
#73590=CARTESIAN_POINT('Ctrl Pts',(7.65929371584855,2.0125865754362,45.4385018233856));
#73591=CARTESIAN_POINT('Ctrl Pts',(7.55906029910967,2.36133071088002,45.4538169325443));
#73592=CARTESIAN_POINT('Ctrl Pts',(7.26453991019311,3.17179284040225,45.4901861215191));
#73593=CARTESIAN_POINT('Ctrl Pts',(7.0496503362616,3.6244006673238,45.5110861423262));
#73594=CARTESIAN_POINT('Ctrl Pts',(6.76704340580693,4.09801247154669,45.5334693609034));
#73595=CARTESIAN_POINT('Ctrl Pts',(6.74017436181341,4.14205652975212,45.5355570637587));
#73596=CARTESIAN_POINT('Ctrl Pts',(6.69878983172536,4.20842542456828,45.5387130728685));
#73597=CARTESIAN_POINT('Ctrl Pts',(6.68458940652093,4.23094483972399,45.5397857150991));
#73598=CARTESIAN_POINT('Ctrl Pts',(6.65975522785723,4.26989041701387,45.5416440113488));
#73599=CARTESIAN_POINT('Ctrl Pts',(6.64917372136912,4.28634957673531,45.5424303772755));
#73600=CARTESIAN_POINT('Ctrl Pts',(6.62570375518043,4.32256023353696,45.5441627216013));
#73601=CARTESIAN_POINT('Ctrl Pts',(6.61278780674016,4.3422937085758,45.5451083141454));
#73602=CARTESIAN_POINT('Ctrl Pts',(6.57878727322889,4.39373748564403,45.5475775818405));
#73603=CARTESIAN_POINT('Ctrl Pts',(6.55756159746115,4.42535388337352,45.5490993212964));
#73604=CARTESIAN_POINT('Ctrl Pts',(6.4636745771138,4.56304315692436,45.555746131145));
#73605=CARTESIAN_POINT('Ctrl Pts',(6.3886612499516,4.66748968178442,45.5608392731761));
#73606=CARTESIAN_POINT('Ctrl Pts',(5.89334484955657,5.32282882894237,45.593217947759));
#73607=CARTESIAN_POINT('Ctrl Pts',(5.40471550970584,5.81834652425665,45.6197648905153));
#73608=CARTESIAN_POINT('Ctrl Pts',(4.73372894053072,6.34038168051431,45.6516398926002));
#73609=CARTESIAN_POINT('Ctrl Pts',(4.60681580363533,6.43318566309756,45.6575115695023));
#73610=CARTESIAN_POINT('Ctrl Pts',(4.15288586092148,6.7447924409901,45.6781147056187));
#73611=CARTESIAN_POINT('Ctrl Pts',(3.8124085891106,6.94292417236386,45.6928447036365));
#73612=CARTESIAN_POINT('Ctrl Pts',(3.43647536749856,7.1256694351127,45.7093541933063));
#73613=CARTESIAN_POINT('Ctrl Pts',(3.41426997914466,7.13633577871017,45.7103303581433));
#73614=CARTESIAN_POINT('Ctrl Pts',(3.36498957925658,7.15972492797071,45.7124995555516));
#73615=CARTESIAN_POINT('Ctrl Pts',(3.33789155321998,7.1723981949203,45.7136941989268));
#73616=CARTESIAN_POINT('Ctrl Pts',(3.30052813416966,7.18961480375685,45.715344631879));
#73617=CARTESIAN_POINT('Ctrl Pts',(3.29032381844827,7.19429052507522,45.7157957111405));
#73618=CARTESIAN_POINT('Ctrl Pts',(3.27314012295885,7.20212006241861,45.7165559111763));
#73619=CARTESIAN_POINT('Ctrl Pts',(3.26616603671938,7.20528549594923,45.7168646076689));
#73620=CARTESIAN_POINT('Ctrl Pts',(3.25240156021569,7.21150889562677,45.7174742128078));
#73621=CARTESIAN_POINT('Ctrl Pts',(3.24561142618429,7.21456741117494,45.7177751006302));
#73622=CARTESIAN_POINT('Ctrl Pts',(3.23069329217432,7.22126174124115,45.718436538354));
#73623=CARTESIAN_POINT('Ctrl Pts',(3.22256345801688,7.22489342772004,45.7187972434623));
#73624=CARTESIAN_POINT('Ctrl Pts',(3.19440447338191,7.23741537183106,45.7200475003356));
#73625=CARTESIAN_POINT('Ctrl Pts',(3.1743446289126,7.24623608290017,45.7209397241607));
#73626=CARTESIAN_POINT('Ctrl Pts',(2.85145635442445,7.38661838651852,45.7353295759499));
#73627=CARTESIAN_POINT('Ctrl Pts',(2.54078839503323,7.49914966629145,45.749751145816));
#73628=CARTESIAN_POINT('Ctrl Pts',(1.83646731017107,7.70548013005092,45.7828292425046));
#73629=CARTESIAN_POINT('Ctrl Pts',(1.44075626866214,7.78917594725617,45.8015590765929));
#73630=CARTESIAN_POINT('Ctrl Pts',(0.661277233459787,7.89258413837518,45.8372279830831));
#73631=CARTESIAN_POINT('Ctrl Pts',(0.27899783434158,7.91532548204458,45.8541608908882));
#73632=CARTESIAN_POINT('Ctrl Pts',(-0.250561852634493,7.90839955156583,
45.8764804014484));
#73633=CARTESIAN_POINT('Ctrl Pts',(-0.397589486122487,7.90237244826539,
45.882560146985));
#73634=CARTESIAN_POINT('Ctrl Pts',(-0.563898923852589,7.8909012310378,45.8893062956878));
#73635=CARTESIAN_POINT('Ctrl Pts',(-0.58342391381474,7.88948165459394,45.890096268826));
#73636=CARTESIAN_POINT('Ctrl Pts',(-0.612761029765393,7.88723917901339,
45.8912802014249));
#73637=CARTESIAN_POINT('Ctrl Pts',(-0.622577148427273,7.88647041722237,
45.8916758310846));
#73638=CARTESIAN_POINT('Ctrl Pts',(-0.63946283684016,7.88511627060822,45.8923555181667));
#73639=CARTESIAN_POINT('Ctrl Pts',(-0.646533089669887,7.88453970026072,
45.8926398477572));
#73640=CARTESIAN_POINT('Ctrl Pts',(-0.661097442567303,7.88333227326004,
45.893225009828));
#73641=CARTESIAN_POINT('Ctrl Pts',(-0.668591438132273,7.88270023839644,
45.8935258054852));
#73642=CARTESIAN_POINT('Ctrl Pts',(-0.686638362266085,7.88115226107306,
45.8942494673423));
#73643=CARTESIAN_POINT('Ctrl Pts',(-0.697190388314609,7.88022580681204,
45.8946720074581));
#73644=CARTESIAN_POINT('Ctrl Pts',(-0.729589935950491,7.8773155816449,45.8959676143639));
#73645=CARTESIAN_POINT('Ctrl Pts',(-0.751431175037266,7.87526211922154,
45.8968385180214));
#73646=CARTESIAN_POINT('Ctrl Pts',(-1.00371285999161,7.85048409935978,45.906869653386));
#73647=CARTESIAN_POINT('Ctrl Pts',(-1.23306591436498,7.81774257525262,45.9157102899084));
#73648=CARTESIAN_POINT('Ctrl Pts',(-2.02701538339099,7.66858548421364,45.9455900920633));
#73649=CARTESIAN_POINT('Ctrl Pts',(-2.58006572148429,7.50061868870378,45.9649768172851));
#73650=CARTESIAN_POINT('Ctrl Pts',(-3.56439635706117,7.07977912513883,46.001501560628));
#73651=CARTESIAN_POINT('Ctrl Pts',(-3.99959071719895,6.84334441092453,46.0185549157974));
#73652=CARTESIAN_POINT('Ctrl Pts',(-4.44137047792762,6.54672378963197,46.0395304672268));
#73653=CARTESIAN_POINT('Ctrl Pts',(-4.4727557192844,6.52532146995297,46.0410421494628));
#73654=CARTESIAN_POINT('Ctrl Pts',(-4.51111378165321,6.49875746885079,46.0429176989488));
#73655=CARTESIAN_POINT('Ctrl Pts',(-4.51823430613906,6.49380897037111,46.0432670574857));
#73656=CARTESIAN_POINT('Ctrl Pts',(-4.52938388294148,6.48603321512082,46.0438159926314));
#73657=CARTESIAN_POINT('Ctrl Pts',(-4.53341847496644,6.48321387564279,46.0440150209249));
#73658=CARTESIAN_POINT('Ctrl Pts',(-4.54056547085831,6.47820968057944,46.0443682824281));
#73659=CARTESIAN_POINT('Ctrl Pts',(-4.54367893883055,6.47602634039058,46.0445224096522));
#73660=CARTESIAN_POINT('Ctrl Pts',(-4.55083677027424,6.47099916045976,46.0448772897093));
#73661=CARTESIAN_POINT('Ctrl Pts',(-4.55488004076056,6.4681537751059,46.0450781514588));
#73662=CARTESIAN_POINT('Ctrl Pts',(-4.56590065167555,6.46038274287609,46.0456267308406));
#73663=CARTESIAN_POINT('Ctrl Pts',(-4.57287268495985,6.45544958561868,46.0459749832781));
#73664=CARTESIAN_POINT('Ctrl Pts',(-4.60799657776681,6.43051174113837,46.0477355469237));
#73665=CARTESIAN_POINT('Ctrl Pts',(-4.63602478417644,6.4103344562795,46.0491602907247));
#73666=CARTESIAN_POINT('Ctrl Pts',(-5.14327904667264,6.04009932827313,46.0752923895468));
#73667=CARTESIAN_POINT('Ctrl Pts',(-5.58171917663632,5.63741612530685,46.1033933036455));
#73668=CARTESIAN_POINT('Ctrl Pts',(-6.20840849175219,4.91635825821291,46.1476676374561));
#73669=CARTESIAN_POINT('Ctrl Pts',(-6.42681954871182,4.62719583013448,46.1642000839799));
#73670=CARTESIAN_POINT('Ctrl Pts',(-6.77369285257917,4.09577036752642,46.1919244031957));
#73671=CARTESIAN_POINT('Ctrl Pts',(-6.91081830424044,3.8599042765408,46.203415992642));
#73672=CARTESIAN_POINT('Ctrl Pts',(-7.04483605475889,3.59925308193642,46.2152557640008));
#73673=CARTESIAN_POINT('Ctrl Pts',(-7.05410097209022,3.58106091410784,46.2160778201236));
#73674=CARTESIAN_POINT('Ctrl Pts',(-7.06758436963312,3.5543301579066,46.2172794507875));
#73675=CARTESIAN_POINT('Ctrl Pts',(-7.07185797943865,3.54581956856509,46.2176611010093));
#73676=CARTESIAN_POINT('Ctrl Pts',(-7.07935817207902,3.53081597376968,46.2183322975193));
#73677=CARTESIAN_POINT('Ctrl Pts',(-7.08259121121235,3.52432621992429,46.2186220863228));
#73678=CARTESIAN_POINT('Ctrl Pts',(-7.08887098723624,3.51167714146238,46.2191858703257));
#73679=CARTESIAN_POINT('Ctrl Pts',(-7.09191862882748,3.50551827579673,46.2194598993123));
#73680=CARTESIAN_POINT('Ctrl Pts',(-7.09920609513537,3.49074290641095,46.2201161615786));
#73681=CARTESIAN_POINT('Ctrl Pts',(-7.10343826802851,3.48212262752236,46.2204981079195));
#73682=CARTESIAN_POINT('Ctrl Pts',(-7.1186897027617,3.45091430748992,46.2218775272241));
#73683=CARTESIAN_POINT('Ctrl Pts',(-7.12961706281217,3.42828137634656,46.2228715625175));
#73684=CARTESIAN_POINT('Ctrl Pts',(-7.30077050251995,3.06942787741506,46.2385331585974));
#73685=CARTESIAN_POINT('Ctrl Pts',(-7.43717168480958,2.7223434963412,46.2522723926034));
#73686=CARTESIAN_POINT('Ctrl Pts',(-7.73140575364928,1.7839622617924,46.2869506279857));
#73687=CARTESIAN_POINT('Ctrl Pts',(-7.84603652606527,1.18185961229528,46.3066355853794));
#73688=CARTESIAN_POINT('Ctrl Pts',(-7.90421915415763,0.380111655674429,
46.3349357750042));
#73689=CARTESIAN_POINT('Ctrl Pts',(-7.91113876675237,0.187192613980867,
46.3419197391759));
#73690=CARTESIAN_POINT('Ctrl Pts',(-7.91092438517952,-0.106463557381466,
46.3530711663491));
#73691=CARTESIAN_POINT('Ctrl Pts',(-7.90892860487414,-0.207137165649146,
46.3569875209991));
#73692=CARTESIAN_POINT('Ctrl Pts',(-7.90455023138246,-0.319605406092795,
46.3614947600475));
#73693=CARTESIAN_POINT('Ctrl Pts',(-7.90406164692202,-0.33146863293588,
46.3619718310198));
#73694=CARTESIAN_POINT('Ctrl Pts',(-7.903315870304,-0.348636573166781,46.3626646663252));
#73695=CARTESIAN_POINT('Ctrl Pts',(-7.90308003975752,-0.353942214200977,
46.3628791204729));
#73696=CARTESIAN_POINT('Ctrl Pts',(-7.90265379610153,-0.363318851561732,
46.3632587238618));
#73697=CARTESIAN_POINT('Ctrl Pts',(-7.90246558160337,-0.367389902399768,
46.3634237353023));
#73698=CARTESIAN_POINT('Ctrl Pts',(-7.90206877279715,-0.375831417670163,
46.3637663046779));
#73699=CARTESIAN_POINT('Ctrl Pts',(-7.90185969834156,-0.380201857035287,
46.3639438918128));
#73700=CARTESIAN_POINT('Ctrl Pts',(-7.90131276192169,-0.39143953753321,
46.3644011029528));
#73701=CARTESIAN_POINT('Ctrl Pts',(-7.90096957356911,-0.398306502814553,
46.3646810486293));
#73702=CARTESIAN_POINT('Ctrl Pts',(-7.8995150231373,-0.426669317667521,
46.3658396015365));
#73703=CARTESIAN_POINT('Ctrl Pts',(-7.89832489483122,-0.44816084724729,
46.3667229023449));
#73704=CARTESIAN_POINT('Ctrl Pts',(-7.88967588585884,-0.593592682527613,
46.3727355835338));
#73705=CARTESIAN_POINT('Ctrl Pts',(-7.87938803540697,-0.717341601911624,
46.3780259846235));
#73706=CARTESIAN_POINT('Ctrl Pts',(-7.84691132147111,-1.0211842857287,46.3913575028096));
#73707=CARTESIAN_POINT('Ctrl Pts',(-7.82143086548019,-1.20085273511072,
46.3995374047983));
#73708=CARTESIAN_POINT('Ctrl Pts',(-7.6612078256242,-2.10561997644481,46.4417163598038));
#73709=CARTESIAN_POINT('Ctrl Pts',(-7.43167658263196,-2.81037363486596,
46.4773872271623));
#73710=CARTESIAN_POINT('Ctrl Pts',(-6.97980237278233,-3.73514862784424,
46.5226707617288));
#73711=CARTESIAN_POINT('Ctrl Pts',(-6.83736531071775,-3.98991693100337,
46.5350251519796));
#73712=CARTESIAN_POINT('Ctrl Pts',(-6.66801722831137,-4.25700253781224,
46.5478494028067));
#73713=CARTESIAN_POINT('Ctrl Pts',(-6.65476712248939,-4.27768616475423,
46.548841765082));
#73714=CARTESIAN_POINT('Ctrl Pts',(-6.63612817948381,-4.30648565231065,
46.5502225038351));
#73715=CARTESIAN_POINT('Ctrl Pts',(-6.63082043187822,-4.31465366966558,
46.5506139907741));
#73716=CARTESIAN_POINT('Ctrl Pts',(-6.62162097811,-4.32875351034982,46.5512895951182));
#73717=CARTESIAN_POINT('Ctrl Pts',(-6.61773635968813,-4.33468993183451,
46.5515739846543));
#73718=CARTESIAN_POINT('Ctrl Pts',(-6.60967281002296,-4.34697643553769,
46.5521624622581));
#73719=CARTESIAN_POINT('Ctrl Pts',(-6.60549269985154,-4.3533257377922,46.5524665045054));
#73720=CARTESIAN_POINT('Ctrl Pts',(-6.59569129499238,-4.36816678359865,
46.5531770325824));
#73721=CARTESIAN_POINT('Ctrl Pts',(-6.59006273620931,-4.37665372653862,
46.5535832378424));
#73722=CARTESIAN_POINT('Ctrl Pts',(-6.5718741641315,-4.40396447059652,46.5548900405642));
#73723=CARTESIAN_POINT('Ctrl Pts',(-6.55924971322905,-4.42274533498227,
46.5557881495011));
#73724=CARTESIAN_POINT('Ctrl Pts',(-6.23985431735601,-4.89352086183233,
46.5782885206768));
#73725=CARTESIAN_POINT('Ctrl Pts',(-5.88715043018444,-5.31261397174747,
46.5978875214552));
#73726=CARTESIAN_POINT('Ctrl Pts',(-5.01460293464638,-6.15481217275843,
46.64002241609));
#73727=CARTESIAN_POINT('Ctrl Pts',(-4.47861256683874,-6.55514695185946,
46.6621351255904));
#73728=CARTESIAN_POINT('Ctrl Pts',(-3.86363855933159,-6.90346673138071,
46.6900374956399));
#73729=CARTESIAN_POINT('Ctrl Pts',(-3.82830507630175,-6.92312328268339,
46.6916473563032));
#73730=CARTESIAN_POINT('Ctrl Pts',(-3.78223001818944,-6.94829495558331,
46.6937540451917));
#73731=CARTESIAN_POINT('Ctrl Pts',(-3.77162391796402,-6.95405778805381,
46.6942394950813));
#73732=CARTESIAN_POINT('Ctrl Pts',(-3.7546963419266,-6.96320528180495,46.6950150509662));
#73733=CARTESIAN_POINT('Ctrl Pts',(-3.74838335621728,-6.96660567500622,
46.6953044570555));
#73734=CARTESIAN_POINT('Ctrl Pts',(-3.73702796834733,-6.97270217768246,
46.6958253168329));
#73735=CARTESIAN_POINT('Ctrl Pts',(-3.73198724462923,-6.9754014150143,46.6960566338297));
#73736=CARTESIAN_POINT('Ctrl Pts',(-3.72018781633386,-6.9817033932352,46.6965983428048));
#73737=CARTESIAN_POINT('Ctrl Pts',(-3.71342680422943,-6.9853017851065,46.6969089212829));
#73738=CARTESIAN_POINT('Ctrl Pts',(-3.6940314743821,-6.99558838301792,46.6978003811812));
#73739=CARTESIAN_POINT('Ctrl Pts',(-3.6813842748136,-7.00225215028686,46.698382289962));
#73740=CARTESIAN_POINT('Ctrl Pts',(-3.59897187279327,-7.0453899823371,46.7021778521312));
#73741=CARTESIAN_POINT('Ctrl Pts',(-3.52868488557851,-7.08085454087484,
46.7054321355445));
#73742=CARTESIAN_POINT('Ctrl Pts',(-3.3032605967931,-7.19040642882663,46.7159019766271));
#73743=CARTESIAN_POINT('Ctrl Pts',(-3.1462353220185,-7.26048724336464,46.723242912383));
#73744=CARTESIAN_POINT('Ctrl Pts',(-2.32255867367755,-7.5963557129978,46.7616679288116));
#73745=CARTESIAN_POINT('Ctrl Pts',(-1.6241903381002,-7.7756709199758,46.793615582705));
#73746=CARTESIAN_POINT('Ctrl Pts',(-0.702815268075138,-7.88251210639145,
46.8324399858931));
#73747=CARTESIAN_POINT('Ctrl Pts',(-0.493505512333553,-7.89837981503203,
46.8410747500611));
#73748=CARTESIAN_POINT('Ctrl Pts',(-0.247386413338868,-7.90721500187279,
46.851043259848));
#73749=CARTESIAN_POINT('Ctrl Pts',(-0.210957581140514,-7.9082707369982,
46.8525141179042));
#73750=CARTESIAN_POINT('Ctrl Pts',(-0.156706664247727,-7.9094678446292,
46.8546977621108));
#73751=CARTESIAN_POINT('Ctrl Pts',(-0.138889360984439,-7.90980077576333,
46.8554138248434));
#73752=CARTESIAN_POINT('Ctrl Pts',(-0.10716935936502,-7.9102862799317,46.8566866631407));
#73753=CARTESIAN_POINT('Ctrl Pts',(-0.0932671139113457,-7.91046241056601,
46.8572438519116));
#73754=CARTESIAN_POINT('Ctrl Pts',(-0.0642250363596227,-7.91075378011629,
46.8584064273096));
#73755=CARTESIAN_POINT('Ctrl Pts',(-0.0490851869109706,-7.910862207828,
46.8590116897727));
#73756=CARTESIAN_POINT('Ctrl Pts',(-0.00962913148823917,-7.91103151026808,
46.8605869917113));
#73757=CARTESIAN_POINT('Ctrl Pts',(0.014687256625856,-7.91102373710685,
46.8615557796971));
#73758=CARTESIAN_POINT('Ctrl Pts',(0.12078563549058,-7.91050063791418,46.8657738980452));
#73759=CARTESIAN_POINT('Ctrl Pts',(0.202557662009064,-7.90882925680557,
46.8690016229055));
#73760=CARTESIAN_POINT('Ctrl Pts',(1.02789316519733,-7.87915079458822,46.9013535511242));
#73761=CARTESIAN_POINT('Ctrl Pts',(1.76395562425671,-7.74764565391003,46.9278208788122));
#73762=CARTESIAN_POINT('Ctrl Pts',(2.77509716481213,-7.41521161927144,46.966919054679));
#73763=CARTESIAN_POINT('Ctrl Pts',(3.07302029087386,-7.2967833073106,46.9788925905246));
#73764=CARTESIAN_POINT('Ctrl Pts',(3.37977385048252,-7.15271950803795,46.9924138521336));
#73765=CARTESIAN_POINT('Ctrl Pts',(3.39659809380275,-7.14474555333893,46.9931593940501));
#73766=CARTESIAN_POINT('Ctrl Pts',(3.4199721298164,-7.13356606494813,46.9942008910661));
#73767=CARTESIAN_POINT('Ctrl Pts',(3.42654596181638,-7.13041071347065,46.99449443747));
#73768=CARTESIAN_POINT('Ctrl Pts',(3.43787121282645,-7.12495546579697,46.9950012553116));
#73769=CARTESIAN_POINT('Ctrl Pts',(3.44262471629478,-7.12265989136816,46.9952143154177));
#73770=CARTESIAN_POINT('Ctrl Pts',(3.45244036299211,-7.11790757181787,46.9956549695163));
#73771=CARTESIAN_POINT('Ctrl Pts',(3.45750218832127,-7.1154501810116,46.9958825954204));
#73772=CARTESIAN_POINT('Ctrl Pts',(3.46929634496883,-7.10970885335086,46.9964138763236));
#73773=CARTESIAN_POINT('Ctrl Pts',(3.47602663471061,-7.10642075469948,46.9967177402365));
#73774=CARTESIAN_POINT('Ctrl Pts',(3.49752594478716,-7.09587936764046,46.9976906455691));
#73775=CARTESIAN_POINT('Ctrl Pts',(3.51227694035261,-7.08858959331064,46.9983615526408));
#73776=CARTESIAN_POINT('Ctrl Pts',(3.83554121031371,-6.92757931004217,47.0131408729135));
#73777=CARTESIAN_POINT('Ctrl Pts',(4.13365837205501,-6.75392689746058,47.0283708399069));
#73778=CARTESIAN_POINT('Ctrl Pts',(4.83901013679456,-6.2788359956522,47.0669723848399));
#73779=CARTESIAN_POINT('Ctrl Pts',(5.23049572949256,-5.9566557253507,47.0906647980545));
#73780=CARTESIAN_POINT('Ctrl Pts',(5.90369255078832,-5.28475035041649,47.1334869520434));
#73781=CARTESIAN_POINT('Ctrl Pts',(6.19174528422648,-4.94414211618902,47.152753477639));
#73782=CARTESIAN_POINT('Ctrl Pts',(6.46657121053869,-4.55721773111413,47.1720587530345));
#73783=CARTESIAN_POINT('Ctrl Pts',(6.48337793949777,-4.53327554716637,47.17324379352));
#73784=CARTESIAN_POINT('Ctrl Pts',(6.50631974554313,-4.50020502852142,47.1748676716268));
#73785=CARTESIAN_POINT('Ctrl Pts',(6.51256905884362,-4.49115644182875,47.1753106612022));
#73786=CARTESIAN_POINT('Ctrl Pts',(6.52322516635678,-4.47565810211321,47.1760671492342));
#73787=CARTESIAN_POINT('Ctrl Pts',(6.52764130411679,-4.4692148105917,47.1763809861977));
#73788=CARTESIAN_POINT('Ctrl Pts',(6.53620623093292,-4.45667852143004,47.1769903080739));
#73789=CARTESIAN_POINT('Ctrl Pts',(6.54035606104994,-4.45058624584818,47.1772858305007));
#73790=CARTESIAN_POINT('Ctrl Pts',(6.55024855768903,-4.43601957003588,47.1779910208877));
#73791=CARTESIAN_POINT('Ctrl Pts',(6.55598330846205,-4.42753979692753,47.1784004029431));
#73792=CARTESIAN_POINT('Ctrl Pts',(6.5730822646045,-4.40215011456622,47.1796227775327));
#73793=CARTESIAN_POINT('Ctrl Pts',(6.58439766010758,-4.38520735537097,47.1804340135589));
#73794=CARTESIAN_POINT('Ctrl Pts',(6.68074219307624,-4.23973518679015,47.1873614975962));
#73795=CARTESIAN_POINT('Ctrl Pts',(6.76206667753845,-4.10878668738035,47.1933441548213));
#73796=CARTESIAN_POINT('Ctrl Pts',(6.95812338321501,-3.7714909698889,47.2081757774451));
#73797=CARTESIAN_POINT('Ctrl Pts',(7.06754294893992,-3.56222828415014,47.2168483091004));
#73798=CARTESIAN_POINT('Ctrl Pts',(7.3887225562299,-2.8747199788652,47.2440626368951));
#73799=CARTESIAN_POINT('Ctrl Pts',(7.56249729312747,-2.38030747265492,47.261659105346));
#73800=CARTESIAN_POINT('Ctrl Pts',(7.69743994340137,-1.82635766556305,47.2816347844914));
#73801=CARTESIAN_POINT('Ctrl Pts',(7.70823568311301,-1.78024341356534,47.2833002460176));
#73802=CARTESIAN_POINT('Ctrl Pts',(7.79617768542062,-1.38879197135364,47.2974759940629));
#73803=CARTESIAN_POINT('Ctrl Pts',(7.85048845373822,-1.03873342964161,47.3104247563517));
#73804=CARTESIAN_POINT('Ctrl Pts',(7.8830933049805,-0.664263670995458,47.3253806609481));
#73805=CARTESIAN_POINT('Ctrl Pts',(7.88491244522759,-0.642309892595684,
47.3262608425196));
#73806=CARTESIAN_POINT('Ctrl Pts',(7.88731710943287,-0.611738839610352,
47.3274909575115));
#73807=CARTESIAN_POINT('Ctrl Pts',(7.88798026308885,-0.603127649032909,
47.327837944498));
#73808=CARTESIAN_POINT('Ctrl Pts',(7.88909958375092,-0.588275375029725,
47.3284372433099));
#73809=CARTESIAN_POINT('Ctrl Pts',(7.88956245031833,-0.582034794041768,
47.3286893068093));
#73810=CARTESIAN_POINT('Ctrl Pts',(7.89050378939273,-0.569135760228505,
47.329210824724));
#73811=CARTESIAN_POINT('Ctrl Pts',(7.89098123927813,-0.56247723954678,47.3294803161161));
#73812=CARTESIAN_POINT('Ctrl Pts',(7.8920748739508,-0.546949923917408,47.3301094025728));
#73813=CARTESIAN_POINT('Ctrl Pts',(7.89268453752551,-0.538080686947398,
47.3304692301211));
#73814=CARTESIAN_POINT('Ctrl Pts',(7.89458736286652,-0.509699668737082,
47.3316221943042));
#73815=CARTESIAN_POINT('Ctrl Pts',(7.89582312584518,-0.490184189690269,
47.3324173256791));
#73816=CARTESIAN_POINT('Ctrl Pts',(7.89854535821062,-0.444509541536959,
47.3342834398075));
#73817=CARTESIAN_POINT('Ctrl Pts',(7.89997424569107,-0.418347233825442,
47.335356305222));
#73818=CARTESIAN_POINT('Ctrl Pts',(7.91471886997849,-0.121285286756925,
47.3475800447112));
#73819=CARTESIAN_POINT('Ctrl Pts',(7.91422397503901,0.150111827592864,47.3591335755547));
#73820=CARTESIAN_POINT('Ctrl Pts',(7.88213717775007,0.752292176635892,47.3850676212605));
#73821=CARTESIAN_POINT('Ctrl Pts',(7.84364992909478,1.08221534899094,47.3994689213465));
#73822=CARTESIAN_POINT('Ctrl Pts',(7.66817541820994,2.0518669186074,47.4417041897312));
#73823=CARTESIAN_POINT('Ctrl Pts',(7.47254266879963,2.67810316934097,47.4686537370505));
#73824=CARTESIAN_POINT('Ctrl Pts',(7.16405182416864,3.35689511887418,47.498944179107));
#73825=CARTESIAN_POINT('Ctrl Pts',(7.12453275336198,3.43997334261176,47.5026707887918));
#73826=CARTESIAN_POINT('Ctrl Pts',(7.06822609170747,3.5532082792783,47.5077765432924));
#73827=CARTESIAN_POINT('Ctrl Pts',(7.05267699734957,3.58397214563691,47.5091664147418));
#73828=CARTESIAN_POINT('Ctrl Pts',(7.02557433002293,3.63673530995529,47.5115549395013));
#73829=CARTESIAN_POINT('Ctrl Pts',(7.01411727383044,3.65878357576404,47.5125544784606));
#73830=CARTESIAN_POINT('Ctrl Pts',(6.99044221932511,3.70382457746943,47.5145993608149));
#73831=CARTESIAN_POINT('Ctrl Pts',(6.9782141969543,3.72681171358358,47.5156445933324));
#73832=CARTESIAN_POINT('Ctrl Pts',(6.94949517145449,3.7801629279324,47.5180742917522));
#73833=CARTESIAN_POINT('Ctrl Pts',(6.93291825824692,3.81048019748771,47.5194578717833));
#73834=CARTESIAN_POINT('Ctrl Pts',(6.89756756062527,3.87413819055065,47.5223692646396));
#73835=CARTESIAN_POINT('Ctrl Pts',(6.87874942628791,3.9074533034501,47.5238965792312));
#73836=CARTESIAN_POINT('Ctrl Pts',(6.82755822776219,3.99656486880716,47.5279920448011));
#73837=CARTESIAN_POINT('Ctrl Pts',(6.79474309315436,4.05210420349975,47.5305553842411));
#73838=CARTESIAN_POINT('Ctrl Pts',(6.69082123317496,4.22317834401804,47.5384874015076));
#73839=CARTESIAN_POINT('Ctrl Pts',(6.61741907635322,4.33729057192499,47.543830172373));
#73840=CARTESIAN_POINT('Ctrl Pts',(6.26220495168031,4.85948826144215,47.5685771929264));
#73841=CARTESIAN_POINT('Ctrl Pts',(5.9453583587887,5.24237996327339,47.5875294426775));
#73842=CARTESIAN_POINT('Ctrl Pts',(5.4454286461338,5.74245946195894,47.6150533307147));
#73843=CARTESIAN_POINT('Ctrl Pts',(5.29017838496186,5.88579158358921,47.6233372769485));
#73844=CARTESIAN_POINT('Ctrl Pts',(5.10810818817175,6.04085529265605,47.6329036302303));
#73845=CARTESIAN_POINT('Ctrl Pts',(5.08673748745857,6.05886158030195,47.6340242980488));
#73846=CARTESIAN_POINT('Ctrl Pts',(5.05446190479015,6.08576485758631,47.6357139857829));
#73847=CARTESIAN_POINT('Ctrl Pts',(5.04362788725564,6.09474665444711,47.636280692567));
#73848=CARTESIAN_POINT('Ctrl Pts',(5.02427938807021,6.11070034718542,47.637292001997));
#73849=CARTESIAN_POINT('Ctrl Pts',(5.01577420716808,6.11768348349997,47.6377362868188));
#73850=CARTESIAN_POINT('Ctrl Pts',(4.99936388303139,6.13109987218547,47.6385930393878));
#73851=CARTESIAN_POINT('Ctrl Pts',(4.99146082162064,6.1375356408873,47.6390054333093));
#73852=CARTESIAN_POINT('Ctrl Pts',(4.96960210718145,6.15526589367509,47.6401455166792));
#73853=CARTESIAN_POINT('Ctrl Pts',(4.95562051187254,6.16652808829732,47.6408741682749));
#73854=CARTESIAN_POINT('Ctrl Pts',(4.89133036672143,6.21795402887717,47.6442220235838));
#73855=CARTESIAN_POINT('Ctrl Pts',(4.84057161149337,6.25754994917423,47.6468576381398));
#73856=CARTESIAN_POINT('Ctrl Pts',(4.69742718465366,6.36643018168268,47.6542613891907));
#73857=CARTESIAN_POINT('Ctrl Pts',(4.60400004349902,6.43431723861928,47.6590605041097));
#73858=CARTESIAN_POINT('Ctrl Pts',(3.94959539979625,6.88827560978451,47.692350318289));
#73859=CARTESIAN_POINT('Ctrl Pts',(3.34224324798903,7.20257910155029,47.7213488155023));
#73860=CARTESIAN_POINT('Ctrl Pts',(2.62952386514692,7.46160162406339,47.7522653285838));
#73861=CARTESIAN_POINT('Ctrl Pts',(2.5565000757106,7.48693542689993,47.7554025908963));
#73862=CARTESIAN_POINT('Ctrl Pts',(2.45557636649406,7.52029966452929,47.7596988390509));
#73863=CARTESIAN_POINT('Ctrl Pts',(2.42798652892013,7.52925253662181,47.7608692830322));
#73864=CARTESIAN_POINT('Ctrl Pts',(2.38060862171707,7.54433911900497,47.7628724545998));
#73865=CARTESIAN_POINT('Ctrl Pts',(2.36084458931395,7.55054719743008,47.7637060895749));
#73866=CARTESIAN_POINT('Ctrl Pts',(2.32055730892999,7.56302818435468,47.7654013889756));
#73867=CARTESIAN_POINT('Ctrl Pts',(2.30003246020295,7.56929535867422,47.7662629774537));
#73868=CARTESIAN_POINT('Ctrl Pts',(2.25447917003463,7.58300246821759,47.7681706521633));
#73869=CARTESIAN_POINT('Ctrl Pts',(2.22943886535724,7.59040217069117,47.7692162495657));
#73870=CARTESIAN_POINT('Ctrl Pts',(2.15071001681499,7.61324426967253,47.7724944563385));
#73871=CARTESIAN_POINT('Ctrl Pts',(2.09689408810176,7.62824207310139,47.7747218452096));
#73872=CARTESIAN_POINT('Ctrl Pts',(1.97087206896162,7.66192838942477,47.7799087440057));
#73873=CARTESIAN_POINT('Ctrl Pts',(1.898551442613,7.68016835071773,47.7828632535244));
#73874=CARTESIAN_POINT('Ctrl Pts',(1.63979627083608,7.74155059314109,47.7933655242799));
#73875=CARTESIAN_POINT('Ctrl Pts',(1.45206617090166,7.77894866047001,47.8008617871516));
#73876=CARTESIAN_POINT('Ctrl Pts',(0.737626000234092,7.89450728526039,47.8291020033859));
#73877=CARTESIAN_POINT('Ctrl Pts',(0.204838750260679,7.9262481048425,47.8493553325807));
#73878=CARTESIAN_POINT('Ctrl Pts',(-0.859939844632741,7.88218405516834,
47.8892992384333));
#73879=CARTESIAN_POINT('Ctrl Pts',(-1.38914831036012,7.80631286403357,47.9089053365519));
#73880=CARTESIAN_POINT('Ctrl Pts',(-1.93726913229037,7.67019583393996,47.9311540884416));
#73881=CARTESIAN_POINT('Ctrl Pts',(-1.96783422549068,7.66241112550565,47.9324017006341));
#73882=CARTESIAN_POINT('Ctrl Pts',(-2.02881930333143,7.64648970287581,47.9349060385753));
#73883=CARTESIAN_POINT('Ctrl Pts',(-2.0592388864327,7.63835373108642,47.9361627232395));
#73884=CARTESIAN_POINT('Ctrl Pts',(-2.10102452542016,7.62691005816075,47.937900104747));
#73885=CARTESIAN_POINT('Ctrl Pts',(-2.11243313162462,7.62375808603977,47.9383756032993));
#73886=CARTESIAN_POINT('Ctrl Pts',(-2.13059010255261,7.61869778877025,47.9391342430108));
#73887=CARTESIAN_POINT('Ctrl Pts',(-2.13734309996184,7.61680606648379,47.9394168126078));
#73888=CARTESIAN_POINT('Ctrl Pts',(-2.15118152165493,7.61290964631828,47.9399967239507));
#73889=CARTESIAN_POINT('Ctrl Pts',(-2.15826667828691,7.61090403086734,47.9402940976044));
#73890=CARTESIAN_POINT('Ctrl Pts',(-2.17460179307648,7.60625535918422,47.9409807923337));
#73891=CARTESIAN_POINT('Ctrl Pts',(-2.18384974101013,7.60360531953823,47.9413703623874));
#73892=CARTESIAN_POINT('Ctrl Pts',(-2.21273488247147,7.59527111230424,47.9425897205102));
#73893=CARTESIAN_POINT('Ctrl Pts',(-2.23235480437353,7.5895277157014,47.9434216731564));
#73894=CARTESIAN_POINT('Ctrl Pts',(-2.35275226495463,7.5537761671532,47.9485508081144));
#73895=CARTESIAN_POINT('Ctrl Pts',(-2.45294329064368,7.5218379881809,47.9529236003825));
#73896=CARTESIAN_POINT('Ctrl Pts',(-2.63539211865668,7.4596450655571,47.9611111491081));
#73897=CARTESIAN_POINT('Ctrl Pts',(-2.71783713640815,7.43000380961191,47.9648925874722));
#73898=CARTESIAN_POINT('Ctrl Pts',(-3.00728413053081,7.32047750159764,47.9784195732065));
#73899=CARTESIAN_POINT('Ctrl Pts',(-3.21139474162638,7.23326239146605,47.9884154079134));
#73900=CARTESIAN_POINT('Ctrl Pts',(-3.58952167362219,7.05252864915296,48.0075030091861));
#73901=CARTESIAN_POINT('Ctrl Pts',(-3.76423803385518,6.96084316891591,48.0165656252967));
#73902=CARTESIAN_POINT('Ctrl Pts',(-4.21856237296,6.70031651382927,48.0405420248595));
#73903=CARTESIAN_POINT('Ctrl Pts',(-4.49146807289192,6.52052486342861,48.0553648519783));
#73904=CARTESIAN_POINT('Ctrl Pts',(-4.77241096900344,6.30940847092551,48.0708082145645));
#73905=CARTESIAN_POINT('Ctrl Pts',(-4.7922575592923,6.29434740125348,48.0719003194724));
#73906=CARTESIAN_POINT('Ctrl Pts',(-4.82645107373434,6.26814334629931,48.0737837648297));
#73907=CARTESIAN_POINT('Ctrl Pts',(-4.8408313310634,6.25704427073916,48.0745764337799));
#73908=CARTESIAN_POINT('Ctrl Pts',(-5.07250449198112,6.07695587478927,48.0873556867056));
#73909=CARTESIAN_POINT('Ctrl Pts',(-5.28088137550097,5.8967792716278,48.0989680267563));
#73910=CARTESIAN_POINT('Ctrl Pts',(-5.49738550172323,5.68887437167324,48.1111458096397));
#73911=CARTESIAN_POINT('Ctrl Pts',(-5.51523481217416,5.67157155930505,48.1121507471062));
#73912=CARTESIAN_POINT('Ctrl Pts',(-5.54017564083878,5.64716527101583,48.1135563454284));
#73913=CARTESIAN_POINT('Ctrl Pts',(-5.54733555898057,5.64013208413544,48.1139600226335));
#73914=CARTESIAN_POINT('Ctrl Pts',(-5.55973254446703,5.62790808422978,48.114659254655));
#73915=CARTESIAN_POINT('Ctrl Pts',(-5.56497576724319,5.6227235465513,48.1149550800527));
#73916=CARTESIAN_POINT('Ctrl Pts',(-5.57586565999506,5.61192538608245,48.1155696828542));
#73917=CARTESIAN_POINT('Ctrl Pts',(-5.58151112073804,5.60631055212167,48.1158884071425));
#73918=CARTESIAN_POINT('Ctrl Pts',(-5.59477642000101,5.59307732036313,48.1166375763864));
#73919=CARTESIAN_POINT('Ctrl Pts',(-5.6023891981491,5.58545185056595,48.1170677123635));
#73920=CARTESIAN_POINT('Ctrl Pts',(-5.62719034241709,5.56050764108037,48.1184696815681));
#73921=CARTESIAN_POINT('Ctrl Pts',(-5.64431424186207,5.543124852365,48.1194387050206));
#73922=CARTESIAN_POINT('Ctrl Pts',(-5.93624299982986,5.24402715662592,48.1359773077054));
#73923=CARTESIAN_POINT('Ctrl Pts',(-6.18974169804896,4.94226095450934,48.1505842561011));
#73924=CARTESIAN_POINT('Ctrl Pts',(-6.50460158135436,4.50501553374898,48.1697118311163));
#73925=CARTESIAN_POINT('Ctrl Pts',(-6.58619638650574,4.38486319206651,48.1747812393075));
#73926=CARTESIAN_POINT('Ctrl Pts',(-6.70021841873724,4.20659050242261,48.1820919168049));
#73927=CARTESIAN_POINT('Ctrl Pts',(-6.73529209956454,4.15020131225435,48.18437473216));
#73928=CARTESIAN_POINT('Ctrl Pts',(-6.80974071934134,4.02707772977019,48.1893046423746));
#73929=CARTESIAN_POINT('Ctrl Pts',(-6.84885359504892,3.96019295183269,48.1919487253613));
#73930=CARTESIAN_POINT('Ctrl Pts',(-7.19215682309999,3.35282664222387,48.2157207396363));
#73931=CARTESIAN_POINT('Ctrl Pts',(-7.43274886908881,2.7789599659171,48.2363760643762));
#73932=CARTESIAN_POINT('Ctrl Pts',(-7.61391684432018,2.14791137832844,48.2622672028282));
#73933=CARTESIAN_POINT('Ctrl Pts',(-7.62374482652852,2.11276305868083,48.2637196372793));
#73934=CARTESIAN_POINT('Ctrl Pts',(-7.63546308353798,2.06970783689401,48.2655127148362));
#73935=CARTESIAN_POINT('Ctrl Pts',(-7.63758497791168,2.06186389814465,48.2658399462566));
#73936=CARTESIAN_POINT('Ctrl Pts',(-7.64106500225261,2.04892032111823,48.2663808700951));
#73937=CARTESIAN_POINT('Ctrl Pts',(-7.64243012502068,2.04382255463084,48.2665941524558));
#73938=CARTESIAN_POINT('Ctrl Pts',(-7.64488203191978,2.03462961485323,48.2669792123101));
#73939=CARTESIAN_POINT('Ctrl Pts',(-7.6459706301708,2.03053492312723,48.2671508825104));
#73940=CARTESIAN_POINT('Ctrl Pts',(-7.64828622352328,2.02179670367436,48.2675175734138));
#73941=CARTESIAN_POINT('Ctrl Pts',(-7.64951227982905,2.01715293135447,48.2677126498599));
#73942=CARTESIAN_POINT('Ctrl Pts',(-7.65280370937594,2.004640259806,48.2682388431482));
#73943=CARTESIAN_POINT('Ctrl Pts',(-7.65486117112818,1.99676929950929,48.2685704342234));
#73944=CARTESIAN_POINT('Ctrl Pts',(-7.66529808349809,1.95658897130564,48.2702662612477));
#73945=CARTESIAN_POINT('Ctrl Pts',(-7.67348501698635,1.92423042792129,48.2716421591186));
#73946=CARTESIAN_POINT('Ctrl Pts',(-7.74935125792392,1.61618656523759,48.2848297104512));
#73947=CARTESIAN_POINT('Ctrl Pts',(-7.80234523184467,1.33711852353933,48.2974500386472));
#73948=CARTESIAN_POINT('Ctrl Pts',(-7.88700764005071,0.708447202027818,
48.3263919145905));
#73949=CARTESIAN_POINT('Ctrl Pts',(-7.91064898259738,0.358344491411203,
48.342843249367));
#73950=CARTESIAN_POINT('Ctrl Pts',(-7.91099612024181,0.0078348911301656,
48.3590392895494));
#73951=CARTESIAN_POINT('',(-7.911,-2.19824158875781E-13,50.357668491763));
#73952=CARTESIAN_POINT('Ctrl Pts',(-7.911,-3.90243393155743E-13,48.357668491763));
#73953=CARTESIAN_POINT('Ctrl Pts',(-7.91099999999989,-2.20167589666719,
48.4462559274957));
#73954=CARTESIAN_POINT('Ctrl Pts',(-6.94214576672347,-4.38610418338723,
48.5348433632285));
#73955=CARTESIAN_POINT('Ctrl Pts',(-3.67820201488239,-7.34180684107656,
48.7120182346939));
#73956=CARTESIAN_POINT('Ctrl Pts',(-1.40868175871689,-8.08992666571347,
48.8006056704267));
#73957=CARTESIAN_POINT('Ctrl Pts',(2.97309270521332,-7.65454228025235,48.9777805418921));
#73958=CARTESIAN_POINT('Ctrl Pts',(5.05102072675654,-6.47444880834186,49.0663679776248));
#73959=CARTESIAN_POINT('Ctrl Pts',(7.66951518847898,-2.93425195367641,49.2435428490903));
#73960=CARTESIAN_POINT('Ctrl Pts',(8.18956872247078,-0.601881960098432,
49.332130284823));
#73961=CARTESIAN_POINT('Ctrl Pts',(7.32306689761308,3.71537198232521,49.5093051562885));
#73962=CARTESIAN_POINT('Ctrl Pts',(5.94329958850145,5.66643518936571,49.5978925920212));
#73963=CARTESIAN_POINT('Ctrl Pts',(2.16154501637763,7.92205913233022,49.7750674634866));
#73964=CARTESIAN_POINT('Ctrl Pts',(-0.21081652930128,8.20894963713001,49.8636548992194));
#73965=CARTESIAN_POINT('Ctrl Pts',(-4.42123908576519,6.9198224471778,50.0408297706848));
#73966=CARTESIAN_POINT('Ctrl Pts',(-6.22631625634254,5.35390358803445,50.1294172064176));
#73967=CARTESIAN_POINT('Ctrl Pts',(-7.65317280859507,2.31334857514446,50.2645592586879));
#73968=CARTESIAN_POINT('Ctrl Pts',(-7.91100000000003,1.15702837836471,50.3111138752254));
#73969=CARTESIAN_POINT('Ctrl Pts',(-7.911,-2.19824158875781E-13,50.357668491763));
#73970=CARTESIAN_POINT('',(-7.91058521897938,0.00383761197256053,54.357668491763));
#73971=CARTESIAN_POINT('Ctrl Pts',(-7.91099932750376,-0.00326193729837859,
50.3656282681517));
#73972=CARTESIAN_POINT('Ctrl Pts',(-7.91063423660574,-0.888697058967943,
50.3987126545666));
#73973=CARTESIAN_POINT('Ctrl Pts',(-7.76164164915843,-1.7676886397623,50.4265561435748));
#73974=CARTESIAN_POINT('Ctrl Pts',(-7.39460813755596,-2.82072656698914,
50.4666422517194));
#73975=CARTESIAN_POINT('Ctrl Pts',(-7.30956138900448,-3.03430811676538,
50.4752003333027));
#73976=CARTESIAN_POINT('Ctrl Pts',(-7.20239712110214,-3.27267384299411,
50.4855406317549));
#73977=CARTESIAN_POINT('Ctrl Pts',(-7.18927519264712,-3.30139978270516,
50.4868001333683));
#73978=CARTESIAN_POINT('Ctrl Pts',(-7.17254955064214,-3.33744219837014,
50.4883981547481));
#73979=CARTESIAN_POINT('Ctrl Pts',(-7.16910589495979,-3.3448330526048,50.4887267866171));
#73980=CARTESIAN_POINT('Ctrl Pts',(-7.16361390435419,-3.35657264730443,
50.4892503004327));
#73981=CARTESIAN_POINT('Ctrl Pts',(-7.16157301362628,-3.36092488425353,
50.4894447153364));
#73982=CARTESIAN_POINT('Ctrl Pts',(-7.15772602583966,-3.36910924224991,
50.4898109406299));
#73983=CARTESIAN_POINT('Ctrl Pts',(-7.15592081400479,-3.3729417799237,50.489982694956));
#73984=CARTESIAN_POINT('Ctrl Pts',(-7.15186248429565,-3.38153985525506,
50.4903686028632));
#73985=CARTESIAN_POINT('Ctrl Pts',(-7.1496076819584,-3.38630459066725,50.4905828639103));
#73986=CARTESIAN_POINT('Ctrl Pts',(-7.14387483622987,-3.39838770299386,
50.4911272548192));
#73987=CARTESIAN_POINT('Ctrl Pts',(-7.14039031243064,-3.40570298789622,
50.491457803182));
#73988=CARTESIAN_POINT('Ctrl Pts',(-7.12015774580656,-3.44801097131292,
50.493375179992));
#73989=CARTESIAN_POINT('Ctrl Pts',(-7.10316401870511,-3.48288483935802,
50.4949779653658));
#73990=CARTESIAN_POINT('Ctrl Pts',(-6.71689667658263,-4.26098149611558,
50.5312134315314));
#73991=CARTESIAN_POINT('Ctrl Pts',(-6.23321298979244,-4.94165389363112,
50.5719986646624));
#73992=CARTESIAN_POINT('Ctrl Pts',(-5.38231149584855,-5.81066124078991,
50.6265882289182));
#73993=CARTESIAN_POINT('Ctrl Pts',(-5.0922640082942,-6.06646249653365,50.6432017720806));
#73994=CARTESIAN_POINT('Ctrl Pts',(-4.76400018778417,-6.31576566792567,
50.6598955089649));
#73995=CARTESIAN_POINT('Ctrl Pts',(-4.74326708212672,-6.33135144869598,
50.6609416686046));
#73996=CARTESIAN_POINT('Ctrl Pts',(-4.71403236474659,-6.3531039773494,50.6624053715415));
#73997=CARTESIAN_POINT('Ctrl Pts',(-4.70559467430217,-6.3593561030386,50.6628264946215));
#73998=CARTESIAN_POINT('Ctrl Pts',(-4.69127469031386,-6.36992276213706,
50.6635389582765));
#73999=CARTESIAN_POINT('Ctrl Pts',(-4.68539884482381,-6.37424598528254,
50.6638306620299));
#74000=CARTESIAN_POINT('Ctrl Pts',(-4.67362046080042,-6.38288698561992,
50.6644141212929));
#74001=CARTESIAN_POINT('Ctrl Pts',(-4.66771789811827,-6.38720471777697,
50.6647058748133));
#74002=CARTESIAN_POINT('Ctrl Pts',(-4.65346027807135,-6.39760386633642,
50.6654090685833));
#74003=CARTESIAN_POINT('Ctrl Pts',(-4.64509926483095,-6.40367711640235,
50.6658201688268));
#74004=CARTESIAN_POINT('Ctrl Pts',(-4.61691819233748,-6.42406297357864,
50.6672015420334));
#74005=CARTESIAN_POINT('Ctrl Pts',(-4.59704359721091,-6.43830015324268,
50.6681686863293));
#74006=CARTESIAN_POINT('Ctrl Pts',(-4.30946534927441,-6.64229651524981,
50.682062213375));
#74007=CARTESIAN_POINT('Ctrl Pts',(-4.03026401943296,-6.81532061400327,
50.6942762938282));
#74008=CARTESIAN_POINT('Ctrl Pts',(-3.56714627047105,-7.06387742817192,
50.7130218432213));
#74009=CARTESIAN_POINT('Ctrl Pts',(-3.3897561518577,-7.15069603207906,50.7198766917271));
#74010=CARTESIAN_POINT('Ctrl Pts',(-2.91880780771747,-7.35972083587991,
50.7375115356681));
#74011=CARTESIAN_POINT('Ctrl Pts',(-2.6208141685694,-7.47102807635808,50.7481113814818));
#74012=CARTESIAN_POINT('Ctrl Pts',(-2.07511709197775,-7.63817860538175,
50.767591464366));
#74013=CARTESIAN_POINT('Ctrl Pts',(-1.82989674434693,-7.70060707156553,
50.7763741630215));
#74014=CARTESIAN_POINT('Ctrl Pts',(-1.42178340387637,-7.78390854928552,
50.7916321369029));
#74015=CARTESIAN_POINT('Ctrl Pts',(-1.26047744385343,-7.81165096422,50.7978253555369));
#74016=CARTESIAN_POINT('Ctrl Pts',(-1.07340306882081,-7.83788019074037,
50.805316173043));
#74017=CARTESIAN_POINT('Ctrl Pts',(-1.04835244484867,-7.84127012383302,
50.8063255981188));
#74018=CARTESIAN_POINT('Ctrl Pts',(-1.01614371614511,-7.84547161314059,
50.8076321223189));
#74019=CARTESIAN_POINT('Ctrl Pts',(-1.00899989738426,-7.84639357226209,
50.8079224531657));
#74020=CARTESIAN_POINT('Ctrl Pts',(-0.997463458267445,-7.84786641375185,
50.8083922014527));
#74021=CARTESIAN_POINT('Ctrl Pts',(-0.993071603142432,-7.84842336966654,
50.8085712418834));
#74022=CARTESIAN_POINT('Ctrl Pts',(-0.984652612487927,-7.84948384953678,
50.8089148537254));
#74023=CARTESIAN_POINT('Ctrl Pts',(-0.980625550133025,-7.84998796188372,
50.8090793889136));
#74024=CARTESIAN_POINT('Ctrl Pts',(-0.971456179871651,-7.85112862836833,
50.8094544209483));
#74025=CARTESIAN_POINT('Ctrl Pts',(-0.966313635628383,-7.85176322910566,
50.8096650369379));
#74026=CARTESIAN_POINT('Ctrl Pts',(-0.950350929076437,-7.85371714083951,
50.8103196699765));
#74027=CARTESIAN_POINT('Ctrl Pts',(-0.939528702607679,-7.85501913627895,
50.8107647326468));
#74028=CARTESIAN_POINT('Ctrl Pts',(-0.858014369367423,-7.86465505765254,
50.8141261609303));
#74029=CARTESIAN_POINT('Ctrl Pts',(-0.787217446142281,-7.87205665017447,
50.8170974954753));
#74030=CARTESIAN_POINT('Ctrl Pts',(0.105485361785373,-7.95322335909915,
50.8551308992811));
#74031=CARTESIAN_POINT('Ctrl Pts',(0.933937673404021,-7.89891116636909,
50.8959169165339));
#74032=CARTESIAN_POINT('Ctrl Pts',(2.0094783372895,-7.65655040098159,50.9461236864054));
#74033=CARTESIAN_POINT('Ctrl Pts',(2.27653369032454,-7.58143664270754,50.958413900549));
#74034=CARTESIAN_POINT('Ctrl Pts',(2.65568166224125,-7.45294738704457,50.9755046828491));
#74035=CARTESIAN_POINT('Ctrl Pts',(2.77131593517592,-7.41072734110451,50.9806690258752));
#74036=CARTESIAN_POINT('Ctrl Pts',(2.92748307521145,-7.34954123333943,50.9875799241129));
#74037=CARTESIAN_POINT('Ctrl Pts',(2.96890622451487,-7.33290593255651,50.9894068764352));
#74038=CARTESIAN_POINT('Ctrl Pts',(3.0295342706359,-7.30796009828118,50.992072135664));
#74039=CARTESIAN_POINT('Ctrl Pts',(3.04885015050332,-7.29992270259909,50.9929199705968));
#74040=CARTESIAN_POINT('Ctrl Pts',(3.08358487765025,-7.28530756361843,50.9944422848897));
#74041=CARTESIAN_POINT('Ctrl Pts',(3.09901509461972,-7.27875727320003,50.9951177210501));
#74042=CARTESIAN_POINT('Ctrl Pts',(3.12266878670622,-7.2686271801626,50.9961518923237));
#74043=CARTESIAN_POINT('Ctrl Pts',(3.13090714140652,-7.26508237449968,50.9965118535135));
#74044=CARTESIAN_POINT('Ctrl Pts',(3.14598101444148,-7.25856597482103,50.9971700637796));
#74045=CARTESIAN_POINT('Ctrl Pts',(3.15281838956543,-7.25559871801612,50.9974684645234));
#74046=CARTESIAN_POINT('Ctrl Pts',(3.1665246744098,-7.24962748641381,50.9980663294654));
#74047=CARTESIAN_POINT('Ctrl Pts',(3.17339352792987,-7.24662340146897,50.9983657893837));
#74048=CARTESIAN_POINT('Ctrl Pts',(3.19277367715162,-7.23811467714271,50.9992102607914));
#74049=CARTESIAN_POINT('Ctrl Pts',(3.20527501973949,-7.23258735745982,50.9997544754803));
#74050=CARTESIAN_POINT('Ctrl Pts',(3.25709765267804,-7.20951384674716,51.0020083352734));
#74051=CARTESIAN_POINT('Ctrl Pts',(3.29629003291522,-7.19167901955263,51.0037078287843));
#74052=CARTESIAN_POINT('Ctrl Pts',(3.92440111653819,-6.89963834637898,51.0308695871601));
#74053=CARTESIAN_POINT('Ctrl Pts',(4.47752131993072,-6.55422069360326,51.0534437952189));
#74054=CARTESIAN_POINT('Ctrl Pts',(5.39998542451969,-5.80632317968186,51.094435484315));
#74055=CARTESIAN_POINT('Ctrl Pts',(5.78215959746906,-5.42585122552941,51.1129358520177));
#74056=CARTESIAN_POINT('Ctrl Pts',(6.14724811627211,-4.97963418290188,51.1357270807106));
#74057=CARTESIAN_POINT('Ctrl Pts',(6.17151244847477,-4.94953028314072,51.1372679193379));
#74058=CARTESIAN_POINT('Ctrl Pts',(6.20262220522515,-4.91034906656276,51.1392764267488));
#74059=CARTESIAN_POINT('Ctrl Pts',(6.20967037756325,-4.90143284932954,51.1397336928014));
#74060=CARTESIAN_POINT('Ctrl Pts',(6.22103623580378,-4.88699072340626,51.1404746467236));
#74061=CARTESIAN_POINT('Ctrl Pts',(6.22536584640322,-4.88147418879481,51.1407577416441));
#74062=CARTESIAN_POINT('Ctrl Pts',(6.23362403128001,-4.87092324059049,51.1412993120964));
#74063=CARTESIAN_POINT('Ctrl Pts',(6.2375538578542,-4.86588981062454,51.1415577262579));
#74064=CARTESIAN_POINT('Ctrl Pts',(6.24653522661612,-4.85435746692604,51.1421499041103));
#74065=CARTESIAN_POINT('Ctrl Pts',(6.25158272431997,-4.84785542218394,51.1424838609734));
#74066=CARTESIAN_POINT('Ctrl Pts',(6.26707029842123,-4.82784035278812,51.1435120966067));
#74067=CARTESIAN_POINT('Ctrl Pts',(6.27747673954671,-4.81430144218547,51.1442079468739));
#74068=CARTESIAN_POINT('Ctrl Pts',(6.35682010230064,-4.71038007803364,51.1495509832883));
#74069=CARTESIAN_POINT('Ctrl Pts',(6.423843875146,-4.61855721634384,51.1542825802134));
#74070=CARTESIAN_POINT('Ctrl Pts',(6.52143169782487,-4.47862602200934,51.1614788080948));
#74071=CARTESIAN_POINT('Ctrl Pts',(6.55349398485417,-4.43157747167014,51.1638960303008));
#74072=CARTESIAN_POINT('Ctrl Pts',(6.79779901849484,-4.06463155035454,51.1827126405753));
#74073=CARTESIAN_POINT('Ctrl Pts',(6.9870065341398,-3.73001785183359,51.1996341410474));
#74074=CARTESIAN_POINT('Ctrl Pts',(7.38844920209015,-2.88142591067553,51.240686806223));
#74075=CARTESIAN_POINT('Ctrl Pts',(7.57231676403376,-2.35624767753718,51.2644782673826));
#74076=CARTESIAN_POINT('Ctrl Pts',(7.71897264172309,-1.73447949806625,51.2906027960045));
#74077=CARTESIAN_POINT('Ctrl Pts',(7.73693055376853,-1.65253249969406,51.2940097092983));
#74078=CARTESIAN_POINT('Ctrl Pts',(7.7585901288799,-1.54558622697846,51.2984123155001));
#74079=CARTESIAN_POINT('Ctrl Pts',(7.7634799916461,-1.52083398198157,51.2994282394327));
#74080=CARTESIAN_POINT('Ctrl Pts',(7.77115261856333,-1.48099403773544,51.3010585091507));
#74081=CARTESIAN_POINT('Ctrl Pts',(7.77401004138998,-1.46592095254761,51.3016741795222));
#74082=CARTESIAN_POINT('Ctrl Pts',(7.77936394008192,-1.43722286271735,51.3028442243728));
#74083=CARTESIAN_POINT('Ctrl Pts',(7.78186851133127,-1.42359943212925,51.3033987431802));
#74084=CARTESIAN_POINT('Ctrl Pts',(7.78740038003018,-1.39305839362213,51.3046398036761));
#74085=CARTESIAN_POINT('Ctrl Pts',(7.79040835784552,-1.37613734333906,51.3053259892732));
#74086=CARTESIAN_POINT('Ctrl Pts',(7.79914666109466,-1.32603403008984,51.3073536044046));
#74087=CARTESIAN_POINT('Ctrl Pts',(7.80472031178468,-1.29282472373236,51.308692115306));
#74088=CARTESIAN_POINT('Ctrl Pts',(7.84212571670478,-1.06089097389523,51.318002652047));
#74089=CARTESIAN_POINT('Ctrl Pts',(7.86657669874312,-0.861046421528195,
51.325829613732));
#74090=CARTESIAN_POINT('Ctrl Pts',(7.94183784018527,0.0372569469019125,
51.3602648290222));
#74091=CARTESIAN_POINT('Ctrl Pts',(7.9074062962736,0.73960622461558,51.3848085260178));
#74092=CARTESIAN_POINT('Ctrl Pts',(7.75162801654313,1.58829116898041,51.4169862370396));
#74093=CARTESIAN_POINT('Ctrl Pts',(7.71731590269283,1.74740880518786,51.4231519121374));
#74094=CARTESIAN_POINT('Ctrl Pts',(7.66041220999307,1.97671770845446,51.4323595058966));
#74095=CARTESIAN_POINT('Ctrl Pts',(7.64170805330582,2.04783439099113,51.4352608630616));
#74096=CARTESIAN_POINT('Ctrl Pts',(7.61860440282805,2.13095053792775,51.4387158590626));
#74097=CARTESIAN_POINT('Ctrl Pts',(7.61516352053112,2.14321436043001,51.4392272915709));
#74098=CARTESIAN_POINT('Ctrl Pts',(7.60985437816535,2.16196273846169,51.440011737437));
#74099=CARTESIAN_POINT('Ctrl Pts',(7.6080074037426,2.16845333903307,51.4402837846418));
#74100=CARTESIAN_POINT('Ctrl Pts',(7.60462856238002,2.18026973997827,51.4407799368376));
#74101=CARTESIAN_POINT('Ctrl Pts',(7.60309939848854,2.18559631389278,51.4410039170493));
#74102=CARTESIAN_POINT('Ctrl Pts',(7.60001808473597,2.19628716163343,51.4414541245232));
#74103=CARTESIAN_POINT('Ctrl Pts',(7.59846584944184,2.20165140730623,51.4416803556896));
#74104=CARTESIAN_POINT('Ctrl Pts',(7.59404318161773,2.21687496292786,51.4423233543292));
#74105=CARTESIAN_POINT('Ctrl Pts',(7.5911592380479,2.2267303084558,51.4427407614954));
#74106=CARTESIAN_POINT('Ctrl Pts',(7.57891501485255,2.2682724409519,51.444505150697));
#74107=CARTESIAN_POINT('Ctrl Pts',(7.56937550295443,2.29990590214824,51.4458608538362));
#74108=CARTESIAN_POINT('Ctrl Pts',(7.39497442130201,2.86538780760916,51.4703268676657));
#74109=CARTESIAN_POINT('Ctrl Pts',(7.17422499549569,3.38030937108751,51.4961903902932));
#74110=CARTESIAN_POINT('Ctrl Pts',(6.66939671667504,4.28108686670812,51.5437815146591));
#74111=CARTESIAN_POINT('Ctrl Pts',(6.40097647765962,4.67291429104499,51.5654411550374));
#74112=CARTESIAN_POINT('Ctrl Pts',(5.95550333857063,5.21217020002396,51.5957110302301));
#74113=CARTESIAN_POINT('Ctrl Pts',(5.8045640074937,5.37975699800221,51.6052068379761));
#74114=CARTESIAN_POINT('Ctrl Pts',(5.61775566994624,5.57013877003414,51.6161019565985));
#74115=CARTESIAN_POINT('Ctrl Pts',(5.58861673988847,5.59937386534448,51.6177783266812));
#74116=CARTESIAN_POINT('Ctrl Pts',(5.54957879140493,5.63793233564672,51.6199939762504));
#74117=CARTESIAN_POINT('Ctrl Pts',(5.53988288856258,5.64745990394324,51.6205418343414));
#74118=CARTESIAN_POINT('Ctrl Pts',(5.52389686009039,5.66308760783795,51.6214411109277));
#74119=CARTESIAN_POINT('Ctrl Pts',(5.51762108939954,5.66920235036549,51.6217931397571));
#74120=CARTESIAN_POINT('Ctrl Pts',(5.50542212751849,5.68104885866696,51.6224754715833));
#74121=CARTESIAN_POINT('Ctrl Pts',(5.49950011348128,5.68678181743053,51.6228058241403));
#74122=CARTESIAN_POINT('Ctrl Pts',(5.48578026008289,5.70002220216885,51.6235691255691));
#74123=CARTESIAN_POINT('Ctrl Pts',(5.4779759427878,5.70752290740185,51.6240017953849));
#74124=CARTESIAN_POINT('Ctrl Pts',(5.45695324696115,5.72764491579377,51.6251632181735));
#74125=CARTESIAN_POINT('Ctrl Pts',(5.44370645120136,5.74023650205877,51.6258907436819));
#74126=CARTESIAN_POINT('Ctrl Pts',(5.3489331746052,5.82969901162738,51.631065315766));
#74127=CARTESIAN_POINT('Ctrl Pts',(5.26582350120573,5.90487770732505,51.6354427939177));
#74128=CARTESIAN_POINT('Ctrl Pts',(4.46784028501046,6.59646017467778,51.6760596632883));
#74129=CARTESIAN_POINT('Ctrl Pts',(3.64977825246519,7.08193125345826,51.7062720770154));
#74130=CARTESIAN_POINT('Ctrl Pts',(2.54270612159614,7.49500767279357,51.7489629801311));
#74131=CARTESIAN_POINT('Ctrl Pts',(2.31622778672315,7.56806331576251,51.7578405315634));
#74132=CARTESIAN_POINT('Ctrl Pts',(2.04837679128682,7.64131274478681,51.7687915318567));
#74133=CARTESIAN_POINT('Ctrl Pts',(2.00987291568815,7.65153048277121,51.7703752781873));
#74134=CARTESIAN_POINT('Ctrl Pts',(1.95990874526714,7.66438627129496,51.772441348935));
#74135=CARTESIAN_POINT('Ctrl Pts',(1.94851702038957,7.66729030523684,51.7729131430695));
#74136=CARTESIAN_POINT('Ctrl Pts',(1.93007339448916,7.67194828561836,51.7736781398163));
#74137=CARTESIAN_POINT('Ctrl Pts',(1.92302545144595,7.67371793317806,51.773970741457));
#74138=CARTESIAN_POINT('Ctrl Pts',(1.90954567749892,7.67708279353225,51.774530870607));
#74139=CARTESIAN_POINT('Ctrl Pts',(1.90311425805807,7.67867964129635,51.7747983366184));
#74140=CARTESIAN_POINT('Ctrl Pts',(1.88837417068295,7.68231977989668,51.7754118300176));
#74141=CARTESIAN_POINT('Ctrl Pts',(1.88006418627116,7.68435767412717,51.7757580552635));
#74142=CARTESIAN_POINT('Ctrl Pts',(1.85444800737679,7.69059560326202,51.7768263920191));
#74143=CARTESIAN_POINT('Ctrl Pts',(1.83713098446359,7.69475067074946,51.7775501119269));
#74144=CARTESIAN_POINT('Ctrl Pts',(1.70079499748576,7.72697682673053,51.78325903948));
#74145=CARTESIAN_POINT('Ctrl Pts',(1.58115643454892,7.75234269729421,51.7883350485991));
#74146=CARTESIAN_POINT('Ctrl Pts',(1.45278627155921,7.77646465831772,51.7938234873725));
#74147=CARTESIAN_POINT('Ctrl Pts',(1.4445886457859,7.77799165446749,51.7941741585694));
#74148=CARTESIAN_POINT('Ctrl Pts',(1.42645633685526,7.78133955901198,51.7949501958034));
#74149=CARTESIAN_POINT('Ctrl Pts',(1.41652055434346,7.78315440758768,51.7953756909288));
#74150=CARTESIAN_POINT('Ctrl Pts',(1.36811606380002,7.79190010934326,51.797449778226));
#74151=CARTESIAN_POINT('Ctrl Pts',(1.32960003092727,7.79856477821357,51.7991038036884));
#74152=CARTESIAN_POINT('Ctrl Pts',(1.28397015148832,7.80611253752531,51.8010667402087));
#74153=CARTESIAN_POINT('Ctrl Pts',(1.27690230142591,7.80727179050651,51.8013708866054));
#74154=CARTESIAN_POINT('Ctrl Pts',(1.26133882707402,7.80980277731577,51.8020408233448));
#74155=CARTESIAN_POINT('Ctrl Pts',(1.25284252157402,7.81117024992796,51.8024066839993));
#74156=CARTESIAN_POINT('Ctrl Pts',(0.857517511695545,7.87413585671681,51.8194356759236));
#74157=CARTESIAN_POINT('Ctrl Pts',(0.466650511508528,7.90693308887498,51.8364900694726));
#74158=CARTESIAN_POINT('Ctrl Pts',(-0.629153019894741,7.91731721787121,
51.8835976835022));
#74159=CARTESIAN_POINT('Ctrl Pts',(-1.33103062751872,7.82995393213053,51.9126928418116));
#74160=CARTESIAN_POINT('Ctrl Pts',(-2.09882235532606,7.62803456406769,51.9449342065091));
#74161=CARTESIAN_POINT('Ctrl Pts',(-2.18517603357127,7.60374726396495,51.9485667238278));
#74162=CARTESIAN_POINT('Ctrl Pts',(-2.30639371131205,7.56741876052888,51.9536744990779));
#74163=CARTESIAN_POINT('Ctrl Pts',(-2.34161474811365,7.55659440705687,51.9551596697928));
#74164=CARTESIAN_POINT('Ctrl Pts',(-2.40226245505702,7.53749103215405,51.9577188867632));
#74165=CARTESIAN_POINT('Ctrl Pts',(-2.42772510493538,7.52932844167626,51.9587939360702));
#74166=CARTESIAN_POINT('Ctrl Pts',(-2.47650989011661,7.51341624784282,51.9608548037052));
#74167=CARTESIAN_POINT('Ctrl Pts',(-2.4998382554459,7.5056867540398,51.9618407926653));
#74168=CARTESIAN_POINT('Ctrl Pts',(-2.56090266114423,7.48513773301162,51.9644230995938));
#74169=CARTESIAN_POINT('Ctrl Pts',(-2.59857856846938,7.47214151115732,51.9660177313941));
#74170=CARTESIAN_POINT('Ctrl Pts',(-2.73049014053044,7.42552054402354,51.9716061759972));
#74171=CARTESIAN_POINT('Ctrl Pts',(-2.82418513209205,7.39039311353117,51.9755849936637));
#74172=CARTESIAN_POINT('Ctrl Pts',(-3.4235573176014,7.15261754702738,52.001117643302));
#74173=CARTESIAN_POINT('Ctrl Pts',(-3.90782265814914,6.89997198770932,52.0220186039863));
#74174=CARTESIAN_POINT('Ctrl Pts',(-4.53175182091598,6.48755844986922,52.0509942942786));
#74175=CARTESIAN_POINT('Ctrl Pts',(-4.69684170747475,6.36905525078565,52.0588944000711));
#74176=CARTESIAN_POINT('Ctrl Pts',(-4.93347142297377,6.18499164411376,52.0707216214523));
#74177=CARTESIAN_POINT('Ctrl Pts',(-5.00866345580982,6.12425928896814,52.0745596792913));
#74178=CARTESIAN_POINT('Ctrl Pts',(-5.09963491146074,6.04798576783761,52.0793176655236));
#74179=CARTESIAN_POINT('Ctrl Pts',(-5.11648747214332,6.0337354946045,52.080204025323));
#74180=CARTESIAN_POINT('Ctrl Pts',(-5.14289908414766,6.01121200946461,52.081601173204));
#74181=CARTESIAN_POINT('Ctrl Pts',(-5.15249835023151,6.00298605378961,52.0821106459879));
#74182=CARTESIAN_POINT('Ctrl Pts',(-5.16952888873589,5.98832102956926,52.0830175728484));
#74183=CARTESIAN_POINT('Ctrl Pts',(-5.17696795872535,5.98189104199851,52.0834147640627));
#74184=CARTESIAN_POINT('Ctrl Pts',(-5.1941418395479,5.96699070419095,52.0843341586887));
#74185=CARTESIAN_POINT('Ctrl Pts',(-5.20386794289899,5.9585103796674,52.0848566582438));
#74186=CARTESIAN_POINT('Ctrl Pts',(-5.23131622395633,5.93445937605739,52.0863364559179));
#74187=CARTESIAN_POINT('Ctrl Pts',(-5.24898944035061,5.91883327701004,52.0872955026801));
#74188=CARTESIAN_POINT('Ctrl Pts',(-5.37073344717693,5.81021696158868,52.0939445722017));
#74189=CARTESIAN_POINT('Ctrl Pts',(-5.47239577361877,5.71456752214339,52.0997124422293));
#74190=CARTESIAN_POINT('Ctrl Pts',(-5.67040371384077,5.51813934773089,52.1113335357878));
#74191=CARTESIAN_POINT('Ctrl Pts',(-5.766723458435,5.41740159149943,52.1171846086875));
#74192=CARTESIAN_POINT('Ctrl Pts',(-6.08380218366205,5.06773548654104,52.1370607437187));
#74193=CARTESIAN_POINT('Ctrl Pts',(-6.29150919565183,4.80744309745239,52.1511313475512));
#74194=CARTESIAN_POINT('Ctrl Pts',(-6.63068332247564,4.32262001343453,52.1758280047974));
#74195=CARTESIAN_POINT('Ctrl Pts',(-6.76864502488835,4.10322503159877,52.1865158486716));
#74196=CARTESIAN_POINT('Ctrl Pts',(-6.92710459605693,3.82142315226304,52.199665809545));
#74197=CARTESIAN_POINT('Ctrl Pts',(-6.95792682315671,3.76501094481418,52.2022708713922));
#74198=CARTESIAN_POINT('Ctrl Pts',(-7.0016838603282,3.68255198023705,52.2060405512808));
#74199=CARTESIAN_POINT('Ctrl Pts',(-7.01516785184059,3.65679996533675,52.2072124863238));
#74200=CARTESIAN_POINT('Ctrl Pts',(-7.03856955574081,3.61150107456979,52.2092648044099));
#74201=CARTESIAN_POINT('Ctrl Pts',(-7.04854852220166,3.59198623835311,52.2101459842405));
#74202=CARTESIAN_POINT('Ctrl Pts',(-7.06779505723496,3.55395872541412,52.2118574351296));
#74203=CARTESIAN_POINT('Ctrl Pts',(-7.07707130966179,3.53545064653251,52.2126878123881));
#74204=CARTESIAN_POINT('Ctrl Pts',(-7.09914875751444,3.49096641865701,52.2146775283098));
#74205=CARTESIAN_POINT('Ctrl Pts',(-7.11188019544711,3.46495594652046,52.2158359743576));
#74206=CARTESIAN_POINT('Ctrl Pts',(-7.15817453133749,3.36904596555332,52.2200898348522));
#74207=CARTESIAN_POINT('Ctrl Pts',(-7.19085222120405,3.29872366486285,52.22317426749));
#74208=CARTESIAN_POINT('Ctrl Pts',(-7.49456182337317,2.61917405639613,52.2526779178102));
#74209=CARTESIAN_POINT('Ctrl Pts',(-7.68859618809676,1.97841047593569,52.2784066827412));
#74210=CARTESIAN_POINT('Ctrl Pts',(-7.87401781437724,0.883504242566689,
52.3202553184965));
#74211=CARTESIAN_POINT('Ctrl Pts',(-7.91116630099991,0.440647754662544,
52.3366328182147));
#74212=CARTESIAN_POINT('Ctrl Pts',(-7.91091146870865,-0.23686117930278,
52.3623571067234));
#74213=CARTESIAN_POINT('Ctrl Pts',(-7.90045139121858,-0.470619476705709,
52.3713670367977));
#74214=CARTESIAN_POINT('Ctrl Pts',(-7.8776860694444,-0.725583981570365,
52.3815784090536));
#74215=CARTESIAN_POINT('Ctrl Pts',(-7.87562726922063,-0.747599511082148,
52.3824633127918));
#74216=CARTESIAN_POINT('Ctrl Pts',(-7.87252027729739,-0.77938568083008,
52.3837458252475));
#74217=CARTESIAN_POINT('Ctrl Pts',(-7.87154612836062,-0.789163547105341,
52.384141011737));
#74218=CARTESIAN_POINT('Ctrl Pts',(-7.86980411313111,-0.806324575807061,
52.3848358032406));
#74219=CARTESIAN_POINT('Ctrl Pts',(-7.86904406699321,-0.813708530067096,
52.3851351458108));
#74220=CARTESIAN_POINT('Ctrl Pts',(-7.86746018889364,-0.828886360994354,
52.3857512697866));
#74221=CARTESIAN_POINT('Ctrl Pts',(-7.86663516551494,-0.836680103412573,
52.3860680915631));
#74222=CARTESIAN_POINT('Ctrl Pts',(-7.86451180998406,-0.856457994449369,
52.3868732314877));
#74223=CARTESIAN_POINT('Ctrl Pts',(-7.8631976683079,-0.868440402595209,
52.387362099298));
#74224=CARTESIAN_POINT('Ctrl Pts',(-7.85786194598504,-0.916086633540163,
52.3893104171707));
#74225=CARTESIAN_POINT('Ctrl Pts',(-7.85362511412198,-0.951725588506763,
52.3907775698038));
#74226=CARTESIAN_POINT('Ctrl Pts',(-7.82649880871162,-1.16737531669752,
52.3997202152366));
#74227=CARTESIAN_POINT('Ctrl Pts',(-7.79766789284609,-1.34655515894044,
52.4074569373015));
#74228=CARTESIAN_POINT('Ctrl Pts',(-7.72560153095527,-1.71349609976965,
52.4238472140258));
#74229=CARTESIAN_POINT('Ctrl Pts',(-7.6816154359338,-1.90099105954356,52.4325038168356));
#74230=CARTESIAN_POINT('Ctrl Pts',(-7.41176413279109,-2.88781397967049,
52.4790053354975));
#74231=CARTESIAN_POINT('Ctrl Pts',(-7.06783154185858,-3.6496557410758,52.5175496634499));
#74232=CARTESIAN_POINT('Ctrl Pts',(-6.58447494170611,-4.38532224694807,
52.5535924613072));
#74233=CARTESIAN_POINT('Ctrl Pts',(-6.55696170838169,-4.42635456513446,
52.5556010966783));
#74234=CARTESIAN_POINT('Ctrl Pts',(-6.52070022393679,-4.47935364318578,
52.5581936020238));
#74235=CARTESIAN_POINT('Ctrl Pts',(-6.51230048757717,-4.49155683852869,
52.5587904003297));
#74236=CARTESIAN_POINT('Ctrl Pts',(-6.49884532553628,-4.5109875000027,52.5597404566713));
#74237=CARTESIAN_POINT('Ctrl Pts',(-6.49381202563496,-4.51823020294322,
52.560094541546));
#74238=CARTESIAN_POINT('Ctrl Pts',(-6.48473633164779,-4.53124324509377,
52.5607306519239));
#74239=CARTESIAN_POINT('Ctrl Pts',(-6.4806983255131,-4.53701662452449,52.5610128416981));
#74240=CARTESIAN_POINT('Ctrl Pts',(-6.47122711641679,-4.55051973689208,
52.5616727809475));
#74241=CARTESIAN_POINT('Ctrl Pts',(-6.4657877624151,-4.55824515359724,52.5620502981512));
#74242=CARTESIAN_POINT('Ctrl Pts',(-6.45013284031551,-4.58039515407062,
52.5631325690474));
#74243=CARTESIAN_POINT('Ctrl Pts',(-6.43988272253188,-4.5947953110369,52.5638360148271));
#74244=CARTESIAN_POINT('Ctrl Pts',(-6.37251544534793,-4.68876980845282,
52.568425720765));
#74245=CARTESIAN_POINT('Ctrl Pts',(-6.31397174789172,-4.76731339799664,
52.5722572288625));
#74246=CARTESIAN_POINT('Ctrl Pts',(-6.13862285440356,-4.99366743489113,
52.5832975892021));
#74247=CARTESIAN_POINT('Ctrl Pts',(-6.01797705504314,-5.13842022819045,
52.5903542799024));
#74248=CARTESIAN_POINT('Ctrl Pts',(-5.64039622850543,-5.55988673723276,
52.6110335599202));
#74249=CARTESIAN_POINT('Ctrl Pts',(-5.36871111293165,-5.82266008754804,
52.62408737501));
#74250=CARTESIAN_POINT('Ctrl Pts',(-4.95849819857212,-6.16620163956753,
52.6423474357867));
#74251=CARTESIAN_POINT('Ctrl Pts',(-4.83470608817608,-6.26373403130721,
52.6476950362528));
#74252=CARTESIAN_POINT('Ctrl Pts',(-4.56188362020029,-6.46577418440707,
52.659280614942));
#74253=CARTESIAN_POINT('Ctrl Pts',(-4.41199414302791,-6.56896668581607,
52.6655247754718));
#74254=CARTESIAN_POINT('Ctrl Pts',(-4.02998926679729,-6.81298390877248,
52.6814314309922));
#74255=CARTESIAN_POINT('Ctrl Pts',(-3.79394396793837,-6.94719601549526,
52.6912535999034));
#74256=CARTESIAN_POINT('Ctrl Pts',(-3.4881974379824,-7.10080393371973,52.7044984634341));
#74257=CARTESIAN_POINT('Ctrl Pts',(-3.42448376551835,-7.13174931277163,
52.7072861532002));
#74258=CARTESIAN_POINT('Ctrl Pts',(-3.35016631470537,-7.16661939651233,
52.7105785158961));
#74259=CARTESIAN_POINT('Ctrl Pts',(-3.33995752211889,-7.17138282750633,
52.7110316623185));
#74260=CARTESIAN_POINT('Ctrl Pts',(-3.32477862669815,-7.17842587075175,
52.7117067774549));
#74261=CARTESIAN_POINT('Ctrl Pts',(-3.31981624155733,-7.18072217958851,
52.7119277055095));
#74262=CARTESIAN_POINT('Ctrl Pts',(-3.31098584997606,-7.18479727110418,
52.7123212276778));
#74263=CARTESIAN_POINT('Ctrl Pts',(-3.30711877625735,-7.18657808175755,
52.712493694284));
#74264=CARTESIAN_POINT('Ctrl Pts',(-3.29898886080286,-7.1903140050098,52.7128565597254));
#74265=CARTESIAN_POINT('Ctrl Pts',(-3.29472571587908,-7.19226844961192,
52.713047000671));
#74266=CARTESIAN_POINT('Ctrl Pts',(-3.28352164091144,-7.19739292100713,
52.7135479356325));
#74267=CARTESIAN_POINT('Ctrl Pts',(-3.27657787293121,-7.2005566915006,52.713858827612));
#74268=CARTESIAN_POINT('Ctrl Pts',(-3.24461790400414,-7.21506272428303,
52.7152918116333));
#74269=CARTESIAN_POINT('Ctrl Pts',(-3.21954769029911,-7.22628452805707,
52.7164216659886));
#74270=CARTESIAN_POINT('Ctrl Pts',(-3.02378328216905,-7.31269067630088,
52.725285934628));
#74271=CARTESIAN_POINT('Ctrl Pts',(-2.85054695268026,-7.38194304846303,
52.7333749929432));
#74272=CARTESIAN_POINT('Ctrl Pts',(-2.36545055719456,-7.55624131054427,
52.7563385332667));
#74273=CARTESIAN_POINT('Ctrl Pts',(-2.04923653957772,-7.64805556867829,
52.771642403684));
#74274=CARTESIAN_POINT('Ctrl Pts',(-1.36278552365656,-7.80172969940686,
52.8043398104943));
#74275=CARTESIAN_POINT('Ctrl Pts',(-0.991962282340157,-7.85749414093702,
52.8216771680337));
#74276=CARTESIAN_POINT('Ctrl Pts',(-0.468143799253162,-7.89857762168305,
52.8450295200146));
#74277=CARTESIAN_POINT('Ctrl Pts',(-0.31740998614995,-7.90606989758888,
52.8516233408258));
#74278=CARTESIAN_POINT('Ctrl Pts',(0.0268727533817371,-7.91331960478729,
52.8663684716413));
#74279=CARTESIAN_POINT('Ctrl Pts',(0.220386218160189,-7.91029624748218,
52.8744283055903));
#74280=CARTESIAN_POINT('Ctrl Pts',(0.433243265201537,-7.8991523591783,52.8830446860985));
#74281=CARTESIAN_POINT('Ctrl Pts',(0.452877772139501,-7.89805099069826,
52.8838371716002));
#74282=CARTESIAN_POINT('Ctrl Pts',(0.482098716436841,-7.89630256116391,
52.8850131705834));
#74283=CARTESIAN_POINT('Ctrl Pts',(0.4916883333252,-7.89571123418149,52.8853985580329));
#74284=CARTESIAN_POINT('Ctrl Pts',(0.508135971705641,-7.89466693858191,
52.8860586211209));
#74285=CARTESIAN_POINT('Ctrl Pts',(0.514994512904093,-7.89422250059581,
52.8863335836545));
#74286=CARTESIAN_POINT('Ctrl Pts',(0.529086589694206,-7.89329088160859,
52.8868979716242));
#74287=CARTESIAN_POINT('Ctrl Pts',(0.536320053833781,-7.89280269367809,
52.8871873628878));
#74288=CARTESIAN_POINT('Ctrl Pts',(0.55304987647261,-7.89165048994534,52.8878559655194));
#74289=CARTESIAN_POINT('Ctrl Pts',(0.562545737255798,-7.8909792748233,52.888234934029));
#74290=CARTESIAN_POINT('Ctrl Pts',(0.592382539874137,-7.88881612820768,
52.8894240263736));
#74291=CARTESIAN_POINT('Ctrl Pts',(0.612719016317665,-7.88726266798573,
52.8902320764152));
#74292=CARTESIAN_POINT('Ctrl Pts',(0.902523276459386,-7.86399751489727,
52.9017130711315));
#74293=CARTESIAN_POINT('Ctrl Pts',(1.17072228710984,-7.82856510553256,52.9119080676503));
#74294=CARTESIAN_POINT('Ctrl Pts',(2.00336928413153,-7.67480390174596,52.9426431463326));
#74295=CARTESIAN_POINT('Ctrl Pts',(2.55702002818255,-7.5085116783787,52.9616069419611));
#74296=CARTESIAN_POINT('Ctrl Pts',(3.28984198859882,-7.19785283838048,52.9887598505677));
#74297=CARTESIAN_POINT('Ctrl Pts',(3.48836297319371,-7.10376396476712,52.9963625440606));
#74298=CARTESIAN_POINT('Ctrl Pts',(3.87259114025051,-6.90166583501651,53.0120368329946));
#74299=CARTESIAN_POINT('Ctrl Pts',(4.05832268135722,-6.79411192860422,53.0200880103857));
#74300=CARTESIAN_POINT('Ctrl Pts',(4.25134774694219,-6.67159368385239,53.0292244624158));
#74301=CARTESIAN_POINT('Ctrl Pts',(4.26323600133538,-6.66400320674952,53.0297903718197));
#74302=CARTESIAN_POINT('Ctrl Pts',(4.27960201795007,-6.65349202660539,53.0305739522016));
#74303=CARTESIAN_POINT('Ctrl Pts',(4.28409728606114,-6.65059847109302,53.0307896505857));
#74304=CARTESIAN_POINT('Ctrl Pts',(4.29181292319384,-6.64562093005595,53.0311606897115));
#74305=CARTESIAN_POINT('Ctrl Pts',(4.29503470564462,-6.64353916153848,53.0313158672887));
#74306=CARTESIAN_POINT('Ctrl Pts',(4.30133694051786,-6.63946044503348,53.0316198919052));
#74307=CARTESIAN_POINT('Ctrl Pts',(4.30441751994875,-6.63746369412842,53.031768724593));
#74308=CARTESIAN_POINT('Ctrl Pts',(4.3118422803706,-6.63264381609797,53.0321279747621));
#74309=CARTESIAN_POINT('Ctrl Pts',(4.31618507609126,-6.62981856695199,53.0323385458193));
#74310=CARTESIAN_POINT('Ctrl Pts',(4.3294165753983,-6.62119217204906,53.032981450937));
#74311=CARTESIAN_POINT('Ctrl Pts',(4.33829634827271,-6.61537742346586,53.0334147609935));
#74312=CARTESIAN_POINT('Ctrl Pts',(4.42642604196963,-6.55741363455715,53.0377334562708));
#74313=CARTESIAN_POINT('Ctrl Pts',(4.5047404593236,-6.50386293122169,53.0417175750196));
#74314=CARTESIAN_POINT('Ctrl Pts',(4.81583027305088,-6.2828281836619,53.0580755027561));
#74315=CARTESIAN_POINT('Ctrl Pts',(5.04037109864804,-6.10416137153501,53.0711003003043));
#74316=CARTESIAN_POINT('Ctrl Pts',(5.5935089917586,-5.61266446858285,53.1054158318387));
#74317=CARTESIAN_POINT('Ctrl Pts',(5.90583663661192,-5.28303544791031,53.1270094049721));
#74318=CARTESIAN_POINT('Ctrl Pts',(6.50065739684575,-4.536176241064,53.1709298409977));
#74319=CARTESIAN_POINT('Ctrl Pts',(6.7751177631064,-4.11501484594846,53.1929613732933));
#74320=CARTESIAN_POINT('Ctrl Pts',(7.02354706551575,-3.64072084298831,53.2147570260163));
#74321=CARTESIAN_POINT('Ctrl Pts',(7.03902599642178,-3.61070279839799,53.2161248337041));
#74322=CARTESIAN_POINT('Ctrl Pts',(7.05991704401952,-3.56954418270733,53.2179846026381));
#74323=CARTESIAN_POINT('Ctrl Pts',(7.065495816075,-3.55848889497136,53.21848260408));
#74324=CARTESIAN_POINT('Ctrl Pts',(7.074294757208,-3.54095002687094,53.2192702480707));
#74325=CARTESIAN_POINT('Ctrl Pts',(7.07753201228149,-3.53447506995757,53.2195605073411));
#74326=CARTESIAN_POINT('Ctrl Pts',(7.08378380862506,-3.52192758519965,53.2201219801343));
#74327=CARTESIAN_POINT('Ctrl Pts',(7.08679943981633,-3.51585560893245,53.2203932327728));
#74328=CARTESIAN_POINT('Ctrl Pts',(7.09394826687652,-3.50141487202013,53.2210372640555));
#74329=CARTESIAN_POINT('Ctrl Pts',(7.09807446902357,-3.49304264962655,53.2214097912304));
#74330=CARTESIAN_POINT('Ctrl Pts',(7.11024032837579,-3.46824708371784,53.2225105558616));
#74331=CARTESIAN_POINT('Ctrl Pts',(7.11823789734397,-3.45180309457151,53.2232372860618));
#74332=CARTESIAN_POINT('Ctrl Pts',(7.18105185857193,-3.32150315085255,53.2289701404294));
#74333=CARTESIAN_POINT('Ctrl Pts',(7.23319150776043,-3.20637356214731,53.2338804779716));
#74334=CARTESIAN_POINT('Ctrl Pts',(7.4032846635376,-2.80550108251657,53.2504927780781));
#74335=CARTESIAN_POINT('Ctrl Pts',(7.50724198535421,-2.51411933936105,53.2617219774346));
#74336=CARTESIAN_POINT('Ctrl Pts',(7.73444228659566,-1.73602638424405,53.290359130794));
#74337=CARTESIAN_POINT('Ctrl Pts',(7.82890567151147,-1.24241400299766,53.307155340267));
#74338=CARTESIAN_POINT('Ctrl Pts',(7.90439811097626,-0.442385861624446,
53.3357622020656));
#74339=CARTESIAN_POINT('Ctrl Pts',(7.91552699806406,-0.140195352286917,
53.3469291407129));
#74340=CARTESIAN_POINT('Ctrl Pts',(7.90884165514487,0.186400276337128,53.3599349172691));
#74341=CARTESIAN_POINT('Ctrl Pts',(7.90822638316683,0.210895337762267,53.360915255557));
#74342=CARTESIAN_POINT('Ctrl Pts',(7.90723402563431,0.244232208488808,53.3622558209888));
#74343=CARTESIAN_POINT('Ctrl Pts',(7.90695588356011,0.253076989101888,53.362612103147));
#74344=CARTESIAN_POINT('Ctrl Pts',(7.90645848343005,0.268092093812745,53.3632179539776));
#74345=CARTESIAN_POINT('Ctrl Pts',(7.90624684071046,0.274262674194214,53.3634672252617));
#74346=CARTESIAN_POINT('Ctrl Pts',(7.90582462582754,0.28616584821239,53.363948631165));
#74347=CARTESIAN_POINT('Ctrl Pts',(7.90561504169541,0.291898474336013,53.3641807276375));
#74348=CARTESIAN_POINT('Ctrl Pts',(7.90510470738206,0.305453508636284,53.3647301119666));
#74349=CARTESIAN_POINT('Ctrl Pts',(7.90479858158932,0.31327570054708,53.3650476034728));
#74350=CARTESIAN_POINT('Ctrl Pts',(7.90388051109705,0.335875916121029,53.3659662193524));
#74351=CARTESIAN_POINT('Ctrl Pts',(7.90323873353962,0.350652651154008,53.3665684526872));
#74352=CARTESIAN_POINT('Ctrl Pts',(7.89837205026681,0.455897169903193,53.3708689095517));
#74353=CARTESIAN_POINT('Ctrl Pts',(7.89263540737975,0.546286428797381,53.3746210676822));
#74354=CARTESIAN_POINT('Ctrl Pts',(7.86874012205068,0.842290098590217,53.387067609252));
#74355=CARTESIAN_POINT('Ctrl Pts',(7.84408702860321,1.04729037750051,53.3959383040296));
#74356=CARTESIAN_POINT('Ctrl Pts',(7.68816280133822,2.02084073528794,53.4387633127628));
#74357=CARTESIAN_POINT('Ctrl Pts',(7.45174956790776,2.76826869911474,53.4732321240039));
#74358=CARTESIAN_POINT('Ctrl Pts',(7.0604543846322,3.57023633092141,53.5099428916943));
#74359=CARTESIAN_POINT('Ctrl Pts',(7.00891488283892,3.6703836996937,53.5145331133996));
#74360=CARTESIAN_POINT('Ctrl Pts',(6.94248359634932,3.79296201625059,53.5201658556018));
#74361=CARTESIAN_POINT('Ctrl Pts',(6.92959341567103,3.81646098459874,53.5212463728707));
#74362=CARTESIAN_POINT('Ctrl Pts',(6.90820670300883,3.85498366065826,53.5230188048607));
#74363=CARTESIAN_POINT('Ctrl Pts',(6.89978000408404,3.87004583608858,53.5237120956994));
#74364=CARTESIAN_POINT('Ctrl Pts',(6.88452553876776,3.89710400460602,53.5249580416985));
#74365=CARTESIAN_POINT('Ctrl Pts',(6.87771554690085,3.9091099209415,53.5255110542392));
#74366=CARTESIAN_POINT('Ctrl Pts',(6.86447685888192,3.93230785170827,53.5265799306335));
#74367=CARTESIAN_POINT('Ctrl Pts',(6.85805212684565,3.94350207472681,53.5270958740905));
#74368=CARTESIAN_POINT('Ctrl Pts',(6.84002525119071,3.97473416544961,53.5285357976572));
#74369=CARTESIAN_POINT('Ctrl Pts',(6.82836246409961,3.99473693610125,53.5294585025199));
#74370=CARTESIAN_POINT('Ctrl Pts',(6.77999160323523,4.07686669739666,53.5332491282327));
#74371=CARTESIAN_POINT('Ctrl Pts',(6.74252183670718,4.13854173603428,53.5361005447936));
#74372=CARTESIAN_POINT('Ctrl Pts',(6.48716751893124,4.54617831469246,53.5549831374363));
#74373=CARTESIAN_POINT('Ctrl Pts',(6.2435849213134,4.87532101312232,53.5703565273262));
#74374=CARTESIAN_POINT('Ctrl Pts',(5.71549509033129,5.4840337500939,53.5999705865717));
#74375=CARTESIAN_POINT('Ctrl Pts',(5.43315798971549,5.76387834828152,53.6141963051885));
#74376=CARTESIAN_POINT('Ctrl Pts',(5.04834805423871,6.0917895137516,53.6329044335495));
#74377=CARTESIAN_POINT('Ctrl Pts',(4.96423891889432,6.16052341475607,53.6369588185984));
#74378=CARTESIAN_POINT('Ctrl Pts',(4.84667365193465,6.25262625973452,53.6426134061685));
#74379=CARTESIAN_POINT('Ctrl Pts',(4.81441109404637,6.27750160460581,53.6441639137852));
#74380=CARTESIAN_POINT('Ctrl Pts',(4.77433324925581,6.30791206637467,53.6460902148908));
#74381=CARTESIAN_POINT('Ctrl Pts',(4.76669790809298,6.31368384259794,53.6464572088161));
#74382=CARTESIAN_POINT('Ctrl Pts',(4.66704474683016,6.3887307547958,53.651247410089));
#74383=CARTESIAN_POINT('Ctrl Pts',(4.5735378470788,6.45600009582695,53.6557459518752));
#74384=CARTESIAN_POINT('Ctrl Pts',(4.46702348212226,6.52915150667185,53.660911534883));
#74385=CARTESIAN_POINT('Ctrl Pts',(4.45542700751392,6.53707031964908,53.661474465096));
#74386=CARTESIAN_POINT('Ctrl Pts',(4.43790791797735,6.54896520048776,53.6623258052633));
#74387=CARTESIAN_POINT('Ctrl Pts',(4.43200086830766,6.55296422914947,53.6626130133131));
#74388=CARTESIAN_POINT('Ctrl Pts',(4.42174728560898,6.55988562208506,53.6631118377694));
#74389=CARTESIAN_POINT('Ctrl Pts',(4.41740323870284,6.56281167329298,53.6633232581933));
#74390=CARTESIAN_POINT('Ctrl Pts',(4.40836473620833,6.56888676314192,53.6637633421691));
#74391=CARTESIAN_POINT('Ctrl Pts',(4.40366980646183,6.57203508738537,53.6639920437876));
#74392=CARTESIAN_POINT('Ctrl Pts',(4.39261549567194,6.57943071919132,53.6645307850083));
#74393=CARTESIAN_POINT('Ctrl Pts',(4.38625333027424,6.58367383787253,53.6648410514329));
#74394=CARTESIAN_POINT('Ctrl Pts',(4.36625231930556,6.59697125072774,53.665817111259));
#74395=CARTESIAN_POINT('Ctrl Pts',(4.35259157888546,6.60599239628847,53.6664847275573));
#74396=CARTESIAN_POINT('Ctrl Pts',(4.32067900468416,6.62692454611349,53.6680468090579));
#74397=CARTESIAN_POINT('Ctrl Pts',(4.30240576751939,6.63880264900475,53.668943153341));
#74398=CARTESIAN_POINT('Ctrl Pts',(4.23950584557569,6.67932054444794,53.6720356870173));
#74399=CARTESIAN_POINT('Ctrl Pts',(4.19464137364148,6.70758647186985,53.6742534785974));
#74400=CARTESIAN_POINT('Ctrl Pts',(4.03520075710186,6.80581352501613,53.6821687202132));
#74401=CARTESIAN_POINT('Ctrl Pts',(3.91913514584814,6.8733048582457,53.6879911051885));
#74402=CARTESIAN_POINT('Ctrl Pts',(3.46989365111189,7.11945649961404,53.7106099671231));
#74403=CARTESIAN_POINT('Ctrl Pts',(3.12579149397269,7.27710318875198,53.7280863387573));
#74404=CARTESIAN_POINT('Ctrl Pts',(2.1275130586585,7.65053823675228,53.7772049572006));
#74405=CARTESIAN_POINT('Ctrl Pts',(1.45449039770815,7.80652220677552,53.8082509850101));
#74406=CARTESIAN_POINT('Ctrl Pts',(0.724926364022209,7.87784407095908,53.8382418648805));
#74407=CARTESIAN_POINT('Ctrl Pts',(0.68010908490133,7.88183970631151,53.8400712356032));
#74408=CARTESIAN_POINT('Ctrl Pts',(0.620698786063482,7.88662585728166,53.8424793844219));
#74409=CARTESIAN_POINT('Ctrl Pts',(0.60613461920027,7.88775856768057,53.8430683891811));
#74410=CARTESIAN_POINT('Ctrl Pts',(0.583500680351651,7.88945583631006,53.8439816816215));
#74411=CARTESIAN_POINT('Ctrl Pts',(0.575433073546684,7.89004836584681,53.8443068056817));
#74412=CARTESIAN_POINT('Ctrl Pts',(0.559266933697071,7.89121076941868,53.8449574850958));
#74413=CARTESIAN_POINT('Ctrl Pts',(0.551168403710126,7.89178055331999,53.8452830373867));
#74414=CARTESIAN_POINT('Ctrl Pts',(0.533068559891482,7.89302599721397,53.846009720431));
#74415=CARTESIAN_POINT('Ctrl Pts',(0.523066802445153,7.89369511720152,53.8464106550906));
#74416=CARTESIAN_POINT('Ctrl Pts',(0.49375888117962,7.89559987717363,53.8475836937924));
#74417=CARTESIAN_POINT('Ctrl Pts',(0.474449365073108,7.89678371615031,53.8483542480299));
#74418=CARTESIAN_POINT('Ctrl Pts',(0.33140770431331,7.90502684172079,53.854045542609));
#74419=CARTESIAN_POINT('Ctrl Pts',(0.207526386493655,7.90924869165333,53.8588808247702));
#74420=CARTESIAN_POINT('Ctrl Pts',(-0.198806816706126,7.91354255136767,
53.8744659897639));
#74421=CARTESIAN_POINT('Ctrl Pts',(-0.481174984656377,7.90140272751994,
53.8848540347579));
#74422=CARTESIAN_POINT('Ctrl Pts',(-1.0031671302955,7.85086849885042,53.903606225286));
#74423=CARTESIAN_POINT('Ctrl Pts',(-1.24283899647044,7.81651047139906,53.9120394342415));
#74424=CARTESIAN_POINT('Ctrl Pts',(-1.68824732699333,7.73165186501636,53.9277301144796));
#74425=CARTESIAN_POINT('Ctrl Pts',(-1.89426142536727,7.68377462359536,53.93499628928));
#74426=CARTESIAN_POINT('Ctrl Pts',(-2.51966507277599,7.5117483989968,53.9575561170548));
#74427=CARTESIAN_POINT('Ctrl Pts',(-2.9308788117101,7.36104718615563,53.9731012009326));
#74428=CARTESIAN_POINT('Ctrl Pts',(-3.36013568333052,7.16203192480498,53.9917897435393));
#74429=CARTESIAN_POINT('Ctrl Pts',(-3.39264328892988,7.14669046204214,53.9932198138907));
#74430=CARTESIAN_POINT('Ctrl Pts',(-3.43565905053655,7.12603020895244,53.9951308167761));
#74431=CARTESIAN_POINT('Ctrl Pts',(-3.44626182499317,7.12090858543764,53.9956033652411));
#74432=CARTESIAN_POINT('Ctrl Pts',(-3.46273726587431,7.11290478091368,53.9963399639399));
#74433=CARTESIAN_POINT('Ctrl Pts',(-3.4686178839139,7.11003894292507,53.9966033397048));
#74434=CARTESIAN_POINT('Ctrl Pts',(-3.48040969550706,7.10427425547591,53.9971323746931));
#74435=CARTESIAN_POINT('Ctrl Pts',(-3.48632083828782,7.10137531452811,53.9973980375087));
#74436=CARTESIAN_POINT('Ctrl Pts',(-3.49954463668613,7.09486961258578,53.9979933747893));
#74437=CARTESIAN_POINT('Ctrl Pts',(-3.50685534406378,7.09125892059902,53.998323205855));
#74438=CARTESIAN_POINT('Ctrl Pts',(-3.52833437565151,7.0806092832481,53.9992942973704));
#74439=CARTESIAN_POINT('Ctrl Pts',(-3.54248714022144,7.07353915275968,53.9999367739565));
#74440=CARTESIAN_POINT('Ctrl Pts',(-3.64910413194198,7.01987752311238,54.0047960190748));
#74441=CARTESIAN_POINT('Ctrl Pts',(-3.7406649877458,6.97151819039129,54.009078498709));
#74442=CARTESIAN_POINT('Ctrl Pts',(-3.96642623023701,6.84655067030594,54.0198723669699));
#74443=CARTESIAN_POINT('Ctrl Pts',(-4.09938078832613,6.76778163993273,54.0264403679699));
#74444=CARTESIAN_POINT('Ctrl Pts',(-4.46888130553644,6.53398583364339,54.0451730440766));
#74445=CARTESIAN_POINT('Ctrl Pts',(-4.69954407027545,6.37009860807926,54.0574360640011));
#74446=CARTESIAN_POINT('Ctrl Pts',(-5.21290431051258,5.96226432200247,54.0856922095261));
#74447=CARTESIAN_POINT('Ctrl Pts',(-5.48811496946418,5.70995437245114,54.1015764354976));
#74448=CARTESIAN_POINT('Ctrl Pts',(-6.01396375523818,5.15458564779419,54.1335084954059));
#74449=CARTESIAN_POINT('Ctrl Pts',(-6.26190347264958,4.8503699500397,54.1495159072819));
#74450=CARTESIAN_POINT('Ctrl Pts',(-6.53224800613117,4.46319444551995,54.1686794611109));
#74451=CARTESIAN_POINT('Ctrl Pts',(-6.57721326679625,4.39666173741613,54.1719296470516));
#74452=CARTESIAN_POINT('Ctrl Pts',(-6.63885337734816,4.30239378809915,54.1764750473568));
#74453=CARTESIAN_POINT('Ctrl Pts',(-6.65638265827357,4.27522354841571,54.1777783156152));
#74454=CARTESIAN_POINT('Ctrl Pts',(-6.68810605806227,4.22538443785885,54.1801565568393));
#74455=CARTESIAN_POINT('Ctrl Pts',(-6.70235272579781,4.20274960419499,54.1812320372807));
#74456=CARTESIAN_POINT('Ctrl Pts',(-6.72939248492138,4.15930217489664,54.1832876475169));
#74457=CARTESIAN_POINT('Ctrl Pts',(-6.74220448772337,4.13850171533463,54.1842679599424));
#74458=CARTESIAN_POINT('Ctrl Pts',(-6.76881186979394,4.0948527708737,54.1863171976192));
#74459=CARTESIAN_POINT('Ctrl Pts',(-6.78258838935449,4.07199313476207,54.1873859165957));
#74460=CARTESIAN_POINT('Ctrl Pts',(-6.82920101787034,3.99375504928013,54.1910284636642));
#74461=CARTESIAN_POINT('Ctrl Pts',(-6.86147678863256,3.93804549094485,54.1935963043661));
#74462=CARTESIAN_POINT('Ctrl Pts',(-7.04277400090847,3.61612097466104,54.2082913735722));
#74463=CARTESIAN_POINT('Ctrl Pts',(-7.17697852327385,3.34185310626648,54.2202433760427));
#74464=CARTESIAN_POINT('Ctrl Pts',(-7.38100014548717,2.85554958851309,54.2407348643938));
#74465=CARTESIAN_POINT('Ctrl Pts',(-7.45831444676199,2.64704982734854,54.2493135582315));
#74466=CARTESIAN_POINT('Ctrl Pts',(-7.59110386877714,2.23668517189618,54.2659907290016));
#74467=CARTESIAN_POINT('Ctrl Pts',(-7.64755222543076,2.03532839821273,54.2740812776687));
#74468=CARTESIAN_POINT('Ctrl Pts',(-7.73100335081559,1.68475791503657,54.2881900296456));
#74469=CARTESIAN_POINT('Ctrl Pts',(-7.76181550329163,1.53656777831262,54.2941613465935));
#74470=CARTESIAN_POINT('Ctrl Pts',(-7.79254206089766,1.36410346536889,54.301172482047));
#74471=CARTESIAN_POINT('Ctrl Pts',(-7.79661987037615,1.34060009833285,54.3021292828589));
#74472=CARTESIAN_POINT('Ctrl Pts',(-7.80297700014814,1.30294906815448,54.3036644465768));
#74473=CARTESIAN_POINT('Ctrl Pts',(-7.80532430100294,1.28881297840809,54.3042413703818));
#74474=CARTESIAN_POINT('Ctrl Pts',(-7.8094172057597,1.26374305178853,54.3052655684844));
#74475=CARTESIAN_POINT('Ctrl Pts',(-7.8111782892817,1.25281176826412,54.3057125018919));
#74476=CARTESIAN_POINT('Ctrl Pts',(-7.8145141071538,1.23182541496056,54.3065712535174));
#74477=CARTESIAN_POINT('Ctrl Pts',(-7.8160923982823,1.22177092968828,54.3069829905181));
#74478=CARTESIAN_POINT('Ctrl Pts',(-7.81942895124563,1.20024438175734,54.3078652153464));
#74479=CARTESIAN_POINT('Ctrl Pts',(-7.82118137950966,1.18877143634277,54.3083358383264));
#74480=CARTESIAN_POINT('Ctrl Pts',(-7.82535396814674,1.16104534543449,54.3094742465409));
#74481=CARTESIAN_POINT('Ctrl Pts',(-7.82774874154296,1.14478847701366,54.3101426239251));
#74482=CARTESIAN_POINT('Ctrl Pts',(-7.83962387873191,1.06239465916568,54.3135343609423));
#74483=CARTESIAN_POINT('Ctrl Pts',(-7.84831668596023,0.996147572399339,
54.316275216298));
#74484=CARTESIAN_POINT('Ctrl Pts',(-7.89254157309554,0.622477371073265,
54.3317951551681));
#74485=CARTESIAN_POINT('Ctrl Pts',(-7.91084855024879,0.313295554748577,
54.3448544452596));
#74486=CARTESIAN_POINT('Ctrl Pts',(-7.9109990642057,0.0038478742852386,
54.3579070163678));
#74487=CARTESIAN_POINT('',(-7.90853756536093,-0.0002840522667073,56.3576029905152));
#74488=CARTESIAN_POINT('Ctrl Pts',(-7.91058521897938,0.00383761197256053,
54.357668491763));
#74489=CARTESIAN_POINT('Ctrl Pts',(-7.90804771810951,-0.914391017526965,
54.3946791517166));
#74490=CARTESIAN_POINT('Ctrl Pts',(-7.51315483011075,-3.14994018213361,
54.4846110786474));
#74491=CARTESIAN_POINT('Ctrl Pts',(-4.71476302132917,-7.33335162650933,
54.6803855395325));
#74492=CARTESIAN_POINT('Ctrl Pts',(2.51764341483423,-9.0087265231168,54.9449918744182));
#74493=CARTESIAN_POINT('Ctrl Pts',(8.94941253689187,-2.74473022419253,55.2625194762814));
#74494=CARTESIAN_POINT('Ctrl Pts',(7.44143434588096,4.5419721744467,55.5271258111673));
#74495=CARTESIAN_POINT('Ctrl Pts',(3.00563183108329,7.65784328303428,55.7388108790757));
#74496=CARTESIAN_POINT('Ctrl Pts',(-2.39221485231201,8.3907978832337,55.9504959469847));
#74497=CARTESIAN_POINT('Ctrl Pts',(-7.0727487270325,5.01925377135236,56.1567599841309));
#74498=CARTESIAN_POINT('Ctrl Pts',(-7.91074264020192,1.18409319209995,56.3101027543002));
#74499=CARTESIAN_POINT('Ctrl Pts',(-7.90853756536093,-0.0002840522667073,
56.3576029905152));
#74500=CARTESIAN_POINT('',(-7.911,4.61852778244065E-13,58.357668491763));
#74501=CARTESIAN_POINT('Ctrl Pts',(-7.91099999456027,-0.000285742256253543,
56.3576799889967));
#74502=CARTESIAN_POINT('Ctrl Pts',(-7.91091617089283,-2.20186489793695,
56.4462635923182));
#74503=CARTESIAN_POINT('Ctrl Pts',(-6.94207516543246,-4.38616811721652,
56.5348471956396));
#74504=CARTESIAN_POINT('Ctrl Pts',(-3.67820201488314,-7.34180684107615,
56.7120182346939));
#74505=CARTESIAN_POINT('Ctrl Pts',(-1.40868175871789,-8.08992666571325,
56.8006056704266));
#74506=CARTESIAN_POINT('Ctrl Pts',(2.97309270521207,-7.6545422802528,56.9777805418921));
#74507=CARTESIAN_POINT('Ctrl Pts',(5.05102072675534,-6.47444880834275,57.0663679776248));
#74508=CARTESIAN_POINT('Ctrl Pts',(7.6695151884783,-2.93425195367807,57.2435428490902));
#74509=CARTESIAN_POINT('Ctrl Pts',(8.18956872247059,-0.601881960100388,
57.3321302848229));
#74510=CARTESIAN_POINT('Ctrl Pts',(7.32306689761406,3.71537198232318,57.5093051562884));
#74511=CARTESIAN_POINT('Ctrl Pts',(5.9432995885031,5.66643518936392,57.5978925920211));
#74512=CARTESIAN_POINT('Ctrl Pts',(2.16154501638024,7.92205913232946,57.7750674634865));
#74513=CARTESIAN_POINT('Ctrl Pts',(-0.210816529298383,8.20894963713004,
57.8636548992193));
#74514=CARTESIAN_POINT('Ctrl Pts',(-4.42123908576248,6.91982244717948,58.0408297706847));
#74515=CARTESIAN_POINT('Ctrl Pts',(-6.22631625634031,5.35390358803698,58.1294172064174));
#74516=CARTESIAN_POINT('Ctrl Pts',(-7.65317280859446,2.31334857514692,58.2645592586878));
#74517=CARTESIAN_POINT('Ctrl Pts',(-7.91099999999993,1.1570283783663,58.3111138752254));
#74518=CARTESIAN_POINT('Ctrl Pts',(-7.911,4.61852778244065E-13,58.357668491763));
#74519=CARTESIAN_POINT('',(-3.42067962509687,7.13322310757536,60.));
#74520=CARTESIAN_POINT('Ctrl Pts',(-7.911,4.61852778244065E-13,58.357668491763));
#74521=CARTESIAN_POINT('Ctrl Pts',(-7.91100000000013,-2.20167589666633,
58.4462559274957));
#74522=CARTESIAN_POINT('Ctrl Pts',(-6.94214576672394,-4.38610418338648,
58.5348433632284));
#74523=CARTESIAN_POINT('Ctrl Pts',(-3.67820201488319,-7.34180684107617,
58.7120182346939));
#74524=CARTESIAN_POINT('Ctrl Pts',(-1.40868175871776,-8.08992666571332,
58.8006056704266));
#74525=CARTESIAN_POINT('Ctrl Pts',(2.97309270521249,-7.65454228025267,58.9777805418921));
#74526=CARTESIAN_POINT('Ctrl Pts',(5.05102072675585,-6.4744488083424,59.0663679776248));
#74527=CARTESIAN_POINT('Ctrl Pts',(7.66951518847866,-2.93425195367724,59.2435428490902));
#74528=CARTESIAN_POINT('Ctrl Pts',(8.18956872247071,-0.601881960099315,
59.332130284823));
#74529=CARTESIAN_POINT('Ctrl Pts',(7.32306689761348,3.71537198232442,59.5093051562884));
#74530=CARTESIAN_POINT('Ctrl Pts',(5.94329958850206,5.66643518936507,59.5978925920212));
#74531=CARTESIAN_POINT('Ctrl Pts',(2.16154501637848,7.92205913232998,59.7750674634866));
#74532=CARTESIAN_POINT('Ctrl Pts',(-0.210816529300396,8.20894963713003,
59.8636548992193));
#74533=CARTESIAN_POINT('Ctrl Pts',(-2.69433568776147,7.44855753134885,59.9681615566347));
#74534=CARTESIAN_POINT('Ctrl Pts',(-3.06393494046689,7.30429714460912,59.9840807783173));
#74535=CARTESIAN_POINT('Ctrl Pts',(-3.42067962509687,7.13322310757536,60.));
#74536=CARTESIAN_POINT('',(3.4206796250979,7.13322310757487,60.));
#74537=CARTESIAN_POINT('Origin',(0.,0.,60.));
#74538=CARTESIAN_POINT('',(-7.91099785401453,-0.00429578758769514,58.6423315082368));
#74539=CARTESIAN_POINT('Ctrl Pts',(3.42067962509791,7.13322310757487,60.));
#74540=CARTESIAN_POINT('Ctrl Pts',(3.6144969028105,7.04027959482263,59.9913511809908));
#74541=CARTESIAN_POINT('Ctrl Pts',(3.80447822695433,6.93945490373599,59.9827023619817));
#74542=CARTESIAN_POINT('Ctrl Pts',(3.99001435172825,6.83108384321277,59.9740535429726));
#74543=CARTESIAN_POINT('Ctrl Pts',(4.17560503493687,6.72268091528133,59.9654021807066));
#74544=CARTESIAN_POINT('Ctrl Pts',(4.35674770625185,6.60672730486513,59.9567508184406));
#74545=CARTESIAN_POINT('Ctrl Pts',(4.53285999276488,6.48360249290405,59.9480994561746));
#74546=CARTESIAN_POINT('Ctrl Pts',(4.71414100545881,6.35686408616373,59.939194184749));
#74547=CARTESIAN_POINT('Ctrl Pts',(4.89009165777409,6.22252729526204,59.9302889133236));
#74548=CARTESIAN_POINT('Ctrl Pts',(5.06011034746729,6.08105289168368,59.9213836418981));
#74549=CARTESIAN_POINT('Ctrl Pts',(5.22528660057382,5.94360793233408,59.9127320085417));
#74550=CARTESIAN_POINT('Ctrl Pts',(5.38486395990082,5.79942650828154,59.9040803751852));
#74551=CARTESIAN_POINT('Ctrl Pts',(5.53832440683672,5.64897192103454,59.8954287418289));
#74552=CARTESIAN_POINT('Ctrl Pts',(5.69853330400857,5.49190106676187,59.8863966513688));
#74553=CARTESIAN_POINT('Ctrl Pts',(5.85207498129762,5.32799306622592,59.8773645609088));
#74554=CARTESIAN_POINT('Ctrl Pts',(5.99840172750653,5.15781908517996,59.8683324704487));
#74555=CARTESIAN_POINT('Ctrl Pts',(6.14472847371554,4.98764510413389,59.8593003799887));
#74556=CARTESIAN_POINT('Ctrl Pts',(6.28384008499756,4.81120535093508,59.8502682895286));
#74557=CARTESIAN_POINT('Ctrl Pts',(6.41523454138166,4.62911295812315,59.8412361990686));
#74558=CARTESIAN_POINT('Ctrl Pts',(6.52959511341658,4.47062689426438,59.8333750224245));
#74559=CARTESIAN_POINT('Ctrl Pts',(6.63814345897899,4.30781131701357,59.8255138457805));
#74560=CARTESIAN_POINT('Ctrl Pts',(6.74054212213741,4.14113666759397,59.8176526691365));
#74561=CARTESIAN_POINT('Ctrl Pts',(6.84290875318325,3.97451415695206,59.8097939516075));
#74562=CARTESIAN_POINT('Ctrl Pts',(6.93912935186777,3.80403527535238,59.8019352340786));
#74563=CARTESIAN_POINT('Ctrl Pts',(7.02890993359229,3.63019918812283,59.7940765165496));
#74564=CARTESIAN_POINT('Ctrl Pts',(7.11867789852752,3.45638752993173,59.7862189033995));
#74565=CARTESIAN_POINT('Ctrl Pts',(7.20200749057793,3.2792199158393,59.7783612902495));
#74566=CARTESIAN_POINT('Ctrl Pts',(7.27865072156316,3.09922001050071,59.7705036770995));
#74567=CARTESIAN_POINT('Ctrl Pts',(7.35531794692297,2.9191637533474,59.7626436039995));
#74568=CARTESIAN_POINT('Ctrl Pts',(7.42529448864377,2.73627375252924,59.7547835308995));
#74569=CARTESIAN_POINT('Ctrl Pts',(7.4883802965523,2.55109418371947,59.7469234577995));
#74570=CARTESIAN_POINT('Ctrl Pts',(7.55147576688006,2.36588625222899,59.7390621808261));
#74571=CARTESIAN_POINT('Ctrl Pts',(7.60767829403273,2.17838838584624,59.7312009038528));
#74572=CARTESIAN_POINT('Ctrl Pts',(7.65683766736361,1.98916010809633,59.7233396268795));
#74573=CARTESIAN_POINT('Ctrl Pts',(7.70603329081186,1.79979229343183,59.7154725530012));
#74574=CARTESIAN_POINT('Ctrl Pts',(7.74817530282766,1.60869185706849,59.707605479123));
#74575=CARTESIAN_POINT('Ctrl Pts',(7.78316440777624,1.41642959638844,59.6997384052448));
#74576=CARTESIAN_POINT('Ctrl Pts',(7.80876147830464,1.27577579418892,59.6939830695421));
#74577=CARTESIAN_POINT('Ctrl Pts',(7.83053139013534,1.13450041533383,59.6882277338395));
#74578=CARTESIAN_POINT('Ctrl Pts',(7.84845284800453,0.992828732788119,59.6824723981369));
#74579=CARTESIAN_POINT('Ctrl Pts',(7.87625500018793,0.77304875132874,59.6735439549132));
#74580=CARTESIAN_POINT('Ctrl Pts',(7.89481335201341,0.552161752406579,59.6646155116895));
#74581=CARTESIAN_POINT('Ctrl Pts',(7.90407626183148,0.330907006804204,59.6556870684658));
#74582=CARTESIAN_POINT('Ctrl Pts',(7.913341078962,0.109606702955013,59.6467567867991));
#74583=CARTESIAN_POINT('Ctrl Pts',(7.91330662441942,-0.112061320222985,
59.6378265051325));
#74584=CARTESIAN_POINT('Ctrl Pts',(7.90397335127518,-0.333356059389596,
59.6288962234659));
#74585=CARTESIAN_POINT('Ctrl Pts',(7.89464653280444,-0.554497756288547,
59.6199721177733));
#74586=CARTESIAN_POINT('Ctrl Pts',(7.8760337594932,-0.775266507043604,59.6110480120807));
#74587=CARTESIAN_POINT('Ctrl Pts',(7.84818748145735,-0.994924246310342,
59.6021239063881));
#74588=CARTESIAN_POINT('Ctrl Pts',(7.82036631196139,-1.2143839237354,59.5932078474177));
#74589=CARTESIAN_POINT('Ctrl Pts',(7.78332829005007,-1.43273441374617,59.5842917884473));
#74590=CARTESIAN_POINT('Ctrl Pts',(7.73717753193906,-1.64924371736181,59.5753757294769));
#74591=CARTESIAN_POINT('Ctrl Pts',(7.69113148038629,-1.86526180599125,59.5664798992066));
#74592=CARTESIAN_POINT('Ctrl Pts',(7.63601401610708,-2.07944687526408,59.5575840689364));
#74593=CARTESIAN_POINT('Ctrl Pts',(7.57197991055836,-2.29107861805322,59.5486882386661));
#74594=CARTESIAN_POINT('Ctrl Pts',(7.51204362770563,-2.48916711929377,59.5403616915126));
#74595=CARTESIAN_POINT('Ctrl Pts',(7.44429588276699,-2.68501857300424,59.532035144359));
#74596=CARTESIAN_POINT('Ctrl Pts',(7.36890430184754,-2.87804975464511,59.5237085972055));
#74597=CARTESIAN_POINT('Ctrl Pts',(7.29691304211312,-3.06237481806564,59.5157575950974));
#74598=CARTESIAN_POINT('Ctrl Pts',(7.21798301215634,-3.24404497807909,59.5078065929893));
#74599=CARTESIAN_POINT('Ctrl Pts',(7.13234293140335,-3.42251447168024,59.4998555908812));
#74600=CARTESIAN_POINT('Ctrl Pts',(7.04671046143499,-3.60096810480033,59.4919052953741));
#74601=CARTESIAN_POINT('Ctrl Pts',(6.95436927559734,-3.77622133369333,59.483954999867));
#74602=CARTESIAN_POINT('Ctrl Pts',(6.85559526707494,-3.94775056634277,59.4760047043599));
#74603=CARTESIAN_POINT('Ctrl Pts',(6.75681432711654,-4.11929183600394,59.4680538509432));
#74604=CARTESIAN_POINT('Ctrl Pts',(6.65159983424772,-4.28710829600644,59.4601029975266));
#74605=CARTESIAN_POINT('Ctrl Pts',(6.54027262080183,-4.45070275862026,59.4521521441099));
#74606=CARTESIAN_POINT('Ctrl Pts',(6.42888006511491,-4.6143932411422,59.4441966240303));
#74607=CARTESIAN_POINT('Ctrl Pts',(6.31136781008364,-4.77385649474633,59.4362411039507));
#74608=CARTESIAN_POINT('Ctrl Pts',(6.1880994011085,-4.92862524462965,59.4282855838711));
#74609=CARTESIAN_POINT('Ctrl Pts',(6.06479256849094,-5.08344223703635,59.4203275839991));
#74610=CARTESIAN_POINT('Ctrl Pts',(5.93572622138635,-5.23356154866874,59.4123695841271));
#74611=CARTESIAN_POINT('Ctrl Pts',(5.80130319447833,-5.37855019923916,59.4044115842551));
#74612=CARTESIAN_POINT('Ctrl Pts',(5.66675620563104,-5.52367255513306,59.3964462456919));
#74613=CARTESIAN_POINT('Ctrl Pts',(5.52684290303172,-5.66365455413246,59.3884809071287));
#74614=CARTESIAN_POINT('Ctrl Pts',(5.38200266167046,-5.79810040873493,59.3805155685654));
#74615=CARTESIAN_POINT('Ctrl Pts',(5.28762398171985,-5.88570605039196,59.3753253111349));
#74616=CARTESIAN_POINT('Ctrl Pts',(5.19115408975717,-5.9709618953036,59.3701350537044));
#74617=CARTESIAN_POINT('Ctrl Pts',(5.092721828791,-6.05376786592909,59.3649447962739));
#74618=CARTESIAN_POINT('Ctrl Pts',(4.94082909758122,-6.18154736540747,59.3569356093563));
#74619=CARTESIAN_POINT('Ctrl Pts',(4.7839914327906,-6.30371885951764,59.3489264224387));
#74620=CARTESIAN_POINT('Ctrl Pts',(4.62265619092145,-6.41988868599259,59.3409172355211));
#74621=CARTESIAN_POINT('Ctrl Pts',(4.4614459590171,-6.53596849874362,59.3329142544899));
#74622=CARTESIAN_POINT('Ctrl Pts',(4.29574536459703,-6.64605571840741,59.3249112734586));
#74623=CARTESIAN_POINT('Ctrl Pts',(4.12603491430888,-6.74979680330483,59.3169082924273));
#74624=CARTESIAN_POINT('Ctrl Pts',(3.95642764726029,-6.85347481405922,59.3089101771749));
#74625=CARTESIAN_POINT('Ctrl Pts',(3.78281566708038,-6.95081420759235,59.3009120619224));
#74626=CARTESIAN_POINT('Ctrl Pts',(3.60570889961232,-7.04150440823951,59.29291394667));
#74627=CARTESIAN_POINT('Ctrl Pts',(3.42868027581228,-7.13215459423883,59.2849193603739));
#74628=CARTESIAN_POINT('Ctrl Pts',(3.24816023449609,-7.21616128422545,59.2769247740778));
#74629=CARTESIAN_POINT('Ctrl Pts',(3.06468414449047,-7.29325936015639,59.2689301877818));
#74630=CARTESIAN_POINT('Ctrl Pts',(2.88125842054413,-7.37033627187861,59.2609377960813));
#74631=CARTESIAN_POINT('Ctrl Pts',(2.69487857250448,-7.44050822182869,59.2529454043807));
#74632=CARTESIAN_POINT('Ctrl Pts',(2.50610122433952,-7.50355766642491,59.2449530126802));
#74633=CARTESIAN_POINT('Ctrl Pts',(2.31169608808739,-7.56848672696366,59.2367223535857));
#74634=CARTESIAN_POINT('Ctrl Pts',(2.11474863075838,-7.62586189743682,59.2284916944911));
#74635=CARTESIAN_POINT('Ctrl Pts',(1.91588563862165,-7.67550019345471,59.2202610353966));
#74636=CARTESIAN_POINT('Ctrl Pts',(1.72274030109593,-7.72371130269914,59.2122670219715));
#74637=CARTESIAN_POINT('Ctrl Pts',(1.52778839519012,-7.76462421241166,59.2042730085466));
#74638=CARTESIAN_POINT('Ctrl Pts',(1.33161656030211,-7.79812274437439,59.1962789951216));
#74639=CARTESIAN_POINT('Ctrl Pts',(1.13539687205975,-7.83162944783188,59.1882830316696));
#74640=CARTESIAN_POINT('Ctrl Pts',(0.937956989962921,-7.85771811123421,
59.1802870682177));
#74641=CARTESIAN_POINT('Ctrl Pts',(0.739891227397327,-7.87632414084264,
59.1722911047658));
#74642=CARTESIAN_POINT('Ctrl Pts',(0.541747183716112,-7.89493752407309,
59.164291981086));
#74643=CARTESIAN_POINT('Ctrl Pts',(0.342977097954888,-7.90606234616173,
59.1562928574063));
#74644=CARTESIAN_POINT('Ctrl Pts',(0.144178255435468,-7.90968606397622,
59.1482937337265));
#74645=CARTESIAN_POINT('Ctrl Pts',(-0.0647419135745792,-7.91349427396705,
59.1398873554502));
#74646=CARTESIAN_POINT('Ctrl Pts',(-0.273693419980003,-7.90901767035084,
59.1314809771739));
#74647=CARTESIAN_POINT('Ctrl Pts',(-0.481986362343147,-7.89630357487066,
59.1230745988976));
#74648=CARTESIAN_POINT('Ctrl Pts',(-0.680540574478752,-7.88418392654056,
59.1150612605836));
#74649=CARTESIAN_POINT('Ctrl Pts',(-0.878496077585479,-7.86457956597611,
59.1070479222697));
#74650=CARTESIAN_POINT('Ctrl Pts',(-1.07526337780495,-7.83758442814822,
59.0990345839557));
#74651=CARTESIAN_POINT('Ctrl Pts',(-1.27217167258296,-7.81056994682405,
59.0910155036455));
#74652=CARTESIAN_POINT('Ctrl Pts',(-1.46788973933417,-7.77615418291552,
59.0829964233353));
#74653=CARTESIAN_POINT('Ctrl Pts',(-1.66183968641545,-7.73448187383322,
59.0749773430251));
#74654=CARTESIAN_POINT('Ctrl Pts',(-1.85603937954027,-7.69275590402826,
59.0669479366818));
#74655=CARTESIAN_POINT('Ctrl Pts',(-2.04846608396256,-7.6437548073047,59.0589185303385));
#74656=CARTESIAN_POINT('Ctrl Pts',(-2.23855734038304,-7.58767303155699,
59.0508891239951));
#74657=CARTESIAN_POINT('Ctrl Pts',(-2.26595593951001,-7.57958974502938,
59.0497318141337));
#74658=CARTESIAN_POINT('Ctrl Pts',(-2.29330605522693,-7.5713594416439,59.0485745042723));
#74659=CARTESIAN_POINT('Ctrl Pts',(-2.32060603944214,-7.56298278523128,
59.0474171944108));
#74660=CARTESIAN_POINT('Ctrl Pts',(-2.50330547103492,-7.50692376508056,
59.0396721403407));
#74661=CARTESIAN_POINT('Ctrl Pts',(-2.68430227468656,-7.44413919422109,
59.0319270862705));
#74662=CARTESIAN_POINT('Ctrl Pts',(-2.86304941426585,-7.37474535502562,
59.0241820322003));
#74663=CARTESIAN_POINT('Ctrl Pts',(-3.04157977881897,-7.30543567298837,
59.0164463709199));
#74664=CARTESIAN_POINT('Ctrl Pts',(-3.2178655779645,-7.22953280398241,59.0087107096395));
#74665=CARTESIAN_POINT('Ctrl Pts',(-3.39137161991687,-7.14720361649382,
59.0009750483591));
#74666=CARTESIAN_POINT('Ctrl Pts',(-3.56470271607927,-7.06495744135791,
58.9932471869302));
#74667=CARTESIAN_POINT('Ctrl Pts',(-3.7352593116472,-6.97629799864975,58.9855193255014));
#74668=CARTESIAN_POINT('Ctrl Pts',(-3.90252292868786,-6.88144140359166,
58.9777914640725));
#74669=CARTESIAN_POINT('Ctrl Pts',(-4.06965203187759,-6.78666109246258,
58.9700698174106));
#74670=CARTESIAN_POINT('Ctrl Pts',(-4.23349311703626,-6.68569372735895,
58.9623481707487));
#74671=CARTESIAN_POINT('Ctrl Pts',(-4.39354913597794,-6.57880285384412,
58.9546265240868));
#74672=CARTESIAN_POINT('Ctrl Pts',(-4.55350906375469,-6.47197615328962,
58.9469095131895));
#74673=CARTESIAN_POINT('Ctrl Pts',(-4.70968815124361,-6.35923322465589,
58.9391925022922));
#74674=CARTESIAN_POINT('Ctrl Pts',(-4.86161529483965,-6.24088276808507,
58.9314754913948));
#74675=CARTESIAN_POINT('Ctrl Pts',(-5.01348217065545,-6.12257925980236,
58.9237615417485));
#74676=CARTESIAN_POINT('Ctrl Pts',(-5.16110017782105,-5.99867287476642,
58.9160475921022));
#74677=CARTESIAN_POINT('Ctrl Pts',(-5.30402842574628,-5.86951475497553,
58.9083336424558));
#74678=CARTESIAN_POINT('Ctrl Pts',(-5.44695652514239,-5.74035676940402,
58.9006197008257));
#74679=CARTESIAN_POINT('Ctrl Pts',(-5.58519459979148,-5.60594729289418,
58.8929057591956));
#74680=CARTESIAN_POINT('Ctrl Pts',(-5.71833572041561,-5.46667701520941,
58.8851918175655));
#74681=CARTESIAN_POINT('Ctrl Pts',(-5.85148343683082,-5.32739983809605,
58.8774774937879));
#74682=CARTESIAN_POINT('Ctrl Pts',(-5.97953344640783,-5.18326164036616,
58.8697631700103));
#74683=CARTESIAN_POINT('Ctrl Pts',(-6.10211664965986,-5.03468900667598,
58.8620488462326));
#74684=CARTESIAN_POINT('Ctrl Pts',(-6.22472853604888,-4.8860816086046,58.8543327173871));
#74685=CARTESIAN_POINT('Ctrl Pts',(-6.34187083937764,-4.7330379865422,58.8466165885416));
#74686=CARTESIAN_POINT('Ctrl Pts',(-6.45321560781147,-4.5760167524932,58.8389004596961));
#74687=CARTESIAN_POINT('Ctrl Pts',(-6.5646069752631,-4.41892980332006,58.8311811015652));
#74688=CARTESIAN_POINT('Ctrl Pts',(-6.67019576834552,-4.25786222139797,
58.8234617434344));
#74689=CARTESIAN_POINT('Ctrl Pts',(-6.76969809502244,-4.09330046566943,
58.8157423853036));
#74690=CARTESIAN_POINT('Ctrl Pts',(-6.86931999294081,-3.92854095724419,
58.8080137508747));
#74691=CARTESIAN_POINT('Ctrl Pts',(-6.96284063123002,-3.76027919802655,
58.8002851164459));
#74692=CARTESIAN_POINT('Ctrl Pts',(-7.05002224248504,-3.58902596542101,
58.792556482017));
#74693=CARTESIAN_POINT('Ctrl Pts',(-7.13726074137302,-3.41766098687617,
58.7848228045096));
#74694=CARTESIAN_POINT('Ctrl Pts',(-7.21815182366781,-3.24330097270297,
58.7770891270021));
#74695=CARTESIAN_POINT('Ctrl Pts',(-7.2925064651054,-3.0664752495978,58.7693554494947));
#74696=CARTESIAN_POINT('Ctrl Pts',(-7.36697586468091,-2.88937661561139,
58.7616098359142));
#74697=CARTESIAN_POINT('Ctrl Pts',(-7.4348885487445,-2.70980500805425,58.7538642223338));
#74698=CARTESIAN_POINT('Ctrl Pts',(-7.49610545161038,-2.52830458179729,
58.7461186087533));
#74699=CARTESIAN_POINT('Ctrl Pts',(-7.53886040783258,-2.40154150794612,
58.7407089366849));
#74700=CARTESIAN_POINT('Ctrl Pts',(-7.57835031313341,-2.27383784497801,
58.7352992646165));
#74701=CARTESIAN_POINT('Ctrl Pts',(-7.61454271413694,-2.14538114436201,
58.7298895925481));
#74702=CARTESIAN_POINT('Ctrl Pts',(-7.68830077885446,-1.88359365928993,
58.7188649870658));
#74703=CARTESIAN_POINT('Ctrl Pts',(-7.74855677595777,-1.61799285473667,
58.7078403815835));
#74704=CARTESIAN_POINT('Ctrl Pts',(-7.79500466405839,-1.34974934239952,
58.6968157761012));
#74705=CARTESIAN_POINT('Ctrl Pts',(-7.83997609327777,-1.09003260129617,
58.6861416144677));
#74706=CARTESIAN_POINT('Ctrl Pts',(-7.87200351402683,-0.827837999041716,
58.6754674528343));
#74707=CARTESIAN_POINT('Ctrl Pts',(-7.89085187608698,-0.564249651886951,
58.6647932912008));
#74708=CARTESIAN_POINT('Ctrl Pts',(-7.90407283064875,-0.379358808341846,
58.6573060302128));
#74709=CARTESIAN_POINT('Ctrl Pts',(-7.91081033794178,-0.193782654100511,
58.6498187692248));
#74710=CARTESIAN_POINT('Ctrl Pts',(-7.91099605152649,-0.00790396939679502,
58.6423315082368));
#74711=CARTESIAN_POINT('',(-7.90222269547159,0.00311450190333342,56.6423315082368));
#74712=CARTESIAN_POINT('Ctrl Pts',(-7.911,5.93636251267071E-12,58.6423315082368));
#74713=CARTESIAN_POINT('Ctrl Pts',(-7.91099999999835,2.20167589667258,58.5537440725041));
#74714=CARTESIAN_POINT('Ctrl Pts',(-6.94214576672053,4.3861041833918,58.4651566367714));
#74715=CARTESIAN_POINT('Ctrl Pts',(-3.67820201487778,7.34180684107883,58.2879817653059));
#74716=CARTESIAN_POINT('Ctrl Pts',(-1.40868175871199,8.08992666571428,58.1993943295732));
#74717=CARTESIAN_POINT('Ctrl Pts',(2.97309270521766,7.65454228025062,58.0222194581077));
#74718=CARTESIAN_POINT('Ctrl Pts',(5.05102072676007,6.47444880833906,57.933632022375));
#74719=CARTESIAN_POINT('Ctrl Pts',(7.66951518848044,2.93425195367247,57.7564571509096));
#74720=CARTESIAN_POINT('Ctrl Pts',(8.18956872247103,0.601881960094407,57.6678697151769));
#74721=CARTESIAN_POINT('Ctrl Pts',(7.32306689761135,-3.71537198232853,57.4906948437114));
#74722=CARTESIAN_POINT('Ctrl Pts',(5.94329958849896,-5.66643518936826,57.4021074079787));
#74723=CARTESIAN_POINT('Ctrl Pts',(2.16154501637446,-7.92205913233104,57.2249325365133));
#74724=CARTESIAN_POINT('Ctrl Pts',(-0.210816529304378,-8.20894963712989,
57.1363451007805));
#74725=CARTESIAN_POINT('Ctrl Pts',(-4.42123908576754,-6.91982244717625,
56.9591702293151));
#74726=CARTESIAN_POINT('Ctrl Pts',(-6.22631625634422,-5.35390358803243,
56.8705827935824));
#74727=CARTESIAN_POINT('Ctrl Pts',(-7.65317280859621,-2.31334857514119,
56.735440741312));
#74728=CARTESIAN_POINT('Ctrl Pts',(-7.91100000000084,-1.15702837836022,
56.6888861247744));
#74729=CARTESIAN_POINT('Ctrl Pts',(-7.911,5.76594327839075E-12,56.6423315082368));
#74730=CARTESIAN_POINT('',(-7.92132537539791,0.00356088473096691,54.6423315082368));
#74731=CARTESIAN_POINT('Ctrl Pts',(-7.89838609934108,0.00447586357080088,
56.6423315082368));
#74732=CARTESIAN_POINT('Ctrl Pts',(-7.90209458248899,1.1298110327076,56.5972864653267));
#74733=CARTESIAN_POINT('Ctrl Pts',(-7.15272636683917,4.89292271398436,56.4463988884626));
#74734=CARTESIAN_POINT('Ctrl Pts',(-2.58089786760515,8.32742667055543,56.2425900446207));
#74735=CARTESIAN_POINT('Ctrl Pts',(2.82873975620344,7.73373310986697,56.0309049767122));
#74736=CARTESIAN_POINT('Ctrl Pts',(6.19471352977467,5.45236858721805,55.8721411757803));
#74737=CARTESIAN_POINT('Ctrl Pts',(8.02841028037048,1.83220300240068,55.7133773748492));
#74738=CARTESIAN_POINT('Ctrl Pts',(7.93460731480094,-3.62384378458733,55.5016923069402));
#74739=CARTESIAN_POINT('Ctrl Pts',(3.7954711336447,-7.85637192923924,55.2900072390316));
#74740=CARTESIAN_POINT('Ctrl Pts',(-1.64811177619533,-8.05978374552938,
55.0783221711231));
#74741=CARTESIAN_POINT('Ctrl Pts',(-6.24123930469383,-5.89715594175713,
54.8800706831835));
#74742=CARTESIAN_POINT('Ctrl Pts',(-7.90119404608586,-2.2838008882752,54.7347404622217));
#74743=CARTESIAN_POINT('Ctrl Pts',(-7.92132537539791,0.00356088473096691,
54.6423315082368));
#74744=CARTESIAN_POINT('',(-7.90965467482103,-0.00646043864732659,52.6423315082368));
#74745=CARTESIAN_POINT('Ctrl Pts',(-7.92132537539791,0.00356088473096691,
54.6423315082368));
#74746=CARTESIAN_POINT('Ctrl Pts',(-7.92425188641814,0.336076901541994,
54.6288979282673));
#74747=CARTESIAN_POINT('Ctrl Pts',(-7.75596513217767,3.2865552664362,54.5096218143437));
#74748=CARTESIAN_POINT('Ctrl Pts',(-4.02499199464678,8.44364384466607,54.2845031664651));
#74749=CARTESIAN_POINT('Ctrl Pts',(3.38756990960737,8.03314424947189,54.0198968315797));
#74750=CARTESIAN_POINT('Ctrl Pts',(7.14415802802205,4.09553804706829,53.8082117636707));
#74751=CARTESIAN_POINT('Ctrl Pts',(8.25041905810794,0.182663886590385,53.6494479627395));
#74752=CARTESIAN_POINT('Ctrl Pts',(7.32226987266179,-3.76785230220073,53.4906841618077));
#74753=CARTESIAN_POINT('Ctrl Pts',(3.73724118410271,-7.8818311594681,53.2789990938992));
#74754=CARTESIAN_POINT('Ctrl Pts',(-2.15499139441648,-8.45483246728375,
53.0673140259903));
#74755=CARTESIAN_POINT('Ctrl Pts',(-6.45081714418401,-5.10522729313052,
52.8556289580818));
#74756=CARTESIAN_POINT('Ctrl Pts',(-7.77803341798768,-2.21995614957399,
52.7316085411562));
#74757=CARTESIAN_POINT('Ctrl Pts',(-7.91375901553935,-0.457593973212717,
52.6605093912079));
#74758=CARTESIAN_POINT('Ctrl Pts',(-7.90965467482103,-0.00646043864732659,
52.6423315082368));
#74759=CARTESIAN_POINT('',(-7.90557077178582,0.000172428555999323,50.6423513293437));
#74760=CARTESIAN_POINT('Ctrl Pts',(-7.90965467482103,-0.00646043864732659,
52.6423315082368));
#74761=CARTESIAN_POINT('Ctrl Pts',(-7.88986108295124,2.16917596066671,52.5546668572536));
#74762=CARTESIAN_POINT('Ctrl Pts',(-5.85400455890075,6.99988501149608,52.361159672316));
#74763=CARTESIAN_POINT('Ctrl Pts',(2.35754329943507,9.05194297588424,52.0618099534242));
#74764=CARTESIAN_POINT('Ctrl Pts',(7.76450970406415,3.96477304772281,51.7972036185382));
#74765=CARTESIAN_POINT('Ctrl Pts',(8.1031421732418,-1.46680360649821,51.5855185506298));
#74766=CARTESIAN_POINT('Ctrl Pts',(6.42995471675893,-5.17285830448992,51.426754749698));
#74767=CARTESIAN_POINT('Ctrl Pts',(3.17601681014416,-7.59771441211321,51.2679909487665));
#74768=CARTESIAN_POINT('Ctrl Pts',(-2.2159366211452,-8.43681569021935,51.0563058808579));
#74769=CARTESIAN_POINT('Ctrl Pts',(-7.0206882469314,-5.13084566170502,50.847759737257));
#74770=CARTESIAN_POINT('Ctrl Pts',(-7.90577022156873,-1.24184940982428,
50.6921348606333));
#74771=CARTESIAN_POINT('Ctrl Pts',(-7.90532993643697,0.00017238839015414,
50.6423525179641));
#74772=CARTESIAN_POINT('',(-7.911,5.08315611824628E-12,48.6423315082368));
#74773=CARTESIAN_POINT('Ctrl Pts',(-7.91099999799831,0.000173334027146164,
50.6423245339043));
#74774=CARTESIAN_POINT('Ctrl Pts',(-7.91094914875265,2.20179054697439,50.5537394229491));
#74775=CARTESIAN_POINT('Ctrl Pts',(-6.94210293929909,4.3861429662668,50.4651543119939));
#74776=CARTESIAN_POINT('Ctrl Pts',(-3.67820201487841,7.34180684107852,50.2879817653059));
#74777=CARTESIAN_POINT('Ctrl Pts',(-1.40868175871268,8.08992666571416,50.1993943295732));
#74778=CARTESIAN_POINT('Ctrl Pts',(2.973092705217,7.65454228025088,50.0222194581078));
#74779=CARTESIAN_POINT('Ctrl Pts',(5.05102072675951,6.4744488083395,49.933632022375));
#74780=CARTESIAN_POINT('Ctrl Pts',(7.66951518848019,2.93425195367313,49.7564571509096));
#74781=CARTESIAN_POINT('Ctrl Pts',(8.18956872247098,0.601881960095113,49.6678697151769));
#74782=CARTESIAN_POINT('Ctrl Pts',(7.32306689761167,-3.7153719823279,49.4906948437114));
#74783=CARTESIAN_POINT('Ctrl Pts',(5.94329958849945,-5.66643518936775,49.4021074079787));
#74784=CARTESIAN_POINT('Ctrl Pts',(2.16154501637514,-7.92205913233085,49.2249325365133));
#74785=CARTESIAN_POINT('Ctrl Pts',(-0.210816529303669,-8.20894963712991,
49.1363451007806));
#74786=CARTESIAN_POINT('Ctrl Pts',(-4.42123908576694,-6.91982244717663,
48.9591702293151));
#74787=CARTESIAN_POINT('Ctrl Pts',(-6.22631625634376,-5.35390358803297,
48.8705827935824));
#74788=CARTESIAN_POINT('Ctrl Pts',(-7.65317280859601,-2.31334857514185,
48.7354407413121));
#74789=CARTESIAN_POINT('Ctrl Pts',(-7.91100000000074,-1.1570283783609,48.6888861247744));
#74790=CARTESIAN_POINT('Ctrl Pts',(-7.911,5.08315611824628E-12,48.6423315082368));
#74791=CARTESIAN_POINT('',(-7.911,4.91273688396632E-12,46.6423315082368));
#74792=CARTESIAN_POINT('Ctrl Pts',(-7.911,5.08315611824628E-12,48.6423315082368));
#74793=CARTESIAN_POINT('Ctrl Pts',(-7.91099999999859,2.20167589667188,48.5537440725041));
#74794=CARTESIAN_POINT('Ctrl Pts',(-6.94214576672087,4.38610418339135,48.4651566367714));
#74795=CARTESIAN_POINT('Ctrl Pts',(-3.67820201487804,7.34180684107875,48.2879817653059));
#74796=CARTESIAN_POINT('Ctrl Pts',(-1.40868175871209,8.08992666571431,48.1993943295732));
#74797=CARTESIAN_POINT('Ctrl Pts',(2.97309270521786,7.65454228025059,48.0222194581077));
#74798=CARTESIAN_POINT('Ctrl Pts',(5.05102072676038,6.47444880833886,47.933632022375));
#74799=CARTESIAN_POINT('Ctrl Pts',(7.66951518848072,2.93425195367186,47.7564571509096));
#74800=CARTESIAN_POINT('Ctrl Pts',(8.18956872247113,0.601881960093575,47.6678697151768));
#74801=CARTESIAN_POINT('Ctrl Pts',(7.32306689761087,-3.71537198232955,47.4906948437114));
#74802=CARTESIAN_POINT('Ctrl Pts',(5.94329958849809,-5.66643518936924,47.4021074079786));
#74803=CARTESIAN_POINT('Ctrl Pts',(2.16154501637293,-7.9220591323315,47.2249325365132));
#74804=CARTESIAN_POINT('Ctrl Pts',(-0.210816529306149,-8.20894963712988,
47.1363451007805));
#74805=CARTESIAN_POINT('Ctrl Pts',(-4.4212390857693,-6.91982244717518,46.959170229315));
#74806=CARTESIAN_POINT('Ctrl Pts',(-6.22631625634571,-5.35390358803076,
46.8705827935823));
#74807=CARTESIAN_POINT('Ctrl Pts',(-7.65317280859644,-2.31334857513992,
46.735440741312));
#74808=CARTESIAN_POINT('Ctrl Pts',(-7.91100000000072,-1.15702837836002,
46.6888861247744));
#74809=CARTESIAN_POINT('Ctrl Pts',(-7.911,4.91273688396632E-12,46.6423315082368));
#74810=CARTESIAN_POINT('',(-7.911,5.19195797465954E-12,44.6423315082368));
#74811=CARTESIAN_POINT('Ctrl Pts',(-7.911,4.91273688396632E-12,46.6423315082368));
#74812=CARTESIAN_POINT('Ctrl Pts',(-7.91099999999863,2.20167589667171,46.5537440725041));
#74813=CARTESIAN_POINT('Ctrl Pts',(-6.94214576672096,4.3861041833912,46.4651566367714));
#74814=CARTESIAN_POINT('Ctrl Pts',(-3.6782020148782,7.34180684107867,46.2879817653059));
#74815=CARTESIAN_POINT('Ctrl Pts',(-1.40868175871226,8.08992666571427,46.1993943295732));
#74816=CARTESIAN_POINT('Ctrl Pts',(2.97309270521769,7.65454228025065,46.0222194581077));
#74817=CARTESIAN_POINT('Ctrl Pts',(5.05102072676024,6.47444880833897,45.933632022375));
#74818=CARTESIAN_POINT('Ctrl Pts',(7.66951518848065,2.93425195367203,45.7564571509096));
#74819=CARTESIAN_POINT('Ctrl Pts',(8.18956872247112,0.601881960093751,45.6678697151768));
#74820=CARTESIAN_POINT('Ctrl Pts',(7.32306689761095,-3.71537198232939,45.4906948437114));
#74821=CARTESIAN_POINT('Ctrl Pts',(5.94329958849821,-5.66643518936911,45.4021074079786));
#74822=CARTESIAN_POINT('Ctrl Pts',(2.1615450163731,-7.92205913233145,45.2249325365132));
#74823=CARTESIAN_POINT('Ctrl Pts',(-0.210816529305973,-8.20894963712989,
45.1363451007805));
#74824=CARTESIAN_POINT('Ctrl Pts',(-4.42123908576915,-6.91982244717527,
44.959170229315));
#74825=CARTESIAN_POINT('Ctrl Pts',(-6.2263162563456,-5.35390358803089,44.8705827935823));
#74826=CARTESIAN_POINT('Ctrl Pts',(-7.65317280859645,-2.31334857513995,
44.735440741312));
#74827=CARTESIAN_POINT('Ctrl Pts',(-7.91100000000076,-1.15702837835989,
44.6888861247744));
#74828=CARTESIAN_POINT('Ctrl Pts',(-7.911,5.19195797465954E-12,44.6423315082368));
#74829=CARTESIAN_POINT('',(-7.90782562621644,0.00332762781947112,42.6423315082368));
#74830=CARTESIAN_POINT('Ctrl Pts',(-7.911,5.19195797465954E-12,44.6423315082368));
#74831=CARTESIAN_POINT('Ctrl Pts',(-7.91099999999856,2.20167589667199,44.5537440725041));
#74832=CARTESIAN_POINT('Ctrl Pts',(-6.94214576672081,4.38610418339144,44.4651566367714));
#74833=CARTESIAN_POINT('Ctrl Pts',(-3.67820201487794,7.3418068410788,44.2879817653059));
#74834=CARTESIAN_POINT('Ctrl Pts',(-1.40868175871198,8.08992666571432,44.1993943295732));
#74835=CARTESIAN_POINT('Ctrl Pts',(2.97309270521796,7.65454228025055,44.0222194581077));
#74836=CARTESIAN_POINT('Ctrl Pts',(5.05102072676047,6.4744488083388,43.933632022375));
#74837=CARTESIAN_POINT('Ctrl Pts',(7.66951518848076,2.93425195367176,43.7564571509095));
#74838=CARTESIAN_POINT('Ctrl Pts',(8.18956872247114,0.601881960093462,43.6678697151768));
#74839=CARTESIAN_POINT('Ctrl Pts',(7.32306689761082,-3.71537198232965,43.4906948437114));
#74840=CARTESIAN_POINT('Ctrl Pts',(5.94329958849801,-5.66643518936932,43.4021074079786));
#74841=CARTESIAN_POINT('Ctrl Pts',(2.16154501637282,-7.92205913233153,43.2249325365132));
#74842=CARTESIAN_POINT('Ctrl Pts',(-0.210816529306261,-8.20894963712988,
43.1363451007805));
#74843=CARTESIAN_POINT('Ctrl Pts',(-4.42123908576939,-6.91982244717511,
42.959170229315));
#74844=CARTESIAN_POINT('Ctrl Pts',(-6.22631625634579,-5.35390358803068,
42.8705827935823));
#74845=CARTESIAN_POINT('Ctrl Pts',(-7.65317280859647,-2.31334857513982,
42.735440741312));
#74846=CARTESIAN_POINT('Ctrl Pts',(-7.91100000000073,-1.15702837835991,
42.6888861247744));
#74847=CARTESIAN_POINT('Ctrl Pts',(-7.911,5.02153874037958E-12,42.6423315082368));
#74848=CARTESIAN_POINT('',(-7.91845049609821,0.000976995136657901,40.6423315082369));
#74849=CARTESIAN_POINT('Ctrl Pts',(-7.90709240406838,0.00409624883905946,
42.6423315082368));
#74850=CARTESIAN_POINT('Ctrl Pts',(-7.90744323469513,0.885716272102219,
42.6068816380023));
#74851=CARTESIAN_POINT('Ctrl Pts',(-7.54808527225096,3.07967697239749,42.5185105007905));
#74852=CARTESIAN_POINT('Ctrl Pts',(-5.54712628819712,6.08619232436321,42.3772180966016));
#74853=CARTESIAN_POINT('Ctrl Pts',(-0.751839041474361,8.69051046575553,
42.1655330286929));
#74854=CARTESIAN_POINT('Ctrl Pts',(4.9699436811625,7.17132064257916,41.9538479607843));
#74855=CARTESIAN_POINT('Ctrl Pts',(7.82683125453677,2.53319956939885,41.7421628928754));
#74856=CARTESIAN_POINT('Ctrl Pts',(8.23123753638788,-2.87248740689012,41.530477824967));
#74857=CARTESIAN_POINT('Ctrl Pts',(3.55408252280707,-8.65990915799413,41.265871490081));
#74858=CARTESIAN_POINT('Ctrl Pts',(-5.26027638092778,-7.67229640261403,
40.9521822955118));
#74859=CARTESIAN_POINT('Ctrl Pts',(-7.90500472213288,-2.5283709606113,40.7443356348972));
#74860=CARTESIAN_POINT('Ctrl Pts',(-7.91845049609821,0.000976995136657901,
40.6423315082369));
#74861=CARTESIAN_POINT('',(-7.90957060305277,-0.00606182810568165,38.6423315082369));
#74862=CARTESIAN_POINT('Ctrl Pts',(-7.91845049609821,0.000976995136657901,
40.6423315082369));
#74863=CARTESIAN_POINT('Ctrl Pts',(-7.91895645951902,0.0961561605313427,
40.6384931009429));
#74864=CARTESIAN_POINT('Ctrl Pts',(-7.91764356014499,0.191342240229911,
40.6346546936489));
#74865=CARTESIAN_POINT('Ctrl Pts',(-7.87092759740858,1.59814129958058,40.5778950193778));
#74866=CARTESIAN_POINT('Ctrl Pts',(-7.08189078581498,4.20229089874874,40.4720524854235));
#74867=CARTESIAN_POINT('Ctrl Pts',(-4.22061022989196,7.09148996933881,40.3132886844917));
#74868=CARTESIAN_POINT('Ctrl Pts',(-0.325041355772333,8.22840781581323,
40.1545248835606));
#74869=CARTESIAN_POINT('Ctrl Pts',(5.02077049564122,7.13316884209834,39.9428398156514));
#74870=CARTESIAN_POINT('Ctrl Pts',(8.42022621943545,2.28647553367909,39.7311547477432));
#74871=CARTESIAN_POINT('Ctrl Pts',(7.61942872714469,-3.10172426520481,39.5194696798341));
#74872=CARTESIAN_POINT('Ctrl Pts',(4.44800486268501,-7.49798026302581,39.3077846119259));
#74873=CARTESIAN_POINT('Ctrl Pts',(-2.85709022741325,-8.91417773190914,
39.0431782770396));
#74874=CARTESIAN_POINT('Ctrl Pts',(-7.51958970425579,-4.00472737273126,
38.8037201534846));
#74875=CARTESIAN_POINT('Ctrl Pts',(-7.91612429028003,-0.696134925501238,
38.6701045638835));
#74876=CARTESIAN_POINT('Ctrl Pts',(-7.90931586281257,-0.00714213791867646,
38.6423315082369));
#74877=CARTESIAN_POINT('',(-7.90205031402523,0.00258408860188915,36.6423315082368));
#74878=CARTESIAN_POINT('Ctrl Pts',(-7.911,4.22939461230953E-12,38.6423315082369));
#74879=CARTESIAN_POINT('Ctrl Pts',(-7.91099999999882,2.20167589667103,38.5537440725041));
#74880=CARTESIAN_POINT('Ctrl Pts',(-6.94214576672134,4.3861041833906,38.4651566367714));
#74881=CARTESIAN_POINT('Ctrl Pts',(-3.67820201487883,7.34180684107835,38.2879817653059));
#74882=CARTESIAN_POINT('Ctrl Pts',(-1.40868175871296,8.08992666571415,38.1993943295732));
#74883=CARTESIAN_POINT('Ctrl Pts',(2.97309270521703,7.65454228025091,38.0222194581078));
#74884=CARTESIAN_POINT('Ctrl Pts',(5.05102072675969,6.47444880833941,37.933632022375));
#74885=CARTESIAN_POINT('Ctrl Pts',(7.6695151884804,2.93425195367269,37.7564571509096));
#74886=CARTESIAN_POINT('Ctrl Pts',(8.18956872247107,0.601881960094457,37.6678697151768));
#74887=CARTESIAN_POINT('Ctrl Pts',(7.32306689761127,-3.71537198232876,37.4906948437114));
#74888=CARTESIAN_POINT('Ctrl Pts',(5.9432995884987,-5.6664351893686,37.4021074079787));
#74889=CARTESIAN_POINT('Ctrl Pts',(2.16154501637379,-7.92205913233127,37.2249325365132));
#74890=CARTESIAN_POINT('Ctrl Pts',(-0.210816529305264,-8.20894963712991,
37.1363451007805));
#74891=CARTESIAN_POINT('Ctrl Pts',(-4.42123908576855,-6.91982244717565,
36.959170229315));
#74892=CARTESIAN_POINT('Ctrl Pts',(-6.22631625634514,-5.35390358803143,
36.8705827935823));
#74893=CARTESIAN_POINT('Ctrl Pts',(-7.65317280859619,-2.31334857514075,
36.735440741312));
#74894=CARTESIAN_POINT('Ctrl Pts',(-7.91100000000059,-1.15702837836087,
36.6888861247744));
#74895=CARTESIAN_POINT('Ctrl Pts',(-7.911,4.05953048954188E-12,36.6423315082369));
#74896=CARTESIAN_POINT('',(-7.92032460290522,0.00410429619978156,34.6423315082369));
#74897=CARTESIAN_POINT('Ctrl Pts',(-7.89801789798098,0.00374838870705885,
36.6423315082368));
#74898=CARTESIAN_POINT('Ctrl Pts',(-7.90109140379909,1.16454375460544,36.5958734928697));
#74899=CARTESIAN_POINT('Ctrl Pts',(-7.11894075804998,4.96435591288772,36.4435729435483));
#74900=CARTESIAN_POINT('Ctrl Pts',(-2.46977960589945,8.36105405809064,36.2383511272497));
#74901=CARTESIAN_POINT('Ctrl Pts',(2.93147714201178,7.69537963103877,36.0266660593408));
#74902=CARTESIAN_POINT('Ctrl Pts',(6.26677020828368,5.36939213081236,35.8679022584095));
#74903=CARTESIAN_POINT('Ctrl Pts',(8.05209744036919,1.72513010441004,35.7091384574778));
#74904=CARTESIAN_POINT('Ctrl Pts',(7.88564631233398,-3.72918440633894,35.4974533895694));
#74905=CARTESIAN_POINT('Ctrl Pts',(3.69051491642543,-7.90621778123017,35.2857683216604));
#74906=CARTESIAN_POINT('Ctrl Pts',(-1.75529427873059,-8.03712196874263,
35.0740832537519));
#74907=CARTESIAN_POINT('Ctrl Pts',(-6.28668782593535,-5.8293691697886,34.8772447382695));
#74908=CARTESIAN_POINT('Ctrl Pts',(-7.89940260670074,-2.24887738882641,
34.7333274897647));
#74909=CARTESIAN_POINT('Ctrl Pts',(-7.92032460290522,0.00410429619978156,
34.6423315082369));
#74910=CARTESIAN_POINT('',(-7.910692815354,-0.00630498622597453,32.6423315082369));
#74911=CARTESIAN_POINT('Ctrl Pts',(-7.92032460290522,0.00410429619978156,
34.6423315082369));
#74912=CARTESIAN_POINT('Ctrl Pts',(-7.92373815489182,0.371692074705317,
34.6274849558103));
#74913=CARTESIAN_POINT('Ctrl Pts',(-7.73535849790647,3.35749249374558,34.5067958694296));
#74914=CARTESIAN_POINT('Ctrl Pts',(-3.91219481221388,8.49649420640381,34.2802642490941));
#74915=CARTESIAN_POINT('Ctrl Pts',(3.49424336047911,7.9873211780795,34.0156579142083));
#74916=CARTESIAN_POINT('Ctrl Pts',(7.19806303432888,4.00003930652512,33.8039728462998));
#74917=CARTESIAN_POINT('Ctrl Pts',(8.2521199516345,0.072780503715108,33.6452090453681));
#74918=CARTESIAN_POINT('Ctrl Pts',(7.27144578913484,-3.86502564053636,33.4864452444366));
#74919=CARTESIAN_POINT('Ctrl Pts',(3.63195094250934,-7.93089947300516,33.274760176528));
#74920=CARTESIAN_POINT('Ctrl Pts',(-2.26738957999657,-8.42538571491713,
33.0630751086194));
#74921=CARTESIAN_POINT('Ctrl Pts',(-6.51822921065279,-5.01887193528488,
32.8513900407104));
#74922=CARTESIAN_POINT('Ctrl Pts',(-7.79222394496349,-2.14925319637973,
32.7287825962423));
#74923=CARTESIAN_POINT('Ctrl Pts',(-7.91444208827574,-0.422243313346306,
32.6590964187509));
#74924=CARTESIAN_POINT('Ctrl Pts',(-7.910692815354,-0.00630498622597453,
32.6423315082369));
#74925=CARTESIAN_POINT('',(-7.90592497177009,4.79922218070005E-5,30.6423372190962));
#74926=CARTESIAN_POINT('Ctrl Pts',(-7.910692815354,-0.00630498622597453,
32.6423315082369));
#74927=CARTESIAN_POINT('Ctrl Pts',(-7.89077166389797,2.20371561880541,32.5532538847966));
#74928=CARTESIAN_POINT('Ctrl Pts',(-5.79915631276819,7.06805053223478,32.3583337274018));
#74929=CARTESIAN_POINT('Ctrl Pts',(2.47787498205179,9.01974598430914,32.057571036053));
#74930=CARTESIAN_POINT('Ctrl Pts',(7.81661836099797,3.86102494974632,31.7929647011671));
#74931=CARTESIAN_POINT('Ctrl Pts',(8.08289089798158,-1.57457950934242,31.5812796332585));
#74932=CARTESIAN_POINT('Ctrl Pts',(6.36049990923886,-5.25802449618405,31.4225158323268));
#74933=CARTESIAN_POINT('Ctrl Pts',(3.07455978983641,-7.63933434043985,31.2637520313955));
#74934=CARTESIAN_POINT('Ctrl Pts',(-2.32808948167419,-8.40655895507157,
31.0520669634867));
#74935=CARTESIAN_POINT('Ctrl Pts',(-7.05624836198249,-5.05965197045065,
30.8449289678837));
#74936=CARTESIAN_POINT('Ctrl Pts',(-7.90630531642784,-1.20693321518151,
30.6907122392577));
#74937=CARTESIAN_POINT('Ctrl Pts',(-7.90538714644296,4.76034783793698E-5,
30.6423380445861));
#74938=CARTESIAN_POINT('',(-7.911,3.37729844090973E-12,28.6423315082369));
#74939=CARTESIAN_POINT('Ctrl Pts',(-7.91099999982219,5.16604830449524E-5,
30.6423294296068));
#74940=CARTESIAN_POINT('Ctrl Pts',(-7.91098484438918,2.20171006714826,30.5537426867508));
#74941=CARTESIAN_POINT('Ctrl Pts',(-6.94213300243702,4.38611574223799,30.4651559438947));
#74942=CARTESIAN_POINT('Ctrl Pts',(-3.67820201487999,7.34180684107772,30.287981765306));
#74943=CARTESIAN_POINT('Ctrl Pts',(-1.40868175871443,8.08992666571386,30.1993943295733));
#74944=CARTESIAN_POINT('Ctrl Pts',(2.97309270521535,7.65454228025152,30.0222194581078));
#74945=CARTESIAN_POINT('Ctrl Pts',(5.05102072675811,6.47444880834058,29.9336320223751));
#74946=CARTESIAN_POINT('Ctrl Pts',(7.66951518847956,2.93425195367478,29.7564571509097));
#74947=CARTESIAN_POINT('Ctrl Pts',(8.18956872247085,0.601881960096879,29.6678697151769));
#74948=CARTESIAN_POINT('Ctrl Pts',(7.32306689761247,-3.71537198232632,29.4906948437115));
#74949=CARTESIAN_POINT('Ctrl Pts',(5.94329958850067,-5.66643518936647,29.4021074079788));
#74950=CARTESIAN_POINT('Ctrl Pts',(2.16154501637685,-7.92205913233039,29.2249325365134));
#74951=CARTESIAN_POINT('Ctrl Pts',(-0.2108165293019,-8.20894963712995,29.1363451007806));
#74952=CARTESIAN_POINT('Ctrl Pts',(-4.42123908576545,-6.91982244717758,
28.9591702293152));
#74953=CARTESIAN_POINT('Ctrl Pts',(-6.22631625634261,-5.35390358803431,
28.8705827935825));
#74954=CARTESIAN_POINT('Ctrl Pts',(-7.65317280859551,-2.3133485751435,28.7354407413121));
#74955=CARTESIAN_POINT('Ctrl Pts',(-7.91100000000049,-1.15702837836261,
28.6888861247745));
#74956=CARTESIAN_POINT('Ctrl Pts',(-7.911,3.37729844090973E-12,28.6423315082369));
#74957=CARTESIAN_POINT('',(-7.911,3.65596442009064E-12,26.6423315082369));
#74958=CARTESIAN_POINT('Ctrl Pts',(-7.911,3.37729844090973E-12,28.6423315082369));
#74959=CARTESIAN_POINT('Ctrl Pts',(-7.91099999999906,2.20167589667017,28.5537440725042));
#74960=CARTESIAN_POINT('Ctrl Pts',(-6.94214576672181,4.38610418338985,28.4651566367714));
#74961=CARTESIAN_POINT('Ctrl Pts',(-3.67820201487962,7.34180684107795,28.287981765306));
#74962=CARTESIAN_POINT('Ctrl Pts',(-1.40868175871383,8.089926665714,28.1993943295733));
#74963=CARTESIAN_POINT('Ctrl Pts',(2.97309270521621,7.65454228025123,28.0222194581078));
#74964=CARTESIAN_POINT('Ctrl Pts',(5.05102072675899,6.47444880833995,27.9336320223751));
#74965=CARTESIAN_POINT('Ctrl Pts',(7.66951518848008,2.93425195367352,27.7564571509096));
#74966=CARTESIAN_POINT('Ctrl Pts',(8.189568722471,0.60188196009534,27.6678697151769));
#74967=CARTESIAN_POINT('Ctrl Pts',(7.32306689761167,-3.71537198232797,27.4906948437114));
#74968=CARTESIAN_POINT('Ctrl Pts',(5.94329958849931,-5.66643518936795,27.4021074079787));
#74969=CARTESIAN_POINT('Ctrl Pts',(2.16154501637464,-7.92205913233103,27.2249325365133));
#74970=CARTESIAN_POINT('Ctrl Pts',(-0.21081652930438,-8.20894963712993,
27.1363451007805));
#74971=CARTESIAN_POINT('Ctrl Pts',(-4.4212390857678,-6.91982244717613,26.9591702293151));
#74972=CARTESIAN_POINT('Ctrl Pts',(-6.22631625634456,-5.3539035880321,26.8705827935823));
#74973=CARTESIAN_POINT('Ctrl Pts',(-7.653172808596,-2.31334857514144,26.735440741312));
#74974=CARTESIAN_POINT('Ctrl Pts',(-7.91100000000053,-1.15702837836143,
26.6888861247745));
#74975=CARTESIAN_POINT('Ctrl Pts',(-7.911,3.65596442009064E-12,26.6423315082369));
#74976=CARTESIAN_POINT('',(-7.911,3.03701508386212E-12,24.6423315082369));
#74977=CARTESIAN_POINT('Ctrl Pts',(-7.911,3.65596442009064E-12,26.6423315082369));
#74978=CARTESIAN_POINT('Ctrl Pts',(-7.91099999999898,2.2016758966703,26.5537440725042));
#74979=CARTESIAN_POINT('Ctrl Pts',(-6.9421457667218,4.3861041833898,26.4651566367714));
#74980=CARTESIAN_POINT('Ctrl Pts',(-3.67820201487989,7.34180684107777,26.287981765306));
#74981=CARTESIAN_POINT('Ctrl Pts',(-1.40868175871432,8.08992666571388,26.1993943295733));
#74982=CARTESIAN_POINT('Ctrl Pts',(2.97309270521546,7.65454228025148,26.0222194581078));
#74983=CARTESIAN_POINT('Ctrl Pts',(5.0510207267582,6.47444880834052,25.9336320223751));
#74984=CARTESIAN_POINT('Ctrl Pts',(7.6695151884796,2.93425195367468,25.7564571509097));
#74985=CARTESIAN_POINT('Ctrl Pts',(8.18956872247086,0.601881960096767,25.6678697151769));
#74986=CARTESIAN_POINT('Ctrl Pts',(7.32306689761242,-3.71537198232642,25.4906948437115));
#74987=CARTESIAN_POINT('Ctrl Pts',(5.9432995885006,-5.66643518936655,25.4021074079788));
#74988=CARTESIAN_POINT('Ctrl Pts',(2.16154501637674,-7.92205913233042,25.2249325365133));
#74989=CARTESIAN_POINT('Ctrl Pts',(-0.210816529302013,-8.20894963712995,
25.1363451007806));
#74990=CARTESIAN_POINT('Ctrl Pts',(-4.42123908576554,-6.91982244717752,
24.9591702293152));
#74991=CARTESIAN_POINT('Ctrl Pts',(-6.22631625634268,-5.35390358803423,
24.8705827935825));
#74992=CARTESIAN_POINT('Ctrl Pts',(-7.65317280859548,-2.31334857514353,
24.7354407413121));
#74993=CARTESIAN_POINT('Ctrl Pts',(-7.91100000000044,-1.1570283783628,24.6888861247745));
#74994=CARTESIAN_POINT('Ctrl Pts',(-7.911,3.03701508386212E-12,24.6423315082369));
#74995=CARTESIAN_POINT('',(-7.90781319780899,0.00316833650103562,22.6423315082369));
#74996=CARTESIAN_POINT('Ctrl Pts',(-7.911,3.03701508386212E-12,24.6423315082369));
#74997=CARTESIAN_POINT('Ctrl Pts',(-7.91099999999916,2.20167589666983,24.5537440725042));
#74998=CARTESIAN_POINT('Ctrl Pts',(-6.942145766722,4.38610418338955,24.4651566367714));
#74999=CARTESIAN_POINT('Ctrl Pts',(-3.67820201487994,7.3418068410778,24.287981765306));
#75000=CARTESIAN_POINT('Ctrl Pts',(-1.40868175871418,8.08992666571394,24.1993943295733));
#75001=CARTESIAN_POINT('Ctrl Pts',(2.97309270521588,7.65454228025136,24.0222194581078));
#75002=CARTESIAN_POINT('Ctrl Pts',(5.05102072675871,6.47444880834017,23.9336320223751));
#75003=CARTESIAN_POINT('Ctrl Pts',(7.66951518847996,2.93425195367385,23.7564571509096));
#75004=CARTESIAN_POINT('Ctrl Pts',(8.18956872247098,0.601881960095694,23.6678697151769));
#75005=CARTESIAN_POINT('Ctrl Pts',(7.32306689761184,-3.71537198232766,23.4906948437114));
#75006=CARTESIAN_POINT('Ctrl Pts',(5.94329958849956,-5.6664351893677,23.4021074079787));
#75007=CARTESIAN_POINT('Ctrl Pts',(2.16154501637498,-7.92205913233094,23.2249325365133));
#75008=CARTESIAN_POINT('Ctrl Pts',(-0.210816529304027,-8.20894963712994,
23.1363451007805));
#75009=CARTESIAN_POINT('Ctrl Pts',(-4.42123908576751,-6.91982244717632,
22.9591702293151));
#75010=CARTESIAN_POINT('Ctrl Pts',(-6.22631625634433,-5.35390358803237,
22.8705827935824));
#75011=CARTESIAN_POINT('Ctrl Pts',(-7.65317280859584,-2.3133485751419,22.7354407413121));
#75012=CARTESIAN_POINT('Ctrl Pts',(-7.91100000000042,-1.15702837836207,
22.6888861247745));
#75013=CARTESIAN_POINT('Ctrl Pts',(-7.911,2.86604073806984E-12,22.6423315082369));
#75014=CARTESIAN_POINT('',(-7.91783831042937,0.00131071308626149,20.6423315082369));
#75015=CARTESIAN_POINT('Ctrl Pts',(-7.90700995084759,0.0039669291065153,
22.6423315082369));
#75016=CARTESIAN_POINT('Ctrl Pts',(-7.9071452622316,0.920854935814697,22.6054686655453));
#75017=CARTESIAN_POINT('Ctrl Pts',(-7.52681417092178,3.15012136567669,22.5156845558762));
#75018=CARTESIAN_POINT('Ctrl Pts',(-5.46558729494383,6.15952129533179,22.3729791792306));
#75019=CARTESIAN_POINT('Ctrl Pts',(-0.63604468917613,8.69975179261806,22.1612941113216));
#75020=CARTESIAN_POINT('Ctrl Pts',(5.06500030754639,7.10450222303656,21.9496090434132));
#75021=CARTESIAN_POINT('Ctrl Pts',(7.85987075412757,2.42874849949774,21.7379239755043));
#75022=CARTESIAN_POINT('Ctrl Pts',(8.19225603304053,-2.98184445809894,21.5262389075959));
#75023=CARTESIAN_POINT('Ctrl Pts',(3.4384472016591,-8.7064694362903,21.2616325727098));
#75024=CARTESIAN_POINT('Ctrl Pts',(-5.32233815554137,-7.60654421846925,
20.9493563505979));
#75025=CARTESIAN_POINT('Ctrl Pts',(-7.90279857213812,-2.49308479875549,
20.7429226624402));
#75026=CARTESIAN_POINT('Ctrl Pts',(-7.91783831042937,0.00131071308626149,
20.6423315082369));
#75027=CARTESIAN_POINT('',(-7.91053182871032,-0.00597217323526291,18.6423315082369));
#75028=CARTESIAN_POINT('Ctrl Pts',(-7.91783831042937,0.00131071308626149,
20.6423315082369));
#75029=CARTESIAN_POINT('Ctrl Pts',(-7.91862346273972,0.131531090670436,
20.6370801284859));
#75030=CARTESIAN_POINT('Ctrl Pts',(-7.9160226862592,0.261758841428933,20.6318287487348));
#75031=CARTESIAN_POINT('Ctrl Pts',(-7.84894794642525,1.70281325792949,20.5736561020066));
#75032=CARTESIAN_POINT('Ctrl Pts',(-7.02530278880841,4.29622469448372,20.4678135680522));
#75033=CARTESIAN_POINT('Ctrl Pts',(-4.1258017534078,7.14706517316476,20.3090497671206));
#75034=CARTESIAN_POINT('Ctrl Pts',(-0.215438464096084,8.23200664081911,
20.1502859661893));
#75035=CARTESIAN_POINT('Ctrl Pts',(5.11531456458206,7.06567696722413,19.9386008982805));
#75036=CARTESIAN_POINT('Ctrl Pts',(8.44992758816854,2.17414436211242,19.7269158303718));
#75037=CARTESIAN_POINT('Ctrl Pts',(7.57744882651523,-3.20291380260486,19.5152307624632));
#75038=CARTESIAN_POINT('Ctrl Pts',(4.34776317168055,-7.5565475374821,19.3035456945544));
#75039=CARTESIAN_POINT('Ctrl Pts',(-2.97554305665166,-8.87534071017187,
19.0389393596687));
#75040=CARTESIAN_POINT('Ctrl Pts',(-7.5451282943228,-3.9335702533891,18.8008942085703));
#75041=CARTESIAN_POINT('Ctrl Pts',(-7.91699102695292,-0.660678904189338,
18.6686915914265));
#75042=CARTESIAN_POINT('Ctrl Pts',(-7.91045528272066,-0.0069486233530125,
18.6423315082369));
#75043=CARTESIAN_POINT('',(-7.90191996158085,0.00205550962533024,16.6423315082369));
#75044=CARTESIAN_POINT('Ctrl Pts',(-7.911,2.7494673204842E-12,18.6423315082369));
#75045=CARTESIAN_POINT('Ctrl Pts',(-7.91099999999924,2.20167589666962,18.5537440725042));
#75046=CARTESIAN_POINT('Ctrl Pts',(-6.94214576672209,4.38610418338945,18.4651566367715));
#75047=CARTESIAN_POINT('Ctrl Pts',(-3.67820201487994,7.34180684107782,18.287981765306));
#75048=CARTESIAN_POINT('Ctrl Pts',(-1.40868175871409,8.08992666571397,18.1993943295733));
#75049=CARTESIAN_POINT('Ctrl Pts',(2.97309270521611,7.65454228025129,18.0222194581078));
#75050=CARTESIAN_POINT('Ctrl Pts',(5.05102072675898,6.47444880833998,17.9336320223751));
#75051=CARTESIAN_POINT('Ctrl Pts',(7.66951518848015,2.93425195367341,17.7564571509096));
#75052=CARTESIAN_POINT('Ctrl Pts',(8.18956872247104,0.601881960095133,17.6678697151769));
#75053=CARTESIAN_POINT('Ctrl Pts',(7.32306689761153,-3.7153719823283,17.4906948437114));
#75054=CARTESIAN_POINT('Ctrl Pts',(5.94329958849902,-5.66643518936829,17.4021074079787));
#75055=CARTESIAN_POINT('Ctrl Pts',(2.16154501637408,-7.9220591323312,17.2249325365132));
#75056=CARTESIAN_POINT('Ctrl Pts',(-0.210816529305057,-8.20894963712993,
17.1363451007805));
#75057=CARTESIAN_POINT('Ctrl Pts',(-4.42123908576851,-6.9198224471757,16.959170229315));
#75058=CARTESIAN_POINT('Ctrl Pts',(-6.22631625634517,-5.35390358803143,
16.8705827935823));
#75059=CARTESIAN_POINT('Ctrl Pts',(-7.65317280859596,-2.3133485751412,16.735440741312));
#75060=CARTESIAN_POINT('Ctrl Pts',(-7.91100000000034,-1.15702837836198,
16.6888861247745));
#75061=CARTESIAN_POINT('Ctrl Pts',(-7.911,2.35367281220533E-12,16.6423315082369));
#75062=CARTESIAN_POINT('',(-7.91926959559151,0.00460530123625597,14.6423315082369));
#75063=CARTESIAN_POINT('Ctrl Pts',(-7.89772730700726,0.00300462915809097,
16.6423315082369));
#75064=CARTESIAN_POINT('Ctrl Pts',(-7.90010539424252,1.19923649303746,16.5944605204127));
#75065=CARTESIAN_POINT('Ctrl Pts',(-7.08451991690688,5.03575724884286,16.4407469986342));
#75066=CARTESIAN_POINT('Ctrl Pts',(-2.35822015041585,8.39320165289849,16.2341122098785));
#75067=CARTESIAN_POINT('Ctrl Pts',(3.03369317972992,7.6556601015982,16.0224271419698));
#75068=CARTESIAN_POINT('Ctrl Pts',(6.33771636031792,5.28546422124097,15.8636633410383));
#75069=CARTESIAN_POINT('Ctrl Pts',(8.0743562618132,1.61775091520958,15.7048995401067));
#75070=CARTESIAN_POINT('Ctrl Pts',(7.83528719697496,-3.83386340922832,15.4932144721981));
#75071=CARTESIAN_POINT('Ctrl Pts',(3.58490407290031,-7.9546616986963,15.2815294042894));
#75072=CARTESIAN_POINT('Ctrl Pts',(-1.86216543943523,-8.01303484464982,
15.0698443363805));
#75073=CARTESIAN_POINT('Ctrl Pts',(-6.33144359478282,-5.76141497936659,
14.8744187933557));
#75074=CARTESIAN_POINT('Ctrl Pts',(-7.89775500108633,-2.21401943858167,
14.7319145173077));
#75075=CARTESIAN_POINT('Ctrl Pts',(-7.91926959559151,0.00460530123625597,
14.6423315082369));
#75076=CARTESIAN_POINT('',(-7.91171611945518,-0.00610363383936718,12.6423315082369));
#75077=CARTESIAN_POINT('Ctrl Pts',(-7.91926959559151,0.00460530123625597,
14.6423315082369));
#75078=CARTESIAN_POINT('Ctrl Pts',(-7.92317454462533,0.407290861127973,
14.6260719833533));
#75079=CARTESIAN_POINT('Ctrl Pts',(-7.71423377210186,3.42846943275032,14.503969924515));
#75080=CARTESIAN_POINT('Ctrl Pts',(-3.79870386219735,8.54783779767484,14.2760253317233));
#75081=CARTESIAN_POINT('Ctrl Pts',(3.60029715467924,7.94008165336425,14.0114189968371));
#75082=CARTESIAN_POINT('Ctrl Pts',(7.25069154288822,3.90383120149957,13.7997339289286));
#75083=CARTESIAN_POINT('Ctrl Pts',(8.25235742781774,-0.037115784206696,
13.6409701279969));
#75084=CARTESIAN_POINT('Ctrl Pts',(7.21933219681781,-3.96151356154354,13.4822063270656));
#75085=CARTESIAN_POINT('Ctrl Pts',(3.52601661662749,-7.97856133140822,13.2705212591568));
#75086=CARTESIAN_POINT('Ctrl Pts',(-2.37938567029377,-8.39444481693599,
13.0588361912482));
#75087=CARTESIAN_POINT('Ctrl Pts',(-6.58448534345744,-4.93162653768452,
12.8471511233393));
#75088=CARTESIAN_POINT('Ctrl Pts',(-7.80591338107149,-2.07856012442669,
12.7259566513281));
#75089=CARTESIAN_POINT('Ctrl Pts',(-7.91509200919393,-0.386870836674057,
12.6576834462939));
#75090=CARTESIAN_POINT('Ctrl Pts',(-7.91171611945518,-0.00610363383936718,
12.6423315082369));
#75091=CARTESIAN_POINT('',(-7.90558071021525,-0.000276217684555168,10.6423315082369));
#75092=CARTESIAN_POINT('Ctrl Pts',(-7.91171611945518,-0.00610363383936718,
12.6423315082369));
#75093=CARTESIAN_POINT('Ctrl Pts',(-7.89181724590517,2.238293845799,12.5518409123396));
#75094=CARTESIAN_POINT('Ctrl Pts',(-5.74352385136303,7.13599824900525,12.3555077824878));
#75095=CARTESIAN_POINT('Ctrl Pts',(2.59776724179471,8.98594944374683,12.053332118682));
#75096=CARTESIAN_POINT('Ctrl Pts',(7.86734082994195,3.75659214309986,11.7887257837959));
#75097=CARTESIAN_POINT('Ctrl Pts',(8.06120621431038,-1.68207617849999,11.5770407158874));
#75098=CARTESIAN_POINT('Ctrl Pts',(6.28991713969547,-5.34225823726834,11.4182769149557));
#75099=CARTESIAN_POINT('Ctrl Pts',(2.97255753145224,-7.67959952006021,11.2595131140244));
#75100=CARTESIAN_POINT('Ctrl Pts',(-2.43982948211331,-8.37481141268209,
11.0478280461154));
#75101=CARTESIAN_POINT('Ctrl Pts',(-7.09110329026493,-4.9884606133613,10.8421008441866));
#75102=CARTESIAN_POINT('Ctrl Pts',(-7.90683872761096,-1.17212167128525,
10.6892949092345));
#75103=CARTESIAN_POINT('Ctrl Pts',(-7.90548959171866,-0.000280861935244084,
10.6423315082369));
#75104=CARTESIAN_POINT('',(-7.911,1.67199587508549E-12,8.64233150823696));
#75105=CARTESIAN_POINT('Ctrl Pts',(-7.911,1.84185999785313E-12,10.642331508237));
#75106=CARTESIAN_POINT('Ctrl Pts',(-7.91099999999949,2.20167589666864,10.5537440725042));
#75107=CARTESIAN_POINT('Ctrl Pts',(-6.94214576672266,4.3861041833885,10.4651566367715));
#75108=CARTESIAN_POINT('Ctrl Pts',(-3.67820201488105,7.34180684107724,10.287981765306));
#75109=CARTESIAN_POINT('Ctrl Pts',(-1.4086817587154,8.08992666571373,10.1993943295733));
#75110=CARTESIAN_POINT('Ctrl Pts',(2.97309270521472,7.65454228025181,10.0222194581079));
#75111=CARTESIAN_POINT('Ctrl Pts',(5.05102072675773,6.47444880834093,9.93363202237514));
#75112=CARTESIAN_POINT('Ctrl Pts',(7.66951518847951,2.93425195367501,9.75645715090968));
#75113=CARTESIAN_POINT('Ctrl Pts',(8.18956872247089,0.601881960096929,9.66786971517696));
#75114=CARTESIAN_POINT('Ctrl Pts',(7.32306689761239,-3.71537198232655,9.49069484371151));
#75115=CARTESIAN_POINT('Ctrl Pts',(5.94329958850041,-5.6664351893668,9.40210740797877));
#75116=CARTESIAN_POINT('Ctrl Pts',(2.16154501637618,-7.92205913233061,9.22493253651332));
#75117=CARTESIAN_POINT('Ctrl Pts',(-0.210816529302787,-8.20894963712997,
9.13634510078059));
#75118=CARTESIAN_POINT('Ctrl Pts',(-4.42123908576646,-6.91982244717699,
8.95917022931514));
#75119=CARTESIAN_POINT('Ctrl Pts',(-6.22631625634352,-5.35390358803331,
8.87058279358241));
#75120=CARTESIAN_POINT('Ctrl Pts',(-7.65317280859549,-2.31334857514306,
8.73544074131211));
#75121=CARTESIAN_POINT('Ctrl Pts',(-7.91100000000024,-1.15702837836326,
8.68888612477454));
#75122=CARTESIAN_POINT('Ctrl Pts',(-7.911,1.67199587508549E-12,8.64233150823696));
#75123=CARTESIAN_POINT('',(-7.911,1.5004664177809E-12,6.64233150823697));
#75124=CARTESIAN_POINT('Ctrl Pts',(-7.911,1.67199587508549E-12,8.64233150823696));
#75125=CARTESIAN_POINT('Ctrl Pts',(-7.91099999999954,2.20167589666832,8.55374407250424));
#75126=CARTESIAN_POINT('Ctrl Pts',(-6.9421457667229,4.38610418338806,8.46515663677151));
#75127=CARTESIAN_POINT('Ctrl Pts',(-3.67820201488173,7.34180684107685,8.28798176530607));
#75128=CARTESIAN_POINT('Ctrl Pts',(-1.40868175871635,8.08992666571352,8.19939432957335));
#75129=CARTESIAN_POINT('Ctrl Pts',(2.97309270521354,7.65454228025223,8.02221945810791));
#75130=CARTESIAN_POINT('Ctrl Pts',(5.05102072675658,6.47444880834178,7.93363202237519));
#75131=CARTESIAN_POINT('Ctrl Pts',(7.66951518847886,2.9342519536766,7.75645715090975));
#75132=CARTESIAN_POINT('Ctrl Pts',(8.18956872247071,0.601881960098821,7.66786971517703));
#75133=CARTESIAN_POINT('Ctrl Pts',(7.32306689761335,-3.71537198232458,7.49069484371159));
#75134=CARTESIAN_POINT('Ctrl Pts',(5.94329958850202,-5.66643518936506,7.40210740797886));
#75135=CARTESIAN_POINT('Ctrl Pts',(2.16154501637873,-7.92205913232988,7.22493253651342));
#75136=CARTESIAN_POINT('Ctrl Pts',(-0.210816529299954,-8.20894963713,7.1363451007807));
#75137=CARTESIAN_POINT('Ctrl Pts',(-4.42123908576381,-6.91982244717863,
6.95917022931526));
#75138=CARTESIAN_POINT('Ctrl Pts',(-6.22631625634134,-5.35390358803579,
6.87058279358254));
#75139=CARTESIAN_POINT('Ctrl Pts',(-7.65317280859497,-2.31334857514532,
6.7354407413122));
#75140=CARTESIAN_POINT('Ctrl Pts',(-7.91100000000022,-1.15702837836448,
6.68888612477459));
#75141=CARTESIAN_POINT('Ctrl Pts',(-7.911,1.5004664177809E-12,6.64233150823697));
#75142=CARTESIAN_POINT('',(-7.911,1.33004718350094E-12,4.64233150823698));
#75143=CARTESIAN_POINT('Ctrl Pts',(-7.911,1.5004664177809E-12,6.64233150823697));
#75144=CARTESIAN_POINT('Ctrl Pts',(-7.91099999999958,2.20167589666815,6.55374407250425));
#75145=CARTESIAN_POINT('Ctrl Pts',(-6.94214576672299,4.38610418338791,6.46515663677152));
#75146=CARTESIAN_POINT('Ctrl Pts',(-3.67820201488189,7.34180684107677,6.28798176530608));
#75147=CARTESIAN_POINT('Ctrl Pts',(-1.40868175871652,8.08992666571349,6.19939432957336));
#75148=CARTESIAN_POINT('Ctrl Pts',(2.97309270521337,7.65454228025229,6.02221945810792));
#75149=CARTESIAN_POINT('Ctrl Pts',(5.05102072675644,6.47444880834189,5.9336320223752));
#75150=CARTESIAN_POINT('Ctrl Pts',(7.6695151884788,2.93425195367677,5.75645715090976));
#75151=CARTESIAN_POINT('Ctrl Pts',(8.18956872247069,0.601881960098999,5.66786971517704));
#75152=CARTESIAN_POINT('Ctrl Pts',(7.32306689761343,-3.71537198232442,5.4906948437116));
#75153=CARTESIAN_POINT('Ctrl Pts',(5.94329958850214,-5.66643518936493,5.40210740797887));
#75154=CARTESIAN_POINT('Ctrl Pts',(2.1615450163789,-7.92205913232983,5.22493253651343));
#75155=CARTESIAN_POINT('Ctrl Pts',(-0.210816529299777,-8.20894963713001,
5.13634510078071));
#75156=CARTESIAN_POINT('Ctrl Pts',(-4.42123908576366,-6.91982244717873,
4.95917022931527));
#75157=CARTESIAN_POINT('Ctrl Pts',(-6.22631625634122,-5.35390358803592,
4.87058279358255));
#75158=CARTESIAN_POINT('Ctrl Pts',(-7.65317280859492,-2.31334857514548,
4.73544074131221));
#75159=CARTESIAN_POINT('Ctrl Pts',(-7.91100000000019,-1.15702837836465,
4.68888612477459));
#75160=CARTESIAN_POINT('Ctrl Pts',(-7.911,1.33004718350094E-12,4.64233150823698));
#75161=CARTESIAN_POINT('',(-7.9078171476394,0.0030170320035519,2.64233150823698));
#75162=CARTESIAN_POINT('Ctrl Pts',(-7.911,1.33004718350094E-12,4.64233150823698));
#75163=CARTESIAN_POINT('Ctrl Pts',(-7.91099999999963,2.20167589666798,4.55374407250426));
#75164=CARTESIAN_POINT('Ctrl Pts',(-6.94214576672309,4.38610418338776,4.46515663677153));
#75165=CARTESIAN_POINT('Ctrl Pts',(-3.67820201488205,7.34180684107669,4.28798176530609));
#75166=CARTESIAN_POINT('Ctrl Pts',(-1.4086817587167,8.08992666571346,4.19939432957337));
#75167=CARTESIAN_POINT('Ctrl Pts',(2.97309270521321,7.65454228025235,4.02221945810792));
#75168=CARTESIAN_POINT('Ctrl Pts',(5.0510207267563,6.474448808342,3.93363202237521));
#75169=CARTESIAN_POINT('Ctrl Pts',(7.66951518847874,2.93425195367693,3.75645715090976));
#75170=CARTESIAN_POINT('Ctrl Pts',(8.18956872247068,0.601881960099174,3.66786971517705));
#75171=CARTESIAN_POINT('Ctrl Pts',(7.32306689761351,-3.71537198232427,3.4906948437116));
#75172=CARTESIAN_POINT('Ctrl Pts',(5.94329958850226,-5.6664351893648,3.40210740797888));
#75173=CARTESIAN_POINT('Ctrl Pts',(2.16154501637907,-7.92205913232978,3.22493253651343));
#75174=CARTESIAN_POINT('Ctrl Pts',(-0.2108165292996,-8.20894963713001,3.13634510078072));
#75175=CARTESIAN_POINT('Ctrl Pts',(-4.42123908576351,-6.91982244717882,
2.95917022931527));
#75176=CARTESIAN_POINT('Ctrl Pts',(-6.22631625634111,-5.35390358803606,
2.87058279358255));
#75177=CARTESIAN_POINT('Ctrl Pts',(-7.65317280859487,-2.31334857514565,
2.73544074131222));
#75178=CARTESIAN_POINT('Ctrl Pts',(-7.91100000000017,-1.15702837836482,
2.6888861247746));
#75179=CARTESIAN_POINT('Ctrl Pts',(-7.911,1.15962794922098E-12,2.64233150823698));
#75180=CARTESIAN_POINT('',(-7.9226973683943,0.00165221630280203,0.642331508236981));
#75181=CARTESIAN_POINT('Ctrl Pts',(-7.90696476388048,0.00382500824235466,
2.64233150823698));
#75182=CARTESIAN_POINT('Ctrl Pts',(-7.90689714804109,0.955993951285606,
2.60405569308827));
#75183=CARTESIAN_POINT('Ctrl Pts',(-7.50511545360724,3.22058475577076,2.5128586109623));
#75184=CARTESIAN_POINT('Ctrl Pts',(-5.38279128402438,6.23167160317878,2.36874026185943));
#75185=CARTESIAN_POINT('Ctrl Pts',(-0.520794108197176,8.70764732515362,
2.15705519395051));
#75186=CARTESIAN_POINT('Ctrl Pts',(5.16041761571073,7.03604612731708,1.94537012604191));
#75187=CARTESIAN_POINT('Ctrl Pts',(7.8900448895937,2.32430843730864,1.73368505813334));
#75188=CARTESIAN_POINT('Ctrl Pts',(8.15525751620599,-3.09170662911801,1.52199999022448));
#75189=CARTESIAN_POINT('Ctrl Pts',(3.31495225340653,-8.74927398045779,1.25739365533871));
#75190=CARTESIAN_POINT('Ctrl Pts',(-5.37156617111391,-7.54432674623615,
0.946530405683787));
#75191=CARTESIAN_POINT('Ctrl Pts',(-7.91185123215259,-2.45352580665413,
0.741509689983209));
#75192=CARTESIAN_POINT('Ctrl Pts',(-7.9226973683943,0.00165221630280203,
0.642331508236981));
#75193=CARTESIAN_POINT('',(-7.90493147168185,-0.00324651952237742,-1.35766849176302));
#75194=CARTESIAN_POINT('Ctrl Pts',(-7.9226973683943,0.00165221630280203,
0.642331508236981));
#75195=CARTESIAN_POINT('Ctrl Pts',(-7.92342618264295,0.16662974251393,0.635667156028865));
#75196=CARTESIAN_POINT('Ctrl Pts',(-7.84288560960201,2.95119247036142,0.52316026986663));
#75197=CARTESIAN_POINT('Ctrl Pts',(-4.56546138485153,8.16671696405687,0.304810849749407));
#75198=CARTESIAN_POINT('Ctrl Pts',(2.87982575388721,8.23246492026226,0.0402045148638317));
#75199=CARTESIAN_POINT('Ctrl Pts',(6.85552241033558,4.54500061088602,-0.17148055304496));
#75200=CARTESIAN_POINT('Ctrl Pts',(8.70655133397208,-0.576037275883916,
-0.383165620953742));
#75201=CARTESIAN_POINT('Ctrl Pts',(6.33123203588563,-6.00082072304389,-0.594850688862375));
#75202=CARTESIAN_POINT('Ctrl Pts',(1.30771107118631,-8.1300716313903,-0.806535756770927));
#75203=CARTESIAN_POINT('Ctrl Pts',(-2.73589803143749,-7.7859037014987,-0.965299557702622));
#75204=CARTESIAN_POINT('Ctrl Pts',(-6.11165572102573,-5.51896580875037,
-1.12406335863396));
#75205=CARTESIAN_POINT('Ctrl Pts',(-7.70344787938649,-2.55725839949862,
-1.25485300332087));
#75206=CARTESIAN_POINT('Ctrl Pts',(-7.91039240334899,-0.623390115977236,
-1.33272138103054));
#75207=CARTESIAN_POINT('Ctrl Pts',(-7.90493147168185,-0.00324651952237742,
-1.35766849176302));
#75208=CARTESIAN_POINT('',(-7.90837905701166,-0.000918770651100465,-3.357668491763));
#75209=CARTESIAN_POINT('Ctrl Pts',(-7.90493147168185,-0.00324651952237742,
-1.35766849176302));
#75210=CARTESIAN_POINT('Ctrl Pts',(-7.88722343394008,2.00767888308271,-1.43856391498488));
#75211=CARTESIAN_POINT('Ctrl Pts',(-6.10452476405389,6.6637469996248,-1.62530187216105));
#75212=CARTESIAN_POINT('Ctrl Pts',(1.77247152912565,9.19149319484671,-1.91788236329163));
#75213=CARTESIAN_POINT('Ctrl Pts',(7.50118080572254,4.44261861729297,-2.18248869817746));
#75214=CARTESIAN_POINT('Ctrl Pts',(8.1730998889146,-0.93638062620659,-2.39417376608628));
#75215=CARTESIAN_POINT('Ctrl Pts',(6.28922068173262,-6.04763295627693,-2.6058588339948));
#75216=CARTESIAN_POINT('Ctrl Pts',(0.980539725566132,-8.66768713018763,
-2.81754390190352));
#75217=CARTESIAN_POINT('Ctrl Pts',(-4.23486739714097,-7.06245238847923,
-3.02922896981223));
#75218=CARTESIAN_POINT('Ctrl Pts',(-7.10657322087715,-4.19516421302404,
-3.18799277074389));
#75219=CARTESIAN_POINT('Ctrl Pts',(-7.88113996482031,-1.50027602753856,
-3.29747261139401));
#75220=CARTESIAN_POINT('Ctrl Pts',(-7.90817870772519,-0.0915277219815716,
-3.3540311850671));
#75221=CARTESIAN_POINT('Ctrl Pts',(-7.90837905701166,-0.000918770651100465,
-3.357668491763));
#75222=CARTESIAN_POINT('',(-7.911,7.02216063075412E-13,-5.35766849176301));
#75223=CARTESIAN_POINT('Ctrl Pts',(-7.911,6.47815134868779E-13,-3.357668491763));
#75224=CARTESIAN_POINT('Ctrl Pts',(-7.91099999999982,2.20167589666714,-3.44625592749572));
#75225=CARTESIAN_POINT('Ctrl Pts',(-6.9421457667236,4.38610418338687,-3.53484336322843));
#75226=CARTESIAN_POINT('Ctrl Pts',(-3.67820201488321,7.34180684107606,-3.71201823469386));
#75227=CARTESIAN_POINT('Ctrl Pts',(-1.40868175871816,8.08992666571316,-3.80060567042658));
#75228=CARTESIAN_POINT('Ctrl Pts',(2.97309270521153,7.65454228025296,-3.977780541892));
#75229=CARTESIAN_POINT('Ctrl Pts',(5.05102072675473,6.47444880834318,-4.06636797762472));
#75230=CARTESIAN_POINT('Ctrl Pts',(7.66951518847789,2.93425195367902,-4.24354284909015));
#75231=CARTESIAN_POINT('Ctrl Pts',(8.18956872247046,0.601881960101596,-4.33213028482286));
#75232=CARTESIAN_POINT('Ctrl Pts',(7.3230668976147,-3.71537198232182,-4.50930515628829));
#75233=CARTESIAN_POINT('Ctrl Pts',(5.94329958850423,-5.66643518936268,-4.59789259202101));
#75234=CARTESIAN_POINT('Ctrl Pts',(2.16154501638213,-7.9220591323289,-4.77506746348644));
#75235=CARTESIAN_POINT('Ctrl Pts',(-0.210816529296236,-8.20894963713006,
-4.86365489921916));
#75236=CARTESIAN_POINT('Ctrl Pts',(-4.42123908576041,-6.91982244718076,
-5.04082977068459));
#75237=CARTESIAN_POINT('Ctrl Pts',(-6.22631625633858,-5.35390358803894,
-5.1294172064173));
#75238=CARTESIAN_POINT('Ctrl Pts',(-7.65317280859422,-2.31334857514834,
-5.26455925868768));
#75239=CARTESIAN_POINT('Ctrl Pts',(-7.9110000000001,-1.15702837836641,-5.31111387522534));
#75240=CARTESIAN_POINT('Ctrl Pts',(-7.911,7.02216063075412E-13,-5.35766849176301));
#75241=CARTESIAN_POINT('',(-7.911,3.06976666308856E-13,-7.35766849176299));
#75242=CARTESIAN_POINT('Ctrl Pts',(-7.911,7.02216063075412E-13,-5.35766849176301));
#75243=CARTESIAN_POINT('Ctrl Pts',(-7.91099999999981,2.2016758966675,-5.44625592749573));
#75244=CARTESIAN_POINT('Ctrl Pts',(-6.9421457667233,4.3861041833875,-5.53484336322846));
#75245=CARTESIAN_POINT('Ctrl Pts',(-3.67820201488211,7.34180684107671,-5.71201823469391));
#75246=CARTESIAN_POINT('Ctrl Pts',(-1.40868175871657,8.08992666571353,-5.80060567042664));
#75247=CARTESIAN_POINT('Ctrl Pts',(2.97309270521362,7.65454228025224,-5.97778054189209));
#75248=CARTESIAN_POINT('Ctrl Pts',(5.0510207267568,6.47444880834166,-6.06636797762481));
#75249=CARTESIAN_POINT('Ctrl Pts',(7.66951518847909,2.93425195367611,-6.24354284909027));
#75250=CARTESIAN_POINT('Ctrl Pts',(8.1895687224708,0.601881960098109,-6.332130284823));
#75251=CARTESIAN_POINT('Ctrl Pts',(7.32306689761293,-3.71537198232549,-6.50930515628846));
#75252=CARTESIAN_POINT('Ctrl Pts',(5.94329958850123,-5.66643518936595,-6.59789259202118));
#75253=CARTESIAN_POINT('Ctrl Pts',(2.16154501637732,-7.9220591323303,-6.77506746348663));
#75254=CARTESIAN_POINT('Ctrl Pts',(-0.210816529301604,-8.20894963713,-6.86365489921936));
#75255=CARTESIAN_POINT('Ctrl Pts',(-4.42123908576546,-6.91982244717762,
-7.04082977068481));
#75256=CARTESIAN_POINT('Ctrl Pts',(-6.22631625634275,-5.35390358803421,
-7.12941720641755));
#75257=CARTESIAN_POINT('Ctrl Pts',(-7.65317280859512,-2.31334857514423,
-7.26455925868784));
#75258=CARTESIAN_POINT('Ctrl Pts',(-7.91100000000004,-1.15702837836455,
-7.31111387522542));
#75259=CARTESIAN_POINT('Ctrl Pts',(-7.911,3.06976666308856E-13,-7.35766849176299));
#75260=CARTESIAN_POINT('',(-7.90153522810969,-6.13663431064494E-5,-9.35774809978824));
#75261=CARTESIAN_POINT('Ctrl Pts',(-7.911,3.06976666308856E-13,-7.35766849176299));
#75262=CARTESIAN_POINT('Ctrl Pts',(-7.91099999999991,2.20167589666695,-7.44625592749571));
#75263=CARTESIAN_POINT('Ctrl Pts',(-6.94214576672365,4.38610418338686,-7.53484336322843));
#75264=CARTESIAN_POINT('Ctrl Pts',(-3.678202014883,7.34180684107621,-7.71201823469387));
#75265=CARTESIAN_POINT('Ctrl Pts',(-1.40868175871774,8.08992666571328,-7.80060567042659));
#75266=CARTESIAN_POINT('Ctrl Pts',(2.97309270521222,7.65454228025274,-7.97778054189203));
#75267=CARTESIAN_POINT('Ctrl Pts',(5.05102072675546,6.47444880834266,-8.06636797762475));
#75268=CARTESIAN_POINT('Ctrl Pts',(7.66951518847836,2.93425195367792,-8.24354284909019));
#75269=CARTESIAN_POINT('Ctrl Pts',(8.1895687224706,0.601881960100234,-8.33213028482292));
#75270=CARTESIAN_POINT('Ctrl Pts',(7.32306689761399,-3.71537198232332,-8.50930515628836));
#75271=CARTESIAN_POINT('Ctrl Pts',(5.94329958850299,-5.66643518936404,-8.59789259202108));
#75272=CARTESIAN_POINT('Ctrl Pts',(2.16154501638009,-7.9220591323295,-8.77506746348652));
#75273=CARTESIAN_POINT('Ctrl Pts',(-0.210816529298536,-8.20894963713004,
-8.86365489921924));
#75274=CARTESIAN_POINT('Ctrl Pts',(-4.42123908576261,-6.9198224471794,-9.04082977068468));
#75275=CARTESIAN_POINT('Ctrl Pts',(-6.22631625634041,-5.35390358803686,
-9.1294172064174));
#75276=CARTESIAN_POINT('Ctrl Pts',(-7.65316473334085,-2.3133657830805,-9.26455849385518));
#75277=CARTESIAN_POINT('Ctrl Pts',(-7.9109915283976,-1.1570663720484,-9.31111234556023));
#75278=CARTESIAN_POINT('Ctrl Pts',(-7.91099999979124,-5.70254707422617E-5,
-9.35766619726528));
#75279=CARTESIAN_POINT('',(-7.91074476364229,0.00235076547380794,-11.3575320716792));
#75280=CARTESIAN_POINT('Ctrl Pts',(-7.89527219315753,-6.42387880278883E-5,
-9.35780229637968));
#75281=CARTESIAN_POINT('Ctrl Pts',(-7.8943301009396,0.251675616834198,-9.36792465872531));
#75282=CARTESIAN_POINT('Ctrl Pts',(-7.88156223750695,0.50372398062786,-9.37784868590548));
#75283=CARTESIAN_POINT('Ctrl Pts',(-7.85712534419498,0.754793832873867,
-9.38764551474725));
#75284=CARTESIAN_POINT('Ctrl Pts',(-7.83259375277481,1.00683663367482,-9.39748030836408));
#75285=CARTESIAN_POINT('Ctrl Pts',(-7.79630326984454,1.25789283539776,-9.40718691589166));
#75286=CARTESIAN_POINT('Ctrl Pts',(-7.74844328219722,1.50670283778631,-9.41683730437658));
#75287=CARTESIAN_POINT('Ctrl Pts',(-7.70059642379473,1.75544458509165,-9.42648504550785));
#75288=CARTESIAN_POINT('Ctrl Pts',(-7.64118718455143,2.00194106078235,-9.43607659843696));
#75289=CARTESIAN_POINT('Ctrl Pts',(-7.57042400098654,2.24498195752224,-9.44568387099945));
#75290=CARTESIAN_POINT('Ctrl Pts',(-7.49983745088267,2.48741619480164,-9.45526716264815));
#75291=CARTESIAN_POINT('Ctrl Pts',(-7.41795433352572,2.72641195855995,-9.46486609555196));
#75292=CARTESIAN_POINT('Ctrl Pts',(-7.3249890753825,2.96081918184579,-9.47455204041744));
#75293=CARTESIAN_POINT('Ctrl Pts',(-7.23232399455102,3.19446952313566,-9.48420671014908));
#75294=CARTESIAN_POINT('Ctrl Pts',(-7.1286489625597,3.42356094898595,-9.49394783084039));
#75295=CARTESIAN_POINT('Ctrl Pts',(-7.01417259474218,3.64700603454982,-9.50384608407707));
#75296=CARTESIAN_POINT('Ctrl Pts',(-6.90790243038578,3.85443352740454,-9.51303478405383));
#75297=CARTESIAN_POINT('Ctrl Pts',(-6.79232442010998,4.0569958014873,-9.52235889603522));
#75298=CARTESIAN_POINT('Ctrl Pts',(-6.66759430689156,4.25386161900847,-9.53187496484008));
#75299=CARTESIAN_POINT('Ctrl Pts',(-6.53521053392643,4.46280747032571,-9.5419749564113));
#75300=CARTESIAN_POINT('Ctrl Pts',(-6.39251823069767,4.66533634529571,-9.55229118519302));
#75301=CARTESIAN_POINT('Ctrl Pts',(-6.24059578980112,4.86088392314525,-9.56289125685668));
#75302=CARTESIAN_POINT('Ctrl Pts',(-6.16211168653307,4.961905050789,-9.56836732157885));
#75303=CARTESIAN_POINT('Ctrl Pts',(-6.08116370595779,5.06106365602323,-9.57391913890214));
#75304=CARTESIAN_POINT('Ctrl Pts',(-5.99789672225837,5.15828587354442,-9.57955602982518));
#75305=CARTESIAN_POINT('Ctrl Pts',(-5.89101188654535,5.28308420639768,-9.58679176881166));
#75306=CARTESIAN_POINT('Ctrl Pts',(-5.78018816140105,5.40448460888323,-9.59403368896476));
#75307=CARTESIAN_POINT('Ctrl Pts',(-5.66550358296166,5.52218078259242,-9.60114611375309));
#75308=CARTESIAN_POINT('Ctrl Pts',(-5.55081900452227,5.63987695630161,-9.60825853854142));
#75309=CARTESIAN_POINT('Ctrl Pts',(-5.43227295202669,5.75386858884513,-9.61524146796497));
#75310=CARTESIAN_POINT('Ctrl Pts',(-5.30997227108176,5.86379653437864,-9.62195922549235));
#75311=CARTESIAN_POINT('Ctrl Pts',(-5.00007320380716,6.14234418861115,-9.63898142664305));
#75312=CARTESIAN_POINT('Ctrl Pts',(-4.66767152718237,6.39691191112764,-9.65584425758327));
#75313=CARTESIAN_POINT('Ctrl Pts',(-4.31753906619885,6.62407803953151,-9.6726110349599));
#75314=CARTESIAN_POINT('Ctrl Pts',(-4.15333299303393,6.73061502783731,-9.68047436378384));
#75315=CARTESIAN_POINT('Ctrl Pts',(-3.98522730228223,6.83112598164767,-9.68831656612694));
#75316=CARTESIAN_POINT('Ctrl Pts',(-3.81371429539387,6.92526179046604,-9.69614417312065));
#75317=CARTESIAN_POINT('Ctrl Pts',(-3.43607642441284,7.13253030654064,-9.71337902249802));
#75318=CARTESIAN_POINT('Ctrl Pts',(-3.04192208333915,7.30888923791777,-9.73054311454239));
#75319=CARTESIAN_POINT('Ctrl Pts',(-2.63652811821922,7.45258697954143,-9.74770616387365));
#75320=CARTESIAN_POINT('Ctrl Pts',(-2.21996567575453,7.60024354914455,-9.76534204986287));
#75321=CARTESIAN_POINT('Ctrl Pts',(-1.79153720395816,7.71341642853467,-9.78297683489474));
#75322=CARTESIAN_POINT('Ctrl Pts',(-1.35692620791112,7.79024165518569,-9.80068615563215));
#75323=CARTESIAN_POINT('Ctrl Pts',(-0.922315211864013,7.86706688183672,
-9.81839547636956));
#75324=CARTESIAN_POINT('Ctrl Pts',(-0.481522224584858,7.90754687054486,
-9.83617933281251));
#75325=CARTESIAN_POINT('Ctrl Pts',(-0.0401750600089637,7.90982063659286,
-9.85411336162388));
#75326=CARTESIAN_POINT('Ctrl Pts',(0.234138411264575,7.91123386569582,-9.86526001915795));
#75327=CARTESIAN_POINT('Ctrl Pts',(0.508667165951846,7.89788740320303,-9.8764646894644));
#75328=CARTESIAN_POINT('Ctrl Pts',(0.782016690662756,7.87024143589644,-9.88774553324992));
#75329=CARTESIAN_POINT('Ctrl Pts',(1.07532735614229,7.84057664289161,-9.89985015205766));
#75330=CARTESIAN_POINT('Ctrl Pts',(1.36680038013542,7.79420532872234,-9.91185505208351));
#75331=CARTESIAN_POINT('Ctrl Pts',(1.65475865274654,7.73181204052291,-9.92378133788048));
#75332=CARTESIAN_POINT('Ctrl Pts',(1.94829366193426,7.66821041429143,-9.93593859378857));
#75333=CARTESIAN_POINT('Ctrl Pts',(2.23817720578776,7.58796037767743,-9.94801416102178));
#75334=CARTESIAN_POINT('Ctrl Pts',(2.52265930792318,7.49173880834698,-9.9600303941952));
#75335=CARTESIAN_POINT('Ctrl Pts',(2.81244630555269,7.39372294206166,-9.97227070073119));
#75336=CARTESIAN_POINT('Ctrl Pts',(3.09662944828447,7.27913446845292,-9.98444943970486));
#75337=CARTESIAN_POINT('Ctrl Pts',(3.3733735729584,7.14863706445015,-9.9965902397732));
#75338=CARTESIAN_POINT('Ctrl Pts',(3.49882216122815,7.08948236649837,-10.0020936853507));
#75339=CARTESIAN_POINT('Ctrl Pts',(3.62274227244574,7.02705795335948,-10.0075893351489));
#75340=CARTESIAN_POINT('Ctrl Pts',(3.74496311571731,6.9614221281404,-10.0130793900722));
#75341=CARTESIAN_POINT('Ctrl Pts',(4.01459670541344,6.81662175945726,-10.0251910984923));
#75342=CARTESIAN_POINT('Ctrl Pts',(4.27596109957176,6.65619488276075,-10.0372755769009));
#75343=CARTESIAN_POINT('Ctrl Pts',(4.52735890105361,6.48136368121027,-10.0493564565806));
#75344=CARTESIAN_POINT('Ctrl Pts',(4.77553132137262,6.30877552737475,-10.0612823411032));
#75345=CARTESIAN_POINT('Ctrl Pts',(5.01399221247215,6.12214982628365,-10.0732047186465));
#75346=CARTESIAN_POINT('Ctrl Pts',(5.24108658267087,5.92261756599295,-10.0851463225595));
#75347=CARTESIAN_POINT('Ctrl Pts',(5.45855407042944,5.73154378757107,-10.0965817033684));
#75348=CARTESIAN_POINT('Ctrl Pts',(5.66559897180327,5.5286339325247,-10.1080347150264));
#75349=CARTESIAN_POINT('Ctrl Pts',(5.86073602097242,5.31484771193084,-10.1195253206034));
#75350=CARTESIAN_POINT('Ctrl Pts',(6.03811594843458,5.12051565421648,-10.1299703016689));
#75351=CARTESIAN_POINT('Ctrl Pts',(6.20565672467288,4.91719604855102,-10.140446345998));
#75352=CARTESIAN_POINT('Ctrl Pts',(6.36221108407443,4.70558972801577,-10.15096844773));
#75353=CARTESIAN_POINT('Ctrl Pts',(6.4541093630474,4.58137564192243,-10.1571449799202));
#75354=CARTESIAN_POINT('Ctrl Pts',(6.54223146098758,4.45447282317314,-10.1633944540145));
#75355=CARTESIAN_POINT('Ctrl Pts',(6.62632645499383,4.32502182821367,-10.1696981874286));
#75356=CARTESIAN_POINT('Ctrl Pts',(6.76675304746766,4.1088572118852,-10.1802245191522));
#75357=CARTESIAN_POINT('Ctrl Pts',(6.89595142361405,3.88558459180187,-10.1909021487313));
#75358=CARTESIAN_POINT('Ctrl Pts',(7.01370242259043,3.6563945797851,-10.2016440851118));
#75359=CARTESIAN_POINT('Ctrl Pts',(7.13162589123027,3.42686887359518,-10.212401755186));
#75360=CARTESIAN_POINT('Ctrl Pts',(7.23806753818029,3.19140821185823,-10.2232239205799));
#75361=CARTESIAN_POINT('Ctrl Pts',(7.33279275849123,2.95125878677734,-10.2340232074323));
#75362=CARTESIAN_POINT('Ctrl Pts',(7.42753659861487,2.71106215634502,-10.2448246170636));
#75363=CARTESIAN_POINT('Ctrl Pts',(7.51055849952725,2.4661749093005,-10.2556031391583));
#75364=CARTESIAN_POINT('Ctrl Pts',(7.58162270374497,2.2178959806029,-10.2662713483209));
#75365=CARTESIAN_POINT('Ctrl Pts',(7.62886775592555,2.05283466639023,-10.2733638093441));
#75366=CARTESIAN_POINT('Ctrl Pts',(7.67082764334959,1.88627535844677,-10.280407513331));
#75367=CARTESIAN_POINT('Ctrl Pts',(7.70743584663393,1.71861221357824,-10.2873767708844));
#75368=CARTESIAN_POINT('Ctrl Pts',(7.75779321985561,1.48797878160987,-10.2969635157176));
#75369=CARTESIAN_POINT('Ctrl Pts',(7.79821517641293,1.25528979134765,-10.306518869809));
#75370=CARTESIAN_POINT('Ctrl Pts',(7.82861986687105,1.02135642216782,-10.3160211309126));
#75371=CARTESIAN_POINT('Ctrl Pts',(7.85899053714492,0.787684803928398,-10.3255127598186));
#75372=CARTESIAN_POINT('Ctrl Pts',(7.87936616761867,0.552770753253131,-10.3349514144832));
#75373=CARTESIAN_POINT('Ctrl Pts',(7.88961438555434,0.317430649804225,-10.3443154654274));
#75374=CARTESIAN_POINT('Ctrl Pts',(7.89975352869977,0.0845953401234145,
-10.3535798520301));
#75375=CARTESIAN_POINT('Ctrl Pts',(7.89997944780537,-0.148657735369844,
-10.3627712145199));
#75376=CARTESIAN_POINT('Ctrl Pts',(7.89011744535605,-0.381518591673179,
-10.3718686067204));
#75377=CARTESIAN_POINT('Ctrl Pts',(7.88049719641686,-0.608671182370837,
-10.380742988786));
#75378=CARTESIAN_POINT('Ctrl Pts',(7.86127723444699,-0.835451096446619,
-10.3895279512));
#75379=CARTESIAN_POINT('Ctrl Pts',(7.83225512777433,-1.06107863291402,-10.3982040507345));
#75380=CARTESIAN_POINT('Ctrl Pts',(7.81094174289927,-1.22677599518276,-10.4045756436268));
#75381=CARTESIAN_POINT('Ctrl Pts',(7.78434102672255,-1.3918513235166,-10.4108885245285));
#75382=CARTESIAN_POINT('Ctrl Pts',(7.75235981311111,-1.55598334814017,-10.4171349925863));
#75383=CARTESIAN_POINT('Ctrl Pts',(7.70451147451017,-1.80154765926557,-10.4264805766008));
#75384=CARTESIAN_POINT('Ctrl Pts',(7.6452308641868,-2.0448997890504,-10.4360084011818));
#75385=CARTESIAN_POINT('Ctrl Pts',(7.57434027445688,-2.28476855324992,-10.4456958405266));
#75386=CARTESIAN_POINT('Ctrl Pts',(7.50474964876695,-2.52023869742153,-10.4552056353796));
#75387=CARTESIAN_POINT('Ctrl Pts',(7.42397084966019,-2.75235117083653,-10.4648692447628));
#75388=CARTESIAN_POINT('Ctrl Pts',(7.33188551855802,-2.97990113339148,-10.4746652648976));
#75389=CARTESIAN_POINT('Ctrl Pts',(7.29948621963131,-3.05996230241089,-10.4781118961996));
#75390=CARTESIAN_POINT('Ctrl Pts',(7.26568773232178,-3.13945871307449,-10.481574918808));
#75391=CARTESIAN_POINT('Ctrl Pts',(7.23048643752592,-3.21833813255745,-10.4850534004867));
#75392=CARTESIAN_POINT('Ctrl Pts',(7.12906088671286,-3.44561353862609,-10.4950759556881));
#75393=CARTESIAN_POINT('Ctrl Pts',(7.01598568581979,-3.66776528176092,-10.5052268505375));
#75394=CARTESIAN_POINT('Ctrl Pts',(6.89226962542617,-3.88396812093333,-10.5154837856883));
#75395=CARTESIAN_POINT('Ctrl Pts',(6.76749883839721,-4.10201417183093,-10.5258281651261));
#75396=CARTESIAN_POINT('Ctrl Pts',(6.63190555753522,-4.31400874328372,-10.5362804006405));
#75397=CARTESIAN_POINT('Ctrl Pts',(6.48657142848231,-4.51913125145167,-10.5468176176773));
#75398=CARTESIAN_POINT('Ctrl Pts',(6.34223603393456,-4.72284416004361,-10.5572824230768));
#75399=CARTESIAN_POINT('Ctrl Pts',(6.18829390950642,-4.91977849361174,-10.5678310460277));
#75400=CARTESIAN_POINT('Ctrl Pts',(6.02584082373453,-5.10916593628471,-10.5784410803237));
#75401=CARTESIAN_POINT('Ctrl Pts',(5.89406586055627,-5.2627888925128,-10.5870474842713));
#75402=CARTESIAN_POINT('Ctrl Pts',(5.75669172154331,-5.41144668954126,-10.5956942953936));
#75403=CARTESIAN_POINT('Ctrl Pts',(5.61431617445421,-5.55475095918828,-10.6043695550134));
#75404=CARTESIAN_POINT('Ctrl Pts',(5.47569223833987,-5.69427914592128,-10.6128162206094));
#75405=CARTESIAN_POINT('Ctrl Pts',(5.33197229166852,-5.82857841806889,-10.6210847911245));
#75406=CARTESIAN_POINT('Ctrl Pts',(5.18360943099864,-5.95746876589514,-10.6292311772605));
#75407=CARTESIAN_POINT('Ctrl Pts',(5.03423940440251,-6.08723408988433,-10.6374328653939));
#75408=CARTESIAN_POINT('Ctrl Pts',(4.88016296020318,-6.21151743703355,-10.6455107046126));
#75409=CARTESIAN_POINT('Ctrl Pts',(4.72179101045929,-6.33012248003263,-10.6535217520204));
#75410=CARTESIAN_POINT('Ctrl Pts',(4.56340416495973,-6.44873867849039,-10.6615335529113));
#75411=CARTESIAN_POINT('Ctrl Pts',(4.40072067015659,-6.56167615829608,-10.6694785494265));
#75412=CARTESIAN_POINT('Ctrl Pts',(4.23410475342769,-6.66871629373732,-10.6774138147709));
#75413=CARTESIAN_POINT('Ctrl Pts',(4.17235649871686,-6.7083856223181,-10.6803546429661));
#75414=CARTESIAN_POINT('Ctrl Pts',(4.11006770474765,-6.74724470401329,-10.6832941346227));
#75415=CARTESIAN_POINT('Ctrl Pts',(4.04725542485125,-6.78528135193709,-10.6862351948125));
#75416=CARTESIAN_POINT('Ctrl Pts',(3.87322138080132,-6.89066952875857,-10.6943839930963));
#75417=CARTESIAN_POINT('Ctrl Pts',(3.69478956963306,-6.98942936383284,-10.7022845483943));
#75418=CARTESIAN_POINT('Ctrl Pts',(3.51265993024444,-7.0811466382946,-10.7100277923973));
#75419=CARTESIAN_POINT('Ctrl Pts',(3.33081252195456,-7.17272178615231,-10.7177590373415));
#75420=CARTESIAN_POINT('Ctrl Pts',(3.14527940909275,-7.25727642932643,-10.7253334581573));
#75421=CARTESIAN_POINT('Ctrl Pts',(2.95673955098527,-7.33444696701495,-10.7328415644625));
#75422=CARTESIAN_POINT('Ctrl Pts',(2.76867816089919,-7.41142166476359,-10.7403306170313));
#75423=CARTESIAN_POINT('Ctrl Pts',(2.57762584290098,-7.48105002179702,-10.7477536912425));
#75424=CARTESIAN_POINT('Ctrl Pts',(2.38422941042553,-7.54301532450862,-10.7552006093872));
#75425=CARTESIAN_POINT('Ctrl Pts',(2.19140278922616,-7.60479805648838,-10.7626255863934));
#75426=CARTESIAN_POINT('Ctrl Pts',(1.99624632021674,-7.65896323288816,-10.7700742670356));
#75427=CARTESIAN_POINT('Ctrl Pts',(1.79936640593767,-7.70523528352425,-10.7776356820015));
#75428=CARTESIAN_POINT('Ctrl Pts',(1.60460627738134,-7.75100912776554,-10.7851156839926));
#75429=CARTESIAN_POINT('Ctrl Pts',(1.40815992522824,-7.78905940092469,-10.7927060057787));
#75430=CARTESIAN_POINT('Ctrl Pts',(1.21057462420595,-7.81915007567315,-10.8004928331463));
#75431=CARTESIAN_POINT('Ctrl Pts',(1.01088526486274,-7.84956118182142,-10.8083625813529));
#75432=CARTESIAN_POINT('Ctrl Pts',(0.810032963616668,-7.87184288689846,
-10.8164330425456));
#75433=CARTESIAN_POINT('Ctrl Pts',(0.608610756537882,-7.88639032445356,
-10.8247931852765));
#75434=CARTESIAN_POINT('Ctrl Pts',(0.407892972403965,-7.90088688604542,
-10.8331240905344));
#75435=CARTESIAN_POINT('Ctrl Pts',(0.206609450497189,-7.90770392506711,
-10.8417426546984));
#75436=CARTESIAN_POINT('Ctrl Pts',(0.00529705867780233,-7.9072451045433,
-10.8507369161467));
#75437=CARTESIAN_POINT('Ctrl Pts',(-0.113003396465576,-7.90697548042177,
-10.8560223593993));
#75438=CARTESIAN_POINT('Ctrl Pts',(-0.231314782286878,-7.90419347896038,
-10.8614375414497));
#75439=CARTESIAN_POINT('Ctrl Pts',(-0.349536553218215,-7.8989815428797,
-10.8670003279862));
#75440=CARTESIAN_POINT('Ctrl Pts',(-0.540788865619985,-7.8905499754986,
-10.8759994808505));
#75441=CARTESIAN_POINT('Ctrl Pts',(-0.731567465986668,-7.87453744660504,
-10.8846651200071));
#75442=CARTESIAN_POINT('Ctrl Pts',(-0.92139693904322,-7.8513257245296,-10.8930793448849));
#75443=CARTESIAN_POINT('Ctrl Pts',(-1.11247201025147,-7.82796169481906,
-10.9015487811204));
#75444=CARTESIAN_POINT('Ctrl Pts',(-1.3025857572263,-7.79730408631012,-10.9097634928579));
#75445=CARTESIAN_POINT('Ctrl Pts',(-1.49129994133902,-7.75971678844881,
-10.9178072062819));
#75446=CARTESIAN_POINT('Ctrl Pts',(-1.68173556735899,-7.72178662102513,
-10.9259242940811));
#75447=CARTESIAN_POINT('Ctrl Pts',(-1.87074633383907,-7.67680016762974,
-10.9338672496608));
#75448=CARTESIAN_POINT('Ctrl Pts',(-2.0579242866238,-7.62509942081404,-10.9417221114086));
#75449=CARTESIAN_POINT('Ctrl Pts',(-2.14284665708554,-7.60164286565404,
-10.9452858509909));
#75450=CARTESIAN_POINT('Ctrl Pts',(-2.22739229822822,-7.57680375416926,
-10.9488314571277));
#75451=CARTESIAN_POINT('Ctrl Pts',(-2.31152562517164,-7.55061154929731,
-10.9523669649785));
#75452=CARTESIAN_POINT('Ctrl Pts',(-2.55696593603283,-7.47420160404176,
-10.9626810245491));
#75453=CARTESIAN_POINT('Ctrl Pts',(-2.79914206145313,-7.3859435225859,-10.972782972479));
#75454=CARTESIAN_POINT('Ctrl Pts',(-3.0367805974362,-7.28640306318918,-10.9827537554328));
#75455=CARTESIAN_POINT('Ctrl Pts',(-3.275600080173,-7.18636793662114,-10.9927740882785));
#75456=CARTESIAN_POINT('Ctrl Pts',(-3.50983661854676,-7.07493897548322,
-11.0026619492579));
#75457=CARTESIAN_POINT('Ctrl Pts',(-3.73824915610893,-6.95270094964151,
-11.0124994978384));
#75458=CARTESIAN_POINT('Ctrl Pts',(-3.96695335934609,-6.83030683501107,
-11.0223496082303));
#75459=CARTESIAN_POINT('Ctrl Pts',(-4.18981874858459,-6.69707695425021,
-11.0321492776509));
#75460=CARTESIAN_POINT('Ctrl Pts',(-4.4056514551113,-6.55359470301871,-11.0419809807038));
#75461=CARTESIAN_POINT('Ctrl Pts',(-4.62095932884421,-6.41046135252605,
-11.0517887763506));
#75462=CARTESIAN_POINT('Ctrl Pts',(-4.82926896525815,-6.25712627609679,
-11.061628450029));
#75463=CARTESIAN_POINT('Ctrl Pts',(-5.02944413836427,-6.09415180425817,
-11.0715818761527));
#75464=CARTESIAN_POINT('Ctrl Pts',(-5.22851875964976,-5.9320733568811,-11.0814805789007));
#75465=CARTESIAN_POINT('Ctrl Pts',(-5.41954859559745,-5.7604619565193,-11.0914917867233));
#75466=CARTESIAN_POINT('Ctrl Pts',(-5.60145879168493,-5.57984225057532,
-11.1016960310228));
#75467=CARTESIAN_POINT('Ctrl Pts',(-5.70701224620803,-5.47503760340664,
-11.1076170473252));
#75468=CARTESIAN_POINT('Ctrl Pts',(-5.80949597148569,-5.36719935489417,
-11.1136030571689));
#75469=CARTESIAN_POINT('Ctrl Pts',(-5.90870552764936,-5.25642413723177,
-11.1196697935519));
#75470=CARTESIAN_POINT('Ctrl Pts',(-6.07735119198448,-5.06811808187836,
-11.1299825983585));
#75471=CARTESIAN_POINT('Ctrl Pts',(-6.23653446489338,-4.87132781030842,
-11.1405286735911));
#75472=CARTESIAN_POINT('Ctrl Pts',(-6.38605251344742,-4.66719413220943,
-11.1513853009217));
#75473=CARTESIAN_POINT('Ctrl Pts',(-6.47850529064013,-4.54097040442988,
-11.1580983724029));
#75474=CARTESIAN_POINT('Ctrl Pts',(-6.56726317871131,-4.41193812238904,
-11.1649301811789));
#75475=CARTESIAN_POINT('Ctrl Pts',(-6.65228203278622,-4.28035772740498,
-11.1718989979642));
#75476=CARTESIAN_POINT('Ctrl Pts',(-6.73767850690118,-4.14819290447768,
-11.1788987674706));
#75477=CARTESIAN_POINT('Ctrl Pts',(-6.81906013954894,-4.01346262579741,
-11.1859143334325));
#75478=CARTESIAN_POINT('Ctrl Pts',(-6.8961809960879,-3.87630285641968,-11.1928178386192));
#75479=CARTESIAN_POINT('Ctrl Pts',(-6.97324733895214,-3.73924003984289,
-11.1997164639919));
#75480=CARTESIAN_POINT('Ctrl Pts',(-7.04605848385439,-3.59975082466254,
-11.2065031869559));
#75481=CARTESIAN_POINT('Ctrl Pts',(-7.11433735457903,-3.4580120805359,-11.2130504212207));
#75482=CARTESIAN_POINT('Ctrl Pts',(-7.12997611780663,-3.42554788427653,
-11.2145500161228));
#75483=CARTESIAN_POINT('Ctrl Pts',(-7.14537700041407,-3.39296585919192,
-11.216037047336));
#75484=CARTESIAN_POINT('Ctrl Pts',(-7.16053647716106,-3.36026846246956,
-11.2175099818246));
#75485=CARTESIAN_POINT('Ctrl Pts',(-7.26445657857949,-3.13612373503488,
-11.2276071312184));
#75486=CARTESIAN_POINT('Ctrl Pts',(-7.35790650102895,-2.90725336245844,
-11.2376559047231));
#75487=CARTESIAN_POINT('Ctrl Pts',(-7.44069004122439,-2.67462442953598,
-11.2476688324051));
#75488=CARTESIAN_POINT('Ctrl Pts',(-7.52496909473305,-2.43779297440435,
-11.2578626470922));
#75489=CARTESIAN_POINT('Ctrl Pts',(-7.5981933250589,-2.1970652754948,-11.2680193091238));
#75490=CARTESIAN_POINT('Ctrl Pts',(-7.6601147676513,-1.95342728081224,-11.278152039988));
#75491=CARTESIAN_POINT('Ctrl Pts',(-7.67375050021579,-1.89977571200254,
-11.2803833705648));
#75492=CARTESIAN_POINT('Ctrl Pts',(-7.68683796295885,-1.84598290739436,
-11.2826135406588));
#75493=CARTESIAN_POINT('Ctrl Pts',(-7.69937421557069,-1.79205922674744,
-11.2848426914563));
#75494=CARTESIAN_POINT('Ctrl Pts',(-7.75656683562454,-1.54604977921671,
-11.2950124749275));
#75495=CARTESIAN_POINT('Ctrl Pts',(-7.80229081606649,-1.2973175900563,-11.3051610433009));
#75496=CARTESIAN_POINT('Ctrl Pts',(-7.83639807134673,-1.04695990943283,
-11.3153018028891));
#75497=CARTESIAN_POINT('Ctrl Pts',(-7.87018914773473,-0.798923078536818,
-11.3253485562575));
#75498=CARTESIAN_POINT('Ctrl Pts',(-7.89257801450306,-0.549289861374268,
-11.3353876449467));
#75499=CARTESIAN_POINT('Ctrl Pts',(-7.90337060055902,-0.299119670074988,
-11.3454321058796));
#75500=CARTESIAN_POINT('Ctrl Pts',(-7.90766935757047,-0.19947526063231,
-11.3494328798033));
#75501=CARTESIAN_POINT('Ctrl Pts',(-7.91012781524847,-0.0997456492172265,
-11.3534345060231));
#75502=CARTESIAN_POINT('Ctrl Pts',(-7.91073139072936,2.07722496012377E-6,
-11.3574378083492));
#75503=CARTESIAN_POINT('',(-7.91701821474139,0.000346299696071325,-13.3576683701812));
#75504=CARTESIAN_POINT('Ctrl Pts',(-7.9107641172329,0.0057498417356433,
-11.357668491763));
#75505=CARTESIAN_POINT('Ctrl Pts',(-7.91457765203306,0.720360372816585,
-11.3863491342362));
#75506=CARTESIAN_POINT('Ctrl Pts',(-7.48577816839556,4.0661084013071,-11.5208723106634));
#75507=CARTESIAN_POINT('Ctrl Pts',(-3.83963961366753,7.83245821801285,-11.7083167540687));
#75508=CARTESIAN_POINT('Ctrl Pts',(1.61179695439645,8.07554689442854,-11.9200018219771));
#75509=CARTESIAN_POINT('Ctrl Pts',(5.28078975215679,6.34161180548053,-12.0787656229088));
#75510=CARTESIAN_POINT('Ctrl Pts',(7.65342116652072,3.0393371559865,-12.2375294238402));
#75511=CARTESIAN_POINT('Ctrl Pts',(8.39493817415805,-2.35203089183565,-12.449214491749));
#75512=CARTESIAN_POINT('Ctrl Pts',(4.10002393395763,-8.40746607421705,-12.7138208266349));
#75513=CARTESIAN_POINT('Ctrl Pts',(-4.86854992279596,-7.99517047053262,
-13.0313484284978));
#75514=CARTESIAN_POINT('Ctrl Pts',(-7.87876404316446,-2.76416089730763,
-13.2459642558688));
#75515=CARTESIAN_POINT('Ctrl Pts',(-7.92001450609604,-0.0721905216786065,
-13.3547375492854));
#75516=CARTESIAN_POINT('Ctrl Pts',(-7.9200591301389,0.000344913405787141,
-13.3576683087477));
#75517=CARTESIAN_POINT('',(-7.90609173527438,-0.00664493357794552,-15.3576684795722));
#75518=CARTESIAN_POINT('Ctrl Pts',(-7.91099999229989,0.000349043278910089,
-13.357668491763));
#75519=CARTESIAN_POINT('Ctrl Pts',(-7.91099075434638,0.20972551476333,-13.3661379354309));
#75520=CARTESIAN_POINT('Ctrl Pts',(-7.90266499763303,0.41926599422585,-13.3746073790987));
#75521=CARTESIAN_POINT('Ctrl Pts',(-7.88600956288663,0.628310571342361,
-13.3830768227666));
#75522=CARTESIAN_POINT('Ctrl Pts',(-7.8693785523935,0.837048596407084,-13.3915338464742));
#75523=CARTESIAN_POINT('Ctrl Pts',(-7.84444225460933,1.04529190279781,-13.3999908701819));
#75524=CARTESIAN_POINT('Ctrl Pts',(-7.81123946961377,1.25238131108219,-13.4084478938895));
#75525=CARTESIAN_POINT('Ctrl Pts',(-7.77810937884916,1.45901731748252,-13.4168864017758));
#75526=CARTESIAN_POINT('Ctrl Pts',(-7.73674896429563,1.66450420300881,-13.4253249096621));
#75527=CARTESIAN_POINT('Ctrl Pts',(-7.68724859145397,1.8681889875462,-13.4337634175484));
#75528=CARTESIAN_POINT('Ctrl Pts',(-7.63781407341306,2.07160279188426,-13.4421906989283));
#75529=CARTESIAN_POINT('Ctrl Pts',(-7.58026126041488,2.2732190173356,-13.4506179803081));
#75530=CARTESIAN_POINT('Ctrl Pts',(-7.5147317215566,2.47239320356429,-13.459045261688));
#75531=CARTESIAN_POINT('Ctrl Pts',(-7.44933605342673,2.67116049553043,-13.467455326919));
#75532=CARTESIAN_POINT('Ctrl Pts',(-7.37599626340356,2.86749544967156,-13.4758653921499));
#75533=CARTESIAN_POINT('Ctrl Pts',(-7.29490394662192,3.06076745434213,-13.4842754573809));
#75534=CARTESIAN_POINT('Ctrl Pts',(-7.21980856354628,3.23974662036612,-13.492063582018));
#75535=CARTESIAN_POINT('Ctrl Pts',(-7.13806543391911,3.41609904358483,-13.4998517066552));
#75536=CARTESIAN_POINT('Ctrl Pts',(-7.04986516082454,3.58933450853949,-13.5076398312923));
#75537=CARTESIAN_POINT('Ctrl Pts',(-6.96044519053985,3.7649655988411,-13.5155356557517));
#75538=CARTESIAN_POINT('Ctrl Pts',(-6.86446279964864,3.93724411927462,-13.5234314802112));
#75539=CARTESIAN_POINT('Ctrl Pts',(-6.7622093011055,4.10566028405204,-13.5313273046706));
#75540=CARTESIAN_POINT('Ctrl Pts',(-6.65993276105922,4.27411439923354,-13.5392249083519));
#75541=CARTESIAN_POINT('Ctrl Pts',(-6.55138247468514,4.43870413154281,-13.5471225120332));
#75542=CARTESIAN_POINT('Ctrl Pts',(-6.43689370421093,4.59894775363775,-13.5550201157145));
#75543=CARTESIAN_POINT('Ctrl Pts',(-6.32236027950089,4.75925387580551,-13.5629207997106));
#75544=CARTESIAN_POINT('Ctrl Pts',(-6.20188395362811,4.91521023122139,-13.5708214837068));
#75545=CARTESIAN_POINT('Ctrl Pts',(-6.07584113021107,5.06636709688861,-13.5787221677029));
#75546=CARTESIAN_POINT('Ctrl Pts',(-5.94965993959841,5.2176898994258,-13.586631524906));
#75547=CARTESIAN_POINT('Ctrl Pts',(-5.81790026256002,5.36420242302357,-13.594540882109));
#75548=CARTESIAN_POINT('Ctrl Pts',(-5.68097715809304,5.5054899445213,-13.6024502393121));
#75549=CARTESIAN_POINT('Ctrl Pts',(-5.5439725304119,5.64686158778152,-13.6103643057));
#75550=CARTESIAN_POINT('Ctrl Pts',(-5.40179859206367,5.78300178958583,-13.618278372088));
#75551=CARTESIAN_POINT('Ctrl Pts',(-5.2549047719409,5.91353505424908,-13.626192438476));
#75552=CARTESIAN_POINT('Ctrl Pts',(-5.10780592246906,6.04425051276001,-13.6341175510461));
#75553=CARTESIAN_POINT('Ctrl Pts',(-4.95597429147119,6.16934317932718,-13.6420426636161));
#75554=CARTESIAN_POINT('Ctrl Pts',(-4.79989076011748,6.28847912383741,-13.6499677761862));
#75555=CARTESIAN_POINT('Ctrl Pts',(-4.69199044414871,6.37083762729002,-13.6554463948654));
#75556=CARTESIAN_POINT('Ctrl Pts',(-4.58205879117334,6.45035035206467,-13.6609250135446));
#75557=CARTESIAN_POINT('Ctrl Pts',(-4.47026179466765,6.52691967831187,-13.6664036322239));
#75558=CARTESIAN_POINT('Ctrl Pts',(-4.30446367426373,6.64047416339802,-13.674528579296));
#75559=CARTESIAN_POINT('Ctrl Pts',(-4.13419830883315,6.74780213904776,-13.6826535263681));
#75560=CARTESIAN_POINT('Ctrl Pts',(-3.95996164627996,6.84854909889618,-13.6907784734402));
#75561=CARTESIAN_POINT('Ctrl Pts',(-3.78587853744792,6.94920727105576,-13.6988962600454));
#75562=CARTESIAN_POINT('Ctrl Pts',(-3.6078313856262,7.04329583102843,-13.7070140466506));
#75563=CARTESIAN_POINT('Ctrl Pts',(-3.42634505531038,7.13050352793897,-13.7151318332557));
#75564=CARTESIAN_POINT('Ctrl Pts',(-3.24499285480648,7.21764677287693,-13.7232436203061));
#75565=CARTESIAN_POINT('Ctrl Pts',(-3.06020683191874,7.29791915628924,-13.7313554073564));
#75566=CARTESIAN_POINT('Ctrl Pts',(-2.87253689653869,7.37105506545867,-13.7394671944068));
#75567=CARTESIAN_POINT('Ctrl Pts',(-2.68497900404071,7.44414731095852,-13.7475741385504));
#75568=CARTESIAN_POINT('Ctrl Pts',(-2.49454093047948,7.51011146233047,-13.755681082694));
#75569=CARTESIAN_POINT('Ctrl Pts',(-2.30179356405779,7.56872957559339,-13.7637880268376));
#75570=CARTESIAN_POINT('Ctrl Pts',(-2.1091339234749,7.62732100977244,-13.771891281237));
#75571=CARTESIAN_POINT('Ctrl Pts',(-1.91416739244046,7.67857298073169,-13.7799945356364));
#75572=CARTESIAN_POINT('Ctrl Pts',(-1.71748160661575,7.72231687584345,-13.7880977900358));
#75573=CARTESIAN_POINT('Ctrl Pts',(-1.51942509676862,7.76636562678205,-13.7962575168712));
#75574=CARTESIAN_POINT('Ctrl Pts',(-1.31962558725591,7.80280114233388,-13.8044172437067));
#75575=CARTESIAN_POINT('Ctrl Pts',(-1.11869634644107,7.83150301567071,-13.8125769705422));
#75576=CARTESIAN_POINT('Ctrl Pts',(-0.919233156929076,7.85999546991737,
-13.8206771611045));
#75577=CARTESIAN_POINT('Ctrl Pts',(-0.718656991572907,7.88086673495674,
-13.8287773516669));
#75578=CARTESIAN_POINT('Ctrl Pts',(-0.517576039129384,7.89405067400249,
-13.8368775422292));
#75579=CARTESIAN_POINT('Ctrl Pts',(-0.316496285765364,7.90723453443019,
-13.8449776844888));
#75580=CARTESIAN_POINT('Ctrl Pts',(-0.11491207127654,7.91273113943406,-13.8530778267483));
#75581=CARTESIAN_POINT('Ctrl Pts',(0.086564994665258,7.91052637323829,-13.8611779690079));
#75582=CARTESIAN_POINT('Ctrl Pts',(0.28806684418487,7.90832133583551,-13.8692791076613));
#75583=CARTESIAN_POINT('Ctrl Pts',(0.489461198268721,7.89841304197515,-13.8773802463147));
#75584=CARTESIAN_POINT('Ctrl Pts',(0.690137595971672,7.88083949199744,-13.885481384968));
#75585=CARTESIAN_POINT('Ctrl Pts',(0.893365828455263,7.86304247380639,-13.8936855390613));
#75586=CARTESIAN_POINT('Ctrl Pts',(1.0958573836457,7.83738394580421,-13.9018896931545));
#75587=CARTESIAN_POINT('Ctrl Pts',(1.29698467679072,7.80395744146328,-13.9100938472478));
#75588=CARTESIAN_POINT('Ctrl Pts',(1.49577570822341,7.77091921392481,-13.9182027032301));
#75589=CARTESIAN_POINT('Ctrl Pts',(1.6932336908906,7.73029260087103,-13.9263115592124));
#75590=CARTESIAN_POINT('Ctrl Pts',(1.88876369041668,7.68221925759501,-13.9344204151948));
#75591=CARTESIAN_POINT('Ctrl Pts',(2.0877405953304,7.63329845220912,-13.9426722183435));
#75592=CARTESIAN_POINT('Ctrl Pts',(2.28472057268627,7.57666601142176,-13.9509240214922));
#75593=CARTESIAN_POINT('Ctrl Pts',(2.4790932858785,7.5125240418858,-13.9591758246409));
#75594=CARTESIAN_POINT('Ctrl Pts',(2.67346599907072,7.44838207234984,-13.9674276277896));
#75595=CARTESIAN_POINT('Ctrl Pts',(2.86523113133767,7.37673072038818,-13.9756794309383));
#75596=CARTESIAN_POINT('Ctrl Pts',(3.05379994502888,7.29782343550059,-13.983931234087));
#75597=CARTESIAN_POINT('Ctrl Pts',(3.23272021792076,7.22295361652636,-13.9917608154601));
#75598=CARTESIAN_POINT('Ctrl Pts',(3.40910472212366,7.14140820148784,-13.9995903968331));
#75599=CARTESIAN_POINT('Ctrl Pts',(3.582415844458,7.05338342339166,-14.0074199782062));
#75600=CARTESIAN_POINT('Ctrl Pts',(3.75558086419229,6.96543285085584,-14.0152429591823));
#75601=CARTESIAN_POINT('Ctrl Pts',(3.92567734919365,6.87101394949806,-14.0230659401585));
#75602=CARTESIAN_POINT('Ctrl Pts',(4.09218683031946,6.77037132997592,-14.0308889211346));
#75603=CARTESIAN_POINT('Ctrl Pts',(4.25858531953984,6.66979579682047,-14.0387066874674));
#75604=CARTESIAN_POINT('Ctrl Pts',(4.42140126671791,6.56300498893785,-14.0465244538002));
#75605=CARTESIAN_POINT('Ctrl Pts',(4.58013989159596,6.45028988289761,-14.0543422201329));
#75606=CARTESIAN_POINT('Ctrl Pts',(4.73880243453417,6.33762880015463,-14.0621562394833));
#75607=CARTESIAN_POINT('Ctrl Pts',(4.8933912614168,6.21904927851853,-14.0699702588337));
#75608=CARTESIAN_POINT('Ctrl Pts',(5.04343959259385,6.09488622337258,-14.0777842781841));
#75609=CARTESIAN_POINT('Ctrl Pts',(5.19344422153273,5.97075933126398,-14.0855960216669));
#75610=CARTESIAN_POINT('Ctrl Pts',(5.33891071871571,5.84105237002629,-14.0934077651497));
#75611=CARTESIAN_POINT('Ctrl Pts',(5.47940435891093,5.7061413294404,-14.1012195086325));
#75612=CARTESIAN_POINT('Ctrl Pts',(5.61990585709268,5.57122274310982,-14.109031689036));
#75613=CARTESIAN_POINT('Ctrl Pts',(5.75543368421152,5.43109973513091,-14.1168438694394));
#75614=CARTESIAN_POINT('Ctrl Pts',(5.88558874019122,5.28618635514625,-14.1246560498429));
#75615=CARTESIAN_POINT('Ctrl Pts',(5.98576841705805,5.17464727223264,-14.1306690449014));
#75616=CARTESIAN_POINT('Ctrl Pts',(6.08276579425345,5.06027103084489,-14.1366820399599));
#75617=CARTESIAN_POINT('Ctrl Pts',(6.1764146710011,4.94326034230875,-14.1426950350184));
#75618=CARTESIAN_POINT('Ctrl Pts',(6.31097163630591,4.77513656224381,-14.1513346513765));
#75619=CARTESIAN_POINT('Ctrl Pts',(6.43855081732628,4.60165334075478,-14.1599742677346));
#75620=CARTESIAN_POINT('Ctrl Pts',(6.558772299389,4.4233954067851,-14.1686138840926));
#75621=CARTESIAN_POINT('Ctrl Pts',(6.67919284757172,4.24484230830184,-14.1772678061711));
#75622=CARTESIAN_POINT('Ctrl Pts',(6.79223121574276,4.06149888478754,-14.1859217282496));
#75623=CARTESIAN_POINT('Ctrl Pts',(6.89755215429033,3.87397667505173,-14.194575650328));
#75624=CARTESIAN_POINT('Ctrl Pts',(7.00595230436682,3.68097197951481,-14.2034825824632));
#75625=CARTESIAN_POINT('Ctrl Pts',(7.10617684071803,3.48354071662988,-14.2123895145984));
#75626=CARTESIAN_POINT('Ctrl Pts',(7.19791305150503,3.28237241990813,-14.2212964467335));
#75627=CARTESIAN_POINT('Ctrl Pts',(7.28734088338441,3.08626616628856,-14.2299792517318));
#75628=CARTESIAN_POINT('Ctrl Pts',(7.36870235703809,2.88660889449176,-14.2386620567301));
#75629=CARTESIAN_POINT('Ctrl Pts',(7.44175776740229,2.6840570655833,-14.2473448617284));
#75630=CARTESIAN_POINT('Ctrl Pts',(7.51764182011688,2.4736626049171,-14.256363857432));
#75631=CARTESIAN_POINT('Ctrl Pts',(7.58456374204374,2.26014525684741,-14.2653828531356));
#75632=CARTESIAN_POINT('Ctrl Pts',(7.64231217849465,2.04425672713394,-14.2744018488392));
#75633=CARTESIAN_POINT('Ctrl Pts',(7.70006061494556,1.82836819742046,-14.2834208445428));
#75634=CARTESIAN_POINT('Ctrl Pts',(7.74863552531833,1.61010875937359,-14.2924398402464));
#75635=CARTESIAN_POINT('Ctrl Pts',(7.78788463880215,1.39024237193,-14.30145883595));
#75636=CARTESIAN_POINT('Ctrl Pts',(7.82410083849344,1.18736581533357,-14.3097809028816));
#75637=CARTESIAN_POINT('Ctrl Pts',(7.8524074670251,0.982949090818679,-14.3181029698132));
#75638=CARTESIAN_POINT('Ctrl Pts',(7.87268864814392,0.777621019125552,-14.3264250367447));
#75639=CARTESIAN_POINT('Ctrl Pts',(7.89295183701053,0.572475102230492,-14.3347397208357));
#75640=CARTESIAN_POINT('Ctrl Pts',(7.90520375286211,0.366419740936222,-14.3430544049267));
#75641=CARTESIAN_POINT('Ctrl Pts',(7.90937998358545,0.160091459040854,-14.3513690890177));
#75642=CARTESIAN_POINT('Ctrl Pts',(7.91355276382944,-0.046066350597841,
-14.3596769033623));
#75643=CARTESIAN_POINT('Ctrl Pts',(7.90966316409722,-0.252496339491838,
-14.3679847177069));
#75644=CARTESIAN_POINT('Ctrl Pts',(7.89769872063863,-0.458558521917263,
-14.3762925320516));
#75645=CARTESIAN_POINT('Ctrl Pts',(7.88574630764296,-0.664413505115063,
-14.3845919927396));
#75646=CARTESIAN_POINT('Ctrl Pts',(7.86573527478703,-0.869901128927133,
-14.3928914534276));
#75647=CARTESIAN_POINT('Ctrl Pts',(7.83770520431504,-1.07438267402863,-14.4011909141156));
#75648=CARTESIAN_POINT('Ctrl Pts',(7.8096929899418,-1.2787339575004,-14.4094850877677));
#75649=CARTESIAN_POINT('Ctrl Pts',(7.77367196712769,-1.48208015174069,-14.4177792614198));
#75650=CARTESIAN_POINT('Ctrl Pts',(7.72973354910974,-1.68378747464379,-14.4260734350718));
#75651=CARTESIAN_POINT('Ctrl Pts',(7.68582757825155,-1.88534584294121,-14.4343614837338));
#75652=CARTESIAN_POINT('Ctrl Pts',(7.63401594334801,-2.08526747025648,-14.4426495323957));
#75653=CARTESIAN_POINT('Ctrl Pts',(7.57444126841368,-2.28292804778246,-14.4509375810576));
#75654=CARTESIAN_POINT('Ctrl Pts',(7.5521942070119,-2.35674073765073,-14.4540325996656));
#75655=CARTESIAN_POINT('Ctrl Pts',(7.52886509214598,-2.43023822453188,-14.4571276182735));
#75656=CARTESIAN_POINT('Ctrl Pts',(7.50446316936996,-2.50338841164726,-14.4602226368814));
#75657=CARTESIAN_POINT('Ctrl Pts',(7.44057615319467,-2.69490394222084,-14.4683257484961));
#75658=CARTESIAN_POINT('Ctrl Pts',(7.36935875614377,-2.88395744816265,-14.4764288601108));
#75659=CARTESIAN_POINT('Ctrl Pts',(7.29103315278047,-3.06997663917107,-14.4845319717255));
#75660=CARTESIAN_POINT('Ctrl Pts',(7.2126902665228,-3.25603687614518,-14.492636871328));
#75661=CARTESIAN_POINT('Ctrl Pts',(7.12723616953897,-3.43906116901714,-14.5007417709305));
#75662=CARTESIAN_POINT('Ctrl Pts',(7.03494071915571,-3.61849831808237,-14.5088466705329));
#75663=CARTESIAN_POINT('Ctrl Pts',(6.94261334424597,-3.79799753354408,-14.5169543735789));
#75664=CARTESIAN_POINT('Ctrl Pts',(6.84344004211401,-3.97390684716521,-14.5250620766249));
#75665=CARTESIAN_POINT('Ctrl Pts',(6.73773631810158,-4.14570021923137,-14.5331697796709));
#75666=CARTESIAN_POINT('Ctrl Pts',(6.63193750652792,-4.31764813091226,-14.5412847761374));
#75667=CARTESIAN_POINT('Ctrl Pts',(6.51959670117142,-4.48547243041464,-14.549399772604));
#75668=CARTESIAN_POINT('Ctrl Pts',(6.40107313684719,-4.64867547767462,-14.5575147690705));
#75669=CARTESIAN_POINT('Ctrl Pts',(6.28249170862118,-4.81195820162294,-14.565633727326));
#75670=CARTESIAN_POINT('Ctrl Pts',(6.15772169320428,-4.9706149192871,-14.5737526855816));
#75671=CARTESIAN_POINT('Ctrl Pts',(6.02716279811976,-5.12418087160877,-14.5818716438371));
#75672=CARTESIAN_POINT('Ctrl Pts',(5.89646408747138,-5.27791127775948,-14.5899992966878));
#75673=CARTESIAN_POINT('Ctrl Pts',(5.75996432141575,-5.42653978663855,-14.5981269495384));
#75674=CARTESIAN_POINT('Ctrl Pts',(5.6181012176356,-5.56963730492403,-14.6062546023891));
#75675=CARTESIAN_POINT('Ctrl Pts',(5.54402580606425,-5.64435727988145,-14.6104985475304));
#75676=CARTESIAN_POINT('Ctrl Pts',(5.468488653673,-5.71756985211167,-14.6147424926717));
#75677=CARTESIAN_POINT('Ctrl Pts',(5.39155571906165,-5.7892182484558,-14.618986437813));
#75678=CARTESIAN_POINT('Ctrl Pts',(5.24655695785499,-5.92425701650521,-14.62698518102));
#75679=CARTESIAN_POINT('Ctrl Pts',(5.09634720996129,-6.05397053172142,-14.6349839242271));
#75680=CARTESIAN_POINT('Ctrl Pts',(4.94135049965329,-6.17794271902679,-14.6429826674341));
#75681=CARTESIAN_POINT('Ctrl Pts',(4.78648003360986,-6.3018139314303,-14.6509748956935));
#75682=CARTESIAN_POINT('Ctrl Pts',(4.62683063523018,-6.41995292735989,-14.6589671239529));
#75683=CARTESIAN_POINT('Ctrl Pts',(4.46286163144894,-6.53198186299847,-14.6669593522123));
#75684=CARTESIAN_POINT('Ctrl Pts',(4.29899840672196,-6.64393852696015,-14.674946424556));
#75685=CARTESIAN_POINT('Ctrl Pts',(4.13082140589961,-6.74979279877053,-14.6829334968998));
#75686=CARTESIAN_POINT('Ctrl Pts',(3.95882167681481,-6.8492081243879,-14.6909205692436));
#75687=CARTESIAN_POINT('Ctrl Pts',(3.78690378681533,-6.94857614726033,-14.6989038412634));
#75688=CARTESIAN_POINT('Ctrl Pts',(3.61116708319462,-7.04151116391887,-14.7068871132832));
#75689=CARTESIAN_POINT('Ctrl Pts',(3.43213048645932,-7.12772062611299,-14.714870385303));
#75690=CARTESIAN_POINT('Ctrl Pts',(3.25314877500478,-7.21390366002025,-14.7228512099789));
#75691=CARTESIAN_POINT('Ctrl Pts',(3.07086948823391,-7.29336510497759,-14.7308320346547));
#75692=CARTESIAN_POINT('Ctrl Pts',(2.88583533747721,-7.36585876900771,-14.7388128593306));
#75693=CARTESIAN_POINT('Ctrl Pts',(2.69484906990006,-7.4406843850331,-14.7470504085117));
#75694=CARTESIAN_POINT('Ctrl Pts',(2.50092808359502,-7.50808631240983,-14.7552879576927));
#75695=CARTESIAN_POINT('Ctrl Pts',(2.30469117493277,-7.56784775138791,-14.7635255068738));
#75696=CARTESIAN_POINT('Ctrl Pts',(2.11454406535485,-7.62575461999568,-14.7715074210686));
#75697=CARTESIAN_POINT('Ctrl Pts',(1.92222296018322,-7.67648802646134,-14.7794893352633));
#75698=CARTESIAN_POINT('Ctrl Pts',(1.72830597348213,-7.71990151893313,-14.787471249458));
#75699=CARTESIAN_POINT('Ctrl Pts',(1.53434587363534,-7.76332466343313,-14.7954549382546));
#75700=CARTESIAN_POINT('Ctrl Pts',(1.33878951142208,-7.79942457607385,-14.8034386270511));
#75701=CARTESIAN_POINT('Ctrl Pts',(1.1422253876637,-7.82810591163511,-14.8114223158476));
#75702=CARTESIAN_POINT('Ctrl Pts',(0.945587380888185,-7.85679802771708,
-14.8194090054919));
#75703=CARTESIAN_POINT('Ctrl Pts',(0.747941188373335,-7.87806595933183,
-14.8273956951363));
#75704=CARTESIAN_POINT('Ctrl Pts',(0.549881009058251,-7.89186618461547,
-14.8353823847806));
#75705=CARTESIAN_POINT('Ctrl Pts',(0.351715968011602,-7.90567371634266,
-14.8433733029281));
#75706=CARTESIAN_POINT('Ctrl Pts',(0.153136836514974,-7.91200563622896,
-14.8513642210756));
#75707=CARTESIAN_POINT('Ctrl Pts',(-0.0452612227829571,-7.91087052237061,
-14.8593551392232));
#75708=CARTESIAN_POINT('Ctrl Pts',(-0.243893599454,-7.90973406788978,-14.8673554950182));
#75709=CARTESIAN_POINT('Ctrl Pts',(-0.442344142214344,-7.90111296470408,
-14.8753558508133));
#75710=CARTESIAN_POINT('Ctrl Pts',(-0.640020581781527,-7.88506782817346,
-14.8833562066083));
#75711=CARTESIAN_POINT('Ctrl Pts',(-0.837835164343456,-7.86901147875769,
-14.8913621533231));
#75712=CARTESIAN_POINT('Ctrl Pts',(-1.03487423365295,-7.84552078800775,
-14.8993681000379));
#75713=CARTESIAN_POINT('Ctrl Pts',(-1.23055425625879,-7.81470775028749,
-14.9073740467526));
#75714=CARTESIAN_POINT('Ctrl Pts',(-1.42648816563034,-7.78385473392054,
-14.9153903808534));
#75715=CARTESIAN_POINT('Ctrl Pts',(-1.62105917916205,-7.74566045817603,
-14.9234067149541));
#75716=CARTESIAN_POINT('Ctrl Pts',(-1.81369636153397,-7.70028743023002,
-14.9314230490548));
#75717=CARTESIAN_POINT('Ctrl Pts',(-1.85447618584592,-7.69068230579165,
-14.9331200459286));
#75718=CARTESIAN_POINT('Ctrl Pts',(-1.89516941090222,-7.68075565024744,
-14.9348170428024));
#75719=CARTESIAN_POINT('Ctrl Pts',(-1.93577072653057,-7.67050928519791,
-14.9365140396761));
#75720=CARTESIAN_POINT('Ctrl Pts',(-2.12148695064299,-7.62364094612004,
-14.9442763460656));
#75721=CARTESIAN_POINT('Ctrl Pts',(-2.30582851698515,-7.56994078708024,
-14.9520386524551));
#75722=CARTESIAN_POINT('Ctrl Pts',(-2.48824141034103,-7.50949903015268,
-14.9598009588446));
#75723=CARTESIAN_POINT('Ctrl Pts',(-2.67043333221745,-7.4491304912099,-14.9675538621251));
#75724=CARTESIAN_POINT('Ctrl Pts',(-2.85070089537913,-7.38203672085767,
-14.9753067654055));
#75725=CARTESIAN_POINT('Ctrl Pts',(-3.02849949459476,-7.30835903683168,
-14.983059668686));
#75726=CARTESIAN_POINT('Ctrl Pts',(-3.20611877614155,-7.23475565997461,
-14.9908047528242));
#75727=CARTESIAN_POINT('Ctrl Pts',(-3.38127372221828,-7.15458172401382,
-14.9985498369623));
#75728=CARTESIAN_POINT('Ctrl Pts',(-3.55343404572194,-7.06802854286146,
-15.0062949211005));
#75729=CARTESIAN_POINT('Ctrl Pts',(-3.72545560752278,-6.98154512381546,
-15.0140337626792));
#75730=CARTESIAN_POINT('Ctrl Pts',(-3.89448703355623,-6.88869285669213,
-15.0217726042579));
#75731=CARTESIAN_POINT('Ctrl Pts',(-4.06001713331067,-6.78971147231042,
-15.0295114458366));
#75732=CARTESIAN_POINT('Ctrl Pts',(-4.22544730722923,-6.69078984018879,
-15.0372456156957));
#75733=CARTESIAN_POINT('Ctrl Pts',(-4.38738005675412,-6.58574664200628,
-15.0449797855547));
#75734=CARTESIAN_POINT('Ctrl Pts',(-4.54532788920346,-6.4748679816371,-15.0527139554138));
#75735=CARTESIAN_POINT('Ctrl Pts',(-4.7032123081869,-6.36403383723271,-15.0604450201304));
#75736=CARTESIAN_POINT('Ctrl Pts',(-4.85711470327773,-6.2473691027134,-15.0681760848471));
#75737=CARTESIAN_POINT('Ctrl Pts',(-5.00657565793525,-6.12520376651832,
-15.0759071495637));
#75738=CARTESIAN_POINT('Ctrl Pts',(-5.15603444218046,-6.00304020435947,
-15.0836381020129));
#75739=CARTESIAN_POINT('Ctrl Pts',(-5.30105162963631,-5.87537641817403,
-15.0913690544621));
#75740=CARTESIAN_POINT('Ctrl Pts',(-5.44119975803647,-5.74258358172903,
-15.0991000069113));
#75741=CARTESIAN_POINT('Ctrl Pts',(-5.58135376516648,-5.60978517508329,
-15.1068312836473));
#75742=CARTESIAN_POINT('Ctrl Pts',(-5.71663804510143,-5.47185753609265,
-15.1145625603832));
#75743=CARTESIAN_POINT('Ctrl Pts',(-5.84666111061152,-5.32920959032977,
-15.1222938371192));
#75744=CARTESIAN_POINT('Ctrl Pts',(-5.97671343882886,-5.18652954053167,
-15.1300268538394));
#75745=CARTESIAN_POINT('Ctrl Pts',(-6.1015019526909,-5.03912733376445,-15.1377598705596));
#75746=CARTESIAN_POINT('Ctrl Pts',(-6.22067463421474,-4.88744596852358,
-15.1454928872798));
#75747=CARTESIAN_POINT('Ctrl Pts',(-6.33989596504546,-4.73570268310777,
-15.1532290608133));
#75748=CARTESIAN_POINT('Ctrl Pts',(-6.45349667690804,-4.57967704279862,
-15.1609652343468));
#75749=CARTESIAN_POINT('Ctrl Pts',(-6.56116732938121,-4.41984210983387,
-15.1687014078803));
#75750=CARTESIAN_POINT('Ctrl Pts',(-6.66896449115314,-4.25981937634201,
-15.1764466711506));
#75751=CARTESIAN_POINT('Ctrl Pts',(-6.77081747789992,-4.09597870938968,
-15.1841919344208));
#75752=CARTESIAN_POINT('Ctrl Pts',(-6.86646166892844,-3.92881981632353,
-15.1919371976911));
#75753=CARTESIAN_POINT('Ctrl Pts',(-6.96216723914695,-3.76155364985849,
-15.199687431446));
#75754=CARTESIAN_POINT('Ctrl Pts',(-7.05165591067077,-3.59096533211792,
-15.207437665201));
#75755=CARTESIAN_POINT('Ctrl Pts',(-7.13471077295075,-3.41757562993719,
-15.2151878989559));
#75756=CARTESIAN_POINT('Ctrl Pts',(-7.21789071619652,-3.24392480214849,
-15.2229498045949));
#75757=CARTESIAN_POINT('Ctrl Pts',(-7.29461735644497,-3.06746449180773,
-15.2307117102339));
#75758=CARTESIAN_POINT('Ctrl Pts',(-7.36472290601075,-2.88873285675234,
-15.2384736158729));
#75759=CARTESIAN_POINT('Ctrl Pts',(-7.41159305387289,-2.76923906183062,
-15.2436629577616));
#75760=CARTESIAN_POINT('Ctrl Pts',(-7.45550474725539,-2.64873033476617,
-15.2488522996503));
#75761=CARTESIAN_POINT('Ctrl Pts',(-7.49642058529095,-2.52737005767382,
-15.254041641539));
#75762=CARTESIAN_POINT('Ctrl Pts',(-7.57449418564336,-2.29579631441745,
-15.2639436898451));
#75763=CARTESIAN_POINT('Ctrl Pts',(-7.64185984319201,-2.06052492540488,
-15.2738457381511));
#75764=CARTESIAN_POINT('Ctrl Pts',(-7.69822398065782,-1.82243478446414,
-15.2837477864572));
#75765=CARTESIAN_POINT('Ctrl Pts',(-7.75419103741931,-1.58602196894888,
-15.2935800756488));
#75766=CARTESIAN_POINT('Ctrl Pts',(-7.79931102614652,-1.34682987051205,
-15.3034123648404));
#75767=CARTESIAN_POINT('Ctrl Pts',(-7.83334275199692,-1.10574062498276,
-15.313244654032));
#75768=CARTESIAN_POINT('Ctrl Pts',(-7.86686461943143,-0.868263343811501,
-15.3229296372828));
#75769=CARTESIAN_POINT('Ctrl Pts',(-7.88962796807497,-0.628945265185901,
-15.3326146205337));
#75770=CARTESIAN_POINT('Ctrl Pts',(-7.90144738229136,-0.388651855625442,
-15.3422996037846));
#75771=CARTESIAN_POINT('Ctrl Pts',(-7.90769935463835,-0.26154676190137,
-15.3474225520421));
#75772=CARTESIAN_POINT('Ctrl Pts',(-7.91089001490665,-0.134169158847204,
-15.3525455002997));
#75773=CARTESIAN_POINT('Ctrl Pts',(-7.91099720514315,-0.00664982836847595,
-15.3576684485573));
#75774=CARTESIAN_POINT('',(-7.90123025115119,0.00640242758643106,-17.357668491763));
#75775=CARTESIAN_POINT('Ctrl Pts',(-7.90416357127559,-0.00664300961161102,
-15.357668491763));
#75776=CARTESIAN_POINT('Ctrl Pts',(-7.88770305298382,1.76662955928556,-15.4289687423093));
#75777=CARTESIAN_POINT('Ctrl Pts',(-6.84972407068773,4.86972663156239,-15.5531902598329));
#75778=CARTESIAN_POINT('Ctrl Pts',(-3.20850006480543,7.57508514008354,-15.7303330443335));
#75779=CARTESIAN_POINT('Ctrl Pts',(2.16791332744694,8.45152836813056,-15.9420181122425));
#75780=CARTESIAN_POINT('Ctrl Pts',(7.06190333620408,5.12052295862938,-16.153703180151));
#75781=CARTESIAN_POINT('Ctrl Pts',(8.23216325382504,-0.209368643025021,
-16.3653882480596));
#75782=CARTESIAN_POINT('Ctrl Pts',(7.1501053363542,-4.12053083678862,-16.5241520489911));
#75783=CARTESIAN_POINT('Ctrl Pts',(4.30140354181539,-7.02213311397595,-16.6829158499228));
#75784=CARTESIAN_POINT('Ctrl Pts',(-0.884203313355227,-8.67324741747039,
-16.8946009178314));
#75785=CARTESIAN_POINT('Ctrl Pts',(-6.57909573114569,-5.95492941612458,
-17.1195184651114));
#75786=CARTESIAN_POINT('Ctrl Pts',(-7.89072598479452,-1.64495943571458,
-17.2915147454144));
#75787=CARTESIAN_POINT('Ctrl Pts',(-7.90123025115119,0.00640242758643106,
-17.357668491763));
#75788=CARTESIAN_POINT('',(-7.92320976604736,0.000404932896808444,-19.357668491763));
#75789=CARTESIAN_POINT('Ctrl Pts',(-7.90123025115119,0.00640242758643106,
-17.357668491763));
#75790=CARTESIAN_POINT('Ctrl Pts',(-7.90753226153451,0.997133170294752,
-17.3973572793687));
#75791=CARTESIAN_POINT('Ctrl Pts',(-7.27867603918967,4.62157268202392,-17.5428886009288));
#75792=CARTESIAN_POINT('Ctrl Pts',(-2.98788410044997,8.19005518207874,-17.7413411894661));
#75793=CARTESIAN_POINT('Ctrl Pts',(2.42295246631377,7.86165942351676,-17.9530262573749));
#75794=CARTESIAN_POINT('Ctrl Pts',(7.10076568002593,5.07023734257003,-18.1647113252837));
#75795=CARTESIAN_POINT('Ctrl Pts',(8.70021840697434,-0.629629868003249,
-18.3763963931923));
#75796=CARTESIAN_POINT('Ctrl Pts',(6.16354960033092,-5.46104416669315,-18.5880814611009));
#75797=CARTESIAN_POINT('Ctrl Pts',(2.81719811372365,-7.75668585711246,-18.7468452620326));
#75798=CARTESIAN_POINT('Ctrl Pts',(-1.2307231308085,-8.1423428124343,-18.9056090629639));
#75799=CARTESIAN_POINT('Ctrl Pts',(-6.06942212463287,-6.14568924132969,
-19.1092168062076));
#75800=CARTESIAN_POINT('Ctrl Pts',(-7.90917992093008,-2.41623274109057,
-19.2599032824738));
#75801=CARTESIAN_POINT('Ctrl Pts',(-7.92320976604736,0.000404932896808444,
-19.357668491763));
#75802=CARTESIAN_POINT('',(-7.90590625482663,-0.00331516544455179,-21.3576684917629));
#75803=CARTESIAN_POINT('Ctrl Pts',(-7.92320976604736,0.000404932896808444,
-19.357668491763));
#75804=CARTESIAN_POINT('Ctrl Pts',(-7.92436890655183,0.200066624748522,
-19.3657458164281));
#75805=CARTESIAN_POINT('Ctrl Pts',(-7.91747607560175,0.399707638355385,
-19.3738231410933));
#75806=CARTESIAN_POINT('Ctrl Pts',(-7.70314717160521,3.20752212073992,-19.4877429997129));
#75807=CARTESIAN_POINT('Ctrl Pts',(-4.45324040862703,8.23372206639351,-19.6994280676215));
#75808=CARTESIAN_POINT('Ctrl Pts',(2.98773583580864,8.19010927024974,-19.9640344025073));
#75809=CARTESIAN_POINT('Ctrl Pts',(6.91606556959596,4.45470813661777,-20.1757194704162));
#75810=CARTESIAN_POINT('Ctrl Pts',(8.69757176104145,-0.693127271215149,
-20.3874045383246));
#75811=CARTESIAN_POINT('Ctrl Pts',(6.25104031345718,-6.0839731343322,-20.5990896062335));
#75812=CARTESIAN_POINT('Ctrl Pts',(1.19920785351243,-8.14703919165728,-20.8107746741421));
#75813=CARTESIAN_POINT('Ctrl Pts',(-2.83927105800281,-7.74863346384884,
-20.9695384750738));
#75814=CARTESIAN_POINT('Ctrl Pts',(-6.18463760817827,-5.43715767248063,
-21.1283022760051));
#75815=CARTESIAN_POINT('Ctrl Pts',(-7.72004795960938,-2.48666735898332,
-21.257678948235));
#75816=CARTESIAN_POINT('Ctrl Pts',(-7.91116624839655,-0.58820461059737,
-21.3341343534875));
#75817=CARTESIAN_POINT('Ctrl Pts',(-7.90590625482663,-0.00331516544455179,
-21.3576684917629));
#75818=CARTESIAN_POINT('',(-7.90816594433051,-0.00119641522101588,-23.3576684917629));
#75819=CARTESIAN_POINT('Ctrl Pts',(-7.90590625482663,-0.00331516544455179,
-21.3576684917629));
#75820=CARTESIAN_POINT('Ctrl Pts',(-7.88750993085865,2.04227967710652,-21.4399768874419));
#75821=CARTESIAN_POINT('Ctrl Pts',(-6.05345660778066,6.73272226081268,-21.6281278170751));
#75822=CARTESIAN_POINT('Ctrl Pts',(1.89472071635594,9.16709128407982,-21.9221212806628));
#75823=CARTESIAN_POINT('Ctrl Pts',(7.5596726420224,4.34232712133296,-22.1867276155486));
#75824=CARTESIAN_POINT('Ctrl Pts',(8.15990728483216,-1.04513188083783,-22.3984126834575));
#75825=CARTESIAN_POINT('Ctrl Pts',(6.20812811174647,-6.13085029181979,-22.6100977513659));
#75826=CARTESIAN_POINT('Ctrl Pts',(0.86502967669206,-8.67997452520378,-22.8217828192748));
#75827=CARTESIAN_POINT('Ctrl Pts',(-4.32853973836911,-7.00543294876879,
-23.0334678871834));
#75828=CARTESIAN_POINT('Ctrl Pts',(-7.16180808017606,-4.10015679219509,
-23.1922316881149));
#75829=CARTESIAN_POINT('Ctrl Pts',(-7.89088696941476,-1.43010423471138,
-23.3002985563082));
#75830=CARTESIAN_POINT('Ctrl Pts',(-7.90804982156466,-0.0566024631711976,
-23.3554441575241));
#75831=CARTESIAN_POINT('Ctrl Pts',(-7.90816594433051,-0.00119641522101588,
-23.3576684917629));
#75832=CARTESIAN_POINT('',(-7.911,-5.53446177775641E-13,-25.357668491763));
#75833=CARTESIAN_POINT('Ctrl Pts',(-7.911,-7.19979631469414E-13,-23.3576684917629));
#75834=CARTESIAN_POINT('Ctrl Pts',(-7.9110000000002,2.20167589666604,-23.4462559274957));
#75835=CARTESIAN_POINT('Ctrl Pts',(-6.94214576672412,4.38610418338618,-23.5348433632284));
#75836=CARTESIAN_POINT('Ctrl Pts',(-3.67820201488356,7.34180684107597,-23.7120182346938));
#75837=CARTESIAN_POINT('Ctrl Pts',(-1.40868175871822,8.08992666571323,-23.8006056704266));
#75838=CARTESIAN_POINT('Ctrl Pts',(2.97309270521199,7.65454228025286,-23.977780541892));
#75839=CARTESIAN_POINT('Ctrl Pts',(5.05102072675538,6.47444880834276,-24.0663679776247));
#75840=CARTESIAN_POINT('Ctrl Pts',(7.66951518847842,2.93425195367785,-24.2435428490902));
#75841=CARTESIAN_POINT('Ctrl Pts',(8.18956872247065,0.601881960100011,-24.3321302848229));
#75842=CARTESIAN_POINT('Ctrl Pts',(7.32306689761382,-3.71537198232373,-24.5093051562884));
#75843=CARTESIAN_POINT('Ctrl Pts',(5.94329958850262,-5.66643518936447,-24.5978925920211));
#75844=CARTESIAN_POINT('Ctrl Pts',(2.16154501637934,-7.92205913232974,-24.7750674634866));
#75845=CARTESIAN_POINT('Ctrl Pts',(-0.210816529299463,-8.20894963713005,
-24.8636548992193));
#75846=CARTESIAN_POINT('Ctrl Pts',(-4.42123908576359,-6.91982244717881,
-25.0408297706847));
#75847=CARTESIAN_POINT('Ctrl Pts',(-6.22631625634127,-5.35390358803591,
-25.1294172064175));
#75848=CARTESIAN_POINT('Ctrl Pts',(-7.65317280859467,-2.31334857514596,
-25.2645592586878));
#75849=CARTESIAN_POINT('Ctrl Pts',(-7.91099999999992,-1.15702837836586,
-25.3111138752254));
#75850=CARTESIAN_POINT('Ctrl Pts',(-7.911,-5.53446177775641E-13,-25.357668491763));
#75851=CARTESIAN_POINT('',(-7.911,-4.99045249569008E-13,-27.357668491763));
#75852=CARTESIAN_POINT('Ctrl Pts',(-7.911,-5.53446177775641E-13,-25.357668491763));
#75853=CARTESIAN_POINT('Ctrl Pts',(-7.91100000000015,2.20167589666617,-25.4462559274957));
#75854=CARTESIAN_POINT('Ctrl Pts',(-6.94214576672406,4.38610418338626,-25.5348433632284));
#75855=CARTESIAN_POINT('Ctrl Pts',(-3.67820201488354,7.34180684107597,-25.7120182346938));
#75856=CARTESIAN_POINT('Ctrl Pts',(-1.40868175871824,8.08992666571321,-25.8006056704266));
#75857=CARTESIAN_POINT('Ctrl Pts',(2.97309270521189,7.65454228025289,-25.977780541892));
#75858=CARTESIAN_POINT('Ctrl Pts',(5.05102072675527,6.47444880834283,-26.0663679776247));
#75859=CARTESIAN_POINT('Ctrl Pts',(7.66951518847833,2.93425195367804,-26.2435428490902));
#75860=CARTESIAN_POINT('Ctrl Pts',(8.18956872247062,0.601881960100267,-26.3321302848229));
#75861=CARTESIAN_POINT('Ctrl Pts',(7.32306689761396,-3.71537198232343,-26.5093051562884));
#75862=CARTESIAN_POINT('Ctrl Pts',(5.94329958850287,-5.6664351893642,-26.5978925920211));
#75863=CARTESIAN_POINT('Ctrl Pts',(2.16154501637977,-7.92205913232961,-26.7750674634865));
#75864=CARTESIAN_POINT('Ctrl Pts',(-0.210816529298972,-8.20894963713005,
-26.8636548992193));
#75865=CARTESIAN_POINT('Ctrl Pts',(-4.42123908576311,-6.9198224471791,-27.0408297706847));
#75866=CARTESIAN_POINT('Ctrl Pts',(-6.22631625634086,-5.35390358803637,
-27.1294172064174));
#75867=CARTESIAN_POINT('Ctrl Pts',(-7.65317280859458,-2.31334857514636,
-27.2645592586878));
#75868=CARTESIAN_POINT('Ctrl Pts',(-7.91099999999993,-1.15702837836603,
-27.3111138752254));
#75869=CARTESIAN_POINT('Ctrl Pts',(-7.911,-4.99045249569008E-13,-27.357668491763));
#75870=CARTESIAN_POINT('',(-7.90149590314777,-6.97287683065524E-5,-29.3577571379651));
#75871=CARTESIAN_POINT('Ctrl Pts',(-7.911,-4.99045249569008E-13,-27.357668491763));
#75872=CARTESIAN_POINT('Ctrl Pts',(-7.91100000000014,2.2016758966663,-27.4462559274957));
#75873=CARTESIAN_POINT('Ctrl Pts',(-6.94214576672396,4.38610418338645,-27.5348433632284));
#75874=CARTESIAN_POINT('Ctrl Pts',(-3.67820201488322,7.34180684107615,-27.7120182346939));
#75875=CARTESIAN_POINT('Ctrl Pts',(-1.4086817587178,8.08992666571331,-27.8006056704266));
#75876=CARTESIAN_POINT('Ctrl Pts',(2.97309270521246,7.65454228025269,-27.977780541892));
#75877=CARTESIAN_POINT('Ctrl Pts',(5.05102072675582,6.47444880834243,-28.0663679776248));
#75878=CARTESIAN_POINT('Ctrl Pts',(7.66951518847865,2.93425195367728,-28.2435428490902));
#75879=CARTESIAN_POINT('Ctrl Pts',(8.18956872247071,0.601881960099353,-28.3321302848229));
#75880=CARTESIAN_POINT('Ctrl Pts',(7.3230668976135,-3.71537198232438,-28.5093051562884));
#75881=CARTESIAN_POINT('Ctrl Pts',(5.94329958850209,-5.66643518936504,-28.5978925920211));
#75882=CARTESIAN_POINT('Ctrl Pts',(2.16154501637852,-7.92205913232997,-28.7750674634866));
#75883=CARTESIAN_POINT('Ctrl Pts',(-0.210816529300357,-8.20894963713003,
-28.8636548992193));
#75884=CARTESIAN_POINT('Ctrl Pts',(-4.42123908576441,-6.9198224471783,-29.0408297706848));
#75885=CARTESIAN_POINT('Ctrl Pts',(-6.22631625634193,-5.35390358803515,
-29.1294172064175));
#75886=CARTESIAN_POINT('Ctrl Pts',(-7.6531636284135,-2.31336813762078,-29.2645583892041));
#75887=CARTESIAN_POINT('Ctrl Pts',(-7.91099036922816,-1.15707157067501,
-29.311112136258));
#75888=CARTESIAN_POINT('Ctrl Pts',(-7.9109999997302,-6.48282003627523E-5,
-29.3576658833118));
#75889=CARTESIAN_POINT('',(-7.91011762826041,0.00206862855998248,-31.357532306749));
#75890=CARTESIAN_POINT('Ctrl Pts',(-7.89569987159112,-7.27173581417825E-5,
-29.3578127892145));
#75891=CARTESIAN_POINT('Ctrl Pts',(-7.8945841079301,0.255048674726026,-29.3680723344091));
#75892=CARTESIAN_POINT('Ctrl Pts',(-7.88131840855623,0.510468153943764,
-29.3781339197719));
#75893=CARTESIAN_POINT('Ctrl Pts',(-7.85608173587964,0.764857387287981,
-29.3880686173644));
#75894=CARTESIAN_POINT('Ctrl Pts',(-7.83074434981928,1.02026182579864,-29.3980429619033));
#75895=CARTESIAN_POINT('Ctrl Pts',(-7.79334103122647,1.27462730778321,-29.4078894038951));
#75896=CARTESIAN_POINT('Ctrl Pts',(-7.74408245254443,1.52665288736753,-29.4176798696952));
#75897=CARTESIAN_POINT('Ctrl Pts',(-7.69482460245071,1.77867473921754,-29.4274701906835));
#75898=CARTESIAN_POINT('Ctrl Pts',(-7.63371264112704,2.02835647531821,-29.437204537136));
#75899=CARTESIAN_POINT('Ctrl Pts',(-7.56097485512378,2.27444610108197,-29.4469548322165));
#75900=CARTESIAN_POINT('Ctrl Pts',(-7.48841280666463,2.51994116398042,-29.4566815701748));
#75901=CARTESIAN_POINT('Ctrl Pts',(-7.40428182726746,2.76186135706339,-29.4664241797891));
#75902=CARTESIAN_POINT('Ctrl Pts',(-7.30881422844452,2.99901519620115,-29.4762540641735));
#75903=CARTESIAN_POINT('Ctrl Pts',(-7.21365811614968,3.23539526259412,-29.4860518761418));
#75904=CARTESIAN_POINT('Ctrl Pts',(-7.10723999461208,3.46704010152067,-29.4959363942986));
#75905=CARTESIAN_POINT('Ctrl Pts',(-6.98978405375929,3.69282117826146,-29.5059783251252));
#75906=CARTESIAN_POINT('Ctrl Pts',(-6.87400734420874,3.91537433269568,-29.5158766895689));
#75907=CARTESIAN_POINT('Ctrl Pts',(-6.74750682809626,4.13223049888618,-29.5259279978963));
#75908=CARTESIAN_POINT('Ctrl Pts',(-6.61048107240587,4.34235580006046,-29.5361999671321));
#75909=CARTESIAN_POINT('Ctrl Pts',(-6.47370176868633,4.55210317378352,-29.5464534613955));
#75910=CARTESIAN_POINT('Ctrl Pts',(-6.32643606094231,4.75514437299453,-29.556926823528));
#75911=CARTESIAN_POINT('Ctrl Pts',(-6.16979938689121,4.95090743069015,-29.5676874058276));
#75912=CARTESIAN_POINT('Ctrl Pts',(-6.10215945038996,5.0354431939272,-29.5723341152133));
#75913=CARTESIAN_POINT('Ctrl Pts',(-6.03277162499537,5.11862225049764,-29.5770343838391));
#75914=CARTESIAN_POINT('Ctrl Pts',(-5.96172351681003,5.20040060098812,-29.5817936352299));
#75915=CARTESIAN_POINT('Ctrl Pts',(-5.85905843910731,5.31857096360503,-29.588670791094));
#75916=CARTESIAN_POINT('Ctrl Pts',(-5.75283076577076,5.43362924400229,-29.5955541844561));
#75917=CARTESIAN_POINT('Ctrl Pts',(-5.64310303154788,5.54530414778243,-29.6023197989571));
#75918=CARTESIAN_POINT('Ctrl Pts',(-5.53544242143685,5.65487524537421,-29.6089579583078));
#75919=CARTESIAN_POINT('Ctrl Pts',(-5.42441198582704,5.76118885449211,-29.6154827345914));
#75920=CARTESIAN_POINT('Ctrl Pts',(-5.31009505383172,5.86394639032005,-29.6217769891479));
#75921=CARTESIAN_POINT('Ctrl Pts',(-4.99017996486874,6.15151259457539,-29.6393914139866));
#75922=CARTESIAN_POINT('Ctrl Pts',(-4.64623847650883,6.41344155099911,-29.6568267531459));
#75923=CARTESIAN_POINT('Ctrl Pts',(-4.28356735312668,6.64607706485341,-29.6741546816272));
#75924=CARTESIAN_POINT('Ctrl Pts',(-4.10061586087137,6.76343136098351,-29.6828958528123));
#75925=CARTESIAN_POINT('Ctrl Pts',(-3.91289804297522,6.87333210944896,-29.6916096906125));
#75926=CARTESIAN_POINT('Ctrl Pts',(-3.72109217012557,6.97531459386228,-29.7003053960622));
#75927=CARTESIAN_POINT('Ctrl Pts',(-3.33363652617021,7.18132334939974,-29.7178710738207));
#75928=CARTESIAN_POINT('Ctrl Pts',(-2.92950218373761,7.35501904141783,-29.7353627613642));
#75929=CARTESIAN_POINT('Ctrl Pts',(-2.51426387279328,7.49464824607955,-29.7528563019399));
#75930=CARTESIAN_POINT('Ctrl Pts',(-2.09919877920832,7.63421920418384,-29.7703425450557));
#75931=CARTESIAN_POINT('Ctrl Pts',(-1.67303963538504,7.73975436701759,-29.7878306396581));
#75932=CARTESIAN_POINT('Ctrl Pts',(-1.24130498229201,7.80951741044183,-29.8053963341193));
#75933=CARTESIAN_POINT('Ctrl Pts',(-0.834176089700127,7.87530446369241,
-29.8219609107229));
#75934=CARTESIAN_POINT('Ctrl Pts',(-0.422088617451437,7.90928259463422,
-29.8385944939792));
#75935=CARTESIAN_POINT('Ctrl Pts',(-0.00962658081288734,7.90997912443843,
-29.855360605038));
#75936=CARTESIAN_POINT('Ctrl Pts',(0.015301500377193,7.91002122080117,-29.8563739030887));
#75937=CARTESIAN_POINT('Ctrl Pts',(0.0402309621464365,7.90994174037809,
-29.857387685219));
#75938=CARTESIAN_POINT('Ctrl Pts',(0.0651607972488829,7.90974035367802,
-29.8584019654515));
#75939=CARTESIAN_POINT('Ctrl Pts',(0.304397112014934,7.90780776921566,-29.8681353898395));
#75940=CARTESIAN_POINT('Ctrl Pts',(0.543667487189482,7.8946490670781,-29.8779146847761));
#75941=CARTESIAN_POINT('Ctrl Pts',(0.782055855848812,7.87057601841741,-29.8877522426792));
#75942=CARTESIAN_POINT('Ctrl Pts',(1.07669559247589,7.84082256711823,-29.8999111222669));
#75943=CARTESIAN_POINT('Ctrl Pts',(1.36946104408517,7.79417976114013,-29.9119816789554));
#75944=CARTESIAN_POINT('Ctrl Pts',(1.65866474447215,7.73135886840473,-29.9239804189653));
#75945=CARTESIAN_POINT('Ctrl Pts',(1.95397836663951,7.66721077708829,-29.9362326528372));
#75946=CARTESIAN_POINT('Ctrl Pts',(2.24557891627073,7.58619388002973,-29.9484100034761));
#75947=CARTESIAN_POINT('Ctrl Pts',(2.53169299840934,7.48901518069949,-29.9605300455267));
#75948=CARTESIAN_POINT('Ctrl Pts',(2.82371124363093,7.38983113131884,-29.9729001930747));
#75949=CARTESIAN_POINT('Ctrl Pts',(3.11001518622114,7.27381144226102,-29.9852106424252));
#75950=CARTESIAN_POINT('Ctrl Pts',(3.38873034071391,7.14165481546951,-29.9974800788239));
#75951=CARTESIAN_POINT('Ctrl Pts',(3.54067584638536,7.06960776254835,-30.0041689354858));
#75952=CARTESIAN_POINT('Ctrl Pts',(3.6903660414768,6.99276382658616,-30.0108456029372));
#75953=CARTESIAN_POINT('Ctrl Pts',(3.83749696044171,6.91122971103455,-30.0175131086534));
#75954=CARTESIAN_POINT('Ctrl Pts',(4.10723893957669,6.76174941246346,-30.029736958001));
#75955=CARTESIAN_POINT('Ctrl Pts',(4.36838012447758,6.59650743440992,-30.0419300132912));
#75956=CARTESIAN_POINT('Ctrl Pts',(4.6191916329761,6.41676870673628,-30.0541109303471));
#75957=CARTESIAN_POINT('Ctrl Pts',(4.86657260539754,6.23948839970459,-30.0661252399148));
#75958=CARTESIAN_POINT('Ctrl Pts',(5.1039054682342,6.04810464874452,-30.0781277410248));
#75959=CARTESIAN_POINT('Ctrl Pts',(5.32950460302231,5.84378910404561,-30.0901363344138));
#75960=CARTESIAN_POINT('Ctrl Pts',(5.54573629318662,5.64795725567181,-30.1016463007416));
#75961=CARTESIAN_POINT('Ctrl Pts',(5.75118907158626,5.44024461804703,-30.1131618639188));
#75962=CARTESIAN_POINT('Ctrl Pts',(5.94434311403979,5.22165265539691,-30.1246987861385));
#75963=CARTESIAN_POINT('Ctrl Pts',(6.09093752971214,5.05575210975818,-30.1334547425243));
#75964=CARTESIAN_POINT('Ctrl Pts',(6.23044718286647,4.88358435767637,-30.1422230018536));
#75965=CARTESIAN_POINT('Ctrl Pts',(6.36218972045515,4.70557793093048,-30.1510104547341));
#75966=CARTESIAN_POINT('Ctrl Pts',(6.47502102515782,4.55312377494704,-30.1585364959936));
#75967=CARTESIAN_POINT('Ctrl Pts',(6.5822020773836,4.39662647188323,-30.1661748264367));
#75968=CARTESIAN_POINT('Ctrl Pts',(6.68326889010009,4.23635763789733,-30.1738931191833));
#75969=CARTESIAN_POINT('Ctrl Pts',(6.82187292273323,4.01656336420068,-30.1844780626576));
#75970=CARTESIAN_POINT('Ctrl Pts',(6.94897773567381,3.78967367522231,-30.1952133964538));
#75971=CARTESIAN_POINT('Ctrl Pts',(7.06437106698293,3.55693002058069,-30.2060157398447));
#75972=CARTESIAN_POINT('Ctrl Pts',(7.17996231729417,3.32378717136383,-30.2168366110743));
#75973=CARTESIAN_POINT('Ctrl Pts',(7.28380100830786,3.08477018935011,-30.2277247219611));
#75974=CARTESIAN_POINT('Ctrl Pts',(7.37566767430952,2.84117894413984,-30.2385962620053));
#75975=CARTESIAN_POINT('Ctrl Pts',(7.46761138924782,2.59738339798738,-30.2494769200533));
#75976=CARTESIAN_POINT('Ctrl Pts',(7.54756210101163,2.34900604493784,-30.260340979451));
#75977=CARTESIAN_POINT('Ctrl Pts',(7.61530687772506,2.09740160556108,-30.2711044186453));
#75978=CARTESIAN_POINT('Ctrl Pts',(7.64910139818574,1.97188858762782,-30.2764737664197));
#75979=CARTESIAN_POINT('Ctrl Pts',(7.67985864228526,1.84557329561306,-30.2818180746663));
#75980=CARTESIAN_POINT('Ctrl Pts',(7.70755389160994,1.71862844955189,-30.2871269129571));
#75981=CARTESIAN_POINT('Ctrl Pts',(7.75778494272112,1.48838776906388,-30.2967555869726));
#75982=CARTESIAN_POINT('Ctrl Pts',(7.7980703493988,1.2561018325183,-30.306339698528));
#75983=CARTESIAN_POINT('Ctrl Pts',(7.82835458766272,1.02258119335211,-30.3158624553201));
#75984=CARTESIAN_POINT('Ctrl Pts',(7.85870170280127,0.788575712935363,-30.3254049834922));
#75985=CARTESIAN_POINT('Ctrl Pts',(7.87900595604867,0.553329539576292,-30.334885901864));
#75986=CARTESIAN_POINT('Ctrl Pts',(7.8891598651935,0.317662158590311,-30.3442883133212));
#75987=CARTESIAN_POINT('Ctrl Pts',(7.89921463198212,0.0842958243343077,
-30.353598920015));
#75988=CARTESIAN_POINT('Ctrl Pts',(7.89931609340655,-0.149484304558608,
-30.3628325453864));
#75989=CARTESIAN_POINT('Ctrl Pts',(7.88931193660423,-0.382866602834017,
-30.3719727824525));
#75990=CARTESIAN_POINT('Ctrl Pts',(7.87955525618199,-0.610475640304844,
-30.3808869142278));
#75991=CARTESIAN_POINT('Ctrl Pts',(7.8601864526231,-0.837706877758794,-30.3897122209094));
#75992=CARTESIAN_POINT('Ctrl Pts',(7.83102226607746,-1.06378235556531,-30.3984334832386));
#75993=CARTESIAN_POINT('Ctrl Pts',(7.80977207922144,-1.22850994498162,-30.4047881420193));
#75994=CARTESIAN_POINT('Ctrl Pts',(7.78332050071093,-1.39262344223998,-30.411087561994));
#75995=CARTESIAN_POINT('Ctrl Pts',(7.75158330011696,-1.55581053101365,-30.4173258556459));
#75996=CARTESIAN_POINT('Ctrl Pts',(7.70457969503489,-1.79749477951883,-30.4265649279559));
#75997=CARTESIAN_POINT('Ctrl Pts',(7.64648254573122,-2.03708246863251,-30.4359439692));
#75998=CARTESIAN_POINT('Ctrl Pts',(7.57715365975328,-2.27333984897705,-30.4454542601858));
#75999=CARTESIAN_POINT('Ctrl Pts',(7.50910989560062,-2.50521782077371,-30.4547882627121));
#76000=CARTESIAN_POINT('Ctrl Pts',(7.43024698951954,-2.73388696816542,-30.4642486942303));
#76001=CARTESIAN_POINT('Ctrl Pts',(7.34048365772138,-2.95818606679694,-30.4738273114881));
#76002=CARTESIAN_POINT('Ctrl Pts',(7.29244812213151,-3.07821645247063,-30.4789531685722));
#76003=CARTESIAN_POINT('Ctrl Pts',(7.24129187452229,-3.19699555119828,-30.4841128704931));
#76004=CARTESIAN_POINT('Ctrl Pts',(7.18700835380188,-3.31434728423305,-30.4893051539998));
#76005=CARTESIAN_POINT('Ctrl Pts',(7.08428777633514,-3.5364116902273,-30.4991304997605));
#76006=CARTESIAN_POINT('Ctrl Pts',(6.97036643537057,-3.7533632004455,-30.5090725133482));
#76007=CARTESIAN_POINT('Ctrl Pts',(6.84623930951474,-3.9644337130622,-30.5191226350746));
#76008=CARTESIAN_POINT('Ctrl Pts',(6.72111484907999,-4.17720013154452,-30.529253507353));
#76009=CARTESIAN_POINT('Ctrl Pts',(6.585620644126,-4.38399005579828,-30.5394942320004));
#76010=CARTESIAN_POINT('Ctrl Pts',(6.44081709798858,-4.58405060379496,-30.5498360413406));
#76011=CARTESIAN_POINT('Ctrl Pts',(6.29708880068084,-4.78262558824133,-30.5601010568543));
#76012=CARTESIAN_POINT('Ctrl Pts',(6.14418968361826,-4.97457026492628,-30.5704656614117));
#76013=CARTESIAN_POINT('Ctrl Pts',(5.98318592183888,-5.15918983316727,-30.5809212812048));
#76014=CARTESIAN_POINT('Ctrl Pts',(5.86457305787863,-5.29520066602083,-30.5886240267458));
#76015=CARTESIAN_POINT('Ctrl Pts',(5.7415621333112,-5.42723669077786,-30.5963761698626));
#76016=CARTESIAN_POINT('Ctrl Pts',(5.6145860317735,-5.55503702543636,-30.6041742823954));
#76017=CARTESIAN_POINT('Ctrl Pts',(5.47707440897578,-5.6934412700159,-30.6126194236162));
#76018=CARTESIAN_POINT('Ctrl Pts',(5.33451368350287,-5.82666177022762,-30.620869880412));
#76019=CARTESIAN_POINT('Ctrl Pts',(5.18736468424763,-5.95453344434437,-30.6289856878826));
#76020=CARTESIAN_POINT('Ctrl Pts',(5.03910865941913,-6.08336711761884,-30.6371625518772));
#76021=CARTESIAN_POINT('Ctrl Pts',(4.88619485176865,-6.20677180674103,-30.6452027329487));
#76022=CARTESIAN_POINT('Ctrl Pts',(4.72904226888832,-6.32456931573893,-30.6531676313768));
#76023=CARTESIAN_POINT('Ctrl Pts',(4.57154450184332,-6.44262556585327,-30.6611500246292));
#76024=CARTESIAN_POINT('Ctrl Pts',(4.40978902703204,-6.55505063482755,-30.6690568041598));
#76025=CARTESIAN_POINT('Ctrl Pts',(4.24414915186498,-6.66164613483122,-30.6769497757334));
#76026=CARTESIAN_POINT('Ctrl Pts',(4.1790019173349,-6.70357083461492,-30.6800541325178));
#76027=CARTESIAN_POINT('Ctrl Pts',(4.11325330167021,-6.74459349773157,-30.6831563533496));
#76028=CARTESIAN_POINT('Ctrl Pts',(4.04692412666748,-6.78470090112318,-30.6862601985267));
#76029=CARTESIAN_POINT('Ctrl Pts',(3.87255137163058,-6.89013924596139,-30.6944198964985));
#76030=CARTESIAN_POINT('Ctrl Pts',(3.69377325136641,-6.98893125659474,-30.7023236757362));
#76031=CARTESIAN_POINT('Ctrl Pts',(3.51129648404317,-7.08067426001595,-30.7100645035343));
#76032=CARTESIAN_POINT('Ctrl Pts',(3.3227320584461,-7.17547792733447,-30.7180635752452));
#76033=CARTESIAN_POINT('Ctrl Pts',(3.13021895902962,-7.26275441992961,-30.7258886416189));
#76034=CARTESIAN_POINT('Ctrl Pts',(2.93451511514658,-7.34211356730782,-30.733642288336));
#76035=CARTESIAN_POINT('Ctrl Pts',(2.74578128959534,-7.41864632813661,-30.7411197878979));
#76036=CARTESIAN_POINT('Ctrl Pts',(2.55408037837696,-7.48781629011548,-30.7485308644529));
#76037=CARTESIAN_POINT('Ctrl Pts',(2.36006295633384,-7.54931729946368,-30.7559675286102));
#76038=CARTESIAN_POINT('Ctrl Pts',(2.16646713096828,-7.61068466812676,-30.7633880330181));
#76039=CARTESIAN_POINT('Ctrl Pts',(1.97056531729853,-7.66441681384306,-30.7708340139462));
#76040=CARTESIAN_POINT('Ctrl Pts',(1.7729674110032,-7.71024644124962,-30.7783968834934));
#76041=CARTESIAN_POINT('Ctrl Pts',(1.57577205934891,-7.75598270264054,-30.7859443456494));
#76042=CARTESIAN_POINT('Ctrl Pts',(1.37688788298791,-7.79384911456881,-30.7936082206489));
#76043=CARTESIAN_POINT('Ctrl Pts',(1.17687850676287,-7.82360973146476,-30.8014793630427));
#76044=CARTESIAN_POINT('Ctrl Pts',(1.15334442373915,-7.82711151144171,-30.8024055202164));
#76045=CARTESIAN_POINT('Ctrl Pts',(1.12979471031162,-7.8305010950992,-30.803334547013));
#76046=CARTESIAN_POINT('Ctrl Pts',(1.10623024247913,-7.83377811993991,-30.8042665914413));
#76047=CARTESIAN_POINT('Ctrl Pts',(0.905979520921187,-7.8616262595024,-30.8121871000065));
#76048=CARTESIAN_POINT('Ctrl Pts',(0.704667374967774,-7.88134454934293,
-30.8203255296031));
#76049=CARTESIAN_POINT('Ctrl Pts',(0.502870338412337,-7.89333825659674,
-30.8287727118013));
#76050=CARTESIAN_POINT('Ctrl Pts',(0.301909383542035,-7.90528227174832,
-30.8371848957933));
#76051=CARTESIAN_POINT('Ctrl Pts',(0.100467690963634,-7.9095663226281,-30.845903279251));
#76052=CARTESIAN_POINT('Ctrl Pts',(-0.100936048976943,-7.90659976529281,
-30.8550175694211));
#76053=CARTESIAN_POINT('Ctrl Pts',(-0.183832286805069,-7.90537875299944,
-30.858768941495));
#76054=CARTESIAN_POINT('Ctrl Pts',(-0.26672270296442,-7.90292947207764,
-30.8625873834358));
#76055=CARTESIAN_POINT('Ctrl Pts',(-0.349573704434322,-7.89928047876121,
-30.8664791502737));
#76056=CARTESIAN_POINT('Ctrl Pts',(-0.555271224667018,-7.89022097600061,
-30.8761413966397));
#76057=CARTESIAN_POINT('Ctrl Pts',(-0.760421052167959,-7.87245429262813,
-30.885478905345));
#76058=CARTESIAN_POINT('Ctrl Pts',(-0.964441435025923,-7.84640026727707,
-30.8945578142934));
#76059=CARTESIAN_POINT('Ctrl Pts',(-1.17049180476456,-7.82008700640792,
-30.903727057677));
#76060=CARTESIAN_POINT('Ctrl Pts',(-1.37539052845679,-7.78532100936025,
-30.9126325296072));
#76061=CARTESIAN_POINT('Ctrl Pts',(-1.57858110370323,-7.74250281151564,
-30.9213423618969));
#76062=CARTESIAN_POINT('Ctrl Pts',(-1.78447308460689,-7.69911534847875,
-30.9301679908479));
#76063=CARTESIAN_POINT('Ctrl Pts',(-1.98861165089484,-7.64746051126545,
-30.9387927435451));
#76064=CARTESIAN_POINT('Ctrl Pts',(-2.19045516918942,-7.58791701913866,
-30.9472875055138));
#76065=CARTESIAN_POINT('Ctrl Pts',(-2.23095995217108,-7.5759681775462,-30.9489921849255));
#76066=CARTESIAN_POINT('Ctrl Pts',(-2.27137241886445,-7.5637015280104,-30.950691629594));
#76067=CARTESIAN_POINT('Ctrl Pts',(-2.31168834357439,-7.55111993061152,
-30.9523864123576));
#76068=CARTESIAN_POINT('Ctrl Pts',(-2.57166766327819,-7.46998685091454,
-30.9633153064138));
#76069=CARTESIAN_POINT('Ctrl Pts',(-2.82801669922837,-7.37561949093419,
-30.9740590899625));
#76070=CARTESIAN_POINT('Ctrl Pts',(-3.07923169674846,-7.26866601893759,
-30.9846904548434));
#76071=CARTESIAN_POINT('Ctrl Pts',(-3.33250716791111,-7.16083531105857,
-30.9954090185275));
#76072=CARTESIAN_POINT('Ctrl Pts',(-3.58056374531226,-7.04021220390749,
-31.0060133118579));
#76073=CARTESIAN_POINT('Ctrl Pts',(-3.82190987656764,-6.90747907848244,
-31.0165778300476));
#76074=CARTESIAN_POINT('Ctrl Pts',(-4.06373872533062,-6.7744804729225,-31.0271634783789));
#76075=CARTESIAN_POINT('Ctrl Pts',(-4.29883021368951,-6.62932435886097,
-31.0377091923015));
#76076=CARTESIAN_POINT('Ctrl Pts',(-4.5257357913364,-6.47270005511793,-31.048289914918));
#76077=CARTESIAN_POINT('Ctrl Pts',(-4.75199172242079,-6.31652417772732,
-31.0588403441844));
#76078=CARTESIAN_POINT('Ctrl Pts',(-4.97010874902366,-6.14894660191629,
-31.0694255819671));
#76079=CARTESIAN_POINT('Ctrl Pts',(-5.17870111614328,-5.97063918916825,
-31.0801199295073));
#76080=CARTESIAN_POINT('Ctrl Pts',(-5.38620263206032,-5.79326424992492,
-31.0907583500641));
#76081=CARTESIAN_POINT('Ctrl Pts',(-5.58427925653382,-5.60527220954998,
-31.1015047421654));
#76082=CARTESIAN_POINT('Ctrl Pts',(-5.77161221360211,-5.40730016750988,
-31.1124322474445));
#76083=CARTESIAN_POINT('Ctrl Pts',(-5.84246648446754,-5.33242191378447,
-31.1165653184804));
#76084=CARTESIAN_POINT('Ctrl Pts',(-5.91178424954878,-5.2561156581599,-31.1207242987006));
#76085=CARTESIAN_POINT('Ctrl Pts',(-5.97949564096399,-5.17841460947582,
-31.1249131455985));
#76086=CARTESIAN_POINT('Ctrl Pts',(-6.15602892318531,-4.97583686192772,
-31.1358340685944));
#76087=CARTESIAN_POINT('Ctrl Pts',(-6.32164132715477,-4.763781453909,-31.1469580012156));
#76088=CARTESIAN_POINT('Ctrl Pts',(-6.4760637532379,-4.54363763691952,-31.1583550752257));
#76089=CARTESIAN_POINT('Ctrl Pts',(-6.6121491758484,-4.34963495783987,-31.1683987953805));
#76090=CARTESIAN_POINT('Ctrl Pts',(-6.73954516965971,-4.14935043551168,
-31.1786546396211));
#76091=CARTESIAN_POINT('Ctrl Pts',(-6.8580827178115,-3.94370481381216,-31.189170605431));
#76092=CARTESIAN_POINT('Ctrl Pts',(-6.92636458653132,-3.82524557821441,
-31.1952281779732));
#76093=CARTESIAN_POINT('Ctrl Pts',(-6.99151032737667,-3.7049668770132,-31.2012588830443));
#76094=CARTESIAN_POINT('Ctrl Pts',(-7.05325504757299,-3.58291852259966,
-31.2071169359491));
#76095=CARTESIAN_POINT('Ctrl Pts',(-7.09044186461077,-3.50941280727845,
-31.2106450488124));
#76096=CARTESIAN_POINT('Ctrl Pts',(-7.12639444898179,-3.43526600339684,
-31.2141105362931));
#76097=CARTESIAN_POINT('Ctrl Pts',(-7.16105018869253,-3.36049679187304,
-31.2174815505884));
#76098=CARTESIAN_POINT('Ctrl Pts',(-7.26544716940653,-3.13526195347102,
-31.2276363970096));
#76099=CARTESIAN_POINT('Ctrl Pts',(-7.3592402758094,-2.90524691619423,-31.2377407236085));
#76100=CARTESIAN_POINT('Ctrl Pts',(-7.44224561077067,-2.67144349523618,
-31.2478073653404));
#76101=CARTESIAN_POINT('Ctrl Pts',(-7.52689158749378,-2.43301883328608,
-31.2580729792569));
#76102=CARTESIAN_POINT('Ctrl Pts',(-7.60031955403292,-2.19065390436773,
-31.2682994038636));
#76103=CARTESIAN_POINT('Ctrl Pts',(-7.6622941268666,-1.94536481155424,-31.2785002503257));
#76104=CARTESIAN_POINT('Ctrl Pts',(-7.68376815431407,-1.86037278222993,
-31.2820348169536));
#76105=CARTESIAN_POINT('Ctrl Pts',(-7.70386670237713,-1.7750294130185,-31.2855663126582));
#76106=CARTESIAN_POINT('Ctrl Pts',(-7.72257873394354,-1.68937622778368,
-31.2890953036726));
#76107=CARTESIAN_POINT('Ctrl Pts',(-7.77687405767233,-1.4408426891231,-31.299335116965));
#76108=CARTESIAN_POINT('Ctrl Pts',(-7.81949938009848,-1.18970175964949,
-31.3095538421798));
#76109=CARTESIAN_POINT('Ctrl Pts',(-7.8503183535253,-0.937080670013483,
-31.3197653124211));
#76110=CARTESIAN_POINT('Ctrl Pts',(-7.88089443223502,-0.686450572330713,
-31.3298963026237));
#76111=CARTESIAN_POINT('Ctrl Pts',(-7.89984967201503,-0.434362651769033,
-31.3400201517598));
#76112=CARTESIAN_POINT('Ctrl Pts',(-7.90700057737854,-0.181910412584309,
-31.3501503684347));
#76113=CARTESIAN_POINT('Ctrl Pts',(-7.9087176329076,-0.12129228228041,-31.3525828079186));
#76114=CARTESIAN_POINT('Ctrl Pts',(-7.90975385920825,-0.0606531482638515,
-31.3550156145312));
#76115=CARTESIAN_POINT('Ctrl Pts',(-7.91010626430346,-8.17558293495676E-6,
-31.357448975289));
#76116=CARTESIAN_POINT('',(-7.91695845694372,0.000899907545194336,-33.3576681232209));
#76117=CARTESIAN_POINT('Ctrl Pts',(-7.91013619988552,0.00546266007265983,
-31.357668491763));
#76118=CARTESIAN_POINT('Ctrl Pts',(-7.91398572774975,0.755458957314721,
-31.3877621066932));
#76119=CARTESIAN_POINT('Ctrl Pts',(-7.45882838377432,4.13741011254259,-31.5236982555779));
#76120=CARTESIAN_POINT('Ctrl Pts',(-3.73499777086688,7.88289450337639,-31.7125556714397));
#76121=CARTESIAN_POINT('Ctrl Pts',(1.71919252665886,8.05336725367734,-31.9242407393484));
#76122=CARTESIAN_POINT('Ctrl Pts',(5.36476995012875,6.27072755588009,-32.0830045402799));
#76123=CARTESIAN_POINT('Ctrl Pts',(7.69321605282543,2.93715043272905,-32.2417683412114));
#76124=CARTESIAN_POINT('Ctrl Pts',(8.3628728449941,-2.46361402060145,-32.45345340912));
#76125=CARTESIAN_POINT('Ctrl Pts',(3.98770187756028,-8.46131879696375,-32.718059744006));
#76126=CARTESIAN_POINT('Ctrl Pts',(-4.97458638376742,-7.92962921668339,
-33.0355873458691));
#76127=CARTESIAN_POINT('Ctrl Pts',(-7.89551479792441,-2.6937012197221,-33.2487900774767));
#76128=CARTESIAN_POINT('Ctrl Pts',(-7.91988269843863,-0.0366651763938352,
-33.3561502751302));
#76129=CARTESIAN_POINT('Ctrl Pts',(-7.91993966167306,0.000895686316540435,
-33.3576679388293));
#76130=CARTESIAN_POINT('',(-7.9066350512344,-0.00678589508903775,-35.3576684826878));
#76131=CARTESIAN_POINT('Ctrl Pts',(-7.91099994785175,0.000908344479788625,
-33.3576684917629));
#76132=CARTESIAN_POINT('Ctrl Pts',(-7.91097574369575,0.211708411063882,
-33.3661955907321));
#76133=CARTESIAN_POINT('Ctrl Pts',(-7.9025215909712,0.422656322421778,-33.3747226897013));
#76134=CARTESIAN_POINT('Ctrl Pts',(-7.8856278558695,0.633083184688264,-33.3832497886705));
#76135=CARTESIAN_POINT('Ctrl Pts',(-7.8687588186536,0.8432024122853,-33.3917644214021));
#76136=CARTESIAN_POINT('Ctrl Pts',(-7.84347483866858,1.05280185273585,-33.4002790541336));
#76137=CARTESIAN_POINT('Ctrl Pts',(-7.80981823579319,1.26121375027078,-33.4087936868652));
#76138=CARTESIAN_POINT('Ctrl Pts',(-7.77586205415544,1.47148073040437,-33.4173841086817));
#76139=CARTESIAN_POINT('Ctrl Pts',(-7.73338344372194,1.68053865778044,-33.4259745304982));
#76140=CARTESIAN_POINT('Ctrl Pts',(-7.68247971765538,1.88770399899287,-33.4345649523148));
#76141=CARTESIAN_POINT('Ctrl Pts',(-7.63221165482289,2.09228235098158,-33.4430481007402));
#76142=CARTESIAN_POINT('Ctrl Pts',(-7.5737276962571,2.29501483569678,-33.4515312491657));
#76143=CARTESIAN_POINT('Ctrl Pts',(-7.5071733698418,2.49524928516933,-33.4600143975911));
#76144=CARTESIAN_POINT('Ctrl Pts',(-7.43935662741166,2.69928182245006,-33.4686584561032));
#76145=CARTESIAN_POINT('Ctrl Pts',(-7.36316031003098,2.90072034532527,-33.4773025146153));
#76146=CARTESIAN_POINT('Ctrl Pts',(-7.27879312200625,3.09888555565296,-33.4859465731274));
#76147=CARTESIAN_POINT('Ctrl Pts',(-7.19442593398151,3.29705076598066,-33.4945906316394));
#76148=CARTESIAN_POINT('Ctrl Pts',(-7.10188792480581,3.49194237486484,-33.5032346901515));
#76149=CARTESIAN_POINT('Ctrl Pts',(-7.00144247287156,3.6828961835857,-33.5118787486636));
#76150=CARTESIAN_POINT('Ctrl Pts',(-6.90969162978071,3.8573209345741,-33.5197745731229));
#76151=CARTESIAN_POINT('Ctrl Pts',(-6.81142359265998,4.02830602410947,-33.5276703975822));
#76152=CARTESIAN_POINT('Ctrl Pts',(-6.70693643722551,4.19534559089199,-33.5355662220415));
#76153=CARTESIAN_POINT('Ctrl Pts',(-6.6024257369623,4.36242279787988,-33.5434638257227));
#76154=CARTESIAN_POINT('Ctrl Pts',(-6.491693306939,4.52555241994048,-33.5513614294039));
#76155=CARTESIAN_POINT('Ctrl Pts',(-6.37508079460592,4.68425723698504,-33.5592590330851));
#76156=CARTESIAN_POINT('Ctrl Pts',(-6.25842279971076,4.84302395391966,-33.5671597170812));
#76157=CARTESIAN_POINT('Ctrl Pts',(-6.13588035452739,4.99736215080486,-33.5750604010772));
#76158=CARTESIAN_POINT('Ctrl Pts',(-6.00783581806122,5.14682715692112,-33.5829610850732));
#76159=CARTESIAN_POINT('Ctrl Pts',(-5.87965071696043,5.29645624261899,-33.5908704422762));
#76160=CARTESIAN_POINT('Ctrl Pts',(-5.74595168043331,5.44120118966321,-33.5987797994791));
#76161=CARTESIAN_POINT('Ctrl Pts',(-5.60715925335904,5.58065283882362,-33.606689156682));
#76162=CARTESIAN_POINT('Ctrl Pts',(-5.46828419008667,5.72018751667909,-33.6146032230699));
#76163=CARTESIAN_POINT('Ctrl Pts',(-5.32430993930035,5.85442237952135,-33.6225172894578));
#76164=CARTESIAN_POINT('Ctrl Pts',(-5.1756908903522,5.98298794980612,-33.6304313558457));
#76165=CARTESIAN_POINT('Ctrl Pts',(-5.02686440403994,6.11173296749824,-33.6383564684156));
#76166=CARTESIAN_POINT('Ctrl Pts',(-4.87338043208956,6.23479266745573,-33.6462815809855));
#76167=CARTESIAN_POINT('Ctrl Pts',(-4.71572425983158,6.35183955285679,-33.6542066935555));
#76168=CARTESIAN_POINT('Ctrl Pts',(-4.60673677950182,6.43275389282588,-33.6596853122353));
#76169=CARTESIAN_POINT('Ctrl Pts',(-4.49575603825922,6.51079565603233,-33.6651639309152));
#76170=CARTESIAN_POINT('Ctrl Pts',(-4.38294931482201,6.5858694417443,-33.6706425495951));
#76171=CARTESIAN_POINT('Ctrl Pts',(-4.21565374072506,6.69720599773693,-33.6787674966672));
#76172=CARTESIAN_POINT('Ctrl Pts',(-4.04397423338339,6.80225710806551,-33.6868924437393));
#76173=CARTESIAN_POINT('Ctrl Pts',(-3.86841141753026,6.90067490211802,-33.6950173908114));
#76174=CARTESIAN_POINT('Ctrl Pts',(-3.69300332412921,6.99900596116147,-33.7031351774165));
#76175=CARTESIAN_POINT('Ctrl Pts',(-3.51371902384952,7.09071520313219,-33.7112529640217));
#76176=CARTESIAN_POINT('Ctrl Pts',(-3.33108747943779,7.17549839414189,-33.7193707506269));
#76177=CARTESIAN_POINT('Ctrl Pts',(-3.14859091122309,7.26021892504141,-33.7274825376773));
#76178=CARTESIAN_POINT('Ctrl Pts',(-2.96275232132562,7.3380234769545,-33.7355943247276));
#76179=CARTESIAN_POINT('Ctrl Pts',(-2.77412510792397,7.40865378362262,-33.743706111778));
#76180=CARTESIAN_POINT('Ctrl Pts',(-2.58561050891936,7.47924192251838,-33.7518130559216));
#76181=CARTESIAN_POINT('Ctrl Pts',(-2.39431090591447,7.54266424523087,-33.7599200000652));
#76182=CARTESIAN_POINT('Ctrl Pts',(-2.20080003875554,7.59871042936982,-33.7680269442088));
#76183=CARTESIAN_POINT('Ctrl Pts',(-2.00737724493054,7.65473110499669,-33.7761301986082));
#76184=CARTESIAN_POINT('Ctrl Pts',(-1.81174550159248,7.70338224834809,-33.7842334530076));
#76185=CARTESIAN_POINT('Ctrl Pts',(-1.61449463763728,7.7445030870315,-33.792336707407));
#76186=CARTESIAN_POINT('Ctrl Pts',(-1.41586911157071,7.7859105011843,-33.8004964342425));
#76187=CARTESIAN_POINT('Ctrl Pts',(-1.21560212248025,7.81968214425426,-33.8086561610779));
#76188=CARTESIAN_POINT('Ctrl Pts',(-1.01430848775576,7.8457057867133,-33.8168158879134));
#76189=CARTESIAN_POINT('Ctrl Pts',(-0.814483563081723,7.87153955140854,
-33.8249160784758));
#76190=CARTESIAN_POINT('Ctrl Pts',(-0.613647249258924,7.88973798165448,
-33.8330162690381));
#76191=CARTESIAN_POINT('Ctrl Pts',(-0.41240856183088,7.90024304550997,-33.8411164596004));
#76192=CARTESIAN_POINT('Ctrl Pts',(-0.211171074422902,7.91074804672199,
-33.84921660186));
#76193=CARTESIAN_POINT('Ctrl Pts',(-0.00953153840357959,7.9135597564478,
-33.8573167441196));
#76194=CARTESIAN_POINT('Ctrl Pts',(0.191898302812708,7.90867220469894,-33.8654168863791));
#76195=CARTESIAN_POINT('Ctrl Pts',(0.393352921797685,7.90378405173516,-33.8735180250325));
#76196=CARTESIAN_POINT('Ctrl Pts',(0.594597474016501,7.8911947568253,-33.8816191636859));
#76197=CARTESIAN_POINT('Ctrl Pts',(0.795022058686897,7.87095044617874,-33.8897203023393));
#76198=CARTESIAN_POINT('Ctrl Pts',(0.997995276040814,7.85044870547761,-33.8979244564325));
#76199=CARTESIAN_POINT('Ctrl Pts',(1.20012719317032,7.82209596204581,-33.9061286105257));
#76200=CARTESIAN_POINT('Ctrl Pts',(1.40079152651456,7.78599409833099,-33.914332764619));
#76201=CARTESIAN_POINT('Ctrl Pts',(1.59912497581198,7.75031158795511,-33.9224416206013));
#76202=CARTESIAN_POINT('Ctrl Pts',(1.79602444336803,7.70705911654199,-33.9305504765836));
#76203=CARTESIAN_POINT('Ctrl Pts',(1.99089693392044,7.65638624930236,-33.9386593325659));
#76204=CARTESIAN_POINT('Ctrl Pts',(2.18920473894702,7.60482009418108,-33.9469111357146));
#76205=CARTESIAN_POINT('Ctrl Pts',(2.3854131010413,7.5455695796454,-33.9551629388633));
#76206=CARTESIAN_POINT('Ctrl Pts',(2.57891442908054,7.47884492201036,-33.963414742012));
#76207=CARTESIAN_POINT('Ctrl Pts',(2.77241575711979,7.41212026437533,-33.9716665451607));
#76208=CARTESIAN_POINT('Ctrl Pts',(2.96320973631898,7.33792161416906,-33.9799183483094));
#76209=CARTESIAN_POINT('Ctrl Pts',(3.1507110563056,7.25651023837724,-33.988170151458));
#76210=CARTESIAN_POINT('Ctrl Pts',(3.32861845617368,7.1792644558524,-33.9959997328312));
#76211=CARTESIAN_POINT('Ctrl Pts',(3.50390141623488,7.0953774368945,-34.0038293142043));
#76212=CARTESIAN_POINT('Ctrl Pts',(3.67602498412764,7.00505255626747,-34.0116588955775));
#76213=CARTESIAN_POINT('Ctrl Pts',(3.84800345053782,6.91480382020479,-34.0194818765537));
#76214=CARTESIAN_POINT('Ctrl Pts',(4.01682751842343,6.81812819118313,-34.0273048575299));
#76215=CARTESIAN_POINT('Ctrl Pts',(4.18198202198616,6.71527716239506,-34.0351278385061));
#76216=CARTESIAN_POINT('Ctrl Pts',(4.3470264368443,6.61249469205547,-34.042945604839));
#76217=CARTESIAN_POINT('Ctrl Pts',(4.5084058612547,6.50354520522174,-34.0507633711718));
#76218=CARTESIAN_POINT('Ctrl Pts',(4.66562943363786,6.3887262414328,-34.0585811375046));
#76219=CARTESIAN_POINT('Ctrl Pts',(4.8227776502318,6.27396230930038,-34.0663951568551));
#76220=CARTESIAN_POINT('Ctrl Pts',(4.9757736987484,6.15333471093492,-34.0742091762056));
#76221=CARTESIAN_POINT('Ctrl Pts',(5.12415530071364,6.02718453792219,-34.0820231955561));
#76222=CARTESIAN_POINT('Ctrl Pts',(5.2724936858831,5.90107110670354,-34.0898349390389));
#76223=CARTESIAN_POINT('Ctrl Pts',(5.41622003437488,5.7694385334315,-34.0976466825218));
#76224=CARTESIAN_POINT('Ctrl Pts',(5.55490466639366,5.63266856359203,-34.1054584260047));
#76225=CARTESIAN_POINT('Ctrl Pts',(5.69359705521876,5.49589094403571,-34.1132706064082));
#76226=CARTESIAN_POINT('Ctrl Pts',(5.82724690900963,5.35397559648287,-34.1210827868118));
#76227=CARTESIAN_POINT('Ctrl Pts',(5.95546067679407,5.20734184850193,-34.1288949672153));
#76228=CARTESIAN_POINT('Ctrl Pts',(6.05414615411811,5.09447860720291,-34.1349079622734));
#76229=CARTESIAN_POINT('Ctrl Pts',(6.14961183275785,4.97882083627733,-34.1409209573315));
#76230=CARTESIAN_POINT('Ctrl Pts',(6.24169422609106,4.86057344229892,-34.1469339523896));
#76231=CARTESIAN_POINT('Ctrl Pts',(6.3740004302427,4.69067273401156,-34.1555735687475));
#76232=CARTESIAN_POINT('Ctrl Pts',(6.49925809951242,4.51550597958778,-34.1642131851054));
#76233=CARTESIAN_POINT('Ctrl Pts',(6.61709513949074,4.33566291527928,-34.1728528014633));
#76234=CARTESIAN_POINT('Ctrl Pts',(6.73512729736257,4.15552206175378,-34.1815067235416));
#76235=CARTESIAN_POINT('Ctrl Pts',(6.84571413915423,3.97068961318091,-34.1901606456199));
#76236=CARTESIAN_POINT('Ctrl Pts',(6.94852858857239,3.7817815185164,-34.1988145676982));
#76237=CARTESIAN_POINT('Ctrl Pts',(7.05434896865036,3.58735041967443,-34.2077214998334));
#76238=CARTESIAN_POINT('Ctrl Pts',(7.15193551328766,3.38860201701987,-34.2166284319687));
#76239=CARTESIAN_POINT('Ctrl Pts',(7.24098472058632,3.18622994716882,-34.2255353641039));
#76240=CARTESIAN_POINT('Ctrl Pts',(7.3277931626481,2.98895021123961,-34.234218169102));
#76241=CARTESIAN_POINT('Ctrl Pts',(7.40648867438301,2.78822718812726,-34.2429009741001));
#76242=CARTESIAN_POINT('Ctrl Pts',(7.47684031378366,2.58472047273578,-34.2515837790982));
#76243=CARTESIAN_POINT('Ctrl Pts',(7.54991590786283,2.37333415319829,-34.260602774802));
#76244=CARTESIAN_POINT('Ctrl Pts',(7.61398857970821,2.15894456789642,-34.2696217705058));
#76245=CARTESIAN_POINT('Ctrl Pts',(7.66885700350564,1.94230617045371,-34.2786407662096));
#76246=CARTESIAN_POINT('Ctrl Pts',(7.72372542730307,1.72566777301096,-34.2876597619135));
#76247=CARTESIAN_POINT('Ctrl Pts',(7.7693895660935,1.50678083725419,-34.2966787576173));
#76248=CARTESIAN_POINT('Ctrl Pts',(7.80570733587141,1.28641128210356,-34.3056977533211));
#76249=CARTESIAN_POINT('Ctrl Pts',(7.83921870685186,1.08307043929824,-34.3140198202528));
#76250=CARTESIAN_POINT('Ctrl Pts',(7.86480069827297,0.87829489340369,-34.3223418871845));
#76251=CARTESIAN_POINT('Ctrl Pts',(7.88234581788412,0.672714952475907,-34.3306639541162));
#76252=CARTESIAN_POINT('Ctrl Pts',(7.89987537251337,0.467317389789561,-34.3389786382073));
#76253=CARTESIAN_POINT('Ctrl Pts',(7.90938225381209,0.261117145926104,-34.3472933222984));
#76254=CARTESIAN_POINT('Ctrl Pts',(7.91081053168458,0.0547515459911957,
-34.3556080063895));
#76255=CARTESIAN_POINT('Ctrl Pts',(7.91223762948737,-0.151443550854259,
-34.3639158207342));
#76256=CARTESIAN_POINT('Ctrl Pts',(7.90559943770837,-0.357803439669933,
-34.372223635079));
#76257=CARTESIAN_POINT('Ctrl Pts',(7.89089201610962,-0.56368802550476,-34.3805314494238));
#76258=CARTESIAN_POINT('Ctrl Pts',(7.87619938308761,-0.769365590688492,
-34.3888309101119));
#76259=CARTESIAN_POINT('Ctrl Pts',(7.85345373671981,-0.974568515980631,
-34.3971303708));
#76260=CARTESIAN_POINT('Ctrl Pts',(7.82270316128366,-1.17865866579036,-34.4054298314882));
#76261=CARTESIAN_POINT('Ctrl Pts',(7.79197217499952,-1.38261880330231,-34.4137240051404));
#76262=CARTESIAN_POINT('Ctrl Pts',(7.75324647473878,-1.58546729094061,-34.4220181787926));
#76263=CARTESIAN_POINT('Ctrl Pts',(7.70662590542911,-1.78657162010622,-34.4303123524448));
#76264=CARTESIAN_POINT('Ctrl Pts',(7.66003976396481,-1.98752743995822,-34.4386004011068));
#76265=CARTESIAN_POINT('Ctrl Pts',(7.6055704552009,-2.18674138772235,-34.4468884497689));
#76266=CARTESIAN_POINT('Ctrl Pts',(7.54336890415005,-2.38359110920941,-34.455176498431));
#76267=CARTESIAN_POINT('Ctrl Pts',(7.5201408844132,-2.45710099985758,-34.4582715170382));
#76268=CARTESIAN_POINT('Ctrl Pts',(7.49583510457647,-2.5302813062398,-34.4613665356454));
#76269=CARTESIAN_POINT('Ctrl Pts',(7.47046123679272,-2.60310005754241,-34.4644615542527));
#76270=CARTESIAN_POINT('Ctrl Pts',(7.40402955775045,-2.79374785140743,-34.4725646658673));
#76271=CARTESIAN_POINT('Ctrl Pts',(7.33030093350632,-2.98183622350412,-34.4806677774819));
#76272=CARTESIAN_POINT('Ctrl Pts',(7.24950513986053,-3.16679589287591,-34.4887708890966));
#76273=CARTESIAN_POINT('Ctrl Pts',(7.16869151826189,-3.35179637442511,-34.496875788699));
#76274=CARTESIAN_POINT('Ctrl Pts',(7.08080774480915,-3.53366648421667,-34.5049806883014));
#76275=CARTESIAN_POINT('Ctrl Pts',(6.98613099298384,-3.71185866499125,-34.5130855879038));
#76276=CARTESIAN_POINT('Ctrl Pts',(6.891421492952,-3.89011248153413,-34.5211932909497));
#76277=CARTESIAN_POINT('Ctrl Pts',(6.78991447785789,-4.06468555036316,-34.5293009939957));
#76278=CARTESIAN_POINT('Ctrl Pts',(6.681932430106,-4.23505607985275,-34.5374086970416));
#76279=CARTESIAN_POINT('Ctrl Pts',(6.57385324528844,-4.40557986901518,-34.545523693508));
#76280=CARTESIAN_POINT('Ctrl Pts',(6.45928755908311,-4.57189329479687,-34.5536386899745));
#76281=CARTESIAN_POINT('Ctrl Pts',(6.33860120130483,-4.73350354503057,-34.5617536864409));
#76282=CARTESIAN_POINT('Ctrl Pts',(6.21785592373628,-4.89519269433973,-34.5698726446964));
#76283=CARTESIAN_POINT('Ctrl Pts',(6.09098421019588,-5.05217383686884,-34.5779916029519));
#76284=CARTESIAN_POINT('Ctrl Pts',(5.95839192175607,-5.20398757749785,-34.5861105612074));
#76285=CARTESIAN_POINT('Ctrl Pts',(5.82565764019086,-5.35596389551176,-34.594238214058));
#76286=CARTESIAN_POINT('Ctrl Pts',(5.68719075730522,-5.50276151854457,-34.6023658669085));
#76287=CARTESIAN_POINT('Ctrl Pts',(5.54343466601592,-5.64395722021465,-34.6104935197591));
#76288=CARTESIAN_POINT('Ctrl Pts',(5.46837080976693,-5.71768414029212,-34.6147374649008));
#76289=CARTESIAN_POINT('Ctrl Pts',(5.39186541572526,-5.78988432594594,-34.6189814100425));
#76290=CARTESIAN_POINT('Ctrl Pts',(5.31398519266527,-5.86050188739277,-34.6232253551842));
#76291=CARTESIAN_POINT('Ctrl Pts',(5.1672010367998,-5.99359779722687,-34.6312240983912));
#76292=CARTESIAN_POINT('Ctrl Pts',(5.01527727034038,-6.12129953400736,-34.6392228415982));
#76293=CARTESIAN_POINT('Ctrl Pts',(4.85864342064975,-6.24319670609352,-34.6472215848053));
#76294=CARTESIAN_POINT('Ctrl Pts',(4.7021371486678,-6.36499459337029,-34.6552138130646));
#76295=CARTESIAN_POINT('Ctrl Pts',(4.54092870148769,-6.48099713351476,-34.663206041324));
#76296=CARTESIAN_POINT('Ctrl Pts',(4.37548239689503,-6.59083263286679,-34.6711982695834));
#76297=CARTESIAN_POINT('Ctrl Pts',(4.2101428243874,-6.70059727556302,-34.6791853419272));
#76298=CARTESIAN_POINT('Ctrl Pts',(4.04057112114329,-6.80420262255289,-34.6871724142709));
#76299=CARTESIAN_POINT('Ctrl Pts',(3.86726277319624,-6.90131868870367,-34.6951594866147));
#76300=CARTESIAN_POINT('Ctrl Pts',(3.69403688698755,-6.99838854611879,-34.7031427586345));
#76301=CARTESIAN_POINT('Ctrl Pts',(3.51707819126993,-7.0889751142768,-34.7111260306543));
#76302=CARTESIAN_POINT('Ctrl Pts',(3.33690945627348,-7.17279278110226,-34.7191093026741));
#76303=CARTESIAN_POINT('Ctrl Pts',(3.15679595362462,-7.25658475286742,-34.7270901273499));
#76304=CARTESIAN_POINT('Ctrl Pts',(2.97347467648266,-7.33361181932799,-34.7350709520258));
#76305=CARTESIAN_POINT('Ctrl Pts',(2.78749156648602,-7.40363503738328,-34.7430517767017));
#76306=CARTESIAN_POINT('Ctrl Pts',(2.59552581386482,-7.47591073895201,-34.7512893258828));
#76307=CARTESIAN_POINT('Ctrl Pts',(2.40072446071612,-7.54072432977293,-34.7595268750638));
#76308=CARTESIAN_POINT('Ctrl Pts',(2.20370913556884,-7.59786726955732,-34.7677644242449));
#76309=CARTESIAN_POINT('Ctrl Pts',(2.01280776602208,-7.65323689857788,-34.7757463384396));
#76310=CARTESIAN_POINT('Ctrl Pts',(1.81982811947343,-7.70140475138358,-34.7837282526344));
#76311=CARTESIAN_POINT('Ctrl Pts',(1.62535020896077,-7.74223208759794,-34.7917101668291));
#76312=CARTESIAN_POINT('Ctrl Pts',(1.43082906059342,-7.78306850086597,-34.7996938556256));
#76313=CARTESIAN_POINT('Ctrl Pts',(1.23480931164135,-7.81656107490002,-34.8076775444222));
#76314=CARTESIAN_POINT('Ctrl Pts',(1.03788068041415,-7.84262230973946,-34.8156612332187));
#76315=CARTESIAN_POINT('Ctrl Pts',(0.840878029161418,-7.86869334027623,
-34.823647922863));
#76316=CARTESIAN_POINT('Ctrl Pts',(0.642966146148042,-7.88732741907902,
-34.8316346125073));
#76317=CARTESIAN_POINT('Ctrl Pts',(0.444739757187343,-7.89848894082767,
-34.8396213021516));
#76318=CARTESIAN_POINT('Ctrl Pts',(0.246408418496715,-7.90965637197465,
-34.8476122202991));
#76319=CARTESIAN_POINT('Ctrl Pts',(0.0477625754923947,-7.91334333987846,
-34.8556031384466));
#76320=CARTESIAN_POINT('Ctrl Pts',(-0.150602776180313,-7.90956634739268,
-34.8635940565941));
#76321=CARTESIAN_POINT('Ctrl Pts',(-0.349202406596975,-7.90578489410239,
-34.8715944123892));
#76322=CARTESIAN_POINT('Ctrl Pts',(-0.547520549466926,-7.89452187716758,
-34.8795947681842));
#76323=CARTESIAN_POINT('Ctrl Pts',(-0.744965795211754,-7.87584579356176,
-34.8875951239792));
#76324=CARTESIAN_POINT('Ctrl Pts',(-0.942549022385511,-7.85715665847581,
-34.895601070694));
#76325=CARTESIAN_POINT('Ctrl Pts',(-1.13925780523297,-7.83104416842073,
-34.9036070174088));
#76326=CARTESIAN_POINT('Ctrl Pts',(-1.33451015342385,-7.79762807848699,
-34.9116129641235));
#76327=CARTESIAN_POINT('Ctrl Pts',(-1.53001583349051,-7.76416863255358,
-34.9196292982243));
#76328=CARTESIAN_POINT('Ctrl Pts',(-1.72406097825754,-7.72338672726847,
-34.927645632325));
#76329=CARTESIAN_POINT('Ctrl Pts',(-1.91607686706567,-7.67545245829168,
-34.9356619664257));
#76330=CARTESIAN_POINT('Ctrl Pts',(-1.95672516826432,-7.66530513863392,
-34.9373589632995));
#76331=CARTESIAN_POINT('Ctrl Pts',(-1.99728259619836,-7.65483746958424,
-34.9390559601734));
#76332=CARTESIAN_POINT('Ctrl Pts',(-2.03774386542381,-7.64405134329484,
-34.9407529570472));
#76333=CARTESIAN_POINT('Ctrl Pts',(-2.22281949725187,-7.59471405911662,
-34.9485152634367));
#76334=CARTESIAN_POINT('Ctrl Pts',(-2.40642961687235,-7.53856386645909,
-34.9562775698263));
#76335=CARTESIAN_POINT('Ctrl Pts',(-2.58802145964085,-7.47569835697231,
-34.9640398762158));
#76336=CARTESIAN_POINT('Ctrl Pts',(-2.76939332553528,-7.41290900155749,
-34.9717927794963));
#76337=CARTESIAN_POINT('Ctrl Pts',(-2.94875144641187,-7.34342063688923,
-34.9795456827767));
#76338=CARTESIAN_POINT('Ctrl Pts',(-3.1255531471949,-7.26738182043988,-34.9872985860572));
#76339=CARTESIAN_POINT('Ctrl Pts',(-3.3021765357247,-7.19141969246487,-34.9950436701955));
#76340=CARTESIAN_POINT('Ctrl Pts',(-3.47624831006344,-7.1089204044593,-35.0027887543336));
#76341=CARTESIAN_POINT('Ctrl Pts',(-3.64724077777109,-7.02008231497065,
-35.0105338384719));
#76342=CARTESIAN_POINT('Ctrl Pts',(-3.81809542507101,-6.93131582923087,
-35.0182726800506));
#76343=CARTESIAN_POINT('Ctrl Pts',(-3.98587539060148,-6.83622087845153,
-35.0260115216293));
#76344=CARTESIAN_POINT('Ctrl Pts',(-4.15007272156713,-6.73504397949296,
-35.033750363208));
#76345=CARTESIAN_POINT('Ctrl Pts',(-4.31417093125197,-6.6339281581643,-35.0414845330671));
#76346=CARTESIAN_POINT('Ctrl Pts',(-4.47469050846732,-6.52673788722465,
-35.0492187029262));
#76347=CARTESIAN_POINT('Ctrl Pts',(-4.63114781367576,-6.4137657369042,-35.0569528727853));
#76348=CARTESIAN_POINT('Ctrl Pts',(-4.78754230384056,-6.30083894305044,
-35.064683937502));
#76349=CARTESIAN_POINT('Ctrl Pts',(-4.9398774798041,-6.1821351029284,-35.0724150022187));
#76350=CARTESIAN_POINT('Ctrl Pts',(-5.087698360072,-6.05799029356441,-35.0801460669354));
#76351=CARTESIAN_POINT('Ctrl Pts',(-5.23551709374356,-5.93384728698225,
-35.0878770193846));
#76352=CARTESIAN_POINT('Ctrl Pts',(-5.37882138040632,-5.80426369085599,
-35.0956079718338));
#76353=CARTESIAN_POINT('Ctrl Pts',(-5.51718873845376,-5.66961633836708,
-35.103338924283));
#76354=CARTESIAN_POINT('Ctrl Pts',(-5.65556190053407,-5.5349633378867,-35.111070201019));
#76355=CARTESIAN_POINT('Ctrl Pts',(-5.78899746349417,-5.39524640787177,
-35.118801477755));
#76356=CARTESIAN_POINT('Ctrl Pts',(-5.91710942029829,-5.25087965089824,
-35.1265327544909));
#76357=CARTESIAN_POINT('Ctrl Pts',(-6.04525020969944,-5.10648040305787,
-35.1342657712112));
#76358=CARTESIAN_POINT('Ctrl Pts',(-6.16806476860649,-4.95742951284821,
-35.1419987879314));
#76359=CARTESIAN_POINT('Ctrl Pts',(-6.28520700946487,-4.80417462715227,
-35.1497318046516));
#76360=CARTESIAN_POINT('Ctrl Pts',(-6.40239707075277,-4.65085717893059,
-35.1574679781851));
#76361=CARTESIAN_POINT('Ctrl Pts',(-6.5139099852212,-4.49333260282782,-35.1652041517186));
#76362=CARTESIAN_POINT('Ctrl Pts',(-6.61944263944751,-4.33207803981694,
-35.1729403252521));
#76363=CARTESIAN_POINT('Ctrl Pts',(-6.72509929089872,-4.17063400826229,
-35.1806855885224));
#76364=CARTESIAN_POINT('Ctrl Pts',(-6.8247614526579,-4.00545153773251,-35.1884308517927));
#76365=CARTESIAN_POINT('Ctrl Pts',(-6.91817118187755,-3.83703381510237,
-35.196176115063));
#76366=CARTESIAN_POINT('Ctrl Pts',(-7.01164085633237,-3.66850801122551,
-35.2039263488179));
#76367=CARTESIAN_POINT('Ctrl Pts',(-7.09884994372007,-3.49674313833837,
-35.2116765825729));
#76368=CARTESIAN_POINT('Ctrl Pts',(-7.17958848754662,-3.32226280560224,
-35.2194268163279));
#76369=CARTESIAN_POINT('Ctrl Pts',(-7.26044862395376,-3.14751970476409,
-35.2271887219669));
#76370=CARTESIAN_POINT('Ctrl Pts',(-7.33481861693578,-2.9700533062728,-35.2349506276059));
#76371=CARTESIAN_POINT('Ctrl Pts',(-7.40253786009505,-2.79040395460218,
-35.2427125332449));
#76372=CARTESIAN_POINT('Ctrl Pts',(-7.44781260595259,-2.67029660607155,
-35.2479018751334));
#76373=CARTESIAN_POINT('Ctrl Pts',(-7.49011564425207,-2.54921381182251,
-35.2530912170218));
#76374=CARTESIAN_POINT('Ctrl Pts',(-7.52941175312994,-2.42731943753368,
-35.2582805589102));
#76375=CARTESIAN_POINT('Ctrl Pts',(-7.60583955379658,-2.19024459204487,
-35.2683734153981));
#76376=CARTESIAN_POINT('Ctrl Pts',(-7.67108903170758,-1.94948830154461,
-35.278466271886));
#76377=CARTESIAN_POINT('Ctrl Pts',(-7.72486690969569,-1.70597544750463,
-35.2885591283739));
#76378=CARTESIAN_POINT('Ctrl Pts',(-7.77818830022531,-1.46452962489109,
-35.2985663127866));
#76379=CARTESIAN_POINT('Ctrl Pts',(-7.82023202030717,-1.22037366359654,
-35.3085734971994));
#76380=CARTESIAN_POINT('Ctrl Pts',(-7.85075827923368,-0.974430829276153,
-35.3185806816121));
#76381=CARTESIAN_POINT('Ctrl Pts',(-7.8807546520397,-0.732757161860744,
-35.3284141576075));
#76382=CARTESIAN_POINT('Ctrl Pts',(-7.89962993631264,-0.489357991626549,
-35.3382476336029));
#76383=CARTESIAN_POINT('Ctrl Pts',(-7.90720121262665,-0.245132582566322,
-35.3480811095982));
#76384=CARTESIAN_POINT('Ctrl Pts',(-7.90966180182129,-0.165761763477523,
-35.3512768910988));
#76385=CARTESIAN_POINT('Ctrl Pts',(-7.91092883589041,-0.0863038717799649,
-35.3544726725994));
#76386=CARTESIAN_POINT('Ctrl Pts',(-7.91099708577542,-0.00679034998251756,
-35.3576684541));
#76387=CARTESIAN_POINT('',(-7.90050494756768,0.00579114955300497,-37.357668491763));
#76388=CARTESIAN_POINT('Ctrl Pts',(-7.90525032249359,-0.00678448088220818,
-35.357668491763));
#76389=CARTESIAN_POINT('Ctrl Pts',(-7.88783545099137,1.80107895371635,-35.4303817147664));
#76390=CARTESIAN_POINT('Ctrl Pts',(-6.8135975783561,4.939319079492,-35.556016204747));
#76391=CARTESIAN_POINT('Ctrl Pts',(-3.10734150823737,7.61713964008616,-35.7345719617048));
#76392=CARTESIAN_POINT('Ctrl Pts',(2.28026636839026,8.42190983339215,-35.9462570296134));
#76393=CARTESIAN_POINT('Ctrl Pts',(7.12946490356375,5.02602867964289,-36.1579420975222));
#76394=CARTESIAN_POINT('Ctrl Pts',(8.22864524405818,-0.318974158456952,
-36.3696271654307));
#76395=CARTESIAN_POINT('Ctrl Pts',(7.09460005342516,-4.21538026514994,-36.5283909663624));
#76396=CARTESIAN_POINT('Ctrl Pts',(4.20751149604049,-7.07879035645357,-36.6871547672938));
#76397=CARTESIAN_POINT('Ctrl Pts',(-0.999622714554145,-8.66070382201061,
-36.8988398352026));
#76398=CARTESIAN_POINT('Ctrl Pts',(-6.62226577165369,-5.88434235214676,
-37.1223444100256));
#76399=CARTESIAN_POINT('Ctrl Pts',(-7.89111861597513,-1.61068309120649,
-37.2929277178714));
#76400=CARTESIAN_POINT('Ctrl Pts',(-7.90050494756768,0.00579114955300497,
-37.357668491763));
#76401=CARTESIAN_POINT('',(-7.92255110667597,0.00112620878001013,-39.357668491763));
#76402=CARTESIAN_POINT('Ctrl Pts',(-7.90050494756768,0.00579114955300497,
-37.357668491763));
#76403=CARTESIAN_POINT('Ctrl Pts',(-7.90646401672607,1.03203678113555,-37.3987702518258));
#76404=CARTESIAN_POINT('Ctrl Pts',(-7.24737305659377,4.69309146320393,-37.5457145458429));
#76405=CARTESIAN_POINT('Ctrl Pts',(-2.87855582146927,8.22911730782232,-37.7455801068374));
#76406=CARTESIAN_POINT('Ctrl Pts',(2.52742786906601,7.82869694853837,-37.9572651747459));
#76407=CARTESIAN_POINT('Ctrl Pts',(7.16765417016174,4.97523000971477,-38.1689502426547));
#76408=CARTESIAN_POINT('Ctrl Pts',(8.69106246208229,-0.745431002793219,
-38.3806353105634));
#76409=CARTESIAN_POINT('Ctrl Pts',(6.09028077099974,-5.54263720594378,-38.5923203784721));
#76410=CARTESIAN_POINT('Ctrl Pts',(2.71365595713207,-7.79351345955097,-38.7510841794036));
#76411=CARTESIAN_POINT('Ctrl Pts',(-1.33904198433904,-8.12523184063725,
-38.9098479803352));
#76412=CARTESIAN_POINT('Ctrl Pts',(-6.1173318547664,-6.07862255922375,-39.1120427511214));
#76413=CARTESIAN_POINT('Ctrl Pts',(-7.90693077504529,-2.3808942637658,-39.2613162549308));
#76414=CARTESIAN_POINT('Ctrl Pts',(-7.92255110667597,0.00112620878001013,
-39.357668491763));
#76415=CARTESIAN_POINT('',(-7.90690567208597,-0.00336307952236492,-41.357668491763));
#76416=CARTESIAN_POINT('Ctrl Pts',(-7.92255110667597,0.00112620878001013,
-39.357668491763));
#76417=CARTESIAN_POINT('Ctrl Pts',(-7.92408964478569,0.23574538088166,-39.3671587888852));
#76418=CARTESIAN_POINT('Ctrl Pts',(-7.8084390703918,3.08644196615606,-39.4824916199614));
#76419=CARTESIAN_POINT('Ctrl Pts',(-4.34320070494277,8.2922938225927,-39.7036669849931));
#76420=CARTESIAN_POINT('Ctrl Pts',(3.0965349810775,8.14959670132102,-39.9682733198783));
#76421=CARTESIAN_POINT('Ctrl Pts',(6.97477370654661,4.36221495204592,-40.1799583877874));
#76422=CARTESIAN_POINT('Ctrl Pts',(8.68757048396973,-0.808887531523498,
-40.3916434556958));
#76423=CARTESIAN_POINT('Ctrl Pts',(6.16946845661581,-6.16667601407484,-40.6033285236047));
#76424=CARTESIAN_POINT('Ctrl Pts',(1.09061100012035,-8.16228612048976,-40.8150135915134));
#76425=CARTESIAN_POINT('Ctrl Pts',(-2.94220442932188,-7.71013708010145,
-40.9737773924447));
#76426=CARTESIAN_POINT('Ctrl Pts',(-6.25649344662526,-5.35431747772463,
-41.1325411933765));
#76427=CARTESIAN_POINT('Ctrl Pts',(-7.73613906322107,-2.41608628745108,
-41.2605048931491));
#76428=CARTESIAN_POINT('Ctrl Pts',(-7.91192326830252,-0.553012152266311,
-41.3355473259446));
#76429=CARTESIAN_POINT('Ctrl Pts',(-7.90690567208597,-0.00336307952236492,
-41.357668491763));
#76430=CARTESIAN_POINT('',(-7.9079676034592,-0.00146772438904264,-43.357668491763));
#76431=CARTESIAN_POINT('Ctrl Pts',(-7.90690567208597,-0.00336307952236492,
-41.357668491763));
#76432=CARTESIAN_POINT('Ctrl Pts',(-7.88791571362478,2.07687865559345,-41.4413898598989));
#76433=CARTESIAN_POINT('Ctrl Pts',(-6.00161559860685,6.8015463040485,-41.6309537619893));
#76434=CARTESIAN_POINT('Ctrl Pts',(2.0166268162176,9.14104728615705,-41.926360198034));
#76435=CARTESIAN_POINT('Ctrl Pts',(7.61682718247753,4.24127327055065,-42.1909665329198));
#76436=CARTESIAN_POINT('Ctrl Pts',(8.14526619226151,-1.15370108892476,-42.4026516008286));
#76437=CARTESIAN_POINT('Ctrl Pts',(6.1259358175118,-6.2129775721734,-42.614336668737));
#76438=CARTESIAN_POINT('Ctrl Pts',(0.74936559032438,-8.69072409594159,-42.8260217366459));
#76439=CARTESIAN_POINT('Ctrl Pts',(-4.42144418447609,-6.94717053122234,
-43.0377068045546));
#76440=CARTESIAN_POINT('Ctrl Pts',(-7.21577302375009,-4.00442260102508,
-43.1964706054861));
#76441=CARTESIAN_POINT('Ctrl Pts',(-7.90016440029126,-1.35993271260852,
-43.3031245012222));
#76442=CARTESIAN_POINT('Ctrl Pts',(-7.90792716545684,-0.0216761063237722,
-43.3568571299812));
#76443=CARTESIAN_POINT('Ctrl Pts',(-7.9079676034592,-0.00146772438904264,
-43.357668491763));
#76444=CARTESIAN_POINT('',(-7.911,-1.23234755733392E-13,-45.357668491763));
#76445=CARTESIAN_POINT('Ctrl Pts',(-7.911,-1.21014309684142E-13,-43.357668491763));
#76446=CARTESIAN_POINT('Ctrl Pts',(-7.91100000000004,2.20167589666662,-43.4462559274957));
#76447=CARTESIAN_POINT('Ctrl Pts',(-6.94214576672381,4.38610418338667,-43.5348433632284));
#76448=CARTESIAN_POINT('Ctrl Pts',(-3.67820201488307,7.34180684107621,-43.7120182346939));
#76449=CARTESIAN_POINT('Ctrl Pts',(-1.4086817587177,8.08992666571331,-43.8006056704266));
#76450=CARTESIAN_POINT('Ctrl Pts',(2.97309270521244,7.65454228025268,-43.977780541892));
#76451=CARTESIAN_POINT('Ctrl Pts',(5.05102072675574,6.47444880834247,-44.0663679776248));
#76452=CARTESIAN_POINT('Ctrl Pts',(7.66951518847856,2.93425195367744,-44.2435428490902));
#76453=CARTESIAN_POINT('Ctrl Pts',(8.18956872247067,0.601881960099604,-44.3321302848229));
#76454=CARTESIAN_POINT('Ctrl Pts',(7.32306689761364,-3.71537198232405,-44.5093051562884));
#76455=CARTESIAN_POINT('Ctrl Pts',(5.94329958850238,-5.66643518936472,-44.5978925920211));
#76456=CARTESIAN_POINT('Ctrl Pts',(2.16154501637904,-7.92205913232982,-44.7750674634866));
#76457=CARTESIAN_POINT('Ctrl Pts',(-0.210816529299753,-8.20894963713003,
-44.8636548992193));
#76458=CARTESIAN_POINT('Ctrl Pts',(-4.4212390857638,-6.91982244717867,-45.0408297706847));
#76459=CARTESIAN_POINT('Ctrl Pts',(-6.22631625634142,-5.35390358803574,
-45.1294172064175));
#76460=CARTESIAN_POINT('Ctrl Pts',(-7.65317280859476,-2.31334857514569,
-45.2645592586878));
#76461=CARTESIAN_POINT('Ctrl Pts',(-7.91099999999998,-1.15702837836551,
-45.3111138752254));
#76462=CARTESIAN_POINT('Ctrl Pts',(-7.911,-1.23234755733392E-13,-45.357668491763));
#76463=CARTESIAN_POINT('',(-7.911,-1.27675647831893E-14,-47.357668491763));
#76464=CARTESIAN_POINT('Ctrl Pts',(-7.911,-1.23234755733392E-13,-45.357668491763));
#76465=CARTESIAN_POINT('Ctrl Pts',(-7.91100000000004,2.20167589666662,-45.4462559274957));
#76466=CARTESIAN_POINT('Ctrl Pts',(-6.94214576672381,4.38610418338667,-45.5348433632284));
#76467=CARTESIAN_POINT('Ctrl Pts',(-3.67820201488307,7.34180684107621,-45.7120182346939));
#76468=CARTESIAN_POINT('Ctrl Pts',(-1.4086817587177,8.08992666571331,-45.8006056704266));
#76469=CARTESIAN_POINT('Ctrl Pts',(2.97309270521244,7.65454228025268,-45.977780541892));
#76470=CARTESIAN_POINT('Ctrl Pts',(5.05102072675574,6.47444880834247,-46.0663679776248));
#76471=CARTESIAN_POINT('Ctrl Pts',(7.66951518847856,2.93425195367745,-46.2435428490902));
#76472=CARTESIAN_POINT('Ctrl Pts',(8.18956872247067,0.601881960099607,-46.3321302848229));
#76473=CARTESIAN_POINT('Ctrl Pts',(7.32306689761365,-3.71537198232405,-46.5093051562884));
#76474=CARTESIAN_POINT('Ctrl Pts',(5.94329958850238,-5.66643518936472,-46.5978925920211));
#76475=CARTESIAN_POINT('Ctrl Pts',(2.16154501637904,-7.92205913232982,-46.7750674634866));
#76476=CARTESIAN_POINT('Ctrl Pts',(-0.210816529299751,-8.20894963713003,
-46.8636548992193));
#76477=CARTESIAN_POINT('Ctrl Pts',(-4.4212390857638,-6.91982244717867,-47.0408297706847));
#76478=CARTESIAN_POINT('Ctrl Pts',(-6.22631625634141,-5.35390358803574,
-47.1294172064175));
#76479=CARTESIAN_POINT('Ctrl Pts',(-7.65317280859478,-2.31334857514566,
-47.2645592586878));
#76480=CARTESIAN_POINT('Ctrl Pts',(-7.911,-1.15702837836543,-47.3111138752254));
#76481=CARTESIAN_POINT('Ctrl Pts',(-7.911,-1.27675647831893E-14,-47.357668491763));
#76482=CARTESIAN_POINT('',(-7.911,-1.49880108324396E-14,-49.357668491763));
#76483=CARTESIAN_POINT('Ctrl Pts',(-7.911,-1.27675647831893E-14,-47.357668491763));
#76484=CARTESIAN_POINT('Ctrl Pts',(-7.911,2.20167589666671,-47.4462559274957));
#76485=CARTESIAN_POINT('Ctrl Pts',(-6.94214576672376,4.38610418338673,-47.5348433632284));
#76486=CARTESIAN_POINT('Ctrl Pts',(-3.67820201488303,7.34180684107622,-47.7120182346939));
#76487=CARTESIAN_POINT('Ctrl Pts',(-1.40868175871768,8.08992666571331,-47.8006056704266));
#76488=CARTESIAN_POINT('Ctrl Pts',(2.97309270521242,7.65454228025268,-47.977780541892));
#76489=CARTESIAN_POINT('Ctrl Pts',(5.05102072675571,6.47444880834249,-48.0663679776248));
#76490=CARTESIAN_POINT('Ctrl Pts',(7.66951518847853,2.93425195367752,-48.2435428490902));
#76491=CARTESIAN_POINT('Ctrl Pts',(8.18956872247066,0.601881960099707,-48.3321302848229));
#76492=CARTESIAN_POINT('Ctrl Pts',(7.3230668976137,-3.71537198232393,-48.5093051562884));
#76493=CARTESIAN_POINT('Ctrl Pts',(5.94329958850248,-5.6664351893646,-48.5978925920211));
#76494=CARTESIAN_POINT('Ctrl Pts',(2.16154501637922,-7.92205913232976,-48.7750674634866));
#76495=CARTESIAN_POINT('Ctrl Pts',(-0.210816529299534,-8.20894963713003,
-48.8636548992193));
#76496=CARTESIAN_POINT('Ctrl Pts',(-4.42123908576359,-6.9198224471788,-49.0408297706847));
#76497=CARTESIAN_POINT('Ctrl Pts',(-6.22631625634123,-5.35390358803594,
-49.1294172064175));
#76498=CARTESIAN_POINT('Ctrl Pts',(-7.65317280859473,-2.31334857514585,
-49.2645592586878));
#76499=CARTESIAN_POINT('Ctrl Pts',(-7.911,-1.15702837836553,-49.3111138752254));
#76500=CARTESIAN_POINT('Ctrl Pts',(-7.911,-1.49880108324396E-14,-49.357668491763));
#76501=CARTESIAN_POINT('',(-7.90980225400435,0.0042058662603975,-51.357668491763));
#76502=CARTESIAN_POINT('Ctrl Pts',(-7.911,-1.49880108324396E-14,-49.357668491763));
#76503=CARTESIAN_POINT('Ctrl Pts',(-7.91100000000001,2.20167589666673,-49.4462559274957));
#76504=CARTESIAN_POINT('Ctrl Pts',(-6.94214576672374,4.38610418338676,-49.5348433632284));
#76505=CARTESIAN_POINT('Ctrl Pts',(-3.67820201488297,7.34180684107626,-49.7120182346939));
#76506=CARTESIAN_POINT('Ctrl Pts',(-1.40868175871759,8.08992666571333,-49.8006056704266));
#76507=CARTESIAN_POINT('Ctrl Pts',(2.97309270521254,7.65454228025264,-49.977780541892));
#76508=CARTESIAN_POINT('Ctrl Pts',(5.05102072675583,6.4744488083424,-50.0663679776248));
#76509=CARTESIAN_POINT('Ctrl Pts',(7.66951518847861,2.93425195367734,-50.2435428490902));
#76510=CARTESIAN_POINT('Ctrl Pts',(8.18956872247068,0.601881960099496,-50.3321302848229));
#76511=CARTESIAN_POINT('Ctrl Pts',(7.3230668976136,-3.71537198232415,-50.5093051562884));
#76512=CARTESIAN_POINT('Ctrl Pts',(5.9432995885023,-5.6664351893648,-50.5978925920211));
#76513=CARTESIAN_POINT('Ctrl Pts',(2.16154501637893,-7.92205913232985,-50.7750674634866));
#76514=CARTESIAN_POINT('Ctrl Pts',(-0.210816529299864,-8.20894963713003,
-50.8636548992193));
#76515=CARTESIAN_POINT('Ctrl Pts',(-4.4212390857639,-6.91982244717861,-51.0408297706847));
#76516=CARTESIAN_POINT('Ctrl Pts',(-6.22631625634149,-5.35390358803565,
-51.1294172064175));
#76517=CARTESIAN_POINT('Ctrl Pts',(-7.6531728085948,-2.31334857514557,-51.2645592586878));
#76518=CARTESIAN_POINT('Ctrl Pts',(-7.91100000000001,-1.15702837836536,
-51.3111138752254));
#76519=CARTESIAN_POINT('Ctrl Pts',(-7.911,3.99680288865056E-14,-51.357668491763));
#76520=CARTESIAN_POINT('',(-7.91971459369528,0.0014675095212946,-53.357668491763));
#76521=CARTESIAN_POINT('Ctrl Pts',(-7.9095354027183,0.0051429103620837,
-51.357668491763));
#76522=CARTESIAN_POINT('Ctrl Pts',(-7.91338204178412,0.79052735029231,-51.3891750791503));
#76523=CARTESIAN_POINT('Ctrl Pts',(-7.43130218892738,4.20872011440281,-51.5265242004919));
#76524=CARTESIAN_POINT('Ctrl Pts',(-3.62969356886065,7.93193284741365,-51.7167945888108));
#76525=CARTESIAN_POINT('Ctrl Pts',(1.82628321975503,8.02975944020611,-51.9284796567195));
#76526=CARTESIAN_POINT('Ctrl Pts',(5.44779876741806,6.19873126434857,-52.0872434576511));
#76527=CARTESIAN_POINT('Ctrl Pts',(7.73164663510024,2.83444283938916,-52.2460072585824));
#76528=CARTESIAN_POINT('Ctrl Pts',(8.32932445584858,-2.57476025556633,-52.4576923264914));
#76529=CARTESIAN_POINT('Ctrl Pts',(3.87467264772705,-8.51367100141516,-52.7222986613769));
#76530=CARTESIAN_POINT('Ctrl Pts',(-2.0949362231413,-8.07967815626293,-52.9339837292857));
#76531=CARTESIAN_POINT('Ctrl Pts',(-6.49724597062893,-5.24286928254714,
-53.1457736727477));
#76532=CARTESIAN_POINT('Ctrl Pts',(-7.91319423021304,-2.62067617436248,
-53.2517210822554));
#76533=CARTESIAN_POINT('Ctrl Pts',(-7.91971459369528,0.0014675095212946,
-53.357668491763));
#76534=CARTESIAN_POINT('',(-7.90637295173893,-0.00687858255987051,-55.357668491763));
#76535=CARTESIAN_POINT('Ctrl Pts',(-7.91971459369528,0.0014675095212946,
-53.357668491763));
#76536=CARTESIAN_POINT('Ctrl Pts',(-7.92296509383969,1.30864592776983,-53.4104848831869));
#76537=CARTESIAN_POINT('Ctrl Pts',(-7.22881565719418,3.92557064294125,-53.516222541588));
#76538=CARTESIAN_POINT('Ctrl Pts',(-3.5727400178991,7.96013245645519,-53.7278027339433));
#76539=CARTESIAN_POINT('Ctrl Pts',(2.33048199300974,8.40589601261067,-53.9394878018521));
#76540=CARTESIAN_POINT('Ctrl Pts',(6.5678014334901,4.96752769388497,-54.1511728697608));
#76541=CARTESIAN_POINT('Ctrl Pts',(8.15955942910485,1.23465406198757,-54.3099366706923));
#76542=CARTESIAN_POINT('Ctrl Pts',(7.74058036951053,-2.80995397960037,-54.4687004716237));
#76543=CARTESIAN_POINT('Ctrl Pts',(4.71476302133078,-7.33335162650678,-54.6803855395325));
#76544=CARTESIAN_POINT('Ctrl Pts',(-2.51764341483412,-9.0087265231183,-54.9449918744182));
#76545=CARTESIAN_POINT('Ctrl Pts',(-7.44792865863706,-4.20704786616543,
-55.1883932808209));
#76546=CARTESIAN_POINT('Ctrl Pts',(-7.91420801088355,-0.795191286074574,
-55.3259521532691));
#76547=CARTESIAN_POINT('Ctrl Pts',(-7.90637295173893,-0.00687858255987051,
-55.357668491763));
#76548=CARTESIAN_POINT('',(-7.90348210374974,0.00514758300883319,-57.3576685050633));
#76549=CARTESIAN_POINT('Ctrl Pts',(-7.90637295173893,-0.00687858255987051,
-55.357668491763));
#76550=CARTESIAN_POINT('Ctrl Pts',(-7.88806115557395,1.83553527476434,-55.4317946872235));
#76551=CARTESIAN_POINT('Ctrl Pts',(-6.77682717523258,5.00881673632035,-55.5588421496612));
#76552=CARTESIAN_POINT('Ctrl Pts',(-3.00563183108224,7.65784328303544,-55.7388108790758));
#76553=CARTESIAN_POINT('Ctrl Pts',(2.39221485231049,8.39079788323256,-55.9504959469846));
#76554=CARTESIAN_POINT('Ctrl Pts',(7.19576250330689,4.93064285982486,-56.1621810148933));
#76555=CARTESIAN_POINT('Ctrl Pts',(8.22366753122325,-0.42852282073491,-56.373866082802));
#76556=CARTESIAN_POINT('Ctrl Pts',(7.03783755391621,-4.30948274059994,-56.5326298837334));
#76557=CARTESIAN_POINT('Ctrl Pts',(4.11287160034719,-7.13419116803278,-56.6913936846651));
#76558=CARTESIAN_POINT('Ctrl Pts',(-1.11486118009225,-8.64662670095146,
-56.9030787525737));
#76559=CARTESIAN_POINT('Ctrl Pts',(-6.66473466282189,-5.813654756809,-57.1251703549397));
#76560=CARTESIAN_POINT('Ctrl Pts',(-7.89158108502462,-1.57638635919126,
-57.2943406903285));
#76561=CARTESIAN_POINT('Ctrl Pts',(-7.89984496754574,0.00514488164946481,
-57.357668491763));
#76562=CARTESIAN_POINT('Ctrl Pts',(-7.91099832163338,0.00515316542435353,
-57.3576685325485));
#76563=CARTESIAN_POINT('Ctrl Pts',(-7.91085916274685,0.218786073952081,
-57.3662108111025));
#76564=CARTESIAN_POINT('Ctrl Pts',(-7.9020624298758,0.432087522141027,-57.3747530896565));
#76565=CARTESIAN_POINT('Ctrl Pts',(-7.88471273520091,0.644380387163226,
-57.3832953682106));
#76566=CARTESIAN_POINT('Ctrl Pts',(-7.86727553774343,0.857743946324986,
-57.3918807295483));
#76567=CARTESIAN_POINT('Ctrl Pts',(-7.84119897104923,1.0700884923815,-57.400466090886));
#76568=CARTESIAN_POINT('Ctrl Pts',(-7.80663937810051,1.28074299540948,-57.4090514522238));
#76569=CARTESIAN_POINT('Ctrl Pts',(-7.77199163430166,1.49193481302781,-57.4176587121672));
#76570=CARTESIAN_POINT('Ctrl Pts',(-7.72881765076389,1.70142773919554,-57.4262659721107));
#76571=CARTESIAN_POINT('Ctrl Pts',(-7.67732369902306,1.90856538279907,-57.4348732320542));
#76572=CARTESIAN_POINT('Ctrl Pts',(-7.62561836094242,2.11655334118395,-57.4435158254128));
#76573=CARTESIAN_POINT('Ctrl Pts',(-7.56552472331091,2.32216642644666,-57.4521584187715));
#76574=CARTESIAN_POINT('Ctrl Pts',(-7.49729893266142,2.52476329867057,-57.4608010121301));
#76575=CARTESIAN_POINT('Ctrl Pts',(-7.4330625818184,2.71551350676614,-57.4689382378609));
#76576=CARTESIAN_POINT('Ctrl Pts',(-7.36161781954197,2.90358999692527,-57.4770754635918));
#76577=CARTESIAN_POINT('Ctrl Pts',(-7.28321501793959,3.08847859025429,-57.4852126893226));
#76578=CARTESIAN_POINT('Ctrl Pts',(-7.20694901075638,3.2683282193331,-57.49312814264));
#76579=CARTESIAN_POINT('Ctrl Pts',(-7.12391001297988,3.44560427246274,-57.5010435959574));
#76580=CARTESIAN_POINT('Ctrl Pts',(-7.03429161510033,3.61976000222794,-57.5089590492749));
#76581=CARTESIAN_POINT('Ctrl Pts',(-6.94477585168995,3.79371628208886,-57.5168654375078));
#76582=CARTESIAN_POINT('Ctrl Pts',(-6.84869585259342,3.96455905283594,-57.5247718257407));
#76583=CARTESIAN_POINT('Ctrl Pts',(-6.74629377754161,4.13176006891777,-57.5326782139736));
#76584=CARTESIAN_POINT('Ctrl Pts',(-6.64398997877225,4.29880062053368,-57.5405770143677));
#76585=CARTESIAN_POINT('Ctrl Pts',(-6.53537636928849,4.46220608781448,-57.5484758147618));
#76586=CARTESIAN_POINT('Ctrl Pts',(-6.42074178691205,4.62147118413622,-57.5563746151559));
#76587=CARTESIAN_POINT('Ctrl Pts',(-6.30619595984499,4.78061297017407,-57.5642672999393));
#76588=CARTESIAN_POINT('Ctrl Pts',(-6.18563864786141,4.9356204933995,-57.5721599847227));
#76589=CARTESIAN_POINT('Ctrl Pts',(-6.05940306125347,5.0860156843321,-57.5800526695061));
#76590=CARTESIAN_POINT('Ctrl Pts',(-5.93324180565368,5.23632231841267,-57.5879407068583));
#76591=CARTESIAN_POINT('Ctrl Pts',(-5.80140915870419,5.38202176850061,-57.5958287442104));
#76592=CARTESIAN_POINT('Ctrl Pts',(-5.66428000406136,5.52266720304516,-57.6037167815625));
#76593=CARTESIAN_POINT('Ctrl Pts',(-5.5201169483989,5.67052690262347,-57.6120094277968));
#76594=CARTESIAN_POINT('Ctrl Pts',(-5.37009998048853,5.81280016037822,-57.6203020740311));
#76595=CARTESIAN_POINT('Ctrl Pts',(-5.21471123017033,5.94900897510967,-57.6285947202654));
#76596=CARTESIAN_POINT('Ctrl Pts',(-5.06697584815294,6.07850909167075,-57.6364789284648));
#76597=CARTESIAN_POINT('Ctrl Pts',(-4.91438539018964,6.20252752270697,-57.6443631366643));
#76598=CARTESIAN_POINT('Ctrl Pts',(-4.75739045796715,6.32069276507276,-57.6522473448637));
#76599=CARTESIAN_POINT('Ctrl Pts',(-4.60039352230813,6.43885951536341,-57.6601316536747));
#76600=CARTESIAN_POINT('Ctrl Pts',(-4.43899227564785,6.55117272033783,-57.6680159624858));
#76601=CARTESIAN_POINT('Ctrl Pts',(-4.27366866590118,6.65730254187794,-57.6759002712968));
#76602=CARTESIAN_POINT('Ctrl Pts',(-4.10831517529886,6.76345154549302,-57.6837860051305));
#76603=CARTESIAN_POINT('Ctrl Pts',(-3.9390381992495,6.86341475255014,-57.6916717389642));
#76604=CARTESIAN_POINT('Ctrl Pts',(-3.76634699959945,6.9569067320619,-57.6995574727979));
#76605=CARTESIAN_POINT('Ctrl Pts',(-3.59359557855781,7.05043131437636,-57.7074459565683));
#76606=CARTESIAN_POINT('Ctrl Pts',(-3.41742786468763,7.13748000874252,-57.7153344403387));
#76607=CARTESIAN_POINT('Ctrl Pts',(-3.23837615719559,7.21781413341374,-57.7232229241091));
#76608=CARTESIAN_POINT('Ctrl Pts',(-3.05914933812736,7.29822682441304,-57.7311191227729));
#76609=CARTESIAN_POINT('Ctrl Pts',(-2.87703320663395,7.37191168846707,-57.7390153214367));
#76610=CARTESIAN_POINT('Ctrl Pts',(-2.69257938423742,7.43867846190301,-57.7469115201004));
#76611=CARTESIAN_POINT('Ctrl Pts',(-2.50802082035909,7.50548314862637,-57.754812202594));
#76612=CARTESIAN_POINT('Ctrl Pts',(-2.32112224657997,7.56536180751737,-57.7627128850875));
#76613=CARTESIAN_POINT('Ctrl Pts',(-2.13244902244087,7.61817446418044,-57.7706135675811));
#76614=CARTESIAN_POINT('Ctrl Pts',(-1.94354909294622,7.67105057930277,-57.7785237433509));
#76615=CARTESIAN_POINT('Ctrl Pts',(-1.75287058839649,7.71684365430557,-57.7864339191206));
#76616=CARTESIAN_POINT('Ctrl Pts',(-1.56098863082943,7.75546487932356,-57.7943440948904));
#76617=CARTESIAN_POINT('Ctrl Pts',(-1.49309807954772,7.76912961513766,-57.7971428269888));
#76618=CARTESIAN_POINT('Ctrl Pts',(-1.42505692050413,7.78189702095104,-57.7999415590872));
#76619=CARTESIAN_POINT('Ctrl Pts',(-1.35689073356133,7.79376472169743,-57.8027402911856));
#76620=CARTESIAN_POINT('Ctrl Pts',(-1.14764710348681,7.83019393823696,-57.8113313080833));
#76621=CARTESIAN_POINT('Ctrl Pts',(-0.93680763769509,7.85821466188491,-57.819922324981));
#76622=CARTESIAN_POINT('Ctrl Pts',(-0.72504044045087,7.87770508204711,-57.8285133418786));
#76623=CARTESIAN_POINT('Ctrl Pts',(-0.513577331250256,7.89716751485426,
-57.8370920224676));
#76624=CARTESIAN_POINT('Ctrl Pts',(-0.301189396300564,7.90812406632587,
-57.8456707030565));
#76625=CARTESIAN_POINT('Ctrl Pts',(-0.0885520643070004,7.91050437910927,
-57.8542493836455));
#76626=CARTESIAN_POINT('Ctrl Pts',(0.132988948679575,7.91298436181182,-57.8631872760181));
#76627=CARTESIAN_POINT('Ctrl Pts',(0.354800446724125,7.90615438536036,-57.8721251683908));
#76628=CARTESIAN_POINT('Ctrl Pts',(0.576111061264889,7.88999474303299,-57.8810630607634));
#76629=CARTESIAN_POINT('Ctrl Pts',(0.787697048110754,7.87454517286209,-57.8896082124811));
#76630=CARTESIAN_POINT('Ctrl Pts',(0.998824916988692,7.85056819881669,-57.8981533641988));
#76631=CARTESIAN_POINT('Ctrl Pts',(1.20881788092876,7.81809953446149,-57.9066985159165));
#76632=CARTESIAN_POINT('Ctrl Pts',(1.4184905733951,7.7856803897987,-57.9152306349674));
#76633=CARTESIAN_POINT('Ctrl Pts',(1.62703156890904,7.74479542895872,-57.9237627540182));
#76634=CARTESIAN_POINT('Ctrl Pts',(1.83376833298211,7.69553212591254,-57.9322948730691));
#76635=CARTESIAN_POINT('Ctrl Pts',(2.04005942046293,7.64637502314053,-57.940808598847));
#76636=CARTESIAN_POINT('Ctrl Pts',(2.24455379595958,7.58887567644805,-57.9493223246248));
#76637=CARTESIAN_POINT('Ctrl Pts',(2.44658818084193,7.52317268666383,-57.9578360504027));
#76638=CARTESIAN_POINT('Ctrl Pts',(2.47560291817479,7.51373689190204,-57.9590587309742));
#76639=CARTESIAN_POINT('Ctrl Pts',(2.50456693108681,7.50413198676287,-57.9602814115457));
#76640=CARTESIAN_POINT('Ctrl Pts',(2.53347826806922,7.49435846922343,-57.9615040921172));
#76641=CARTESIAN_POINT('Ctrl Pts',(2.72023584712716,7.43122481076774,-57.9694022001719));
#76642=CARTESIAN_POINT('Ctrl Pts',(2.90462196341087,7.36110954243289,-57.9773003082265));
#76643=CARTESIAN_POINT('Ctrl Pts',(3.08608986276696,7.28422750598353,-57.9851984162812));
#76644=CARTESIAN_POINT('Ctrl Pts',(3.26759908676467,7.20732796162994,-57.9930983229267));
#76645=CARTESIAN_POINT('Ctrl Pts',(3.44618845437253,7.12365871143836,-58.0009982295721));
#76646=CARTESIAN_POINT('Ctrl Pts',(3.62133263770538,7.03348213384308,-58.0088981362176));
#76647=CARTESIAN_POINT('Ctrl Pts',(3.79654549278514,6.94327019918943,-58.0168011403132));
#76648=CARTESIAN_POINT('Ctrl Pts',(3.96831016761474,6.84654600880677,-58.0247041444089));
#76649=CARTESIAN_POINT('Ctrl Pts',(4.13612706728578,6.74361726992761,-58.0326071485046));
#76650=CARTESIAN_POINT('Ctrl Pts',(4.30412849990507,6.64057534969614,-58.0405188428135));
#76651=CARTESIAN_POINT('Ctrl Pts',(4.46817319296667,6.53131542959639,-58.0484305371224));
#76652=CARTESIAN_POINT('Ctrl Pts',(4.62779060407383,6.41618852005191,-58.0563422314313));
#76653=CARTESIAN_POINT('Ctrl Pts',(4.78750324303065,6.3009929257195,-58.0642586458621));
#76654=CARTESIAN_POINT('Ctrl Pts',(4.94278306407319,6.1799235724126,-58.0721750602929));
#76655=CARTESIAN_POINT('Ctrl Pts',(5.09319337766763,6.05337114488139,-58.0800914747237));
#76656=CARTESIAN_POINT('Ctrl Pts',(5.24381364271843,5.92664206811761,-58.0880189393459));
#76657=CARTESIAN_POINT('Ctrl Pts',(5.38955056562051,5.79441485351669,-58.095946403968));
#76658=CARTESIAN_POINT('Ctrl Pts',(5.53000404279176,5.65711731243987,-58.1038738685901));
#76659=CARTESIAN_POINT('Ctrl Pts',(5.62682346950656,5.56247338133801,-58.1093385434096));
#76660=CARTESIAN_POINT('Ctrl Pts',(5.72113309984425,5.46542086394359,-58.1148032182291));
#76661=CARTESIAN_POINT('Ctrl Pts',(5.81281330100186,5.36610869510634,-58.1202678930487));
#76662=CARTESIAN_POINT('Ctrl Pts',(5.94910954444989,5.21846639752973,-58.1283919442633));
#76663=CARTESIAN_POINT('Ctrl Pts',(6.07989121708775,5.0655052690018,-58.1365159954779));
#76664=CARTESIAN_POINT('Ctrl Pts',(6.20473593274536,4.90766472009841,-58.1446400466925));
#76665=CARTESIAN_POINT('Ctrl Pts',(6.32947055221235,4.74996336525756,-58.1527569335903));
#76666=CARTESIAN_POINT('Ctrl Pts',(6.4482784550839,4.58739141945296,-58.1608738204881));
#76667=CARTESIAN_POINT('Ctrl Pts',(6.56077587581787,4.42042315930119,-58.1689907073859));
#76668=CARTESIAN_POINT('Ctrl Pts',(6.67319011625287,4.25357835504472,-58.1771015926787));
#76669=CARTESIAN_POINT('Ctrl Pts',(6.77930299951989,4.08234398301251,-58.1852124779716));
#76670=CARTESIAN_POINT('Ctrl Pts',(6.87877229876129,3.90722569885518,-58.1933233632644));
#76671=CARTESIAN_POINT('Ctrl Pts',(6.97818220307628,3.73221198100805,-58.2014294054003));
#76672=CARTESIAN_POINT('Ctrl Pts',(7.07095627605335,3.55331925393053,-58.2095354475361));
#76673=CARTESIAN_POINT('Ctrl Pts',(7.15679642731891,3.37108082043658,-58.2176414896719));
#76674=CARTESIAN_POINT('Ctrl Pts',(7.24259752190372,3.18892530418136,-58.2257438436141));
#76675=CARTESIAN_POINT('Ctrl Pts',(7.32147085031128,3.00342740715577,-58.2338461975563));
#76676=CARTESIAN_POINT('Ctrl Pts',(7.3931647158307,2.81514413211755,-58.2419485514985));
#76677=CARTESIAN_POINT('Ctrl Pts',(7.46537122377707,2.62551454949265,-58.2501088408074));
#76678=CARTESIAN_POINT('Ctrl Pts',(7.53029503972041,2.43305989051288,-58.2582691301163));
#76679=CARTESIAN_POINT('Ctrl Pts',(7.58772835729282,2.2383698032127,-58.2664294194251));
#76680=CARTESIAN_POINT('Ctrl Pts',(7.64473244252684,2.04513474732919,-58.2745287221811));
#76681=CARTESIAN_POINT('Ctrl Pts',(7.69435753628214,1.84969787995055,-58.2826280249371));
#76682=CARTESIAN_POINT('Ctrl Pts',(7.73645038245148,1.65265134855068,-58.290727327693));
#76683=CARTESIAN_POINT('Ctrl Pts',(7.77854301549651,1.45560581483591,-58.2988265894406));
#76684=CARTESIAN_POINT('Ctrl Pts',(7.81310341012868,1.25695094704828,-58.3069258511882));
#76685=CARTESIAN_POINT('Ctrl Pts',(7.84002929200141,1.05728979024667,-58.3150251129358));
#76686=CARTESIAN_POINT('Ctrl Pts',(7.86695851597118,0.857603851082755,-58.3231253799808));
#76687=CARTESIAN_POINT('Ctrl Pts',(7.88625129500784,0.656911691738669,-58.3312256470258));
#76688=CARTESIAN_POINT('Ctrl Pts',(7.8978570906672,0.455822745590702,-58.3393259140708));
#76689=CARTESIAN_POINT('Ctrl Pts',(7.90961408817888,0.252113985857309,-58.3475317124742));
#76690=CARTESIAN_POINT('Ctrl Pts',(7.9134823826409,0.0479983655472201,-58.3557375108776));
#76691=CARTESIAN_POINT('Ctrl Pts',(7.90946392466752,-0.155889141325008,
-58.363943309281));
#76692=CARTESIAN_POINT('Ctrl Pts',(7.90549335173915,-0.357347068864224,
-58.3720513251449));
#76693=CARTESIAN_POINT('Ctrl Pts',(7.89382300183199,-0.558581968020428,
-58.3801593410087));
#76694=CARTESIAN_POINT('Ctrl Pts',(7.87450716322381,-0.758984806393986,
-58.3882673568725));
#76695=CARTESIAN_POINT('Ctrl Pts',(7.85484190156595,-0.96301292722977,-58.3965220465457));
#76696=CARTESIAN_POINT('Ctrl Pts',(7.82725193743623,-1.16617824928713,-58.4047767362189));
#76697=CARTESIAN_POINT('Ctrl Pts',(7.79184931729559,-1.36784692731325,-58.4130314258921));
#76698=CARTESIAN_POINT('Ctrl Pts',(7.75644669715494,-1.56951560533937,-58.4212861155654));
#76699=CARTESIAN_POINT('Ctrl Pts',(7.71323152042349,-1.76968730392838,-58.4295408052386));
#76700=CARTESIAN_POINT('Ctrl Pts',(7.66236985097129,-1.96774217491169,-58.4377954949118));
#76701=CARTESIAN_POINT('Ctrl Pts',(7.61414229894411,-2.15553981697616,-58.4456226755759));
#76702=CARTESIAN_POINT('Ctrl Pts',(7.55894713824618,-2.34179431903526,-58.4534498562401));
#76703=CARTESIAN_POINT('Ctrl Pts',(7.49690066953181,-2.52594563503917,-58.4612770369042));
#76704=CARTESIAN_POINT('Ctrl Pts',(7.43490653106102,-2.70994163707567,-58.4690976160924));
#76705=CARTESIAN_POINT('Ctrl Pts',(7.36607270179688,-2.8918376534716,-58.4769181952806));
#76706=CARTESIAN_POINT('Ctrl Pts',(7.29056612145986,-3.07108557819898,-58.4847387744688));
#76707=CARTESIAN_POINT('Ctrl Pts',(7.21510988267937,-3.25021399520272,-58.4925541395402));
#76708=CARTESIAN_POINT('Ctrl Pts',(7.13298988893582,-3.42669751336263,-58.5003695046116));
#76709=CARTESIAN_POINT('Ctrl Pts',(7.04442238528958,-3.60000475800118,-58.508184869683));
#76710=CARTESIAN_POINT('Ctrl Pts',(6.95589726898374,-3.77322905988,-58.5159964944149));
#76711=CARTESIAN_POINT('Ctrl Pts',(6.86093094902157,-3.94327980316541,-58.5238081191467));
#76712=CARTESIAN_POINT('Ctrl Pts',(6.7597871872997,-4.10964696566735,-58.5316197438785));
#76713=CARTESIAN_POINT('Ctrl Pts',(6.65867285555185,-4.27596572003035,-58.5394290956485));
#76714=CARTESIAN_POINT('Ctrl Pts',(6.55138484618283,-4.43860272842584,-58.5472384474184));
#76715=CARTESIAN_POINT('Ctrl Pts',(6.43823220753763,-4.59707374770355,-58.5550477991884));
#76716=CARTESIAN_POINT('Ctrl Pts',(6.3250730511939,-4.75555389506118,-58.5628576007843));
#76717=CARTESIAN_POINT('Ctrl Pts',(6.20604879017585,-4.9098672834239,-58.5706674023803));
#76718=CARTESIAN_POINT('Ctrl Pts',(6.08151128181401,-5.05955942046033,-58.5784772039763));
#76719=CARTESIAN_POINT('Ctrl Pts',(5.98539707458308,-5.17508719413442,-58.5845045679319));
#76720=CARTESIAN_POINT('Ctrl Pts',(5.88599991776427,-5.28786298909097,-58.5905319318876));
#76721=CARTESIAN_POINT('Ctrl Pts',(5.78349774602666,-5.3976916197301,-58.5965592958433));
#76722=CARTESIAN_POINT('Ctrl Pts',(5.63624585190805,-5.55546850987703,-58.6052180466187));
#76723=CARTESIAN_POINT('Ctrl Pts',(5.48265750959305,-5.70708495534743,-58.6138767973941));
#76724=CARTESIAN_POINT('Ctrl Pts',(5.32325943148045,-5.85207911986454,-58.6225355481695));
#76725=CARTESIAN_POINT('Ctrl Pts',(5.16358670029539,-5.99732311859072,-58.6312092185257));
#76726=CARTESIAN_POINT('Ctrl Pts',(4.99808438945357,-6.13592187420624,-58.6398828888818));
#76727=CARTESIAN_POINT('Ctrl Pts',(4.82731218949133,-6.26745387100603,-58.648556559238));
#76728=CARTESIAN_POINT('Ctrl Pts',(4.65213878395515,-6.40237576005756,-58.6574537706994));
#76729=CARTESIAN_POINT('Ctrl Pts',(4.47142045450506,-6.52986163258815,-58.6663509821608));
#76730=CARTESIAN_POINT('Ctrl Pts',(4.28579100704396,-6.64950497736043,-58.6752481936222));
#76731=CARTESIAN_POINT('Ctrl Pts',(4.10420815118273,-6.76654018123396,-58.6839514521216));
#76732=CARTESIAN_POINT('Ctrl Pts',(3.91792627144628,-6.87607113708023,-58.6926547106211));
#76733=CARTESIAN_POINT('Ctrl Pts',(3.72756326656371,-6.97776419018047,-58.7013579691205));
#76734=CARTESIAN_POINT('Ctrl Pts',(3.53083687456925,-7.08285660264607,-58.7103521570629));
#76735=CARTESIAN_POINT('Ctrl Pts',(3.329752063795,-7.1795779754511,-58.7193463450053));
#76736=CARTESIAN_POINT('Ctrl Pts',(3.12501450883253,-7.26761345419431,-58.7283405329477));
#76737=CARTESIAN_POINT('Ctrl Pts',(2.92027695387007,-7.35564893293752,-58.73733472089));
#76738=CARTESIAN_POINT('Ctrl Pts',(2.71188690799654,-7.43499844067692,-58.7463289088324));
#76739=CARTESIAN_POINT('Ctrl Pts',(2.5005704045462,-7.50540263089913,-58.7553230967748));
#76740=CARTESIAN_POINT('Ctrl Pts',(2.30602259325594,-7.5702200062094,-58.7636035649349));
#76741=CARTESIAN_POINT('Ctrl Pts',(2.10882647462805,-7.62751117665964,-58.7718840330949));
#76742=CARTESIAN_POINT('Ctrl Pts',(1.90958123564917,-7.67707108892816,-58.780164501255));
#76743=CARTESIAN_POINT('Ctrl Pts',(1.71051044070642,-7.72658761029224,-58.7884377196646));
#76744=CARTESIAN_POINT('Ctrl Pts',(1.50939439240345,-7.76838630330906,-58.7967109380741));
#76745=CARTESIAN_POINT('Ctrl Pts',(1.3068474972431,-7.80231187654976,-58.8049841564836));
#76746=CARTESIAN_POINT('Ctrl Pts',(1.10446218895956,-7.83621038481166,-58.8132507747251));
#76747=CARTESIAN_POINT('Ctrl Pts',(0.900648604277325,-7.86224825325279,
-58.8215173929667));
#76748=CARTESIAN_POINT('Ctrl Pts',(0.696032189003861,-7.88032107162332,
-58.8297840112083));
#76749=CARTESIAN_POINT('Ctrl Pts',(0.491605623434067,-7.89837712145059,
-58.8380429594151));
#76750=CARTESIAN_POINT('Ctrl Pts',(0.286378010497993,-7.90848284528599,
-58.8463019076219));
#76751=CARTESIAN_POINT('Ctrl Pts',(0.0809811801980997,-7.91058550604528,
-58.8545608558286));
#76752=CARTESIAN_POINT('Ctrl Pts',(-0.124296303540743,-7.91268694504605,
-58.8628150051441));
#76753=CARTESIAN_POINT('Ctrl Pts',(-0.329742510875407,-7.90679459287275,
-58.8710691544595));
#76754=CARTESIAN_POINT('Ctrl Pts',(-0.534723027352655,-7.89290772048038,
-58.879323303775));
#76755=CARTESIAN_POINT('Ctrl Pts',(-0.739574435034937,-7.87902959485767,
-58.8875722541414));
#76756=CARTESIAN_POINT('Ctrl Pts',(-0.943960440065985,-7.8571670181748,
-58.8958212045077));
#76757=CARTESIAN_POINT('Ctrl Pts',(-1.14724860916018,-7.8273713102663,-58.9040701548741));
#76758=CARTESIAN_POINT('Ctrl Pts',(-1.22953323205989,-7.81531094984196,
-58.9074090691515));
#76759=CARTESIAN_POINT('Ctrl Pts',(-1.31163802229569,-7.80195143964422,
-58.9107479834289));
#76760=CARTESIAN_POINT('Ctrl Pts',(-1.39352124695277,-7.78729860312876,
-58.9140868977063));
#76761=CARTESIAN_POINT('Ctrl Pts',(-1.593574597164,-7.75149946298389,-58.9222443803904));
#76762=CARTESIAN_POINT('Ctrl Pts',(-1.79221772401568,-7.70799244489013,
-58.9304018630746));
#76763=CARTESIAN_POINT('Ctrl Pts',(-1.98884540888124,-7.65691941576846,
-58.9385593457587));
#76764=CARTESIAN_POINT('Ctrl Pts',(-2.1855319194016,-7.60583110698573,-58.9467192689398));
#76765=CARTESIAN_POINT('Ctrl Pts',(-2.38020148346095,-7.54717235000572,
-58.9548791921208));
#76766=CARTESIAN_POINT('Ctrl Pts',(-2.57226312296309,-7.48113516962795,
-58.9630391153019));
#76767=CARTESIAN_POINT('Ctrl Pts',(-2.76440328367153,-7.41507099104753,
-58.9712023745318));
#76768=CARTESIAN_POINT('Ctrl Pts',(-2.95393309825705,-7.34162247254659,
-58.9793656337617));
#76769=CARTESIAN_POINT('Ctrl Pts',(-3.14028006557105,-7.26103037521378,
-58.9875288929916));
#76770=CARTESIAN_POINT('Ctrl Pts',(-3.32680413727205,-7.1803616830525,-58.9956999105931));
#76771=CARTESIAN_POINT('Ctrl Pts',(-3.51013903017709,-7.09253596794178,
-59.0038709281946));
#76772=CARTESIAN_POINT('Ctrl Pts',(-3.68973410881148,-6.99784132474245,
-59.0120419457962));
#76773=CARTESIAN_POINT('Ctrl Pts',(-3.86942144382874,-6.9030980377533,-59.0202171607762));
#76774=CARTESIAN_POINT('Ctrl Pts',(-4.0453648593851,-6.80147893396333,-59.0283923757563));
#76775=CARTESIAN_POINT('Ctrl Pts',(-4.21704044198085,-6.69331688407907,
-59.0365675907364));
#76776=CARTESIAN_POINT('Ctrl Pts',(-4.38889848638682,-6.58503987641735,
-59.044751494573));
#76777=CARTESIAN_POINT('Ctrl Pts',(-4.55647937343348,-6.47020619796347,
-59.0529353984097));
#76778=CARTESIAN_POINT('Ctrl Pts',(-4.71928897235881,-6.34919149147138,
-59.0611193022464));
#76779=CARTESIAN_POINT('Ctrl Pts',(-4.79708330211563,-6.29136776335945,
-59.0650297677102));
#76780=CARTESIAN_POINT('Ctrl Pts',(-4.87378875650194,-6.23213340341129,
-59.068940233174));
#76781=CARTESIAN_POINT('Ctrl Pts',(-4.94935420446545,-6.17153254538451,
-59.0728506986378));
#76782=CARTESIAN_POINT('Ctrl Pts',(-5.1009359491697,-6.04996926431046,-59.0806949607123));
#76783=CARTESIAN_POINT('Ctrl Pts',(-5.24821928464149,-5.92267130269681,
-59.0885392227869));
#76784=CARTESIAN_POINT('Ctrl Pts',(-5.39074057696754,-5.78997729113299,
-59.0963834848614));
#76785=CARTESIAN_POINT('Ctrl Pts',(-5.53313583457969,-5.6574006238025,-59.1042208100825));
#76786=CARTESIAN_POINT('Ctrl Pts',(-5.67077718123352,-5.51943764764221,
-59.1120581353035));
#76787=CARTESIAN_POINT('Ctrl Pts',(-5.80323284396378,-5.37646813054258,
-59.1198954605245));
#76788=CARTESIAN_POINT('Ctrl Pts',(-5.93559695283294,-5.23359743452043,
-59.1277273685564));
#76789=CARTESIAN_POINT('Ctrl Pts',(-6.06278228019247,-5.08572734678121,
-59.1355592765882));
#76790=CARTESIAN_POINT('Ctrl Pts',(-6.18439267908374,-4.93327560459534,
-59.1433911846201));
#76791=CARTESIAN_POINT('Ctrl Pts',(-6.30594249857902,-4.78089980521159,
-59.15121919124));
#76792=CARTESIAN_POINT('Ctrl Pts',(-6.42192270412385,-4.62394717177293,
-59.1590471978599));
#76793=CARTESIAN_POINT('Ctrl Pts',(-6.53197621747703,-4.46286989439694,
-59.1668752044799));
#76794=CARTESIAN_POINT('Ctrl Pts',(-6.64374089025095,-4.29928811814352,
-59.1748249243179));
#76795=CARTESIAN_POINT('Ctrl Pts',(-6.74939279949715,-4.13145264848913,
-59.1827746441559));
#76796=CARTESIAN_POINT('Ctrl Pts',(-6.84860216557749,-3.95986986877693,
-59.190724363994));
#76797=CARTESIAN_POINT('Ctrl Pts',(-6.9462700263592,-3.79095312529222,-59.198550561873));
#76798=CARTESIAN_POINT('Ctrl Pts',(-7.03769392991793,-3.61840499634442,
-59.206376759752));
#76799=CARTESIAN_POINT('Ctrl Pts',(-7.12260440071309,-3.44273547501729,
-59.214202957631));
#76800=CARTESIAN_POINT('Ctrl Pts',(-7.20752447139024,-3.26704609269235,
-59.2220300403311));
#76801=CARTESIAN_POINT('Ctrl Pts',(-7.28592948924982,-3.08823493065946,
-59.2298571230312));
#76802=CARTESIAN_POINT('Ctrl Pts',(-7.35759718539343,-2.90683412968312,
-59.2376842057313));
#76803=CARTESIAN_POINT('Ctrl Pts',(-7.42928551732976,-2.72538109667577,
-59.2455135421394));
#76804=CARTESIAN_POINT('Ctrl Pts',(-7.49423253421238,-2.54133726544852,
-59.2533428785474));
#76805=CARTESIAN_POINT('Ctrl Pts',(-7.55226505272291,-2.3552523375257,-59.2611722149555));
#76806=CARTESIAN_POINT('Ctrl Pts',(-7.61186909651773,-2.16412821473829,
-59.2692135704252));
#76807=CARTESIAN_POINT('Ctrl Pts',(-7.66417875621187,-1.97085127087421,
-59.277254925895));
#76808=CARTESIAN_POINT('Ctrl Pts',(-7.70906204074682,-1.77603025084496,
-59.2852962813648));
#76809=CARTESIAN_POINT('Ctrl Pts',(-7.7528314978707,-1.58604392583883,-59.2931380818725));
#76810=CARTESIAN_POINT('Ctrl Pts',(-7.78953877974173,-1.39458960276944,
-59.3009798823802));
#76811=CARTESIAN_POINT('Ctrl Pts',(-7.81911395936368,-1.20223869946197,
-59.3088216828878));
#76812=CARTESIAN_POINT('Ctrl Pts',(-7.84981806476796,-1.00254549437397,
-59.3169628158387));
#76813=CARTESIAN_POINT('Ctrl Pts',(-7.87283483272258,-0.801886345405845,
-59.3251039487895));
#76814=CARTESIAN_POINT('Ctrl Pts',(-7.88814537586744,-0.600902262586137,
-59.3332450817403));
#76815=CARTESIAN_POINT('Ctrl Pts',(-7.9034559190123,-0.399918179766429,
-59.3413862146912));
#76816=CARTESIAN_POINT('Ctrl Pts',(-7.91106028968049,-0.198609580813962,
-59.349527347642));
#76817=CARTESIAN_POINT('Ctrl Pts',(-7.91099963985057,0.00238710789585057,
-59.3576684805928));
#76818=CARTESIAN_POINT('Origin',(0.,0.,-63.6971797838103));
#76819=CARTESIAN_POINT('',(-6.76699852120032,-0.00296022942052201,59.3028202161897));
#76820=CARTESIAN_POINT('Ctrl Pts',(3.09908550384712,6.01564277861017,58.6513967904261));
#76821=CARTESIAN_POINT('Ctrl Pts',(2.93373232018322,6.10082796552483,58.6601462383254));
#76822=CARTESIAN_POINT('Ctrl Pts',(2.76486502144422,6.17919158180192,58.6688956862247));
#76823=CARTESIAN_POINT('Ctrl Pts',(2.59305716434349,6.2504674659138,58.677645134124));
#76824=CARTESIAN_POINT('Ctrl Pts',(2.42125069459275,6.32174277447228,58.6863945113714));
#76825=CARTESIAN_POINT('Ctrl Pts',(2.24650397871046,6.3859303555783,58.6951438886188));
#76826=CARTESIAN_POINT('Ctrl Pts',(2.06941053323754,6.44281220003544,58.7038932658663));
#76827=CARTESIAN_POINT('Ctrl Pts',(1.89231845896675,6.49969360406687,58.7126425753688));
#76828=CARTESIAN_POINT('Ctrl Pts',(1.71287996431505,6.5492692970088,58.7213918848715));
#76829=CARTESIAN_POINT('Ctrl Pts',(1.53170449173513,6.59137090065477,58.730141194374));
#76830=CARTESIAN_POINT('Ctrl Pts',(1.35053036178176,6.63347219230082,58.7388904390386));
#76831=CARTESIAN_POINT('Ctrl Pts',(1.16761955878847,6.66809944062454,58.7476396837032));
#76832=CARTESIAN_POINT('Ctrl Pts',(0.983593309310479,6.69513503985392,58.7563889283678));
#76833=CARTESIAN_POINT('Ctrl Pts',(0.799568362460015,6.72217044771214,58.765138111101));
#76834=CARTESIAN_POINT('Ctrl Pts',(0.614428268438671,6.74161427235976,58.7738872938342));
#76835=CARTESIAN_POINT('Ctrl Pts',(0.428801816330387,6.75340047696801,58.7826364765673));
#76836=CARTESIAN_POINT('Ctrl Pts',(0.243176616522917,6.76518660206241,58.7913856002755));
#76837=CARTESIAN_POINT('Ctrl Pts',(0.0570653511656112,6.76931519233997,
58.8001347239836));
#76838=CARTESIAN_POINT('Ctrl Pts',(-0.128899900799864,6.76577222610795,
58.8088838476917));
#76839=CARTESIAN_POINT('Ctrl Pts',(-0.314863959941901,6.76222928260134,
58.817632915281));
#76840=CARTESIAN_POINT('Ctrl Pts',(-0.500681721080607,6.75101488651277,
58.8263819828702));
#76841=CARTESIAN_POINT('Ctrl Pts',(-0.685722110173271,6.73216712415991,
58.8351310504595));
#76842=CARTESIAN_POINT('Ctrl Pts',(-0.870761373827518,6.71331947644146,
58.8438800648359));
#76843=CARTESIAN_POINT('Ctrl Pts',(-1.05502298984327,6.68683858439999,58.8526290792122));
#76844=CARTESIAN_POINT('Ctrl Pts',(-1.23788117676037,6.6528143813143,58.8613780935886));
#76845=CARTESIAN_POINT('Ctrl Pts',(-1.43009641451765,6.61704912302383,58.8705748044761));
#76846=CARTESIAN_POINT('Ctrl Pts',(-1.62076048992662,6.57294837083173,58.8797715153636));
#76847=CARTESIAN_POINT('Ctrl Pts',(-1.80915798961093,6.5206776004206,58.8889682262512));
#76848=CARTESIAN_POINT('Ctrl Pts',(-1.98840443002967,6.47094578577423,58.8977182239577));
#76849=CARTESIAN_POINT('Ctrl Pts',(-2.16559895952141,6.41381888474493,58.9064682216642));
#76850=CARTESIAN_POINT('Ctrl Pts',(-2.34013966242265,6.34949095285255,58.9152182193707));
#76851=CARTESIAN_POINT('Ctrl Pts',(-2.5146768255395,6.28516432556711,58.9239680396223));
#76852=CARTESIAN_POINT('Ctrl Pts',(-2.68656000078769,6.21363705879692,58.9327178598738));
#76853=CARTESIAN_POINT('Ctrl Pts',(-2.85520533840808,6.13515211510897,58.9414676801254));
#76854=CARTESIAN_POINT('Ctrl Pts',(-3.02384747998247,6.05666865881161,58.9502173345567));
#76855=CARTESIAN_POINT('Ctrl Pts',(-3.18925164684457,5.97122791039887,58.9589669889879));
#76856=CARTESIAN_POINT('Ctrl Pts',(-3.35085601829078,5.87912008251954,58.9677166434192));
#76857=CARTESIAN_POINT('Ctrl Pts',(-3.51245754191336,5.78701387778224,58.9764661436623));
#76858=CARTESIAN_POINT('Ctrl Pts',(-3.67025915510852,5.68824097061037,58.9852156439055));
#76859=CARTESIAN_POINT('Ctrl Pts',(-3.82372487928749,5.58313684656913,58.9939651441486));
#76860=CARTESIAN_POINT('Ctrl Pts',(-3.97718810300705,5.4780344350184,59.0027145018337));
#76861=CARTESIAN_POINT('Ctrl Pts',(-4.12631534262926,5.36660117496452,59.0114638595189));
#76862=CARTESIAN_POINT('Ctrl Pts',(-4.27060009886119,5.24921554097437,59.020213217204));
#76863=CARTESIAN_POINT('Ctrl Pts',(-4.41488269594112,5.13183166360378,59.0289624439592));
#76864=CARTESIAN_POINT('Ctrl Pts',(-4.55432273234992,5.00849577139558,59.0377116707143));
#76865=CARTESIAN_POINT('Ctrl Pts',(-4.68844662480115,4.8796267527743,59.0464608974695));
#76866=CARTESIAN_POINT('Ctrl Pts',(-4.82256868835062,4.75075949139979,59.055210004921));
#76867=CARTESIAN_POINT('Ctrl Pts',(-4.95137454637762,4.61635945312632,59.0639591123725));
#76868=CARTESIAN_POINT('Ctrl Pts',(-5.07442674460975,4.47688309134707,59.072708219824));
#76869=CARTESIAN_POINT('Ctrl Pts',(-5.19747742838423,4.33740844616489,59.0814572195963));
#76870=CARTESIAN_POINT('Ctrl Pts',(-5.314774404508,4.1928578173619,59.0902062193687));
#76871=CARTESIAN_POINT('Ctrl Pts',(-5.42591931531016,4.04372211999591,59.098955219141));
#76872=CARTESIAN_POINT('Ctrl Pts',(-5.53707636462847,3.89457013500993,59.1077051744216));
#76873=CARTESIAN_POINT('Ctrl Pts',(-5.64207983273339,3.74083230916619,59.1164551297022));
#76874=CARTESIAN_POINT('Ctrl Pts',(-5.74057303468619,3.58303087252034,59.1252050849828));
#76875=CARTESIAN_POINT('Ctrl Pts',(-5.83906243363648,3.4252355288763,59.1339547024116));
#76876=CARTESIAN_POINT('Ctrl Pts',(-5.9310419176832,3.26337713157185,59.1427043198404));
#76877=CARTESIAN_POINT('Ctrl Pts',(-6.01619906699561,3.0980054529134,59.1514539372692));
#76878=CARTESIAN_POINT('Ctrl Pts',(-6.10135338095297,2.93263928039775,59.1602032633746));
#76879=CARTESIAN_POINT('Ctrl Pts',(-6.17968568352761,2.76376031540399,59.16895258948));
#76880=CARTESIAN_POINT('Ctrl Pts',(-6.25092992694816,2.59194213831711,59.1777019155854));
#76881=CARTESIAN_POINT('Ctrl Pts',(-6.32217217691038,2.42012876880992,59.1864509968792));
#76882=CARTESIAN_POINT('Ctrl Pts',(-6.38632665483789,2.24537661647845,59.195200078173));
#76883=CARTESIAN_POINT('Ctrl Pts',(-6.44317547869293,2.06827917621634,59.2039491594668));
#76884=CARTESIAN_POINT('Ctrl Pts',(-6.50002944235881,1.8911657242361,59.2126990317817));
#76885=CARTESIAN_POINT('Ctrl Pts',(-6.54957634250346,1.71170683289395,59.2214489040967));
#76886=CARTESIAN_POINT('Ctrl Pts',(-6.59164787708347,1.53051209225571,59.2301987764117));
#76887=CARTESIAN_POINT('Ctrl Pts',(-6.63371649074966,1.34932993148241,59.2389480412464));
#76888=CARTESIAN_POINT('Ctrl Pts',(-6.66831071257086,1.16641244174219,59.2476973060812));
#76889=CARTESIAN_POINT('Ctrl Pts',(-6.69531304840301,0.982380875162206,
59.256446570916));
#76890=CARTESIAN_POINT('Ctrl Pts',(-6.72231677033018,0.798339861798014,
59.2651962848717));
#76891=CARTESIAN_POINT('Ctrl Pts',(-6.7417277847787,0.613184940732301,59.2739459988273));
#76892=CARTESIAN_POINT('Ctrl Pts',(-6.75348015835505,0.427545027692672,
59.282695712783));
#76893=CARTESIAN_POINT('Ctrl Pts',(-6.76249038365204,0.285219953550303,
59.2894038805852));
#76894=CARTESIAN_POINT('Ctrl Pts',(-6.76699999999987,0.142609995762151,
59.2961120483875));
#76895=CARTESIAN_POINT('Ctrl Pts',(-6.767,6.12589398735536E-12,59.3028202161897));
#76896=CARTESIAN_POINT('',(3.93017071637407,-5.50872463825845,59.9999950688108));
#76897=CARTESIAN_POINT('Ctrl Pts',(-6.7669966225104,-0.00676098608203946,
59.3028202161897));
#76898=CARTESIAN_POINT('Ctrl Pts',(-6.76676245139478,-0.241140280658097,
59.3138571345979));
#76899=CARTESIAN_POINT('Ctrl Pts',(-6.75434836748514,-0.474955858725596,
59.3248940530061));
#76900=CARTESIAN_POINT('Ctrl Pts',(-6.72994860126805,-0.707163930280838,
59.3359309714143));
#76901=CARTESIAN_POINT('Ctrl Pts',(-6.70469071231455,-0.947538597532459,
59.3473560505344));
#76902=CARTESIAN_POINT('Ctrl Pts',(-6.66658916004148,-1.18619120591911,
59.3587811296546));
#76903=CARTESIAN_POINT('Ctrl Pts',(-6.61590677114137,-1.42199388028421,
59.3702062087747));
#76904=CARTESIAN_POINT('Ctrl Pts',(-6.58607853721709,-1.56077142182427,
59.3769302393501));
#76905=CARTESIAN_POINT('Ctrl Pts',(-6.55189355796116,-1.69856235289583,
59.3836542699255));
#76906=CARTESIAN_POINT('Ctrl Pts',(-6.51341303837284,-1.83514021032582,
59.390378300501));
#76907=CARTESIAN_POINT('Ctrl Pts',(-6.46732120164663,-1.99873270783956,
59.3984323216717));
#76908=CARTESIAN_POINT('Ctrl Pts',(-6.4149747861413,-2.16089713411304,59.4064863428424));
#76909=CARTESIAN_POINT('Ctrl Pts',(-6.35647389237976,-2.32110505050818,
59.4145403640131));
#76910=CARTESIAN_POINT('Ctrl Pts',(-6.29804717134514,-2.48110984080951,
59.422584173567));
#76911=CARTESIAN_POINT('Ctrl Pts',(-6.23348162378241,-2.63916270946047,
59.4306279831208));
#76912=CARTESIAN_POINT('Ctrl Pts',(-6.16292816805098,-2.79474603415836,
59.4386717926746));
#76913=CARTESIAN_POINT('Ctrl Pts',(-6.09244856921295,-2.9501664908449,59.4467071817935));
#76914=CARTESIAN_POINT('Ctrl Pts',(-6.01599368843736,-3.10312220959545,
59.4547425709124));
#76915=CARTESIAN_POINT('Ctrl Pts',(-5.9337639612522,-3.25311147244368,59.4627779600313));
#76916=CARTESIAN_POINT('Ctrl Pts',(-5.85160216824035,-3.40297682150881,
59.4708067107052));
#76917=CARTESIAN_POINT('Ctrl Pts',(-5.76367520277198,-3.549880265369,59.4788354613792));
#76918=CARTESIAN_POINT('Ctrl Pts',(-5.6702311985322,-3.69334092052062,59.4868642120531));
#76919=CARTESIAN_POINT('Ctrl Pts',(-5.57684379896657,-3.83671467289336,
59.4948880992281));
#76920=CARTESIAN_POINT('Ctrl Pts',(-5.47794621688296,-3.97664947481862,
59.5029119864031));
#76921=CARTESIAN_POINT('Ctrl Pts',(-5.37383196588725,-4.11268999590394,
59.5109358735781));
#76922=CARTESIAN_POINT('Ctrl Pts',(-5.26734063065929,-4.25183652576834,
59.5191429581109));
#76923=CARTESIAN_POINT('Ctrl Pts',(-5.15539175069455,-4.38690846339147,
59.5273500426437));
#76924=CARTESIAN_POINT('Ctrl Pts',(-5.03834590325707,-4.51745055967774,
59.5355571271764));
#76925=CARTESIAN_POINT('Ctrl Pts',(-4.92395316522499,-4.64503362349048,
59.5435781795376));
#76926=CARTESIAN_POINT('Ctrl Pts',(-4.80469231569053,-4.76828971445624,
59.5515992318988));
#76927=CARTESIAN_POINT('Ctrl Pts',(-4.68093990593028,-4.8868282757909,59.5596202842601));
#76928=CARTESIAN_POINT('Ctrl Pts',(-4.55717567703545,-5.00537815830478,
59.5676421026823));
#76929=CARTESIAN_POINT('Ctrl Pts',(-4.42891930459848,-5.11920935457248,
59.5756639211046));
#76930=CARTESIAN_POINT('Ctrl Pts',(-4.29658302598711,-5.22796932860164,
59.5836857395269));
#76931=CARTESIAN_POINT('Ctrl Pts',(-4.16420771428784,-5.33676138179813,
59.5917099240149));
#76932=CARTESIAN_POINT('Ctrl Pts',(-4.02775039091781,-5.44047899770564,
59.5997341085029));
#76933=CARTESIAN_POINT('Ctrl Pts',(-3.88765492987487,-5.53881107695682,
59.607758292991));
#76934=CARTESIAN_POINT('Ctrl Pts',(-3.74194723076937,-5.64108234905435,
59.6161039271054));
#76935=CARTESIAN_POINT('Ctrl Pts',(-3.59230424695664,-5.73752741084,59.6244495612198));
#76936=CARTESIAN_POINT('Ctrl Pts',(-3.43925576289736,-5.82784769853994,
59.6327951953342));
#76937=CARTESIAN_POINT('Ctrl Pts',(-3.29184412045361,-5.91484145112546,
59.6408334561481));
#76938=CARTESIAN_POINT('Ctrl Pts',(-3.14127371831896,-5.99615343455977,
59.648871716962));
#76939=CARTESIAN_POINT('Ctrl Pts',(-2.98803986133646,-6.07156543134177,
59.6569099777759));
#76940=CARTESIAN_POINT('Ctrl Pts',(-2.8346906192944,-6.14703421334025,59.6649542913983));
#76941=CARTESIAN_POINT('Ctrl Pts',(-2.67867426953415,-6.21659401200429,
59.6729986050208));
#76942=CARTESIAN_POINT('Ctrl Pts',(-2.52050341237357,-6.28007575975109,
59.6810429186433));
#76943=CARTESIAN_POINT('Ctrl Pts',(-2.36210941707737,-6.34364706381118,
59.6890985807099));
#76944=CARTESIAN_POINT('Ctrl Pts',(-2.20155520008267,-6.40112308495481,
59.6971542427765));
#76945=CARTESIAN_POINT('Ctrl Pts',(-2.03936627375364,-6.4523851560083,59.7052099048432));
#76946=CARTESIAN_POINT('Ctrl Pts',(-2.02127295671169,-6.4581038010773,59.7061085706834));
#76947=CARTESIAN_POINT('Ctrl Pts',(-2.00315930335778,-6.46374516653992,
59.7070072365237));
#76948=CARTESIAN_POINT('Ctrl Pts',(-1.98502604839923,-6.46930912750168,
59.7079059023639));
#76949=CARTESIAN_POINT('Ctrl Pts',(-1.8179755959339,-6.52056645544894,59.716184754427));
#76950=CARTESIAN_POINT('Ctrl Pts',(-1.64870852544739,-6.56541988083409,
59.7244636064902));
#76951=CARTESIAN_POINT('Ctrl Pts',(-1.47775383359712,-6.60367568913624,
59.7327424585533));
#76952=CARTESIAN_POINT('Ctrl Pts',(-1.30700296077214,-6.64188588733272,
59.7410114402377));
#76953=CARTESIAN_POINT('Ctrl Pts',(-1.13456881615889,-6.67351405838662,
59.749280421922));
#76954=CARTESIAN_POINT('Ctrl Pts',(-0.960996955664091,-6.69841577174815,
59.7575494036064));
#76955=CARTESIAN_POINT('Ctrl Pts',(-0.787598457064301,-6.7232926135193,
59.7658101263118));
#76956=CARTESIAN_POINT('Ctrl Pts',(-0.613064854139222,-6.74145633030057,
59.7740708490173));
#76957=CARTESIAN_POINT('Ctrl Pts',(-0.437953487104271,-6.75281317253285,
59.7823315717228));
#76958=CARTESIAN_POINT('Ctrl Pts',(-0.262983158915239,-6.7641608676952,
59.7905856410463));
#76959=CARTESIAN_POINT('Ctrl Pts',(-0.0874363452809178,-6.7687125879057,
59.79883971037));
#76960=CARTESIAN_POINT('Ctrl Pts',(0.0881227175283366,-6.76642619014317,
59.8070937796936));
#76961=CARTESIAN_POINT('Ctrl Pts',(0.263568487755914,-6.76414126784936,
59.8153425224632));
#76962=CARTESIAN_POINT('Ctrl Pts',(0.439026138577658,-6.7550270268809,59.8235912652328));
#76963=CARTESIAN_POINT('Ctrl Pts',(0.613929548963045,-6.73909337440208,
59.8318400080024));
#76964=CARTESIAN_POINT('Ctrl Pts',(0.788771168558378,-6.72316535104721,
59.8400858366131));
#76965=CARTESIAN_POINT('Ctrl Pts',(0.963058585888288,-6.70042274672029,
59.8483316652238));
#76966=CARTESIAN_POINT('Ctrl Pts',(1.13622860175855,-6.6709274890787,59.8565774938345));
#76967=CARTESIAN_POINT('Ctrl Pts',(1.30936777225028,-6.64143748518951,59.8648218536822));
#76968=CARTESIAN_POINT('Ctrl Pts',(1.48138958922909,-6.60519728369291,59.87306621353));
#76969=CARTESIAN_POINT('Ctrl Pts',(1.65173875488613,-6.56232032787239,59.8813105733777));
#76970=CARTESIAN_POINT('Ctrl Pts',(1.82208741484256,-6.51944349933693,59.8895549087511));
#76971=CARTESIAN_POINT('Ctrl Pts',(1.99076309056789,-6.4699300429887,59.8977992441246));
#76972=CARTESIAN_POINT('Ctrl Pts',(2.15722329153252,-6.41394392479928,59.906043579498));
#76973=CARTESIAN_POINT('Ctrl Pts',(2.32377430564038,-6.35792726312055,59.9142924126072));
#76974=CARTESIAN_POINT('Ctrl Pts',(2.48810709374139,-6.29543099531484,59.9225412457165));
#76975=CARTESIAN_POINT('Ctrl Pts',(2.64969617231629,-6.22666838641761,59.9307900788258));
#76976=CARTESIAN_POINT('Ctrl Pts',(2.81132951822863,-6.15788693999967,59.9390411717033));
#76977=CARTESIAN_POINT('Ctrl Pts',(2.97021733406415,-6.08283587684997,59.9472922645809));
#76978=CARTESIAN_POINT('Ctrl Pts',(3.12585648725734,-6.00177558902957,59.9555433574585));
#76979=CARTESIAN_POINT('Ctrl Pts',(3.28164598528946,-5.92063699831645,59.9638024207549));
#76980=CARTESIAN_POINT('Ctrl Pts',(3.43418024003722,-5.83347775498091,59.9720614840512));
#76981=CARTESIAN_POINT('Ctrl Pts',(3.58298213321032,-5.74060345548233,59.9803205473475));
#76982=CARTESIAN_POINT('Ctrl Pts',(3.70113944056089,-5.66685589141029,59.9868787211686));
#76983=CARTESIAN_POINT('Ctrl Pts',(3.81694387682903,-5.5895057333956,59.9934368949897));
#76984=CARTESIAN_POINT('Ctrl Pts',(3.93017071637407,-5.50872463825845,59.9999950688108));
#76985=CARTESIAN_POINT('',(-3.9288823673735,-5.5096435767971,60.));
#76986=CARTESIAN_POINT('Origin',(0.,0.,60.));
#76987=CARTESIAN_POINT('',(-6.767,6.12589399508461E-12,59.6971797838098));
#76988=CARTESIAN_POINT('Ctrl Pts',(-6.76699999999828,4.8251696278534E-6,
59.6972856394408));
#76989=CARTESIAN_POINT('Ctrl Pts',(-6.76700012330983,-0.172931943421076,
59.7054271911032));
#76990=CARTESIAN_POINT('Ctrl Pts',(-6.76036657910632,-0.346010060321547,
59.7135687427657));
#76991=CARTESIAN_POINT('Ctrl Pts',(-6.74709290135145,-0.518677530391343,
59.7217102944281));
#76992=CARTESIAN_POINT('Ctrl Pts',(-6.73382589159082,-0.691258261448973,
59.7298477562053));
#76993=CARTESIAN_POINT('Ctrl Pts',(-6.71392541802703,-0.863428392473532,
59.7379852179824));
#76994=CARTESIAN_POINT('Ctrl Pts',(-6.68743708328302,-1.03463725871978,
59.7461226797596));
#76995=CARTESIAN_POINT('Ctrl Pts',(-6.66095324210352,-1.2058170805548,59.754258761072));
#76996=CARTESIAN_POINT('Ctrl Pts',(-6.62788381370195,-1.37603559988613,
59.7623948423845));
#76997=CARTESIAN_POINT('Ctrl Pts',(-6.58832614279841,-1.54474840544311,
59.770530923697));
#76998=CARTESIAN_POINT('Ctrl Pts',(-6.54877357131926,-1.71343946204029,
59.778665956178));
#76999=CARTESIAN_POINT('Ctrl Pts',(-6.50273450992899,-1.88062483587207,
59.786800988659));
#77000=CARTESIAN_POINT('Ctrl Pts',(-6.45035713046092,-2.04577171001849,
59.79493602114));
#77001=CARTESIAN_POINT('Ctrl Pts',(-6.39795895982377,-2.21098413911664,
59.8030742828173));
#77002=CARTESIAN_POINT('Ctrl Pts',(-6.33921755402332,-2.37415610228029,
59.8112125444945));
#77003=CARTESIAN_POINT('Ctrl Pts',(-6.27433070659144,-2.53477083467593,
59.8193508061717));
#77004=CARTESIAN_POINT('Ctrl Pts',(-6.21616619078512,-2.6787457465556,59.8266459371373));
#77005=CARTESIAN_POINT('Ctrl Pts',(-6.15306435077641,-2.8206659006872,59.8339410681029));
#77006=CARTESIAN_POINT('Ctrl Pts',(-6.08520006302406,-2.9601738450591,59.8412361990685));
#77007=CARTESIAN_POINT('Ctrl Pts',(-6.00156606930072,-3.13209941785128,
59.8502265083695));
#77008=CARTESIAN_POINT('Ctrl Pts',(-5.91066731636849,-3.30042675591245,
59.8592168176706));
#77009=CARTESIAN_POINT('Ctrl Pts',(-5.8128322377742,-3.46457362102366,59.8682071269716));
#77010=CARTESIAN_POINT('Ctrl Pts',(-5.71495502541899,-3.62879117780161,
59.877201308049));
#77011=CARTESIAN_POINT('Ctrl Pts',(-5.61013564670481,-3.78882445698208,
59.8861954891264));
#77012=CARTESIAN_POINT('Ctrl Pts',(-5.49874687476357,-3.94411863504103,
59.8951896702038));
#77013=CARTESIAN_POINT('Ctrl Pts',(-5.38731626860201,-4.09947113684972,
59.9041872292208));
#77014=CARTESIAN_POINT('Ctrl Pts',(-5.26931148017941,-4.25008078234281,
59.9131847882379));
#77015=CARTESIAN_POINT('Ctrl Pts',(-5.1451475288827,-4.39542329088249,59.9221823472549));
#77016=CARTESIAN_POINT('Ctrl Pts',(-5.02099117538933,-4.54075690566689,
59.9311793556961));
#77017=CARTESIAN_POINT('Ctrl Pts',(-4.89067657261529,-4.68082384439261,
59.9401763641372));
#77018=CARTESIAN_POINT('Ctrl Pts',(-4.75465817488559,-4.81513391714017,
59.9491733725783));
#77019=CARTESIAN_POINT('Ctrl Pts',(-4.61867977633247,-4.94940449308137,
59.9581677352528));
#77020=CARTESIAN_POINT('Ctrl Pts',(-4.47700110815396,-5.07792141547894,
59.9671620979274));
#77021=CARTESIAN_POINT('Ctrl Pts',(-4.3301132284925,-5.20023157450073,59.9761564606019));
#77022=CARTESIAN_POINT('Ctrl Pts',(-4.20031611473255,-5.30831064583825,
59.9841043070679));
#77023=CARTESIAN_POINT('Ctrl Pts',(-4.06645208522247,-5.41154372129691,
59.992052153534));
#77024=CARTESIAN_POINT('Ctrl Pts',(-3.9288823673735,-5.5096435767971,60.));
#77025=CARTESIAN_POINT('Ctrl Pts',(3.0990855038472,6.01564277861012,59.0457563580462));
#77026=CARTESIAN_POINT('Ctrl Pts',(2.93373232018322,6.10082796552483,59.0545058059455));
#77027=CARTESIAN_POINT('Ctrl Pts',(2.76486502144412,6.17919158180197,59.0632552538448));
#77028=CARTESIAN_POINT('Ctrl Pts',(2.59305716434331,6.25046746591388,59.0720047017441));
#77029=CARTESIAN_POINT('Ctrl Pts',(2.42125069459259,6.32174277447234,59.0807540789916));
#77030=CARTESIAN_POINT('Ctrl Pts',(2.24650397871033,6.38593035557835,59.089503456239));
#77031=CARTESIAN_POINT('Ctrl Pts',(2.06941053323744,6.44281220003548,59.0982528334864));
#77032=CARTESIAN_POINT('Ctrl Pts',(1.89231845896655,6.49969360406694,59.107002142989));
#77033=CARTESIAN_POINT('Ctrl Pts',(1.71287996431475,6.54926929700888,59.1157514524916));
#77034=CARTESIAN_POINT('Ctrl Pts',(1.53170449173474,6.59137090065486,59.1245007619942));
#77035=CARTESIAN_POINT('Ctrl Pts',(1.35053036178139,6.6334721923009,59.1332500066587));
#77036=CARTESIAN_POINT('Ctrl Pts',(1.16761955878813,6.6680994406246,59.1419992513233));
#77037=CARTESIAN_POINT('Ctrl Pts',(0.983593309310163,6.69513503985396,59.1507484959879));
#77038=CARTESIAN_POINT('Ctrl Pts',(0.7995683624596,6.72217044771219,59.1594976787211));
#77039=CARTESIAN_POINT('Ctrl Pts',(0.614428268438157,6.74161427235981,59.1682468614543));
#77040=CARTESIAN_POINT('Ctrl Pts',(0.428801816329773,6.75340047696805,59.1769960441875));
#77041=CARTESIAN_POINT('Ctrl Pts',(0.243176616522205,6.76518660206244,59.1857451678956));
#77042=CARTESIAN_POINT('Ctrl Pts',(0.0570653511647989,6.76931519233997,
59.1944942916037));
#77043=CARTESIAN_POINT('Ctrl Pts',(-0.128899900800774,6.76577222610794,
59.2032434153119));
#77044=CARTESIAN_POINT('Ctrl Pts',(-0.314863959942781,6.76222928260129,
59.2119924829011));
#77045=CARTESIAN_POINT('Ctrl Pts',(-0.500681721081455,6.75101488651271,
59.2207415504904));
#77046=CARTESIAN_POINT('Ctrl Pts',(-0.685722110174087,6.73216712415983,
59.2294906180797));
#77047=CARTESIAN_POINT('Ctrl Pts',(-0.870761373828302,6.71331947644136,
59.238239632456));
#77048=CARTESIAN_POINT('Ctrl Pts',(-1.05502298984402,6.68683858439987,59.2469886468324));
#77049=CARTESIAN_POINT('Ctrl Pts',(-1.23788117676109,6.65281438131417,59.2557376612087));
#77050=CARTESIAN_POINT('Ctrl Pts',(-1.43009641451833,6.61704912302368,59.2649343720963));
#77051=CARTESIAN_POINT('Ctrl Pts',(-1.62076048992727,6.57294837083157,59.2741310829838));
#77052=CARTESIAN_POINT('Ctrl Pts',(-1.80915798961154,6.52067760042043,59.2833277938713));
#77053=CARTESIAN_POINT('Ctrl Pts',(-1.98840443003037,6.47094578577401,59.2920777915778));
#77054=CARTESIAN_POINT('Ctrl Pts',(-2.1655989595222,6.41381888474466,59.3008277892843));
#77055=CARTESIAN_POINT('Ctrl Pts',(-2.34013966242353,6.34949095285223,59.3095777869908));
#77056=CARTESIAN_POINT('Ctrl Pts',(-2.51467682554033,6.28516432556677,59.3183276072424));
#77057=CARTESIAN_POINT('Ctrl Pts',(-2.68656000078849,6.21363705879657,59.327077427494));
#77058=CARTESIAN_POINT('Ctrl Pts',(-2.85520533840885,6.13515211510861,59.3358272477456));
#77059=CARTESIAN_POINT('Ctrl Pts',(-3.0238474799832,6.05666865881125,59.3445769021768));
#77060=CARTESIAN_POINT('Ctrl Pts',(-3.18925164684526,5.9712279103985,59.3533265566081));
#77061=CARTESIAN_POINT('Ctrl Pts',(-3.35085601829143,5.87912008251916,59.3620762110393));
#77062=CARTESIAN_POINT('Ctrl Pts',(-3.51245754191409,5.7870138777818,59.3708257112825));
#77063=CARTESIAN_POINT('Ctrl Pts',(-3.67025915510932,5.68824097060985,59.3795752115256));
#77064=CARTESIAN_POINT('Ctrl Pts',(-3.82372487928835,5.58313684656854,59.3883247117687));
#77065=CARTESIAN_POINT('Ctrl Pts',(-3.97718810300798,5.47803443501773,59.3970740694539));
#77066=CARTESIAN_POINT('Ctrl Pts',(-4.12631534263025,5.36660117496376,59.405823427139));
#77067=CARTESIAN_POINT('Ctrl Pts',(-4.27060009886224,5.24921554097352,59.4145727848241));
#77068=CARTESIAN_POINT('Ctrl Pts',(-4.41488269594212,5.13183166360292,59.4233220115793));
#77069=CARTESIAN_POINT('Ctrl Pts',(-4.55432273235087,5.00849577139472,59.4320712383345));
#77070=CARTESIAN_POINT('Ctrl Pts',(-4.68844662480206,4.87962675277343,59.4408204650896));
#77071=CARTESIAN_POINT('Ctrl Pts',(-4.82256868835157,4.75075949139883,59.4495695725411));
#77072=CARTESIAN_POINT('Ctrl Pts',(-4.95137454637862,4.61635945312526,59.4583186799926));
#77073=CARTESIAN_POINT('Ctrl Pts',(-5.07442674461078,4.47688309134591,59.4670677874441));
#77074=CARTESIAN_POINT('Ctrl Pts',(-5.19747742838537,4.33740844616353,59.4758167872165));
#77075=CARTESIAN_POINT('Ctrl Pts',(-5.31477440450924,4.19285781736032,59.4845657869889));
#77076=CARTESIAN_POINT('Ctrl Pts',(-5.42591931531149,4.04372211999411,59.4933147867612));
#77077=CARTESIAN_POINT('Ctrl Pts',(-5.53707636462981,3.89457013500802,59.5020647420418));
#77078=CARTESIAN_POINT('Ctrl Pts',(-5.64207983273473,3.74083230916417,59.5108146973224));
#77079=CARTESIAN_POINT('Ctrl Pts',(-5.74057303468752,3.58303087251819,59.519564652603));
#77080=CARTESIAN_POINT('Ctrl Pts',(-5.83906243363768,3.42523552887426,59.5283142700318));
#77081=CARTESIAN_POINT('Ctrl Pts',(-5.93104191768426,3.26337713156991,59.5370638874606));
#77082=CARTESIAN_POINT('Ctrl Pts',(-6.01619906699655,3.09800545291158,59.5458135048894));
#77083=CARTESIAN_POINT('Ctrl Pts',(-6.10135338095373,2.93263928039616,59.5545628309948));
#77084=CARTESIAN_POINT('Ctrl Pts',(-6.17968568352821,2.76376031540263,59.5633121571001));
#77085=CARTESIAN_POINT('Ctrl Pts',(-6.25092992694862,2.59194213831601,59.5720614832055));
#77086=CARTESIAN_POINT('Ctrl Pts',(-6.32217217691089,2.42012876880859,59.5808105644993));
#77087=CARTESIAN_POINT('Ctrl Pts',(-6.38632665483844,2.2453766164769,59.5895596457932));
#77088=CARTESIAN_POINT('Ctrl Pts',(-6.44317547869351,2.06827917621455,59.598308727087));
#77089=CARTESIAN_POINT('Ctrl Pts',(-6.50002944235937,1.89116572423421,59.6070585994019));
#77090=CARTESIAN_POINT('Ctrl Pts',(-6.54957634250399,1.71170683289195,59.6158084717169));
#77091=CARTESIAN_POINT('Ctrl Pts',(-6.59164787708396,1.5305120922536,59.6245583440318));
#77092=CARTESIAN_POINT('Ctrl Pts',(-6.63371649075008,1.34932993148032,59.6333076088666));
#77093=CARTESIAN_POINT('Ctrl Pts',(-6.66831071257123,1.16641244174011,59.6420568737014));
#77094=CARTESIAN_POINT('Ctrl Pts',(-6.69531304840331,0.982380875160149,
59.6508061385362));
#77095=CARTESIAN_POINT('Ctrl Pts',(-6.72231677033042,0.798339861795978,
59.6595558524919));
#77096=CARTESIAN_POINT('Ctrl Pts',(-6.74172778477889,0.61318494073029,59.6683055664475));
#77097=CARTESIAN_POINT('Ctrl Pts',(-6.75348015835517,0.427545027690687,
59.6770552804032));
#77098=CARTESIAN_POINT('Ctrl Pts',(-6.76249038365208,0.285219953548977,
59.6837634482054));
#77099=CARTESIAN_POINT('Ctrl Pts',(-6.76699999999987,0.142609995761487,
59.6904716160076));
#77100=CARTESIAN_POINT('Ctrl Pts',(-6.767,6.12589398735536E-12,59.6971797838098));
#77101=CARTESIAN_POINT('Ctrl Pts',(-2.92312393079455,6.09699903205172,-60.6636842274549));
#77102=CARTESIAN_POINT('Ctrl Pts',(-3.93696870157765,5.61092651139488,-60.6107538653005));
#77103=CARTESIAN_POINT('Ctrl Pts',(-5.71385275345024,4.12729922236996,-60.5049022361689));
#77104=CARTESIAN_POINT('Ctrl Pts',(-6.99683237773153,0.880191322515334,
-60.3461293400603));
#77105=CARTESIAN_POINT('Ctrl Pts',(-6.55662514285608,-2.55525940431229,
-60.1873655391287));
#77106=CARTESIAN_POINT('Ctrl Pts',(-3.87957147477697,-6.36386071307339,
-59.9756804712201));
#77107=CARTESIAN_POINT('Ctrl Pts',(2.33603082002131,-7.64687216116862,-59.7110741363342));
#77108=CARTESIAN_POINT('Ctrl Pts',(7.70057569811667,-2.15972995654168,-59.3935465344711));
#77109=CARTESIAN_POINT('Ctrl Pts',(6.26959392394697,4.02615150262351,-59.1289401995852));
#77110=CARTESIAN_POINT('Ctrl Pts',(2.40708136811262,6.61358385766357,-58.9172551316766));
#77111=CARTESIAN_POINT('Ctrl Pts',(-1.05041112263128,6.97500520632018,-58.758491330745));
#77112=CARTESIAN_POINT('Ctrl Pts',(-4.24145056983912,5.61648152126252,-58.5997275298136));
#77113=CARTESIAN_POINT('Ctrl Pts',(-7.18314404472123,1.99726048125854,-58.3880424619048));
#77114=CARTESIAN_POINT('Ctrl Pts',(-6.80569859354872,-3.04864719331499,
-58.1763573939962));
#77115=CARTESIAN_POINT('Ctrl Pts',(-3.35804436576745,-6.17750544855752,
-57.9646723260874));
#77116=CARTESIAN_POINT('Ctrl Pts',(1.11993342530363,-7.36667282618036,-57.7529872581789));
#77117=CARTESIAN_POINT('Ctrl Pts',(6.71700196989707,-4.34658677302633,-57.4883809232929));
#77118=CARTESIAN_POINT('Ctrl Pts',(7.27905940725944,3.30630186467041,-57.17085332143));
#77119=CARTESIAN_POINT('Ctrl Pts',(2.20588712983283,7.11743132022739,-56.9062469865439));
#77120=CARTESIAN_POINT('Ctrl Pts',(-2.41771698918159,6.61000287796941,-56.6945619186354));
#77121=CARTESIAN_POINT('Ctrl Pts',(-5.29460658627333,4.66012616950757,-56.5357981177038));
#77122=CARTESIAN_POINT('Ctrl Pts',(-6.86186273884577,1.56597944961906,-56.3770343167724));
#77123=CARTESIAN_POINT('Ctrl Pts',(-6.78168957233196,-3.09729046827898,
-56.1653492488635));
#77124=CARTESIAN_POINT('Ctrl Pts',(-3.24397994606998,-6.7148219785863,-55.953664180955));
#77125=CARTESIAN_POINT('Ctrl Pts',(1.40863712635378,-6.88867756320579,-55.7419791130463));
#77126=CARTESIAN_POINT('Ctrl Pts',(5.60038102276455,-4.91503719715207,-55.5302940451375));
#77127=CARTESIAN_POINT('Ctrl Pts',(7.93799707766255,0.999673053673553,-55.2656877102517));
#77128=CARTESIAN_POINT('Ctrl Pts',(3.44015086769524,7.21676185626268,-54.9481601083886));
#77129=CARTESIAN_POINT('Ctrl Pts',(-2.8953477620337,6.86590885072102,-54.6835537735029));
#77130=CARTESIAN_POINT('Ctrl Pts',(-6.1060944895583,3.50044640710944,-54.4718687055941));
#77131=CARTESIAN_POINT('Ctrl Pts',(-7.05161310117804,0.156122379568802,
-54.3131049046626));
#77132=CARTESIAN_POINT('Ctrl Pts',(-6.25832624994688,-3.22037419800652,
-54.1543411037311));
#77133=CARTESIAN_POINT('Ctrl Pts',(-3.19421094982843,-6.73658192074147,
-53.9426560358224));
#77134=CARTESIAN_POINT('Ctrl Pts',(1.84186590314193,-7.22632474479682,-53.7309709679136));
#77135=CARTESIAN_POINT('Ctrl Pts',(5.5134977225823,-4.36342534981377,-53.5192859000051));
#77136=CARTESIAN_POINT('Ctrl Pts',(7.44970212626647,-0.154258536351977,
-53.3076008320962));
#77137=CARTESIAN_POINT('Ctrl Pts',(5.42959217157294,5.87628054081612,-53.0429944972106));
#77138=CARTESIAN_POINT('Ctrl Pts',(-2.01498652368906,7.73667364412597,-52.7254668953474));
#77139=CARTESIAN_POINT('Ctrl Pts',(-6.63630755816859,3.38868188023253,-52.4608605604616));
#77140=CARTESIAN_POINT('Ctrl Pts',(-6.92573590590944,-1.25367347471575,
-52.2491754925529));
#77141=CARTESIAN_POINT('Ctrl Pts',(-5.49566665660641,-4.42122941071933,
-52.0904116916214));
#77142=CARTESIAN_POINT('Ctrl Pts',(-2.71453384249522,-6.49374802783983,
-51.9316478906898));
#77143=CARTESIAN_POINT('Ctrl Pts',(1.8939556401918,-7.21092584926551,-51.7199628227812));
#77144=CARTESIAN_POINT('Ctrl Pts',(6.06237564429645,-4.3427918283758,-51.5082777548724));
#77145=CARTESIAN_POINT('Ctrl Pts',(7.0280343009548,0.211829618358026,-51.2965926869638));
#77146=CARTESIAN_POINT('Ctrl Pts',(5.7990414182339,4.67899306415061,-51.084907619055));
#77147=CARTESIAN_POINT('Ctrl Pts',(0.370283363009991,7.9921232707625,-50.8203012841692));
#77148=CARTESIAN_POINT('Ctrl Pts',(-6.5234529958798,4.62178004425476,-50.5027736823062));
#77149=CARTESIAN_POINT('Ctrl Pts',(-7.25943048449507,-1.68059868276578,
-50.2381673474203));
#77150=CARTESIAN_POINT('Ctrl Pts',(-4.49156266215061,-5.41879874803109,
-50.0264822795117));
#77151=CARTESIAN_POINT('Ctrl Pts',(-1.3577735496372,-6.92142127677832,-49.86771847858));
#77152=CARTESIAN_POINT('Ctrl Pts',(2.10458729961294,-6.71626158881723,-49.7089546776486));
#77153=CARTESIAN_POINT('Ctrl Pts',(6.09231344885727,-4.29746860506485,-49.4972696097399));
#77154=CARTESIAN_POINT('Ctrl Pts',(7.43469033521331,0.58104985727342,-49.2855845418312));
#77155=CARTESIAN_POINT('Ctrl Pts',(5.24069490095294,4.68756385319076,-49.0738994739225));
#77156=CARTESIAN_POINT('Ctrl Pts',(1.42390403077878,7.31398350940805,-48.8622144060138));
#77157=CARTESIAN_POINT('Ctrl Pts',(-4.86299012607282,6.35314655723462,-48.5976080711279));
#77158=CARTESIAN_POINT('Ctrl Pts',(-7.96710335872743,-0.664495175513357,
-48.280080469265));
#77159=CARTESIAN_POINT('Ctrl Pts',(-4.47196403319157,-5.96030876528817,
-48.015474134379));
#77160=CARTESIAN_POINT('Ctrl Pts',(0.0528141213109033,-7.03809105427595,
-47.8037890664705));
#77161=CARTESIAN_POINT('Ctrl Pts',(3.41802194588758,-6.16982556318776,-47.6450252655387));
#77162=CARTESIAN_POINT('Ctrl Pts',(5.93494174663343,-3.7833746702093,-47.4862614646075));
#77163=CARTESIAN_POINT('Ctrl Pts',(7.42841097714051,0.635003878211527,-47.2745763966986));
#77164=CARTESIAN_POINT('Ctrl Pts',(5.31407594064479,5.23190560065949,-47.06289132879));
#77165=CARTESIAN_POINT('Ctrl Pts',(0.991198393882503,6.96101024755598,-46.8512062608813));
#77166=CARTESIAN_POINT('Ctrl Pts',(-3.62020483763898,6.51275474728599,-46.6395211929726));
#77167=CARTESIAN_POINT('Ctrl Pts',(-7.81155787921683,1.7293662549123,-46.3749148580867));
#77168=CARTESIAN_POINT('Ctrl Pts',(-5.66768900817763,-5.63858059031783,
-46.0573872562237));
#77169=CARTESIAN_POINT('Ctrl Pts',(0.416498227822971,-7.43977634865123,
-45.7927809213378));
#77170=CARTESIAN_POINT('Ctrl Pts',(4.5723780380445,-5.35078256864332,-45.5810958534292));
#77171=CARTESIAN_POINT('Ctrl Pts',(6.58797943991901,-2.51955321474632,-45.4223320524976));
#77172=CARTESIAN_POINT('Ctrl Pts',(6.97697150051971,0.926998442312364,-45.2635682515661));
#77173=CARTESIAN_POINT('Ctrl Pts',(5.27452955658915,5.26914201054712,-45.0518831836575));
#77174=CARTESIAN_POINT('Ctrl Pts',(0.696828925394616,7.42473358214861,-44.8401981157487));
#77175=CARTESIAN_POINT('Ctrl Pts',(-3.72397799269562,5.96406956972614,-44.6285130478401));
#77176=CARTESIAN_POINT('Ctrl Pts',(-6.96348714803389,2.65173607358044,-44.4168279799313));
#77177=CARTESIAN_POINT('Ctrl Pts',(-7.09013851937479,-3.70689626507969,
-44.1522216450455));
#77178=CARTESIAN_POINT('Ctrl Pts',(-0.705509311452106,-7.96357623046209,
-43.8346940431824));
#77179=CARTESIAN_POINT('Ctrl Pts',(5.10928337137563,-5.42392536109363,-43.5700877082966));
#77180=CARTESIAN_POINT('Ctrl Pts',(6.94377013876049,-1.14959613767053,-43.3584026403879));
#77181=CARTESIAN_POINT('Ctrl Pts',(6.66280533293569,2.31444304275086,-43.1996388394564));
#77182=CARTESIAN_POINT('Ctrl Pts',(4.74111534605175,5.20185377596739,-43.0408750385248));
#77183=CARTESIAN_POINT('Ctrl Pts',(0.642595000024069,7.4277581568458,-42.8291899706162));
#77184=CARTESIAN_POINT('Ctrl Pts',(-4.24779877571826,6.12931031015385,-42.6175049027075));
#77185=CARTESIAN_POINT('Ctrl Pts',(-6.68957363577079,2.16511951037697,-42.4058198347988));
#77186=CARTESIAN_POINT('Ctrl Pts',(-7.03521870122052,-2.45510799981555,
-42.1941347668902));
#77187=CARTESIAN_POINT('Ctrl Pts',(-3.03766568752031,-7.40160329353348,
-41.9295284320042));
#77188=CARTESIAN_POINT('Ctrl Pts',(4.58812924676499,-6.54716425499665,-41.6120008301413));
#77189=CARTESIAN_POINT('Ctrl Pts',(7.40165051643521,-0.859832846711758,
-41.3473944952554));
#77190=CARTESIAN_POINT('Ctrl Pts',(6.05287482910103,3.59168780978024,-41.1357094273467));
#77191=CARTESIAN_POINT('Ctrl Pts',(3.6073452975506,6.06107922790767,-40.9769456264152));
#77192=CARTESIAN_POINT('Ctrl Pts',(0.277812056168763,7.03280014592772,-40.8181818254836));
#77193=CARTESIAN_POINT('Ctrl Pts',(-4.29124033042278,6.09670205908065,-40.606496757575));
#77194=CARTESIAN_POINT('Ctrl Pts',(-7.19674686893622,1.95424507716112,-40.3948116896662));
#77195=CARTESIAN_POINT('Ctrl Pts',(-6.51230720008338,-2.65103618503351,
-40.1831266217576));
#77196=CARTESIAN_POINT('Ctrl Pts',(-3.80169893709803,-6.40850549320421,
-39.9714415538489));
#77197=CARTESIAN_POINT('Ctrl Pts',(2.44194806796726,-7.61892602519113,-39.706835218963));
#77198=CARTESIAN_POINT('Ctrl Pts',(7.72619583474277,-2.05479626487146,-39.3893076171001));
#77199=CARTESIAN_POINT('Ctrl Pts',(6.21661117867084,4.10822204182721,-39.1247012822141));
#77200=CARTESIAN_POINT('Ctrl Pts',(2.31824809444377,6.64554292682674,-38.9130162143055));
#77201=CARTESIAN_POINT('Ctrl Pts',(-1.14289969095182,6.96012943839095,-38.7542524133739));
#77202=CARTESIAN_POINT('Ctrl Pts',(-4.31601150658888,5.55963147214867,-38.5954886124424));
#77203=CARTESIAN_POINT('Ctrl Pts',(-7.20898655868447,1.90132384599566,-38.3838035445337));
#77204=CARTESIAN_POINT('Ctrl Pts',(-6.76455528773798,-3.13895381875682,
-38.172118476625));
#77205=CARTESIAN_POINT('Ctrl Pts',(-3.27546111720417,-6.2216952988955,-37.9604334087163));
#77206=CARTESIAN_POINT('Ctrl Pts',(1.217916036499,-7.35109093895588,-37.7487483408077));
#77207=CARTESIAN_POINT('Ctrl Pts',(6.77429797690968,-4.25676297954459,-37.4841420059218));
#77208=CARTESIAN_POINT('Ctrl Pts',(7.23437967918326,3.40294584505053,-37.1666144040588));
#77209=CARTESIAN_POINT('Ctrl Pts',(2.11091462183016,7.14617256656133,-36.9020080691729));
#77210=CARTESIAN_POINT('Ctrl Pts',(-2.50552638293833,6.5772222529035,-36.6903230012642));
#77211=CARTESIAN_POINT('Ctrl Pts',(-5.35619325413247,4.58920639404244,-36.5315592003327));
#77212=CARTESIAN_POINT('Ctrl Pts',(-6.88210809687881,1.47446450414678,-36.3727953994011));
#77213=CARTESIAN_POINT('Ctrl Pts',(-6.73984272261571,-3.18732484146961,
-36.1611103314925));
#77214=CARTESIAN_POINT('Ctrl Pts',(-3.15427412249773,-6.75742510704284,
-35.9494252635838));
#77215=CARTESIAN_POINT('Ctrl Pts',(1.50024575056515,-6.86930859770662,-35.7377401956751));
#77216=CARTESIAN_POINT('Ctrl Pts',(5.66533577993045,-4.8400235500874,-35.5260551277664));
#77217=CARTESIAN_POINT('Ctrl Pts',(7.92398104023708,1.1052911914726,-35.2614487928805));
#77218=CARTESIAN_POINT('Ctrl Pts',(3.34374339023025,7.26193293188651,-34.9439211910175));
#77219=CARTESIAN_POINT('Ctrl Pts',(-2.98652130102637,6.82674398306001,-34.6793148561316));
#77220=CARTESIAN_POINT('Ctrl Pts',(-6.15216696733666,3.41882386584927,-34.467629788223));
#77221=CARTESIAN_POINT('Ctrl Pts',(-7.05306685073663,0.0622053194999262,
-34.3088659872914));
#77222=CARTESIAN_POINT('Ctrl Pts',(-6.21488702937856,-3.3034280139237,-34.15010218636));
#77223=CARTESIAN_POINT('Ctrl Pts',(-3.10421963643972,-6.77852048897011,
-33.9384171184512));
#77224=CARTESIAN_POINT('Ctrl Pts',(1.93793235897052,-7.20115667717395,-33.7267320505425));
#77225=CARTESIAN_POINT('Ctrl Pts',(5.57111465182142,-4.28961763550966,-33.5150469826339));
#77226=CARTESIAN_POINT('Ctrl Pts',(7.45109575912954,-0.0550404673175772,
-33.3033619147252));
#77227=CARTESIAN_POINT('Ctrl Pts',(5.35085890249345,5.94806297458176,-33.0387555798393));
#77228=CARTESIAN_POINT('Ctrl Pts',(-2.11783372013389,7.70915495374104,-32.7212279779763));
#77229=CARTESIAN_POINT('Ctrl Pts',(-6.68084470050438,3.30000863324214,-32.4566216430904));
#77230=CARTESIAN_POINT('Ctrl Pts',(-6.90842719020237,-1.34578927673002,
-32.2449365751818));
#77231=CARTESIAN_POINT('Ctrl Pts',(-5.43630380155726,-4.49402074760545,
-32.0861727742502));
#77232=CARTESIAN_POINT('Ctrl Pts',(-2.62781877401236,-6.5293204793502,-31.9274089733187));
#77233=CARTESIAN_POINT('Ctrl Pts',(1.9898124172897,-7.1850654913261,-31.71572390541));
#77234=CARTESIAN_POINT('Ctrl Pts',(6.11966913731047,-4.26167677880455,-31.5040388375013));
#77235=CARTESIAN_POINT('Ctrl Pts',(7.02459028872639,0.305400062451879,-31.2923537695926));
#77236=CARTESIAN_POINT('Ctrl Pts',(5.73621913850456,4.755801452943,-31.0806687016839));
#77237=CARTESIAN_POINT('Ctrl Pts',(0.263822956621364,7.99634551476757,-30.8160623667981));
#77238=CARTESIAN_POINT('Ctrl Pts',(-6.58442076827012,4.53450029367066,-30.498534764935));
#77239=CARTESIAN_POINT('Ctrl Pts',(-7.23640700599555,-1.77712029286393,
-30.2339284300492));
#77240=CARTESIAN_POINT('Ctrl Pts',(-4.41900465028644,-5.47813042199944,
-30.0222433621405));
#77241=CARTESIAN_POINT('Ctrl Pts',(-1.26548364847116,-6.93888842958194,
-29.863479561209));
#77242=CARTESIAN_POINT('Ctrl Pts',(2.19383817480087,-6.68764020368173,-29.7047157602774));
#77243=CARTESIAN_POINT('Ctrl Pts',(6.14900073797299,-4.21595890575949,-29.4930306923688));
#77244=CARTESIAN_POINT('Ctrl Pts',(7.42629352233101,0.680002821564867,-29.28134562446));
#77245=CARTESIAN_POINT('Ctrl Pts',(5.17780799600353,4.75693622819738,-29.0696605565514));
#77246=CARTESIAN_POINT('Ctrl Pts',(1.32638068810365,7.33229648438925,-28.8579754886427));
#77247=CARTESIAN_POINT('Ctrl Pts',(-4.9471609732356,6.28782493783651,-28.5933691537568));
#77248=CARTESIAN_POINT('Ctrl Pts',(-7.95754813273417,-0.770530649711755,
-28.2758415518938));
#77249=CARTESIAN_POINT('Ctrl Pts',(-4.39219670953444,-6.0193314376669,-28.0112352170079));
#77250=CARTESIAN_POINT('Ctrl Pts',(0.146532586535858,-7.03676368942229,
-27.7995501490993));
#77251=CARTESIAN_POINT('Ctrl Pts',(3.4998797126913,-6.12376220141065,-27.6407863481677));
#77252=CARTESIAN_POINT('Ctrl Pts',(5.9847970280502,-3.7040062046594,-27.4820225472362));
#77253=CARTESIAN_POINT('Ctrl Pts',(7.41929623919157,0.733868439001849,-27.2703374793275));
#77254=CARTESIAN_POINT('Ctrl Pts',(5.24393377056136,5.30220689214575,-27.0586524114188));
#77255=CARTESIAN_POINT('Ctrl Pts',(0.898413807847284,6.97359237068558,-26.8469673435102));
#77256=CARTESIAN_POINT('Ctrl Pts',(-3.70661131342256,6.46396859800302,-26.6352822756014));
#77257=CARTESIAN_POINT('Ctrl Pts',(-7.83389444007708,1.62518984912946,-26.3706759407156));
#77258=CARTESIAN_POINT('Ctrl Pts',(-5.59209997235955,-5.71355473116891,
-26.0531483388526));
#77259=CARTESIAN_POINT('Ctrl Pts',(0.515533510984028,-7.43357034612457,
-25.7885420039666));
#77260=CARTESIAN_POINT('Ctrl Pts',(4.64322661531511,-5.28941978089454,-25.576856936058));
#77261=CARTESIAN_POINT('Ctrl Pts',(6.62094706514696,-2.43160059698462,-25.4180931351265));
#77262=CARTESIAN_POINT('Ctrl Pts',(6.96400842882034,1.01982549214703,-25.259329334195));
#77263=CARTESIAN_POINT('Ctrl Pts',(5.20389503224099,5.3389133785877,-25.0476442662863));
#77264=CARTESIAN_POINT('Ctrl Pts',(0.597895242178444,7.43335459913841,-24.8359591983776));
#77265=CARTESIAN_POINT('Ctrl Pts',(-3.80306866895886,5.91395017072331,-24.6242741304689));
#77266=CARTESIAN_POINT('Ctrl Pts',(-6.99818169797508,2.55877126505823,-24.4125890625602));
#77267=CARTESIAN_POINT('Ctrl Pts',(-7.04014674245482,-3.8009838185247,-24.1479827276743));
#77268=CARTESIAN_POINT('Ctrl Pts',(-0.599399329136246,-7.97226506152157,
-23.8304551258113));
#77269=CARTESIAN_POINT('Ctrl Pts',(5.18105835187421,-5.35540635677676,-23.5658487909255));
#77270=CARTESIAN_POINT('Ctrl Pts',(6.95846310331139,-1.05702708552953,-23.3541637230168));
#77271=CARTESIAN_POINT('Ctrl Pts',(6.63139413153894,2.40296345684338,-23.1953999220853));
#77272=CARTESIAN_POINT('Ctrl Pts',(4.6714241668463,5.26452786909883,-23.0366361211537));
#77273=CARTESIAN_POINT('Ctrl Pts',(0.543625848766956,7.43565669643223,-22.824951053245));
#77274=CARTESIAN_POINT('Ctrl Pts',(-4.32904344307952,6.07220076949717,-22.6132659853364));
#77275=CARTESIAN_POINT('Ctrl Pts',(-6.71781241570783,2.07584543499186,-22.4015809174276));
#77276=CARTESIAN_POINT('Ctrl Pts',(-7.00190130512566,-2.54857520549042,
-22.189895849519));
#77277=CARTESIAN_POINT('Ctrl Pts',(-2.93883245980067,-7.44139825014128,
-21.9252895146331));
#77278=CARTESIAN_POINT('Ctrl Pts',(4.67490811358557,-6.48548563304697,-21.6077619127701));
#77279=CARTESIAN_POINT('Ctrl Pts',(7.41244423136772,-0.761192097038367,
-21.3431555778842));
#77280=CARTESIAN_POINT('Ctrl Pts',(6.00450920570145,3.67197279651351,-21.1314705099755));
#77281=CARTESIAN_POINT('Ctrl Pts',(3.52631272330616,6.10857921944075,-20.972706709044));
#77282=CARTESIAN_POINT('Ctrl Pts',(0.184134731243384,7.03587605290655,-20.8139429081125));
#77283=CARTESIAN_POINT('Ctrl Pts',(-4.37204691618338,6.03901691778854,-20.6022578402038));
#77284=CARTESIAN_POINT('Ctrl Pts',(-7.22213255654739,1.85823589805217,-20.3905727722951));
#77285=CARTESIAN_POINT('Ctrl Pts',(-6.47642708112463,-2.73752263652566,
-20.1788877043864));
#77286=CARTESIAN_POINT('Ctrl Pts',(-3.71602260761794,-6.45856280022372,
-19.9672026364777));
#77287=CARTESIAN_POINT('Ctrl Pts',(2.54318941299879,-7.58573211717858,-19.7025963015919));
#77288=CARTESIAN_POINT('Ctrl Pts',(7.75287357221985,-1.95172773206238,-19.3850686997289));
#77289=CARTESIAN_POINT('Ctrl Pts',(6.16135257878985,4.19064163244365,-19.120462364843));
#77290=CARTESIAN_POINT('Ctrl Pts',(2.2295467787481,6.67582475661716,-18.9087772969343));
#77291=CARTESIAN_POINT('Ctrl Pts',(-1.23548331867775,6.94429279855072,-18.7500134960028));
#77292=CARTESIAN_POINT('Ctrl Pts',(-4.38966396424912,5.50166408571866,-18.5912496950713));
#77293=CARTESIAN_POINT('Ctrl Pts',(-7.23366643236317,1.80515636883538,-18.3795646271625));
#77294=CARTESIAN_POINT('Ctrl Pts',(-6.72215541861812,-3.22875608324548,
-18.1678795592539));
#77295=CARTESIAN_POINT('Ctrl Pts',(-3.19231911765856,-6.26476149375589,
-17.9561944913452));
#77296=CARTESIAN_POINT('Ctrl Pts',(1.31569927410357,-7.33422067331522,-17.7445094234365));
#77297=CARTESIAN_POINT('Ctrl Pts',(6.83038273611529,-4.1661752030084,-17.4799030885506));
#77298=CARTESIAN_POINT('Ctrl Pts',(7.18842268592018,3.49898114534428,-17.1623754866876));
#77299=CARTESIAN_POINT('Ctrl Pts',(2.01556502657803,7.17364903764925,-16.8977691518017));
#77300=CARTESIAN_POINT('Ctrl Pts',(-2.59289018175187,6.54327406770214,-16.686084083893));
#77301=CARTESIAN_POINT('Ctrl Pts',(-5.41683075771138,4.51747341387265,-16.5273202829615));
#77302=CARTESIAN_POINT('Ctrl Pts',(-6.90113265742603,1.38268777231947,-16.36855648203));
#77303=CARTESIAN_POINT('Ctrl Pts',(-6.69680090920865,-3.27679373062556,
-16.1568714141213));
#77304=CARTESIAN_POINT('Ctrl Pts',(-3.06400879141773,-6.79883000546907,
-15.9451863462126));
#77305=CARTESIAN_POINT('Ctrl Pts',(1.59158827167064,-6.84872139133249,-15.7335012783039));
#77306=CARTESIAN_POINT('Ctrl Pts',(5.72928589328394,-4.76415161574215,-15.5218162103953));
#77307=CARTESIAN_POINT('Ctrl Pts',(7.90855975212633,1.21071333974291,-15.2572098755094));
#77308=CARTESIAN_POINT('Ctrl Pts',(3.24674295129907,7.30581617446789,-14.9396822736464));
#77309=CARTESIAN_POINT('Ctrl Pts',(-3.07716522097081,6.78636847618651,-14.6750759387605));
#77310=CARTESIAN_POINT('Ctrl Pts',(-6.19714842559212,3.33659503249492,-14.4633908708518));
#77311=CARTESIAN_POINT('Ctrl Pts',(-7.05326982105232,-0.0317227704806144,
-14.3046270699203));
#77312=CARTESIAN_POINT('Ctrl Pts',(-6.1703456687824,-3.3858960053215,-14.1458632689888));
#77313=CARTESIAN_POINT('Ctrl Pts',(-3.01367782577689,-6.81925696341364,
-13.9341782010801));
#77314=CARTESIAN_POINT('Ctrl Pts',(2.03365514493514,-7.17471156692939,-13.7224931331714));
#77315=CARTESIAN_POINT('Ctrl Pts',(5.62774360737277,-4.21504920639009,-13.5108080652627));
#77316=CARTESIAN_POINT('Ctrl Pts',(7.45116802533417,0.0441873624320021,
-13.299122997354));
#77317=CARTESIAN_POINT('Ctrl Pts',(5.27117671963474,6.01879058734929,-13.0345166624682));
#77318=CARTESIAN_POINT('Ctrl Pts',(-2.22030534292114,7.68026913272724,-12.7169890606051));
#77319=CARTESIAN_POINT('Ctrl Pts',(-6.72419707133592,3.21075016741692,-12.4523827257193));
#77320=CARTESIAN_POINT('Ctrl Pts',(-6.88989334381324,-1.43766641839012,
-12.2406976578106));
#77321=CARTESIAN_POINT('Ctrl Pts',(-5.37597688010952,-4.56601512122575,
-12.081933856879));
#77322=CARTESIAN_POINT('Ctrl Pts',(-2.54063769187477,-6.56373503043344,
-11.9231700559475));
#77323=CARTESIAN_POINT('Ctrl Pts',(2.08531632387576,-7.15793094406632,-11.7114849880388));
#77324=CARTESIAN_POINT('Ctrl Pts',(6.17587737688397,-4.17980596952113,-11.4997999201302));
#77325=CARTESIAN_POINT('Ctrl Pts',(7.01990054562355,0.398916347332255,-11.2881148522215));
#77326=CARTESIAN_POINT('Ctrl Pts',(5.67237960581295,4.83176645465385,-11.0764297843128));
#77327=CARTESIAN_POINT('Ctrl Pts',(0.157315764243724,7.9991496982057,-10.8118234494269));
#77328=CARTESIAN_POINT('Ctrl Pts',(-6.64422086882444,4.44641640123863,-10.4942958475639));
#77329=CARTESIAN_POINT('Ctrl Pts',(-7.21210023334577,-1.87332675097102,
-10.229689512678));
#77330=CARTESIAN_POINT('Ctrl Pts',(-4.34566297840795,-5.53649061209207,
-10.0180044447693));
#77331=CARTESIAN_POINT('Ctrl Pts',(-1.17296932823043,-6.95512504975756,
-9.85924064383781));
#77332=CARTESIAN_POINT('Ctrl Pts',(2.28269999784015,-6.65783284192195,-9.70047684290628));
#77333=CARTESIAN_POINT('Ctrl Pts',(6.20459757202321,-4.13370155428382,-9.48879177499759));
#77334=CARTESIAN_POINT('Ctrl Pts',(7.41657974109306,0.778835195121069,-9.27710670708891));
#77335=CARTESIAN_POINT('Ctrl Pts',(5.11400286593109,4.82546501488344,-9.06542163918021));
#77336=CARTESIAN_POINT('Ctrl Pts',(1.2286221269591,7.3493091603161,-8.85373657127153));
#77337=CARTESIAN_POINT('Ctrl Pts',(-5.03045449789125,6.22138824448616,-8.58913023638566));
#77338=CARTESIAN_POINT('Ctrl Pts',(-7.94658172644672,-0.876429479098477,
-8.27160263452264));
#77339=CARTESIAN_POINT('Ctrl Pts',(-4.31165047994483,-6.07728665034922,
-8.00699629963675));
#77340=CARTESIAN_POINT('Ctrl Pts',(0.240225065879416,-7.03418843488154,
-7.7953112317281));
#77341=CARTESIAN_POINT('Ctrl Pts',(3.58111681579404,-6.07661286033268,-7.63654743079656));
#77342=CARTESIAN_POINT('Ctrl Pts',(6.03359097405248,-3.62398087590763,-7.47778362986505));
#77343=CARTESIAN_POINT('Ctrl Pts',(7.40886577377939,0.832602856610925,-7.26609856195636));
#77344=CARTESIAN_POINT('Ctrl Pts',(5.17286164869607,5.37156789777357,-7.05441349404767));
#77345=CARTESIAN_POINT('Ctrl Pts',(0.805469898391115,6.98493780685348,-6.84272842613898));
#77346=CARTESIAN_POINT('Ctrl Pts',(-3.79236046403696,6.41403613766814,-6.63104335823029));
#77347=CARTESIAN_POINT('Ctrl Pts',(-7.85484174916773,1.52072523455442,-6.36643702334443));
#77348=CARTESIAN_POINT('Ctrl Pts',(-5.51551924154778,-5.78751563845428,
-6.04890942148139));
#77349=CARTESIAN_POINT('Ctrl Pts',(0.614477370300083,-7.42604608457251,
-5.78430308659554));
#77350=CARTESIAN_POINT('Ctrl Pts',(4.71325176917766,-5.22711897523551,-5.57261801868683));
#77351=CARTESIAN_POINT('Ctrl Pts',(6.65274054142896,-2.3432167619946,-5.41385421775533));
#77352=CARTESIAN_POINT('Ctrl Pts',(6.94981036898054,1.11247168640414,-5.25509041682382));
#77353=CARTESIAN_POINT('Ctrl Pts',(5.13233765828268,5.40773795397972,-5.04340534891511));
#77354=CARTESIAN_POINT('Ctrl Pts',(0.498855525711081,7.44065739044357,-4.83172028100644));
#77355=CARTESIAN_POINT('Ctrl Pts',(-3.88148491049595,5.86278200618377,-4.62003521309773));
#77356=CARTESIAN_POINT('Ctrl Pts',(-7.03163520948331,2.46535267365039,-4.40835014518906));
#77357=CARTESIAN_POINT('Ctrl Pts',(-6.98890645635959,-3.89439728104558,
-4.14374381030317));
#77358=CARTESIAN_POINT('Ctrl Pts',(-0.493183084648223,-7.9795401550328,
-3.82621620844016));
#77359=CARTESIAN_POINT('Ctrl Pts',(5.25191458918605,-5.28593754317327,-3.56160987355429));
#77360=CARTESIAN_POINT('Ctrl Pts',(6.97192198309366,-0.964270705111193,
-3.3499248056456));
#77361=CARTESIAN_POINT('Ctrl Pts',(6.59880710436197,2.4910580020008,-3.19116100471409));
#77362=CARTESIAN_POINT('Ctrl Pts',(4.60090423538341,5.32626785654532,-3.03239720378256));
#77363=CARTESIAN_POINT('Ctrl Pts',(0.444561041262034,7.44223775212194,-2.82071213587389));
#77364=CARTESIAN_POINT('Ctrl Pts',(-4.40952184136037,6.01401219799929,-2.60902706796518));
#77365=CARTESIAN_POINT('Ctrl Pts',(-6.74485818788436,1.98620579880015,-2.3973420000565));
#77366=CARTESIAN_POINT('Ctrl Pts',(-6.96734613170004,-2.64159645294223,
-2.18565693214781));
#77367=CARTESIAN_POINT('Ctrl Pts',(-2.83946969726026,-7.47986078096427,
-1.92105059726195));
#77368=CARTESIAN_POINT('Ctrl Pts',(4.7608431875892,-6.4226794151087,-1.60352299539891));
#77369=CARTESIAN_POINT('Ctrl Pts',(7.42194841553578,-0.662378202151734,
-1.33891666051305));
#77370=CARTESIAN_POINT('Ctrl Pts',(5.9550441596121,3.75155376618664,-1.12723159260437));
#77371=CARTESIAN_POINT('Ctrl Pts',(3.44473025469408,6.15511117604201,-0.968467791672837));
#77372=CARTESIAN_POINT('Ctrl Pts',(0.0902840996684676,7.03748939660186,
-0.809703990741332));
#77373=CARTESIAN_POINT('Ctrl Pts',(-4.45175724995302,5.98075099950192,-0.598018922832637));
#77374=CARTESIAN_POINT('Ctrl Pts',(-7.24685279529469,1.76095730151135,-0.386333854923946));
#77375=CARTESIAN_POINT('Ctrl Pts',(-6.43867929370588,-2.8224249160729,-0.174648787015262));
#77376=CARTESIAN_POINT('Ctrl Pts',(-3.63136500170378,-6.51004176743807,
0.0370362808934363));
#77377=CARTESIAN_POINT('Ctrl Pts',(2.64750335128596,-7.54575664707182,0.30164261577929));
#77378=CARTESIAN_POINT('Ctrl Pts',(7.7722224652204,-1.85774493315581,0.61917021764233));
#77379=CARTESIAN_POINT('Ctrl Pts',(5.78168950601745,5.51640505597175,0.936697819505367));
#77380=CARTESIAN_POINT('Ctrl Pts',(-1.50915260430786,7.85303608732375,1.25422542136839));
#77381=CARTESIAN_POINT('Ctrl Pts',(-6.41397970440127,3.79846283921743,1.51883175625427));
#77382=CARTESIAN_POINT('Ctrl Pts',(-6.98435547543984,-0.800907015052163,
1.73051682416294));
#77383=CARTESIAN_POINT('Ctrl Pts',(-5.37638526453188,-5.1683969992388,1.94220189207163));
#77384=CARTESIAN_POINT('Ctrl Pts',(-0.837541475616295,-7.40851195633607,
2.15388695998032));
#77385=CARTESIAN_POINT('Ctrl Pts',(3.61930145044134,-6.03614655527597,2.365572027889));
#77386=CARTESIAN_POINT('Ctrl Pts',(6.0740939213309,-3.58565798032842,2.52433582882053));
#77387=CARTESIAN_POINT('Ctrl Pts',(7.03395291651438,-0.245383316014028,
2.68309962975204));
#77388=CARTESIAN_POINT('Ctrl Pts',(6.08050492620003,4.30714789716092,2.89478469766074));
#77389=CARTESIAN_POINT('Ctrl Pts',(0.882264463901975,7.94594539005975,3.15939103254659));
#77390=CARTESIAN_POINT('Ctrl Pts',(-6.21766375310328,5.03503355675137,3.47691863440964));
#77391=CARTESIAN_POINT('Ctrl Pts',(-7.35021948757106,-1.22319966630272,
3.74152496929548));
#77392=CARTESIAN_POINT('Ctrl Pts',(-4.82923170259673,-5.11044485465725,
3.95321003720419));
#77393=CARTESIAN_POINT('Ctrl Pts',(-0.784305848368582,-7.4160022871715,
4.16489510511287));
#77394=CARTESIAN_POINT('Ctrl Pts',(4.12912677557379,-6.207644428425,4.37658017302156));
#77395=CARTESIAN_POINT('Ctrl Pts',(6.65614737669631,-2.28760817504574,4.58826524093025));
#77396=CARTESIAN_POINT('Ctrl Pts',(6.95598832049435,1.16784059488296,4.74702904186177));
#77397=CARTESIAN_POINT('Ctrl Pts',(5.53969319297264,4.34157960410871,4.90579284279328));
#77398=CARTESIAN_POINT('Ctrl Pts',(1.87864408485616,7.21071695220868,5.11747791070198));
#77399=CARTESIAN_POINT('Ctrl Pts',(-4.44151621939306,6.6474975978659,5.38208424558783));
#77400=CARTESIAN_POINT('Ctrl Pts',(-7.99926348658972,-0.151417668957308,
5.69961184745087));
#77401=CARTESIAN_POINT('Ctrl Pts',(-4.83594761117343,-5.66881541653162,
5.96421818233674));
#77402=CARTESIAN_POINT('Ctrl Pts',(-0.404092264403739,-7.01960450483423,
6.17590325024542));
#77403=CARTESIAN_POINT('Ctrl Pts',(4.17525112536443,-6.17895762063777,6.38758831815411));
#77404=CARTESIAN_POINT('Ctrl Pts',(7.156391420427,-2.090593565277,6.5992733860628));
#77405=CARTESIAN_POINT('Ctrl Pts',(6.56560655093786,2.53579731763451,6.81095845397148));
#77406=CARTESIAN_POINT('Ctrl Pts',(4.56997778699433,5.37260872683312,6.96972225490302));
#77407=CARTESIAN_POINT('Ctrl Pts',(1.4427462000845,6.88883142652401,7.12848605583452));
#77408=CARTESIAN_POINT('Ctrl Pts',(-3.20579129558015,6.72656264803865,7.34017112374322));
#77409=CARTESIAN_POINT('Ctrl Pts',(-7.67862993198306,2.22596768550027,7.60477745862907));
#77410=CARTESIAN_POINT('Ctrl Pts',(-6.02267558443041,-5.2667374102175,7.92230506049211));
#77411=CARTESIAN_POINT('Ctrl Pts',(-0.0496813718136637,-7.45113341886978,
8.18691139537797));
#77412=CARTESIAN_POINT('Ctrl Pts',(4.21089851742052,-5.63084998901683,8.39859646328667));
#77413=CARTESIAN_POINT('Ctrl Pts',(7.1732101275522,-2.03894477191619,8.61028153119536));
#77414=CARTESIAN_POINT('Ctrl Pts',(6.82147720567854,3.00864891656105,8.82196659910403));
#77415=CARTESIAN_POINT('Ctrl Pts',(3.39044470865432,6.16784744531429,9.03365166701273));
#77416=CARTESIAN_POINT('Ctrl Pts',(0.0369233981766486,7.05324451337045,
9.19241546794424));
#77417=CARTESIAN_POINT('Ctrl Pts',(-3.33202473910315,6.19960693574218,9.35117926887578));
#77418=CARTESIAN_POINT('Ctrl Pts',(-6.78409772386992,3.08216822459523,9.56286433678446));
#77419=CARTESIAN_POINT('Ctrl Pts',(-7.30820813198778,-3.24135522065651,
9.82747067167031));
#77420=CARTESIAN_POINT('Ctrl Pts',(-1.21654428380106,-7.90766489866231,
10.1449982735333));
#77421=CARTESIAN_POINT('Ctrl Pts',(4.75992590661602,-5.73279712080287,10.4096046084192));
#77422=CARTESIAN_POINT('Ctrl Pts',(6.84754599281427,-1.5966376542311,10.6212896763279));
#77423=CARTESIAN_POINT('Ctrl Pts',(6.80108736415966,3.05899493007411,10.8329747442366));
#77424=CARTESIAN_POINT('Ctrl Pts',(3.28173063850979,6.69438298776749,11.0446598121453));
#77425=CARTESIAN_POINT('Ctrl Pts',(-1.37759893649087,6.90215028822854,11.2563448800539));
#77426=CARTESIAN_POINT('Ctrl Pts',(-4.51347815651237,5.42016018521777,11.4151086809855));
#77427=CARTESIAN_POINT('Ctrl Pts',(-6.54136045533796,2.59771407453355,11.573872481917));
#77428=CARTESIAN_POINT('Ctrl Pts',(-7.17513323814465,-2.01027508232136,
11.7855575498257));
#77429=CARTESIAN_POINT('Ctrl Pts',(-3.50428048372235,-7.1858408038537,12.0501638847115));
#77430=CARTESIAN_POINT('Ctrl Pts',(4.16113777706602,-6.8334527542274,12.3676914865746));
#77431=CARTESIAN_POINT('Ctrl Pts',(7.3332485659688,-1.32110670821003,12.6322978214604));
#77432=CARTESIAN_POINT('Ctrl Pts',(6.26711360556603,3.18769900987276,12.8439828893691));
#77433=CARTESIAN_POINT('Ctrl Pts',(3.23371169900418,6.71977291021621,13.0556679572778));
#77434=CARTESIAN_POINT('Ctrl Pts',(-1.79982222873307,7.23499547447016,13.2673530251865));
#77435=CARTESIAN_POINT('Ctrl Pts',(-5.49842592883326,4.39371935110196,13.4790380930952));
#77436=CARTESIAN_POINT('Ctrl Pts',(-6.94337994338588,1.24060326636724,13.6378018940267));
#77437=CARTESIAN_POINT('Ctrl Pts',(-6.67746686908588,-2.22462384055129,
13.7965656949582));
#77438=CARTESIAN_POINT('Ctrl Pts',(-4.19518348608569,-6.15826098909458,
14.0082507628669));
#77439=CARTESIAN_POINT('Ctrl Pts',(1.94601072151856,-7.7543105456682,14.2728570977528));
#77440=CARTESIAN_POINT('Ctrl Pts',(7.58385486765223,-2.54878196210885,14.5903846996158));
#77441=CARTESIAN_POINT('Ctrl Pts',(6.46130100527587,3.71125946061199,14.8549910345017));
#77442=CARTESIAN_POINT('Ctrl Pts',(2.74229720123972,6.47440684408134,15.0666761024104));
#77443=CARTESIAN_POINT('Ctrl Pts',(-1.85291024787358,7.22350073928682,15.278361170319));
#77444=CARTESIAN_POINT('Ctrl Pts',(-6.03579160453311,4.3764985179128,15.4900462382278));
#77445=CARTESIAN_POINT('Ctrl Pts',(-7.03600990966135,-0.178946869939357,
15.7017313061364));
#77446=CARTESIAN_POINT('Ctrl Pts',(-6.11117763952622,-3.52180768368873,
15.860495107068));
#77447=CARTESIAN_POINT('Ctrl Pts',(-3.67639914473557,-6.00180009232866,
16.0192589079995));
#77448=CARTESIAN_POINT('Ctrl Pts',(0.755726421246436,-7.41300347146555,
16.2309439759082));
#77449=CARTESIAN_POINT('Ctrl Pts',(6.482036887681,-4.67968883085927,16.495550310794));
#77450=CARTESIAN_POINT('Ctrl Pts',(7.44356313702867,2.933344843187,16.8130779126571));
#77451=CARTESIAN_POINT('Ctrl Pts',(2.55373727311784,7.00002024315999,17.0776842475429));
#77452=CARTESIAN_POINT('Ctrl Pts',(-2.07089157952434,6.71934118708596,17.2893693154516));
#77453=CARTESIAN_POINT('Ctrl Pts',(-6.06900715527003,4.33351952417816,17.5010543833603));
#77454=CARTESIAN_POINT('Ctrl Pts',(-7.43605551059056,-0.538143116708798,
17.712739451269));
#77455=CARTESIAN_POINT('Ctrl Pts',(-5.26797085158183,-4.66754116618141,
17.9244245191776));
#77456=CARTESIAN_POINT('Ctrl Pts',(-2.40785237543088,-6.62962053520908,
18.0831883201092));
#77457=CARTESIAN_POINT('Ctrl Pts',(1.05189606637116,-6.9592405968785,18.2419521210407));
#77458=CARTESIAN_POINT('Ctrl Pts',(5.35158471534051,-5.18500568237527,18.4536371889494));
#77459=CARTESIAN_POINT('Ctrl Pts',(7.97270485365884,0.593520920752225,18.7182435238353));
#77460=CARTESIAN_POINT('Ctrl Pts',(3.80617374547976,7.03734222297062,19.0357711256983));
#77461=CARTESIAN_POINT('Ctrl Pts',(-2.55361055168965,7.00006647218875,19.3003774605842));
#77462=CARTESIAN_POINT('Ctrl Pts',(-5.91114442013924,3.80742820902396,19.5120625284928));
#77463=CARTESIAN_POINT('Ctrl Pts',(-7.43379342875041,-0.592414192789416,
19.7237475964015));
#77464=CARTESIAN_POINT('Ctrl Pts',(-5.3427489512837,-5.19995703964968,19.9354326643102));
#77465=CARTESIAN_POINT('Ctrl Pts',(-1.02496003552201,-6.96325458077588,
20.1471177322189));
#77466=CARTESIAN_POINT('Ctrl Pts',(2.42671806721124,-6.6227381742754,20.3058815331504));
#77467=CARTESIAN_POINT('Ctrl Pts',(5.28599472059724,-4.64712543767729,20.4646453340819));
#77468=CARTESIAN_POINT('Ctrl Pts',(7.43318820353908,-0.521014416784694,
20.6763304019907));
#77469=CARTESIAN_POINT('Ctrl Pts',(5.7176764398638,5.58788563733667,20.9409367368765));
#77470=CARTESIAN_POINT('Ctrl Pts',(-1.61941318767134,7.83509062306115,21.2584643387396));
#77471=CARTESIAN_POINT('Ctrl Pts',(-6.46123381947619,3.71137642860669,21.5230706736254));
#77472=CARTESIAN_POINT('Ctrl Pts',(-6.97425290871281,-0.893271676437503,
21.7347557415341));
#77473=CARTESIAN_POINT('Ctrl Pts',(-5.30607199686021,-5.2400228321342,21.9464408094428));
#77474=CARTESIAN_POINT('Ctrl Pts',(-0.739338760625791,-7.41875311408065,
22.1581258773514));
#77475=CARTESIAN_POINT('Ctrl Pts',(3.69959238591993,-5.98752650174991,22.3698109452601));
#77476=CARTESIAN_POINT('Ctrl Pts',(6.12117994620704,-3.5043940373318,22.5285747461917));
#77477=CARTESIAN_POINT('Ctrl Pts',(7.03665373271079,-0.151721012440911,
22.6873385471232));
#77478=CARTESIAN_POINT('Ctrl Pts',(6.02256833025328,4.38775724022655,22.8990236150319));
#77479=CARTESIAN_POINT('Ctrl Pts',(0.776397834368402,7.95697782890683,23.1636299499177));
#77480=CARTESIAN_POINT('Ctrl Pts',(-6.2841755041135,4.95179587397182,23.4811575517808));
#77481=CARTESIAN_POINT('Ctrl Pts',(-7.33327248069457,-1.32097395456858,
23.7457638866666));
#77482=CARTESIAN_POINT('Ctrl Pts',(-4.76075272415858,-5.17429912374916,
23.9574489545753));
#77483=CARTESIAN_POINT('Ctrl Pts',(-0.685478317186439,-7.42579011242699,
24.169134022484));
#77484=CARTESIAN_POINT('Ctrl Pts',(4.21142387439496,-6.1521076486698,24.3808190903927));
#77485=CARTESIAN_POINT('Ctrl Pts',(6.68602078785581,-2.19876862254172,24.5925041583014));
#77486=CARTESIAN_POINT('Ctrl Pts',(6.93981963119231,1.26036700577737,24.7512679592329));
#77487=CARTESIAN_POINT('Ctrl Pts',(5.48138722818666,4.41496422118694,24.9100317601644));
#77488=CARTESIAN_POINT('Ctrl Pts',(1.78245547991169,7.23509470248057,25.1217168280731));
#77489=CARTESIAN_POINT('Ctrl Pts',(-4.5296441244476,6.5877624329345,25.3863231629589));
#77490=CARTESIAN_POINT('Ctrl Pts',(-7.99653786750668,-0.257926884050681,
25.703850764822));
#77491=CARTESIAN_POINT('Ctrl Pts',(-4.76002968637034,-5.73271095116737,
25.9684570997079));
#77492=CARTESIAN_POINT('Ctrl Pts',(-0.310579469273625,-7.02436319646701,
26.1801421676165));
#77493=CARTESIAN_POINT('Ctrl Pts',(4.2571633622848,-6.1228097654567,26.3918272355252));
#77494=CARTESIAN_POINT('Ctrl Pts',(7.1835963760093,-1.9951096905261,26.6035123034339));
#77495=CARTESIAN_POINT('Ctrl Pts',(6.53125629229405,2.62300375056602,26.8151973713426));
#77496=CARTESIAN_POINT('Ctrl Pts',(4.49802791353949,5.43298871632856,26.9739611722741));
#77497=CARTESIAN_POINT('Ctrl Pts',(1.35088274939726,6.90743301213046,27.1327249732057));
#77498=CARTESIAN_POINT('Ctrl Pts',(-3.29508170266839,6.68327610266628,27.3444100411143));
#77499=CARTESIAN_POINT('Ctrl Pts',(-7.70759130112504,2.12351738908524,27.6090163760003));
#77500=CARTESIAN_POINT('Ctrl Pts',(-5.95200674357977,-5.34647172145942,
27.9265439778632));
#77501=CARTESIAN_POINT('Ctrl Pts',(0.049546484282045,-7.45113431704577,
28.1911503127491));
#77502=CARTESIAN_POINT('Ctrl Pts',(4.28550868087525,-5.57427603090819,28.4028353806578));
#77503=CARTESIAN_POINT('Ctrl Pts',(7.19972581056599,-1.94324151093504,28.6145204485665));
#77504=CARTESIAN_POINT('Ctrl Pts',(6.78080750212263,3.09922073912179,28.8262055164751));
#77505=CARTESIAN_POINT('Ctrl Pts',(3.30800958166722,6.21244960049673,29.0378905843839));
#77506=CARTESIAN_POINT('Ctrl Pts',(-0.0570048159302318,7.05311079976029,
29.1966543853154));
#77507=CARTESIAN_POINT('Ctrl Pts',(-3.41428671659465,6.15468612006932,29.3554181862469));
#77508=CARTESIAN_POINT('Ctrl Pts',(-6.82454005487817,2.99155409964336,29.5671032541556));
#77509=CARTESIAN_POINT('Ctrl Pts',(-7.26439642334094,-3.33838798995519,
29.8317095890415));
#77510=CARTESIAN_POINT('Ctrl Pts',(-1.11113353487349,-7.92316391422415,
30.1492371909045));
#77511=CARTESIAN_POINT('Ctrl Pts',(4.83584497311704,-5.66890296801239,30.4138435257904));
#77512=CARTESIAN_POINT('Ctrl Pts',(6.86820054380616,-1.50531033766313,30.6255285936991));
#77513=CARTESIAN_POINT('Ctrl Pts',(6.75974903295088,3.14929076597755,30.8372136616077));
#77514=CARTESIAN_POINT('Ctrl Pts',(3.19229350999306,6.73749075819042,31.0488987295164));
#77515=CARTESIAN_POINT('Ctrl Pts',(-1.46938967088129,6.88319340322654,31.2605837974251));
#77516=CARTESIAN_POINT('Ctrl Pts',(-4.58525582745349,5.35957558949753,31.4193475983566));
#77517=CARTESIAN_POINT('Ctrl Pts',(-6.57537304786625,2.51037533071907,31.5781113992881));
#77518=CARTESIAN_POINT('Ctrl Pts',(-7.14772707930367,-2.10564491107097,
31.7897964671968));
#77519=CARTESIAN_POINT('Ctrl Pts',(-3.40827909532261,-7.23186859499761,
32.0544028020827));
#77520=CARTESIAN_POINT('Ctrl Pts',(4.25176688234156,-6.77743480398061,32.3719304039457));
#77521=CARTESIAN_POINT('Ctrl Pts',(7.35019092621592,-1.22333593625597,32.6365367388316));
#77522=CARTESIAN_POINT('Ctrl Pts',(6.22410872607908,3.27087274111372,32.8482218067403));
#77523=CARTESIAN_POINT('Ctrl Pts',(3.14394072191596,6.76223898233638,33.059906874649));
#77524=CARTESIAN_POINT('Ctrl Pts',(-1.89600787713411,7.21038651533262,33.2715919425577));
#77525=CARTESIAN_POINT('Ctrl Pts',(-5.55644760618287,4.32010965495771,33.4832770104663));
#77526=CARTESIAN_POINT('Ctrl Pts',(-6.95928484424909,1.14803134074789,33.6420408113979));
#77527=CARTESIAN_POINT('Ctrl Pts',(-6.64725045028281,-2.3133474600465,33.8008046123294));
#77528=CARTESIAN_POINT('Ctrl Pts',(-4.11280466208001,-6.21358034496234,
34.0124896802381));
#77529=CARTESIAN_POINT('Ctrl Pts',(2.04909889679104,-7.72770881167863,34.2770960151239));
#77530=CARTESIAN_POINT('Ctrl Pts',(7.61712341562411,-2.44756511969248,34.594623616987));
#77531=CARTESIAN_POINT('Ctrl Pts',(6.41130688418545,3.79697267590346,34.8592299518729));
#77532=CARTESIAN_POINT('Ctrl Pts',(2.65583722899417,6.51035072294137,35.0709150197815));
#77533=CARTESIAN_POINT('Ctrl Pts',(-1.94893811868904,7.19818584968968,35.2826000876902));
#77534=CARTESIAN_POINT('Ctrl Pts',(-6.0935363118243,4.29573448750313,35.4942851555989));
#77535=CARTESIAN_POINT('Ctrl Pts',(-7.03300307526989,-0.272626437379933,
35.7059702235076));
#77536=CARTESIAN_POINT('Ctrl Pts',(-6.06373740921473,-3.60287525940376,
35.8647340244391));
#77537=CARTESIAN_POINT('Ctrl Pts',(-3.59614984158672,-6.05022489966651,
36.0234978253707));
#77538=CARTESIAN_POINT('Ctrl Pts',(0.854375102710567,-7.40228249093471,
36.2351828932793));
#77539=CARTESIAN_POINT('Ctrl Pts',(6.54377947812764,-4.59295546555386,36.4997892281652));
#77540=CARTESIAN_POINT('Ctrl Pts',(7.4038410646272,3.03220738633166,36.8173168300282));
#77541=CARTESIAN_POINT('Ctrl Pts',(2.46029465899688,7.03340654702068,37.0819231649141));
#77542=CARTESIAN_POINT('Ctrl Pts',(-2.16018645213729,6.6911682398978,37.2936082328227));
#77543=CARTESIAN_POINT('Ctrl Pts',(-6.12617658509613,4.2523169878751,37.5052933007315));
#77544=CARTESIAN_POINT('Ctrl Pts',(-7.42822994676136,-0.637118064947822,
37.7169783686402));
#77545=CARTESIAN_POINT('Ctrl Pts',(-5.20534816136745,-4.73727853836591,
37.9286634365488));
#77546=CARTESIAN_POINT('Ctrl Pts',(-2.3193551460399,-6.66109699743759,38.0874272374804));
#77547=CARTESIAN_POINT('Ctrl Pts',(1.1444759270142,-6.9446158909024,38.2461910384118));
#77548=CARTESIAN_POINT('Ctrl Pts',(5.4201566233756,-5.11328124297969,38.4578761063206));
#77549=CARTESIAN_POINT('Ctrl Pts',(7.96409426376987,0.69963728082014,38.7224824412064));
#77550=CARTESIAN_POINT('Ctrl Pts',(3.712123078394,7.0874033605291,39.0400100430695));
#77551=CARTESIAN_POINT('Ctrl Pts',(-2.64660091651398,6.96544047806516,39.3046163779553));
#77552=CARTESIAN_POINT('Ctrl Pts',(-5.96132212199443,3.72837450914394,39.516301445864));
#77553=CARTESIAN_POINT('Ctrl Pts',(-7.42524536156241,-0.691354205706398,
39.7279865137728));
#77554=CARTESIAN_POINT('Ctrl Pts',(-5.27302968365255,-5.27064298980338,
39.9396715816813));
#77555=CARTESIAN_POINT('Ctrl Pts',(-0.932142569072262,-6.97628609376343,
40.1513566495901));
#77556=CARTESIAN_POINT('Ctrl Pts',(2.51469496931212,-6.58983540872235,40.3101204505215));
#77557=CARTESIAN_POINT('Ctrl Pts',(5.34740973093818,-4.57632212471511,40.4688842514532));
#77558=CARTESIAN_POINT('Ctrl Pts',(7.43946722675043,-0.421983736459396,
40.6805693193617));
#77559=CARTESIAN_POINT('Ctrl Pts',(5.64275805398072,5.66352993380997,40.9451756542477));
#77560=CARTESIAN_POINT('Ctrl Pts',(-1.7236060347068,7.81283088138394,41.2627032561106));
#77561=CARTESIAN_POINT('Ctrl Pts',(-6.51008366618329,3.62500594814068,41.5273095909966));
#77562=CARTESIAN_POINT('Ctrl Pts',(-6.96173920250525,-0.986065514515229,
41.7389946589052));
#77563=CARTESIAN_POINT('Ctrl Pts',(-5.23582244289624,-5.31021681888934,
41.950679726814));
#77564=CARTESIAN_POINT('Ctrl Pts',(-0.64048094734282,-7.42794074604368,
42.1623647947226));
#77565=CARTESIAN_POINT('Ctrl Pts',(3.77899759003504,-5.93772975518615,42.3740498626313));
#77566=CARTESIAN_POINT('Ctrl Pts',(6.16730365221708,-3.42257025699746,42.5328136635628));
#77567=CARTESIAN_POINT('Ctrl Pts',(7.03805019928911,-0.0580035514068519,
42.6915774644943));
#77568=CARTESIAN_POINT('Ctrl Pts',(5.96360448931232,4.4675680617965,42.903262532403));
#77569=CARTESIAN_POINT('Ctrl Pts',(0.670369434414901,7.96661123617363,43.1678688672888));
#77570=CARTESIAN_POINT('Ctrl Pts',(-6.34955916802911,4.86767321373177,43.485396469152));
#77571=CARTESIAN_POINT('Ctrl Pts',(-7.3150314182536,-1.41851077356636,43.7500028040378));
#77572=CARTESIAN_POINT('Ctrl Pts',(-4.69142673684704,-5.23723716241792,
43.9616878719465));
#77573=CARTESIAN_POINT('Ctrl Pts',(-0.58653157107381,-7.43425988470175,
44.1733729398552));
#77574=CARTESIAN_POINT('Ctrl Pts',(4.29297534917504,-6.09548047507495,44.3850580077638));
#77575=CARTESIAN_POINT('Ctrl Pts',(6.71470797317736,-2.10953887521942,44.5967430756726));
#77576=CARTESIAN_POINT('Ctrl Pts',(6.9224205318893,1.35266976103254,44.755506876604));
#77577=CARTESIAN_POINT('Ctrl Pts',(5.42210907004846,4.48756596076176,44.9142706775357));
#77578=CARTESIAN_POINT('Ctrl Pts',(1.68595087211227,7.25818934366925,45.1259557454442));
#77579=CARTESIAN_POINT('Ctrl Pts',(-4.61696880509652,6.52685903170057,45.3905620803302));
#77580=CARTESIAN_POINT('Ctrl Pts',(-7.99239412183842,-0.364390374716451,
45.7080896821931));
#77581=CARTESIAN_POINT('Ctrl Pts',(-4.6832676396441,-5.79558984748086,45.972696017079));
#77582=CARTESIAN_POINT('Ctrl Pts',(-0.217011590012495,-7.02787620070355,
46.1843810849877));
#77583=CARTESIAN_POINT('Ctrl Pts',(4.33832063441401,-6.0655760971378,46.3960661528965));
#77584=CARTESIAN_POINT('Ctrl Pts',(7.20952740566221,-1.89927200728346,46.607751220805));
#77585=CARTESIAN_POINT('Ctrl Pts',(6.49574778867412,2.70974502436097,46.8194362887139));
#77586=CARTESIAN_POINT('Ctrl Pts',(4.42528036686922,5.49240522697806,46.9782000896452));
#77587=CARTESIAN_POINT('Ctrl Pts',(1.25877973477203,6.92480964352208,47.1369638905769));
#77588=CARTESIAN_POINT('Ctrl Pts',(-3.38378776442068,6.63880435448184,47.3486489584854));
#77589=CARTESIAN_POINT('Ctrl Pts',(-7.73518581709401,2.02069051117516,47.6132552933714));
#77590=CARTESIAN_POINT('Ctrl Pts',(-5.88028238222423,-5.42525789703002,
47.9307828952344));
#77591=CARTESIAN_POINT('Ctrl Pts',(0.148765553839371,-7.44981384161723,
48.1953892301203));
#77592=CARTESIAN_POINT('Ctrl Pts',(4.35935885831631,-5.51671353860559,48.407074298029));
#77593=CARTESIAN_POINT('Ctrl Pts',(7.22496470440797,-1.84719363825532,48.6187593659376));
#77594=CARTESIAN_POINT('Ctrl Pts',(6.73893529979263,3.18924295027096,48.8304444338464));
#77595=CARTESIAN_POINT('Ctrl Pts',(3.2249878169521,6.25595004868359,49.042129501755));
#77596=CARTESIAN_POINT('Ctrl Pts',(-0.150922920881917,7.05172629748821,
49.2008933026865));
#77597=CARTESIAN_POINT('Ctrl Pts',(-3.495943209325,6.1086738410938,49.359657103618));
#77598=CARTESIAN_POINT('Ctrl Pts',(-6.86377213163642,2.90040945673224,49.5713421715268));
#77599=CARTESIAN_POINT('Ctrl Pts',(-7.2192964569405,-3.43482873426469,49.8359485064125));
#77600=CARTESIAN_POINT('Ctrl Pts',(-1.00552573910145,-7.93725784714026,
50.1534761082757));
#77601=CARTESIAN_POINT('Ctrl Pts',(4.91090645773264,-5.6040035000133,50.4180824431614));
#77602=CARTESIAN_POINT('Ctrl Pts',(6.88763709785911,-1.41371607149604,50.6297675110702));
#77603=CARTESIAN_POINT('Ctrl Pts',(6.71721193744111,3.23902811112609,50.8414525789789));
#77604=CARTESIAN_POINT('Ctrl Pts',(3.10229026467322,6.7794037115615,51.0531376468875));
#77605=CARTESIAN_POINT('Ctrl Pts',(-1.56091982579034,6.86301586247476,51.2648227147963));
#77606=CARTESIAN_POINT('Ctrl Pts',(-4.65622035563679,5.29804053424458,51.4235865157277));
#77607=CARTESIAN_POINT('Ctrl Pts',(-6.60821957306057,2.42259140051073,51.5823503166593));
#77608=CARTESIAN_POINT('Ctrl Pts',(-7.11905335270188,-2.20064132775103,
51.794035384568));
#77609=CARTESIAN_POINT('Ctrl Pts',(-3.31167328750886,-7.27661389680405,
52.0586417194539));
#77610=CARTESIAN_POINT('Ctrl Pts',(4.34164198524954,-6.72021495310217,52.3761693213169));
#77611=CARTESIAN_POINT('Ctrl Pts',(7.36582981413719,-1.12534821957666,52.6407756562027));
#77612=CARTESIAN_POINT('Ctrl Pts',(6.18000007184479,3.35346642033527,52.8524607241115));
#77613=CARTESIAN_POINT('Ctrl Pts',(3.0536122031964,6.80350584881866,53.0641457920201));
#77614=CARTESIAN_POINT('Ctrl Pts',(-1.99185729091034,7.18449887601852,53.2758308599288));
#77615=CARTESIAN_POINT('Ctrl Pts',(-5.61348391010628,4.24573383726985,53.4875159278375));
#77616=CARTESIAN_POINT('Ctrl Pts',(-6.97395559726895,1.05525582368896,53.646279728769));
#77617=CARTESIAN_POINT('Ctrl Pts',(-6.61585521413192,-2.40166083161287,
53.8050435297005));
#77618=CARTESIAN_POINT('Ctrl Pts',(-4.02969648644615,-6.26779779800259,
54.0167285976093));
#77619=CARTESIAN_POINT('Ctrl Pts',(2.15182370290406,-7.69973664706345,54.281334932495));
#77620=CARTESIAN_POINT('Ctrl Pts',(7.64904112730664,-2.34591424651271,54.5988625343582));
#77621=CARTESIAN_POINT('Ctrl Pts',(6.36017583535967,3.88201256989678,54.8634688692439));
#77622=CARTESIAN_POINT('Ctrl Pts',(2.5689062153214,6.54514002756553,55.0751539371527));
#77623=CARTESIAN_POINT('Ctrl Pts',(-2.04462021559947,7.17159454156269,55.2868390050613));
#77624=CARTESIAN_POINT('Ctrl Pts',(-6.15020070906691,4.21420845931486,55.49852407297));
#77625=CARTESIAN_POINT('Ctrl Pts',(-7.02874863621731,-0.366257412569875,
55.7102091408788));
#77626=CARTESIAN_POINT('Ctrl Pts',(-6.01522263894987,-3.68330441628207,
55.8689729418102));
#77627=CARTESIAN_POINT('Ctrl Pts',(-3.51526135293355,-6.09757583857006,
56.0277367427418));
#77628=CARTESIAN_POINT('Ctrl Pts',(0.952869138907655,-7.39025080980567,
56.2394218106504));
#77629=CARTESIAN_POINT('Ctrl Pts',(6.60436808219333,-4.50540343472597,56.5040281455363));
#77630=CARTESIAN_POINT('Ctrl Pts',(7.36279468941762,3.13052494009091,56.8215557473994));
#77631=CARTESIAN_POINT('Ctrl Pts',(2.36643471902825,7.06555773634852,57.0861620822851));
#77632=CARTESIAN_POINT('Ctrl Pts',(-2.24912350964978,6.66179247408394,57.297847150194));
#77633=CARTESIAN_POINT('Ctrl Pts',(-6.18219453733946,4.17040210987243,57.5095322181025));
#77634=CARTESIAN_POINT('Ctrl Pts',(-7.41921937995394,-0.736064935536567,
57.7212172860114));
#77635=CARTESIAN_POINT('Ctrl Pts',(-5.14163886745774,-4.80607088708851,
57.9329023539199));
#77636=CARTESIAN_POINT('Ctrl Pts',(-2.23078681769651,-6.69161051830819,
58.0916661548515));
#77637=CARTESIAN_POINT('Ctrl Pts',(1.23747337014818,-6.92836140896512,58.250429955783));
#77638=CARTESIAN_POINT('Ctrl Pts',(5.48642653137197,-5.0415104690091,58.4621150236917));
#77639=CARTESIAN_POINT('Ctrl Pts',(7.95684541214289,0.807409843183617,58.7267213585775));
#77640=CARTESIAN_POINT('Ctrl Pts',(3.61256597258128,7.13309616752026,59.0442489604406));
#77641=CARTESIAN_POINT('Ctrl Pts',(-2.73097502532573,6.93480882320121,59.3088552953264));
#77642=CARTESIAN_POINT('Ctrl Pts',(-6.02140560873619,3.6416148042235,59.5205403632351));
#77643=CARTESIAN_POINT('Ctrl Pts',(-7.04413462746363,0.332516821336018,
59.6793041641666));
#77644=CARTESIAN_POINT('Ctrl Pts',(-6.33691269983105,-3.08643256639824,
59.8380746593449));
#77645=CARTESIAN_POINT('Ctrl Pts',(-4.84078143417837,-4.8527243283379,59.9439238875458));
#77646=CARTESIAN_POINT('Ctrl Pts',(-3.92534899164063,-5.50542332685364,
59.9968518487696));
#77647=CARTESIAN_POINT('Ctrl Pts',(-3.09289325614769,6.45110082070439,-60.4369614153577));
#77648=CARTESIAN_POINT('Ctrl Pts',(-4.16562014990033,5.93679815796041,-60.3840310532033));
#77649=CARTESIAN_POINT('Ctrl Pts',(-6.04570215501001,4.36700469538412,-60.2781794240718));
#77650=CARTESIAN_POINT('Ctrl Pts',(-7.40319472859208,0.93131111440289,-60.1194065279632));
#77651=CARTESIAN_POINT('Ctrl Pts',(-6.93742111779479,-2.70366387687074,
-59.9606427270316));
#77652=CARTESIAN_POINT('Ctrl Pts',(-4.10488940433561,-6.73346130664272,
-59.7489576591229));
#77653=CARTESIAN_POINT('Ctrl Pts',(2.47170292483413,-8.09098755230349,-59.4843513242371));
#77654=CARTESIAN_POINT('Ctrl Pts',(8.14781008572697,-2.28516285174072,-59.166823722374));
#77655=CARTESIAN_POINT('Ctrl Pts',(6.63371968662535,4.25998251374448,-58.9022173874882));
#77656=CARTESIAN_POINT('Ctrl Pts',(2.54687994990649,6.99768788344637,-58.6905323195795));
#77657=CARTESIAN_POINT('Ctrl Pts',(-1.11141694785635,7.38009987772104,-58.5317685186479));
#77658=CARTESIAN_POINT('Ctrl Pts',(-4.48778573003331,5.94267579194522,-58.3730047177166));
#77659=CARTESIAN_POINT('Ctrl Pts',(-7.60032701309895,2.11325746684096,-58.1613196498077));
#77660=CARTESIAN_POINT('Ctrl Pts',(-7.20096026774904,-3.22570666445012,
-57.9496345818991));
#77661=CARTESIAN_POINT('Ctrl Pts',(-3.55307302003504,-6.5362828925506,-57.7379495139904));
#77662=CARTESIAN_POINT('Ctrl Pts',(1.18497697000321,-7.79451478752187,-57.5262644460818));
#77663=CARTESIAN_POINT('Ctrl Pts',(7.10711231753246,-4.59902803843737,-57.2616581111957));
#77664=CARTESIAN_POINT('Ctrl Pts',(7.70181295244941,3.49832541559333,-56.944130509333));
#77665=CARTESIAN_POINT('Ctrl Pts',(2.33400074345349,7.53079782198634,-56.6795241744469));
#77666=CARTESIAN_POINT('Ctrl Pts',(-2.55813326706307,6.99389892744948,-56.4678391065383));
#77667=CARTESIAN_POINT('Ctrl Pts',(-5.60210698976003,4.93077719032846,-56.3090753056067));
#77668=CARTESIAN_POINT('Ctrl Pts',(-7.26038631684579,1.65692847571967,-56.1503115046752));
#77669=CARTESIAN_POINT('Ctrl Pts',(-7.17555684949993,-3.27717504576235,
-55.9386264367666));
#77670=CARTESIAN_POINT('Ctrl Pts',(-3.43238396175318,-7.1048057165866,-55.7269413688578));
#77671=CARTESIAN_POINT('Ctrl Pts',(1.49044801780787,-7.28875849380132,-55.5152563009492));
#77672=CARTESIAN_POINT('Ctrl Pts',(5.92564020795954,-5.20049295229579,-55.3035712330405));
#77673=CARTESIAN_POINT('Ctrl Pts',(8.39902043501333,1.05773211100905,-55.0389648981546));
#77674=CARTESIAN_POINT('Ctrl Pts',(3.63994810713719,7.6358972814368,-54.7214372962916));
#77675=CARTESIAN_POINT('Ctrl Pts',(-3.06350390178714,7.26466741899136,-54.4568309614057));
#77676=CARTESIAN_POINT('Ctrl Pts',(-6.46072452460837,3.70374549364738,-54.245145893497));
#77677=CARTESIAN_POINT('Ctrl Pts',(-7.46115700940049,0.165189662269874,
-54.0863820925655));
#77678=CARTESIAN_POINT('Ctrl Pts',(-6.62179760813936,-3.40740723797466,
-53.9276182916339));
#77679=CARTESIAN_POINT('Ctrl Pts',(-3.37972447947155,-7.12782943365753,
-53.7159332237254));
#77680=CARTESIAN_POINT('Ctrl Pts',(1.9488378753097,-7.64601556384835,-53.5042481558165));
#77681=CARTESIAN_POINT('Ctrl Pts',(5.83371089549533,-4.61684456685773,-53.292563087908));
#77682=CARTESIAN_POINT('Ctrl Pts',(7.88236626709611,-0.16321757068143,-53.0808780199992));
#77683=CARTESIAN_POINT('Ctrl Pts',(5.74493227405618,6.21756343083984,-52.8162716851135));
#77684=CARTESIAN_POINT('Ctrl Pts',(-2.13201300317532,8.18600452989546,-52.4987440832501));
#77685=CARTESIAN_POINT('Ctrl Pts',(-7.02173133206871,3.58548990146649,-52.2341377483646));
#77686=CARTESIAN_POINT('Ctrl Pts',(-7.32796911262751,-1.32648438012215,
-52.0224526804557));
#77687=CARTESIAN_POINT('Ctrl Pts',(-5.81484423605366,-4.67800577465704,
-51.8636888795243));
#77688=CARTESIAN_POINT('Ctrl Pts',(-2.87218866315881,-6.87089222281699,
-51.7049250785927));
#77689=CARTESIAN_POINT('Ctrl Pts',(2.00395288249048,-7.62972233055806,-51.4932400106842));
#77690=CARTESIAN_POINT('Ctrl Pts',(6.4144665742518,-4.59501269081789,-51.2815549427753));
#77691=CARTESIAN_POINT('Ctrl Pts',(7.43620879853939,0.224132268622218,-51.0698698748668));
#77692=CARTESIAN_POINT('Ctrl Pts',(6.13583841096293,4.95073983734211,-50.8581848069579));
#77693=CARTESIAN_POINT('Ctrl Pts',(0.391788697102781,8.45629017163187,-50.5935784720722));
#77694=CARTESIAN_POINT('Ctrl Pts',(-6.90232239734956,4.89020399705925,-50.276050870209));
#77695=CARTESIAN_POINT('Ctrl Pts',(-7.68104402021101,-1.77820456993238,
-50.0114445353233));
#77696=CARTESIAN_POINT('Ctrl Pts',(-4.75242384388133,-5.73351198956874,
-49.7997594674145));
#77697=CARTESIAN_POINT('Ctrl Pts',(-1.43663038395558,-7.32340389826851,
-49.6409956664831));
#77698=CARTESIAN_POINT('Ctrl Pts',(2.22681761706147,-7.10632893656609,-49.4822318655515));
#77699=CARTESIAN_POINT('Ctrl Pts',(6.44614310799523,-4.54705718327047,-49.2705467976428));
#77700=CARTESIAN_POINT('Ctrl Pts',(7.86648262055552,0.614796097461046,-49.0588617297342));
#77701=CARTESIAN_POINT('Ctrl Pts',(5.54506421911325,4.95980840106012,-48.8471766618254));
#77702=CARTESIAN_POINT('Ctrl Pts',(1.50660159420562,7.73876537820023,-48.6354915939168));
#77703=CARTESIAN_POINT('Ctrl Pts',(-5.14542308904248,6.72212489357063,-48.3708852590308));
#77704=CARTESIAN_POINT('Ctrl Pts',(-8.42981715200117,-0.703087756710445,
-48.0533576571679));
#77705=CARTESIAN_POINT('Ctrl Pts',(-4.73168696485318,-6.30647185037608,
-47.7887513222819));
#77706=CARTESIAN_POINT('Ctrl Pts',(0.0558814622644325,-7.4468496284399,
-47.5770662543734));
#77707=CARTESIAN_POINT('Ctrl Pts',(3.61653398079731,-6.5281569744467,-47.4183024534417));
#77708=CARTESIAN_POINT('Ctrl Pts',(6.27963156485163,-4.00310567735237,-47.2595386525103));
#77709=CARTESIAN_POINT('Ctrl Pts',(7.85983856963731,0.671883662495001,-47.0478535846016));
#77710=CARTESIAN_POINT('Ctrl Pts',(5.62270708618466,5.53576445343586,-46.8361685166929));
#77711=CARTESIAN_POINT('Ctrl Pts',(1.04876525953824,7.36529211910175,-46.6244834487842));
#77712=CARTESIAN_POINT('Ctrl Pts',(-3.83045925978348,6.89100281538415,-46.4127983808755));
#77713=CARTESIAN_POINT('Ctrl Pts',(-8.26523789501724,1.8298044673638,-46.1481920459897));
#77714=CARTESIAN_POINT('Ctrl Pts',(-5.99685730962747,-5.96605833174442,
-45.8306644441266));
#77715=CARTESIAN_POINT('Ctrl Pts',(0.440687630948982,-7.87186401971451,
-45.5660581092408));
#77716=CARTESIAN_POINT('Ctrl Pts',(4.83793281887333,-5.66154556340304,-45.354373041332));
#77717=CARTESIAN_POINT('Ctrl Pts',(6.97059641115693,-2.6658839415933,-45.1956092404006));
#77718=CARTESIAN_POINT('Ctrl Pts',(7.38218037044503,0.980836700245129,-45.036845439469));
#77719=CARTESIAN_POINT('Ctrl Pts',(5.58086392542702,5.57516348124011,-44.8251603715604));
#77720=CARTESIAN_POINT('Ctrl Pts',(0.737299387595404,7.85594759873095,-44.6134753036517));
#77721=CARTESIAN_POINT('Ctrl Pts',(-3.94025935688594,6.31045107498579,-44.4017902357429));
#77722=CARTESIAN_POINT('Ctrl Pts',(-7.36791287311896,2.80574372254866,-44.1901051678343));
#77723=CARTESIAN_POINT('Ctrl Pts',(-7.50191990859716,-3.92218555591228,
-43.9254988329484));
#77724=CARTESIAN_POINT('Ctrl Pts',(-0.746483913511334,-8.4260851750192,
-43.6079712310853));
#77725=CARTESIAN_POINT('Ctrl Pts',(5.40602056471108,-5.7389363462987,-43.3433648961995));
#77726=CARTESIAN_POINT('Ctrl Pts',(7.34705073847908,-1.21636243473493,-43.1316798282908));
#77727=CARTESIAN_POINT('Ctrl Pts',(7.04976804581042,2.4488613716479,-42.9729160273593));
#77728=CARTESIAN_POINT('Ctrl Pts',(5.01647005997232,5.50396727749474,-42.8141522264277));
#77729=CARTESIAN_POINT('Ctrl Pts',(0.679915661826589,7.85914783481573,-42.6024671585192));
#77730=CARTESIAN_POINT('Ctrl Pts',(-4.49450262730389,6.48528867469395,-42.3907820906104));
#77731=CARTESIAN_POINT('Ctrl Pts',(-7.07809099936217,2.29086542033022,-42.1790970227017));
#77732=CARTESIAN_POINT('Ctrl Pts',(-7.44381045473222,-2.59769587452286,
-41.9674119547931));
#77733=CARTESIAN_POINT('Ctrl Pts',(-3.21408737425887,-7.83147394815582,
-41.7028056199072));
#77734=CARTESIAN_POINT('Ctrl Pts',(4.85459882701441,-6.92741076005743,-41.3852780180441));
#77735=CARTESIAN_POINT('Ctrl Pts',(7.83152391367127,-0.909770258110416,
-41.1206716831583));
#77736=CARTESIAN_POINT('Ctrl Pts',(6.40441397027651,3.80028601867642,-40.9089866152495));
#77737=CARTESIAN_POINT('Ctrl Pts',(3.81685286273701,6.41309486453266,-40.7502228143181));
#77738=CARTESIAN_POINT('Ctrl Pts',(0.293946837473347,7.44125143447466,-40.5914590133865));
#77739=CARTESIAN_POINT('Ctrl Pts',(-4.54046718260951,6.45078660012343,-40.3797739454779));
#77740=CARTESIAN_POINT('Ctrl Pts',(-7.61471986276085,2.06774381213691,-40.1680888775692));
#77741=CARTESIAN_POINT('Ctrl Pts',(-6.89052927551469,-2.8050031858434,-39.9564038096605));
#77742=CARTESIAN_POINT('Ctrl Pts',(-4.02249418185155,-6.78069896835596,
-39.7447187417518));
#77743=CARTESIAN_POINT('Ctrl Pts',(2.58377163955079,-8.06141835936246,-39.4801124068659));
#77744=CARTESIAN_POINT('Ctrl Pts',(8.17491818981989,-2.17413481632614,-39.162584805003));
#77745=CARTESIAN_POINT('Ctrl Pts',(6.57765980704569,4.34681954947786,-38.897978470117));
#77746=CARTESIAN_POINT('Ctrl Pts',(2.45288741330638,7.03150307289015,-38.6862934022084));
#77747=CARTESIAN_POINT('Ctrl Pts',(-1.20927707147813,7.36436015426162,-38.5275296012768));
#77748=CARTESIAN_POINT('Ctrl Pts',(-4.56667702027796,5.88252400307868,-38.3687658003453));
#77749=CARTESIAN_POINT('Ctrl Pts',(-7.62767040977012,2.01174901928726,-38.1570807324367));
#77750=CARTESIAN_POINT('Ctrl Pts',(-7.15742743914158,-3.32125812221487,
-37.9453956645279));
#77751=CARTESIAN_POINT('Ctrl Pts',(-3.46569349778444,-6.5830392030377,-37.7337105966193));
#77752=CARTESIAN_POINT('Ctrl Pts',(1.28865021977318,-7.77802793473847,-37.5220255287106));
#77753=CARTESIAN_POINT('Ctrl Pts',(7.16773596466101,-4.50398745456938,-37.2574191938247));
#77754=CARTESIAN_POINT('Ctrl Pts',(7.65453831308241,3.60058228948636,-36.9398915919617));
#77755=CARTESIAN_POINT('Ctrl Pts',(2.2335124177871,7.56120830373943,-36.6752852570758));
#77756=CARTESIAN_POINT('Ctrl Pts',(-2.65104245880669,6.95921446774165,-36.4636001891671));
#77757=CARTESIAN_POINT('Ctrl Pts',(-5.66727049093198,4.85573853290007,-36.3048363882356));
#77758=CARTESIAN_POINT('Ctrl Pts',(-7.28180748570867,1.56009852105847,-36.1460725873041));
#77759=CARTESIAN_POINT('Ctrl Pts',(-7.13127961653182,-3.3724384393972,-35.9343875193954));
#77760=CARTESIAN_POINT('Ctrl Pts',(-3.33746819925646,-7.14988315148624,
-35.7227024514867));
#77761=CARTESIAN_POINT('Ctrl Pts',(1.58737709188624,-7.26826461663796,-35.511017383578));
#77762=CARTESIAN_POINT('Ctrl Pts',(5.99436741048307,-5.12112265920587,-35.2993323156693));
#77763=CARTESIAN_POINT('Ctrl Pts',(8.38419037352516,1.16948434384604,-35.0347259807835));
#77764=CARTESIAN_POINT('Ctrl Pts',(3.53794147178642,7.68369180485678,-34.7171983789205));
#77765=CARTESIAN_POINT('Ctrl Pts',(-3.15997262174759,7.22322793235497,-34.4525920440345));
#77766=CARTESIAN_POINT('Ctrl Pts',(-6.50947280185845,3.61738247470258,-34.2409069761259));
#77767=CARTESIAN_POINT('Ctrl Pts',(-7.46269518989241,0.0658180828906648,
-34.0821431751943));
#77768=CARTESIAN_POINT('Ctrl Pts',(-6.57583552253201,-3.49528465721146,
-33.9233793742629));
#77769=CARTESIAN_POINT('Ctrl Pts',(-3.28450664646774,-7.17220371196996,
-33.7116943063541));
#77770=CARTESIAN_POINT('Ctrl Pts',(2.05048368315385,-7.6193857840429,-33.5000092384455));
#77771=CARTESIAN_POINT('Ctrl Pts',(5.89467410338615,-4.53875024474639,-33.2883241705368));
#77772=CARTESIAN_POINT('Ctrl Pts',(7.88384083943231,-0.0582371100955341,
-33.0766391026281));
#77773=CARTESIAN_POINT('Ctrl Pts',(5.66162633057394,6.29351484807696,-32.8120327677422));
#77774=CARTESIAN_POINT('Ctrl Pts',(-2.24083336379937,8.15688760775168,-32.4945051658792));
#77775=CARTESIAN_POINT('Ctrl Pts',(-7.06885510459415,3.49166668558162,-32.2298988309934));
#77776=CARTESIAN_POINT('Ctrl Pts',(-7.30965514053794,-1.42395008789908,
-32.0182137630846));
#77777=CARTESIAN_POINT('Ctrl Pts',(-5.75203370239377,-4.75502469013619,
-31.8594499621531));
#77778=CARTESIAN_POINT('Ctrl Pts',(-2.78043735296234,-6.90853065279322,
-31.7006861612216));
#77779=CARTESIAN_POINT('Ctrl Pts',(2.10537683387303,-7.60236005356738,-31.4890010933129));
#77780=CARTESIAN_POINT('Ctrl Pts',(6.47508756137363,-4.50918663768756,-31.2773160254043));
#77781=CARTESIAN_POINT('Ctrl Pts',(7.43256476481124,0.323137101247964,-31.0656309574955));
#77782=CARTESIAN_POINT('Ctrl Pts',(6.06936753599808,5.03200910725189,-30.8539458895869));
#77783=CARTESIAN_POINT('Ctrl Pts',(0.279145278362542,8.46075763531737,-30.589339554701));
#77784=CARTESIAN_POINT('Ctrl Pts',(-6.96683105881335,4.79785520912865,-30.271811952838));
#77785=CARTESIAN_POINT('Ctrl Pts',(-7.65668338307411,-1.88033196651658,
-30.0072056179521));
#77786=CARTESIAN_POINT('Ctrl Pts',(-4.67565180448538,-5.79628953121159,
-29.7955205500434));
#77787=CARTESIAN_POINT('Ctrl Pts',(-1.33898046568837,-7.34188550917158,
-29.6367567491119));
#77788=CARTESIAN_POINT('Ctrl Pts',(2.32125200866079,-7.07604527731557,-29.4779929481804));
#77789=CARTESIAN_POINT('Ctrl Pts',(6.50612268408102,-4.46081355992071,-29.2663078802717));
#77790=CARTESIAN_POINT('Ctrl Pts',(7.85759813719054,0.719496056538602,-29.054622812363));
#77791=CARTESIAN_POINT('Ctrl Pts',(5.47852496562181,5.03320978803537,-28.8429377444543));
#77792=CARTESIAN_POINT('Ctrl Pts',(1.40341428637399,7.75814193498001,-28.6312526765456));
#77793=CARTESIAN_POINT('Ctrl Pts',(-5.23448241451663,6.65300952217338,-28.3666463416597));
#77794=CARTESIAN_POINT('Ctrl Pts',(-8.41970697715564,-0.815281564029267,
-28.0491187397968));
#77795=CARTESIAN_POINT('Ctrl Pts',(-4.6472869109242,-6.36892244422085,-27.7845124049108));
#77796=CARTESIAN_POINT('Ctrl Pts',(0.15504291279928,-7.44544517282956,-27.5728273370022));
#77797=CARTESIAN_POINT('Ctrl Pts',(3.70314588672555,-6.47941834263744,-27.4140635360706));
#77798=CARTESIAN_POINT('Ctrl Pts',(6.33238234358283,-3.91912764643002,-27.2552997351391));
#77799=CARTESIAN_POINT('Ctrl Pts',(7.85019446552089,0.776490083768835,-27.0436146672305));
#77800=CARTESIAN_POINT('Ctrl Pts',(5.54849119593889,5.61014870654456,-26.8319295993218));
#77801=CARTESIAN_POINT('Ctrl Pts',(0.950591926071428,7.37860498735393,-26.6202445314131));
#77802=CARTESIAN_POINT('Ctrl Pts',(-3.92188405481974,6.8393832618917,-26.4085594635044));
#77803=CARTESIAN_POINT('Ctrl Pts',(-8.28887171968077,1.719577699521,-26.1439531286185));
#77804=CARTESIAN_POINT('Ctrl Pts',(-5.9168782103298,-6.04538682417708,-25.8264255267555));
#77805=CARTESIAN_POINT('Ctrl Pts',(0.545474689815221,-7.86529758468923,
-25.5618191918696));
#77806=CARTESIAN_POINT('Ctrl Pts',(4.91289614305521,-5.5966189448607,-25.3501341239609));
#77807=CARTESIAN_POINT('Ctrl Pts',(7.00547873163074,-2.5728232076744,-25.1913703230294));
#77808=CARTESIAN_POINT('Ctrl Pts',(7.3684644288746,1.0790549637259,-25.0326065220979));
#77809=CARTESIAN_POINT('Ctrl Pts',(5.50612708594302,5.64898703398499,-24.8209214541893));
#77810=CARTESIAN_POINT('Ctrl Pts',(0.632619829400307,7.86506930753982,-24.6092363862805));
#77811=CARTESIAN_POINT('Ctrl Pts',(-4.0239434650627,6.25742083923526,-24.3975513183718));
#77812=CARTESIAN_POINT('Ctrl Pts',(-7.40462241471851,2.707379699625,-24.1858662504631));
#77813=CARTESIAN_POINT('Ctrl Pts',(-7.44902470697067,-4.02173753058972,
-23.9212599155773));
#77814=CARTESIAN_POINT('Ctrl Pts',(-0.634211270789191,-8.43527863640637,
-23.6037323137142));
#77815=CARTESIAN_POINT('Ctrl Pts',(5.48196409580995,-5.66643789211513,-23.3391259788284));
#77816=CARTESIAN_POINT('Ctrl Pts',(7.3625970416972,-1.1184171529497,-23.1274409109197));
#77817=CARTESIAN_POINT('Ctrl Pts',(7.01653254322224,2.54252287839892,-22.9686771099882));
#77818=CARTESIAN_POINT('Ctrl Pts',(4.94273135327337,5.5702813594737,-22.8099133090567));
#77819=CARTESIAN_POINT('Ctrl Pts',(0.57519857567604,7.86750510614556,-22.598228241148));
#77820=CARTESIAN_POINT('Ctrl Pts',(-4.58046582617219,6.42486232352286,-22.3865431732393));
#77821=CARTESIAN_POINT('Ctrl Pts',(-7.10796983245198,2.19640648111162,-22.1748581053306));
#77822=CARTESIAN_POINT('Ctrl Pts',(-7.40855804938307,-2.696591472844,-21.9631730374219));
#77823=CARTESIAN_POINT('Ctrl Pts',(-3.10951410581919,-7.87358011807365,
-21.698566702536));
#77824=CARTESIAN_POINT('Ctrl Pts',(4.94641764083134,-6.86214996428105,-21.3810391006731));
#77825=CARTESIAN_POINT('Ctrl Pts',(7.84294450647332,-0.805400646465767,
-21.1164327657871));
#77826=CARTESIAN_POINT('Ctrl Pts',(6.35323936598892,3.88523380054131,-20.9047476978785));
#77827=CARTESIAN_POINT('Ctrl Pts',(3.73111407493928,6.46335356274661,-20.7459838969469));
#77828=CARTESIAN_POINT('Ctrl Pts',(0.194828916586261,7.44450598411966,-20.5872200960154));
#77829=CARTESIAN_POINT('Ctrl Pts',(-4.62596685695389,6.38975121855693,-20.3755350281067));
#77830=CARTESIAN_POINT('Ctrl Pts',(-7.64157990149821,1.96615860753231,-20.163849960198));
#77831=CARTESIAN_POINT('Ctrl Pts',(-6.85256530936594,-2.89651260142109,
-19.9521648922894));
#77832=CARTESIAN_POINT('Ctrl Pts',(-3.93184193858918,-6.83366350594211,
-19.7404798243806));
#77833=CARTESIAN_POINT('Ctrl Pts',(2.69089288404973,-8.02629661404211,-19.4758734894948));
#77834=CARTESIAN_POINT('Ctrl Pts',(8.20314531815434,-2.06508026455434,-19.1583458876318));
#77835=CARTESIAN_POINT('Ctrl Pts',(6.51919189567336,4.43402590884787,-18.8937395527459));
#77836=CARTESIAN_POINT('Ctrl Pts',(2.35903449854064,7.0635436121762,-18.6820544848372));
#77837=CARTESIAN_POINT('Ctrl Pts',(-1.30723777536977,7.34760375332838,-18.5232906839057));
#77838=CARTESIAN_POINT('Ctrl Pts',(-4.64460706874297,5.82118998412822,-18.3645268829742));
#77839=CARTESIAN_POINT('Ctrl Pts',(-7.65378364228116,1.90999632298988,-18.1528418150655));
#77840=CARTESIAN_POINT('Ctrl Pts',(-7.11256506848367,-3.41627592672793,
-17.9411567471568));
#77841=CARTESIAN_POINT('Ctrl Pts',(-3.37772277338639,-6.62860659833298,
-17.7294716792481));
#77842=CARTESIAN_POINT('Ctrl Pts',(1.39211251672382,-7.76017787703827,-17.5177866113394));
#77843=CARTESIAN_POINT('Ctrl Pts',(7.227078017077,-4.40813851700414,-17.2531802764535));
#77844=CARTESIAN_POINT('Ctrl Pts',(7.6059122274626,3.70219513234312,-16.9356526745905));
#77845=CARTESIAN_POINT('Ctrl Pts',(2.13262510438074,7.59028055457192,-16.6710463397047));
#77846=CARTESIAN_POINT('Ctrl Pts',(-2.74348017632364,6.92329463828742,-16.459361271796));
#77847=CARTESIAN_POINT('Ctrl Pts',(-5.73142970221724,4.77983944142699,-16.3005974708645));
#77848=CARTESIAN_POINT('Ctrl Pts',(-7.3019369555535,1.46299157600233,-16.1418336699329));
#77849=CARTESIAN_POINT('Ctrl Pts',(-7.08573801871702,-3.46710350678975,
-15.9301486020242));
#77850=CARTESIAN_POINT('Ctrl Pts',(-3.24196043414937,-7.19369276549707,
-15.7184635341156));
#77851=CARTESIAN_POINT('Ctrl Pts',(1.68402460811039,-7.24648174555041,-15.5067784662069));
#77852=CARTESIAN_POINT('Ctrl Pts',(6.06203162144491,-5.04084423118742,-15.2950933982982));
#77853=CARTESIAN_POINT('Ctrl Pts',(8.36787344713815,1.28102920446546,-15.0304870634123));
#77854=CARTESIAN_POINT('Ctrl Pts',(3.43530743692631,7.73012370040796,-14.7129594615493));
#77855=CARTESIAN_POINT('Ctrl Pts',(-3.25588096342051,7.18050749494654,-14.4483531266634));
#77856=CARTESIAN_POINT('Ctrl Pts',(-6.55706669530387,3.53037795140363,-14.2366680587547));
#77857=CARTESIAN_POINT('Ctrl Pts',(-7.46290994832736,-0.033565166995917,
-14.0779042578232));
#77858=CARTESIAN_POINT('Ctrl Pts',(-6.52870728675789,-3.58254222838565,
-13.9191404568917));
#77859=CARTESIAN_POINT('Ctrl Pts',(-3.18870634438395,-7.21530608123946,
-13.707455388983));
#77860=CARTESIAN_POINT('Ctrl Pts',(2.15176586145997,-7.59140479347599,-13.4957703210743));
#77861=CARTESIAN_POINT('Ctrl Pts',(5.95459195800815,-4.45985102698973,-13.2840852531656));
#77862=CARTESIAN_POINT('Ctrl Pts',(7.88391730271688,0.046753678088791,-13.0724001852569));
#77863=CARTESIAN_POINT('Ctrl Pts',(5.57731636225459,6.36835018237381,-12.8077938503711));
#77864=CARTESIAN_POINT('Ctrl Pts',(-2.34925633818179,8.1263241547038,-12.4902662485081));
#77865=CARTESIAN_POINT('Ctrl Pts',(-7.11472529640173,3.39722426249561,-12.2256599136221));
#77866=CARTESIAN_POINT('Ctrl Pts',(-7.2900448845705,-1.52116327439485,-12.0139748457135));
#77867=CARTESIAN_POINT('Ctrl Pts',(-5.68820311124292,-4.83120035628055,
-11.855211044782));
#77868=CARTESIAN_POINT('Ctrl Pts',(-2.68819296394879,-6.94494393374836,
-11.6964472438505));
#77869=CARTESIAN_POINT('Ctrl Pts',(2.20642742071403,-7.57364958483073,-11.4847621759418));
#77870=CARTESIAN_POINT('Ctrl Pts',(6.53456026565597,-4.42256093179789,-11.2730771080331));
#77871=CARTESIAN_POINT('Ctrl Pts',(7.42760265059398,0.422084629198934,-11.0613920401244));
#77872=CARTESIAN_POINT('Ctrl Pts',(6.00182032800683,5.11238600780666,-10.8497069722157));
#77873=CARTESIAN_POINT('Ctrl Pts',(0.166452356394491,8.46372468024947,-10.5851006373298));
#77874=CARTESIAN_POINT('Ctrl Pts',(-7.03010423234284,4.7046555763631,-10.2675730354668));
#77875=CARTESIAN_POINT('Ctrl Pts',(-7.63096492057063,-1.98212590769799,
-10.0029667005809));
#77876=CARTESIAN_POINT('Ctrl Pts',(-4.59805059163296,-5.85803916709372,
-9.79128163267221));
#77877=CARTESIAN_POINT('Ctrl Pts',(-1.24109309452522,-7.3590651205164,-9.6325178317407));
#77878=CARTESIAN_POINT('Ctrl Pts',(2.41527475272299,-7.04450676223615,-9.47375403080917));
#77879=CARTESIAN_POINT('Ctrl Pts',(6.56494847360213,-4.37377886222366,-9.26206896290048));
#77880=CARTESIAN_POINT('Ctrl Pts',(7.84732019852157,0.824068421206676,-9.0503838949918));
#77881=CARTESIAN_POINT('Ctrl Pts',(5.41101415828665,5.105718592729,-8.83869882708312));
#77882=CARTESIAN_POINT('Ctrl Pts',(1.29997809904393,7.77614267387747,-8.62701375917442));
#77883=CARTESIAN_POINT('Ctrl Pts',(-5.32261346430697,6.58271431550789,-8.36240742428857));
#77884=CARTESIAN_POINT('Ctrl Pts',(-8.40810366342223,-0.927330790472802,
-8.04487982242553));
#77885=CARTESIAN_POINT('Ctrl Pts',(-4.5620627137284,-6.43024358239611,-7.78027348753966));
#77886=CARTESIAN_POINT('Ctrl Pts',(0.254176868243534,-7.44272035253782,
-7.56858841963099));
#77887=CARTESIAN_POINT('Ctrl Pts',(3.78910108201798,-6.42953065997176,-7.40982461869945));
#77888=CARTESIAN_POINT('Ctrl Pts',(6.38401014661282,-3.83445460297475,-7.25106081776795));
#77889=CARTESIAN_POINT('Ctrl Pts',(7.8391582190614,0.88095880339981,-7.03937574985924));
#77890=CARTESIAN_POINT('Ctrl Pts',(5.47329134412917,5.68353806382972,-6.82769068195057));
#77891=CARTESIAN_POINT('Ctrl Pts',(0.852250015990716,7.39060934428252,-6.61600561404187));
#77892=CARTESIAN_POINT('Ctrl Pts',(-4.01261334852559,6.78655082184165,-6.40432054613319));
#77893=CARTESIAN_POINT('Ctrl Pts',(-8.31103560754686,1.60904598428258,-6.13971421124732));
#77894=CARTESIAN_POINT('Ctrl Pts',(-5.83584982033124,-6.12364323641863,
-5.82218660938429));
#77895=CARTESIAN_POINT('Ctrl Pts',(0.650165015118219,-7.85733632873061,
-5.55758027449843));
#77896=CARTESIAN_POINT('Ctrl Pts',(4.98698822100662,-5.53069983016105,-5.34589520658973));
#77897=CARTESIAN_POINT('Ctrl Pts',(7.03911871088246,-2.47930621227326,-5.18713140565822));
#77898=CARTESIAN_POINT('Ctrl Pts',(7.353441773466,1.17708186789058,-5.02836760472671));
#77899=CARTESIAN_POINT('Ctrl Pts',(5.43041379954702,5.72180880621457,-4.816682536818));
#77900=CARTESIAN_POINT('Ctrl Pts',(0.527828079749971,7.87279623069239,-4.60499746890933));
#77901=CARTESIAN_POINT('Ctrl Pts',(-4.10691396866242,6.20328092769522,-4.39331240100062));
#77902=CARTESIAN_POINT('Ctrl Pts',(-7.44001884079827,2.60853553899251,-4.18162733309195));
#77903=CARTESIAN_POINT('Ctrl Pts',(-7.39480848519591,-4.1205762644595,-3.91702099820607));
#77904=CARTESIAN_POINT('Ctrl Pts',(-0.521826194395602,-8.44297625313128,
-3.59949339634306));
#77905=CARTESIAN_POINT('Ctrl Pts',(5.55693552491327,-5.59293446557778,-3.33488706145718));
#77906=CARTESIAN_POINT('Ctrl Pts',(7.37683758691506,-1.02027366322683,-3.1232019935485));
#77907=CARTESIAN_POINT('Ctrl Pts',(6.98205292519039,2.63573378257931,-2.96443819261698));
#77908=CARTESIAN_POINT('Ctrl Pts',(4.86811576200549,5.63560708473504,-2.80567439168545));
#77909=CARTESIAN_POINT('Ctrl Pts',(0.470380277749741,7.87446837668858,-2.59398932377678));
#77910=CARTESIAN_POINT('Ctrl Pts',(-4.66561825254938,6.36329427350808,-2.38230425586808));
#77911=CARTESIAN_POINT('Ctrl Pts',(-7.13658637022202,2.10156075002914,-2.17061918795939));
#77912=CARTESIAN_POINT('Ctrl Pts',(-7.37199597901472,-2.79501521255998,
-1.9589341200507));
#77913=CARTESIAN_POINT('Ctrl Pts',(-3.00438054821123,-7.914276477521,-1.69432778516484));
#77914=CARTESIAN_POINT('Ctrl Pts',(5.03734365599351,-6.79569608394466,-1.37680018330181));
#77915=CARTESIAN_POINT('Ctrl Pts',(7.85300067508422,-0.700847833672291,
-1.11219384841594));
#77916=CARTESIAN_POINT('Ctrl Pts',(6.30090148669033,3.96943667741106,-0.900508780507268));
#77917=CARTESIAN_POINT('Ctrl Pts',(3.64479345598366,6.51258800445165,-0.741744979575735));
#77918=CARTESIAN_POINT('Ctrl Pts',(0.0955276237381259,7.44621302766392,
-0.582981178644231));
#77919=CARTESIAN_POINT('Ctrl Pts',(-4.71030661113408,6.32810132960302,-0.371296110735536));
#77920=CARTESIAN_POINT('Ctrl Pts',(-7.66773584340214,1.86323026021221,-0.159611042826847));
#77921=CARTESIAN_POINT('Ctrl Pts',(-6.81262520422293,-2.98634583944321,
0.0520740250818385));
#77922=CARTESIAN_POINT('Ctrl Pts',(-3.84226758436661,-6.88813227096892,
0.263759092990537));
#77923=CARTESIAN_POINT('Ctrl Pts',(2.80126517201592,-7.98399944675405,0.528365427876391));
#77924=CARTESIAN_POINT('Ctrl Pts',(8.22361795704757,-1.96563912835421,0.845893029739429));
#77925=CARTESIAN_POINT('Ctrl Pts',(6.11747873359508,5.83678708112643,1.16342063160247));
#77926=CARTESIAN_POINT('Ctrl Pts',(-1.59680123828806,8.30912507639158,1.4809482334655));
#77927=CARTESIAN_POINT('Ctrl Pts',(-6.78649111104133,4.01907013773023,1.74555456835137));
#77928=CARTESIAN_POINT('Ctrl Pts',(-7.38999319219831,-0.847422129305244,
1.95723963626005));
#77929=CARTESIAN_POINT('Ctrl Pts',(-5.68863521383442,-5.46856739655706,
2.16892470416873));
#77930=CARTESIAN_POINT('Ctrl Pts',(-0.886184247744874,-7.83878385259253,
2.38060977207743));
#77931=CARTESIAN_POINT('Ctrl Pts',(3.82950340562284,-6.3867141509991,2.59229483998611));
#77932=CARTESIAN_POINT('Ctrl Pts',(6.42686542591582,-3.79390598851325,2.75105864091764));
#77933=CARTESIAN_POINT('Ctrl Pts',(7.44247115572417,-0.259634699464653,
2.90982244184915));
#77934=CARTESIAN_POINT('Ctrl Pts',(6.43364876941854,4.55729862973626,3.12150750975785));
#77935=CARTESIAN_POINT('Ctrl Pts',(0.933504659789757,8.40743036986156,3.38611384464369));
#77936=CARTESIAN_POINT('Ctrl Pts',(-6.57877351294465,5.32745846595636,3.70364144650676));
#77937=CARTESIAN_POINT('Ctrl Pts',(-7.77710587116025,-1.2942407124703,3.96824778139258));
#77938=CARTESIAN_POINT('Ctrl Pts',(-5.10970404230305,-5.40724950467182,
4.1799328493013));
#77939=CARTESIAN_POINT('Ctrl Pts',(-0.829856799302938,-7.84670920720481,
4.39161791720997));
#77940=CARTESIAN_POINT('Ctrl Pts',(4.36893838930713,-6.56817228546896,4.60330298511867));
#77941=CARTESIAN_POINT('Ctrl Pts',(7.04272340848429,-2.4204679872681,4.81498805302735));
#77942=CARTESIAN_POINT('Ctrl Pts',(7.3599785283304,1.23566649436854,4.97375185395888));
#77943=CARTESIAN_POINT('Ctrl Pts',(5.8614277476127,4.59373006293499,5.13251565489037));
#77944=CARTESIAN_POINT('Ctrl Pts',(1.98775206194297,7.62950130116858,5.34420072279909));
#77945=CARTESIAN_POINT('Ctrl Pts',(-4.69947080153288,7.03357126740298,5.60880705768493));
#77946=CARTESIAN_POINT('Ctrl Pts',(-8.46384507724044,-0.160211711261087,
5.92633465954799));
#77947=CARTESIAN_POINT('Ctrl Pts',(-5.11680999772523,-5.99804913757792,
6.19094099443383));
#77948=CARTESIAN_POINT('Ctrl Pts',(-0.427561153418098,-7.42728941633418,
6.40262606234254));
#77949=CARTESIAN_POINT('Ctrl Pts',(4.41774155119458,-6.53781940394695,6.61431113025119));
#77950=CARTESIAN_POINT('Ctrl Pts',(7.57202064866731,-2.21201115398199,6.82599619815993));
#77951=CARTESIAN_POINT('Ctrl Pts',(6.94692414850596,2.68307147023272,7.03768126606858));
#77952=CARTESIAN_POINT('Ctrl Pts',(4.83539316593233,5.68463934220696,7.19644506700012));
#77953=CARTESIAN_POINT('Ctrl Pts',(1.5265380798821,7.28892129320051,7.35520886793162));
#77954=CARTESIAN_POINT('Ctrl Pts',(-3.39197738907421,7.11722826117605,7.56689393584032));
#77955=CARTESIAN_POINT('Ctrl Pts',(-8.12458975238406,2.3552475385514,7.83150027072619));
#77956=CARTESIAN_POINT('Ctrl Pts',(-6.37246081249254,-5.57261922642259,
8.14902787258922));
#77957=CARTESIAN_POINT('Ctrl Pts',(-0.052566768797828,-7.88388068637668,
8.41363420747508));
#77958=CARTESIAN_POINT('Ctrl Pts',(4.45545927411695,-5.95787875222696,8.62531927538377));
#77959=CARTESIAN_POINT('Ctrl Pts',(7.58981615343419,-2.15736269963801,8.83700434329246));
#77960=CARTESIAN_POINT('Ctrl Pts',(7.21765527083583,3.18338536594938,9.04868941120114));
#77961=CARTESIAN_POINT('Ctrl Pts',(3.58735511151804,6.52606397135328,9.26037447910983));
#77962=CARTESIAN_POINT('Ctrl Pts',(0.0390678369844106,7.46288317082481,
9.41913828004134));
#77963=CARTESIAN_POINT('Ctrl Pts',(-3.52554222430388,6.55966799091853,9.57790208097286));
#77964=CARTESIAN_POINT('Ctrl Pts',(-7.17810486177338,3.26117453171754,9.78958714888157));
#77965=CARTESIAN_POINT('Ctrl Pts',(-7.73265457814575,-3.42960679741785,
10.0541934837674));
#77966=CARTESIAN_POINT('Ctrl Pts',(-1.28719879835849,-8.36692662233385,
10.3717210856304));
#77967=CARTESIAN_POINT('Ctrl Pts',(5.03637310113398,-6.06574677419579,10.6363274205163));
#77968=CARTESIAN_POINT('Ctrl Pts',(7.24523808218346,-1.68936724894143,10.848012488425));
#77969=CARTESIAN_POINT('Ctrl Pts',(7.19608122716862,3.236655377538,11.0596975563337));
#77970=CARTESIAN_POINT('Ctrl Pts',(3.47232714063519,7.08317966912418,11.2713826242423));
#77971=CARTESIAN_POINT('Ctrl Pts',(-1.45760719053445,7.30301368836414,11.483067692151));
#77972=CARTESIAN_POINT('Ctrl Pts',(-4.77561214732757,5.73495249636615,11.6418314930825));
#77973=CARTESIAN_POINT('Ctrl Pts',(-6.92126988705709,2.74858423137024,11.8005952940141));
#77974=CARTESIAN_POINT('Ctrl Pts',(-7.59185095453138,-2.12702793050032,
12.0122803619227));
#77975=CARTESIAN_POINT('Ctrl Pts',(-3.70780224593713,-7.60318039473171,
12.2768866968086));
#77976=CARTESIAN_POINT('Ctrl Pts',(4.40280852720821,-7.23032633584101,12.5944142986716));
#77977=CARTESIAN_POINT('Ctrl Pts',(7.75914931159707,-1.39783400403488,12.8590206335575));
#77978=CARTESIAN_POINT('Ctrl Pts',(6.63109531620007,3.37283433876996,13.0707057014662));
#77979=CARTESIAN_POINT('Ctrl Pts',(3.42151935496463,7.11004418865015,13.2823907693749));
#77980=CARTESIAN_POINT('Ctrl Pts',(-1.90435238645548,7.65518987255624,13.4940758372836));
#77981=CARTESIAN_POINT('Ctrl Pts',(-5.81776376141959,4.64889798453833,13.7057609051923));
#77982=CARTESIAN_POINT('Ctrl Pts',(-7.34663788131966,1.31265507961464,13.8645247061238));
#77983=CARTESIAN_POINT('Ctrl Pts',(-7.06528109532774,-2.35382564571477,
14.0232885070553));
#77984=CARTESIAN_POINT('Ctrl Pts',(-4.43883154447283,-6.51592075249081,
14.234973574964));
#77985=CARTESIAN_POINT('Ctrl Pts',(2.05903122121148,-8.20466574821215,14.4995799098498));
#77986=CARTESIAN_POINT('Ctrl Pts',(8.02431033753216,-2.696810237482,14.8171075117129));
#77987=CARTESIAN_POINT('Ctrl Pts',(6.83656074059215,3.92680215731425,15.0817138465987));
#77988=CARTESIAN_POINT('Ctrl Pts',(2.90156446352231,6.85042774090353,15.2933989145075));
#77989=CARTESIAN_POINT('Ctrl Pts',(-1.96052365399983,7.64302754561716,15.5050839824161));
#77990=CARTESIAN_POINT('Ctrl Pts',(-6.38633858541117,4.63067699901154,15.7167690503248));
#77991=CARTESIAN_POINT('Ctrl Pts',(-7.44464761501319,-0.189339754436876,
15.9284541182335));
#77992=CARTESIAN_POINT('Ctrl Pts',(-6.46610289399227,-3.72634739142553,
16.087217919165));
#77993=CARTESIAN_POINT('Ctrl Pts',(-3.88991722241724,-6.35037291260615,
16.2459817200965));
#77994=CARTESIAN_POINT('Ctrl Pts',(0.799617534905987,-7.84353622614305,
16.4576667880052));
#77995=CARTESIAN_POINT('Ctrl Pts',(6.85850092252447,-4.95147601282085,16.7222731228911));
#77996=CARTESIAN_POINT('Ctrl Pts',(7.87587073736038,3.10370777915764,17.0398007247542));
#77997=CARTESIAN_POINT('Ctrl Pts',(2.70205334327046,7.40656773901479,17.30440705964));
#77998=CARTESIAN_POINT('Ctrl Pts',(-2.19116491540037,7.10958739188392,17.5160921275487));
#77999=CARTESIAN_POINT('Ctrl Pts',(-6.42148323042302,4.58520186931298,17.7277771954574));
#78000=CARTESIAN_POINT('Ctrl Pts',(-7.86792708265074,-0.569397417255415,
17.9394622633661));
#78001=CARTESIAN_POINT('Ctrl Pts',(-5.57392430365033,-4.93862283551883,
18.1511473312747));
#78002=CARTESIAN_POINT('Ctrl Pts',(-2.54769573582305,-7.01465593988385,
18.3099111322063));
#78003=CARTESIAN_POINT('Ctrl Pts',(1.11298813422668,-7.36341969057114,18.4686749331378));
#78004=CARTESIAN_POINT('Ctrl Pts',(5.6623942972133,-5.48614067955183,18.6803600010465));
#78005=CARTESIAN_POINT('Ctrl Pts',(8.43574397081144,0.627991455935019,18.9449663359324));
#78006=CARTESIAN_POINT('Ctrl Pts',(4.02722887835911,7.44605730647597,19.2624939377953));
#78007=CARTESIAN_POINT('Ctrl Pts',(-2.70191926211008,7.40661665293494,19.5271002726813));
#78008=CARTESIAN_POINT('Ctrl Pts',(-6.25445213614084,4.02855619869448,19.7387853405899));
#78009=CARTESIAN_POINT('Ctrl Pts',(-7.86553362351802,-0.62682045137493,
19.9504704084987));
#78010=CARTESIAN_POINT('Ctrl Pts',(-5.6530453692469,-5.50196038243845,20.1621554764072));
#78011=CARTESIAN_POINT('Ctrl Pts',(-1.08448771134512,-7.36766679880903,
20.373840544316));
#78012=CARTESIAN_POINT('Ctrl Pts',(2.56765711011421,-7.00737386487682,20.5326043452475));
#78013=CARTESIAN_POINT('Ctrl Pts',(5.59299496375529,-4.91702140140031,20.6913681461791));
#78014=CARTESIAN_POINT('Ctrl Pts',(7.86489324800924,-0.551273915912889,
20.9030532140877));
#78015=CARTESIAN_POINT('Ctrl Pts',(6.04974791365749,5.9124191149653,21.1676595489736));
#78016=CARTESIAN_POINT('Ctrl Pts',(-1.71346554085533,8.29013737463471,21.4851871508366));
#78017=CARTESIAN_POINT('Ctrl Pts',(-6.83648965277288,3.92692591858082,21.7497934857225));
#78018=CARTESIAN_POINT('Ctrl Pts',(-7.37930388813884,-0.94515114971917,
21.9614785536312));
#78019=CARTESIAN_POINT('Ctrl Pts',(-5.61423828898686,-5.54435311785144,
22.1731636215399));
#78020=CARTESIAN_POINT('Ctrl Pts',(-0.782278110981478,-7.84961979676501,
22.3848486894485));
#78021=CARTESIAN_POINT('Ctrl Pts',(3.91445748172455,-6.33527033978052,22.5965337573573));
#78022=CARTESIAN_POINT('Ctrl Pts',(6.47668611509837,-3.70792239451836,22.7552975582887));
#78023=CARTESIAN_POINT('Ctrl Pts',(7.44532883004716,-0.160532672340616,
22.9140613592203));
#78024=CARTESIAN_POINT('Ctrl Pts',(6.37234732920244,4.64258960591542,23.1257464271289));
#78025=CARTESIAN_POINT('Ctrl Pts',(0.821489503303927,8.41910355119662,23.3903527620148));
#78026=CARTESIAN_POINT('Ctrl Pts',(-6.64914813647221,5.23938650122914,23.7078803638778));
#78027=CARTESIAN_POINT('Ctrl Pts',(-7.75917461524326,-1.39769354032214,
23.9724866987637));
#78028=CARTESIAN_POINT('Ctrl Pts',(-5.03724793862302,-5.47481230492465,
24.1841717666724));
#78029=CARTESIAN_POINT('Ctrl Pts',(-0.725289558244549,-7.85706549022317,
24.3958568345811));
#78030=CARTESIAN_POINT('Ctrl Pts',(4.45601514279779,-6.50941003807893,24.6075419024897));
#78031=CARTESIAN_POINT('Ctrl Pts',(7.07433180898348,-2.32646880717035,24.8192269703985));
#78032=CARTESIAN_POINT('Ctrl Pts',(7.34287079315154,1.33356665838692,24.97799077133));
#78033=CARTESIAN_POINT('Ctrl Pts',(5.79973548633705,4.67137671516041,25.1367545722615));
#78034=CARTESIAN_POINT('Ctrl Pts',(1.88597701080095,7.65529486353575,25.3484396401702));
#78035=CARTESIAN_POINT('Ctrl Pts',(-4.79271700308801,6.97036680083047,25.613045975056));
#78036=CARTESIAN_POINT('Ctrl Pts',(-8.46096115952763,-0.27290677342026,
25.9305735769191));
#78037=CARTESIAN_POINT('Ctrl Pts',(-5.03648290821302,-6.06565559999674,
26.1951799118049));
#78038=CARTESIAN_POINT('Ctrl Pts',(-0.328617317895261,-7.43232448347727,
26.4068649797136));
#78039=CARTESIAN_POINT('Ctrl Pts',(4.50441109075738,-6.47841059106454,26.6185500476223));
#78040=CARTESIAN_POINT('Ctrl Pts',(7.60080561490422,-2.11098176238599,26.830235115531));
#78041=CARTESIAN_POINT('Ctrl Pts',(6.91057889396949,2.77534268236474,27.0419201834397));
#78042=CARTESIAN_POINT('Ctrl Pts',(4.75926458443607,5.74852608349403,27.2006839843712));
#78043=CARTESIAN_POINT('Ctrl Pts',(1.42933937950413,7.30860322254663,27.3594477853027));
#78044=CARTESIAN_POINT('Ctrl Pts',(-3.48645360850935,7.07142771784166,27.5711328532114));
#78045=CARTESIAN_POINT('Ctrl Pts',(-8.15523314124773,2.24684712913524,27.8357391880973));
#78046=CARTESIAN_POINT('Ctrl Pts',(-6.29768766347067,-5.65698435063977,
28.1532667899603));
#78047=CARTESIAN_POINT('Ctrl Pts',(0.0524240472627744,-7.88388163671697,
28.4178731248462));
#78048=CARTESIAN_POINT('Ctrl Pts',(4.53440265005737,-5.89801908919164,28.6295581927548));
#78049=CARTESIAN_POINT('Ctrl Pts',(7.61787181549885,-2.05610118028825,28.8412432606637));
#78050=CARTESIAN_POINT('Ctrl Pts',(7.17462355037663,3.27921742296345,29.0529283285722));
#78051=CARTESIAN_POINT('Ctrl Pts',(3.5001323134553,6.57325653254444,29.264613396481));
#78052=CARTESIAN_POINT('Ctrl Pts',(-0.0603155442375287,7.46274169138947,
29.4233771974124));
#78053=CARTESIAN_POINT('Ctrl Pts',(-3.61258181668668,6.5121382620584,29.582140998344));
#78054=CARTESIAN_POINT('Ctrl Pts',(-7.22089600433169,3.16529771547212,29.7938260662526));
#78055=CARTESIAN_POINT('Ctrl Pts',(-7.68629837108023,-3.53227504032997,
30.0584324011386));
#78056=CARTESIAN_POINT('Ctrl Pts',(-1.17566599913336,-8.38332579043041,
30.3759600030015));
#78057=CARTESIAN_POINT('Ctrl Pts',(5.1167013986517,-5.99814177387708,30.6405663378874));
#78058=CARTESIAN_POINT('Ctrl Pts',(7.26709220913254,-1.59273582030463,30.8522514057961));
#78059=CARTESIAN_POINT('Ctrl Pts',(7.15234204646914,3.33219541912908,31.0639364737048));
#78060=CARTESIAN_POINT('Ctrl Pts',(3.3776956784777,7.12879105460941,31.2756215416134));
#78061=CARTESIAN_POINT('Ctrl Pts',(-1.55472895139519,7.28295582452796,31.4873066095222));
#78062=CARTESIAN_POINT('Ctrl Pts',(-4.85155852512464,5.67084926572459,31.6460704104537));
#78063=CARTESIAN_POINT('Ctrl Pts',(-6.95725786448992,2.65617302399775,31.8048342113852));
#78064=CARTESIAN_POINT('Ctrl Pts',(-7.56285309954371,-2.22793665252618,
32.0165192792939));
#78065=CARTESIAN_POINT('Ctrl Pts',(-3.60622528451092,-7.65188139003492,
32.2811256141798));
#78066=CARTESIAN_POINT('Ctrl Pts',(4.49870119380519,-7.17105497251761,32.5986532160427));
#78067=CARTESIAN_POINT('Ctrl Pts',(7.77707565101753,-1.29438489671535,32.8632595509287));
#78068=CARTESIAN_POINT('Ctrl Pts',(6.58559279735529,3.46083863777819,33.0749446188373));
#78069=CARTESIAN_POINT('Ctrl Pts',(3.32653465496305,7.15497660724926,33.2866296867461));
#78070=CARTESIAN_POINT('Ctrl Pts',(-2.00612430934377,7.62915167316433,33.4983147546547));
#78071=CARTESIAN_POINT('Ctrl Pts',(-5.87915522440015,4.5710131810946,33.7099998225634));
#78072=CARTESIAN_POINT('Ctrl Pts',(-7.36346650774268,1.21470675746504,33.8687636234949));
#78073=CARTESIAN_POINT('Ctrl Pts',(-7.03330976597137,-2.44770215964113,
34.0275274244265));
#78074=CARTESIAN_POINT('Ctrl Pts',(-4.35166831935865,-6.57445294843889,
34.2392124923351));
#78075=CARTESIAN_POINT('Ctrl Pts',(2.16810655624256,-8.17651903749918,34.503818827221));
#78076=CARTESIAN_POINT('Ctrl Pts',(8.05951105775482,-2.58971491866223,34.821346429084));
#78077=CARTESIAN_POINT('Ctrl Pts',(6.78366305865034,4.01749342864384,35.08595276397));
#78078=CARTESIAN_POINT('Ctrl Pts',(2.81008306505412,6.88845917000401,35.2976378318785));
#78079=CARTESIAN_POINT('Ctrl Pts',(-2.0621286358887,7.61624241670414,35.5093228997874));
#78080=CARTESIAN_POINT('Ctrl Pts',(-6.44743699245361,4.54522235154967,35.7210079676959));
#78081=CARTESIAN_POINT('Ctrl Pts',(-7.44146614955639,-0.288460048080047,
35.9326930356047));
#78082=CARTESIAN_POINT('Ctrl Pts',(-6.41590742781489,-3.81212321351088,
36.0914568365361));
#78083=CARTESIAN_POINT('Ctrl Pts',(-3.80500719656959,-6.40161013811945,
36.2502206374678));
#78084=CARTESIAN_POINT('Ctrl Pts',(0.903995539004252,-7.83219259201457,
36.4619057053764));
#78085=CARTESIAN_POINT('Ctrl Pts',(6.92382940196311,-4.85970534315815,36.7265120402622));
#78086=CARTESIAN_POINT('Ctrl Pts',(7.83384168462113,3.2083120656049,37.0440396421253));
#78087=CARTESIAN_POINT('Ctrl Pts',(2.60318376473262,7.44189305415814,37.3086459770111));
#78088=CARTESIAN_POINT('Ctrl Pts',(-2.28564585970917,7.07977821498037,37.5203310449198));
#78089=CARTESIAN_POINT('Ctrl Pts',(-6.48197294900942,4.4992832483924,37.7320161128285));
#78090=CARTESIAN_POINT('Ctrl Pts',(-7.85964702536755,-0.67412063706526,
37.9437011807372));
#78091=CARTESIAN_POINT('Ctrl Pts',(-5.50766460996938,-5.01241041799476,
38.1553862486459));
#78092=CARTESIAN_POINT('Ctrl Pts',(-2.45405876029574,-7.04796049352537,
38.3141500495774));
#78093=CARTESIAN_POINT('Ctrl Pts',(1.21094485225064,-7.34794561025246,38.4729138505089));
#78094=CARTESIAN_POINT('Ctrl Pts',(5.73494872765964,-5.41025062488443,38.6845989184177));
#78095=CARTESIAN_POINT('Ctrl Pts',(8.42663329468905,0.740270846816575,38.9492052533034));
#78096=CARTESIAN_POINT('Ctrl Pts',(3.92771593232857,7.49902589707133,39.2667328551665));
#78097=CARTESIAN_POINT('Ctrl Pts',(-2.80031032559594,7.36997964874085,39.5313391900524));
#78098=CARTESIAN_POINT('Ctrl Pts',(-6.30754406085944,3.94491121441702,39.7430242579611));
#78099=CARTESIAN_POINT('Ctrl Pts',(-7.85648910129288,-0.731506706887516,
39.9547093258698));
#78100=CARTESIAN_POINT('Ctrl Pts',(-5.57927694280141,-5.57675163443824,
40.1663943937784));
#78101=CARTESIAN_POINT('Ctrl Pts',(-0.986279587833537,-7.38145515660392,
40.3780794616871));
#78102=CARTESIAN_POINT('Ctrl Pts',(2.66074353875926,-6.97256017100103,40.5368432626186));
#78103=CARTESIAN_POINT('Ctrl Pts',(5.65797683787586,-4.84210597038945,40.6956070635502));
#78104=CARTESIAN_POINT('Ctrl Pts',(7.87153694461785,-0.446491727206108,
40.9072921314589));
#78105=CARTESIAN_POINT('Ctrl Pts',(5.9704784143324,5.99245668434905,41.1718984663447));
#78106=CARTESIAN_POINT('Ctrl Pts',(-1.82370970482655,8.26658483066225,41.4894260682078));
#78107=CARTESIAN_POINT('Ctrl Pts',(-6.8881766031114,3.83553920939982,41.7540324030937));
#78108=CARTESIAN_POINT('Ctrl Pts',(-7.36606341032977,-1.04333427256905,
41.9657174710023));
#78109=CARTESIAN_POINT('Ctrl Pts',(-5.53990877821464,-5.61862383417993,
42.177402538911));
#78110=CARTESIAN_POINT('Ctrl Pts',(-0.677678829097026,-7.85934102843741,
42.3890876068197));
#78111=CARTESIAN_POINT('Ctrl Pts',(3.99847438491617,-6.28258149549219,42.6007726747284));
#78112=CARTESIAN_POINT('Ctrl Pts',(6.52548859581569,-3.62134644892725,42.7595364756599));
#78113=CARTESIAN_POINT('Ctrl Pts',(7.44680640067528,-0.0613722843181,42.9183002765914));
#78114=CARTESIAN_POINT('Ctrl Pts',(6.30995898361038,4.72703568403096,43.1299853445001));
#78115=CARTESIAN_POINT('Ctrl Pts',(0.709303181088316,8.42929644793126,43.394591679386));
#78116=CARTESIAN_POINT('Ctrl Pts',(-6.71832915581128,5.15037816128001,43.712119281249));
#78117=CARTESIAN_POINT('Ctrl Pts',(-7.73987414754349,-1.50089510715489,
43.9767256161348));
#78118=CARTESIAN_POINT('Ctrl Pts',(-4.96389563344953,-5.54140566188194,
44.1884106840436));
#78119=CARTESIAN_POINT('Ctrl Pts',(-0.620596178485482,-7.86602717031948,
44.4000957519522));
#78120=CARTESIAN_POINT('Ctrl Pts',(4.54230296786022,-6.44949406890597,44.6117808198609));
#78121=CARTESIAN_POINT('Ctrl Pts',(7.10468508996624,-2.23205677050182,44.8234658877696));
#78122=CARTESIAN_POINT('Ctrl Pts',(7.32446118816338,1.43123017728363,44.9822296887011));
#78123=CARTESIAN_POINT('Ctrl Pts',(5.73701456861917,4.74819502188697,45.1409934896327));
#78124=CARTESIAN_POINT('Ctrl Pts',(1.78386760397576,7.67973079635173,45.3526785575413));
#78125=CARTESIAN_POINT('Ctrl Pts',(-4.88511333053378,6.90592624907402,45.6172848924272));
#78126=CARTESIAN_POINT('Ctrl Pts',(-8.45657675320892,-0.385553455566417,
45.9348124942902));
#78127=CARTESIAN_POINT('Ctrl Pts',(-4.95526267182601,-6.13218637972633,
46.1994188291761));
#78128=CARTESIAN_POINT('Ctrl Pts',(-0.229615199062717,-7.43604151613453,
46.4111038970848));
#78129=CARTESIAN_POINT('Ctrl Pts',(4.59028181864933,-6.41785290313922,46.6227889649935));
#78130=CARTESIAN_POINT('Ctrl Pts',(7.62824266808339,-2.00957801379248,46.8344740329021));
#78131=CARTESIAN_POINT('Ctrl Pts',(6.87300812585219,2.8671217198266,47.0461591008109));
#78132=CARTESIAN_POINT('Ctrl Pts',(4.6822920024229,5.81139338896664,47.2049229017423));
#78133=CARTESIAN_POINT('Ctrl Pts',(1.33188720178281,7.326989054731,47.3636867026739));
#78134=CARTESIAN_POINT('Ctrl Pts',(-3.58031154497339,7.02437313743209,47.5753717705826));
#78135=CARTESIAN_POINT('Ctrl Pts',(-8.1844302927773,2.13804826710671,47.8399781054684));
#78136=CARTESIAN_POINT('Ctrl Pts',(-6.22179769137573,-5.74034627331874,
48.1575057073316));
#78137=CARTESIAN_POINT('Ctrl Pts',(0.157405566479999,-7.8824844706561,48.4221120422172));
#78138=CARTESIAN_POINT('Ctrl Pts',(4.61254190148167,-5.83711347982825,48.6337971101261));
#78139=CARTESIAN_POINT('Ctrl Pts',(7.64457653497177,-1.95447503486593,48.8454821780346));
#78140=CARTESIAN_POINT('Ctrl Pts',(7.13031949236453,3.37446794820925,49.0571672459435));
#78141=CARTESIAN_POINT('Ctrl Pts',(3.41228880689173,6.61928340175076,49.2688523138521));
#78142=CARTESIAN_POINT('Ctrl Pts',(-0.159688229184292,7.46127677993111,
49.4276161147836));
#78143=CARTESIAN_POINT('Ctrl Pts',(-3.6989807589367,6.46345367983997,49.5863799157152));
#78144=CARTESIAN_POINT('Ctrl Pts',(-7.26240660343833,3.06885956982117,49.7980649836238));
#78145=CARTESIAN_POINT('Ctrl Pts',(-7.63857908676835,-3.63431687459858,
50.0626713185097));
#78146=CARTESIAN_POINT('Ctrl Pts',(-1.06392470896808,-8.39823827142704,
50.3801989203728));
#78147=CARTESIAN_POINT('Ctrl Pts',(5.19612230760402,-5.92947307160712,50.6448052552585));
#78148=CARTESIAN_POINT('Ctrl Pts',(7.28765760026079,-1.49582193815768,50.8564903231673));
#78149=CARTESIAN_POINT('Ctrl Pts',(7.10733447958075,3.42714453391363,51.068175391076));
#78150=CARTESIAN_POINT('Ctrl Pts',(3.28246522055953,7.17313823040342,51.2798604589846));
#78151=CARTESIAN_POINT('Ctrl Pts',(-1.65157499882752,7.26160641164148,51.4915455268934));
#78152=CARTESIAN_POINT('Ctrl Pts',(-4.92664453442159,5.60574037471812,51.6503093278248));
#78153=CARTESIAN_POINT('Ctrl Pts',(-6.99201205167683,2.56329077467563,51.8090731287563));
#78154=CARTESIAN_POINT('Ctrl Pts',(-7.53251405893683,-2.3284502754392,52.0207581966651));
#78155=CARTESIAN_POINT('Ctrl Pts',(-3.50400880017233,-7.69922541152626,
52.2853645315508));
#78156=CARTESIAN_POINT('Ctrl Pts',(4.59379606705064,-7.11051190452267,52.602892133414));
#78157=CARTESIAN_POINT('Ctrl Pts',(7.7936228149868,-1.19070624494491,52.8674984682998));
#78158=CARTESIAN_POINT('Ctrl Pts',(6.53892239868291,3.5482291964793,53.0791835362085));
#78159=CARTESIAN_POINT('Ctrl Pts',(3.23096003240178,7.1986401726906,53.2908686041172));
#78160=CARTESIAN_POINT('Ctrl Pts',(-2.10754046975733,7.60176053035004,53.5025536720258));
#78161=CARTESIAN_POINT('Ctrl Pts',(-5.93950408539159,4.49231776126522,53.7142387399347));
#78162=CARTESIAN_POINT('Ctrl Pts',(-7.37898930942744,1.11654301968292,53.873002540866));
#78163=CARTESIAN_POINT('Ctrl Pts',(-7.00009115585931,-2.54114459924067,
54.0317663417977));
#78164=CARTESIAN_POINT('Ctrl Pts',(-4.26373338329906,-6.63181924519665,
54.2434514097062));
#78165=CARTESIAN_POINT('Ctrl Pts',(2.27679741834353,-8.14692230422807,54.5080577445922));
#78166=CARTESIAN_POINT('Ctrl Pts',(8.09328248775631,-2.48216036142054,54.8255853464552));
#78167=CARTESIAN_POINT('Ctrl Pts',(6.72956241843219,4.10747227349011,55.090191681341));
#78168=CARTESIAN_POINT('Ctrl Pts',(2.71810326799314,6.92526896945336,55.3018767492498));
#78169=CARTESIAN_POINT('Ctrl Pts',(-2.16336776199988,7.58810673736746,55.5135618171584));
#78170=CARTESIAN_POINT('Ctrl Pts',(-6.50739234715102,4.45896145096741,55.7252468850672));
#78171=CARTESIAN_POINT('Ctrl Pts',(-7.43696462099792,-0.387528927329647,
55.9369319529758));
#78172=CARTESIAN_POINT('Ctrl Pts',(-6.36457501450357,-3.89722353864109,
56.0956957539074));
#78173=CARTESIAN_POINT('Ctrl Pts',(-3.71942086257268,-6.4517111270184,56.2544595548388));
#78174=CARTESIAN_POINT('Ctrl Pts',(1.0082099163406,-7.81946213435861,56.4661446227476));
#78175=CARTESIAN_POINT('Ctrl Pts',(6.98793687374695,-4.7670684614793,56.7307509576334));
#78176=CARTESIAN_POINT('Ctrl Pts',(7.79041141615472,3.3123397107483,57.0482785594965));
#78177=CARTESIAN_POINT('Ctrl Pts',(2.50387262287746,7.47591152173031,57.3128848943822));
#78178=CARTESIAN_POINT('Ctrl Pts',(-2.37974820771574,7.04869636209595,57.524569962291));
#78179=CARTESIAN_POINT('Ctrl Pts',(-6.54124431444534,4.41261091435839,57.7362550301996));
#78180=CARTESIAN_POINT('Ctrl Pts',(-7.85011314244894,-0.778814148529765,
57.9479400981084));
#78181=CARTESIAN_POINT('Ctrl Pts',(-5.440255204774,-5.08519809189294,58.1596251660171));
#78182=CARTESIAN_POINT('Ctrl Pts',(-2.36034655652782,-7.08024618005674,
58.3183889669485));
#78183=CARTESIAN_POINT('Ctrl Pts',(1.30934340514053,-7.33074709976975,58.4771527678801));
#78184=CARTESIAN_POINT('Ctrl Pts',(5.80506746240374,-5.33431154462047,58.6888378357887));
#78185=CARTESIAN_POINT('Ctrl Pts',(8.41896344392571,0.854302628986389,58.9534441706747));
#78186=CARTESIAN_POINT('Ctrl Pts',(3.82237674437087,7.54737245299685,59.2709717725376));
#78187=CARTESIAN_POINT('Ctrl Pts',(-2.88958471775843,7.33756896722465,59.5355781074236));
#78188=CARTESIAN_POINT('Ctrl Pts',(-6.37111707909232,3.85311267538591,59.7472631753321));
#78189=CARTESIAN_POINT('Ctrl Pts',(-7.45324420054764,0.351828748494111,
59.9060269762639));
#78190=CARTESIAN_POINT('Ctrl Pts',(-6.70494820545435,-3.26568653815952,
60.0647974714419));
#78191=CARTESIAN_POINT('Ctrl Pts',(-5.12192455972379,-5.13456107383707,
60.1706466996429));
#78192=CARTESIAN_POINT('Ctrl Pts',(-4.15332558991753,-5.82516755464222,
60.2235746608667));
#78193=CARTESIAN_POINT('Ctrl Pts',(-3.26266258150082,6.80520260935705,-60.2102386032606));
#78194=CARTESIAN_POINT('Ctrl Pts',(-4.39427159822301,6.26266980452596,-60.1573082411063));
#78195=CARTESIAN_POINT('Ctrl Pts',(-6.37755155656977,4.60671016839827,-60.0514566119747));
#78196=CARTESIAN_POINT('Ctrl Pts',(-7.80955707945264,0.982430906290448,
-59.892683715866));
#78197=CARTESIAN_POINT('Ctrl Pts',(-7.31821709273351,-2.8520683494292,-59.7339199149344));
#78198=CARTESIAN_POINT('Ctrl Pts',(-4.33020733389426,-7.10306190021205,
-59.5222348470259));
#78199=CARTESIAN_POINT('Ctrl Pts',(2.60737502964694,-8.53510294343834,-59.2576285121399));
#78200=CARTESIAN_POINT('Ctrl Pts',(8.59504447333725,-2.41059574693977,-58.9401009102769));
#78201=CARTESIAN_POINT('Ctrl Pts',(6.99784544930374,4.49381352486545,-58.675494575391));
#78202=CARTESIAN_POINT('Ctrl Pts',(2.68667853170036,7.38179190922916,-58.4638095074824));
#78203=CARTESIAN_POINT('Ctrl Pts',(-1.17242277308143,7.78519454912189,-58.3050457065508));
#78204=CARTESIAN_POINT('Ctrl Pts',(-4.73412089022752,6.26887006262792,-58.1462819056193));
#78205=CARTESIAN_POINT('Ctrl Pts',(-8.01750998147662,2.22925445242337,-57.9345968377106));
#78206=CARTESIAN_POINT('Ctrl Pts',(-7.59622194194939,-3.40276613558523,
-57.7229117698019));
#78207=CARTESIAN_POINT('Ctrl Pts',(-3.74810167430262,-6.89506033654368,
-57.5112267018932));
#78208=CARTESIAN_POINT('Ctrl Pts',(1.25002051470277,-8.22235674886337,-57.2995416339846));
#78209=CARTESIAN_POINT('Ctrl Pts',(7.49722266516787,-4.85146930384844,-57.0349352990986));
#78210=CARTESIAN_POINT('Ctrl Pts',(8.12456649763937,3.69034896651629,-56.7174076972357));
#78211=CARTESIAN_POINT('Ctrl Pts',(2.46211435707413,7.94416432374526,-56.4528013623498));
#78212=CARTESIAN_POINT('Ctrl Pts',(-2.69854954494453,7.37779497692955,-56.2411162944411));
#78213=CARTESIAN_POINT('Ctrl Pts',(-5.90960739324672,5.20142821114934,-56.0823524935096));
#78214=CARTESIAN_POINT('Ctrl Pts',(-7.6589098948458,1.74787750182028,-55.9235886925781));
#78215=CARTESIAN_POINT('Ctrl Pts',(-7.56942412666791,-3.45705962324571,
-55.7119036246693));
#78216=CARTESIAN_POINT('Ctrl Pts',(-3.62078797743637,-7.49478945458689,
-55.5002185567607));
#78217=CARTESIAN_POINT('Ctrl Pts',(1.57225890926194,-7.68883942439684,-55.288533488852));
#78218=CARTESIAN_POINT('Ctrl Pts',(6.25089939315454,-5.48594870743951,-55.0768484209433));
#78219=CARTESIAN_POINT('Ctrl Pts',(8.86004379236408,1.11579116834456,-54.8122420860574));
#78220=CARTESIAN_POINT('Ctrl Pts',(3.83974534657913,8.05503270661092,-54.4947144841945));
#78221=CARTESIAN_POINT('Ctrl Pts',(-3.23166004154058,7.6634259872617,-54.2301081493085));
#78222=CARTESIAN_POINT('Ctrl Pts',(-6.81535455965847,3.90704458018533,-54.0184230813999));
#78223=CARTESIAN_POINT('Ctrl Pts',(-7.87070091762291,0.174256944970944,
-53.8596592804683));
#78224=CARTESIAN_POINT('Ctrl Pts',(-6.98526896633185,-3.59444027794282,
-53.7008954795368));
#78225=CARTESIAN_POINT('Ctrl Pts',(-3.56523800911463,-7.51907694657359,
-53.4892104116282));
#78226=CARTESIAN_POINT('Ctrl Pts',(2.05580984747745,-8.06570638289985,-53.2775253437196));
#78227=CARTESIAN_POINT('Ctrl Pts',(6.1539240684084,-4.8702637839017,-53.0658402758107));
#78228=CARTESIAN_POINT('Ctrl Pts',(8.31503040792571,-0.172176605010883,
-52.8541552079022));
#78229=CARTESIAN_POINT('Ctrl Pts',(6.06027237653944,6.55884632086358,-52.5895488730162));
#78230=CARTESIAN_POINT('Ctrl Pts',(-2.24903948266158,8.63533541566494,-52.2720212711532));
#78231=CARTESIAN_POINT('Ctrl Pts',(-7.40715510596884,3.78229792270048,-52.0074149362673));
#78232=CARTESIAN_POINT('Ctrl Pts',(-7.73020231934559,-1.39929528552856,
-51.7957298683586));
#78233=CARTESIAN_POINT('Ctrl Pts',(-6.13402181550093,-4.93478213859474,
-51.6369660674271));
#78234=CARTESIAN_POINT('Ctrl Pts',(-3.02984348382236,-7.24803641779415,
-51.4782022664956));
#78235=CARTESIAN_POINT('Ctrl Pts',(2.11395012478913,-8.04851881185056,-51.2665171985869));
#78236=CARTESIAN_POINT('Ctrl Pts',(6.76655750420719,-4.84723355326002,-51.0548321306782));
#78237=CARTESIAN_POINT('Ctrl Pts',(7.84438329612395,0.236434918886423,-50.8431470627695));
#78238=CARTESIAN_POINT('Ctrl Pts',(6.47263540369198,5.22248661053359,-50.6314619948608));
#78239=CARTESIAN_POINT('Ctrl Pts',(0.413294031195558,8.92045707250124,-50.366855659975));
#78240=CARTESIAN_POINT('Ctrl Pts',(-7.28119179881932,5.15862794986372,-50.0493280581119));
#78241=CARTESIAN_POINT('Ctrl Pts',(-8.10265755592695,-1.87581045709897,
-49.7847217232261));
#78242=CARTESIAN_POINT('Ctrl Pts',(-5.01328502561204,-6.04822523110639,
-49.5730366553175));
#78243=CARTESIAN_POINT('Ctrl Pts',(-1.51548721827395,-7.72538651975872,
-49.4142728543859));
#78244=CARTESIAN_POINT('Ctrl Pts',(2.34904793451002,-7.49639628431493,-49.2555090534543));
#78245=CARTESIAN_POINT('Ctrl Pts',(6.7999727671332,-4.7966457614761,-49.0438239855458));
#78246=CARTESIAN_POINT('Ctrl Pts',(8.29827490589769,0.648542337648683,-48.8321389176368));
#78247=CARTESIAN_POINT('Ctrl Pts',(5.84943353727355,5.23205294892948,-48.6204538497284));
#78248=CARTESIAN_POINT('Ctrl Pts',(1.58929915763245,8.16354724699242,-48.4087687818195));
#78249=CARTESIAN_POINT('Ctrl Pts',(-5.42785605201213,7.09110322990665,-48.1441624469338));
#78250=CARTESIAN_POINT('Ctrl Pts',(-8.89253094527492,-0.741680337907531,
-47.8266348450706));
#78251=CARTESIAN_POINT('Ctrl Pts',(-4.99140989651476,-6.65263493546399,
-47.5620285101848));
#78252=CARTESIAN_POINT('Ctrl Pts',(0.0589488032179521,-7.85560820260387,
-47.3503434422762));
#78253=CARTESIAN_POINT('Ctrl Pts',(3.81504601570707,-6.88648838570566,-47.1915796413446));
#78254=CARTESIAN_POINT('Ctrl Pts',(6.62432138306982,-4.22283668449543,-47.0328158404131));
#78255=CARTESIAN_POINT('Ctrl Pts',(8.29126616213413,0.708763446778455,-46.8211307725044));
#78256=CARTESIAN_POINT('Ctrl Pts',(5.93133823172453,5.83962330621226,-46.6094457045957));
#78257=CARTESIAN_POINT('Ctrl Pts',(1.106332125194,7.76957399064748,-46.3977606366871));
#78258=CARTESIAN_POINT('Ctrl Pts',(-4.04071368192798,7.26925088348232,-46.1860755687783));
#78259=CARTESIAN_POINT('Ctrl Pts',(-8.71891791081765,1.93024267981529,-45.9214692338925));
#78260=CARTESIAN_POINT('Ctrl Pts',(-6.3260256110773,-6.29353607317102,-45.6039416320294));
#78261=CARTESIAN_POINT('Ctrl Pts',(0.464877034074995,-8.30395169077777,
-45.3393352971436));
#78262=CARTESIAN_POINT('Ctrl Pts',(5.10348759970218,-5.97230855816275,-45.1276502292349));
#78263=CARTESIAN_POINT('Ctrl Pts',(7.35321338239484,-2.8122146684403,-44.9688864283033));
#78264=CARTESIAN_POINT('Ctrl Pts',(7.78738924037035,1.03467495817789,-44.8101226273719));
#78265=CARTESIAN_POINT('Ctrl Pts',(5.8871982942649,5.8811849519331,-44.5984375594632));
#78266=CARTESIAN_POINT('Ctrl Pts',(0.777769849796183,8.28716161531329,-44.3867524915545));
#78267=CARTESIAN_POINT('Ctrl Pts',(-4.15654072107625,6.65683258024544,-44.1750674236458));
#78268=CARTESIAN_POINT('Ctrl Pts',(-7.77233859820406,2.95975137151687,-43.9633823557371));
#78269=CARTESIAN_POINT('Ctrl Pts',(-7.91370129781951,-4.13747484674488,
-43.6987760208512));
#78270=CARTESIAN_POINT('Ctrl Pts',(-0.78745851557057,-8.88859411957631,
-43.3812484189883));
#78271=CARTESIAN_POINT('Ctrl Pts',(5.70275775804652,-6.05394733150377,-43.1166420841023));
#78272=CARTESIAN_POINT('Ctrl Pts',(7.75033133819768,-1.28312873179931,-42.9049570161937));
#78273=CARTESIAN_POINT('Ctrl Pts',(7.43673075868515,2.58327970054494,-42.7461932152622));
#78274=CARTESIAN_POINT('Ctrl Pts',(5.29182477389289,5.8060807790221,-42.5874294143306));
#78275=CARTESIAN_POINT('Ctrl Pts',(0.717236323629105,8.29053751278568,-42.375744346422));
#78276=CARTESIAN_POINT('Ctrl Pts',(-4.74120647888952,6.84126703923405,-42.1640592785132));
#78277=CARTESIAN_POINT('Ctrl Pts',(-7.46660836295353,2.41661133028347,-41.9523742106046));
#78278=CARTESIAN_POINT('Ctrl Pts',(-7.85240220824392,-2.74028374923017,
-41.7406891426959));
#78279=CARTESIAN_POINT('Ctrl Pts',(-3.39050906099741,-8.26134460277815,
-41.47608280781));
#78280=CARTESIAN_POINT('Ctrl Pts',(5.12106840726382,-7.30765726511821,-41.1585552059471));
#78281=CARTESIAN_POINT('Ctrl Pts',(8.26139731090733,-0.959707669509055,
-40.8939488710611));
#78282=CARTESIAN_POINT('Ctrl Pts',(6.75595311145198,4.00888422757258,-40.6822638031524));
#78283=CARTESIAN_POINT('Ctrl Pts',(4.02636042792342,6.76511050115767,-40.5235000022209));
#78284=CARTESIAN_POINT('Ctrl Pts',(0.310081618777929,7.84970272302158,-40.3647362012893));
#78285=CARTESIAN_POINT('Ctrl Pts',(-4.78969403479622,6.80487114116623,-40.1530511333807));
#78286=CARTESIAN_POINT('Ctrl Pts',(-8.0326928565855,2.18124254711268,-39.9413660654719));
#78287=CARTESIAN_POINT('Ctrl Pts',(-7.26875135094599,-2.95897018665329,
-39.7296809975633));
#78288=CARTESIAN_POINT('Ctrl Pts',(-4.24328942660509,-7.15289244350772,
-39.5179959296546));
#78289=CARTESIAN_POINT('Ctrl Pts',(2.72559521113433,-8.5039106935338,-39.2533895947687));
#78290=CARTESIAN_POINT('Ctrl Pts',(8.62364054489699,-2.29347336778082,-38.9358619929058));
#78291=CARTESIAN_POINT('Ctrl Pts',(6.93870843542055,4.58541705712851,-38.6712556580198));
#78292=CARTESIAN_POINT('Ctrl Pts',(2.58752673216899,7.41746321895357,-38.4595705901112));
#78293=CARTESIAN_POINT('Ctrl Pts',(-1.27565445200444,7.76859087013229,-38.3008067891796));
#78294=CARTESIAN_POINT('Ctrl Pts',(-4.81734253396703,6.20541653400868,-38.1420429882481));
#78295=CARTESIAN_POINT('Ctrl Pts',(-8.04635426085578,2.12217419257887,-37.9303579203395));
#78296=CARTESIAN_POINT('Ctrl Pts',(-7.55029959054519,-3.50356242567293,
-37.7186728524307));
#78297=CARTESIAN_POINT('Ctrl Pts',(-3.6559258783647,-6.9443831071799,-37.5069877845221));
#78298=CARTESIAN_POINT('Ctrl Pts',(1.35938440304736,-8.20496493052104,-37.2953027166133));
#78299=CARTESIAN_POINT('Ctrl Pts',(7.56117395241235,-4.75121192959417,-37.0306963817275));
#78300=CARTESIAN_POINT('Ctrl Pts',(8.07469694698156,3.79821873392218,-36.7131687798645));
#78301=CARTESIAN_POINT('Ctrl Pts',(2.35611021374405,7.97624404091755,-36.4485624449786));
#78302=CARTESIAN_POINT('Ctrl Pts',(-2.79655853467506,7.34120668257979,-36.23687737707));
#78303=CARTESIAN_POINT('Ctrl Pts',(-5.97834772773149,5.12227067175771,-36.0781135761384));
#78304=CARTESIAN_POINT('Ctrl Pts',(-7.68150687453854,1.64573253797016,-35.9193497752069));
#78305=CARTESIAN_POINT('Ctrl Pts',(-7.52271651044792,-3.55755203732478,
-35.7076647072982));
#78306=CARTESIAN_POINT('Ctrl Pts',(-3.52066227601521,-7.54234119592964,
-35.4959796393895));
#78307=CARTESIAN_POINT('Ctrl Pts',(1.67450843320736,-7.66722063556932,-35.2842945714808));
#78308=CARTESIAN_POINT('Ctrl Pts',(6.32339904103569,-5.40222176832433,-35.0726095035722));
#78309=CARTESIAN_POINT('Ctrl Pts',(8.84439970681327,1.23367749621947,-34.8080031686863));
#78310=CARTESIAN_POINT('Ctrl Pts',(3.73213955334257,8.10545067782704,-34.4904755668233));
#78311=CARTESIAN_POINT('Ctrl Pts',(-3.33342394246881,7.61971188164993,-34.2258692319374));
#78312=CARTESIAN_POINT('Ctrl Pts',(-6.86677863638025,3.8159410835559,-34.0141841640287));
#78313=CARTESIAN_POINT('Ctrl Pts',(-7.87232352904819,0.0694308462814094,
-33.8554203630972));
#78314=CARTESIAN_POINT('Ctrl Pts',(-6.93678401568545,-3.68714130049925,
-33.6966565621657));
#78315=CARTESIAN_POINT('Ctrl Pts',(-3.46479365649576,-7.56588693496979,
-33.484971494257));
#78316=CARTESIAN_POINT('Ctrl Pts',(2.16303500733719,-8.03761489091188,-33.2732864263483));
#78317=CARTESIAN_POINT('Ctrl Pts',(6.21823355495086,-4.78788285398311,-33.0616013584396));
#78318=CARTESIAN_POINT('Ctrl Pts',(8.31658591973511,-0.0614337528735027,
-32.8499162905309));
#78319=CARTESIAN_POINT('Ctrl Pts',(5.97239375865441,6.63896672157217,-32.585309955645));
#78320=CARTESIAN_POINT('Ctrl Pts',(-2.36383300746484,8.60462026176232,-32.267782353782));
#78321=CARTESIAN_POINT('Ctrl Pts',(-7.45686550868394,3.68332473792107,-32.0031760188961));
#78322=CARTESIAN_POINT('Ctrl Pts',(-7.71088309087349,-1.50211089906813,
-31.7914909509875));
#78323=CARTESIAN_POINT('Ctrl Pts',(-6.0677636032303,-5.01602863266695,-31.6327271500559));
#78324=CARTESIAN_POINT('Ctrl Pts',(-2.93305593191232,-7.28774082623624,
-31.4739633491245));
#78325=CARTESIAN_POINT('Ctrl Pts',(2.22094125045637,-8.01965461580867,-31.2622782812157));
#78326=CARTESIAN_POINT('Ctrl Pts',(6.83050598543679,-4.75669649657056,-31.0505932133071));
#78327=CARTESIAN_POINT('Ctrl Pts',(7.84053924089609,0.340874140044041,-30.8389081453983));
#78328=CARTESIAN_POINT('Ctrl Pts',(6.40251593349158,5.30821676156078,-30.6272230774897));
#78329=CARTESIAN_POINT('Ctrl Pts',(0.294467600103715,8.92516975586717,-30.3626167426038));
#78330=CARTESIAN_POINT('Ctrl Pts',(-7.34924134935658,5.06121012458663,-30.0450891407408));
#78331=CARTESIAN_POINT('Ctrl Pts',(-8.07695976015268,-1.98354364016924,
-29.7804828058548));
#78332=CARTESIAN_POINT('Ctrl Pts',(-4.93229895868432,-6.11444864042372,
-29.5687977379463));
#78333=CARTESIAN_POINT('Ctrl Pts',(-1.4124772829056,-7.74488258876122,-29.4100339370147));
#78334=CARTESIAN_POINT('Ctrl Pts',(2.44866584252073,-7.46445035094941,-29.2512701360832));
#78335=CARTESIAN_POINT('Ctrl Pts',(6.86324463018906,-4.70566821408192,-29.0395850681745));
#78336=CARTESIAN_POINT('Ctrl Pts',(8.28890275205008,0.758989291512339,-28.8279000002658));
#78337=CARTESIAN_POINT('Ctrl Pts',(5.7792419352401,5.30948334787337,-28.6162149323571));
#78338=CARTESIAN_POINT('Ctrl Pts',(1.48044788464432,8.18398738557075,-28.4045298644485));
#78339=CARTESIAN_POINT('Ctrl Pts',(-5.52180385579767,7.01819410651025,-28.1399235295625));
#78340=CARTESIAN_POINT('Ctrl Pts',(-8.8818658215771,-0.860032478346779,
-27.8223959276996));
#78341=CARTESIAN_POINT('Ctrl Pts',(-4.90237711231396,-6.7185134507748,-27.5577895928137));
#78342=CARTESIAN_POINT('Ctrl Pts',(0.163553239062703,-7.85412665623684,
-27.346104524905));
#78343=CARTESIAN_POINT('Ctrl Pts',(3.90641206075979,-6.83507448386419,-27.1873407239735));
#78344=CARTESIAN_POINT('Ctrl Pts',(6.67996765911546,-4.13424908820067,-27.0285769230419));
#78345=CARTESIAN_POINT('Ctrl Pts',(8.28109269185019,0.819111728535833,-26.8168918551333));
#78346=CARTESIAN_POINT('Ctrl Pts',(5.85304862131644,5.91809052094336,-26.6052067872245));
#78347=CARTESIAN_POINT('Ctrl Pts',(1.00277004429556,7.78361760402229,-26.3935217193159));
#78348=CARTESIAN_POINT('Ctrl Pts',(-4.13715679621693,7.21479792578039,-26.1818366514072));
#78349=CARTESIAN_POINT('Ctrl Pts',(-8.74384899928446,1.81396554991253,-25.9172303165214));
#78350=CARTESIAN_POINT('Ctrl Pts',(-6.24165644830004,-6.37721891718524,
-25.5997027146583));
#78351=CARTESIAN_POINT('Ctrl Pts',(0.57541586864642,-8.2970248232539,-25.3350963797725));
#78352=CARTESIAN_POINT('Ctrl Pts',(5.18256567079529,-5.90381810882687,-25.1234113118638));
#78353=CARTESIAN_POINT('Ctrl Pts',(7.39001039811455,-2.71404581836418,-24.9646475109322));
#78354=CARTESIAN_POINT('Ctrl Pts',(7.77292042892884,1.13828443530474,-24.8058837100007));
#78355=CARTESIAN_POINT('Ctrl Pts',(5.80835913964507,5.9590606893823,-24.5941986420921));
#78356=CARTESIAN_POINT('Ctrl Pts',(0.667344416622147,8.29678401594118,-24.3825135741833));
#78357=CARTESIAN_POINT('Ctrl Pts',(-4.24481826116653,6.60089150774721,-24.1708285062747));
#78358=CARTESIAN_POINT('Ctrl Pts',(-7.81106313146197,2.85598813419176,-23.959143438366));
#78359=CARTESIAN_POINT('Ctrl Pts',(-7.8579026714865,-4.24249124265474,-23.6945371034801));
#78360=CARTESIAN_POINT('Ctrl Pts',(-0.66902321244215,-8.89829221129115,
-23.377009501617));
#78361=CARTESIAN_POINT('Ctrl Pts',(5.7828698397457,-5.97746942745352,-23.1124031667312));
#78362=CARTESIAN_POINT('Ctrl Pts',(7.766730980083,-1.17980722036984,-22.9007180988225));
#78363=CARTESIAN_POINT('Ctrl Pts',(7.40167095490554,2.68208229995444,-22.741954297891));
#78364=CARTESIAN_POINT('Ctrl Pts',(5.21403853970046,5.87603484984857,-22.5831904969595));
#78365=CARTESIAN_POINT('Ctrl Pts',(0.606771302585118,8.29935351585887,-22.3715054290508));
#78366=CARTESIAN_POINT('Ctrl Pts',(-4.83188820926486,6.77752387754858,-22.1598203611421));
#78367=CARTESIAN_POINT('Ctrl Pts',(-7.49812724919615,2.31696752723136,-21.9481352932334));
#78368=CARTESIAN_POINT('Ctrl Pts',(-7.81521479364046,-2.84460774019756,
-21.7364502253247));
#78369=CARTESIAN_POINT('Ctrl Pts',(-3.28019575183774,-8.30576198600601,
-21.4718438904388));
#78370=CARTESIAN_POINT('Ctrl Pts',(5.21792716807712,-7.23881429551514,-21.1543162885758));
#78371=CARTESIAN_POINT('Ctrl Pts',(8.27344478157893,-0.849609195893172,
-20.88970995369));
#78372=CARTESIAN_POINT('Ctrl Pts',(6.70196952627641,4.09849480456911,-20.6780248857812));
#78373=CARTESIAN_POINT('Ctrl Pts',(3.93591542657239,6.81812790605245,-20.5192610848498));
#78374=CARTESIAN_POINT('Ctrl Pts',(0.205523101929143,7.8531359153328,-20.3604972839182));
#78375=CARTESIAN_POINT('Ctrl Pts',(-4.87988679772441,6.74048551932531,-20.1488122160095));
#78376=CARTESIAN_POINT('Ctrl Pts',(-8.06102724644903,2.07408131701245,-19.9371271481009));
#78377=CARTESIAN_POINT('Ctrl Pts',(-7.22870353760725,-3.05550256631652,
-19.7254420801922));
#78378=CARTESIAN_POINT('Ctrl Pts',(-4.14766126956044,-7.20876421166052,
-19.5137570122835));
#78379=CARTESIAN_POINT('Ctrl Pts',(2.83859635510066,-8.46686111090562,-19.2491506773976));
#78380=CARTESIAN_POINT('Ctrl Pts',(8.65341706408883,-2.17843279704631,-18.9316230755346));
#78381=CARTESIAN_POINT('Ctrl Pts',(6.87703121255687,4.67741018525212,-18.6670167406487));
#78382=CARTESIAN_POINT('Ctrl Pts',(2.48852221833318,7.45126246773523,-18.45533167274));
#78383=CARTESIAN_POINT('Ctrl Pts',(-1.37899223206182,7.75091470810606,-18.2965678718085));
#78384=CARTESIAN_POINT('Ctrl Pts',(-4.89955017323679,6.14071588253778,-18.137804070877));
#78385=CARTESIAN_POINT('Ctrl Pts',(-8.07390085219916,2.01483627714438,-17.9261190029683));
#78386=CARTESIAN_POINT('Ctrl Pts',(-7.5029747183492,-3.6037957702104,-17.7144339350596));
#78387=CARTESIAN_POINT('Ctrl Pts',(-3.56312642911424,-6.99245170291008,
-17.5027488671509));
#78388=CARTESIAN_POINT('Ctrl Pts',(1.46852575934409,-8.18613508076134,-17.2910637992423));
#78389=CARTESIAN_POINT('Ctrl Pts',(7.62377329803872,-4.6501018309999,-17.0264574643564));
#78390=CARTESIAN_POINT('Ctrl Pts',(8.02340176900499,3.90540911934195,-16.7089298624934));
#78391=CARTESIAN_POINT('Ctrl Pts',(2.24968518218346,8.00691207149459,-16.4443235276075));
#78392=CARTESIAN_POINT('Ctrl Pts',(-2.89407017089541,7.30331520887269,-16.2326384596988));
#78393=CARTESIAN_POINT('Ctrl Pts',(-6.04602864672309,5.04220546898135,-16.0738746587673));
#78394=CARTESIAN_POINT('Ctrl Pts',(-7.70274125368099,1.54329537968519,-15.9151108578358));
#78395=CARTESIAN_POINT('Ctrl Pts',(-7.47467512822539,-3.65741328295393,
-15.703425789927));
#78396=CARTESIAN_POINT('Ctrl Pts',(-3.419912076881,-7.58855552552508,-15.4917407220184));
#78397=CARTESIAN_POINT('Ctrl Pts',(1.77646094455016,-7.64424209976831,-15.2800556541097));
#78398=CARTESIAN_POINT('Ctrl Pts',(6.39477734960587,-5.31753684663269,-15.068370586201));
#78399=CARTESIAN_POINT('Ctrl Pts',(8.82718714214999,1.35134506918803,-14.8037642513151));
#78400=CARTESIAN_POINT('Ctrl Pts',(3.62387192255354,8.154431226348,-14.4862366494521));
#78401=CARTESIAN_POINT('Ctrl Pts',(-3.4345967058702,7.57464651370659,-14.2216303145662));
#78402=CARTESIAN_POINT('Ctrl Pts',(-6.91698496501562,3.72416087031233,-14.0099452466575));
#78403=CARTESIAN_POINT('Ctrl Pts',(-7.87255007560244,-0.0354075635112222,
-13.851181445726));
#78404=CARTESIAN_POINT('Ctrl Pts',(-6.88706890473335,-3.7791884514498,-13.6924176447945));
#78405=CARTESIAN_POINT('Ctrl Pts',(-3.36373486299103,-7.61135519906527,
-13.4807325768858));
#78406=CARTESIAN_POINT('Ctrl Pts',(2.26987657798482,-8.00809802002258,-13.2690475089771));
#78407=CARTESIAN_POINT('Ctrl Pts',(6.2814403086435,-4.70465284758939,-13.0573624410685));
#78408=CARTESIAN_POINT('Ctrl Pts',(8.31666658009959,0.0493199937455939,
-12.8456773731598));
#78409=CARTESIAN_POINT('Ctrl Pts',(5.88345600487443,6.71790977739831,-12.5810710382739));
#78410=CARTESIAN_POINT('Ctrl Pts',(-2.47820733344243,8.57237917668041,-12.2635434364109));
#78411=CARTESIAN_POINT('Ctrl Pts',(-7.50525352146753,3.5836983575743,-11.998937101525));
#78412=CARTESIAN_POINT('Ctrl Pts',(-7.69019642532775,-1.60466013039959,
-11.7872520336163));
#78413=CARTESIAN_POINT('Ctrl Pts',(-6.00042934237632,-5.09638559133537,
-11.6284882326848));
#78414=CARTESIAN_POINT('Ctrl Pts',(-2.83574823602284,-7.32615283706326,
-11.4697244317533));
#78415=CARTESIAN_POINT('Ctrl Pts',(2.3275385175523,-7.98936822559517,-11.2580393638446));
#78416=CARTESIAN_POINT('Ctrl Pts',(6.89324315442797,-4.66531589407465,-11.0463542959359));
#78417=CARTESIAN_POINT('Ctrl Pts',(7.83530475556439,0.445252911065612,-10.8346692280272));
#78418=CARTESIAN_POINT('Ctrl Pts',(6.33126105020073,5.39300556095946,-10.6229841601185));
#78419=CARTESIAN_POINT('Ctrl Pts',(0.175588948545246,8.92829966229325,-10.3583778252327));
#78420=CARTESIAN_POINT('Ctrl Pts',(-7.41598759586123,4.96289475148757,-10.0408502233696));
#78421=CARTESIAN_POINT('Ctrl Pts',(-8.04982960779548,-2.09092506442495,
-9.7762438884838));
#78422=CARTESIAN_POINT('Ctrl Pts',(-4.85043820485799,-6.17958772209538,
-9.56455882057513));
#78423=CARTESIAN_POINT('Ctrl Pts',(-1.30921686082002,-7.76300519127524,
-9.40579501964359));
#78424=CARTESIAN_POINT('Ctrl Pts',(2.54784950760582,-7.43118068255035,-9.24703121871208));
#78425=CARTESIAN_POINT('Ctrl Pts',(6.92529937518107,-4.61385617016351,-9.03534615080339));
#78426=CARTESIAN_POINT('Ctrl Pts',(8.27806065595005,0.86930164729228,-8.8236610828947));
#78427=CARTESIAN_POINT('Ctrl Pts',(5.7080254506422,5.38597217057458,-8.61197601498602));
#78428=CARTESIAN_POINT('Ctrl Pts',(1.37133407112876,8.20297618743883,-8.40029094707731));
#78429=CARTESIAN_POINT('Ctrl Pts',(-5.6147724307227,6.94404038652962,-8.13568461219148));
#78430=CARTESIAN_POINT('Ctrl Pts',(-8.86962560039774,-0.978232101847115,
-7.81815701032842));
#78431=CARTESIAN_POINT('Ctrl Pts',(-4.81247494751196,-6.78320051444302,
-7.55355067544256));
#78432=CARTESIAN_POINT('Ctrl Pts',(0.268128670607651,-7.85125227019408,
-7.34186560753389));
#78433=CARTESIAN_POINT('Ctrl Pts',(3.99708534824191,-6.78244845961086,-7.18310180660235));
#78434=CARTESIAN_POINT('Ctrl Pts',(6.73442931917313,-4.04492833004187,-7.02433800567085));
#78435=CARTESIAN_POINT('Ctrl Pts',(8.26945066434343,0.929314750188685,-6.81265293776215));
#78436=CARTESIAN_POINT('Ctrl Pts',(5.77372103956225,5.99550822988587,-6.60096786985345));
#78437=CARTESIAN_POINT('Ctrl Pts',(0.899030133590318,7.79628088171154,-6.38928280194479));
#78438=CARTESIAN_POINT('Ctrl Pts',(-4.23286623301421,7.15906550601515,-6.17759773403607));
#78439=CARTESIAN_POINT('Ctrl Pts',(-8.76722946592603,1.69736673401073,-5.91299139915023));
#78440=CARTESIAN_POINT('Ctrl Pts',(-6.15618039911467,-6.45977083438301,
-5.59546379728718));
#78441=CARTESIAN_POINT('Ctrl Pts',(0.685852659936336,-8.28862657288868,
-5.33085746240133));
#78442=CARTESIAN_POINT('Ctrl Pts',(5.26072467283561,-5.8342806850866,-5.11917239449263));
#78443=CARTESIAN_POINT('Ctrl Pts',(7.42549688033595,-2.61539566255192,-4.96040859356112));
#78444=CARTESIAN_POINT('Ctrl Pts',(7.75707317795147,1.24169204937703,-4.80164479262961));
#78445=CARTESIAN_POINT('Ctrl Pts',(5.72848994081137,6.03587965844944,-4.58995972472091));
#78446=CARTESIAN_POINT('Ctrl Pts',(0.556800633788882,8.30493507094121,-4.37827465681223));
#78447=CARTESIAN_POINT('Ctrl Pts',(-4.33234302682892,6.54377984920668,-4.16658958890353));
#78448=CARTESIAN_POINT('Ctrl Pts',(-7.8484024721132,2.75171840433465,-3.95490452099485));
#78449=CARTESIAN_POINT('Ctrl Pts',(-7.80071051403226,-4.34675524787344,
-3.69029818610897));
#78450=CARTESIAN_POINT('Ctrl Pts',(-0.550469304142969,-8.90641235122975,
-3.37277058424596));
#78451=CARTESIAN_POINT('Ctrl Pts',(5.86195646064047,-5.89993138798228,-3.10816424936009));
#78452=CARTESIAN_POINT('Ctrl Pts',(7.78175319073645,-1.07627662134248,-2.8964791814514));
#78453=CARTESIAN_POINT('Ctrl Pts',(7.3652987460188,2.78040956315781,-2.73771538051989));
#78454=CARTESIAN_POINT('Ctrl Pts',(5.13532728862757,5.94494631292473,-2.57895157958836));
#78455=CARTESIAN_POINT('Ctrl Pts',(0.496199514237444,8.30669900125524,-2.36726651167968));
#78456=CARTESIAN_POINT('Ctrl Pts',(-4.92171466373837,6.71257634901686,-2.15558144377098));
#78457=CARTESIAN_POINT('Ctrl Pts',(-7.52831455255968,2.21691570125815,-1.9438963758623));
#78458=CARTESIAN_POINT('Ctrl Pts',(-7.77664582632939,-2.94843397217774,
-1.73221130795361));
#78459=CARTESIAN_POINT('Ctrl Pts',(-3.16929139916222,-8.34869217407772,
-1.46760497306774));
#78460=CARTESIAN_POINT('Ctrl Pts',(5.31384412439784,-7.16871275278065,-1.15007737120471));
#78461=CARTESIAN_POINT('Ctrl Pts',(8.28405293463262,-0.739317465192835,
-0.885471036318848));
#78462=CARTESIAN_POINT('Ctrl Pts',(6.64675881376857,4.18731958863545,-0.673785968410167));
#78463=CARTESIAN_POINT('Ctrl Pts',(3.84485665727322,6.8700648328613,-0.515022167478636));
#78464=CARTESIAN_POINT('Ctrl Pts',(0.100771147807785,7.85493665872597,-0.356258366547131));
#78465=CARTESIAN_POINT('Ctrl Pts',(-4.96885597231511,6.67545165970414,-0.144573298638437));
#78466=CARTESIAN_POINT('Ctrl Pts',(-8.08861889150961,1.96550321891304,0.0671117692702526));
#78467=CARTESIAN_POINT('Ctrl Pts',(-7.18657111473999,-3.15026676281351,
0.278796837178939));
#78468=CARTESIAN_POINT('Ctrl Pts',(-4.05317016702944,-7.26622277449979,
0.490481905087635));
#78469=CARTESIAN_POINT('Ctrl Pts',(2.9550269927459,-8.42224224643628,0.755088239973491));
#78470=CARTESIAN_POINT('Ctrl Pts',(8.67501344887474,-2.07353332355263,1.07261584183653));
#78471=CARTESIAN_POINT('Ctrl Pts',(6.45326796117271,6.15716910628112,1.39014344369957));
#78472=CARTESIAN_POINT('Ctrl Pts',(-1.68444987226829,8.76521406545941,1.70767104556259));
#78473=CARTESIAN_POINT('Ctrl Pts',(-7.15900251768137,4.23967743624303,1.97227738044847));
#78474=CARTESIAN_POINT('Ctrl Pts',(-7.79563090895679,-0.893937243558322,
2.18396244835714));
#78475=CARTESIAN_POINT('Ctrl Pts',(-6.00088516313695,-5.76873779387534,
2.39564751626584));
#78476=CARTESIAN_POINT('Ctrl Pts',(-0.934827019873464,-8.26905574884899,
2.60733258417452));
#78477=CARTESIAN_POINT('Ctrl Pts',(4.03970536080434,-6.73728174672223,2.81901765208321));
#78478=CARTESIAN_POINT('Ctrl Pts',(6.77963693050073,-4.00215399669808,2.97778145301474));
#78479=CARTESIAN_POINT('Ctrl Pts',(7.85098939493397,-0.273886082915279,
3.13654525394624));
#78480=CARTESIAN_POINT('Ctrl Pts',(6.78679261263705,4.80744936231159,3.34823032185494));
#78481=CARTESIAN_POINT('Ctrl Pts',(0.984744855677549,8.86891534966339,3.6128366567408));
#78482=CARTESIAN_POINT('Ctrl Pts',(-6.93988327278603,5.61988337516134,3.93036425860384));
#78483=CARTESIAN_POINT('Ctrl Pts',(-8.20399225474943,-1.36528175863787,
4.19497059348969));
#78484=CARTESIAN_POINT('Ctrl Pts',(-5.39017638200938,-5.7040541546864,4.40665566139839));
#78485=CARTESIAN_POINT('Ctrl Pts',(-0.875407750237295,-8.27741612723811,
4.61834072930707));
#78486=CARTESIAN_POINT('Ctrl Pts',(4.60875000304047,-6.92870014251292,4.83002579721577));
#78487=CARTESIAN_POINT('Ctrl Pts',(7.42929944027226,-2.55332779949047,5.04171086512445));
#78488=CARTESIAN_POINT('Ctrl Pts',(7.76396873616646,1.30349239385412,5.20047466605597));
#78489=CARTESIAN_POINT('Ctrl Pts',(6.18316230225275,4.84588052176129,5.35923846698748));
#78490=CARTESIAN_POINT('Ctrl Pts',(2.09686003902976,8.04828565012845,5.57092353489619));
#78491=CARTESIAN_POINT('Ctrl Pts',(-4.95742538367269,7.41964493694006,5.83552986978204));
#78492=CARTESIAN_POINT('Ctrl Pts',(-8.92842666789117,-0.169005753564876,
6.15305747164507));
#78493=CARTESIAN_POINT('Ctrl Pts',(-5.39767238427704,-6.32728285862421,
6.41766380653094));
#78494=CARTESIAN_POINT('Ctrl Pts',(-0.451030042432455,-7.83497432783414,
6.62934887443963));
#78495=CARTESIAN_POINT('Ctrl Pts',(4.66023197702472,-6.89668118725614,6.84103394234832));
#78496=CARTESIAN_POINT('Ctrl Pts',(7.98764987690763,-2.33342874268697,7.05271901025701));
#78497=CARTESIAN_POINT('Ctrl Pts',(7.32824174607405,2.83034562283092,7.26440407816568));
#78498=CARTESIAN_POINT('Ctrl Pts',(5.10080854487034,5.9966699575808,7.42316787909722));
#78499=CARTESIAN_POINT('Ctrl Pts',(1.6103299596797,7.68901115987702,7.58193168002873));
#78500=CARTESIAN_POINT('Ctrl Pts',(-3.57816348256826,7.50789387431347,7.79361674793741));
#78501=CARTESIAN_POINT('Ctrl Pts',(-8.57054957278509,2.48452739160254,8.05822308282328));
#78502=CARTESIAN_POINT('Ctrl Pts',(-6.72224604055467,-5.87850104262768,
8.37575068468631));
#78503=CARTESIAN_POINT('Ctrl Pts',(-0.0554521657819921,-8.31662795388359,
8.64035701957219));
#78504=CARTESIAN_POINT('Ctrl Pts',(4.70002003081336,-6.28490751543709,8.85204208748085));
#78505=CARTESIAN_POINT('Ctrl Pts',(8.00642217931619,-2.27578062735984,9.06372715538958));
#78506=CARTESIAN_POINT('Ctrl Pts',(7.61383333599314,3.35812181533772,9.27541222329822));
#78507=CARTESIAN_POINT('Ctrl Pts',(3.78426551438176,6.88428049739225,9.48709729120694));
#78508=CARTESIAN_POINT('Ctrl Pts',(0.0412122757921709,7.87252182827916,
9.64586109213845));
#78509=CARTESIAN_POINT('Ctrl Pts',(-3.71905970950459,6.91972904609487,9.80462489306996));
#78510=CARTESIAN_POINT('Ctrl Pts',(-7.57211199967683,3.44018083883985,10.0163099609787));
#78511=CARTESIAN_POINT('Ctrl Pts',(-8.15710102430372,-3.61785837417917,
10.2809162958645));
#78512=CARTESIAN_POINT('Ctrl Pts',(-1.35785331291593,-8.82618834600539,
10.5984438977276));
#78513=CARTESIAN_POINT('Ctrl Pts',(5.31282029565194,-6.39869642758869,10.8630502326134));
#78514=CARTESIAN_POINT('Ctrl Pts',(7.64293017155263,-1.78209684365176,11.0747353005222));
#78515=CARTESIAN_POINT('Ctrl Pts',(7.59107509017759,3.41431582500192,11.2864203684308));
#78516=CARTESIAN_POINT('Ctrl Pts',(3.66292364276056,7.47197635048085,11.4981054363395));
#78517=CARTESIAN_POINT('Ctrl Pts',(-1.53761544457804,7.70387708849976,11.7097905042482));
#78518=CARTESIAN_POINT('Ctrl Pts',(-5.03774613814279,6.04974480751453,11.8685543051797));
#78519=CARTESIAN_POINT('Ctrl Pts',(-7.3011793187762,2.89945438820694,12.0273181061112));
#78520=CARTESIAN_POINT('Ctrl Pts',(-8.00856867091811,-2.2437807786793,12.2390031740199));
#78521=CARTESIAN_POINT('Ctrl Pts',(-3.91132400815189,-8.02051998560973,
12.5036095089058));
#78522=CARTESIAN_POINT('Ctrl Pts',(4.64447927735037,-7.62719991745463,12.8211371107688));
#78523=CARTESIAN_POINT('Ctrl Pts',(8.18505005722536,-1.47456129985973,13.0857434456547));
#78524=CARTESIAN_POINT('Ctrl Pts',(6.99507702683413,3.55796966766715,13.2974285135634));
#78525=CARTESIAN_POINT('Ctrl Pts',(3.60932701092508,7.50031546708409,13.5091135814721));
#78526=CARTESIAN_POINT('Ctrl Pts',(-2.0088825441779,8.07538427064232,13.7207986493808));
#78527=CARTESIAN_POINT('Ctrl Pts',(-6.13710159400592,4.90407661797473,13.9324837172894));
#78528=CARTESIAN_POINT('Ctrl Pts',(-7.74989581925343,1.38470689286203,14.091247518221));
#78529=CARTESIAN_POINT('Ctrl Pts',(-7.45309532156961,-2.48302745087824,
14.2500113191525));
#78530=CARTESIAN_POINT('Ctrl Pts',(-4.68247960285998,-6.87358051588703,
14.4616963870612));
#78531=CARTESIAN_POINT('Ctrl Pts',(2.1720517209044,-8.6550209507561,14.726302721947));
#78532=CARTESIAN_POINT('Ctrl Pts',(8.46476580741211,-2.84483851285514,15.0438303238101));
#78533=CARTESIAN_POINT('Ctrl Pts',(7.21182047590841,4.14234485401649,15.3084366586959));
#78534=CARTESIAN_POINT('Ctrl Pts',(3.06083172580491,7.22644863772574,15.5201217266046));
#78535=CARTESIAN_POINT('Ctrl Pts',(-2.06813706012608,8.06255435194748,15.7318067945133));
#78536=CARTESIAN_POINT('Ctrl Pts',(-6.73688556628923,4.8848554801103,15.943491862422));
#78537=CARTESIAN_POINT('Ctrl Pts',(-7.85328532036503,-0.199732638934405,
16.1551769303307));
#78538=CARTESIAN_POINT('Ctrl Pts',(-6.82102814845832,-3.93088709916232,
16.3139407312622));
#78539=CARTESIAN_POINT('Ctrl Pts',(-4.1034353000989,-6.69894573288364,16.4727045321937));
#78540=CARTESIAN_POINT('Ctrl Pts',(0.843508648565539,-8.27406898082055,
16.6843896001024));
#78541=CARTESIAN_POINT('Ctrl Pts',(7.23496495736793,-5.22326319478244,16.9489959349882));
#78542=CARTESIAN_POINT('Ctrl Pts',(8.30817833769211,3.27407071512828,17.2665235368513));
#78543=CARTESIAN_POINT('Ctrl Pts',(2.85036941342305,7.81311523486957,17.5311298717372));
#78544=CARTESIAN_POINT('Ctrl Pts',(-2.31143825127639,7.49983359668189,17.7428149396458));
#78545=CARTESIAN_POINT('Ctrl Pts',(-6.77395930557603,4.83688421444779,17.9545000075546));
#78546=CARTESIAN_POINT('Ctrl Pts',(-8.29979865471094,-0.600651717802035,
18.1661850754632));
#78547=CARTESIAN_POINT('Ctrl Pts',(-5.87987775571883,-5.20970450485624,
18.377870143372));
#78548=CARTESIAN_POINT('Ctrl Pts',(-2.68753909621523,-7.39969134455864,
18.5366339443034));
#78549=CARTESIAN_POINT('Ctrl Pts',(1.17408020208218,-7.7675987842638,18.695397745235));
#78550=CARTESIAN_POINT('Ctrl Pts',(5.9732038790861,-5.7872756767284,18.9070828131436));
#78551=CARTESIAN_POINT('Ctrl Pts',(8.89878308796401,0.662461991117818,19.1716891480295));
#78552=CARTESIAN_POINT('Ctrl Pts',(4.24828401123849,7.85477238998132,19.4892167498925));
#78553=CARTESIAN_POINT('Ctrl Pts',(-2.85022797253053,7.81316683368111,19.7538230847783));
#78554=CARTESIAN_POINT('Ctrl Pts',(-6.59775985214242,4.24968418836499,19.9655081526871));
#78555=CARTESIAN_POINT('Ctrl Pts',(-8.29727381828563,-0.661226709960443,
20.1771932205958));
#78556=CARTESIAN_POINT('Ctrl Pts',(-5.96334178721012,-5.80396372522722,
20.3888782885045));
#78557=CARTESIAN_POINT('Ctrl Pts',(-1.14401538716822,-7.77207901684218,
20.6005633564131));
#78558=CARTESIAN_POINT('Ctrl Pts',(2.7085961530172,-7.39200955547825,20.7593271573447));
#78559=CARTESIAN_POINT('Ctrl Pts',(5.89999520691335,-5.18691736512331,20.9180909582762));
#78560=CARTESIAN_POINT('Ctrl Pts',(8.2965982924794,-0.581533415041086,21.1297760261849));
#78561=CARTESIAN_POINT('Ctrl Pts',(6.38181938745116,6.23695259259394,21.3943823610707));
#78562=CARTESIAN_POINT('Ctrl Pts',(-1.80751789403929,8.74518412620829,21.7119099629338));
#78563=CARTESIAN_POINT('Ctrl Pts',(-7.2117454860696,4.14247540855493,21.9765162978196));
#78564=CARTESIAN_POINT('Ctrl Pts',(-7.78435486756486,-0.997030623000835,
22.1882013657284));
#78565=CARTESIAN_POINT('Ctrl Pts',(-5.92240458111352,-5.84868340356868,
22.399886433637));
#78566=CARTESIAN_POINT('Ctrl Pts',(-0.825217461337168,-8.28048647944938,
22.6115715015457));
#78567=CARTESIAN_POINT('Ctrl Pts',(4.12932257752919,-6.68301417781114,22.8232565694544));
#78568=CARTESIAN_POINT('Ctrl Pts',(6.83219228398968,-3.91145075170492,22.982020370386));
#78569=CARTESIAN_POINT('Ctrl Pts',(7.85400392738354,-0.169344332240322,
23.1407841713174));
#78570=CARTESIAN_POINT('Ctrl Pts',(6.7221263281516,4.89742197160429,23.3524692392262));
#78571=CARTESIAN_POINT('Ctrl Pts',(0.866581172239455,8.88122927348642,23.617075574112));
#78572=CARTESIAN_POINT('Ctrl Pts',(-7.01412076883092,5.52697712848645,23.934603175975));
#78573=CARTESIAN_POINT('Ctrl Pts',(-8.18507674979193,-1.47441312607569,
24.1992095108609));
#78574=CARTESIAN_POINT('Ctrl Pts',(-5.31374315308747,-5.77532548610016,
24.4108945787696));
#78575=CARTESIAN_POINT('Ctrl Pts',(-0.765100799302659,-8.28834086801934,
24.6225796466782));
#78576=CARTESIAN_POINT('Ctrl Pts',(4.70060641120063,-6.86671242748808,24.834264714587));
#78577=CARTESIAN_POINT('Ctrl Pts',(7.46264283011114,-2.45416899179898,25.0459497824956));
#78578=CARTESIAN_POINT('Ctrl Pts',(7.74592195511079,1.40676631099648,25.2047135834272));
#78579=CARTESIAN_POINT('Ctrl Pts',(6.11808374448742,4.92778920913389,25.3634773843586));
#78580=CARTESIAN_POINT('Ctrl Pts',(1.98949854169024,8.07549502459095,25.5751624522674));
#78581=CARTESIAN_POINT('Ctrl Pts',(-5.05578988172845,7.35297116872643,25.8397687871532));
#78582=CARTESIAN_POINT('Ctrl Pts',(-8.92538445154858,-0.287886662789833,
26.1572963890163));
#78583=CARTESIAN_POINT('Ctrl Pts',(-5.31293613005572,-6.39860024882612,
26.4219027239021));
#78584=CARTESIAN_POINT('Ctrl Pts',(-0.346655166516884,-7.84028577048752,
26.6335877918108));
#78585=CARTESIAN_POINT('Ctrl Pts',(4.75165881922995,-6.83401141667239,26.8452728597195));
#78586=CARTESIAN_POINT('Ctrl Pts',(8.01801485379917,-2.22685383424587,27.0569579276282));
#78587=CARTESIAN_POINT('Ctrl Pts',(7.28990149564492,2.92768161416345,27.2686429955369));
#78588=CARTESIAN_POINT('Ctrl Pts',(5.02050125533267,6.06406345065949,27.4274067964684));
#78589=CARTESIAN_POINT('Ctrl Pts',(1.507796009611,7.70977343296281,27.5861705973999));
#78590=CARTESIAN_POINT('Ctrl Pts',(-3.67782551435031,7.45957933301706,27.7978556653086));
#78591=CARTESIAN_POINT('Ctrl Pts',(-8.60287498137043,2.37017686918522,28.0624620001945));
#78592=CARTESIAN_POINT('Ctrl Pts',(-6.64336858336157,-5.96749697982012,
28.3799896020575));
#78593=CARTESIAN_POINT('Ctrl Pts',(0.0553016102434953,-8.31662895638818,
28.6445959369434));
#78594=CARTESIAN_POINT('Ctrl Pts',(4.78329661923949,-6.22176214747512,28.856281004852));
#78595=CARTESIAN_POINT('Ctrl Pts',(8.03601782043171,-2.16896084964146,29.0679660727609));
#78596=CARTESIAN_POINT('Ctrl Pts',(7.56843959863063,3.4592141068051,29.2796511406694));
#78597=CARTESIAN_POINT('Ctrl Pts',(3.69225504524338,6.93406346459216,29.4913362085781));
#78598=CARTESIAN_POINT('Ctrl Pts',(-0.0636262725448295,7.87237258301866,
29.6501000095096));
#78599=CARTESIAN_POINT('Ctrl Pts',(-3.81087691677871,6.86959040404745,29.8088638104412));
#78600=CARTESIAN_POINT('Ctrl Pts',(-7.61725195378524,3.33904133130091,30.0205488783499));
#78601=CARTESIAN_POINT('Ctrl Pts',(-8.1082003188195,-3.72616209070479,30.2851552132357));
#78602=CARTESIAN_POINT('Ctrl Pts',(-1.24019846339322,-8.84348766663666,
30.6026828150987));
#78603=CARTESIAN_POINT('Ctrl Pts',(5.39755782418636,-6.32738057974178,30.8672891499846));
#78604=CARTESIAN_POINT('Ctrl Pts',(7.66598387445893,-1.68016130294613,31.0789742178933));
#78605=CARTESIAN_POINT('Ctrl Pts',(7.54493505998739,3.51510007228062,31.290659285802));
#78606=CARTESIAN_POINT('Ctrl Pts',(3.56309784696235,7.52009135102838,31.5023443537107));
#78607=CARTESIAN_POINT('Ctrl Pts',(-1.64006823190909,7.68271824582937,31.7140294216193));
#78608=CARTESIAN_POINT('Ctrl Pts',(-5.1178612227958,5.98212294195165,31.8727932225509));
#78609=CARTESIAN_POINT('Ctrl Pts',(-7.33914268111359,2.80197071727642,32.0315570234824));
#78610=CARTESIAN_POINT('Ctrl Pts',(-7.97797911978374,-2.35022839398137,
32.2432420913911));
#78611=CARTESIAN_POINT('Ctrl Pts',(-3.80417147369922,-8.07189418507224,
32.5078484262769));
#78612=CARTESIAN_POINT('Ctrl Pts',(4.74563550526883,-7.5646751410546,32.82537602814));
#78613=CARTESIAN_POINT('Ctrl Pts',(8.20396037581917,-1.36543385717473,33.0899823630259));
#78614=CARTESIAN_POINT('Ctrl Pts',(6.9470768686315,3.65080453444267,33.3016674309345));
#78615=CARTESIAN_POINT('Ctrl Pts',(3.50912858801016,7.54771423216215,33.5133524988433));
#78616=CARTESIAN_POINT('Ctrl Pts',(-2.11624074155345,8.04791683099602,33.7250375667519));
#78617=CARTESIAN_POINT('Ctrl Pts',(-6.20186284261742,4.8219167072315,33.9367226346606));
#78618=CARTESIAN_POINT('Ctrl Pts',(-7.76764817123625,1.2813821741822,34.0954864355922));
#78619=CARTESIAN_POINT('Ctrl Pts',(-7.41936908165992,-2.58205685923576,
34.2542502365237));
#78620=CARTESIAN_POINT('Ctrl Pts',(-4.5905319766373,-6.93532555191544,34.4659353044323));
#78621=CARTESIAN_POINT('Ctrl Pts',(2.2871142156941,-8.62532926331976,34.7305416393182));
#78622=CARTESIAN_POINT('Ctrl Pts',(8.50189869988551,-2.73186471763199,35.0480692411812));
#78623=CARTESIAN_POINT('Ctrl Pts',(7.15601923311525,4.23801418138421,35.3126755760671));
#78624=CARTESIAN_POINT('Ctrl Pts',(2.96432890111406,7.26656761706666,35.5243606439757));
#78625=CARTESIAN_POINT('Ctrl Pts',(-2.17531915308836,8.03429898371857,35.7360457118845));
#78626=CARTESIAN_POINT('Ctrl Pts',(-6.80133767308289,4.79471021559624,35.9477307797929));
#78627=CARTESIAN_POINT('Ctrl Pts',(-7.84992922384292,-0.304293658780176,
36.1594158477019));
#78628=CARTESIAN_POINT('Ctrl Pts',(-6.76807744641505,-4.02137116761797,
36.3181796486333));
#78629=CARTESIAN_POINT('Ctrl Pts',(-4.01386455155247,-6.75299537657241,
36.4769434495648));
#78630=CARTESIAN_POINT('Ctrl Pts',(0.953615975297951,-8.26210269309442,
36.6886285174736));
#78631=CARTESIAN_POINT('Ctrl Pts',(7.30387932579855,-5.12645522076245,36.9532348523594));
#78632=CARTESIAN_POINT('Ctrl Pts',(8.26384230461509,3.38441674487815,37.2707624542225));
#78633=CARTESIAN_POINT('Ctrl Pts',(2.74607287046835,7.85037956129559,37.5353687891083));
#78634=CARTESIAN_POINT('Ctrl Pts',(-2.41110526728106,7.46838819006294,37.747053857017));
#78635=CARTESIAN_POINT('Ctrl Pts',(-6.83776931292273,4.74624950890969,37.9587389249257));
#78636=CARTESIAN_POINT('Ctrl Pts',(-8.2910641039737,-0.711123209182693,
38.1704239928344));
#78637=CARTESIAN_POINT('Ctrl Pts',(-5.80998105857133,-5.2875422976236,38.3821090607431));
#78638=CARTESIAN_POINT('Ctrl Pts',(-2.58876237455158,-7.43482398961316,
38.5408728616746));
#78639=CARTESIAN_POINT('Ctrl Pts',(1.27741377748707,-7.75127532960252,38.6996366626061));
#78640=CARTESIAN_POINT('Ctrl Pts',(6.04974083194368,-5.70722000678919,38.9113217305148));
#78641=CARTESIAN_POINT('Ctrl Pts',(8.88917232560822,0.78090441281303,39.1759280654007));
#78642=CARTESIAN_POINT('Ctrl Pts',(4.14330878626316,7.91064843361354,39.4934556672637));
#78643=CARTESIAN_POINT('Ctrl Pts',(-2.95401973467792,7.77451881941656,39.7580620021495));
#78644=CARTESIAN_POINT('Ctrl Pts',(-6.65376599972446,4.16144791969008,39.9697470700583));
#78645=CARTESIAN_POINT('Ctrl Pts',(-8.28773284102336,-0.771659208068619,
40.1814321379668));
#78646=CARTESIAN_POINT('Ctrl Pts',(-5.88552420195028,-5.88286027907313,
40.3931172058756));
#78647=CARTESIAN_POINT('Ctrl Pts',(-1.04041660659482,-7.7866242194444,40.6048022737843));
#78648=CARTESIAN_POINT('Ctrl Pts',(2.80679210820641,-7.35528493327974,40.7635660747157));
#78649=CARTESIAN_POINT('Ctrl Pts',(5.96854394481355,-5.10788981606378,40.9223298756474));
#78650=CARTESIAN_POINT('Ctrl Pts',(8.30360666248527,-0.470999717952826,
41.134014943556));
#78651=CARTESIAN_POINT('Ctrl Pts',(6.29819877468409,6.32138343488813,41.3986212784418));
#78652=CARTESIAN_POINT('Ctrl Pts',(-1.92381337494631,8.72033877994056,41.7161488803048));
#78653=CARTESIAN_POINT('Ctrl Pts',(-7.26626954003949,4.04607247065895,41.9807552151907));
#78654=CARTESIAN_POINT('Ctrl Pts',(-7.7703876181543,-1.10060303062287,42.1924402830995));
#78655=CARTESIAN_POINT('Ctrl Pts',(-5.84399511353304,-5.92703084947052,
42.4041253510082));
#78656=CARTESIAN_POINT('Ctrl Pts',(-0.71487671085122,-8.29074131083116,
42.6158104189167));
#78657=CARTESIAN_POINT('Ctrl Pts',(4.21795117979728,-6.62743323579823,42.8274954868256));
#78658=CARTESIAN_POINT('Ctrl Pts',(6.88367353941432,-3.82012264085702,42.9862592877569));
#78659=CARTESIAN_POINT('Ctrl Pts',(7.85556260206146,-0.0647410172293493,
43.1450230886886));
#78660=CARTESIAN_POINT('Ctrl Pts',(6.65631347790844,4.98650330626542,43.3567081565972));
#78661=CARTESIAN_POINT('Ctrl Pts',(0.748236927761726,8.8919816596889,43.621314491483));
#78662=CARTESIAN_POINT('Ctrl Pts',(-7.08709914359345,5.43308310882824,43.938842093346));
#78663=CARTESIAN_POINT('Ctrl Pts',(-8.1647168768334,-1.58327944074342,44.2034484282321));
#78664=CARTESIAN_POINT('Ctrl Pts',(-5.236364530052,-5.84557416134595,44.4151334961406));
#78665=CARTESIAN_POINT('Ctrl Pts',(-0.654660785897164,-8.29779445593723,
44.6268185640494));
#78666=CARTESIAN_POINT('Ctrl Pts',(4.79163058654542,-6.80350766273701,44.8385036319579));
#78667=CARTESIAN_POINT('Ctrl Pts',(7.49466220675512,-2.3545746657842,45.0501886998668));
#78668=CARTESIAN_POINT('Ctrl Pts',(7.72650184443749,1.50979059353471,45.2089525007983));
#78669=CARTESIAN_POINT('Ctrl Pts',(6.05192006718989,5.00882408301219,45.3677163017298));
#78670=CARTESIAN_POINT('Ctrl Pts',(1.88178433583927,8.10127224903418,45.5794013696383));
#78671=CARTESIAN_POINT('Ctrl Pts',(-5.15325785597106,7.28499346644748,45.8440077045244));
#78672=CARTESIAN_POINT('Ctrl Pts',(-8.92075938457942,-0.4067165364164,46.1615353063873));
#78673=CARTESIAN_POINT('Ctrl Pts',(-5.22725770400791,-6.4687829119718,46.4261416412733));
#78674=CARTESIAN_POINT('Ctrl Pts',(-0.242218808112939,-7.84420683156551,
46.637826709182));
#78675=CARTESIAN_POINT('Ctrl Pts',(4.84224300288465,-6.77012970914063,46.8495117770905));
#78676=CARTESIAN_POINT('Ctrl Pts',(8.04695793050456,-2.1198840203015,47.0611968449994));
#78677=CARTESIAN_POINT('Ctrl Pts',(7.25026846303026,3.02449841529221,47.272881912908));
#78678=CARTESIAN_POINT('Ctrl Pts',(4.93930363797658,6.13038155095525,47.4316457138395));
#78679=CARTESIAN_POINT('Ctrl Pts',(1.4049946687936,7.72916846593991,47.5904095147711));
#78680=CARTESIAN_POINT('Ctrl Pts',(-3.77683532552611,7.40994192038234,47.8020945826797));
#78681=CARTESIAN_POINT('Ctrl Pts',(-8.63367476846056,2.25540602303826,48.0667009175657));
#78682=CARTESIAN_POINT('Ctrl Pts',(-6.56331300052723,-6.05543464960746,
48.3842285194284));
#78683=CARTESIAN_POINT('Ctrl Pts',(0.166045579120638,-8.31515509969495,
48.6488348543146));
#78684=CARTESIAN_POINT('Ctrl Pts',(4.86572494464703,-6.15751342105094,48.860519922223));
#78685=CARTESIAN_POINT('Ctrl Pts',(8.06418836553557,-2.06175643147653,49.072204990132));
#78686=CARTESIAN_POINT('Ctrl Pts',(7.52170368493643,3.55969294614753,49.2838900580404));
#78687=CARTESIAN_POINT('Ctrl Pts',(3.59958979683137,6.98261675481792,49.4955751259492));
#78688=CARTESIAN_POINT('Ctrl Pts',(-0.168453537486675,7.870827262374,49.6543389268806));
#78689=CARTESIAN_POINT('Ctrl Pts',(-3.90201830854838,6.81823351858615,49.8131027278124));
#78690=CARTESIAN_POINT('Ctrl Pts',(-7.66104107524026,3.2373096829101,50.0247877957208));
#78691=CARTESIAN_POINT('Ctrl Pts',(-8.0578617165962,-3.83380501493248,50.2893941306069));
#78692=CARTESIAN_POINT('Ctrl Pts',(-1.12232367883472,-8.85921869571382,
50.6069217324699));
#78693=CARTESIAN_POINT('Ctrl Pts',(5.4813381574754,-6.25494264320094,50.8715280673556));
#78694=CARTESIAN_POINT('Ctrl Pts',(7.68767810266248,-1.57792780481932,51.0832131352645));
#78695=CARTESIAN_POINT('Ctrl Pts',(7.49745702172037,3.61526095670117,51.294898203173));
#78696=CARTESIAN_POINT('Ctrl Pts',(3.46264017644585,7.56687274924533,51.5065832710818));
#78697=CARTESIAN_POINT('Ctrl Pts',(-1.7422301718647,7.66019696080821,51.7182683389905));
#78698=CARTESIAN_POINT('Ctrl Pts',(-5.1970687132064,5.91344021519166,51.8770321399219));
#78699=CARTESIAN_POINT('Ctrl Pts',(-7.3758045302931,2.70399014884053,52.0357959408536));
#78700=CARTESIAN_POINT('Ctrl Pts',(-7.94597476517177,-2.45625922312734,
52.247481008762));
#78701=CARTESIAN_POINT('Ctrl Pts',(-3.69634431283579,-8.12183692624851,
52.5120873436481));
#78702=CARTESIAN_POINT('Ctrl Pts',(4.84595014885174,-7.50080885594317,52.829614945511));
#78703=CARTESIAN_POINT('Ctrl Pts',(8.22141581583643,-1.25606427031315,53.094221280397));
#78704=CARTESIAN_POINT('Ctrl Pts',(6.89784472552101,3.74299197262333,53.3059063483056));
#78705=CARTESIAN_POINT('Ctrl Pts',(3.40830786160718,7.59377449656253,53.5175914162142));
#78706=CARTESIAN_POINT('Ctrl Pts',(-2.22322364860433,8.01902218468158,53.729276484123));
#78707=CARTESIAN_POINT('Ctrl Pts',(-6.26552426067689,4.73890168526058,53.9409615520318));
#78708=CARTESIAN_POINT('Ctrl Pts',(-7.78402302158592,1.17783021567688,54.0997253529632));
#78709=CARTESIAN_POINT('Ctrl Pts',(-7.38432709758672,-2.68062836686848,
54.2584891538947));
#78710=CARTESIAN_POINT('Ctrl Pts',(-4.49777028015197,-6.9958406923907,54.4701742218034));
#78711=CARTESIAN_POINT('Ctrl Pts',(2.40177113378299,-8.5941079613927,54.7347805566892));
#78712=CARTESIAN_POINT('Ctrl Pts',(8.53752384820599,-2.61840647632836,55.0523081585523));
#78713=CARTESIAN_POINT('Ctrl Pts',(7.09894900150471,4.33293197708344,55.3169144934381));
#78714=CARTESIAN_POINT('Ctrl Pts',(2.86730032066488,7.3053979113412,55.5285995613469));
#78715=CARTESIAN_POINT('Ctrl Pts',(-2.28211530840029,8.00461893317224,55.7402846292555));
#78716=CARTESIAN_POINT('Ctrl Pts',(-6.86458398523512,4.70371444261994,55.9519696971641));
#78717=CARTESIAN_POINT('Ctrl Pts',(-7.84518060577856,-0.408800442089421,
56.163654765073));
#78718=CARTESIAN_POINT('Ctrl Pts',(-6.71392739005728,-4.1111426610001,56.3224185660044));
#78719=CARTESIAN_POINT('Ctrl Pts',(-3.92358037221183,-6.80584641546676,
56.4811823669359));
#78720=CARTESIAN_POINT('Ctrl Pts',(1.06355069377355,-8.24867345891154,56.6928674348446));
#78721=CARTESIAN_POINT('Ctrl Pts',(7.37150566530056,-5.02873348823263,56.9574737697305));
#78722=CARTESIAN_POINT('Ctrl Pts',(8.21802814289185,3.4941544814057,57.2750013715935));
#78723=CARTESIAN_POINT('Ctrl Pts',(2.64131052672665,7.8862653071121,57.5396077064795));
#78724=CARTESIAN_POINT('Ctrl Pts',(-2.51037290578171,7.43560025010796,57.7512927743881));
#78725=CARTESIAN_POINT('Ctrl Pts',(-6.90029409155121,4.65481971884436,57.9629778422968));
#78726=CARTESIAN_POINT('Ctrl Pts',(-8.28100690494395,-0.821563361522968,
58.1746629102055));
#78727=CARTESIAN_POINT('Ctrl Pts',(-5.73887154209026,-5.36432529669737,
58.3863479781142));
#78728=CARTESIAN_POINT('Ctrl Pts',(-2.48990629535911,-7.46888184180529,
58.5451117790458));
#78729=CARTESIAN_POINT('Ctrl Pts',(1.38121344013289,-7.73313279057438,58.7038755799772));
#78730=CARTESIAN_POINT('Ctrl Pts',(6.1237083934355,-5.62711262023186,58.9155606478858));
#78731=CARTESIAN_POINT('Ctrl Pts',(8.88108147570853,0.901195414789174,59.1801669827717));
#78732=CARTESIAN_POINT('Ctrl Pts',(4.03218751616045,7.96164873847342,59.4976945846348));
#78733=CARTESIAN_POINT('Ctrl Pts',(-3.04819441019116,7.74032911124811,59.7623009195206));
#78734=CARTESIAN_POINT('Ctrl Pts',(-6.72082854944846,4.06461054654832,59.9739859874293));
#78735=CARTESIAN_POINT('Ctrl Pts',(-7.86235377363163,0.371140675652209,
60.1327497883608));
#78736=CARTESIAN_POINT('Ctrl Pts',(-7.07298371107766,-3.44494050992081,
60.291520283539));
#78737=CARTESIAN_POINT('Ctrl Pts',(-5.4030676852692,-5.41639781933624,60.39736951174));
#78738=CARTESIAN_POINT('Ctrl Pts',(-4.38130218819444,-6.1449117824308,60.4502974729639));
#78739=CARTESIAN_POINT('Ctrl Pts',(-3.43243190685397,7.15930439800971,-59.9835157911635));
#78740=CARTESIAN_POINT('Ctrl Pts',(-4.6229230465457,6.5885414510915,-59.9305854290092));
#78741=CARTESIAN_POINT('Ctrl Pts',(-6.70940095812955,4.84641564141242,-59.8247337998776));
#78742=CARTESIAN_POINT('Ctrl Pts',(-8.21591943031317,1.033550698178,-59.6659609037689));
#78743=CARTESIAN_POINT('Ctrl Pts',(-7.69901306767222,-3.00047282198764,
-59.5071971028374));
#78744=CARTESIAN_POINT('Ctrl Pts',(-4.55552526345291,-7.47266249378137,
-59.2955120349288));
#78745=CARTESIAN_POINT('Ctrl Pts',(2.74304713445976,-8.9792183345732,-59.0309057000428));
#78746=CARTESIAN_POINT('Ctrl Pts',(9.04227886094756,-2.5360286421388,-58.7133780981799));
#78747=CARTESIAN_POINT('Ctrl Pts',(7.36197121198212,4.72764453598642,-58.4487717632939));
#78748=CARTESIAN_POINT('Ctrl Pts',(2.82647711349423,7.76589593501196,-58.2370866953853));
#78749=CARTESIAN_POINT('Ctrl Pts',(-1.2334285983065,8.19028922052275,-58.0783228944537));
#78750=CARTESIAN_POINT('Ctrl Pts',(-4.98045605042172,6.59506433331062,-57.9195590935222));
#78751=CARTESIAN_POINT('Ctrl Pts',(-8.43469294985433,2.3452514380058,-57.7078740256135));
#78752=CARTESIAN_POINT('Ctrl Pts',(-7.99148361614971,-3.57982560672035,
-57.4961889577049));
#78753=CARTESIAN_POINT('Ctrl Pts',(-3.9431303285702,-7.25383778053677,-57.2845038897961));
#78754=CARTESIAN_POINT('Ctrl Pts',(1.31506405940233,-8.65019871020488,-57.0728188218875));
#78755=CARTESIAN_POINT('Ctrl Pts',(7.8873330128033,-5.10391056925949,-56.8082124870015));
#78756=CARTESIAN_POINT('Ctrl Pts',(8.54732004282932,3.88237251743919,-56.4906848851387));
#78757=CARTESIAN_POINT('Ctrl Pts',(2.5902279706948,8.35753082550421,-56.2260785502526));
#78758=CARTESIAN_POINT('Ctrl Pts',(-2.83896582282601,7.76169102640962,-56.0143934823441));
#78759=CARTESIAN_POINT('Ctrl Pts',(-6.2171077967334,5.47207923197023,-55.8556296814125));
#78760=CARTESIAN_POINT('Ctrl Pts',(-8.05743347284584,1.83882652792089,-55.696865880481));
#78761=CARTESIAN_POINT('Ctrl Pts',(-7.96329140383586,-3.63694420072908,
-55.4851808125723));
#78762=CARTESIAN_POINT('Ctrl Pts',(-3.80919199311957,-7.88477319258719,
-55.2734957446636));
#78763=CARTESIAN_POINT('Ctrl Pts',(1.65406980071603,-8.08892035499237,-55.0618106767549));
#78764=CARTESIAN_POINT('Ctrl Pts',(6.57615857834954,-5.77140446258325,-54.8501256088461));
#78765=CARTESIAN_POINT('Ctrl Pts',(9.32106714971483,1.17385022568006,-54.5855192739605));
#78766=CARTESIAN_POINT('Ctrl Pts',(4.03954258602107,8.47416813178503,-54.2679916720972));
#78767=CARTESIAN_POINT('Ctrl Pts',(-3.39981618129403,8.06218455553205,-54.0033853372115));
#78768=CARTESIAN_POINT('Ctrl Pts',(-7.16998459470855,4.11034366672326,-53.7917002693027));
#78769=CARTESIAN_POINT('Ctrl Pts',(-8.28024482584534,0.183324227672024,
-53.6329364683713));
#78770=CARTESIAN_POINT('Ctrl Pts',(-7.34874032452431,-3.78147331791097,
-53.4741726674397));
#78771=CARTESIAN_POINT('Ctrl Pts',(-3.75075153875775,-7.91032445948964,
-53.2624875995311));
#78772=CARTESIAN_POINT('Ctrl Pts',(2.16278181964522,-8.48539720195137,-53.0508025316223));
#78773=CARTESIAN_POINT('Ctrl Pts',(6.47413724132143,-5.12368300094565,-52.8391174637137));
#78774=CARTESIAN_POINT('Ctrl Pts',(8.74769454875537,-0.181135639340342,
-52.6274323958049));
#78775=CARTESIAN_POINT('Ctrl Pts',(6.37561247902266,6.9001292108873,-52.3628260609192));
#78776=CARTESIAN_POINT('Ctrl Pts',(-2.3660659621478,9.08466630143443,-52.045298459056));
#78777=CARTESIAN_POINT('Ctrl Pts',(-7.79257887986899,3.97910594393446,-51.7806921241703));
#78778=CARTESIAN_POINT('Ctrl Pts',(-8.13243552606366,-1.47210619093496,
-51.5690070562615));
#78779=CARTESIAN_POINT('Ctrl Pts',(-6.45319939494819,-5.19155850253244,
-51.41024325533));
#78780=CARTESIAN_POINT('Ctrl Pts',(-3.18749830448594,-7.62518061277131,
-51.2514794543985));
#78781=CARTESIAN_POINT('Ctrl Pts',(2.22394736708779,-8.46731529314309,-51.0397943864898));
#78782=CARTESIAN_POINT('Ctrl Pts',(7.11864843416257,-5.09945441570212,-50.8281093185811));
#78783=CARTESIAN_POINT('Ctrl Pts',(8.25255779370852,0.248737569150617,-50.6164242506724));
#78784=CARTESIAN_POINT('Ctrl Pts',(6.80943239642104,5.49423338372509,-50.4047391827638));
#78785=CARTESIAN_POINT('Ctrl Pts',(0.434799365288336,9.38462397337061,-50.1401328478779));
#78786=CARTESIAN_POINT('Ctrl Pts',(-7.66006120028907,5.42705190266821,-49.8226052460149));
#78787=CARTESIAN_POINT('Ctrl Pts',(-8.52427109164289,-1.97341634426556,
-49.557998911129));
#78788=CARTESIAN_POINT('Ctrl Pts',(-5.27414620734275,-6.36293847264405,
-49.3463138432203));
#78789=CARTESIAN_POINT('Ctrl Pts',(-1.59434405259234,-8.1273691412489,-49.1875500422887));
#78790=CARTESIAN_POINT('Ctrl Pts',(2.47127825195855,-7.88646363206378,-49.0287862413573));
#78791=CARTESIAN_POINT('Ctrl Pts',(7.15380242627116,-5.04623433968172,-48.8171011734485));
#78792=CARTESIAN_POINT('Ctrl Pts',(8.73006719123986,0.682288577836312,-48.6054161055399));
#78793=CARTESIAN_POINT('Ctrl Pts',(6.15380285543387,5.50429749679883,-48.3937310376312));
#78794=CARTESIAN_POINT('Ctrl Pts',(1.67199672105926,8.5883291157846,-48.1820459697225));
#78795=CARTESIAN_POINT('Ctrl Pts',(-5.71028901498176,7.46008156624264,-47.9174396348366));
#78796=CARTESIAN_POINT('Ctrl Pts',(-9.35524473854869,-0.780272919104606,
-47.5999120329737));
#78797=CARTESIAN_POINT('Ctrl Pts',(-5.25113282817633,-6.99879802055191,
-47.3353056980877));
#78798=CARTESIAN_POINT('Ctrl Pts',(0.0620161441714672,-8.26436677676782,
-47.1236206301791));
#78799=CARTESIAN_POINT('Ctrl Pts',(4.0135580506168,-7.24481979696462,-46.9648568292474));
#78800=CARTESIAN_POINT('Ctrl Pts',(6.96901120128802,-4.44256769163848,-46.8060930283161));
#78801=CARTESIAN_POINT('Ctrl Pts',(8.72269375463095,0.745643231061926,-46.5944079604073));
#78802=CARTESIAN_POINT('Ctrl Pts',(6.23996937726438,6.14348215898863,-46.3827228924987));
#78803=CARTESIAN_POINT('Ctrl Pts',(1.16389899084976,8.17385586219323,-46.17103782459));
#78804=CARTESIAN_POINT('Ctrl Pts',(-4.25096810407249,7.64749895158049,-45.9593527566812));
#78805=CARTESIAN_POINT('Ctrl Pts',(-9.17259792661805,2.03068089226677,-45.6947464217955));
#78806=CARTESIAN_POINT('Ctrl Pts',(-6.65519391252716,-6.6210138145976,-45.3772188199323));
#78807=CARTESIAN_POINT('Ctrl Pts',(0.489066437201014,-8.73603936184105,
-45.1126124850466));
#78808=CARTESIAN_POINT('Ctrl Pts',(5.36904238053102,-6.28307155292245,-44.9009274171378));
#78809=CARTESIAN_POINT('Ctrl Pts',(7.73583035363276,-2.95854539528728,-44.7421636162063));
#78810=CARTESIAN_POINT('Ctrl Pts',(8.19259811029568,1.08851321611066,-44.5833998152748));
#78811=CARTESIAN_POINT('Ctrl Pts',(6.19353266310277,6.18720642262607,-44.3717147473661));
#78812=CARTESIAN_POINT('Ctrl Pts',(0.818240311996971,8.71837563189565,-44.1600296794574));
#78813=CARTESIAN_POINT('Ctrl Pts',(-4.37282208526656,7.00321408550508,-43.9483446115487));
#78814=CARTESIAN_POINT('Ctrl Pts',(-8.17676432328914,3.11375902048511,-43.73665954364));
#78815=CARTESIAN_POINT('Ctrl Pts',(-8.32548268704189,-4.35276413757749,
-43.4720532087542));
#78816=CARTESIAN_POINT('Ctrl Pts',(-0.828433117629804,-9.35110306413339,
-43.1545256068911));
#78817=CARTESIAN_POINT('Ctrl Pts',(5.99949495138197,-6.36895831670886,-42.8899192720053));
#78818=CARTESIAN_POINT('Ctrl Pts',(8.15361193791628,-1.3498950288637,-42.6782342040966));
#78819=CARTESIAN_POINT('Ctrl Pts',(7.82369347155987,2.71769802944199,-42.5194704031651));
#78820=CARTESIAN_POINT('Ctrl Pts',(5.56717948781346,6.10819428054944,-42.3607066022336));
#78821=CARTESIAN_POINT('Ctrl Pts',(0.754556985431625,8.72192719075563,-42.1490215343248));
#78822=CARTESIAN_POINT('Ctrl Pts',(-4.98791033047516,7.19724540377413,-41.9373364664162));
#78823=CARTESIAN_POINT('Ctrl Pts',(-7.85512572654492,2.54235724023673,-41.7256513985074));
#78824=CARTESIAN_POINT('Ctrl Pts',(-8.26099396175561,-2.88287162393748,
-41.5139663305988));
#78825=CARTESIAN_POINT('Ctrl Pts',(-3.56693074773598,-8.69121525740047,
-41.2493599957129));
#78826=CARTESIAN_POINT('Ctrl Pts',(5.38753798751325,-7.687903770179,-40.9318323938499));
#78827=CARTESIAN_POINT('Ctrl Pts',(8.69127070814338,-1.0096450809077,-40.667226058964));
#78828=CARTESIAN_POINT('Ctrl Pts',(7.10749225262746,4.21748243646874,-40.4555409910554));
#78829=CARTESIAN_POINT('Ctrl Pts',(4.23586799310983,7.11712613778268,-40.2967771901239));
#78830=CARTESIAN_POINT('Ctrl Pts',(0.326216400082517,8.25815401156851,-40.1380133891923));
#78831=CARTESIAN_POINT('Ctrl Pts',(-5.03892088698296,7.15895568220903,-39.9263283212837));
#78832=CARTESIAN_POINT('Ctrl Pts',(-8.45066585041011,2.29474128208847,-39.7146432533749));
#78833=CARTESIAN_POINT('Ctrl Pts',(-7.64697342637731,-3.11293718746318,
-39.5029581854663));
#78834=CARTESIAN_POINT('Ctrl Pts',(-4.46408467135861,-7.52508591865946,
-39.2912731175575));
#78835=CARTESIAN_POINT('Ctrl Pts',(2.86741878271786,-8.94640302770514,-39.0266667826717));
#78836=CARTESIAN_POINT('Ctrl Pts',(9.07236289997408,-2.41281191923549,-38.7091391808087));
#78837=CARTESIAN_POINT('Ctrl Pts',(7.29975706379542,4.82401456477915,-38.4445328459229));
#78838=CARTESIAN_POINT('Ctrl Pts',(2.72216605103158,7.80342336501699,-38.2328477780141));
#78839=CARTESIAN_POINT('Ctrl Pts',(-1.34203183253074,8.17282158600294,-38.0740839770826));
#78840=CARTESIAN_POINT('Ctrl Pts',(-5.06800804765613,6.52830906493869,-37.915320176151));
#78841=CARTESIAN_POINT('Ctrl Pts',(-8.46503811194142,2.23259936587045,-37.7036351082425));
#78842=CARTESIAN_POINT('Ctrl Pts',(-7.94317174194882,-3.68586672913096,
-37.4919500403336));
#78843=CARTESIAN_POINT('Ctrl Pts',(-3.84615825894495,-7.3057270113221,-37.2802649724251));
#78844=CARTESIAN_POINT('Ctrl Pts',(1.43011858632153,-8.6319019263036,-37.0685799045163));
#78845=CARTESIAN_POINT('Ctrl Pts',(7.95461194016368,-4.99843640461897,-36.8039735696305));
#78846=CARTESIAN_POINT('Ctrl Pts',(8.49485558088072,3.99585517835802,-36.4864459677674));
#78847=CARTESIAN_POINT('Ctrl Pts',(2.47870800970099,8.39127977809564,-36.2218396328816));
#78848=CARTESIAN_POINT('Ctrl Pts',(-2.94207461054343,7.72319889741794,-36.0101545649728));
#78849=CARTESIAN_POINT('Ctrl Pts',(-6.289424964531,5.38880281061534,-35.8513907640414));
#78850=CARTESIAN_POINT('Ctrl Pts',(-8.08120626336839,1.73136655488185,-35.6926269631098));
#78851=CARTESIAN_POINT('Ctrl Pts',(-7.91415340436405,-3.74266563525237,
-35.4809418952012));
#78852=CARTESIAN_POINT('Ctrl Pts',(-3.70385635277393,-7.93479924037305,
-35.2692568272924));
#78853=CARTESIAN_POINT('Ctrl Pts',(1.76163977452845,-8.06617665450065,-35.0575717593838));
#78854=CARTESIAN_POINT('Ctrl Pts',(6.65243067158831,-5.68332087744279,-34.8458866914751));
#78855=CARTESIAN_POINT('Ctrl Pts',(9.30460904010135,1.29787064859291,-34.5812803565892));
#78856=CARTESIAN_POINT('Ctrl Pts',(3.92633763489875,8.52720955079729,-34.2637527547262));
#78857=CARTESIAN_POINT('Ctrl Pts',(-3.50687526319002,8.0161958309449,-33.9991464198403));
#78858=CARTESIAN_POINT('Ctrl Pts',(-7.22408447090204,4.01449969240922,-33.7874613519316));
#78859=CARTESIAN_POINT('Ctrl Pts',(-8.28195186820398,0.0730436096721498,
-33.6286975510001));
#78860=CARTESIAN_POINT('Ctrl Pts',(-7.2977325088389,-3.87899794378701,-33.4699337500686));
#78861=CARTESIAN_POINT('Ctrl Pts',(-3.64508066652378,-7.95957015796966,
-33.25824868216));
#78862=CARTESIAN_POINT('Ctrl Pts',(2.27558633152054,-8.45584399778082,-33.0465636142511));
#78863=CARTESIAN_POINT('Ctrl Pts',(6.54179300651556,-5.03701546321985,-32.8348785463426));
#78864=CARTESIAN_POINT('Ctrl Pts',(8.7493310000379,-0.0646303956514614,
-32.6231934784338));
#78865=CARTESIAN_POINT('Ctrl Pts',(6.28316118673488,6.98441859506738,-32.358587143548));
#78866=CARTESIAN_POINT('Ctrl Pts',(-2.48683265113032,9.05235291577295,-32.0410595416849));
#78867=CARTESIAN_POINT('Ctrl Pts',(-7.84487591277371,3.87498279026055,-31.7764532067991));
#78868=CARTESIAN_POINT('Ctrl Pts',(-8.11211104120906,-1.58027171023717,
-31.5647681388904));
#78869=CARTESIAN_POINT('Ctrl Pts',(-6.38349350406684,-5.27703257519772,
-31.4060043379588));
#78870=CARTESIAN_POINT('Ctrl Pts',(-3.08567451086231,-7.66695099967925,
-31.2472405370274));
#78871=CARTESIAN_POINT('Ctrl Pts',(2.3365056670397,-8.43694917804998,-31.0355554691186));
#78872=CARTESIAN_POINT('Ctrl Pts',(7.18592440949995,-5.00420635545355,-30.82387040121));
#78873=CARTESIAN_POINT('Ctrl Pts',(8.24851371698094,0.35861117884011,-30.6121853333012));
#78874=CARTESIAN_POINT('Ctrl Pts',(6.73566433098507,5.58442441586969,-30.4005002653926));
#78875=CARTESIAN_POINT('Ctrl Pts',(0.309789921844893,9.38958187641696,-30.1358939305067));
#78876=CARTESIAN_POINT('Ctrl Pts',(-7.73165163989981,5.32456504004463,-29.8183663286437));
#78877=CARTESIAN_POINT('Ctrl Pts',(-8.49723613723125,-2.0867553138219,-29.5537599937579));
#78878=CARTESIAN_POINT('Ctrl Pts',(-5.18894611288327,-6.43260774963586,
-29.3420749258491));
#78879=CARTESIAN_POINT('Ctrl Pts',(-1.48597410012283,-8.14787966835088,
-29.1833111249176));
#78880=CARTESIAN_POINT('Ctrl Pts',(2.57607967638066,-7.85285542458324,-29.0245473239861));
#78881=CARTESIAN_POINT('Ctrl Pts',(7.22036657629709,-4.95052286824314,-28.8128622560774));
#78882=CARTESIAN_POINT('Ctrl Pts',(8.72020736690963,0.798482526486089,-28.6011771881687));
#78883=CARTESIAN_POINT('Ctrl Pts',(6.07995890485837,5.58575690771135,-28.3894921202601));
#78884=CARTESIAN_POINT('Ctrl Pts',(1.55748148291466,8.60983283616151,-28.1778070523513));
#78885=CARTESIAN_POINT('Ctrl Pts',(-5.80912529707869,7.38337869084711,-27.9132007174655));
#78886=CARTESIAN_POINT('Ctrl Pts',(-9.34402466599859,-0.904783392664291,
-27.5956731156025));
#78887=CARTESIAN_POINT('Ctrl Pts',(-5.1574673137037,-7.06810445732873,-27.3310667807166));
#78888=CARTESIAN_POINT('Ctrl Pts',(0.172063565326116,-8.26280813964411,
-27.1193817128079));
#78889=CARTESIAN_POINT('Ctrl Pts',(4.10967823479405,-7.19073062509099,-26.9606179118764));
#78890=CARTESIAN_POINT('Ctrl Pts',(7.02755297464808,-4.34937052997129,-26.8018541109449));
#78891=CARTESIAN_POINT('Ctrl Pts',(8.71199091817952,0.861733373302816,-26.5901690430362));
#78892=CARTESIAN_POINT('Ctrl Pts',(6.15760604669396,6.22603233534218,-26.3784839751275));
#78893=CARTESIAN_POINT('Ctrl Pts',(1.05494816251971,8.18863022069064,-26.1667989072188));
#78894=CARTESIAN_POINT('Ctrl Pts',(-4.35242953761413,7.59021258966908,-25.9551138393102));
#78895=CARTESIAN_POINT('Ctrl Pts',(-9.19882627888814,1.90835340030406,-25.6905075044242));
#78896=CARTESIAN_POINT('Ctrl Pts',(-6.5664346862703,-6.7090510101934,-25.3729799025613));
#78897=CARTESIAN_POINT('Ctrl Pts',(0.605357047477619,-8.72875206181856,
-25.1083735676753));
#78898=CARTESIAN_POINT('Ctrl Pts',(5.45223519853537,-6.21101727279304,-24.8966884997667));
#78899=CARTESIAN_POINT('Ctrl Pts',(7.77454206459834,-2.85526842905397,-24.7379246988352));
#78900=CARTESIAN_POINT('Ctrl Pts',(8.1773764289831,1.19751390688361,-24.5791608979036));
#78901=CARTESIAN_POINT('Ctrl Pts',(6.11059119334711,6.26913434477958,-24.367475829995));
#78902=CARTESIAN_POINT('Ctrl Pts',(0.702069003843994,8.72849872434259,-24.1557907620863));
#78903=CARTESIAN_POINT('Ctrl Pts',(-4.46569305727037,6.94436217625916,-23.9441056941776));
#78904=CARTESIAN_POINT('Ctrl Pts',(-8.21750384820542,3.00459656875853,-23.7324206262689));
#78905=CARTESIAN_POINT('Ctrl Pts',(-8.26678063600234,-4.46324495471978,
-23.467814291383));
#78906=CARTESIAN_POINT('Ctrl Pts',(-0.703835154095096,-9.36130578617593,
-23.15028668952));
#78907=CARTESIAN_POINT('Ctrl Pts',(6.08377558368143,-6.2885009627919,-22.8856803546341));
#78908=CARTESIAN_POINT('Ctrl Pts',(8.17086491846883,-1.24119728778999,-22.6739952867254));
#78909=CARTESIAN_POINT('Ctrl Pts',(7.78680936658882,2.82164172150997,-22.5152314857939));
#78910=CARTESIAN_POINT('Ctrl Pts',(5.48534572612754,6.18178834022344,-22.3564676848624));
#78911=CARTESIAN_POINT('Ctrl Pts',(0.638344029494194,8.73120192557217,-22.1447826169537));
#78912=CARTESIAN_POINT('Ctrl Pts',(-5.08331059235753,7.13018543157429,-21.933097549045));
#78913=CARTESIAN_POINT('Ctrl Pts',(-7.8882846659403,2.43752857335111,-21.7214124811363));
#78914=CARTESIAN_POINT('Ctrl Pts',(-8.22187153789785,-2.99262400755114,
-21.5097274132277));
#78915=CARTESIAN_POINT('Ctrl Pts',(-3.45087739785627,-8.73794385393837,
-21.2451210783418));
#78916=CARTESIAN_POINT('Ctrl Pts',(5.4894366953229,-7.61547862674922,-20.9275934764787));
#78917=CARTESIAN_POINT('Ctrl Pts',(8.70394505668451,-0.893817745320576,
-20.6629871415929));
#78918=CARTESIAN_POINT('Ctrl Pts',(7.0506996865639,4.3117558085969,-20.4513020736842));
#78919=CARTESIAN_POINT('Ctrl Pts',(4.14071677820549,7.17290224935829,-20.2925382727527));
#78920=CARTESIAN_POINT('Ctrl Pts',(0.216217287272026,8.26176584654593,-20.1337744718212));
#78921=CARTESIAN_POINT('Ctrl Pts',(-5.13380673849493,7.09121982009368,-19.9220894039125));
#78922=CARTESIAN_POINT('Ctrl Pts',(-8.48047459139985,2.1820040264926,-19.7104043360038));
#78923=CARTESIAN_POINT('Ctrl Pts',(-7.60484176584855,-3.21449253121196,
-19.4987192680951));
#78924=CARTESIAN_POINT('Ctrl Pts',(-4.36348060053169,-7.58386491737891,
-19.2870342001864));
#78925=CARTESIAN_POINT('Ctrl Pts',(2.9862998261516,-8.90742560776914,-19.0224278653005));
#78926=CARTESIAN_POINT('Ctrl Pts',(9.10368881002332,-2.29178532953828,-18.7049002634375));
#78927=CARTESIAN_POINT('Ctrl Pts',(7.23487052944038,4.92079446165636,-18.4402939285516));
#78928=CARTESIAN_POINT('Ctrl Pts',(2.61800993812571,7.83898132329426,-18.2286088606429));
#78929=CARTESIAN_POINT('Ctrl Pts',(-1.45074668875384,8.15422566288372,-18.0698450597114));
#78930=CARTESIAN_POINT('Ctrl Pts',(-5.15449327773064,6.46024178094735,-17.9110812587799));
#78931=CARTESIAN_POINT('Ctrl Pts',(-8.49401806211714,2.11967623129888,-17.6993961908712));
#78932=CARTESIAN_POINT('Ctrl Pts',(-7.89338436821475,-3.79131561369287,
-17.4877111229625));
#78933=CARTESIAN_POINT('Ctrl Pts',(-3.74853008484207,-7.35629680748716,
-17.2760260550539));
#78934=CARTESIAN_POINT('Ctrl Pts',(1.54493900196434,-8.61209228448443,-17.0643409871452));
#78935=CARTESIAN_POINT('Ctrl Pts',(8.02046857900044,-4.89206514499563,-16.7997346522593));
#78936=CARTESIAN_POINT('Ctrl Pts',(8.44089131054738,4.10862310634076,-16.4822070503963));
#78937=CARTESIAN_POINT('Ctrl Pts',(2.36674525998617,8.42354358841728,-16.2176007155104));
#78938=CARTESIAN_POINT('Ctrl Pts',(-3.04466016546718,7.68333577945795,-16.0059156476017));
#78939=CARTESIAN_POINT('Ctrl Pts',(-6.36062759122894,5.3045714965357,-15.8471518466702));
#78940=CARTESIAN_POINT('Ctrl Pts',(-8.10354555180846,1.62359918336805,-15.6883880457387));
#78941=CARTESIAN_POINT('Ctrl Pts',(-7.86361223773377,-3.84772305911811,
-15.4767029778299));
#78942=CARTESIAN_POINT('Ctrl Pts',(-3.59786371961263,-7.98341828555309,
-15.2650179099214));
#78943=CARTESIAN_POINT('Ctrl Pts',(1.86889728098991,-8.04200245398623,-15.0533328420126));
#78944=CARTESIAN_POINT('Ctrl Pts',(6.72752307776684,-5.59422946207796,-14.841647774104));
#78945=CARTESIAN_POINT('Ctrl Pts',(9.28650083716182,1.42166093391058,-14.577041439218));
#78946=CARTESIAN_POINT('Ctrl Pts',(3.81243640818078,8.57873875228808,-14.2595138373551));
#78947=CARTESIAN_POINT('Ctrl Pts',(-3.61331244831989,7.96878553246661,-13.9949075024691));
#78948=CARTESIAN_POINT('Ctrl Pts',(-7.27690323472737,3.91794378922106,-13.7832224345605));
#78949=CARTESIAN_POINT('Ctrl Pts',(-8.28219020287749,-0.0372499600265304,
-13.624458633629));
#78950=CARTESIAN_POINT('Ctrl Pts',(-7.24543052270881,-3.97583467451395,
-13.4656948326974));
#78951=CARTESIAN_POINT('Ctrl Pts',(-3.5387633815981,-8.00740431689109,-13.2540097647887));
#78952=CARTESIAN_POINT('Ctrl Pts',(2.38798729450963,-8.42479124656918,-13.0423246968801));
#78953=CARTESIAN_POINT('Ctrl Pts',(6.60828865927887,-4.94945466818906,-12.8306396289714));
#78954=CARTESIAN_POINT('Ctrl Pts',(8.74941585748231,0.0518863094023924,
-12.6189545610627));
#78955=CARTESIAN_POINT('Ctrl Pts',(6.18959564749428,7.06746937242281,-12.3543482261768));
#78956=CARTESIAN_POINT('Ctrl Pts',(-2.60715832870307,9.018434198657,-12.0368206243138));
#78957=CARTESIAN_POINT('Ctrl Pts',(-7.89578174653336,3.77017245265299,-11.7722142894279));
#78958=CARTESIAN_POINT('Ctrl Pts',(-8.09034796608499,-1.68815698640432,
-11.5605292215192));
#78959=CARTESIAN_POINT('Ctrl Pts',(-6.31265557350973,-5.36157082639018,
-11.4017654205877));
#78960=CARTESIAN_POINT('Ctrl Pts',(-2.98330350809687,-7.70736174037816,
-11.2430016196562));
#78961=CARTESIAN_POINT('Ctrl Pts',(2.44864961439056,-8.40508686635958,-11.0313165517475));
#78962=CARTESIAN_POINT('Ctrl Pts',(7.25192604319999,-4.90807085635143,-10.8196314838388));
#78963=CARTESIAN_POINT('Ctrl Pts',(8.24300686053481,0.4684211929323,-10.6079464159301));
#78964=CARTESIAN_POINT('Ctrl Pts',(6.66070177239462,5.67362511411226,-10.3962613480214));
#78965=CARTESIAN_POINT('Ctrl Pts',(0.184725540696012,9.39287464433703,-10.1316550131356));
#78966=CARTESIAN_POINT('Ctrl Pts',(-7.80187095937965,5.22113392661204,-9.81412741127258));
#78967=CARTESIAN_POINT('Ctrl Pts',(-8.46869429502031,-2.19972422115192,
-9.54952107638669));
#78968=CARTESIAN_POINT('Ctrl Pts',(-5.10282581808303,-6.50113627709704,
-9.33783600847803));
#78969=CARTESIAN_POINT('Ctrl Pts',(-1.3773406271148,-8.16694526203408,-9.17907220754648));
#78970=CARTESIAN_POINT('Ctrl Pts',(2.68042426248865,-7.81785460286454,-9.02030840661499));
#78971=CARTESIAN_POINT('Ctrl Pts',(7.28565027676,-4.85393347810338,-8.80862333870625));
#78972=CARTESIAN_POINT('Ctrl Pts',(8.70880111337855,0.914534873377897,-8.59693827079764));
#78973=CARTESIAN_POINT('Ctrl Pts',(6.00503674299778,5.66622574842014,-8.38525320288888));
#78974=CARTESIAN_POINT('Ctrl Pts',(1.44269004321358,8.6298097010002,-8.17356813498026));
#78975=CARTESIAN_POINT('Ctrl Pts',(-5.90693139713842,7.30536645755135,-7.90896180009433));
#78976=CARTESIAN_POINT('Ctrl Pts',(-9.33114753737324,-1.02913341322142,
-7.59143419823135));
#78977=CARTESIAN_POINT('Ctrl Pts',(-5.06288718129553,-7.13615744648993,
-7.32682786334546));
#78978=CARTESIAN_POINT('Ctrl Pts',(0.282080472971771,-8.25978418785034,
-7.11514279543679));
#78979=CARTESIAN_POINT('Ctrl Pts',(4.20506961446584,-7.13536625924996,-6.95637899450525));
#78980=CARTESIAN_POINT('Ctrl Pts',(7.08484849173346,-4.25540205710899,-6.79761519357375));
#78981=CARTESIAN_POINT('Ctrl Pts',(8.69974310962545,0.977670696977567,-6.58593012566506));
#78982=CARTESIAN_POINT('Ctrl Pts',(6.07415073499534,6.30747839594202,-6.37424505775635));
#78983=CARTESIAN_POINT('Ctrl Pts',(0.945810251189927,8.20195241914058,-6.16255998984768));
#78984=CARTESIAN_POINT('Ctrl Pts',(-4.45311911750285,7.53158019018864,-5.95087492193897));
#78985=CARTESIAN_POINT('Ctrl Pts',(-9.22342332430518,1.7856874837389,-5.68626858705313));
#78986=CARTESIAN_POINT('Ctrl Pts',(-6.47651097789812,-6.79589843234738,
-5.36874098519009));
#78987=CARTESIAN_POINT('Ctrl Pts',(0.72154030475446,-8.71991681704676,-5.10413465030423));
#78988=CARTESIAN_POINT('Ctrl Pts',(5.5344611246646,-6.13786154001214,-4.89244958239554));
#78989=CARTESIAN_POINT('Ctrl Pts',(7.81187504978943,-2.75148511283057,-4.73368578146402));
#78990=CARTESIAN_POINT('Ctrl Pts',(8.16070458243695,1.30630223086348,-4.57492198053251));
#78991=CARTESIAN_POINT('Ctrl Pts',(6.02656608207569,6.3499505106843,-4.36323691262381));
#78992=CARTESIAN_POINT('Ctrl Pts',(0.585773187827785,8.73707391119004,-4.15155184471514));
#78993=CARTESIAN_POINT('Ctrl Pts',(-4.55777208499541,6.88427877071814,-3.93986677680643));
#78994=CARTESIAN_POINT('Ctrl Pts',(-8.25678610342815,2.89490126967677,-3.72818170889775));
#78995=CARTESIAN_POINT('Ctrl Pts',(-8.20661254286858,-4.57293423128735,
-3.46357537401188));
#78996=CARTESIAN_POINT('Ctrl Pts',(-0.579112413890349,-9.36984844932824,
-3.14604777214886));
#78997=CARTESIAN_POINT('Ctrl Pts',(6.1669773963677,-6.20692831038676,-2.88144143726299));
#78998=CARTESIAN_POINT('Ctrl Pts',(8.18666879455784,-1.13227957945813,-2.6697563693543));
#78999=CARTESIAN_POINT('Ctrl Pts',(7.74854456684722,2.92508534373634,-2.51099256842279));
#79000=CARTESIAN_POINT('Ctrl Pts',(5.40253881524966,6.25428554111442,-2.35222876749126));
#79001=CARTESIAN_POINT('Ctrl Pts',(0.522018750725154,8.73892962582191,-2.14054369958259));
#79002=CARTESIAN_POINT('Ctrl Pts',(-5.17781107492739,7.06185842452563,-1.92885863167389));
#79003=CARTESIAN_POINT('Ctrl Pts',(-7.92004273489733,2.33227065248713,-1.7171735637652));
#79004=CARTESIAN_POINT('Ctrl Pts',(-8.18129567364406,-3.10185273179549,
-1.50548849585651));
#79005=CARTESIAN_POINT('Ctrl Pts',(-3.3342022501132,-8.78310787063445,-1.24088216097064));
#79006=CARTESIAN_POINT('Ctrl Pts',(5.59034459280216,-7.54172942161662,-0.923354559107611));
#79007=CARTESIAN_POINT('Ctrl Pts',(8.71510519418105,-0.777787096713387,
-0.658748224221747));
#79008=CARTESIAN_POINT('Ctrl Pts',(6.9926161408468,4.40520249985987,-0.447063156313067));
#79009=CARTESIAN_POINT('Ctrl Pts',(4.0449198585628,7.22754166127095,-0.288299355381536));
#79010=CARTESIAN_POINT('Ctrl Pts',(0.106014671877446,8.26366028978802,-0.129535554450031));
#79011=CARTESIAN_POINT('Ctrl Pts',(-5.22740533349617,7.02280198980525,0.0821495134586626));
#79012=CARTESIAN_POINT('Ctrl Pts',(-8.50950193961704,2.06777617761388,0.293834581367354));
#79013=CARTESIAN_POINT('Ctrl Pts',(-7.56051702525706,-3.31418768618381,
0.505519649276039));
#79014=CARTESIAN_POINT('Ctrl Pts',(-4.26407274969228,-7.64431327803062,
0.717204717184737));
#79015=CARTESIAN_POINT('Ctrl Pts',(3.10878881347585,-8.86048504611851,0.98181105207059));
#79016=CARTESIAN_POINT('Ctrl Pts',(9.12640894070192,-2.18142751875103,1.29933865393363));
#79017=CARTESIAN_POINT('Ctrl Pts',(6.78905718875035,6.47755113143582,1.61686625579666));
#79018=CARTESIAN_POINT('Ctrl Pts',(-1.77209850624849,9.22130305452722,1.93439385765969));
#79019=CARTESIAN_POINT('Ctrl Pts',(-7.53151392432143,4.46028473475584,2.19900019254556));
#79020=CARTESIAN_POINT('Ctrl Pts',(-8.20126862571526,-0.940452357811408,
2.41068526045425));
#79021=CARTESIAN_POINT('Ctrl Pts',(-6.31313511243949,-6.06890819119358,
2.62237032836292));
#79022=CARTESIAN_POINT('Ctrl Pts',(-0.98346979200203,-8.69932764510544,
2.83405539627164));
#79023=CARTESIAN_POINT('Ctrl Pts',(4.24990731598581,-7.08784934244536,3.04574046418029));
#79024=CARTESIAN_POINT('Ctrl Pts',(7.13240843508565,-4.21040200488291,3.20450426511184));
#79025=CARTESIAN_POINT('Ctrl Pts',(8.25950763414373,-0.288137466365907,
3.36326806604334));
#79026=CARTESIAN_POINT('Ctrl Pts',(7.13993645585559,5.05760009488693,3.57495313395204));
#79027=CARTESIAN_POINT('Ctrl Pts',(1.03598505156533,9.33040032946519,3.83955946883789));
#79028=CARTESIAN_POINT('Ctrl Pts',(-7.3009930326274,5.91230828436634,4.15708707070094));
#79029=CARTESIAN_POINT('Ctrl Pts',(-8.63087863833863,-1.43632280480546,
4.42169340558678));
#79030=CARTESIAN_POINT('Ctrl Pts',(-5.67064872171571,-6.00085880470096,
4.63337847349549));
#79031=CARTESIAN_POINT('Ctrl Pts',(-0.920958701171648,-8.70812304727144,
4.84506354140417));
#79032=CARTESIAN_POINT('Ctrl Pts',(4.84856161677379,-7.28922799955687,5.05674860931286));
#79033=CARTESIAN_POINT('Ctrl Pts',(7.81587547206024,-2.68618761171285,5.26843367722155));
#79034=CARTESIAN_POINT('Ctrl Pts',(8.16795894400251,1.37131829333971,5.42719747815307));
#79035=CARTESIAN_POINT('Ctrl Pts',(6.50489685689283,5.09803098058757,5.58596127908458));
#79036=CARTESIAN_POINT('Ctrl Pts',(2.20596801611654,8.46706999908836,5.79764634699328));
#79037=CARTESIAN_POINT('Ctrl Pts',(-5.21537996581248,7.80571860647714,6.06225268187913));
#79038=CARTESIAN_POINT('Ctrl Pts',(-9.39300825854191,-0.177799795868655,
6.37978028374218));
#79039=CARTESIAN_POINT('Ctrl Pts',(-5.67853477082882,-6.65651657967052,
6.64438661862803));
#79040=CARTESIAN_POINT('Ctrl Pts',(-0.474498931446816,-8.2426592393341,
6.85607168653673));
#79041=CARTESIAN_POINT('Ctrl Pts',(4.90272240285487,-7.25554297056533,7.06775675444541));
#79042=CARTESIAN_POINT('Ctrl Pts',(8.40327910514793,-2.45484633139196,7.27944182235409));
#79043=CARTESIAN_POINT('Ctrl Pts',(7.70955934364213,2.97761977542913,7.49112689026279));
#79044=CARTESIAN_POINT('Ctrl Pts',(5.36622392380833,6.30870057295464,7.64989069119431));
#79045=CARTESIAN_POINT('Ctrl Pts',(1.6941218394773,8.08910102655353,7.80865449212583));
#79046=CARTESIAN_POINT('Ctrl Pts',(-3.76434957606231,7.89855948745089,8.02033956003451));
#79047=CARTESIAN_POINT('Ctrl Pts',(-9.01650939318612,2.61380724465366,8.28494589492038));
#79048=CARTESIAN_POINT('Ctrl Pts',(-7.07203126861679,-6.18438285883276,
8.6024734967834));
#79049=CARTESIAN_POINT('Ctrl Pts',(-0.0583375627661657,-8.7493752213905,
8.86707983166928));
#79050=CARTESIAN_POINT('Ctrl Pts',(4.94458078750979,-6.61193627864721,9.07876489957795));
#79051=CARTESIAN_POINT('Ctrl Pts',(8.42302820519816,-2.39419855508166,9.29044996748667));
#79052=CARTESIAN_POINT('Ctrl Pts',(8.01001140115047,3.53285826472605,9.50213503539534));
#79053=CARTESIAN_POINT('Ctrl Pts',(3.98117591724546,7.24249702343123,9.71382010330402));
#79054=CARTESIAN_POINT('Ctrl Pts',(0.0433567145999381,8.28216048573352,
9.87258390423556));
#79055=CARTESIAN_POINT('Ctrl Pts',(-3.91257719470531,7.2797901012712,10.0313477051671));
#79056=CARTESIAN_POINT('Ctrl Pts',(-7.9661191375803,3.61918714596217,10.2430327730758));
#79057=CARTESIAN_POINT('Ctrl Pts',(-8.58154747046168,-3.80610995094048,
10.5076391079616));
#79058=CARTESIAN_POINT('Ctrl Pts',(-1.42850782747337,-9.28545006967693,
10.8251667098247));
#79059=CARTESIAN_POINT('Ctrl Pts',(5.58926749016992,-6.7316460809816,11.0897730447105));
#79060=CARTESIAN_POINT('Ctrl Pts',(8.0406222609218,-1.8748264383621,11.3014581126192));
#79061=CARTESIAN_POINT('Ctrl Pts',(7.98606895318656,3.59197627246583,11.5131431805279));
#79062=CARTESIAN_POINT('Ctrl Pts',(3.85352014488595,7.86077303183749,11.7248282484366));
#79063=CARTESIAN_POINT('Ctrl Pts',(-1.61762369862161,8.1047404886354,11.9365133163453));
#79064=CARTESIAN_POINT('Ctrl Pts',(-5.299880128958,6.36453711866289,12.0952771172768));
#79065=CARTESIAN_POINT('Ctrl Pts',(-7.68108875049532,3.05032454504364,12.2540409182083));
#79066=CARTESIAN_POINT('Ctrl Pts',(-8.42528638730484,-2.36053362685826,
12.465725986117));
#79067=CARTESIAN_POINT('Ctrl Pts',(-4.11484577036667,-8.43785957648776,
12.7303323210029));
#79068=CARTESIAN_POINT('Ctrl Pts',(4.88615002749256,-8.02407349906823,13.0478599228659));
#79069=CARTESIAN_POINT('Ctrl Pts',(8.61095080285362,-1.55128859568458,13.3124662577518));
#79070=CARTESIAN_POINT('Ctrl Pts',(7.35905873746818,3.74310499656434,13.5241513256605));
#79071=CARTESIAN_POINT('Ctrl Pts',(3.79713466688552,7.89058674551804,13.7358363935691));
#79072=CARTESIAN_POINT('Ctrl Pts',(-2.11341270190033,8.4955786687284,13.9475214614779));
#79073=CARTESIAN_POINT('Ctrl Pts',(-6.45643942659223,5.15925525141111,14.1592065293865));
#79074=CARTESIAN_POINT('Ctrl Pts',(-8.15315375718723,1.45675870610943,14.3179703303181));
#79075=CARTESIAN_POINT('Ctrl Pts',(-7.84090954781147,-2.61222925604173,
14.4767341312496));
#79076=CARTESIAN_POINT('Ctrl Pts',(-4.92612766124713,-7.23124027928325,
14.6884191991583));
#79077=CARTESIAN_POINT('Ctrl Pts',(2.28507222059734,-9.10537615330006,14.9530255340441));
#79078=CARTESIAN_POINT('Ctrl Pts',(8.90522127729204,-2.99286678822828,15.2705531359072));
#79079=CARTESIAN_POINT('Ctrl Pts',(7.58708021122468,4.35788755071873,15.535159470793));
#79080=CARTESIAN_POINT('Ctrl Pts',(3.22009898808751,7.60246953454795,15.7468445387017));
#79081=CARTESIAN_POINT('Ctrl Pts',(-2.17575046625231,8.48208115827781,15.9585296066104));
#79082=CARTESIAN_POINT('Ctrl Pts',(-7.08743254716731,5.13903396120905,16.1702146745191));
#79083=CARTESIAN_POINT('Ctrl Pts',(-8.26192302571686,-0.210125523431927,
16.3818997424278));
#79084=CARTESIAN_POINT('Ctrl Pts',(-7.17595340292437,-4.13542680689911,
16.5406635433593));
#79085=CARTESIAN_POINT('Ctrl Pts',(-4.31695337778056,-7.04751855316114,
16.6994273442908));
#79086=CARTESIAN_POINT('Ctrl Pts',(0.887399762225084,-8.70460173549805,
16.9111124121995));
#79087=CARTESIAN_POINT('Ctrl Pts',(7.6114289922114,-5.49505037674401,17.1757187470854));
#79088=CARTESIAN_POINT('Ctrl Pts',(8.74048593802383,3.44443365109889,17.4932463489484));
#79089=CARTESIAN_POINT('Ctrl Pts',(2.99868548357566,8.21966273072438,17.7578526838342));
#79090=CARTESIAN_POINT('Ctrl Pts',(-2.43171158715242,7.89007980147984,17.9695377517429));
#79091=CARTESIAN_POINT('Ctrl Pts',(-7.12643538072904,5.08856655958259,18.1812228196516));
#79092=CARTESIAN_POINT('Ctrl Pts',(-8.7316702267711,-0.631906018348646,
18.3929078875603));
#79093=CARTESIAN_POINT('Ctrl Pts',(-6.18583120778734,-5.48078617419366,
18.604592955469));
#79094=CARTESIAN_POINT('Ctrl Pts',(-2.82738245660738,-7.7847267492334,18.7633567564005));
#79095=CARTESIAN_POINT('Ctrl Pts',(1.23517226993769,-8.17177787795647,18.922120557332));
#79096=CARTESIAN_POINT('Ctrl Pts',(6.28401346095891,-6.08841067390496,19.1338056252407));
#79097=CARTESIAN_POINT('Ctrl Pts',(9.36182220511659,0.696932526300606,19.3984119601266));
#79098=CARTESIAN_POINT('Ctrl Pts',(4.46933914411785,8.26348747348669,19.7159395619896));
#79099=CARTESIAN_POINT('Ctrl Pts',(-2.99853668295097,8.21971701442728,19.9805458968755));
#79100=CARTESIAN_POINT('Ctrl Pts',(-6.94106756814404,4.47081217803551,20.1922309647842));
#79101=CARTESIAN_POINT('Ctrl Pts',(-8.72901401305323,-0.695632968545975,
20.4039160326929));
#79102=CARTESIAN_POINT('Ctrl Pts',(-6.27363820517334,-6.10596706801597,
20.6156011006015));
#79103=CARTESIAN_POINT('Ctrl Pts',(-1.20354306299133,-8.17649123487534,
20.8272861685103));
#79104=CARTESIAN_POINT('Ctrl Pts',(2.84953519592018,-7.77664524607966,20.9860499694417));
#79105=CARTESIAN_POINT('Ctrl Pts',(6.2069954500714,-5.45681332884632,21.1448137703733));
#79106=CARTESIAN_POINT('Ctrl Pts',(8.72830333694957,-0.611792914169276,
21.356498838282));
#79107=CARTESIAN_POINT('Ctrl Pts',(6.71389086124484,6.56148607022255,21.6211051731678));
#79108=CARTESIAN_POINT('Ctrl Pts',(-1.90157024722326,9.20023087778187,21.9386327750308));
#79109=CARTESIAN_POINT('Ctrl Pts',(-7.58700131936631,4.35802489852905,22.2032391099167));
#79110=CARTESIAN_POINT('Ctrl Pts',(-8.18940584699088,-1.04891009628249,
22.4149241778254));
#79111=CARTESIAN_POINT('Ctrl Pts',(-6.23057087324017,-6.15301368928593,
22.6266092457341));
#79112=CARTESIAN_POINT('Ctrl Pts',(-0.868156811692852,-8.71135316213372,
22.8382943136427));
#79113=CARTESIAN_POINT('Ctrl Pts',(4.34418767333381,-7.03075801584175,23.0499793815515));
#79114=CARTESIAN_POINT('Ctrl Pts',(7.18769845288102,-4.11497910889147,23.208743182483));
#79115=CARTESIAN_POINT('Ctrl Pts',(8.26267902471989,-0.178155992140028,
23.3675069834145));
#79116=CARTESIAN_POINT('Ctrl Pts',(7.07190532710078,5.15225433729316,23.5791920513232));
#79117=CARTESIAN_POINT('Ctrl Pts',(0.911672841174965,9.34335499577618,23.8437983862091));
#79118=CARTESIAN_POINT('Ctrl Pts',(-7.37909340118962,5.81456775574379,24.1613259880721));
#79119=CARTESIAN_POINT('Ctrl Pts',(-8.6109788843406,-1.55113271182926,24.425932322958));
#79120=CARTESIAN_POINT('Ctrl Pts',(-5.59023836755192,-6.07583866727565,
24.6376173908666));
#79121=CARTESIAN_POINT('Ctrl Pts',(-0.804912040360767,-8.71961624581554,
24.8493024587754));
#79122=CARTESIAN_POINT('Ctrl Pts',(4.94519767960346,-7.22401481689722,25.060987526684));
#79123=CARTESIAN_POINT('Ctrl Pts',(7.85095385123881,-2.5818691764276,25.2726725945928));
#79124=CARTESIAN_POINT('Ctrl Pts',(8.14897311707001,1.47996596360603,25.4314363955242));
#79125=CARTESIAN_POINT('Ctrl Pts',(6.4364320026378,5.18420170310737,25.5902001964558));
#79126=CARTESIAN_POINT('Ctrl Pts',(2.09302007257951,8.49569518564614,25.8018852643645));
#79127=CARTESIAN_POINT('Ctrl Pts',(-5.31886276036888,7.73557553662241,26.0664915992503));
#79128=CARTESIAN_POINT('Ctrl Pts',(-9.38980774356954,-0.302866552159413,
26.3840192011134));
#79129=CARTESIAN_POINT('Ctrl Pts',(-5.58938935189839,-6.7315448976555,26.6486255359992));
#79130=CARTESIAN_POINT('Ctrl Pts',(-0.36469301513852,-8.24824705749777,
26.8603106039079));
#79131=CARTESIAN_POINT('Ctrl Pts',(4.99890654770252,-7.18961224228023,27.0719956718166));
#79132=CARTESIAN_POINT('Ctrl Pts',(8.43522409269409,-2.34272590610575,27.2836807397253));
#79133=CARTESIAN_POINT('Ctrl Pts',(7.66922409732036,3.08002054596217,27.495365807634));
#79134=CARTESIAN_POINT('Ctrl Pts',(5.28173792622925,6.37960081782495,27.6541296085655));
#79135=CARTESIAN_POINT('Ctrl Pts',(1.58625263971785,8.11094364337897,27.812893409497));
#79136=CARTESIAN_POINT('Ctrl Pts',(-3.86919742019125,7.84773094819247,28.0245784774057));
#79137=CARTESIAN_POINT('Ctrl Pts',(-9.05051682149315,2.49350660923522,28.2891848122916));
#79138=CARTESIAN_POINT('Ctrl Pts',(-6.98904950325245,-6.27800960900046,
28.6067124141546));
#79139=CARTESIAN_POINT('Ctrl Pts',(0.0581791732242141,-8.74937627605938,
28.8713187490405));
#79140=CARTESIAN_POINT('Ctrl Pts',(5.03219058842161,-6.54550520575857,29.0830038169491));
#79141=CARTESIAN_POINT('Ctrl Pts',(8.45416382536456,-2.28182051899467,29.2946888848579));
#79142=CARTESIAN_POINT('Ctrl Pts',(7.96225564688464,3.63921079064677,29.5063739527665));
#79143=CARTESIAN_POINT('Ctrl Pts',(3.88437777703145,7.29487039663986,29.7180590206752));
#79144=CARTESIAN_POINT('Ctrl Pts',(-0.0669370008521218,8.28200347464785,
29.8768228216067));
#79145=CARTESIAN_POINT('Ctrl Pts',(-4.00917201687075,7.22704254603652,30.0355866225382));
#79146=CARTESIAN_POINT('Ctrl Pts',(-8.01360790323876,3.51278494712968,30.2472716904469));
#79147=CARTESIAN_POINT('Ctrl Pts',(-8.53010226655877,-3.92004914107959,
30.5118780253328));
#79148=CARTESIAN_POINT('Ctrl Pts',(-1.30473092765309,-9.30364954284291,
30.8294056271958));
#79149=CARTESIAN_POINT('Ctrl Pts',(5.67841424972103,-6.65661938560647,31.0940119620817));
#79150=CARTESIAN_POINT('Ctrl Pts',(8.06487553978532,-1.76758678558764,31.3056970299904));
#79151=CARTESIAN_POINT('Ctrl Pts',(7.93752807350566,3.69800472543214,31.5173820978991));
#79152=CARTESIAN_POINT('Ctrl Pts',(3.74850001544698,7.91139164744737,31.7290671658077));
#79153=CARTESIAN_POINT('Ctrl Pts',(-1.725407512423,8.08248066713078,31.9407522337164));
#79154=CARTESIAN_POINT('Ctrl Pts',(-5.38416392046695,6.29339661817871,32.0995160346479));
#79155=CARTESIAN_POINT('Ctrl Pts',(-7.72102749773726,2.94776841055509,32.2582798355795));
#79156=CARTESIAN_POINT('Ctrl Pts',(-8.39310514002376,-2.47252013543657,
32.4699649034881));
#79157=CARTESIAN_POINT('Ctrl Pts',(-4.00211766288754,-8.49190698010957,
32.734571238374));
#79158=CARTESIAN_POINT('Ctrl Pts',(4.99256981673248,-7.95829530959158,33.052098840237));
#79159=CARTESIAN_POINT('Ctrl Pts',(8.63084510062077,-1.43648281763411,33.316705175123));
#79160=CARTESIAN_POINT('Ctrl Pts',(7.30856093990772,3.84077043110713,33.5283902430316));
#79161=CARTESIAN_POINT('Ctrl Pts',(3.69172252105726,7.94045185707503,33.7400753109404));
#79162=CARTESIAN_POINT('Ctrl Pts',(-2.2263571737631,8.46668198882771,33.9517603788489));
#79163=CARTESIAN_POINT('Ctrl Pts',(-6.52457046083469,5.07282023336842,34.1634454467577));
#79164=CARTESIAN_POINT('Ctrl Pts',(-8.17182983472982,1.34805759089933,34.3222092476892));
#79165=CARTESIAN_POINT('Ctrl Pts',(-7.80542839734849,-2.71641155883038,
34.4809730486207));
#79166=CARTESIAN_POINT('Ctrl Pts',(-4.82939563391592,-7.29619815539201,
34.6926581165294));
#79167=CARTESIAN_POINT('Ctrl Pts',(2.40612187514562,-9.0741394891403,34.9572644514153));
#79168=CARTESIAN_POINT('Ctrl Pts',(8.94428634201623,-2.87401451660175,35.2747920532783));
#79169=CARTESIAN_POINT('Ctrl Pts',(7.52837540758014,4.45853493412458,35.5393983881642));
#79170=CARTESIAN_POINT('Ctrl Pts',(3.11857473717401,7.64467606412931,35.7510834560729));
#79171=CARTESIAN_POINT('Ctrl Pts',(-2.28850967028801,8.45235555073301,35.9627685239815));
#79172=CARTESIAN_POINT('Ctrl Pts',(-7.15523835371221,5.04419807964279,36.1744535918902));
#79173=CARTESIAN_POINT('Ctrl Pts',(-8.25839229812943,-0.320127269480299,
36.3861386597989));
#79174=CARTESIAN_POINT('Ctrl Pts',(-7.12024746501521,-4.23061912172507,
36.5449024607304));
#79175=CARTESIAN_POINT('Ctrl Pts',(-4.22272190653533,-7.10438061502535,
36.703666261662));
#79176=CARTESIAN_POINT('Ctrl Pts',(1.00323641159163,-8.69201279417427,36.9153513295706));
#79177=CARTESIAN_POINT('Ctrl Pts',(7.68392924963401,-5.39320509836674,37.1799576644565));
#79178=CARTESIAN_POINT('Ctrl Pts',(8.69384292460902,3.56052142415137,37.4974852663195));
#79179=CARTESIAN_POINT('Ctrl Pts',(2.8889619762041,8.25886606843306,37.7620916012054));
#79180=CARTESIAN_POINT('Ctrl Pts',(-2.53656467485294,7.8569981651455,37.973776669114));
#79181=CARTESIAN_POINT('Ctrl Pts',(-7.19356567683603,4.99321576942699,38.1854617370228));
#79182=CARTESIAN_POINT('Ctrl Pts',(-8.72248118257988,-0.748125781300136,
38.3971468049315));
#79183=CARTESIAN_POINT('Ctrl Pts',(-6.11229750717327,-5.56267417725245,
38.6088318728402));
#79184=CARTESIAN_POINT('Ctrl Pts',(-2.72346598880742,-7.82168748570094,
38.7675956737716));
#79185=CARTESIAN_POINT('Ctrl Pts',(1.34388270272352,-8.15460504895256,38.9263594747032));
#79186=CARTESIAN_POINT('Ctrl Pts',(6.36453293622773,-6.00418938869395,39.1380445426119));
#79187=CARTESIAN_POINT('Ctrl Pts',(9.35171135652741,0.821537978809482,39.4026508774977));
#79188=CARTESIAN_POINT('Ctrl Pts',(4.35890164019773,8.32227097015575,39.7201784793608));
#79189=CARTESIAN_POINT('Ctrl Pts',(-3.10772914375988,8.17905799009226,39.9847848142466));
#79190=CARTESIAN_POINT('Ctrl Pts',(-6.99998793858948,4.37798462496313,40.1964698821553));
#79191=CARTESIAN_POINT('Ctrl Pts',(-8.71897658075383,-0.811811709249727,
40.408154950064));
#79192=CARTESIAN_POINT('Ctrl Pts',(-6.19177146109914,-6.18896892370799,
40.6198400179727));
#79193=CARTESIAN_POINT('Ctrl Pts',(-1.09455362535609,-8.19179328228488,
40.8315250858814));
#79194=CARTESIAN_POINT('Ctrl Pts',(2.95284067765355,-7.73800969555844,40.9902888868129));
#79195=CARTESIAN_POINT('Ctrl Pts',(6.27911105175123,-5.3736736617381,41.1490526877445));
#79196=CARTESIAN_POINT('Ctrl Pts',(8.73567638035269,-0.495507708699551,
41.3607377556531));
#79197=CARTESIAN_POINT('Ctrl Pts',(6.62591913503577,6.65031018542722,41.625344090539));
#79198=CARTESIAN_POINT('Ctrl Pts',(-2.02391704506606,9.17409272921886,41.9428716924019));
#79199=CARTESIAN_POINT('Ctrl Pts',(-7.64436247696758,4.25660573191808,42.2074780272879));
#79200=CARTESIAN_POINT('Ctrl Pts',(-8.17471182597883,-1.15787178867669,
42.4191630951966));
#79201=CARTESIAN_POINT('Ctrl Pts',(-6.14808144885145,-6.23543786476111,
42.6308481631052));
#79202=CARTESIAN_POINT('Ctrl Pts',(-0.75207459260542,-8.72214159322487,
42.842533231014));
#79203=CARTESIAN_POINT('Ctrl Pts',(4.4374279746784,-6.97228497610427,43.0542182989226));
#79204=CARTESIAN_POINT('Ctrl Pts',(7.24185848301294,-4.01889883278679,43.2129820998541));
#79205=CARTESIAN_POINT('Ctrl Pts',(8.26431880344762,-0.0681097501406032,
43.3717459007857));
#79206=CARTESIAN_POINT('Ctrl Pts',(7.00266797220651,5.24597092849989,43.5834309686943));
#79207=CARTESIAN_POINT('Ctrl Pts',(0.787170674435132,9.35466687144652,43.8480373035802));
#79208=CARTESIAN_POINT('Ctrl Pts',(-7.45586913137561,5.71578805637648,44.1655649054432));
#79209=CARTESIAN_POINT('Ctrl Pts',(-8.58955960612328,-1.66566377433196,
44.4301712403291));
#79210=CARTESIAN_POINT('Ctrl Pts',(-5.50883342665449,-6.14974266080996,
44.6418563082378));
#79211=CARTESIAN_POINT('Ctrl Pts',(-0.68872539330883,-8.72956174155499,
44.8535413761465));
#79212=CARTESIAN_POINT('Ctrl Pts',(5.04095820523059,-7.15752125656805,45.0652264440551));
#79213=CARTESIAN_POINT('Ctrl Pts',(7.884639323544,-2.47709256106658,45.2769115119639));
#79214=CARTESIAN_POINT('Ctrl Pts',(8.12854250071157,1.5883510097858,45.4356753128953));
#79215=CARTESIAN_POINT('Ctrl Pts',(6.3668255657606,5.26945314413741,45.594439113827));
#79216=CARTESIAN_POINT('Ctrl Pts',(1.97970106770277,8.52281370171664,45.8061241817355));
#79217=CARTESIAN_POINT('Ctrl Pts',(-5.42140238140834,7.66406068382094,46.0707305166215));
#79218=CARTESIAN_POINT('Ctrl Pts',(-9.38494201594991,-0.427879617266375,
46.3882581184846));
#79219=CARTESIAN_POINT('Ctrl Pts',(-5.49925273618984,-6.80537944421727,
46.6528644533703));
#79220=CARTESIAN_POINT('Ctrl Pts',(-0.25482241716316,-8.25237214699649,
46.864549521279));
#79221=CARTESIAN_POINT('Ctrl Pts',(5.09420418711999,-7.12240651514204,47.0762345891877));
#79222=CARTESIAN_POINT('Ctrl Pts',(8.46567319292571,-2.23019002681052,47.2879196570964));
#79223=CARTESIAN_POINT('Ctrl Pts',(7.62752880020834,3.18187511075783,47.4996047250052));
#79224=CARTESIAN_POINT('Ctrl Pts',(5.19631527353026,6.44936971294384,47.6583685259366));
#79225=CARTESIAN_POINT('Ctrl Pts',(1.47810213580437,8.13134787714882,47.8171323268681));
#79226=CARTESIAN_POINT('Ctrl Pts',(-3.97335910607881,7.79551070333261,48.0288173947768));
#79227=CARTESIAN_POINT('Ctrl Pts',(-9.08291924414386,2.3727637789698,48.2934237296627));
#79228=CARTESIAN_POINT('Ctrl Pts',(-6.90482830967873,-6.37052302589617,
48.6109513315257));
#79229=CARTESIAN_POINT('Ctrl Pts',(0.174685591761263,-8.74782572873383,
48.8755576664116));
#79230=CARTESIAN_POINT('Ctrl Pts',(5.11890798781239,-6.4779133622736,49.0872427343203));
#79231=CARTESIAN_POINT('Ctrl Pts',(8.48380019609937,-2.16903782808714,49.298927802229));
#79232=CARTESIAN_POINT('Ctrl Pts',(7.91308787750832,3.74491794408583,49.5106128701377));
#79233=CARTESIAN_POINT('Ctrl Pts',(3.786890786771,7.34595010788508,49.7222979380464));
#79234=CARTESIAN_POINT('Ctrl Pts',(-0.177218845789058,8.28037774481689,
49.8810617389778));
#79235=CARTESIAN_POINT('Ctrl Pts',(-4.10505585816007,7.17301335733233,50.0398255399094));
#79236=CARTESIAN_POINT('Ctrl Pts',(-8.05967554704219,3.40575979599903,50.251510607818));
#79237=CARTESIAN_POINT('Ctrl Pts',(-8.47714434642404,-4.03329315526637,
50.5161169427039));
#79238=CARTESIAN_POINT('Ctrl Pts',(-1.18072264870137,-9.32019912000061,
50.833644544567));
#79239=CARTESIAN_POINT('Ctrl Pts',(5.76655400734678,-6.58041221479475,51.0982508794527));
#79240=CARTESIAN_POINT('Ctrl Pts',(8.08769860506414,-1.66003367148095,51.3099359473616));
#79241=CARTESIAN_POINT('Ctrl Pts',(7.88757956386002,3.80337737948872,51.5216210152701));
#79242=CARTESIAN_POINT('Ctrl Pts',(3.64281513233217,7.96060726808723,51.7333060831789));
#79243=CARTESIAN_POINT('Ctrl Pts',(-1.83288534490189,8.05878750997495,51.9449911510876));
#79244=CARTESIAN_POINT('Ctrl Pts',(-5.46749289199121,6.22114005566518,52.1037549520191));
#79245=CARTESIAN_POINT('Ctrl Pts',(-7.75959700890935,2.84468952300543,52.2625187529506));
#79246=CARTESIAN_POINT('Ctrl Pts',(-8.35943547140671,-2.58406817081551,
52.4742038208594));
#79247=CARTESIAN_POINT('Ctrl Pts',(-3.88867982549927,-8.54444844097074,
52.7388101557451));
#79248=CARTESIAN_POINT('Ctrl Pts',(5.09810423065285,-7.89110580736366,53.0563377576083));
#79249=CARTESIAN_POINT('Ctrl Pts',(8.64920881668602,-1.32142229568139,53.320944092494));
#79250=CARTESIAN_POINT('Ctrl Pts',(7.25676705235914,3.93775474876736,53.5326291604028));
#79251=CARTESIAN_POINT('Ctrl Pts',(3.58565569081256,7.98890882043448,53.7443142283114));
#79252=CARTESIAN_POINT('Ctrl Pts',(-2.33890682745132,8.43628383901313,53.9559992962201));
#79253=CARTESIAN_POINT('Ctrl Pts',(-6.5915444359622,4.98548560925594,54.1676843641289));
#79254=CARTESIAN_POINT('Ctrl Pts',(-8.1890567337444,1.23911741167084,54.3264481650602));
#79255=CARTESIAN_POINT('Ctrl Pts',(-7.76856303931412,-2.82011213449629,
54.485211965992));
#79256=CARTESIAN_POINT('Ctrl Pts',(-4.73180717700486,-7.35986213958475,
54.6968970339004));
#79257=CARTESIAN_POINT('Ctrl Pts',(2.52674484922246,-9.04129361855733,54.9615033687864));
#79258=CARTESIAN_POINT('Ctrl Pts',(8.98176520865567,-2.75465259123618,55.2790309706494));
#79259=CARTESIAN_POINT('Ctrl Pts',(7.46833558457723,4.55839168067677,55.5436373055353));
#79260=CARTESIAN_POINT('Ctrl Pts',(3.0164973733366,7.68552685322903,55.7553223734439));
#79261=CARTESIAN_POINT('Ctrl Pts',(-2.40086285480069,8.42113112897703,55.9670074413527));
#79262=CARTESIAN_POINT('Ctrl Pts',(-7.22177562331924,4.94846743427247,56.1786925092613));
#79263=CARTESIAN_POINT('Ctrl Pts',(-8.25339659055917,-0.430071956849194,
56.3903775771701));
#79264=CARTESIAN_POINT('Ctrl Pts',(-7.06327976561099,-4.3250617833591,56.5491413781016));
#79265=CARTESIAN_POINT('Ctrl Pts',(-4.12773988185095,-7.15998170391512,
56.7079051790331));
#79266=CARTESIAN_POINT('Ctrl Pts',(1.11889147120648,-8.67788478346445,56.9195902469418));
#79267=CARTESIAN_POINT('Ctrl Pts',(7.7550744568542,-5.29039851498598,57.1841965818276));
#79268=CARTESIAN_POINT('Ctrl Pts',(8.64564486962893,3.67596925206309,57.5017241836908));
#79269=CARTESIAN_POINT('Ctrl Pts',(2.77874843057585,8.29661909249389,57.7663305185765));
#79270=CARTESIAN_POINT('Ctrl Pts',(-2.64099760384767,7.82250413811996,57.9780155864852));
#79271=CARTESIAN_POINT('Ctrl Pts',(-7.25934386865709,4.89702852333033,58.189700654394));
#79272=CARTESIAN_POINT('Ctrl Pts',(-8.71190066743893,-0.86431257451617,
58.4013857223026));
#79273=CARTESIAN_POINT('Ctrl Pts',(-6.03748787940653,-5.6434525015018,58.6130707902113));
#79274=CARTESIAN_POINT('Ctrl Pts',(-2.61946603419042,-7.85751750355384,
58.7718345911428));
#79275=CARTESIAN_POINT('Ctrl Pts',(1.45308347512525,-8.13551848137901,58.9305983920743));
#79276=CARTESIAN_POINT('Ctrl Pts',(6.44234932446726,-5.91991369584324,59.1422834599831));
#79277=CARTESIAN_POINT('Ctrl Pts',(9.34319950749135,0.948088200591955,59.4068897948688));
#79278=CARTESIAN_POINT('Ctrl Pts',(4.24199828795001,8.37592502394999,59.7244173967321));
#79279=CARTESIAN_POINT('Ctrl Pts',(-3.20680410262386,8.14308925527156,59.9890237316177));
#79280=CARTESIAN_POINT('Ctrl Pts',(-7.07054001980459,4.27610841771073,60.2007087995265));
#79281=CARTESIAN_POINT('Ctrl Pts',(-8.27146334671563,0.390452602810304,
60.359472600458));
#79282=CARTESIAN_POINT('Ctrl Pts',(-7.44101921670096,-3.62419448168208,
60.5182430956361));
#79283=CARTESIAN_POINT('Ctrl Pts',(-5.68421081081461,-5.69823456483541,
60.6240923238372));
#79284=CARTESIAN_POINT('Ctrl Pts',(-4.60927878647134,-6.46465601021938,
60.6770202850609));
#79285=CARTESIAN_POINT('Ctrl Pts',(-3.42485771374982,7.13737126555386,59.9999999999999));
#79286=CARTESIAN_POINT('Ctrl Pts',(-3.60849199590157,7.03465838837373,59.9999999999999));
#79287=CARTESIAN_POINT('Ctrl Pts',(-3.78755911055656,6.92445885384906,60.));
#79288=CARTESIAN_POINT('Ctrl Pts',(-3.96154458364211,6.80675795931572,60.));
#79289=CARTESIAN_POINT('Ctrl Pts',(-4.13247087319123,6.69112659755657,60.));
#79290=CARTESIAN_POINT('Ctrl Pts',(-4.2984929941888,6.56825460060961,60.));
#79291=CARTESIAN_POINT('Ctrl Pts',(-4.45931652738607,6.43861171335742,60.));
#79292=CARTESIAN_POINT('Ctrl Pts',(-4.62009538315812,6.30900484142145,60.));
#79293=CARTESIAN_POINT('Ctrl Pts',(-4.77567893444557,6.17263015411101,60.));
#79294=CARTESIAN_POINT('Ctrl Pts',(-4.92573131027231,6.02992581332935,60.));
#79295=CARTESIAN_POINT('Ctrl Pts',(-4.96262713058505,5.99483677401014,60.));
#79296=CARTESIAN_POINT('Ctrl Pts',(-4.99918832229332,5.95936492333879,60.));
#79297=CARTESIAN_POINT('Ctrl Pts',(-5.03540946333644,5.9235165595251,60.));
#79298=CARTESIAN_POINT('Ctrl Pts',(-5.06052699232729,5.89865753268521,60.));
#79299=CARTESIAN_POINT('Ctrl Pts',(-5.08548260315889,5.87361570900131,60.));
#79300=CARTESIAN_POINT('Ctrl Pts',(-5.11025822621535,5.84840998085388,60.0000000000001));
#79301=CARTESIAN_POINT('Ctrl Pts',(-5.25368359056449,5.70249475058922,60.0000000000001));
#79302=CARTESIAN_POINT('Ctrl Pts',(-5.39120059555047,5.55097235209628,60.));
#79303=CARTESIAN_POINT('Ctrl Pts',(-5.52252818805357,5.39430470386248,60.));
#79304=CARTESIAN_POINT('Ctrl Pts',(-5.65352735584239,5.2380288508838,60.0000000000001));
#79305=CARTESIAN_POINT('Ctrl Pts',(-5.77836838570734,5.076632761517,60.));
#79306=CARTESIAN_POINT('Ctrl Pts',(-5.89672849428091,4.91054798451264,60.));
#79307=CARTESIAN_POINT('Ctrl Pts',(-6.00771815129665,4.75480554174704,60.));
#79308=CARTESIAN_POINT('Ctrl Pts',(-6.11300877241676,4.5949394925689,60.));
#79309=CARTESIAN_POINT('Ctrl Pts',(-6.21229482069967,4.43129207005651,60.));
#79310=CARTESIAN_POINT('Ctrl Pts',(-6.23475787616974,4.39426752136105,60.));
#79311=CARTESIAN_POINT('Ctrl Pts',(-6.25691341041412,4.35704937873796,60.));
#79312=CARTESIAN_POINT('Ctrl Pts',(-6.27875759151048,4.31964155207945,60.));
#79313=CARTESIAN_POINT('Ctrl Pts',(-6.2951680303997,4.29153892600024,60.));
#79314=CARTESIAN_POINT('Ctrl Pts',(-6.31140442788322,4.26332614950814,60.));
#79315=CARTESIAN_POINT('Ctrl Pts',(-6.32745245424683,4.23502760248424,60.));
#79316=CARTESIAN_POINT('Ctrl Pts',(-6.38414409403106,4.13505948192255,60.));
#79317=CARTESIAN_POINT('Ctrl Pts',(-6.43851755582811,4.03396718679547,60.));
#79318=CARTESIAN_POINT('Ctrl Pts',(-6.4905241514475,3.93183211822126,60.));
#79319=CARTESIAN_POINT('Ctrl Pts',(-6.58454597607521,3.74718389444401,60.));
#79320=CARTESIAN_POINT('Ctrl Pts',(-6.67083516273044,3.55912849623771,59.9999999999999));
#79321=CARTESIAN_POINT('Ctrl Pts',(-6.74928129002232,3.36812873857614,59.9999999999999));
#79322=CARTESIAN_POINT('Ctrl Pts',(-6.82527147153296,3.18310869036922,59.9999999999999));
#79323=CARTESIAN_POINT('Ctrl Pts',(-6.89390186093913,2.99532499045739,59.9999999999999));
#79324=CARTESIAN_POINT('Ctrl Pts',(-6.95502099206733,2.80518508079014,59.9999999999999));
#79325=CARTESIAN_POINT('Ctrl Pts',(-7.01575663887716,2.61623818012524,59.9999999999999));
#79326=CARTESIAN_POINT('Ctrl Pts',(-7.069075069887,2.42496390511742,60.));
#79327=CARTESIAN_POINT('Ctrl Pts',(-7.11477647237383,2.23175902296667,60.));
#79328=CARTESIAN_POINT('Ctrl Pts',(-7.1597701772088,2.04154596675526,59.9999999999999));
#79329=CARTESIAN_POINT('Ctrl Pts',(-7.19738093165887,1.84946105664228,59.9999999999999));
#79330=CARTESIAN_POINT('Ctrl Pts',(-7.22736781049597,1.65588890955698,60.));
#79331=CARTESIAN_POINT('Ctrl Pts',(-7.23119593616582,1.63117748462834,60.));
#79332=CARTESIAN_POINT('Ctrl Pts',(-7.23489974672764,1.60644183693712,60.));
#79333=CARTESIAN_POINT('Ctrl Pts',(-7.23847868072504,1.58168278120198,60.));
#79334=CARTESIAN_POINT('Ctrl Pts',(-7.24275065143607,1.55212929935218,60.));
#79335=CARTESIAN_POINT('Ctrl Pts',(-7.24684510735891,1.52253890325882,59.9999999999999));
#79336=CARTESIAN_POINT('Ctrl Pts',(-7.25075778712086,1.49293926291434,59.9999999999999));
#79337=CARTESIAN_POINT('Ctrl Pts',(-7.27632909266145,1.29949091211867,60.));
#79338=CARTESIAN_POINT('Ctrl Pts',(-7.29417366705118,1.10543161726051,59.9999999999999));
#79339=CARTESIAN_POINT('Ctrl Pts',(-7.30417158068525,0.911143029985696,
60.));
#79340=CARTESIAN_POINT('Ctrl Pts',(-7.31396241695766,0.720878559093373,
60.));
#79341=CARTESIAN_POINT('Ctrl Pts',(-7.31622819308078,0.530393618398438,
60.));
#79342=CARTESIAN_POINT('Ctrl Pts',(-7.31080782602039,0.340046611414723,
60.));
#79343=CARTESIAN_POINT('Ctrl Pts',(-7.30524905362152,0.144839224749122,
60.));
#79344=CARTESIAN_POINT('Ctrl Pts',(-7.29160651157262,-0.0502238645111097,
60.));
#79345=CARTESIAN_POINT('Ctrl Pts',(-7.27000990910251,-0.244634982193785,
60.));
#79346=CARTESIAN_POINT('Ctrl Pts',(-7.24855927055549,-0.437732142763655,
60.));
#79347=CARTESIAN_POINT('Ctrl Pts',(-7.21926140690079,-0.630186811838858,
60.));
#79348=CARTESIAN_POINT('Ctrl Pts',(-7.18219679971437,-0.821480864997494,
60.));
#79349=CARTESIAN_POINT('Ctrl Pts',(-7.16291568882707,-0.92099255906403,
60.));
#79350=CARTESIAN_POINT('Ctrl Pts',(-7.14153207281526,-1.02018977269293,
60.0000000000001));
#79351=CARTESIAN_POINT('Ctrl Pts',(-7.11805266783406,-1.11899638281762,
60.0000000000001));
#79352=CARTESIAN_POINT('Ctrl Pts',(-7.10912968526417,-1.15654629775968,
60.0000000000001));
#79353=CARTESIAN_POINT('Ctrl Pts',(-7.09990398456901,-1.1940397736015,60.0000000000001));
#79354=CARTESIAN_POINT('Ctrl Pts',(-7.09037582080005,-1.23147253281501,
60.0000000000001));
#79355=CARTESIAN_POINT('Ctrl Pts',(-7.08335466798265,-1.25905613960301,
60.));
#79356=CARTESIAN_POINT('Ctrl Pts',(-7.07616842942188,-1.28660971580694,
60.));
#79357=CARTESIAN_POINT('Ctrl Pts',(-7.06882369474851,-1.31410786163049,
60.));
#79358=CARTESIAN_POINT('Ctrl Pts',(-7.01922252390528,-1.49981099312826,
60.));
#79359=CARTESIAN_POINT('Ctrl Pts',(-6.96234315275086,-1.68320568927462,
60.));
#79360=CARTESIAN_POINT('Ctrl Pts',(-6.89834858945776,-1.86382382254377,
60.));
#79361=CARTESIAN_POINT('Ctrl Pts',(-6.83476009194915,-2.04329587651797,
60.));
#79362=CARTESIAN_POINT('Ctrl Pts',(-6.76414607432457,-2.22002716239884,
60.));
#79363=CARTESIAN_POINT('Ctrl Pts',(-6.68661966823323,-2.39353830166946,
60.0000000000001));
#79364=CARTESIAN_POINT('Ctrl Pts',(-6.60956772599301,-2.56598754774135,
60.0000000000001));
#79365=CARTESIAN_POINT('Ctrl Pts',(-6.52568743586049,-2.73525657050835,
60.));
#79366=CARTESIAN_POINT('Ctrl Pts',(-6.43504829728646,-2.90084515405146,
60.));
#79367=CARTESIAN_POINT('Ctrl Pts',(-6.401950884911,-2.96131079527905,60.));
#79368=CARTESIAN_POINT('Ctrl Pts',(-6.36795187632475,-3.02128535832417,
60.));
#79369=CARTESIAN_POINT('Ctrl Pts',(-6.3330533832055,-3.08074324429221,60.));
#79370=CARTESIAN_POINT('Ctrl Pts',(-6.2364595051223,-3.24531389691768,60.));
#79371=CARTESIAN_POINT('Ctrl Pts',(-6.13297666239597,-3.40592940627831,
60.));
#79372=CARTESIAN_POINT('Ctrl Pts',(-6.02288068162145,-3.56221579876367,
60.));
#79373=CARTESIAN_POINT('Ctrl Pts',(-6.01281665044061,-3.57650216159043,
60.));
#79374=CARTESIAN_POINT('Ctrl Pts',(-6.00269734068414,-3.59075231937767,
60.));
#79375=CARTESIAN_POINT('Ctrl Pts',(-5.9925229520943,-3.60496596753975,60.));
#79376=CARTESIAN_POINT('Ctrl Pts',(-5.97091601107585,-3.6351509221228,60.));
#79377=CARTESIAN_POINT('Ctrl Pts',(-5.94906067036394,-3.66517122529426,
60.));
#79378=CARTESIAN_POINT('Ctrl Pts',(-5.92695881890567,-3.69502390954886,
60.));
#79379=CARTESIAN_POINT('Ctrl Pts',(-5.90764738480234,-3.72110761325478,
60.));
#79380=CARTESIAN_POINT('Ctrl Pts',(-5.88814412064115,-3.74706799764837,
60.));
#79381=CARTESIAN_POINT('Ctrl Pts',(-5.86847065476455,-3.77287665540249,
60.));
#79382=CARTESIAN_POINT('Ctrl Pts',(-5.75525480403238,-3.92139899316552,
60.));
#79383=CARTESIAN_POINT('Ctrl Pts',(-5.63630504801428,-4.06503978380686,
59.9999999999999));
#79384=CARTESIAN_POINT('Ctrl Pts',(-5.51195816007129,-4.20352564428108,
60.));
#79385=CARTESIAN_POINT('Ctrl Pts',(-5.38717446497607,-4.34249797944989,
60.));
#79386=CARTESIAN_POINT('Ctrl Pts',(-5.25695511161658,-4.47627956078094,
59.9999999999999));
#79387=CARTESIAN_POINT('Ctrl Pts',(-5.12160437608111,-4.60455649665402,
59.9999999999999));
#79388=CARTESIAN_POINT('Ctrl Pts',(-4.98709347465071,-4.73203749044954,
59.9999999999999));
#79389=CARTESIAN_POINT('Ctrl Pts',(-4.84751410863532,-4.85408231728632,
60.));
#79390=CARTESIAN_POINT('Ctrl Pts',(-4.70313771916586,-4.97033965601283,
60.));
#79391=CARTESIAN_POINT('Ctrl Pts',(-4.56146741367584,-5.08441795339487,
60.));
#79392=CARTESIAN_POINT('Ctrl Pts',(-4.41517767953588,-5.19292392882823,
60.));
#79393=CARTESIAN_POINT('Ctrl Pts',(-4.26450693334287,-5.29547942882985,
60.));
#79394=CARTESIAN_POINT('Ctrl Pts',(-4.1549207018082,-5.37007035674584,60.));
#79395=CARTESIAN_POINT('Ctrl Pts',(-4.04301652795845,-5.44151256479602,
60.));
#79396=CARTESIAN_POINT('Ctrl Pts',(-3.9288823673735,-5.5096435767971,60.));
#79397=CARTESIAN_POINT('Ctrl Pts',(-3.93301173192423,-5.51252654933308,
-60.));
#79398=CARTESIAN_POINT('Ctrl Pts',(-4.08952080384978,-5.42059770583385,
-60.));
#79399=CARTESIAN_POINT('Ctrl Pts',(-4.24181965717463,-5.32232120961294,
-60.));
#79400=CARTESIAN_POINT('Ctrl Pts',(-4.38947572522641,-5.21781239717533,
-60.));
#79401=CARTESIAN_POINT('Ctrl Pts',(-4.53705291796563,-5.11335941153411,
-60.));
#79402=CARTESIAN_POINT('Ctrl Pts',(-4.67999341387791,-5.00268139404814,
-60.));
#79403=CARTESIAN_POINT('Ctrl Pts',(-4.81813643652202,-4.88627279397718,
-60.));
#79404=CARTESIAN_POINT('Ctrl Pts',(-4.95837547651839,-4.7680979487421,-60.));
#79405=CARTESIAN_POINT('Ctrl Pts',(-5.09367081531429,-4.64401689247806,
-60.));
#79406=CARTESIAN_POINT('Ctrl Pts',(-5.22383156481562,-4.51449705972283,
-60.));
#79407=CARTESIAN_POINT('Ctrl Pts',(-5.35596904369448,-4.38301023108473,
-60.));
#79408=CARTESIAN_POINT('Ctrl Pts',(-5.48281531429085,-4.24591770621096,
-60.));
#79409=CARTESIAN_POINT('Ctrl Pts',(-5.6041399810699,-4.1036642545346,-60.));
#79410=CARTESIAN_POINT('Ctrl Pts',(-5.70214434390653,-3.98875391302721,
-60.));
#79411=CARTESIAN_POINT('Ctrl Pts',(-5.79654527992217,-3.87047499888056,
-60.));
#79412=CARTESIAN_POINT('Ctrl Pts',(-5.88720352206258,-3.74904468981495,
-60.));
#79413=CARTESIAN_POINT('Ctrl Pts',(-5.90038741125276,-3.73138580187213,
-60.));
#79414=CARTESIAN_POINT('Ctrl Pts',(-5.91349113483187,-3.71366150064713,
-60.));
#79415=CARTESIAN_POINT('Ctrl Pts',(-5.92650729286421,-3.6958821765402,-60.));
#79416=CARTESIAN_POINT('Ctrl Pts',(-6.03764306928045,-3.54407709059468,
-60.));
#79417=CARTESIAN_POINT('Ctrl Pts',(-6.14253987674664,-3.38807418550578,
-60.));
#79418=CARTESIAN_POINT('Ctrl Pts',(-6.24102436169895,-3.22837952733627,
-60.));
#79419=CARTESIAN_POINT('Ctrl Pts',(-6.34131022385272,-3.06576389824877,
-60.));
#79420=CARTESIAN_POINT('Ctrl Pts',(-6.43494756756259,-2.89931974799542,
-60.));
#79421=CARTESIAN_POINT('Ctrl Pts',(-6.52172278078293,-2.72953725844725,
-60.));
#79422=CARTESIAN_POINT('Ctrl Pts',(-6.54759921289344,-2.6789079957661,-60.));
#79423=CARTESIAN_POINT('Ctrl Pts',(-6.57286520629013,-2.62798160952088,
-60.));
#79424=CARTESIAN_POINT('Ctrl Pts',(-6.59751447498585,-2.57677045843014,
-60.));
#79425=CARTESIAN_POINT('Ctrl Pts',(-6.68040386452845,-2.40456003287614,
-60.));
#79426=CARTESIAN_POINT('Ctrl Pts',(-6.75632263423444,-2.22913159646629,
-60.));
#79427=CARTESIAN_POINT('Ctrl Pts',(-6.82519899342782,-2.05090247570647,
-60.));
#79428=CARTESIAN_POINT('Ctrl Pts',(-6.89423580505223,-1.87225815739493,
-60.));
#79429=CARTESIAN_POINT('Ctrl Pts',(-6.95619763361968,-1.69079948329051,
-60.));
#79430=CARTESIAN_POINT('Ctrl Pts',(-7.01096564304006,-1.50692333508897,
-60.));
#79431=CARTESIAN_POINT('Ctrl Pts',(-7.02583863164074,-1.45698929722488,
-60.));
#79432=CARTESIAN_POINT('Ctrl Pts',(-7.04018082205761,-1.40687687506854,
-60.));
#79433=CARTESIAN_POINT('Ctrl Pts',(-7.05398920151378,-1.35659381192878,
-60.));
#79434=CARTESIAN_POINT('Ctrl Pts',(-7.06130669006673,-1.32994725719725,
-60.));
#79435=CARTESIAN_POINT('Ctrl Pts',(-7.06847426548418,-1.30325278069041,
-60.));
#79436=CARTESIAN_POINT('Ctrl Pts',(-7.07549144748142,-1.27651152744079,
-60.));
#79437=CARTESIAN_POINT('Ctrl Pts',(-7.08197914199504,-1.25178805838116,
-60.));
#79438=CARTESIAN_POINT('Ctrl Pts',(-7.08833643947356,-1.22703150330183,
-60.));
#79439=CARTESIAN_POINT('Ctrl Pts',(-7.09456102669435,-1.20225171368677,
-60.));
#79440=CARTESIAN_POINT('Ctrl Pts',(-7.14220708680675,-1.01257498434034,
-60.));
#79441=CARTESIAN_POINT('Ctrl Pts',(-7.18212278214278,-0.821380786189583,
-60.));
#79442=CARTESIAN_POINT('Ctrl Pts',(-7.2142837787498,-0.629129382873918,
-60.));
#79443=CARTESIAN_POINT('Ctrl Pts',(-7.24659626634971,-0.435972399537559,
-60.));
#79444=CARTESIAN_POINT('Ctrl Pts',(-7.27108109768127,-0.241747604229979,
-60.));
#79445=CARTESIAN_POINT('Ctrl Pts',(-7.28766818194827,-0.0468948140504708,
-60.));
#79446=CARTESIAN_POINT('Ctrl Pts',(-7.30418370687894,0.147117350005538,
-60.));
#79447=CARTESIAN_POINT('Ctrl Pts',(-7.31286968915527,0.341752756646404,
-60.));
#79448=CARTESIAN_POINT('Ctrl Pts',(-7.31360856011759,0.536594313533747,
-60.));
#79449=CARTESIAN_POINT('Ctrl Pts',(-7.31409810186552,0.665687323263242,
-60.));
#79450=CARTESIAN_POINT('Ctrl Pts',(-7.31109804508312,0.794871162698884,
-60.));
#79451=CARTESIAN_POINT('Ctrl Pts',(-7.30456172141964,0.924026543564304,
-60.));
#79452=CARTESIAN_POINT('Ctrl Pts',(-7.29714775632053,1.07052380034001,-60.));
#79453=CARTESIAN_POINT('Ctrl Pts',(-7.28518443291222,1.21698458021077,-60.));
#79454=CARTESIAN_POINT('Ctrl Pts',(-7.26874210131775,1.36321456224292,-60.));
#79455=CARTESIAN_POINT('Ctrl Pts',(-7.26405275890041,1.40491925926174,-60.));
#79456=CARTESIAN_POINT('Ctrl Pts',(-7.25899899522214,1.44660517619321,-60.));
#79457=CARTESIAN_POINT('Ctrl Pts',(-7.25358219346459,1.4882677788116,-60.));
#79458=CARTESIAN_POINT('Ctrl Pts',(-7.24901532725683,1.52339321639291,-60.));
#79459=CARTESIAN_POINT('Ctrl Pts',(-7.2441894596039,1.55850797715054,-60.));
#79460=CARTESIAN_POINT('Ctrl Pts',(-7.2391110333888,1.59357215124191,-60.));
#79461=CARTESIAN_POINT('Ctrl Pts',(-7.2112095232227,1.78621911871558,-60.));
#79462=CARTESIAN_POINT('Ctrl Pts',(-7.17566576866628,1.97753353254058,-60.));
#79463=CARTESIAN_POINT('Ctrl Pts',(-7.13276029827355,2.16706682927203,-60.));
#79464=CARTESIAN_POINT('Ctrl Pts',(-7.08881801138619,2.36118022375171,-60.));
#79465=CARTESIAN_POINT('Ctrl Pts',(-7.03715395035248,2.55342602264969,-60.));
#79466=CARTESIAN_POINT('Ctrl Pts',(-6.9780154261089,2.74333156236495,-60.));
#79467=CARTESIAN_POINT('Ctrl Pts',(-6.91852012664441,2.93438277813066,-60.));
#79468=CARTESIAN_POINT('Ctrl Pts',(-6.85145977804132,3.12306613872702,-60.));
#79469=CARTESIAN_POINT('Ctrl Pts',(-6.77703309916436,3.30889912524294,-60.));
#79470=CARTESIAN_POINT('Ctrl Pts',(-6.70296831599029,3.49382850890717,-60.));
#79471=CARTESIAN_POINT('Ctrl Pts',(-6.62160844992583,3.67593589277402,-60.));
#79472=CARTESIAN_POINT('Ctrl Pts',(-6.53309963579732,3.85473369085425,-60.));
#79473=CARTESIAN_POINT('Ctrl Pts',(-6.46222636298705,3.99790570424058,-60.));
#79474=CARTESIAN_POINT('Ctrl Pts',(-6.38676821807548,4.13895553781842,-60.));
#79475=CARTESIAN_POINT('Ctrl Pts',(-6.30677843138628,4.27762247763241,-60.));
#79476=CARTESIAN_POINT('Ctrl Pts',(-6.29320342493038,4.30115553955328,-60.));
#79477=CARTESIAN_POINT('Ctrl Pts',(-6.2795014627675,4.32461364165953,-60.));
#79478=CARTESIAN_POINT('Ctrl Pts',(-6.2656767166826,4.34798939028162,-60.));
#79479=CARTESIAN_POINT('Ctrl Pts',(-6.24175455611388,4.38843848124628,-60.));
#79480=CARTESIAN_POINT('Ctrl Pts',(-6.21746139506088,4.42864682897115,-60.));
#79481=CARTESIAN_POINT('Ctrl Pts',(-6.19280011122744,4.46860844401354,-60.));
#79482=CARTESIAN_POINT('Ctrl Pts',(-6.08720463490951,4.63971736937743,-60.));
#79483=CARTESIAN_POINT('Ctrl Pts',(-5.97486400026855,4.80630398343347,-60.));
#79484=CARTESIAN_POINT('Ctrl Pts',(-5.85618687666969,4.96812701738046,-60.));
#79485=CARTESIAN_POINT('Ctrl Pts',(-5.73620135676387,5.13173412439543,-60.));
#79486=CARTESIAN_POINT('Ctrl Pts',(-5.60973852475551,5.29047255139371,-60.));
#79487=CARTESIAN_POINT('Ctrl Pts',(-5.47717146481258,5.44407198105424,-60.));
#79488=CARTESIAN_POINT('Ctrl Pts',(-5.40441740036826,5.52836881021334,-60.));
#79489=CARTESIAN_POINT('Ctrl Pts',(-5.32982396086839,5.61111740341094,-60.));
#79490=CARTESIAN_POINT('Ctrl Pts',(-5.25344719017398,5.69226956964437,-60.));
#79491=CARTESIAN_POINT('Ctrl Pts',(-5.20079500682673,5.74821378798068,-60.));
#79492=CARTESIAN_POINT('Ctrl Pts',(-5.14729523733269,5.80339927185339,-60.));
#79493=CARTESIAN_POINT('Ctrl Pts',(-5.09296524201554,5.85780942633472,-60.));
#79494=CARTESIAN_POINT('Ctrl Pts',(-5.06656807641211,5.88424553865109,-60.));
#79495=CARTESIAN_POINT('Ctrl Pts',(-5.03997397463221,5.91049937778292,-60.));
#79496=CARTESIAN_POINT('Ctrl Pts',(-5.01320308796063,5.93655167337536,-60.));
#79497=CARTESIAN_POINT('Ctrl Pts',(-4.86528754035126,6.08049683351553,-60.));
#79498=CARTESIAN_POINT('Ctrl Pts',(-4.71185216667681,6.21841958267782,-60.));
#79499=CARTESIAN_POINT('Ctrl Pts',(-4.55329863095189,6.35005394068721,-60.));
#79500=CARTESIAN_POINT('Ctrl Pts',(-4.39412852588249,6.48220018705946,-60.));
#79501=CARTESIAN_POINT('Ctrl Pts',(-4.22979994004088,6.60800956229862,-60.));
#79502=CARTESIAN_POINT('Ctrl Pts',(-4.06067591285683,6.72718329191288,-60.));
#79503=CARTESIAN_POINT('Ctrl Pts',(-3.89230921701461,6.84582336583042,-60.));
#79504=CARTESIAN_POINT('Ctrl Pts',(-3.71918944625603,6.95788757299026,-60.));
#79505=CARTESIAN_POINT('Ctrl Pts',(-3.54163890299614,7.06304431300309,-60.));
#79506=CARTESIAN_POINT('Ctrl Pts',(-3.50154405698965,7.08679103447151,-60.));
#79507=CARTESIAN_POINT('Ctrl Pts',(-3.46122313234071,7.11018533926288,-60.));
#79508=CARTESIAN_POINT('Ctrl Pts',(-3.4206796250969,7.13322310757535,-60.));
#79509=CARTESIAN_POINT('Ctrl Pts',(4.59493373696683,-6.44781750921883,-60.6643731623753));
#79510=CARTESIAN_POINT('Ctrl Pts',(5.66758804391333,-5.68341533656089,-60.6114196764411));
#79511=CARTESIAN_POINT('Ctrl Pts',(7.420231908041,-3.6147783613617,-60.5055449235297));
#79512=CARTESIAN_POINT('Ctrl Pts',(8.24850409473424,0.389368816384953,-60.3467489036408));
#79513=CARTESIAN_POINT('Ctrl Pts',(7.05091419264973,4.26423914542533,-60.1879851027094));
#79514=CARTESIAN_POINT('Ctrl Pts',(3.1979029178683,8.12048633360201,-59.9763000348008));
#79515=CARTESIAN_POINT('Ctrl Pts',(-4.23022369577523,8.35267581578188,-59.7116936999148));
#79516=CARTESIAN_POINT('Ctrl Pts',(-9.31726541786132,0.94545657484609,-59.3941660980519));
#79517=CARTESIAN_POINT('Ctrl Pts',(-6.42446717770634,-5.90348168320496,
-59.1295597631658));
#79518=CARTESIAN_POINT('Ctrl Pts',(-1.4490501247666,-8.11293657404488,-58.9178746952573));
#79519=CARTESIAN_POINT('Ctrl Pts',(2.61219513444578,-7.83570724861456,-58.7591108943257));
#79520=CARTESIAN_POINT('Ctrl Pts',(6.02072951395808,-5.62778786725318,-58.6003470933942));
#79521=CARTESIAN_POINT('Ctrl Pts',(8.68771888553699,-0.861913486306708,
-58.3886620254857));
#79522=CARTESIAN_POINT('Ctrl Pts',(7.23919397520838,4.88343575175983,-58.1769769575768));
#79523=CARTESIAN_POINT('Ctrl Pts',(2.63366693853143,7.8007910704191,-57.9652918896683));
#79524=CARTESIAN_POINT('Ctrl Pts',(-2.77103540777255,8.27359001524915,-57.7536068217594));
#79525=CARTESIAN_POINT('Ctrl Pts',(-8.62164699515589,3.66576579702773,-57.4890004868736));
#79526=CARTESIAN_POINT('Ctrl Pts',(-7.73354855495184,-5.27571385914043,
-57.1714728850106));
#79527=CARTESIAN_POINT('Ctrl Pts',(-1.1157857437006,-8.65379742007332,-56.9068665501247));
#79528=CARTESIAN_POINT('Ctrl Pts',(4.11628243882215,-7.14010761184303,-56.695181482216));
#79529=CARTESIAN_POINT('Ctrl Pts',(7.04367409087663,-4.31305663032169,-56.5364176812845));
#79530=CARTESIAN_POINT('Ctrl Pts',(8.23048748680303,-0.42887819825834,-56.3776538803531));
#79531=CARTESIAN_POINT('Ctrl Pts',(7.20173000873569,4.93473188277679,-56.1659688124443));
#79532=CARTESIAN_POINT('Ctrl Pts',(2.39419873589606,8.39775644139713,-55.9542837445356));
#79533=CARTESIAN_POINT('Ctrl Pts',(-3.00812442644778,7.66419399588113,-55.742598676627));
#79534=CARTESIAN_POINT('Ctrl Pts',(-7.44760558900325,4.54573886957917,-55.5309136087182));
#79535=CARTESIAN_POINT('Ctrl Pts',(-8.95683435881455,-2.74700645169454,
-55.2663072738324));
#79536=CARTESIAN_POINT('Ctrl Pts',(-2.51973131736528,-9.01619753462101,
-54.9487796719692));
#79537=CARTESIAN_POINT('Ctrl Pts',(4.718673013345,-7.33943323573433,-54.6841733370835));
#79538=CARTESIAN_POINT('Ctrl Pts',(7.74699969690703,-2.8122842977038,-54.4724882691748));
#79539=CARTESIAN_POINT('Ctrl Pts',(8.16632621930467,1.23567797082505,-54.3137244682434));
#79540=CARTESIAN_POINT('Ctrl Pts',(6.57324816560372,4.97164730573518,-54.1549606673117));
#79541=CARTESIAN_POINT('Ctrl Pts',(2.33241468102429,8.41286709177905,-53.943275599403));
#79542=CARTESIAN_POINT('Ctrl Pts',(-3.57570292077998,7.96673386021558,-53.7315905314943));
#79543=CARTESIAN_POINT('Ctrl Pts',(-7.23662431142663,3.92682465094442,-53.5199054635857));
#79544=CARTESIAN_POINT('Ctrl Pts',(-8.62520104969994,-1.31775439966483,
-53.3082203956771));
#79545=CARTESIAN_POINT('Ctrl Pts',(-5.08395332956645,-7.86920232075575,
-53.0436140607911));
#79546=CARTESIAN_POINT('Ctrl Pts',(3.87788594583802,-8.52073145927405,-52.7260864589282));
#79547=CARTESIAN_POINT('Ctrl Pts',(8.3362320335911,-2.5768955255669,-52.4614801240423));
#79548=CARTESIAN_POINT('Ctrl Pts',(7.73805855367662,2.8367934663068,-52.2497950561336));
#79549=CARTESIAN_POINT('Ctrl Pts',(5.45231667204648,6.20387192351473,-52.0910312552021));
#79550=CARTESIAN_POINT('Ctrl Pts',(1.82779777155195,8.0364185862005,-51.9322674542705));
#79551=CARTESIAN_POINT('Ctrl Pts',(-3.63270370379316,7.93851086500441,-51.7205823863618));
#79552=CARTESIAN_POINT('Ctrl Pts',(-7.86568586511065,3.79282027538551,-51.5088973184531));
#79553=CARTESIAN_POINT('Ctrl Pts',(-8.06524943223459,-1.65542588568015,
-51.2972122505444));
#79554=CARTESIAN_POINT('Ctrl Pts',(-5.75054767799861,-6.56214684434599,
-51.0855271826359));
#79555=CARTESIAN_POINT('Ctrl Pts',(1.17744529526638,-9.29432887296655,-50.8209208477498));
#79556=CARTESIAN_POINT('Ctrl Pts',(8.45361418193282,-4.02209786974241,-50.5033932458868));
#79557=CARTESIAN_POINT('Ctrl Pts',(8.03730415832691,3.39630636628952,-50.238786911001));
#79558=CARTESIAN_POINT('Ctrl Pts',(4.09366137959014,7.15310309306182,-50.0271018430924));
#79559=CARTESIAN_POINT('Ctrl Pts',(0.176726936200001,8.25739374897774,-49.8683380421608));
#79560=CARTESIAN_POINT('Ctrl Pts',(-3.77637944480456,7.32555981991549,-49.7095742412292));
#79561=CARTESIAN_POINT('Ctrl Pts',(-7.89112337486653,3.73452310690604,-49.4978891733208));
#79562=CARTESIAN_POINT('Ctrl Pts',(-8.46025155684443,-2.1630171901463,-49.2862041054118));
#79563=CARTESIAN_POINT('Ctrl Pts',(-5.10469934135701,-6.45993249976306,
-49.0745190375033));
#79564=CARTESIAN_POINT('Ctrl Pts',(-0.174200713771704,-8.72354422898261,
-48.8628339695944));
#79565=CARTESIAN_POINT('Ctrl Pts',(6.88566245154638,-6.35284024870503,-48.5982276347087));
#79566=CARTESIAN_POINT('Ctrl Pts',(9.05770761919772,2.36617765518383,-48.2807000328456));
#79567=CARTESIAN_POINT('Ctrl Pts',(3.96233018059051,7.77387256180204,-48.0160936979597));
#79568=CARTESIAN_POINT('Ctrl Pts',(-1.47399934069216,8.10877754623701,-47.804408630051));
#79569=CARTESIAN_POINT('Ctrl Pts',(-5.1818917662573,6.43146807956242,-47.6456448291196));
#79570=CARTESIAN_POINT('Ctrl Pts',(-7.6063569291163,3.17304312186065,-47.486881028188));
#79571=CARTESIAN_POINT('Ctrl Pts',(-8.44217486912475,-2.22399964759411,
-47.2751959602793));
#79572=CARTESIAN_POINT('Ctrl Pts',(-5.08006411145565,-7.10263672120833,
-47.0635108923708));
#79573=CARTESIAN_POINT('Ctrl Pts',(0.254115101922676,-8.22946588680703,
-46.8518258244619));
#79574=CARTESIAN_POINT('Ctrl Pts',(5.48398835986514,-6.78648962811834,-46.6401407565533));
#79575=CARTESIAN_POINT('Ctrl Pts',(9.35889206087632,-0.426691943992846,
-46.3755344216674));
#79576=CARTESIAN_POINT('Ctrl Pts',(5.40635409573626,7.64278741051195,-46.0580068198043));
#79577=CARTESIAN_POINT('Ctrl Pts',(-1.97420597526809,8.49915677196114,-45.7934004849185));
#79578=CARTESIAN_POINT('Ctrl Pts',(-6.3491530516771,5.2548266267402,-45.5817154170098));
#79579=CARTESIAN_POINT('Ctrl Pts',(-8.1059799567344,1.58394219485922,-45.4229516160784));
#79580=CARTESIAN_POINT('Ctrl Pts',(-7.86275378607339,-2.47021684997314,
-45.2641878151467));
#79581=CARTESIAN_POINT('Ctrl Pts',(-5.02696592541148,-7.13765399400476,
-45.0525027472383));
#79582=CARTESIAN_POINT('Ctrl Pts',(0.686813685647454,-8.70533093748678,
-44.8408176793293));
#79583=CARTESIAN_POINT('Ctrl Pts',(5.4935424570323,-6.13267270771309,-44.6291326114208));
#79584=CARTESIAN_POINT('Ctrl Pts',(8.5657174085411,-1.66104036095169,-44.417447543512));
#79585=CARTESIAN_POINT('Ctrl Pts',(7.43517373916352,5.69992263900624,-44.1528412086262));
#79586=CARTESIAN_POINT('Ctrl Pts',(-0.784985710407776,9.32870095164485,
-43.8353136067632));
#79587=CARTESIAN_POINT('Ctrl Pts',(-6.98323053873475,5.23140959111778,-43.5707072718773));
#79588=CARTESIAN_POINT('Ctrl Pts',(-8.24137938270553,-0.067920696662337,
-43.3590222039687));
#79589=CARTESIAN_POINT('Ctrl Pts',(-7.22175712406885,-4.00774350184691,
-43.2002584030371));
#79590=CARTESIAN_POINT('Ctrl Pts',(-4.42511092475034,-6.95293187727002,
-43.0414946021055));
#79591=CARTESIAN_POINT('Ctrl Pts',(0.74998704541379,-8.69793138539803,-42.8298095341971));
#79592=CARTESIAN_POINT('Ctrl Pts',(6.13101610681114,-6.21813004592047,-42.6181244662881));
#79593=CARTESIAN_POINT('Ctrl Pts',(8.15202112896183,-1.15465786279127,-42.4064393983796));
#79594=CARTESIAN_POINT('Ctrl Pts',(7.62314388033113,4.24479059359405,-42.1947543304707));
#79595=CARTESIAN_POINT('Ctrl Pts',(2.01829922153478,9.14862803236388,-41.9301479955849));
#79596=CARTESIAN_POINT('Ctrl Pts',(-6.60752745019684,6.63185079790396,-41.6126203937219));
#79597=CARTESIAN_POINT('Ctrl Pts',(-8.71142860376982,-0.49413231889662,
-41.348014058836));
#79598=CARTESIAN_POINT('Ctrl Pts',(-6.26168200844734,-5.35875785754551,
-41.1363289909274));
#79599=CARTESIAN_POINT('Ctrl Pts',(-2.94464442381838,-7.71653116062592,
-40.9775651899958));
#79600=CARTESIAN_POINT('Ctrl Pts',(1.09151545285383,-8.16905517195739,-40.8188013890643));
#79601=CARTESIAN_POINT('Ctrl Pts',(6.17458484789321,-6.17179008955651,-40.6071163211557));
#79602=CARTESIAN_POINT('Ctrl Pts',(8.69477515810992,-0.809558348651662,
-40.3954312532469));
#79603=CARTESIAN_POINT('Ctrl Pts',(6.98055794413596,4.36583257302729,-40.1837461853383));
#79604=CARTESIAN_POINT('Ctrl Pts',(3.09910296317843,8.15635522934804,-39.9720611174295));
#79605=CARTESIAN_POINT('Ctrl Pts',(-4.34680255725139,8.29917069052533,-39.7074547825437));
#79606=CARTESIAN_POINT('Ctrl Pts',(-9.32575364040251,0.819257620827232,
-39.3899271806806));
#79607=CARTESIAN_POINT('Ctrl Pts',(-6.34686678583791,-5.9875234504747,-39.1253208457948));
#79608=CARTESIAN_POINT('Ctrl Pts',(-1.34015246294474,-8.13197016268393,
-38.9136357778861));
#79609=CARTESIAN_POINT('Ctrl Pts',(2.71590641448793,-7.79997668479713,-38.7548719769546));
#79610=CARTESIAN_POINT('Ctrl Pts',(6.09533149127371,-5.54723376087484,-38.5961081760231));
#79611=CARTESIAN_POINT('Ctrl Pts',(8.69827003214864,-0.746049194896171,
-38.3844231081144));
#79612=CARTESIAN_POINT('Ctrl Pts',(7.17359836511665,4.97935600915946,-38.1727380402057));
#79613=CARTESIAN_POINT('Ctrl Pts',(2.52952388592635,7.83518935174345,-37.961052972297));
#79614=CARTESIAN_POINT('Ctrl Pts',(-2.8809430316479,8.23594178294709,-37.7493679043883));
#79615=CARTESIAN_POINT('Ctrl Pts',(-8.66971126591377,3.55063841976205,-37.4847615695025));
#79616=CARTESIAN_POINT('Ctrl Pts',(-7.66260082678378,-5.37823508040855,
-37.1672339676394));
#79617=CARTESIAN_POINT('Ctrl Pts',(-1.00045170994875,-8.66788621540555,
-36.9026276327536));
#79618=CARTESIAN_POINT('Ctrl Pts',(4.21100082016462,-7.08466085591197,-36.6909425648448));
#79619=CARTESIAN_POINT('Ctrl Pts',(7.10048366399641,-4.21887611490971,-36.5321787639134));
#79620=CARTESIAN_POINT('Ctrl Pts',(8.23546932769645,-0.319238686367667,
-36.3734149629817));
#79621=CARTESIAN_POINT('Ctrl Pts',(7.13537742784409,5.03019680684496,-36.1617298950732));
#79622=CARTESIAN_POINT('Ctrl Pts',(2.28215741217129,8.42889419295488,-35.9500448271644));
#79623=CARTESIAN_POINT('Ctrl Pts',(-3.10991845228071,7.62345659706342,-35.7383597592558));
#79624=CARTESIAN_POINT('Ctrl Pts',(-7.50747875837207,4.44615929722344,-35.5266746913471));
#79625=CARTESIAN_POINT('Ctrl Pts',(-8.91945952295018,-2.86603706198215,
-35.2620683564612));
#79626=CARTESIAN_POINT('Ctrl Pts',(-2.39944315868245,-9.04895223432061,
-34.9445407545982));
#79627=CARTESIAN_POINT('Ctrl Pts',(4.81599059219255,-7.27594596482617,-34.6799344197123));
#79628=CARTESIAN_POINT('Ctrl Pts',(7.78376272709339,-2.70887156562104,-34.4682493518036));
#79629=CARTESIAN_POINT('Ctrl Pts',(8.1491471373085,1.3443157628072,-34.3094855508721));
#79630=CARTESIAN_POINT('Ctrl Pts',(6.50646009136296,5.05873951353536,-34.1507217499406));
#79631=CARTESIAN_POINT('Ctrl Pts',(2.22017743346687,8.44318086489356,-33.9390366820319));
#79632=CARTESIAN_POINT('Ctrl Pts',(-3.68147533938544,7.91841139973504,-33.7273516141232));
#79633=CARTESIAN_POINT('Ctrl Pts',(-7.28827443373505,3.83010953442713,-33.5156665462146));
#79634=CARTESIAN_POINT('Ctrl Pts',(-8.60688830613688,-1.43249554602399,
-33.3039814783058));
#79635=CARTESIAN_POINT('Ctrl Pts',(-4.97871184944764,-7.93620532385422,
-33.03937514342));
#79636=CARTESIAN_POINT('Ctrl Pts',(3.99100891174753,-8.4683358387062,-32.7218475415569));
#79637=CARTESIAN_POINT('Ctrl Pts',(8.3698082446935,-2.46565711610875,-32.4572412066711));
#79638=CARTESIAN_POINT('Ctrl Pts',(7.69959610060171,2.93958623590426,-32.2455561387624));
#79639=CARTESIAN_POINT('Ctrl Pts',(5.36921899827152,6.27592792216698,-32.0867923378309));
#79640=CARTESIAN_POINT('Ctrl Pts',(1.72061826725716,8.06004597782691,-31.9280285368993));
#79641=CARTESIAN_POINT('Ctrl Pts',(-3.73809523544606,7.88943185306239,-31.7163434689907));
#79642=CARTESIAN_POINT('Ctrl Pts',(-7.91549573176501,3.68774010613095,-31.5046584010819));
#79643=CARTESIAN_POINT('Ctrl Pts',(-8.04248971735526,-1.76268046264216,
-31.2929733331733));
#79644=CARTESIAN_POINT('Ctrl Pts',(-5.66265257150908,-6.63814248552081,
-31.0812882652646));
#79645=CARTESIAN_POINT('Ctrl Pts',(1.30110936217168,-9.2778252327726,-30.8166819303787));
#79646=CARTESIAN_POINT('Ctrl Pts',(8.50642510580062,-3.90916818903571,-30.4991543285157));
#79647=CARTESIAN_POINT('Ctrl Pts',(7.99136438532443,3.50303444575207,-30.2345479936298));
#79648=CARTESIAN_POINT('Ctrl Pts',(3.99804368483144,7.20698231195957,-30.0228629257211));
#79649=CARTESIAN_POINT('Ctrl Pts',(0.0667512025953981,8.25901496624065,
-29.8640991247897));
#79650=CARTESIAN_POINT('Ctrl Pts',(-3.87359583864445,7.2746218915583,-29.7053353238581));
#79651=CARTESIAN_POINT('Ctrl Pts',(-7.94015466836669,3.62910936674481,-29.4936502559494));
#79652=CARTESIAN_POINT('Ctrl Pts',(-8.43069744832558,-2.27548682807728,
-29.2819651880407));
#79653=CARTESIAN_POINT('Ctrl Pts',(-5.0182226450366,-6.52733672733278,-29.070280120132));
#79654=CARTESIAN_POINT('Ctrl Pts',(-0.0580176842298914,-8.72509047242555,
-28.8585950522234));
#79655=CARTESIAN_POINT('Ctrl Pts',(6.96964987081364,-6.26058362299151,-28.5939887173375));
#79656=CARTESIAN_POINT('Ctrl Pts',(9.02539513654387,2.48658533736819,-28.2764611154745));
#79657=CARTESIAN_POINT('Ctrl Pts',(3.85845761819846,7.82594785797371,-28.0118547805886));
#79658=CARTESIAN_POINT('Ctrl Pts',(-1.58184964927522,8.08842994887182,-27.8001697126799));
#79659=CARTESIAN_POINT('Ctrl Pts',(-5.26707730973789,6.36189284324087,-27.6414059117484));
#79660=CARTESIAN_POINT('Ctrl Pts',(-7.64793649183002,3.07147127664212,-27.4826421108169));
#79661=CARTESIAN_POINT('Ctrl Pts',(-8.41181028701722,-2.33622315899216,
-27.2709570429082));
#79662=CARTESIAN_POINT('Ctrl Pts',(-4.98503099143786,-7.16965590418124,
-27.0592719749995));
#79663=CARTESIAN_POINT('Ctrl Pts',(0.363680730071077,-8.22535224739468,
-26.8475869070908));
#79664=CARTESIAN_POINT('Ctrl Pts',(5.57387478172201,-6.71286002545695,-26.6359018391822));
#79665=CARTESIAN_POINT('Ctrl Pts',(9.36374428260679,-0.302025879935631,
-26.3712955042962));
#79666=CARTESIAN_POINT('Ctrl Pts',(5.30409909579721,7.7141037582293,-26.0537679024333));
#79667=CARTESIAN_POINT('Ctrl Pts',(-2.08721043851178,8.47211352925138,-25.7891615675473));
#79668=CARTESIAN_POINT('Ctrl Pts',(-6.41856628069534,5.16981181969319,-25.5774764996387));
#79669=CARTESIAN_POINT('Ctrl Pts',(-8.12635386345765,1.47585799503287,-25.4187126987071));
#79670=CARTESIAN_POINT('Ctrl Pts',(-7.82916181514927,-2.57470263496797,
-25.2599488977757));
#79671=CARTESIAN_POINT('Ctrl Pts',(-4.93147120402558,-7.20396298694315,
-25.0482638298669));
#79672=CARTESIAN_POINT('Ctrl Pts',(0.80267783129953,-8.69541304764167,-24.8365787619583));
#79673=CARTESIAN_POINT('Ctrl Pts',(5.57472144074746,-6.05897385084444,-24.6248936940496));
#79674=CARTESIAN_POINT('Ctrl Pts',(8.5870772328764,-1.54682720441233,-24.4132086261409));
#79675=CARTESIAN_POINT('Ctrl Pts',(7.35861111677501,5.7984281537566,-24.148602291255));
#79676=CARTESIAN_POINT('Ctrl Pts',(-0.909142294207787,9.31742047455447,
-23.831074689392));
#79677=CARTESIAN_POINT('Ctrl Pts',(-7.05227571023749,5.13795313076632,-23.5664683545061));
#79678=CARTESIAN_POINT('Ctrl Pts',(-8.23974415554159,-0.177661481296447,
-23.3547832865974));
#79679=CARTESIAN_POINT('Ctrl Pts',(-7.16774742692252,-4.10355708617308,
-23.1960194856659));
#79680=CARTESIAN_POINT('Ctrl Pts',(-4.33212943221437,-7.01124261232236,
-23.0372556847344));
#79681=CARTESIAN_POINT('Ctrl Pts',(0.865747052963905,-8.68717289995225,
-22.8255706168257));
#79682=CARTESIAN_POINT('Ctrl Pts',(6.21327656379671,-6.13593465673581,-22.613885548917));
#79683=CARTESIAN_POINT('Ctrl Pts',(8.16667436351112,-1.04599861735849,-22.4022004810083));
#79684=CARTESIAN_POINT('Ctrl Pts',(7.56594194114363,4.34592824917043,-22.1905154130997));
#79685=CARTESIAN_POINT('Ctrl Pts',(1.89629202393501,9.17469362879016,-21.9259090782138));
#79686=CARTESIAN_POINT('Ctrl Pts',(-6.69525499167751,6.54327323341937,-21.6083814763508));
#79687=CARTESIAN_POINT('Ctrl Pts',(-8.70407602585803,-0.610094749395952,
-21.3437751414648));
#79688=CARTESIAN_POINT('Ctrl Pts',(-6.18976657936131,-5.44166675236,-21.1320900735562));
#79689=CARTESIAN_POINT('Ctrl Pts',(-2.84162568899887,-7.75505946974343,
-20.9733262726247));
#79690=CARTESIAN_POINT('Ctrl Pts',(1.200202366515,-8.15379559872055,-20.8145624716932));
#79691=CARTESIAN_POINT('Ctrl Pts',(6.25622435294957,-6.0890186236323,-20.6028774037845));
#79692=CARTESIAN_POINT('Ctrl Pts',(8.7047847293251,-0.693702087401876,-20.3911923358758));
#79693=CARTESIAN_POINT('Ctrl Pts',(6.92180112003964,4.458402462964,-20.1795072679671));
#79694=CARTESIAN_POINT('Ctrl Pts',(2.99021358987876,8.19690139568593,-19.9678222000584));
#79695=CARTESIAN_POINT('Ctrl Pts',(-4.4569335177732,8.24055036028256,-19.7032158651726));
#79696=CARTESIAN_POINT('Ctrl Pts',(-9.33583642412451,0.694998037950466,
-19.3856882633095));
#79697=CARTESIAN_POINT('Ctrl Pts',(-6.2665708099483,-6.07151096112495,-19.1210819284237));
#79698=CARTESIAN_POINT('Ctrl Pts',(-1.23174377969414,-8.14909532475251,
-18.909396860515));
#79699=CARTESIAN_POINT('Ctrl Pts',(2.81953443944885,-7.76311854092135,-18.7506330595834));
#79700=CARTESIAN_POINT('Ctrl Pts',(6.16866108305093,-5.46557305584287,-18.5918692586519));
#79701=CARTESIAN_POINT('Ctrl Pts',(8.70743357014198,-0.630152025265054,
-18.3801841907432));
#79702=CARTESIAN_POINT('Ctrl Pts',(7.10665440379958,5.07444213238395,-18.1684991228345));
#79703=CARTESIAN_POINT('Ctrl Pts',(2.42496184085793,7.86817916277512,-17.9568140549259));
#79704=CARTESIAN_POINT('Ctrl Pts',(-2.99036197747448,8.1968472626595,-17.7451289870171));
#79705=CARTESIAN_POINT('Ctrl Pts',(-8.71622481146367,3.43487287366311,-17.4805226521313));
#79706=CARTESIAN_POINT('Ctrl Pts',(-7.59030180965086,-5.47979766498507,
-17.1629950502683));
#79707=CARTESIAN_POINT('Ctrl Pts',(-0.884936590487096,-8.68044021337483,
-16.8983887153824));
#79708=CARTESIAN_POINT('Ctrl Pts',(4.30497073139276,-7.02795662711218,-16.6867036474737));
#79709=CARTESIAN_POINT('Ctrl Pts',(7.15603497791545,-4.12394802713198,-16.5279398465422));
#79710=CARTESIAN_POINT('Ctrl Pts',(8.23899025497878,-0.209542274176545,
-16.3691760456107));
#79711=CARTESIAN_POINT('Ctrl Pts',(7.06775983111587,5.12476945072128,-16.157490977702));
#79712=CARTESIAN_POINT('Ctrl Pts',(2.16971119591914,8.45853729058758,-15.9458059097933));
#79713=CARTESIAN_POINT('Ctrl Pts',(-3.21116090047537,7.5813672209176,-15.7341208418846));
#79714=CARTESIAN_POINT('Ctrl Pts',(-7.56602061402016,4.34579128259928,-15.5224357739759));
#79715=CARTESIAN_POINT('Ctrl Pts',(-8.88050289184019,-2.984559433186,-15.2578294390901));
#79716=CARTESIAN_POINT('Ctrl Pts',(-2.27872950387278,-9.08010219430069,
-14.940301837227));
#79717=CARTESIAN_POINT('Ctrl Pts',(4.91245411866735,-7.21116839348148,-14.6756955023412));
#79718=CARTESIAN_POINT('Ctrl Pts',(7.81914539187849,-2.60497844355453,-14.4640104344325));
#79719=CARTESIAN_POINT('Ctrl Pts',(8.13052289929572,1.45271515434484,-14.305246633501));
#79720=CARTESIAN_POINT('Ctrl Pts',(6.43851816967762,5.14493461231858,-14.1464828325695));
#79721=CARTESIAN_POINT('Ctrl Pts',(2.10754646363905,8.47199733575168,-13.9347977646608));
#79722=CARTESIAN_POINT('Ctrl Pts',(-3.78659489079374,7.86868469967962,-13.7231126967521));
#79723=CARTESIAN_POINT('Ctrl Pts',(-7.33863206363579,3.7327151916162,-13.5114276288434));
#79724=CARTESIAN_POINT('Ctrl Pts',(-8.58704922933571,-1.54698265557786,
-13.2997425609347));
#79725=CARTESIAN_POINT('Ctrl Pts',(-4.87258745156184,-8.00180093160806,
-13.0351362260488));
#79726=CARTESIAN_POINT('Ctrl Pts',(4.10342411775835,-8.41443845545048,-12.7176086241858));
#79727=CARTESIAN_POINT('Ctrl Pts',(8.40190016589835,-2.35398145052911,-12.4530022892999));
#79728=CARTESIAN_POINT('Ctrl Pts',(7.65976821207041,3.04185770345587,-12.2413172213913));
#79729=CARTESIAN_POINT('Ctrl Pts',(5.28516915482317,6.34687095666369,-12.0825534204597));
#79730=CARTESIAN_POINT('Ctrl Pts',(1.6131336309578,8.08224401233811,-11.9237896195282));
#79731=CARTESIAN_POINT('Ctrl Pts',(-3.84282385859219,7.8389537404691,-11.7121045516196));
#79732=CARTESIAN_POINT('Ctrl Pts',(-7.9639018756391,3.58200595827936,-11.5004194837108));
#79733=CARTESIAN_POINT('Ctrl Pts',(-8.01830375876113,-1.86962244835244,
-11.2887344158021));
#79734=CARTESIAN_POINT('Ctrl Pts',(-5.57375325824777,-6.71296092792641,
-11.0770493478935));
#79735=CARTESIAN_POINT('Ctrl Pts',(1.42454269218899,-9.25967627621681,-10.8124430130076));
#79736=CARTESIAN_POINT('Ctrl Pts',(8.55772751231042,-3.79554526198939,-10.4949154111446));
#79737=CARTESIAN_POINT('Ctrl Pts',(7.94400743510141,3.60914130205669,-10.2303090762587));
#79738=CARTESIAN_POINT('Ctrl Pts',(3.90171698267865,7.2595834548406,-10.01862400835));
#79739=CARTESIAN_POINT('Ctrl Pts',(-0.0432363685727964,8.25917154150874,
-9.85986020741853));
#79740=CARTESIAN_POINT('Ctrl Pts',(-3.97012529449484,7.22239389207724,-9.701096406487));
#79741=CARTESIAN_POINT('Ctrl Pts',(-7.98777786610472,3.5230520454781,-9.48941133857833));
#79742=CARTESIAN_POINT('Ctrl Pts',(-8.39964825188414,-2.38755293440294,
-9.27772627066964));
#79743=CARTESIAN_POINT('Ctrl Pts',(-4.93085602423302,-6.59358340626946,
-9.06604120276094));
#79744=CARTESIAN_POINT('Ctrl Pts',(0.0581756340859371,-8.72508942070459,
-8.85435613485225));
#79745=CARTESIAN_POINT('Ctrl Pts',(7.05240130226248,-6.16721675426193,-8.58974979996641));
#79746=CARTESIAN_POINT('Ctrl Pts',(8.99148210312331,2.60655205203753,-8.27222219810335));
#79747=CARTESIAN_POINT('Ctrl Pts',(3.75390080240723,7.87663531165635,-8.00761586321752));
#79748=CARTESIAN_POINT('Ctrl Pts',(-1.68941943488566,8.06664796081758,-7.7959307953088));
#79749=CARTESIAN_POINT('Ctrl Pts',(-5.35132879720302,6.29118939786795,-7.63716699437731));
#79750=CARTESIAN_POINT('Ctrl Pts',(-7.68815978033691,2.96935474106919,-7.47840319344575));
#79751=CARTESIAN_POINT('Ctrl Pts',(-8.37995396641292,-2.44803236789822,
-7.26671812553711));
#79752=CARTESIAN_POINT('Ctrl Pts',(-4.88911383309103,-7.23540363053417,
-7.05503305762839));
#79753=CARTESIAN_POINT('Ctrl Pts',(0.473181863587134,-8.21977993570431,
-6.84334798971971));
#79754=CARTESIAN_POINT('Ctrl Pts',(5.66277274055247,-6.63803997368177,-6.63166292181101));
#79755=CARTESIAN_POINT('Ctrl Pts',(9.36693595117432,-0.177306255126965,
-6.36705658692516));
#79756=CARTESIAN_POINT('Ctrl Pts',(5.20090347451901,7.7840520978901,-6.04952898506212));
#79757=CARTESIAN_POINT('Ctrl Pts',(-2.1998447589334,8.44356785368252,-5.78492265017626));
#79758=CARTESIAN_POINT('Ctrl Pts',(-6.48684125011734,5.08388020592419,-5.57323758226758));
#79759=CARTESIAN_POINT('Ctrl Pts',(-8.14528665446643,1.36751206783572,-5.41447378133604));
#79760=CARTESIAN_POINT('Ctrl Pts',(-7.79418143112824,-2.67873182434494,
-5.25570998040454));
#79761=CARTESIAN_POINT('Ctrl Pts',(-4.83510194401677,-7.26899444274413,
-5.04402491249584));
#79762=CARTESIAN_POINT('Ctrl Pts',(0.918399634047416,-8.68395311899561,
-4.83233984458715));
#79763=CARTESIAN_POINT('Ctrl Pts',(5.6549118079481,-5.9842005118547,-4.62065477667849));
#79764=CARTESIAN_POINT('Ctrl Pts',(8.60691424489449,-1.43233971771471,-4.40896970876977));
#79765=CARTESIAN_POINT('Ctrl Pts',(7.28074351218162,5.89590534512943,-4.14436337388392));
#79766=CARTESIAN_POINT('Ctrl Pts',(-1.03313762282123,9.30448772696622,-3.82683577202088));
#79767=CARTESIAN_POINT('Ctrl Pts',(-7.12007029059323,5.04358539856761,-3.56222943713502));
#79768=CARTESIAN_POINT('Ctrl Pts',(-8.23664763540929,-0.287370601108435,
-3.35054436922633));
#79769=CARTESIAN_POINT('Ctrl Pts',(-7.1124667608933,-4.19864329744608,-3.19178056829482));
#79770=CARTESIAN_POINT('Ctrl Pts',(-4.23837940774058,-7.06830933872544,
-3.0330167673633));
#79771=CARTESIAN_POINT('Ctrl Pts',(0.981352895278001,-8.67487531489779,
-2.8213316994546));
#79772=CARTESIAN_POINT('Ctrl Pts',(6.29443638452256,-6.05264830836724,-2.60964663154593));
#79773=CARTESIAN_POINT('Ctrl Pts',(8.17987790832939,-0.937157174411471,
-2.39796156363723));
#79774=CARTESIAN_POINT('Ctrl Pts',(7.50740159707945,4.44630291769865,-2.18627649572855));
#79775=CARTESIAN_POINT('Ctrl Pts',(1.77394145444216,9.19911577626299,-1.92167016084267));
#79776=CARTESIAN_POINT('Ctrl Pts',(-6.78178271222209,6.45356424815529,-1.60414255897965));
#79777=CARTESIAN_POINT('Ctrl Pts',(-8.69520103819224,-0.725998020850346,
-1.33953622409378));
#79778=CARTESIAN_POINT('Ctrl Pts',(-6.11672416772516,-5.52354273279491,
-1.1278511561851));
#79779=CARTESIAN_POINT('Ctrl Pts',(-2.73816693432726,-7.79236061590932,
-0.969087355253568));
#79780=CARTESIAN_POINT('Ctrl Pts',(1.30879556680406,-8.13681396711638,-0.81032355432205));
#79781=CARTESIAN_POINT('Ctrl Pts',(6.33648257904002,-6.00579725335872,-0.598638486413376));
#79782=CARTESIAN_POINT('Ctrl Pts',(8.71377174908705,-0.576514988363227,
-0.386953418504678));
#79783=CARTESIAN_POINT('Ctrl Pts',(6.86120775183791,4.54876981752662,-0.175268350595999));
#79784=CARTESIAN_POINT('Ctrl Pts',(2.88221401723271,8.23929217159093,0.0364167173126955));
#79785=CARTESIAN_POINT('Ctrl Pts',(-4.56924755978218,8.17348969005498,0.301023052198559));
#79786=CARTESIAN_POINT('Ctrl Pts',(-9.33928858972985,0.5826915139453,0.618550654061595));
#79787=CARTESIAN_POINT('Ctrl Pts',(-5.56239871442755,-7.52472998215995,
0.936078255924624));
#79788=CARTESIAN_POINT('Ctrl Pts',(3.31770137076159,-8.75652982581897,1.25360585778766));
#79789=CARTESIAN_POINT('Ctrl Pts',(8.16202073879245,-3.0942706070242,1.51821219267352));
#79790=CARTESIAN_POINT('Ctrl Pts',(7.89658816915579,2.32623600553997,1.72989726058221));
#79791=CARTESIAN_POINT('Ctrl Pts',(5.16469719276892,7.04188117863399,1.9415823284909));
#79792=CARTESIAN_POINT('Ctrl Pts',(-0.521226007064963,8.71486864918164,
2.1532673963996));
#79793=CARTESIAN_POINT('Ctrl Pts',(-5.38725527740725,6.23683958004327,2.36495246430828));
#79794=CARTESIAN_POINT('Ctrl Pts',(-7.72719108742934,2.9170121746353,2.5237162652398));
#79795=CARTESIAN_POINT('Ctrl Pts',(-8.16387417419938,-1.12915779804422,
2.68248006617132));
#79796=CARTESIAN_POINT('Ctrl Pts',(-6.14991068781707,-6.18968438231958,
2.89416513408));
#79797=CARTESIAN_POINT('Ctrl Pts',(0.57753512490799,-9.34384939092878,3.15877146896587));
#79798=CARTESIAN_POINT('Ctrl Pts',(8.18381619041701,-4.56023594897756,3.47629907082889));
#79799=CARTESIAN_POINT('Ctrl Pts',(8.23387562737699,2.88686344128947,3.74090540571477));
#79800=CARTESIAN_POINT('Ctrl Pts',(4.54511755749296,6.86517097771756,3.95259047362344));
#79801=CARTESIAN_POINT('Ctrl Pts',(-0.584144307352823,8.71282137839226,
4.16427554153215));
#79802=CARTESIAN_POINT('Ctrl Pts',(-6.00983956524825,6.33232529439785,4.37596060944082));
#79803=CARTESIAN_POINT('Ctrl Pts',(-8.13805209380252,1.30267610342289,4.58764567734951));
#79804=CARTESIAN_POINT('Ctrl Pts',(-7.7901918458369,-2.74384765777136,4.74640947828103));
#79805=CARTESIAN_POINT('Ctrl Pts',(-5.51909885455878,-6.12082461486054,
4.90517327921254));
#79806=CARTESIAN_POINT('Ctrl Pts',(-0.71953763145969,-8.69571274896694,
5.11685834712126));
#79807=CARTESIAN_POINT('Ctrl Pts',(6.45853407846523,-6.77703495389075,5.38146468200709));
#79808=CARTESIAN_POINT('Ctrl Pts',(9.19782165965666,1.78073093027871,5.69899228387014));
#79809=CARTESIAN_POINT('Ctrl Pts',(4.44075853215298,7.51067463980576,5.963598618756));
#79810=CARTESIAN_POINT('Ctrl Pts',(-0.943184956415734,8.17918611230628,
6.1752836866647));
#79811=CARTESIAN_POINT('Ctrl Pts',(-6.05729059692325,6.28997061083414,6.38696875457337));
#79812=CARTESIAN_POINT('Ctrl Pts',(-8.67559507725891,0.974956959624878,
6.59865382248207));
#79813=CARTESIAN_POINT('Ctrl Pts',(-7.06518294672293,-4.24359026031473,
6.81033889039075));
#79814=CARTESIAN_POINT('Ctrl Pts',(-4.19339752672706,-7.11556049246613,
6.96910269132226));
#79815=CARTESIAN_POINT('Ctrl Pts',(-0.281297496662247,-8.23685735403881,
7.12786649225378));
#79816=CARTESIAN_POINT('Ctrl Pts',(5.04883403253763,-7.11634948376184,7.33955156016249));
#79817=CARTESIAN_POINT('Ctrl Pts',(9.30524690078142,-1.02627682884742,7.60415789504834));
#79818=CARTESIAN_POINT('Ctrl Pts',(5.89053541961087,7.28508881838927,7.92168549691137));
#79819=CARTESIAN_POINT('Ctrl Pts',(-1.43868554204972,8.60585578048106,8.18629183179724));
#79820=CARTESIAN_POINT('Ctrl Pts',(-5.98836845278024,5.65049790205964,8.39797689970593));
#79821=CARTESIAN_POINT('Ctrl Pts',(-8.68462793494931,0.911996382211341,
8.60966196761461));
#79822=CARTESIAN_POINT('Ctrl Pts',(-7.26542736414225,-4.84046032623451,
8.82134703552331));
#79823=CARTESIAN_POINT('Ctrl Pts',(-2.67298415987235,-7.79615444096457,
9.03303210343198));
#79824=CARTESIAN_POINT('Ctrl Pts',(1.37351751756126,-8.14427612280999,9.19179590436352));
#79825=CARTESIAN_POINT('Ctrl Pts',(5.08866181120061,-6.48309095431802,9.35055970529502));
#79826=CARTESIAN_POINT('Ctrl Pts',(8.44518758549035,-2.19361840642918,9.56224477320372));
#79827=CARTESIAN_POINT('Ctrl Pts',(7.7802151635707,5.20664152974954,9.82685110808959));
#79828=CARTESIAN_POINT('Ctrl Pts',(-0.184212794636262,9.36680267052184,
10.1443787099526));
#79829=CARTESIAN_POINT('Ctrl Pts',(-6.64221354075295,5.65787672919185,10.4089850448385));
#79830=CARTESIAN_POINT('Ctrl Pts',(-8.2201265957422,0.467120987666701,10.6206701127472));
#79831=CARTESIAN_POINT('Ctrl Pts',(-7.23179673954533,-4.89444743437479,
10.8323551806559));
#79832=CARTESIAN_POINT('Ctrl Pts',(-2.44185285290457,-8.38175671313248,
11.0440402485646));
#79833=CARTESIAN_POINT('Ctrl Pts',(2.97502269802595,-7.68596827553516,11.2557253164733));
#79834=CARTESIAN_POINT('Ctrl Pts',(6.29513342006344,-5.34668861625921,11.4144891174048));
#79835=CARTESIAN_POINT('Ctrl Pts',(8.06789143937566,-1.68347113820463,11.5732529183363));
#79836=CARTESIAN_POINT('Ctrl Pts',(7.87386528083567,3.75970751607194,11.784937986245));
#79837=CARTESIAN_POINT('Ctrl Pts',(2.59992159168183,8.99340156602993,12.0495443211308));
#79838=CARTESIAN_POINT('Ctrl Pts',(-6.1724150737335,7.04785206852052,12.3670719229939));
#79839=CARTESIAN_POINT('Ctrl Pts',(-8.72512994398167,0.0517422876257268,
12.6316782578797));
#79840=CARTESIAN_POINT('Ctrl Pts',(-6.58994591167402,-4.93571637640952,
12.8433633257884));
#79841=CARTESIAN_POINT('Ctrl Pts',(-2.38135891453366,-8.40140639953382,
13.0550483936971));
#79842=CARTESIAN_POINT('Ctrl Pts',(3.52894077140471,-7.98517801838488,13.2667334616058));
#79843=CARTESIAN_POINT('Ctrl Pts',(7.22531924878866,-3.9647988775456,13.4784185295145));
#79844=CARTESIAN_POINT('Ctrl Pts',(8.25920117616535,-0.0371465646322164,
13.637182330446));
#79845=CARTESIAN_POINT('Ctrl Pts',(7.25670460142574,3.90706868104012,13.7959461313775));
#79846=CARTESIAN_POINT('Ctrl Pts',(3.60328291092042,7.94666642882579,14.0076311992862));
#79847=CARTESIAN_POINT('Ctrl Pts',(-3.80185415876567,8.55492659034786,14.2722375341721));
#79848=CARTESIAN_POINT('Ctrl Pts',(-9.26072412706714,1.41771480367452,14.5897651360351));
#79849=CARTESIAN_POINT('Ctrl Pts',(-6.70884936900753,-5.57870145711901,
14.854371470921));
#79850=CARTESIAN_POINT('Ctrl Pts',(-1.86370974865146,-8.01968012079831,
15.0660565388297));
#79851=CARTESIAN_POINT('Ctrl Pts',(3.58787706353087,-7.96125856551249,15.2777416067384));
#79852=CARTESIAN_POINT('Ctrl Pts',(7.8417850655293,-3.83704286390198,15.489426674647));
#79853=CARTESIAN_POINT('Ctrl Pts',(8.08105239231934,1.61909252944133,15.7011117425558));
#79854=CARTESIAN_POINT('Ctrl Pts',(6.34297228097692,5.28984750048557,15.8598755434872));
#79855=CARTESIAN_POINT('Ctrl Pts',(3.03620904660201,7.66200900391343,16.0186393444188));
#79856=CARTESIAN_POINT('Ctrl Pts',(-2.36017584191269,8.40016220452973,16.2303244123274));
#79857=CARTESIAN_POINT('Ctrl Pts',(-8.41746177427002,4.09721872609548,16.4949307472134));
#79858=CARTESIAN_POINT('Ctrl Pts',(-7.99820601778327,-4.87848615036436,
16.8124583490763));
#79859=CARTESIAN_POINT('Ctrl Pts',(-1.54065068654177,-8.58818754253497,
17.0770646839623));
#79860=CARTESIAN_POINT('Ctrl Pts',(3.73812522137653,-7.33587779999464,17.2887497518709));
#79861=CARTESIAN_POINT('Ctrl Pts',(7.87147455696352,-3.78079198965415,17.5004348197796));
#79862=CARTESIAN_POINT('Ctrl Pts',(8.47044106094497,2.11379260724371,17.7121198876883));
#79863=CARTESIAN_POINT('Ctrl Pts',(5.14018585653609,6.44230996976773,17.923804955597));
#79864=CARTESIAN_POINT('Ctrl Pts',(1.44671982465644,8.13159182968389,18.0825687565285));
#79865=CARTESIAN_POINT('Ctrl Pts',(-2.61074308009303,7.81722251956952,18.24133255746));
#79866=CARTESIAN_POINT('Ctrl Pts',(-7.21478856708646,4.9071357225367,18.4530176253687));
#79867=CARTESIAN_POINT('Ctrl Pts',(-9.07841953461377,-2.28542397911376,
18.7176239602546));
#79868=CARTESIAN_POINT('Ctrl Pts',(-2.97801069914672,-8.88270110371666,
19.0351515621176));
#79869=CARTESIAN_POINT('Ctrl Pts',(4.35136880768079,-7.56281424492468,19.2997578970034));
#79870=CARTESIAN_POINT('Ctrl Pts',(7.58373286757206,-3.20557000554551,19.5114429649122));
#79871=CARTESIAN_POINT('Ctrl Pts',(8.45693518308693,2.17594739803703,19.7231280328208));
#79872=CARTESIAN_POINT('Ctrl Pts',(5.11955673730547,7.07153659163915,19.9348131007296));
#79873=CARTESIAN_POINT('Ctrl Pts',(-0.215617128995803,8.23883351209298,
20.1464981686382));
#79874=CARTESIAN_POINT('Ctrl Pts',(-4.12922331496766,7.15299229349241,20.3052619695698));
#79875=CARTESIAN_POINT('Ctrl Pts',(-7.0311289305844,4.29978758919758,20.4640257705013));
#79876=CARTESIAN_POINT('Ctrl Pts',(-8.6797853573168,-0.8913367590688,20.67571083841));
#79877=CARTESIAN_POINT('Ctrl Pts',(-5.47419956556276,-7.5943402035435,20.9403171732958));
#79878=CARTESIAN_POINT('Ctrl Pts',(3.44129873439396,-8.71368978348783,21.2578447751588));
#79879=CARTESIAN_POINT('Ctrl Pts',(8.19904993880632,-2.98431732640053,21.5224511100447));
#79880=CARTESIAN_POINT('Ctrl Pts',(7.8663890100263,2.43076268074111,21.7341361779534));
#79881=CARTESIAN_POINT('Ctrl Pts',(5.06920075424374,7.11039404555973,21.9458212458621));
#79882=CARTESIAN_POINT('Ctrl Pts',(-0.636572166304518,8.70696656881521,
22.1575063137708));
#79883=CARTESIAN_POINT('Ctrl Pts',(-5.47011995174442,6.16462943734903,22.3691913816794));
#79884=CARTESIAN_POINT('Ctrl Pts',(-7.76519537751747,2.8138096390156,22.527955182611));
#79885=CARTESIAN_POINT('Ctrl Pts',(-8.14818489938332,-1.23775207379351,
22.6867189835425));
#79886=CARTESIAN_POINT('Ctrl Pts',(-6.06688873660663,-6.27104585573993,
22.8984040514512));
#79887=CARTESIAN_POINT('Ctrl Pts',(0.701881505993874,-9.33532143861735,
23.163010386337));
#79888=CARTESIAN_POINT('Ctrl Pts',(8.24383438190629,-4.45085624412889,23.4805379882001));
#79889=CARTESIAN_POINT('Ctrl Pts',(8.19469437259043,2.99625665514973,23.7451443230859));
#79890=CARTESIAN_POINT('Ctrl Pts',(4.45329755143643,6.92508658325054,23.9568293909947));
#79891=CARTESIAN_POINT('Ctrl Pts',(-0.700120258078465,8.70427087091072,
24.1685144589033));
#79892=CARTESIAN_POINT('Ctrl Pts',(-6.09362991369378,6.25173299400388,24.3801995268121));
#79893=CARTESIAN_POINT('Ctrl Pts',(-8.15467833577869,1.19418994564688,24.5918845947207));
#79894=CARTESIAN_POINT('Ctrl Pts',(-7.75296212610164,-2.84734300829175,
24.7506483956523));
#79895=CARTESIAN_POINT('Ctrl Pts',(-5.43710132964985,-6.19377723863542,
24.9094121965837));
#79896=CARTESIAN_POINT('Ctrl Pts',(-0.60367674685806,-8.70452350519323,
25.1210972644925));
#79897=CARTESIAN_POINT('Ctrl Pts',(6.54820811350255,-6.69042857468967,25.3857035993782));
#79898=CARTESIAN_POINT('Ctrl Pts',(9.1732929286674,1.90305634889304,25.7032312012414));
#79899=CARTESIAN_POINT('Ctrl Pts',(4.34034841940176,7.56914429786426,25.9678375361272));
#79900=CARTESIAN_POINT('Ctrl Pts',(-1.05201992362399,8.16590089013109,26.1795226040359));
#79901=CARTESIAN_POINT('Ctrl Pts',(-6.14051426705278,6.208750623602,26.3912076719445));
#79902=CARTESIAN_POINT('Ctrl Pts',(-8.68780888576682,0.859341444230168,
26.6028927398533));
#79903=CARTESIAN_POINT('Ctrl Pts',(-7.00804646742056,-4.33729790270126,
26.8145778077619));
#79904=CARTESIAN_POINT('Ctrl Pts',(-4.09827092580945,-7.17077118267629,
26.9733416086935));
#79905=CARTESIAN_POINT('Ctrl Pts',(-0.171585965343747,-8.23987291207912,
27.132105409625));
#79906=CARTESIAN_POINT('Ctrl Pts',(5.14315163742236,-7.04848539060961,27.3437904775337));
#79907=CARTESIAN_POINT('Ctrl Pts',(9.31808828596101,-0.902271968865942,
27.6083968124195));
#79908=CARTESIAN_POINT('Ctrl Pts',(5.79300080182397,7.3628845116753,27.9259244142826));
#79909=CARTESIAN_POINT('Ctrl Pts',(-1.55315835309708,8.58593436580423,28.1905307491684));
#79910=CARTESIAN_POINT('Ctrl Pts',(-6.06308265180774,5.57025242017754,28.4022158170771));
#79911=CARTESIAN_POINT('Ctrl Pts',(-8.69600252795008,0.796266163945025,
28.6139008849858));
#79912=CARTESIAN_POINT('Ctrl Pts',(-7.20032487283164,-4.93678161144116,
28.8255859528945));
#79913=CARTESIAN_POINT('Ctrl Pts',(-2.56892920494273,-7.83105811026166,
29.0372710208032));
#79914=CARTESIAN_POINT('Ctrl Pts',(1.48184945465475,-8.12526344984419,29.1960348217347));
#79915=CARTESIAN_POINT('Ctrl Pts',(5.17454306032357,-6.41475264274277,29.3547986226662));
#79916=CARTESIAN_POINT('Ctrl Pts',(8.47365020358878,-2.08096306896043,29.5664836905749));
#79917=CARTESIAN_POINT('Ctrl Pts',(7.71019075313911,5.30978554755018,29.8310900254608));
#79918=CARTESIAN_POINT('Ctrl Pts',(-0.308930032296374,9.36351904239792,
30.1486176273238));
#79919=CARTESIAN_POINT('Ctrl Pts',(-6.71696802439972,5.56892362695756,30.4132239622097));
#79920=CARTESIAN_POINT('Ctrl Pts',(-8.22561816670618,0.357615775237553,
30.6249090301183));
#79921=CARTESIAN_POINT('Ctrl Pts',(-7.16597830778628,-4.99031608841498,
30.8365940980271));
#79922=CARTESIAN_POINT('Ctrl Pts',(-2.33002018555819,-8.41353058402189,
31.0482791659357));
#79923=CARTESIAN_POINT('Ctrl Pts',(3.07710954772786,-7.64566970366785,31.2599642338444));
#79924=CARTESIAN_POINT('Ctrl Pts',(6.36577472448202,-5.26238501943575,31.4187280347759));
#79925=CARTESIAN_POINT('Ctrl Pts',(8.08959410633424,-1.57588532117043,31.5774918357075));
#79926=CARTESIAN_POINT('Ctrl Pts',(7.82310074732932,3.86422692970949,31.7891769036162));
#79927=CARTESIAN_POINT('Ctrl Pts',(2.47992990429178,9.02722613434294,32.053783238502));
#79928=CARTESIAN_POINT('Ctrl Pts',(-6.2657209013968,6.96503181672575,32.371310840365));
#79929=CARTESIAN_POINT('Ctrl Pts',(-8.72504532207758,-0.0644509998803956,
32.6359171752509));
#79930=CARTESIAN_POINT('Ctrl Pts',(-6.52363483210948,-5.02303412734111,
32.8476022431596));
#79931=CARTESIAN_POINT('Ctrl Pts',(-2.26926994495205,-8.43237295705634,
33.0592873110683));
#79932=CARTESIAN_POINT('Ctrl Pts',(3.63496294949945,-7.93747663361272,33.270972378977));
#79933=CARTESIAN_POINT('Ctrl Pts',(7.27747605933994,-3.86823093830196,33.4826574468857));
#79934=CARTESIAN_POINT('Ctrl Pts',(8.25896350304176,0.072840861189232,33.6414212478171));
#79935=CARTESIAN_POINT('Ctrl Pts',(7.20403244760854,4.00335657224304,33.8001850487487));
#79936=CARTESIAN_POINT('Ctrl Pts',(3.49714116543082,7.99394512967198,34.0118701166574));
#79937=CARTESIAN_POINT('Ctrl Pts',(-3.9154392277668,8.50354041940355,34.2764764515432));
#79938=CARTESIAN_POINT('Ctrl Pts',(-9.27878206673691,1.29426812531432,34.5940040534063));
#79939=CARTESIAN_POINT('Ctrl Pts',(-6.63396539819317,-5.66754557981407,
34.8586103882921));
#79940=CARTESIAN_POINT('Ctrl Pts',(-1.75674995881094,-8.04378722054254,
35.0702954562009));
#79941=CARTESIAN_POINT('Ctrl Pts',(3.69357549100292,-7.91277447310475,35.2819805241094));
#79942=CARTESIAN_POINT('Ctrl Pts',(7.89218594411954,-3.73227704984803,35.4936655920182));
#79943=CARTESIAN_POINT('Ctrl Pts',(8.05877511145054,1.72656076909226,35.7053506599269));
#79944=CARTESIAN_POINT('Ctrl Pts',(6.27196729271126,5.37384501216737,35.8641144608584));
#79945=CARTESIAN_POINT('Ctrl Pts',(2.93390824027782,7.70176147308837,36.0228782617899));
#79946=CARTESIAN_POINT('Ctrl Pts',(-2.47182781457673,8.36798794945601,36.2345633296987));
#79947=CARTESIAN_POINT('Ctrl Pts',(-8.47127625499191,3.9847638101116,36.4991696645844));
#79948=CARTESIAN_POINT('Ctrl Pts',(-7.93253217842265,-4.98456215333826,
36.8166972664475));
#79949=CARTESIAN_POINT('Ctrl Pts',(-1.42614898002516,-8.60794219836928,
37.0813036013334));
#79950=CARTESIAN_POINT('Ctrl Pts',(3.83548240717228,-7.28544837133703,37.2929886692421));
#79951=CARTESIAN_POINT('Ctrl Pts',(7.92112373497429,-3.67563580148848,37.5046737371507));
#79952=CARTESIAN_POINT('Ctrl Pts',(8.44154155094658,2.22640229900672,37.7163588050595));
#79953=CARTESIAN_POINT('Ctrl Pts',(5.05394068509545,6.51018831815488,37.9280438729681));
#79954=CARTESIAN_POINT('Ctrl Pts',(1.33830673024671,8.15013613575943,38.0868076738997));
#79955=CARTESIAN_POINT('Ctrl Pts',(-2.71461008497256,7.78176326016691,38.2455714748312));
#79956=CARTESIAN_POINT('Ctrl Pts',(-7.27949499470204,4.81062445938832,38.4572565427398));
#79957=CARTESIAN_POINT('Ctrl Pts',(-9.04718057646558,-2.40611463309362,
38.7218628776258));
#79958=CARTESIAN_POINT('Ctrl Pts',(-2.85945963599839,-8.9215703333157,39.0393904794887));
#79959=CARTESIAN_POINT('Ctrl Pts',(4.45169362994984,-7.5041984001464,39.3039968143747));
#79960=CARTESIAN_POINT('Ctrl Pts',(7.6257475824808,-3.10429655082013,39.5156818822832));
#79961=CARTESIAN_POINT('Ctrl Pts',(8.42720918276421,2.28837172677223,39.7273669501921));
#79962=CARTESIAN_POINT('Ctrl Pts',(5.02493426218586,7.13908443808384,39.9390520181006));
#79963=CARTESIAN_POINT('Ctrl Pts',(-0.325310915258221,8.23523170255197,
40.1507370860094));
#79964=CARTESIAN_POINT('Ctrl Pts',(-4.22411041690589,7.09737100068912,40.3095008869408));
#79965=CARTESIAN_POINT('Ctrl Pts',(-7.08776385648449,4.20577589339118,40.4682646878724));
#79966=CARTESIAN_POINT('Ctrl Pts',(-8.66714618919647,-1.00684259060368,
40.6799497557811));
#79967=CARTESIAN_POINT('Ctrl Pts',(-5.37258369985886,-7.66656431517888,
40.944556090667));
#79968=CARTESIAN_POINT('Ctrl Pts',(3.55702995286921,-8.66709089236948,41.2620836925299));
#79969=CARTESIAN_POINT('Ctrl Pts',(8.23806376983713,-2.87486958448408,41.5266900274159));
#79970=CARTESIAN_POINT('Ctrl Pts',(7.83332211050503,2.53530037278001,41.7383750953245));
#79971=CARTESIAN_POINT('Ctrl Pts',(4.9740652966121,7.17726787816896,41.9500601632332));
#79972=CARTESIAN_POINT('Ctrl Pts',(-0.752462547816077,8.69771757804969,
42.1617452311419));
#79973=CARTESIAN_POINT('Ctrl Pts',(-5.55172656596247,6.09123965405151,42.3734302990506));
#79974=CARTESIAN_POINT('Ctrl Pts',(-7.80197710260423,2.71015446535334,42.5321940999822));
#79975=CARTESIAN_POINT('Ctrl Pts',(-8.1309798082442,-1.34614810056075,42.6909579009136));
#79976=CARTESIAN_POINT('Ctrl Pts',(-5.98284204359866,-6.35127988270911,
42.9026429688224));
#79977=CARTESIAN_POINT('Ctrl Pts',(0.826133620683909,-9.3251470364568,43.1672493037082));
#79978=CARTESIAN_POINT('Ctrl Pts',(8.30237349258994,-4.34068209061006,43.4847769055712));
#79979=CARTESIAN_POINT('Ctrl Pts',(8.15406792911807,3.10511610266412,43.7493832404571));
#79980=CARTESIAN_POINT('Ctrl Pts',(4.36068436308684,6.98377513617638,43.9610683083658));
#79981=CARTESIAN_POINT('Ctrl Pts',(-0.815969107408102,8.69417587731647,
44.1727533762745));
#79982=CARTESIAN_POINT('Ctrl Pts',(-6.17634116129579,6.17003248068141,44.3844384441832));
#79983=CARTESIAN_POINT('Ctrl Pts',(-8.16985776599225,1.08549181008368,44.5961235120918));
#79984=CARTESIAN_POINT('Ctrl Pts',(-7.71435786793978,-2.95033330676227,
44.7548873130234));
#79985=CARTESIAN_POINT('Ctrl Pts',(-5.35413943147089,-6.26563151638265,
44.9136511139549));
#79986=CARTESIAN_POINT('Ctrl Pts',(-0.487708926553712,-8.71179057772378,
45.1253361818636));
#79987=CARTESIAN_POINT('Ctrl Pts',(6.63672096915272,-6.60263574554677,45.3899425167495));
#79988=CARTESIAN_POINT('Ctrl Pts',(9.14713737891418,2.0250442942005,45.7074701186125));
#79989=CARTESIAN_POINT('Ctrl Pts',(4.23916861421562,7.62627164897394,45.9720764534983));
#79990=CARTESIAN_POINT('Ctrl Pts',(-1.16066833514873,8.15116754109057,46.183761521407));
#79991=CARTESIAN_POINT('Ctrl Pts',(-6.2226489802212,6.12642958328167,46.3954465893157));
#79992=CARTESIAN_POINT('Ctrl Pts',(-8.69848201415944,0.743573535518887,
46.6071316572243));
#79993=CARTESIAN_POINT('Ctrl Pts',(-6.94966718953088,-4.43023637530331,
46.8188167251331));
#79994=CARTESIAN_POINT('Ctrl Pts',(-4.00241754418439,-7.22471021824686,
46.9775805260645));
#79995=CARTESIAN_POINT('Ctrl Pts',(-0.0618440048273914,-8.24142722286535,
47.1363443269962));
#79996=CARTESIAN_POINT('Ctrl Pts',(5.23655716281452,-6.97937132897605,47.3480293949047));
#79997=CARTESIAN_POINT('Ctrl Pts',(9.32927721475058,-0.778107101303471,
47.6126357297907));
#79998=CARTESIAN_POINT('Ctrl Pts',(5.69443886140186,7.43937448149761,47.9301633316538));
#79999=CARTESIAN_POINT('Ctrl Pts',(-1.66735572920219,8.56449033369709,48.1947696665395));
#80000=CARTESIAN_POINT('Ctrl Pts',(-6.13672163238016,5.48901911764058,48.4064547344483));
#80001=CARTESIAN_POINT('Ctrl Pts',(-8.70583498418567,0.68039473696197,48.6181398023569));
#80002=CARTESIAN_POINT('Ctrl Pts',(-7.13394548613349,-5.03222741479912,
48.8298248702656));
#80003=CARTESIAN_POINT('Ctrl Pts',(-2.46441867975,-7.8645730308264,49.0415099381744));
#80004=CARTESIAN_POINT('Ctrl Pts',(1.58991860266646,-8.10480985418721,49.2002737391058));
#80005=CARTESIAN_POINT('Ctrl Pts',(5.25950666332379,-6.34527674803642,49.3590375400374));
#80006=CARTESIAN_POINT('Ctrl Pts',(8.5006101165834,-1.96793869645312,49.570722607946));
#80007=CARTESIAN_POINT('Ctrl Pts',(7.63879902841993,5.4119879355161,49.835328942832));
#80008=CARTESIAN_POINT('Ctrl Pts',(-0.433592484742793,9.35857490109356,
50.1528565446949));
#80009=CARTESIAN_POINT('Ctrl Pts',(-6.79053133046797,5.47898293970952,50.4174628795808));
#80010=CARTESIAN_POINT('Ctrl Pts',(-8.22965101821615,0.248047143734746,
50.6291479474895));
#80011=CARTESIAN_POINT('Ctrl Pts',(-7.09888907160326,-5.08529976688182,
50.8408330153982));
#80012=CARTESIAN_POINT('Ctrl Pts',(-2.21777431573672,-8.44381241133431,
51.0525180833069));
#80013=CARTESIAN_POINT('Ctrl Pts',(3.17865070718642,-7.60401525958635,51.2642031512156));
#80014=CARTESIAN_POINT('Ctrl Pts',(6.43528713144793,-5.1771481987163,51.422966952147));
#80015=CARTESIAN_POINT('Ctrl Pts',(8.10986217614476,-1.46802003887728,51.5817307530786));
#80016=CARTESIAN_POINT('Ctrl Pts',(7.77094887625473,3.96806106684268,51.7934158209873));
#80017=CARTESIAN_POINT('Ctrl Pts',(2.35949842961515,9.05944982714925,52.0580221558731));
#80018=CARTESIAN_POINT('Ctrl Pts',(-6.35791557494276,6.88097639612989,52.3755497577362));
#80019=CARTESIAN_POINT('Ctrl Pts',(-8.72341341312283,-0.180632857834922,
52.640156092622));
#80020=CARTESIAN_POINT('Ctrl Pts',(-6.45616686025931,-5.10946110039852,
52.8518411605307));
#80021=CARTESIAN_POINT('Ctrl Pts',(-2.15677854662195,-8.46184412985793,
53.0635262284394));
#80022=CARTESIAN_POINT('Ctrl Pts',(3.74034050916199,-7.888367627318,53.2752112963481));
#80023=CARTESIAN_POINT('Ctrl Pts',(7.32834229169904,-3.77097701331254,53.4868963642568));
#80024=CARTESIAN_POINT('Ctrl Pts',(8.25726119895179,0.182815371261993,53.6456601651883));
#80025=CARTESIAN_POINT('Ctrl Pts',(7.15008273743028,4.09893451068573,53.8044239661198));
#80026=CARTESIAN_POINT('Ctrl Pts',(3.39037924938521,8.0398062025158,54.0161090340285));
#80027=CARTESIAN_POINT('Ctrl Pts',(-4.02832995383727,8.45064622842747,54.2807153689144));
#80028=CARTESIAN_POINT('Ctrl Pts',(-9.29519449327465,1.17059194815611,54.5982429707774));
#80029=CARTESIAN_POINT('Ctrl Pts',(-6.55790501479776,-5.75538466973715,
54.8628493056633));
#80030=CARTESIAN_POINT('Ctrl Pts',(-1.64947856894098,-8.06646779092916,
55.074534373572));
#80031=CARTESIAN_POINT('Ctrl Pts',(3.79861874928655,-7.86288728353405,55.2862194414806));
#80032=CARTESIAN_POINT('Ctrl Pts',(7.94118755034809,-3.62684906824275,55.4979045093893));
#80033=CARTESIAN_POINT('Ctrl Pts',(8.03506830749714,1.83372246351997,55.709589577298));
#80034=CARTESIAN_POINT('Ctrl Pts',(6.19985085699822,5.45689028163728,55.8683533782295));
#80035=CARTESIAN_POINT('Ctrl Pts',(2.83108565350718,7.74014675877405,56.0271171791611));
#80036=CARTESIAN_POINT('Ctrl Pts',(-2.58303822757656,8.33433267444918,56.2388022470697));
#80037=CARTESIAN_POINT('Ctrl Pts',(-8.52359509037462,3.8715961450888,56.5034085819557));
#80038=CARTESIAN_POINT('Ctrl Pts',(-7.86543999841054,-5.08974355141217,
56.8209361838186));
#80039=CARTESIAN_POINT('Ctrl Pts',(-1.31141381205942,-8.62618819555302,
57.0855425187045));
#80040=CARTESIAN_POINT('Ctrl Pts',(3.93218530965132,-7.2337031704381,57.2972275866132));
#80041=CARTESIAN_POINT('Ctrl Pts',(7.96930150902302,-3.56988901935955,57.5089126545219));
#80042=CARTESIAN_POINT('Ctrl Pts',(8.41128061848056,2.3387416807266,57.7205977224305));
#80043=CARTESIAN_POINT('Ctrl Pts',(4.96663170753987,6.57675829270832,57.9322827903394));
#80044=CARTESIAN_POINT('Ctrl Pts',(1.23000494800474,8.16755528504679,58.0910465912707));
#80045=CARTESIAN_POINT('Ctrl Pts',(-2.81863160931247,7.74433999573533,58.2498103922024));
#80046=CARTESIAN_POINT('Ctrl Pts',(-7.3415364539406,4.71452192664591,58.4614954601109));
#80047=CARTESIAN_POINT('Ctrl Pts',(-9.01718004225608,-2.52898934108735,
58.7261017949969));
#80048=CARTESIAN_POINT('Ctrl Pts',(-2.73543320839727,-8.95429455413672,
59.0436293968599));
#80049=CARTESIAN_POINT('Ctrl Pts',(4.54288040872128,-7.45192048792684,59.3082357317457));
#80050=CARTESIAN_POINT('Ctrl Pts',(7.67764277639221,-2.99214435473956,59.5199207996544));
#80051=CARTESIAN_POINT('Ctrl Pts',(8.19311435259575,1.03068185261496,59.678684600586));
#80052=CARTESIAN_POINT('Ctrl Pts',(6.69025189752799,4.83429374004656,59.8375130498614));
#80053=CARTESIAN_POINT('Ctrl Pts',(4.60790684111087,6.57207682948263,59.9434202321596));
#80054=CARTESIAN_POINT('Ctrl Pts',(3.41916591565856,7.14122334375564,59.9964061474807));
#80055=CARTESIAN_POINT('Ctrl Pts',(4.37098981058075,-6.1335693280065,-60.4415856688784));
#80056=CARTESIAN_POINT('Ctrl Pts',(5.39136601496843,-5.40642193064725,-60.3886321829441));
#80057=CARTESIAN_POINT('Ctrl Pts',(7.05859103065204,-3.43860440421756,-60.2827574300326));
#80058=CARTESIAN_POINT('Ctrl Pts',(7.8464956002649,0.370392094075909,-60.1239614101439));
#80059=CARTESIAN_POINT('Ctrl Pts',(6.70727280426418,4.05641232746857,-59.9651976092124));
#80060=CARTESIAN_POINT('Ctrl Pts',(3.04204627735459,7.72471705861125,-59.7535125413037));
#80061=CARTESIAN_POINT('Ctrl Pts',(-4.02405469353209,7.94559028961535,-59.4889062064178));
#80062=CARTESIAN_POINT('Ctrl Pts',(-8.86316855372843,0.89937772589701,-59.1713786045548));
#80063=CARTESIAN_POINT('Ctrl Pts',(-6.11135702485761,-5.6157628730622,-58.906772269669));
#80064=CARTESIAN_POINT('Ctrl Pts',(-1.3784275667397,-7.71753525273869,-58.6950872017603));
#80065=CARTESIAN_POINT('Ctrl Pts',(2.48488421585976,-7.45381729160668,-58.5363234008287));
#80066=CARTESIAN_POINT('Ctrl Pts',(5.7272963799356,-5.35350558506947,-58.3775595998972));
#80067=CARTESIAN_POINT('Ctrl Pts',(8.26430431855175,-0.819906288515342,
-58.1658745319886));
#80068=CARTESIAN_POINT('Ctrl Pts',(6.88637636880123,4.64543106244188,-57.9541894640798));
#80069=CARTESIAN_POINT('Ctrl Pts',(2.50530954563564,7.42060282805745,-57.7425043961712));
#80070=CARTESIAN_POINT('Ctrl Pts',(-2.63598306863222,7.87035890477309,-57.5308193282625));
#80071=CARTESIAN_POINT('Ctrl Pts',(-8.20145258310699,3.48710685812043,-57.2662129933766));
#80072=CARTESIAN_POINT('Ctrl Pts',(-7.35663752044499,-5.01859065699272,
-56.9486853915136));
#80073=CARTESIAN_POINT('Ctrl Pts',(-1.06140553829354,-8.23203608828134,
-56.6840790566278));
#80074=CARTESIAN_POINT('Ctrl Pts',(3.91566660751038,-6.7921191913466,-56.472393988719));
#80075=CARTESIAN_POINT('Ctrl Pts',(6.70038556434063,-4.10285058779559,-56.3136301877875));
#80076=CARTESIAN_POINT('Ctrl Pts',(7.82935707026716,-0.407975901695247,
-56.154866386856));
#80077=CARTESIAN_POINT('Ctrl Pts',(6.85073828888755,4.69422716676729,-55.9431813189473));
#80078=CARTESIAN_POINT('Ctrl Pts',(2.27751233819034,7.98847381449242,-55.7314962510387));
#80079=CARTESIAN_POINT('Ctrl Pts',(-2.86151704673791,7.2906631041924,-55.5198111831299));
#80080=CARTESIAN_POINT('Ctrl Pts',(-7.08463059670744,4.32419256030661,-55.3081261152213));
#80081=CARTESIAN_POINT('Ctrl Pts',(-8.52030387347526,-2.61312521513784,
-55.0435197803354));
#80082=CARTESIAN_POINT('Ctrl Pts',(-2.39692682072872,-8.57677385790295,
-54.7259921784723));
#80083=CARTESIAN_POINT('Ctrl Pts',(4.48869838858835,-6.98173025450676,-54.4613858435864));
#80084=CARTESIAN_POINT('Ctrl Pts',(7.36943309221841,-2.67522160566258,-54.2497007756778));
#80085=CARTESIAN_POINT('Ctrl Pts',(7.76832283941139,1.17545456122282,-54.0909369747463));
#80086=CARTESIAN_POINT('Ctrl Pts',(6.25288685299758,4.72934343760845,-53.9321731738148));
#80087=CARTESIAN_POINT('Ctrl Pts',(2.21873946141778,8.00284801499922,-53.720488105906));
#80088=CARTESIAN_POINT('Ctrl Pts',(-3.40143338883267,7.5784580409641,-53.5088030379974));
#80089=CARTESIAN_POINT('Ctrl Pts',(-6.88393194308128,3.73544245026433,-53.2971179700887));
#80090=CARTESIAN_POINT('Ctrl Pts',(-8.20483342319923,-1.25353081970317,
-53.08543290218));
#80091=CARTESIAN_POINT('Ctrl Pts',(-4.83617598709369,-7.48567990974514,
-52.8208265672942));
#80092=CARTESIAN_POINT('Ctrl Pts',(3.68888887765348,-8.10545538177222,-52.503298965431));
#80093=CARTESIAN_POINT('Ctrl Pts',(7.92994793033033,-2.4513050089426,-52.2386926305453));
#80094=CARTESIAN_POINT('Ctrl Pts',(7.36092771473285,2.69853626749654,-52.0270075626365));
#80095=CARTESIAN_POINT('Ctrl Pts',(5.18658635397621,5.90151295233514,-51.8682437617051));
#80096=CARTESIAN_POINT('Ctrl Pts',(1.73871613664041,7.64474653273967,-51.7094799607735));
#80097=CARTESIAN_POINT('Ctrl Pts',(-3.45565611673432,7.55161055380676,-51.4977948928649));
#80098=CARTESIAN_POINT('Ctrl Pts',(-7.48233483608931,3.6079690646464,-51.2861098249562));
#80099=CARTESIAN_POINT('Ctrl Pts',(-7.67217224580976,-1.57474516341014,
-51.0744247570474));
#80100=CARTESIAN_POINT('Ctrl Pts',(-5.47028243379752,-6.24232657838186,
-50.8627396891388));
#80101=CARTESIAN_POINT('Ctrl Pts',(1.12005997969442,-8.84134987042121,-50.5981333542529));
#80102=CARTESIAN_POINT('Ctrl Pts',(8.04160920853718,-3.8260723249102,-50.2806057523899));
#80103=CARTESIAN_POINT('Ctrl Pts',(7.64558894461407,3.23078010923851,-50.015999417504));
#80104=CARTESIAN_POINT('Ctrl Pts',(3.8941480339976,6.80448130998449,-49.8043143495953));
#80105=CARTESIAN_POINT('Ctrl Pts',(0.168113770862944,7.85495199818969,-49.6455505486638));
#80106=CARTESIAN_POINT('Ctrl Pts',(-3.59232951311789,6.96853298928954,-49.4867867477323));
#80107=CARTESIAN_POINT('Ctrl Pts',(-7.50653259438449,3.55251313339772,-49.2751016798236));
#80108=CARTESIAN_POINT('Ctrl Pts',(-8.04792309678225,-2.05759791967763,
-49.0634166119149));
#80109=CARTESIAN_POINT('Ctrl Pts',(-4.85591089761415,-6.14509386856656,
-48.8517315440062));
#80110=CARTESIAN_POINT('Ctrl Pts',(-0.165710669289473,-8.29838363723738,
-48.6400464760975));
#80111=CARTESIAN_POINT('Ctrl Pts',(6.55007496031395,-6.04322098748476,-48.3754401412117));
#80112=CARTESIAN_POINT('Ctrl Pts',(8.61626085969852,2.25085692479618,-48.0579125393486));
#80113=CARTESIAN_POINT('Ctrl Pts',(3.76921754196017,7.39499625054909,-47.7933062044627));
#80114=CARTESIAN_POINT('Ctrl Pts',(-1.40216082924845,7.71357892404924,-47.581621136554));
#80115=CARTESIAN_POINT('Ctrl Pts',(-4.92934118453569,6.11801672278348,-47.4228573356226));
#80116=CARTESIAN_POINT('Ctrl Pts',(-7.23564485061669,3.01839807669211,-47.264093534691));
#80117=CARTESIAN_POINT('Ctrl Pts',(-8.0307274151131,-2.1156082665917,-47.0524084667824));
#80118=CARTESIAN_POINT('Ctrl Pts',(-4.83247631834833,-6.75647452473442,
-46.8407233988736));
#80119=CARTESIAN_POINT('Ctrl Pts',(0.241730258758975,-7.82838526013267,
-46.629038330965));
#80120=CARTESIAN_POINT('Ctrl Pts',(5.21671445432797,-6.45573553661324,-46.4173532630562));
#80121=CARTESIAN_POINT('Ctrl Pts',(8.90276643323724,-0.405896199208848,
-46.1527469281705));
#80122=CARTESIAN_POINT('Ctrl Pts',(5.142863862158,7.27029981455958,-45.8352193263073));
#80123=CARTESIAN_POINT('Ctrl Pts',(-1.87798882331211,8.08493218300378,-45.5706129914216));
#80124=CARTESIAN_POINT('Ctrl Pts',(-6.03971349389217,4.99872140855163,-45.3589279235128));
#80125=CARTESIAN_POINT('Ctrl Pts',(-7.71091768105629,1.50674538319905,-45.2001641225813));
#80126=CARTESIAN_POINT('Ctrl Pts',(-7.47954565819725,-2.34982554683893,
-45.0414003216498));
#80127=CARTESIAN_POINT('Ctrl Pts',(-4.78196598600291,-6.78978515582278,
-44.8297152537411));
#80128=CARTESIAN_POINT('Ctrl Pts',(0.65334035126103,-8.28105800946939,-44.6180301858325));
#80129=CARTESIAN_POINT('Ctrl Pts',(5.22580291212903,-5.83378378264447,-44.4063451179237));
#80130=CARTESIAN_POINT('Ctrl Pts',(8.14824884455549,-1.58008600521795,-44.1946600500151));
#80131=CARTESIAN_POINT('Ctrl Pts',(7.07280463966759,5.42212471439058,-43.9300537151291));
#80132=CARTESIAN_POINT('Ctrl Pts',(-0.746727752358712,8.87404675230713,
-43.6125261132662));
#80133=CARTESIAN_POINT('Ctrl Pts',(-6.64288785802943,4.97644565226029,-43.3479197783803));
#80134=CARTESIAN_POINT('Ctrl Pts',(-7.83971812631999,-0.0646104361960217,
-43.1362347104716));
#80135=CARTESIAN_POINT('Ctrl Pts',(-6.86978933990756,-3.81241754784422,
-42.9774709095401));
#80136=CARTESIAN_POINT('Ctrl Pts',(-4.20944367644864,-6.61406586665424,
-42.8187071086085));
#80137=CARTESIAN_POINT('Ctrl Pts',(0.713434822181756,-8.27401909038279,
-42.6070220406999));
#80138=CARTESIAN_POINT('Ctrl Pts',(5.83220791973128,-5.91507617464108,-42.3953369727912));
#80139=CARTESIAN_POINT('Ctrl Pts',(7.7547149382516,-1.09838314149463,-42.1836519048825));
#80140=CARTESIAN_POINT('Ctrl Pts',(7.25161365384919,4.03791164242033,-41.9719668369739));
#80141=CARTESIAN_POINT('Ctrl Pts',(1.91993309088656,8.7027500720075,-41.7073605020879));
#80142=CARTESIAN_POINT('Ctrl Pts',(-6.28549546331617,6.30863336063426,-41.389832900225));
#80143=CARTESIAN_POINT('Ctrl Pts',(-8.28685849294037,-0.470049723154454,
-41.125226565339));
#80144=CARTESIAN_POINT('Ctrl Pts',(-5.9565055390961,-5.0975873284656,-40.9135414974304));
#80145=CARTESIAN_POINT('Ctrl Pts',(-2.80113087785069,-7.34044950523941,
-40.7547776964988));
#80146=CARTESIAN_POINT('Ctrl Pts',(1.03831811199606,-7.77091879071807,-40.5960138955673));
#80147=CARTESIAN_POINT('Ctrl Pts',(5.87365324500275,-5.87099469519337,-40.3843288276587));
#80148=CARTESIAN_POINT('Ctrl Pts',(8.27101668858417,-0.770102790506085,
-40.1726437597499));
#80149=CARTESIAN_POINT('Ctrl Pts',(6.64034551804669,4.15305438202045,-39.9609586918413));
#80150=CARTESIAN_POINT('Ctrl Pts',(2.94806154983591,7.75883780698274,-39.7492736239326));
#80151=CARTESIAN_POINT('Ctrl Pts',(-4.13495183477746,7.8946928511107,-39.4846672890467));
#80152=CARTESIAN_POINT('Ctrl Pts',(-8.87124308458381,0.779329347900915,
-39.1671396871837));
#80153=CARTESIAN_POINT('Ctrl Pts',(-6.03753865411047,-5.69570868499937,
-38.9025333522978));
#80154=CARTESIAN_POINT('Ctrl Pts',(-1.27483726544981,-7.73564119871364,
-38.6908482843891));
#80155=CARTESIAN_POINT('Ctrl Pts',(2.58354090478207,-7.41982813326131,-38.5320844834576));
#80156=CARTESIAN_POINT('Ctrl Pts',(5.7982624702782,-5.27687745540841,-38.3733206825261));
#80157=CARTESIAN_POINT('Ctrl Pts',(8.27434123245942,-0.709688891234698,
-38.1616356146175));
#80158=CARTESIAN_POINT('Ctrl Pts',(6.82397770110707,4.73667644087881,-37.9499505467087));
#80159=CARTESIAN_POINT('Ctrl Pts',(2.40624212751001,7.45332463554742,-37.7382654788));
#80160=CARTESIAN_POINT('Ctrl Pts',(-2.74053410931411,7.83454553961946,-37.5265804108914));
#80161=CARTESIAN_POINT('Ctrl Pts',(-8.2471743387975,3.37759045989717,-37.2619740760054));
#80162=CARTESIAN_POINT('Ctrl Pts',(-7.28914758159962,-5.11611528720145,
-36.9444464741425));
#80163=CARTESIAN_POINT('Ctrl Pts',(-0.951692555430078,-8.24543823603053,
-36.6798401392565));
#80164=CARTESIAN_POINT('Ctrl Pts',(4.00576868589115,-6.73937475169243,-36.4681550713479));
#80165=CARTESIAN_POINT('Ctrl Pts',(6.75442640137216,-4.01326016129843,-36.3093912704164));
#80166=CARTESIAN_POINT('Ctrl Pts',(7.83409611048614,-0.303679905986814,
-36.1506274694848));
#80167=CARTESIAN_POINT('Ctrl Pts',(6.78761954298498,4.78503940351681,-35.9389424015762));
#80168=CARTESIAN_POINT('Ctrl Pts',(2.17093158808615,8.0180940011098,-35.7272573336675));
#80169=CARTESIAN_POINT('Ctrl Pts',(-2.95834992293678,7.25191112966243,-35.5155722657588));
#80170=CARTESIAN_POINT('Ctrl Pts',(-7.14158571907033,4.22946621145696,-35.3038871978501));
#80171=CARTESIAN_POINT('Ctrl Pts',(-8.48475058019903,-2.72635461397087,
-35.0392808629642));
#80172=CARTESIAN_POINT('Ctrl Pts',(-2.28250116281199,-8.60793218723506,
-34.7217532611012));
#80173=CARTESIAN_POINT('Ctrl Pts',(4.58127298702289,-6.92133717157529,-34.4571469262153));
#80174=CARTESIAN_POINT('Ctrl Pts',(7.40440439747531,-2.57684891432614,-34.2454618583067));
#80175=CARTESIAN_POINT('Ctrl Pts',(7.7519810167304,1.27879765798563,-34.0866980573751));
#80176=CARTESIAN_POINT('Ctrl Pts',(6.18935383844591,4.81219102033048,-33.9279342564436));
#80177=CARTESIAN_POINT('Ctrl Pts',(2.11197233624808,8.03168438152565,-33.7162491885349));
#80178=CARTESIAN_POINT('Ctrl Pts',(-3.50205076232064,7.53249067897944,-33.5045641206263));
#80179=CARTESIAN_POINT('Ctrl Pts',(-6.93306478617521,3.64344095186944,-33.2928790527176));
#80180=CARTESIAN_POINT('Ctrl Pts',(-8.18741319037323,-1.36267981080949,
-33.0811939848088));
#80181=CARTESIAN_POINT('Ctrl Pts',(-4.73606367566928,-7.54941737813681,
-32.8165876499231));
#80182=CARTESIAN_POINT('Ctrl Pts',(3.7964985537964,-8.0556133738715,-32.4990600480599));
#80183=CARTESIAN_POINT('Ctrl Pts',(7.96188773294944,-2.34548804136043,-32.2344537131741));
#80184=CARTESIAN_POINT('Ctrl Pts',(7.32433981159772,2.7963192115458,-32.0227686452654));
#80185=CARTESIAN_POINT('Ctrl Pts',(5.10753862311752,5.97005714773156,-31.8640048443339));
#80186=CARTESIAN_POINT('Ctrl Pts',(1.63676025479456,7.66722239288512,-31.7052410434024));
#80187=CARTESIAN_POINT('Ctrl Pts',(-3.5559111666103,7.50492351251473,-31.4935559754937));
#80188=CARTESIAN_POINT('Ctrl Pts',(-7.52971711232564,3.50801020225614,-31.281870907585));
#80189=CARTESIAN_POINT('Ctrl Pts',(-7.65052177432877,-1.67677245909613,
-31.0701858396763));
#80190=CARTESIAN_POINT('Ctrl Pts',(-5.38667108337155,-6.31461840939378,
-30.8585007717676));
#80191=CARTESIAN_POINT('Ctrl Pts',(1.23769701372374,-8.8256505704411,-30.5938944368818));
#80192=CARTESIAN_POINT('Ctrl Pts',(8.09184627904301,-3.71864651380223,-30.2763668350187));
#80193=CARTESIAN_POINT('Ctrl Pts',(7.60188814473553,3.33230656740715,-30.0117605001329));
#80194=CARTESIAN_POINT('Ctrl Pts',(3.803190472164,6.85573460987635,-29.8000754322242));
#80195=CARTESIAN_POINT('Ctrl Pts',(0.0634979399251427,7.85649420196077,
-29.6413116312926));
#80196=CARTESIAN_POINT('Ctrl Pts',(-3.68480785801259,6.92007762985091,-29.4825478303612));
#80197=CARTESIAN_POINT('Ctrl Pts',(-7.55317424289503,3.45223695739262,-29.2708627624524));
#80198=CARTESIAN_POINT('Ctrl Pts',(-8.01980937097215,-2.16458610917884,
-29.0591776945438));
#80199=CARTESIAN_POINT('Ctrl Pts',(-4.77364882810306,-6.20921300689647,
-28.8474926266351));
#80200=CARTESIAN_POINT('Ctrl Pts',(-0.0551900682622783,-8.299854521198,
-28.6358075587264));
#80201=CARTESIAN_POINT('Ctrl Pts',(6.62996907301482,-5.95546068580551,-28.3712012238405));
#80202=CARTESIAN_POINT('Ctrl Pts',(8.58552319501832,2.36539628098087,-28.0536736219775));
#80203=CARTESIAN_POINT('Ctrl Pts',(3.67040743112835,7.44453354574839,-27.7890672870916));
#80204=CARTESIAN_POINT('Ctrl Pts',(-1.50475482230041,7.69422301037469,-27.577382219183));
#80205=CARTESIAN_POINT('Ctrl Pts',(-5.010375028303,6.0518323844581,-27.4186184182514));
#80206=CARTESIAN_POINT('Ctrl Pts',(-7.27519794438339,2.92177655266003,-27.2598546173199));
#80207=CARTESIAN_POINT('Ctrl Pts',(-8.00184271587865,-2.22236232506314,
-27.0481695494112));
#80208=CARTESIAN_POINT('Ctrl Pts',(-4.74207484075496,-6.82022738443972,
-26.8364844815025));
#80209=CARTESIAN_POINT('Ctrl Pts',(0.345955971607388,-7.82447210773809,
-26.6247994135939));
#80210=CARTESIAN_POINT('Ctrl Pts',(5.3022200691065,-6.38569443016573,-26.4131143456851));
#80211=CARTESIAN_POINT('Ctrl Pts',(8.90738217156051,-0.287306002502551,
-26.1485080107993));
#80212=CARTESIAN_POINT('Ctrl Pts',(5.0455924784123,7.33814040749187,-25.8309804089362));
#80213=CARTESIAN_POINT('Ctrl Pts',(-1.98548577227016,8.05920695058564,-25.5663740740504));
#80214=CARTESIAN_POINT('Ctrl Pts',(-6.1057437206868,4.91784998001252,-25.3546890061417));
#80215=CARTESIAN_POINT('Ctrl Pts',(-7.73029862184605,1.40392889809396,-25.1959252052102));
#80216=CARTESIAN_POINT('Ctrl Pts',(-7.44759086384508,-2.44921899355802,
-25.0371614042787));
#80217=CARTESIAN_POINT('Ctrl Pts',(-4.69112540417169,-6.85286243812432,
-24.8254763363699));
#80218=CARTESIAN_POINT('Ctrl Pts',(0.763557609887108,-8.27162348920492,
-24.6137912684613));
#80219=CARTESIAN_POINT('Ctrl Pts',(5.30302546439297,-5.76367679724166,-24.4021062005526));
#80220=CARTESIAN_POINT('Ctrl Pts',(8.16856765215318,-1.47143927121796,-24.190421132644));
#80221=CARTESIAN_POINT('Ctrl Pts',(6.99997346048449,5.51582935213016,-23.925814797758));
#80222=CARTESIAN_POINT('Ctrl Pts',(-0.864833299418169,8.86331605340198,
-23.6082871958951));
#80223=CARTESIAN_POINT('Ctrl Pts',(-6.708567965379,4.88754399245119,-23.3436808610091));
#80224=CARTESIAN_POINT('Ctrl Pts',(-7.83816259545043,-0.169002768904056,
-23.1319957931005));
#80225=CARTESIAN_POINT('Ctrl Pts',(-6.81841192090368,-3.90356145214814,
-22.9732319921689));
#80226=CARTESIAN_POINT('Ctrl Pts',(-4.12099383588237,-6.66953470327981,
-22.8144681912375));
#80227=CARTESIAN_POINT('Ctrl Pts',(0.823553018099068,-8.26378494274268,
-22.6027831233287));
#80228=CARTESIAN_POINT('Ctrl Pts',(5.91045923735201,-5.83688675360274,-22.3910980554201));
#80229=CARTESIAN_POINT('Ctrl Pts',(7.768654016065,-0.995019636861024,-22.1794129875113));
#80230=CARTESIAN_POINT('Ctrl Pts',(7.19719957354974,4.1341201379714,-21.9677279196027));
#80231=CARTESIAN_POINT('Ctrl Pts',(1.80387217509234,8.72754530582543,-21.7031215847168));
#80232=CARTESIAN_POINT('Ctrl Pts',(-6.36894741537249,6.22437281326372,-21.3855939828538));
#80233=CARTESIAN_POINT('Ctrl Pts',(-8.27986425864372,-0.580360476505481,
-21.1209876479679));
#80234=CARTESIAN_POINT('Ctrl Pts',(-5.88809506230738,-5.17645548091035,
-20.9093025800592));
#80235=CARTESIAN_POINT('Ctrl Pts',(-2.70313298147792,-7.377100054782,-20.7505387791277));
#80236=CARTESIAN_POINT('Ctrl Pts',(1.14170793638774,-7.7564029254303,-20.5917749781962));
#80237=CARTESIAN_POINT('Ctrl Pts',(5.9513138741151,-5.79225727374789,-20.3800899102875));
#80238=CARTESIAN_POINT('Ctrl Pts',(8.280538421931,-0.659893032019098,-20.1684048423788));
#80239=CARTESIAN_POINT('Ctrl Pts',(6.58445233348109,4.24111268032075,-19.9567197744701));
#80240=CARTESIAN_POINT('Ctrl Pts',(2.84447913310934,7.79740786915694,-19.7450347065614));
#80241=CARTESIAN_POINT('Ctrl Pts',(-4.23971532731654,7.83892950807863,-19.4804283716756));
#80242=CARTESIAN_POINT('Ctrl Pts',(-8.88083446226933,0.661125821645083,
-19.1629007698126));
#80243=CARTESIAN_POINT('Ctrl Pts',(-5.96115607439654,-5.77560288462947,
-18.8982944349267));
#80244=CARTESIAN_POINT('Ctrl Pts',(-1.17171211131436,-7.75193172937009,
-18.686609367018));
#80245=CARTESIAN_POINT('Ctrl Pts',(2.68211839623764,-7.38476634988415,-18.5278455660865));
#80246=CARTESIAN_POINT('Ctrl Pts',(5.86801818751382,-5.19919665954668,-18.3690817651549));
#80247=CARTESIAN_POINT('Ctrl Pts',(8.28305816582356,-0.599440218123851,
-18.1573966972463));
#80248=CARTESIAN_POINT('Ctrl Pts',(6.76029639696928,4.82712833845422,-17.9457116293376));
#80249=CARTESIAN_POINT('Ctrl Pts',(2.30677613741518,7.48470661755781,-17.7340265614289));
#80250=CARTESIAN_POINT('Ctrl Pts',(-2.84462028871749,7.79735637441958,-17.5223414935202));
#80251=CARTESIAN_POINT('Ctrl Pts',(-8.29142094719077,3.26746699536407,-17.2577351586343));
#80252=CARTESIAN_POINT('Ctrl Pts',(-7.22037221174813,-5.21272800192871,
-16.9402075567713));
#80253=CARTESIAN_POINT('Ctrl Pts',(-0.841807312456317,-8.25738038804991,
-16.6756012218854));
#80254=CARTESIAN_POINT('Ctrl Pts',(4.09515877244995,-6.68543412480008,-16.4639161539767));
#80255=CARTESIAN_POINT('Ctrl Pts',(6.80727030315708,-3.92295859697418,-16.3051523530452));
#80256=CARTESIAN_POINT('Ctrl Pts',(7.83744543784448,-0.199329783135814,
-16.1463885521137));
#80257=CARTESIAN_POINT('Ctrl Pts',(6.72329743449899,4.87500284725866,-15.934703484205));
#80258=CARTESIAN_POINT('Ctrl Pts',(2.06396567875818,8.0462923789589,-15.7230184162963));
#80259=CARTESIAN_POINT('Ctrl Pts',(-3.05465810381368,7.21187306931196,-15.5113333483876));
#80260=CARTESIAN_POINT('Ctrl Pts',(-7.19727441213497,4.13398984675969,-15.299648280479));
#80261=CARTESIAN_POINT('Ctrl Pts',(-8.44769258385265,-2.83910054383924,
-15.0350419455931));
#80262=CARTESIAN_POINT('Ctrl Pts',(-2.1676707462325,-8.63756398727118,-14.7175143437301));
#80263=CARTESIAN_POINT('Ctrl Pts',(4.6730351571543,-6.85971667375965,-14.4529080088442));
#80264=CARTESIAN_POINT('Ctrl Pts',(7.43806261239201,-2.47801924583956,-14.2412229409355));
#80265=CARTESIAN_POINT('Ctrl Pts',(7.73426447080314,1.38191397325961,-14.082459140004));
#80266=CARTESIAN_POINT('Ctrl Pts',(6.12472321167347,4.89418521656284,-13.9236953390725));
#80267=CARTESIAN_POINT('Ctrl Pts',(2.00483067770523,8.05909642002457,-13.7120102711638));
#80268=CARTESIAN_POINT('Ctrl Pts',(-3.60204708749114,7.48518751603995,-13.5003252032551));
#80269=CARTESIAN_POINT('Ctrl Pts',(-6.98096812924419,3.55079333072749,-13.2886401353464));
#80270=CARTESIAN_POINT('Ctrl Pts',(-8.16854101342506,-1.4715871461377,-13.0769550674377));
#80271=CARTESIAN_POINT('Ctrl Pts',(-4.63511147736421,-7.61181604360706,
-12.8123487325518));
#80272=CARTESIAN_POINT('Ctrl Pts',(3.90343496423354,-8.00434279490049,-12.4948211306888));
#80273=CARTESIAN_POINT('Ctrl Pts',(7.99241558571472,-2.23925512826935,-12.2302147958029));
#80274=CARTESIAN_POINT('Ctrl Pts',(7.28645302042453,2.89360626031973,-12.0185297278943));
#80275=CARTESIAN_POINT('Ctrl Pts',(5.02758512861158,6.03754262166171,-11.8597659269627));
#80276=CARTESIAN_POINT('Ctrl Pts',(1.53451411220522,7.68833855869245,-11.7010021260312));
#80277=CARTESIAN_POINT('Ctrl Pts',(-3.65553561624384,7.45690555873499,-11.4893170581226));
#80278=CARTESIAN_POINT('Ctrl Pts',(-7.57576407921462,3.40742923431496,-11.2776319902138));
#80279=CARTESIAN_POINT('Ctrl Pts',(-7.62751457017181,-1.77850239833385,
-11.0659469223052));
#80280=CARTESIAN_POINT('Ctrl Pts',(-5.3021044683393,-6.38579041493706,-10.8542618543965));
#80281=CARTESIAN_POINT('Ctrl Pts',(1.35511455632098,-8.8083861421122,-10.5896555195106));
#80282=CARTESIAN_POINT('Ctrl Pts',(8.14064835301168,-3.61056124319814,-10.2721279176476));
#80283=CARTESIAN_POINT('Ctrl Pts',(7.55683923680033,3.4332420790575,-10.0075215827617));
#80284=CARTESIAN_POINT('Ctrl Pts',(3.71155845792856,6.90577212352062,-9.79583651485306));
#80285=CARTESIAN_POINT('Ctrl Pts',(-0.0411291516472582,7.85664314619816,
-9.63707271392151));
#80286=CARTESIAN_POINT('Ctrl Pts',(-3.77663274431041,6.87039507366472,-9.47830891299001));
#80287=CARTESIAN_POINT('Ctrl Pts',(-7.59847642220299,3.35134856658408,-9.26662384508131));
#80288=CARTESIAN_POINT('Ctrl Pts',(-7.99027342354806,-2.27119043405084,
-9.05493877717264));
#80289=CARTESIAN_POINT('Ctrl Pts',(-4.69054020648244,-6.27223101220251,
-8.84325370926394));
#80290=CARTESIAN_POINT('Ctrl Pts',(0.0553403200935083,-8.29985352073492,
-8.63156864135525));
#80291=CARTESIAN_POINT('Ctrl Pts',(6.70868743640794,-5.86664425117891,-8.36696230646939));
#80292=CARTESIAN_POINT('Ctrl Pts',(8.55326298583737,2.47951616114584,-8.04943470460635));
#80293=CARTESIAN_POINT('Ctrl Pts',(3.57094641545068,7.49275063793162,-7.78482836972049));
#80294=CARTESIAN_POINT('Ctrl Pts',(-1.60708196426699,7.67350261411015,-7.57314330181181));
#80295=CARTESIAN_POINT('Ctrl Pts',(-5.09052033927314,5.98457482276319,-7.41437950088028));
#80296=CARTESIAN_POINT('Ctrl Pts',(-7.31346086486846,2.82463688492333,-7.25561569994876));
#80297=CARTESIAN_POINT('Ctrl Pts',(-7.97153898121459,-2.32872227296088,
-7.04393063204009));
#80298=CARTESIAN_POINT('Ctrl Pts',(-4.65083241033187,-6.8827707546837,-6.83224556413139));
#80299=CARTESIAN_POINT('Ctrl Pts',(0.450120333107332,-7.81917137457972,
-6.6205604962227));
#80300=CARTESIAN_POINT('Ctrl Pts',(5.38678539571902,-6.31452089368896,-6.40887542831401));
#80301=CARTESIAN_POINT('Ctrl Pts',(8.91041828733191,-0.168664855442598,
-6.14426909342813));
#80302=CARTESIAN_POINT('Ctrl Pts',(4.94742631652087,7.40467966516704,-5.82674149156514));
#80303=CARTESIAN_POINT('Ctrl Pts',(-2.09263061810849,8.0320525095882,-5.56213515667924));
#80304=CARTESIAN_POINT('Ctrl Pts',(-6.1706911634019,4.83610642728852,-5.35045008877058));
#80305=CARTESIAN_POINT('Ctrl Pts',(-7.74830868277893,1.30086344146143,-5.19168628783903));
#80306=CARTESIAN_POINT('Ctrl Pts',(-7.41431532367873,-2.54817809782355,
-5.03292248690753));
#80307=CARTESIAN_POINT('Ctrl Pts',(-4.59945290622839,-6.91472444679411,
-4.82123741899884));
#80308=CARTESIAN_POINT('Ctrl Pts',(0.873639462994944,-8.26072208469958,
-4.60955235109015));
#80309=CARTESIAN_POINT('Ctrl Pts',(5.37930758248336,-5.69254769690278,-4.39786728318148));
#80310=CARTESIAN_POINT('Ctrl Pts',(8.18743786494988,-1.36253157712688,-4.18618221527277));
#80311=CARTESIAN_POINT('Ctrl Pts',(6.92590090019624,5.60855578403209,-3.92157588038692));
#80312=CARTESIAN_POINT('Ctrl Pts',(-0.98278545040757,8.85101361093665,-3.60404827852388));
#80313=CARTESIAN_POINT('Ctrl Pts',(-6.77305843181678,4.79777547357795,-3.33944194363801));
#80314=CARTESIAN_POINT('Ctrl Pts',(-7.83521699085168,-0.273364980042835,
-3.12775687572932));
#80315=CARTESIAN_POINT('Ctrl Pts',(-6.76582547640464,-3.99401343348083,
-2.96899307479781));
#80316=CARTESIAN_POINT('Ctrl Pts',(-4.03181291942652,-6.72382016067921,
-2.81022927386629));
#80317=CARTESIAN_POINT('Ctrl Pts',(0.933524562352959,-8.25208670680614,
-2.59854420595759));
#80318=CARTESIAN_POINT('Ctrl Pts',(5.98766356057595,-5.75765954361041,-2.38685913804893));
#80319=CARTESIAN_POINT('Ctrl Pts',(7.78121405787801,-0.891482814498843,
-2.17517407014022));
#80320=CARTESIAN_POINT('Ctrl Pts',(7.14151231839871,4.2296028322805,-1.96348900223155));
#80321=CARTESIAN_POINT('Ctrl Pts',(1.68748462236888,8.75077718769076,-1.69888266734567));
#80322=CARTESIAN_POINT('Ctrl Pts',(-6.45125802233304,6.13903598732601,-1.38135506548265));
#80323=CARTESIAN_POINT('Ctrl Pts',(-8.27142181248957,-0.690614954054182,
-1.11674873059677));
#80324=CARTESIAN_POINT('Ctrl Pts',(-5.81861252887425,-5.2543410602677,-0.905063662688093));
#80325=CARTESIAN_POINT('Ctrl Pts',(-2.60471651056193,-7.41258324978489,
-0.746299861756561));
#80326=CARTESIAN_POINT('Ctrl Pts',(1.24500861472902,-7.740248929974,-0.587536060825044));
#80327=CARTESIAN_POINT('Ctrl Pts',(6.02766054384712,-5.71309187500411,-0.375850992916369));
#80328=CARTESIAN_POINT('Ctrl Pts',(8.28908744005743,-0.548417296970164,
-0.164165925007672));
#80329=CARTESIAN_POINT('Ctrl Pts',(6.52681211271625,4.32707578852068,0.0475191429010087));
#80330=CARTESIAN_POINT('Ctrl Pts',(2.74174315069786,7.83773263990448,0.259204210809702));
#80331=CARTESIAN_POINT('Ctrl Pts',(-4.34655550419588,7.77513718308878,0.523810545695566));
#80332=CARTESIAN_POINT('Ctrl Pts',(-8.88411837919809,0.554292796363548,
0.841338147558601));
#80333=CARTESIAN_POINT('Ctrl Pts',(-5.29130331250487,-7.15799616755843,
1.15886574942163));
#80334=CARTESIAN_POINT('Ctrl Pts',(3.1560060963405,-8.32976161044042,1.47639335128466));
#80335=CARTESIAN_POINT('Ctrl Pts',(7.76422719570322,-2.94346470889751,1.74099968617053));
#80336=CARTESIAN_POINT('Ctrl Pts',(7.51173105023254,2.21286191690165,1.95268475407922));
#80337=CARTESIAN_POINT('Ctrl Pts',(4.91298462537403,6.698680033512,2.1643698219879));
#80338=CARTESIAN_POINT('Ctrl Pts',(-0.495822942463844,8.29013088037915,
2.37605488989661));
#80339=CARTESIAN_POINT('Ctrl Pts',(-5.12469586560105,5.93287385958993,2.58773995780528));
#80340=CARTESIAN_POINT('Ctrl Pts',(-7.35058989770351,2.77484534544985,2.74650375873681));
#80341=CARTESIAN_POINT('Ctrl Pts',(-7.76599029997037,-1.07412587695898,
2.90526755966833));
#80342=CARTESIAN_POINT('Ctrl Pts',(-5.85018163290799,-5.8880168713139,3.116952627577));
#80343=CARTESIAN_POINT('Ctrl Pts',(0.5493877149772,-8.88845689999296,3.38155896246287));
#80344=CARTESIAN_POINT('Ctrl Pts',(7.78496039936211,-4.33798309352451,3.6990865643259));
#80345=CARTESIAN_POINT('Ctrl Pts',(7.83258008256155,2.7461659751253,3.96369289921177));
#80346=CARTESIAN_POINT('Ctrl Pts',(4.32360152919418,6.53058218230311,4.17537796712045));
#80347=CARTESIAN_POINT('Ctrl Pts',(-0.555674784775465,8.28818338771179,
4.38706303502915));
#80348=CARTESIAN_POINT('Ctrl Pts',(-5.7169371761748,6.02370587336679,4.59874810293782));
#80349=CARTESIAN_POINT('Ctrl Pts',(-7.74142671390708,1.23918739648874,4.81043317084652));
#80350=CARTESIAN_POINT('Ctrl Pts',(-7.41052017936217,-2.61012037179468,
4.96919697177804));
#80351=CARTESIAN_POINT('Ctrl Pts',(-5.25011376394542,-5.82251313194528,
5.12796077270955));
#80352=CARTESIAN_POINT('Ctrl Pts',(-0.684469425562928,-8.27190858394483,
5.33964584061826));
#80353=CARTESIAN_POINT('Ctrl Pts',(6.14376360232249,-6.44674165616213,5.60425217550411));
#80354=CARTESIAN_POINT('Ctrl Pts',(8.74954614262611,1.69394319857397,5.92177977736714));
#80355=CARTESIAN_POINT('Ctrl Pts',(4.22432866422699,7.14462584238486,6.18638611225301));
#80356=CARTESIAN_POINT('Ctrl Pts',(-0.897216819650257,7.78055597801422,
6.3980711801617));
#80357=CARTESIAN_POINT('Ctrl Pts',(-5.76207558030114,5.98341543592307,6.60975624807037));
#80358=CARTESIAN_POINT('Ctrl Pts',(-8.25277139000861,0.92744034630844,6.82144131597908));
#80359=CARTESIAN_POINT('Ctrl Pts',(-6.72084614008006,-4.03676980995147,
7.03312638388776));
#80360=CARTESIAN_POINT('Ctrl Pts',(-3.9890233266215,-6.76876842835001,7.19189018481927));
#80361=CARTESIAN_POINT('Ctrl Pts',(-0.267587861335669,-7.83541648839507,
7.3506539857508));
#80362=CARTESIAN_POINT('Ctrl Pts',(4.80276830414162,-6.76951896646725,7.56233905365949));
#80363=CARTESIAN_POINT('Ctrl Pts',(8.85173578479164,-0.976259031907224,
7.82694538854534));
#80364=CARTESIAN_POINT('Ctrl Pts',(5.60344757332302,6.93003442860875,8.14447299040839));
#80365=CARTESIAN_POINT('Ctrl Pts',(-1.3685681241356,8.18643098706431,8.40907932529423));
#80366=CARTESIAN_POINT('Ctrl Pts',(-5.69651250430969,5.37510879774223,8.62076439320295));
#80367=CARTESIAN_POINT('Ctrl Pts',(-8.26136401205398,0.867548287337313,
8.83244946111161));
#80368=CARTESIAN_POINT('Ctrl Pts',(-6.91133121739989,-4.6045501362241,9.04413452902033));
#80369=CARTESIAN_POINT('Ctrl Pts',(-2.54271055807657,-7.4161921746593,9.25581959692898));
#80370=CARTESIAN_POINT('Ctrl Pts',(1.30657620274551,-7.74734740154486,9.41458339786053));
#80371=CARTESIAN_POINT('Ctrl Pts',(4.84065499080121,-6.16712364629238,9.57334719879202));
#80372=CARTESIAN_POINT('Ctrl Pts',(8.03359330030085,-2.08670772021527,9.78503226670073));
#80373=CARTESIAN_POINT('Ctrl Pts',(7.40102973205109,4.95288471535275,10.0496386015866));
#80374=CARTESIAN_POINT('Ctrl Pts',(-0.175234789971888,8.91029150239721,
10.3671662034496));
#80375=CARTESIAN_POINT('Ctrl Pts',(-6.31849105303928,5.38212800194741,10.6317725383355));
#80376=CARTESIAN_POINT('Ctrl Pts',(-7.81950113939896,0.444354846942566,
10.8434576062442));
#80377=CARTESIAN_POINT('Ctrl Pts',(-6.87933965324438,-4.65590606714548,
11.0551426741529));
#80378=CARTESIAN_POINT('Ctrl Pts',(-2.32284392985198,-7.97325386721565,
11.2668277420615));
#80379=CARTESIAN_POINT('Ctrl Pts',(2.83002860187081,-7.31137616774212,11.4785128099703));
#80380=CARTESIAN_POINT('Ctrl Pts',(5.98832662459847,-5.08610630747561,11.6372766109017));
#80381=CARTESIAN_POINT('Ctrl Pts',(7.67468548908019,-1.60142357055152,11.7960404118333));
#80382=CARTESIAN_POINT('Ctrl Pts',(7.49011561048965,3.57647012650109,12.007725479742));
#80383=CARTESIAN_POINT('Ctrl Pts',(2.47320885046191,8.55508889961241,12.2723318146278));
#80384=CARTESIAN_POINT('Ctrl Pts',(-5.87158921942888,6.70435991930579,12.5898594164909));
#80385=CARTESIAN_POINT('Ctrl Pts',(-8.29989206902337,0.049220516537637,
12.8544657513767));
#80386=CARTESIAN_POINT('Ctrl Pts',(-6.26877079868885,-4.69516367899656,
13.0661508192854));
#80387=CARTESIAN_POINT('Ctrl Pts',(-2.26529829299243,-7.99194588411035,
13.2778358871941));
#80388=CARTESIAN_POINT('Ctrl Pts',(3.35695029285333,-7.59600328362433,13.4895209551028));
#80389=CARTESIAN_POINT('Ctrl Pts',(6.87317785685779,-3.77156592168745,13.7012060230115));
#80390=CARTESIAN_POINT('Ctrl Pts',(7.85667133654639,-0.035336147331286,
13.859969823943));
#80391=CARTESIAN_POINT('Ctrl Pts',(6.90303357718645,3.71664932982005,14.0187336248745));
#80392=CARTESIAN_POINT('Ctrl Pts',(3.42766920914769,7.55936863877645,14.2304186927832));
#80393=CARTESIAN_POINT('Ctrl Pts',(-3.6165626623917,8.13798393997374,14.4950250276691));
#80394=CARTESIAN_POINT('Ctrl Pts',(-8.8093829237094,1.348619439562,14.8125526295321));
#80395=CARTESIAN_POINT('Ctrl Pts',(-6.38187924163906,-5.3068115061515,15.077158964418));
#80396=CARTESIAN_POINT('Ctrl Pts',(-1.77287786670344,-7.6288238522603,15.2888440323267));
#80397=CARTESIAN_POINT('Ctrl Pts',(3.41301419869038,-7.57324959646258,15.5005291002354));
#80398=CARTESIAN_POINT('Ctrl Pts',(7.45959889311056,-3.6500363706987,15.712214168144));
#80399=CARTESIAN_POINT('Ctrl Pts',(7.68720501482482,1.54018259102167,15.9238992360527));
#80400=CARTESIAN_POINT('Ctrl Pts',(6.03383395627602,5.03203546508849,16.0826630369842));
#80401=CARTESIAN_POINT('Ctrl Pts',(2.88823290284334,7.28858460248274,16.2414268379158));
#80402=CARTESIAN_POINT('Ctrl Pts',(-2.24514762273551,7.99076232761187,16.4531119058244));
#80403=CARTESIAN_POINT('Ctrl Pts',(-8.00721876580877,3.89753200561023,16.7177182407104));
#80404=CARTESIAN_POINT('Ctrl Pts',(-7.60839633559909,-4.64072269045992,
17.0352458425733));
#80405=CARTESIAN_POINT('Ctrl Pts',(-1.46556377916027,-8.16962384849504,
17.2998521774592));
#80406=CARTESIAN_POINT('Ctrl Pts',(3.5559396911123,-6.97834810053455,17.5115372453679));
#80407=CARTESIAN_POINT('Ctrl Pts',(7.48784140366001,-3.59652700315428,17.7232223132766));
#80408=CARTESIAN_POINT('Ctrl Pts',(8.05761599360032,2.01077240213722,17.9349073811853));
#80409=CARTESIAN_POINT('Ctrl Pts',(4.88966790155371,6.1283302102734,18.146592449094));
#80410=CARTESIAN_POINT('Ctrl Pts',(1.376210838791,7.7352813045818,18.3053562500255));
#80411=CARTESIAN_POINT('Ctrl Pts',(-2.48350293048252,7.43623345537914,18.464120050957));
#80412=CARTESIAN_POINT('Ctrl Pts',(-6.86316041045839,4.66797596443816,18.6758051188657));
#80413=CARTESIAN_POINT('Ctrl Pts',(-8.63596333560425,-2.17403895189931,
18.9404114537515));
#80414=CARTESIAN_POINT('Ctrl Pts',(-2.83287097636486,-8.44978366117008,
19.2579390556146));
#80415=CARTESIAN_POINT('Ctrl Pts',(4.13929553922285,-7.19422431229763,19.5225453905004));
#80416=CARTESIAN_POINT('Ctrl Pts',(7.21412342111526,-3.04933969311035,19.7342304584091));
#80417=CARTESIAN_POINT('Ctrl Pts',(8.04476835359511,2.06989794622304,19.9459155263178));
#80418=CARTESIAN_POINT('Ctrl Pts',(4.87004418658415,6.72689012651754,20.1576005942265));
#80419=CARTESIAN_POINT('Ctrl Pts',(-0.205108566907885,7.83729633415856,
20.3692856621352));
#80420=CARTESIAN_POINT('Ctrl Pts',(-3.92797678237034,6.80437591046944,20.5280494630667));
#80421=CARTESIAN_POINT('Ctrl Pts',(-6.68845181927522,4.09022824177934,20.6868132639982));
#80422=CARTESIAN_POINT('Ctrl Pts',(-8.25675744780296,-0.847895555128566,
20.8984983319069));
#80423=CARTESIAN_POINT('Ctrl Pts',(-5.20740273785928,-7.224213785874,21.1631046667928));
#80424=CARTESIAN_POINT('Ctrl Pts',(3.27357967802362,-8.28900946922719,21.4806322686558));
#80425=CARTESIAN_POINT('Ctrl Pts',(7.7994516984316,-2.83887023664659,21.7452386035417));
#80426=CARTESIAN_POINT('Ctrl Pts',(7.48300371173338,2.31229426095535,21.9569236714504));
#80427=CARTESIAN_POINT('Ctrl Pts',(4.82214241009197,6.76385377928702,22.1686087393591));
#80428=CARTESIAN_POINT('Ctrl Pts',(-0.605547459853415,8.28261392480565,
22.3802938072677));
#80429=CARTESIAN_POINT('Ctrl Pts',(-5.20352195274805,5.86418303269119,22.5919788751764));
#80430=CARTESIAN_POINT('Ctrl Pts',(-7.38674196740523,2.67667260620213,22.750742676108));
#80431=CARTESIAN_POINT('Ctrl Pts',(-7.75106567552916,-1.17742757834563,
22.9095064770395));
#80432=CARTESIAN_POINT('Ctrl Pts',(-5.77120593411264,-5.96541301925682,
23.1211915449482));
#80433=CARTESIAN_POINT('Ctrl Pts',(0.667673809145736,-8.88034457568269,
23.385797879834));
#80434=CARTESIAN_POINT('Ctrl Pts',(7.84205347588213,-4.23393424260604,23.7033254816971));
#80435=CARTESIAN_POINT('Ctrl Pts',(7.79530841005407,2.85022767666477,23.9679318165829));
#80436=CARTESIAN_POINT('Ctrl Pts',(4.23625656757878,6.5875776726129,24.1796168844917));
#80437=CARTESIAN_POINT('Ctrl Pts',(-0.665998399415621,8.2800496075059,24.3913019524002));
#80438=CARTESIAN_POINT('Ctrl Pts',(-5.79664382272207,5.9470414111572,24.6029870203091));
#80439=CARTESIAN_POINT('Ctrl Pts',(-7.75724264040923,1.13598854371463,24.8146720882177));
#80440=CARTESIAN_POINT('Ctrl Pts',(-7.37510492967002,-2.70857165498245,
24.9734358891492));
#80441=CARTESIAN_POINT('Ctrl Pts',(-5.17211256384402,-5.89191025352067,
25.1321996900807));
#80442=CARTESIAN_POINT('Ctrl Pts',(-0.57425526905304,-8.28028992911609,
25.3438847579894));
#80443=CARTESIAN_POINT('Ctrl Pts',(6.22906718140751,-6.36435622414303,25.6084910928752));
#80444=CARTESIAN_POINT('Ctrl Pts',(8.72621287182006,1.81030682620079,25.9260186947383));
#80445=CARTESIAN_POINT('Ctrl Pts',(4.12881225314493,7.20024585656392,26.1906250296241));
#80446=CARTESIAN_POINT('Ctrl Pts',(-1.00074748188264,7.76791823956505,26.4023100975329));
#80447=CARTESIAN_POINT('Ctrl Pts',(-5.84124316681254,5.90615387853627,26.6139951654415));
#80448=CARTESIAN_POINT('Ctrl Pts',(-8.26438993242782,0.817459600412216,
26.8256802333502));
#80449=CARTESIAN_POINT('Ctrl Pts',(-6.6664943293382,-4.12591040990177,27.0373653012589));
#80450=CARTESIAN_POINT('Ctrl Pts',(-3.89853292411994,-6.82128830745126,
27.1961291021904));
#80451=CARTESIAN_POINT('Ctrl Pts',(-0.163223356220313,-7.83828507676261,
27.354892903122));
#80452=CARTESIAN_POINT('Ctrl Pts',(4.89248913876279,-6.70496237508786,27.5665779710306));
#80453=CARTESIAN_POINT('Ctrl Pts',(8.86395131759078,-0.8582978140814,27.8311843059165));
#80454=CARTESIAN_POINT('Ctrl Pts',(5.51066651380619,7.00403858234108,28.1487119077796));
#80455=CARTESIAN_POINT('Ctrl Pts',(-1.47746185782562,8.167480485153,28.4133182426654));
#80456=CARTESIAN_POINT('Ctrl Pts',(-5.76758534699895,5.29877425110231,28.6250033105741));
#80457=CARTESIAN_POINT('Ctrl Pts',(-8.27218423992927,0.757458428859326,
28.8366883784828));
#80458=CARTESIAN_POINT('Ctrl Pts',(-6.84940163528804,-4.69617699751986,
29.0483734463915));
#80459=CARTESIAN_POINT('Ctrl Pts',(-2.44372694399771,-7.44939473895791,
29.2600585143002));
#80460=CARTESIAN_POINT('Ctrl Pts',(1.40962835111201,-7.72926135187306,29.4188223152317));
#80461=CARTESIAN_POINT('Ctrl Pts',(4.92235063350798,-6.10211594853941,29.5775861161632));
#80462=CARTESIAN_POINT('Ctrl Pts',(8.06066873181136,-1.97954288164058,29.7892711840719));
#80463=CARTESIAN_POINT('Ctrl Pts',(7.33441811107692,5.05100178877253,30.0538775189577));
#80464=CARTESIAN_POINT('Ctrl Pts',(-0.293873666226079,8.90716790891514,
30.3714051208208));
#80465=CARTESIAN_POINT('Ctrl Pts',(-6.38960221699068,5.29751021946285,30.6360114557066));
#80466=CARTESIAN_POINT('Ctrl Pts',(-7.82472506690299,0.340186605324074,
30.8476965236154));
#80467=CARTESIAN_POINT('Ctrl Pts',(-6.81672902357357,-4.74710235722308,
31.059381591524));
#80468=CARTESIAN_POINT('Ctrl Pts',(-2.21646166681117,-8.00347917052808,
31.2710666594327));
#80469=CARTESIAN_POINT('Ctrl Pts',(2.92714003054094,-7.27304163299227,31.4827517273414));
#80470=CARTESIAN_POINT('Ctrl Pts',(6.05552507391138,-5.00591142680821,31.6415155282729));
#80471=CARTESIAN_POINT('Ctrl Pts',(7.69533043013239,-1.49908117848691,31.8002793292044));
#80472=CARTESIAN_POINT('Ctrl Pts',(7.44182519513283,3.67589556289904,32.0119643971131));
#80473=CARTESIAN_POINT('Ctrl Pts',(2.35906521467522,8.5872649552221,32.276570731999));
#80474=CARTESIAN_POINT('Ctrl Pts',(-5.96034758795615,6.62557608967355,32.594098333862));
#80475=CARTESIAN_POINT('Ctrl Pts',(-8.29981157134884,-0.0613098425100343,
32.8587046687479));
#80476=CARTESIAN_POINT('Ctrl Pts',(-6.20569153145733,-4.77822581252294,
33.0703897366566));
#80477=CARTESIAN_POINT('Ctrl Pts',(-2.15867221915416,-8.02140322020008,
33.2820748045652));
#80478=CARTESIAN_POINT('Ctrl Pts',(3.45780525326754,-7.55062672789463,33.493759872474));
#80479=CARTESIAN_POINT('Ctrl Pts',(6.92279269365902,-3.67970442756689,33.7054449403826));
#80480=CARTESIAN_POINT('Ctrl Pts',(7.85644524693097,0.0692908059781572,
33.8642087413142));
#80481=CARTESIAN_POINT('Ctrl Pts',(6.85292851347593,3.80824442464031,34.0229725422456));
#80482=CARTESIAN_POINT('Ctrl Pts',(3.32670050871143,7.60434311098562,34.2346576101544));
#80483=CARTESIAN_POINT('Ctrl Pts',(-3.72461192004342,8.08910218400948,34.4992639450402));
#80484=CARTESIAN_POINT('Ctrl Pts',(-8.82656077105497,1.23118919918194,34.8167915469033));
#80485=CARTESIAN_POINT('Ctrl Pts',(-6.31064490135422,-5.39132562044787,
35.0813978817891));
#80486=CARTESIAN_POINT('Ctrl Pts',(-1.67113099105788,-7.65175604092209,
35.2930829496978));
#80487=CARTESIAN_POINT('Ctrl Pts',(3.51356118716118,-7.52712848002853,35.5047680176065));
#80488=CARTESIAN_POINT('Ctrl Pts',(7.50754337705162,-3.55037654273579,35.7164530855152));
#80489=CARTESIAN_POINT('Ctrl Pts',(7.66601346490072,1.64241313608831,35.9281381534239));
#80490=CARTESIAN_POINT('Ctrl Pts',(5.9662895480264,5.11193917832848,36.0869019543554));
#80491=CARTESIAN_POINT('Ctrl Pts',(2.79091794518469,7.32639965002328,36.2456657552869));
#80492=CARTESIAN_POINT('Ctrl Pts',(-2.35135799763592,7.96015615369499,36.4573508231956));
#80493=CARTESIAN_POINT('Ctrl Pts',(-8.0584104826783,3.79055782055054,36.7219571580814));
#80494=CARTESIAN_POINT('Ctrl Pts',(-7.5459232513068,-4.74162885248265,37.0394847599445));
#80495=CARTESIAN_POINT('Ctrl Pts',(-1.35664255828353,-8.18841571891282,
37.3040910948304));
#80496=CARTESIAN_POINT('Ctrl Pts',(3.6485519661657,-6.93037645797473,37.515776162739));
#80497=CARTESIAN_POINT('Ctrl Pts',(7.53507082275758,-3.4964958267972,37.7274612306477));
#80498=CARTESIAN_POINT('Ctrl Pts',(8.03012496305131,2.11789381964731,37.9391462985564));
#80499=CARTESIAN_POINT('Ctrl Pts',(4.80762607306203,6.19290036212831,38.1508313664651));
#80500=CARTESIAN_POINT('Ctrl Pts',(1.27308148848372,7.75292181422578,38.3095951673966));
#80501=CARTESIAN_POINT('Ctrl Pts',(-2.58230775465909,7.4025023788475,38.4683589683282));
#80502=CARTESIAN_POINT('Ctrl Pts',(-6.92471323188677,4.57616838418209,38.6800440362368));
#80503=CARTESIAN_POINT('Ctrl Pts',(-8.60624687491617,-2.28884748864364,
38.9446503711227));
#80504=CARTESIAN_POINT('Ctrl Pts',(-2.72009775291531,-8.48675851570514,
39.2621779729857));
#80505=CARTESIAN_POINT('Ctrl Pts',(4.23473081663686,-7.13846523612135,39.5267843078716));
#80506=CARTESIAN_POINT('Ctrl Pts',(7.25409045900377,-2.95300201687236,39.7384693757802));
#80507=CARTESIAN_POINT('Ctrl Pts',(8.01649111349595,2.17684303476906,39.950154443689));
#80508=CARTESIAN_POINT('Ctrl Pts',(4.78003334023127,6.79114588414926,40.1618395115976));
#80509=CARTESIAN_POINT('Ctrl Pts',(-0.309456191810431,7.8338700665115,40.3735245795064));
#80510=CARTESIAN_POINT('Ctrl Pts',(-4.01823935838767,6.75146544037091,40.5322883804379));
#80511=CARTESIAN_POINT('Ctrl Pts',(-6.74232652089295,4.00079840710311,40.6910521813694));
#80512=CARTESIAN_POINT('Ctrl Pts',(-8.24473427658207,-0.957771962842544,
40.9027372492781));
#80513=CARTESIAN_POINT('Ctrl Pts',(-5.11073933877439,-7.29291790090763,
41.167343584164));
#80514=CARTESIAN_POINT('Ctrl Pts',(3.38367048796323,-8.24468167476436,41.4848711860269));
#80515=CARTESIAN_POINT('Ctrl Pts',(7.83656410693827,-2.7347566645924,41.7494775209129));
#80516=CARTESIAN_POINT('Ctrl Pts',(7.45154839830587,2.41173708491767,41.9611625888215));
#80517=CARTESIAN_POINT('Ctrl Pts',(4.73164358252729,6.82746837258959,42.1728476567303));
#80518=CARTESIAN_POINT('Ctrl Pts',(-0.715789675678205,8.27381570339301,
42.3845327246388));
#80519=CARTESIAN_POINT('Ctrl Pts',(-5.28115129402745,5.79437005749779,42.5962177925476));
#80520=CARTESIAN_POINT('Ctrl Pts',(-7.42173105642654,2.57806928919524,42.7549815934791));
#80521=CARTESIAN_POINT('Ctrl Pts',(-7.73469911131649,-1.28054069283851,
42.9137453944107));
#80522=CARTESIAN_POINT('Ctrl Pts',(-5.69125543650362,-6.04173666926352,
43.1254304623193));
#80523=CARTESIAN_POINT('Ctrl Pts',(0.785870231192877,-8.87066604477925,
43.3900367972052));
#80524=CARTESIAN_POINT('Ctrl Pts',(7.89773955776408,-4.12912966217305,43.7075643990682));
#80525=CARTESIAN_POINT('Ctrl Pts',(7.7566619832233,2.95378162610321,43.9721707339541));
#80526=CARTESIAN_POINT('Ctrl Pts',(4.14815708110641,6.64340591334962,44.1838558018628));
#80527=CARTESIAN_POINT('Ctrl Pts',(-0.776201107218263,8.27044661502238,
44.3955408697715));
#80528=CARTESIAN_POINT('Ctrl Pts',(-5.87532396071409,5.86932274714715,44.6072259376801));
#80529=CARTESIAN_POINT('Ctrl Pts',(-7.77168226861542,1.03258804434432,44.8189110055888));
#80530=CARTESIAN_POINT('Ctrl Pts',(-7.33838213262225,-2.80654250091254,
44.9776748065203));
#80531=CARTESIAN_POINT('Ctrl Pts',(-5.09319399126717,-5.96026255931195,
45.1364386074519));
#80532=CARTESIAN_POINT('Ctrl Pts',(-0.463939388580697,-8.28720282531922,
45.3481236753605));
#80533=CARTESIAN_POINT('Ctrl Pts',(6.31326617366714,-6.28084216635835,45.6127300102465));
#80534=CARTESIAN_POINT('Ctrl Pts',(8.70133206874304,1.92634942800435,45.9302576121094));
#80535=CARTESIAN_POINT('Ctrl Pts',(4.03256366223554,7.25458898399512,46.1948639469953));
#80536=CARTESIAN_POINT('Ctrl Pts',(-1.10410068062192,7.75390295181156,46.4065490149041));
#80537=CARTESIAN_POINT('Ctrl Pts',(-5.91937486901007,5.82784493023922,46.6182340828126));
#80538=CARTESIAN_POINT('Ctrl Pts',(-8.2745428830734,0.70733388841374,46.8299191507214));
#80539=CARTESIAN_POINT('Ctrl Pts',(-6.61096029045708,-4.21431932720265,
47.0416042186301));
#80540=CARTESIAN_POINT('Ctrl Pts',(-3.80735116212366,-6.87259850872246,
47.2003680195615));
#80541=CARTESIAN_POINT('Ctrl Pts',(-0.0588299049391507,-7.83976363488727,
47.3591318204932));
#80542=CARTESIAN_POINT('Ctrl Pts',(4.98134234603678,-6.63921673511537,47.5708168884017));
#80543=CARTESIAN_POINT('Ctrl Pts',(8.87459492999746,-0.740184386986363,
47.8354232232877));
#80544=CARTESIAN_POINT('Ctrl Pts',(5.41690820042068,7.07680064983623,48.1529508251507));
#80545=CARTESIAN_POINT('Ctrl Pts',(-1.58609358048459,8.14708157382943,48.4175571600365));
#80546=CARTESIAN_POINT('Ctrl Pts',(-5.83763537430491,5.22150002736057,48.6292422279453));
#80547=CARTESIAN_POINT('Ctrl Pts',(-8.28153749037398,0.647234243773531,
48.8409272958538));
#80548=CARTESIAN_POINT('Ctrl Pts',(-6.78625739001722,-4.78697104544792,
49.0526123637627));
#80549=CARTESIAN_POINT('Ctrl Pts',(-2.3443099628472,-7.48127623816482,49.2642974316713));
#80550=CARTESIAN_POINT('Ctrl Pts',(1.51243051798487,-7.70980460596024,49.4230612326029));
#80551=CARTESIAN_POINT('Ctrl Pts',(5.00317335353904,-6.03602611020303,49.5818250335343));
#80552=CARTESIAN_POINT('Ctrl Pts',(8.08631469576634,-1.87202699373947,49.7935101014431));
#80553=CARTESIAN_POINT('Ctrl Pts',(7.26650581480223,5.14822312470218,50.0581164363288));
#80554=CARTESIAN_POINT('Ctrl Pts',(-0.412460427341156,8.90246473091509,
50.375644038192));
#80555=CARTESIAN_POINT('Ctrl Pts',(-6.45958025795135,5.21195298403308,50.6402503730777));
#80556=CARTESIAN_POINT('Ctrl Pts',(-7.82856136876646,0.235958035496164,
50.8519354409865));
#80557=CARTESIAN_POINT('Ctrl Pts',(-6.75290952485123,-4.83745680290527,
51.0636205088951));
#80558=CARTESIAN_POINT('Ctrl Pts',(-2.10968633960191,-8.03228514819943,
51.2753055768039));
#80559=CARTESIAN_POINT('Ctrl Pts',(3.02373236434919,-7.23341730736144,51.4869906447125));
#80560=CARTESIAN_POINT('Ctrl Pts',(6.12164964500423,-4.924828804908,51.645754445644));
#80561=CARTESIAN_POINT('Ctrl Pts',(7.7146106921978,-1.39647294150067,51.8045182465756));
#80562=CARTESIAN_POINT('Ctrl Pts',(7.39221505707234,3.77466912120921,52.0162033144842));
#80563=CARTESIAN_POINT('Ctrl Pts',(2.24450322557626,8.61791815741794,52.2808096493702));
#80564=CARTESIAN_POINT('Ctrl Pts',(-6.04804895683927,6.54561728983433,52.5983372512331));
#80565=CARTESIAN_POINT('Ctrl Pts',(-8.29825919696842,-0.171829329049749,
52.8629435861191));
#80566=CARTESIAN_POINT('Ctrl Pts',(-6.14151175556086,-4.86044058214065,
53.0746286540277));
#80567=CARTESIAN_POINT('Ctrl Pts',(-2.05166332979347,-8.04943805234253,
53.2863137219364));
#80568=CARTESIAN_POINT('Ctrl Pts',(3.55804701210798,-7.50391115408883,53.4979987898451));
#80569=CARTESIAN_POINT('Ctrl Pts',(6.97117985135743,-3.58719038068351,53.7096838577538));
#80570=CARTESIAN_POINT('Ctrl Pts',(7.85482590827286,0.173905473015555,53.8684476586853));
#80571=CARTESIAN_POINT('Ctrl Pts',(6.8016081578469,3.89916416776701,54.0272114596168));
#80572=CARTESIAN_POINT('Ctrl Pts',(3.22514186305803,7.64796904632611,54.2388965275255));
#80573=CARTESIAN_POINT('Ctrl Pts',(-3.83200067505273,8.03878590459606,54.5035028624114));
#80574=CARTESIAN_POINT('Ctrl Pts',(-8.84217330287154,1.11354064511878,54.8210304642744));
#80575=CARTESIAN_POINT('Ctrl Pts',(-6.23829148347237,-5.4748836843946,55.0856367991602));
#80576=CARTESIAN_POINT('Ctrl Pts',(-1.56908770187694,-7.67333122518657,
55.297321867069));
#80577=CARTESIAN_POINT('Ctrl Pts',(3.61348493751562,-7.47967264937361,55.5090069349776));
#80578=CARTESIAN_POINT('Ctrl Pts',(7.55415678516325,-3.45008681937387,55.7206920028864));
#80579=CARTESIAN_POINT('Ctrl Pts',(7.64346206275794,1.74435207606906,55.932377070795));
#80580=CARTESIAN_POINT('Ctrl Pts',(5.89768786109866,5.19093705891806,56.0911408717265));
#80581=CARTESIAN_POINT('Ctrl Pts',(2.69310663716597,7.36291414668697,56.2499046726581));
#80582=CARTESIAN_POINT('Ctrl Pts',(-2.45714833322707,7.92814114052003,56.4615897405667));
#80583=CARTESIAN_POINT('Ctrl Pts',(-8.10817944768413,3.68290562380125,56.7261960754527));
#80584=CARTESIAN_POINT('Ctrl Pts',(-7.4821009522292,-4.84168401008916,57.0437236773156));
#80585=CARTESIAN_POINT('Ctrl Pts',(-1.24749925420084,-8.2057724583871,57.3083300122015));
#80586=CARTESIAN_POINT('Ctrl Pts',(3.74054184579962,-6.8811531701488,57.5200150801102));
#80587=CARTESIAN_POINT('Ctrl Pts',(7.58090054991324,-3.39590284033723,57.7317001480188));
#80588=CARTESIAN_POINT('Ctrl Pts',(8.00133886187132,2.22475810125255,57.9433852159276));
#80589=CARTESIAN_POINT('Ctrl Pts',(4.72457228532241,6.25622590654754,58.1550702838363));
#80590=CARTESIAN_POINT('Ctrl Pts',(1.17005802530752,7.76949200400492,58.3138340847677));
#80591=CARTESIAN_POINT('Ctrl Pts',(-2.68125956745956,7.36690301727387,58.4725978856994));
#80592=CARTESIAN_POINT('Ctrl Pts',(-6.98373096787359,4.4847496139812,58.6842829536079));
#80593=CARTESIAN_POINT('Ctrl Pts',(-8.57770848092659,-2.40573363485677,
58.9488892884939));
#80594=CARTESIAN_POINT('Ctrl Pts',(-2.60211601861391,-8.51788785161202,
59.2664168903568));
#80595=CARTESIAN_POINT('Ctrl Pts',(4.32147341265364,-7.08873519980074,59.5310232252428));
#80596=CARTESIAN_POINT('Ctrl Pts',(7.3034564296118,-2.84631579801383,59.7427082931514));
#80597=CARTESIAN_POINT('Ctrl Pts',(7.79380539571414,0.98044936741639,59.901472094083));
#80598=CARTESIAN_POINT('Ctrl Pts',(6.36418815772075,4.59868409180725,60.0603005433583));
#80599=CARTESIAN_POINT('Ctrl Pts',(4.38333064273928,6.25177260444803,60.1662077256567));
#80600=CARTESIAN_POINT('Ctrl Pts',(3.25252554956235,6.7931805456771,60.2191936409778));
#80601=CARTESIAN_POINT('Ctrl Pts',(4.14704588419467,-5.81932114679417,-60.2187981753814));
#80602=CARTESIAN_POINT('Ctrl Pts',(5.11514398602353,-5.1294285247336,-60.165844689447));
#80603=CARTESIAN_POINT('Ctrl Pts',(6.69695015326308,-3.2624304470734,-60.0599699365356));
#80604=CARTESIAN_POINT('Ctrl Pts',(7.44448710579558,0.351415371766862,-59.901173916647));
#80605=CARTESIAN_POINT('Ctrl Pts',(6.36363141587864,3.84858550951182,-59.7424101157154));
#80606=CARTESIAN_POINT('Ctrl Pts',(2.88618963684088,7.3289477836205,-59.5307250478067));
#80607=CARTESIAN_POINT('Ctrl Pts',(-3.81788569128896,7.53850476344882,-59.2661187129209));
#80608=CARTESIAN_POINT('Ctrl Pts',(-8.40907168959556,0.853298876947923,
-58.9485911110578));
#80609=CARTESIAN_POINT('Ctrl Pts',(-5.79824687200889,-5.32804406291944,
-58.683984776172));
#80610=CARTESIAN_POINT('Ctrl Pts',(-1.30780500871279,-7.32213393143249,
-58.4722997082633));
#80611=CARTESIAN_POINT('Ctrl Pts',(2.35757329727375,-7.07192733459881,-58.3135359073319));
#80612=CARTESIAN_POINT('Ctrl Pts',(5.4338632459131,-5.07922330288575,-58.1547721064002));
#80613=CARTESIAN_POINT('Ctrl Pts',(7.84088975156651,-0.777899090723996,
-57.9430870384916));
#80614=CARTESIAN_POINT('Ctrl Pts',(6.5335587623941,4.40742637312395,-57.7314019705828));
#80615=CARTESIAN_POINT('Ctrl Pts',(2.37695215273987,7.04041458569579,-57.5197169026742));
#80616=CARTESIAN_POINT('Ctrl Pts',(-2.50093072949188,7.46712779429702,-57.3080318347655));
#80617=CARTESIAN_POINT('Ctrl Pts',(-7.78125817105807,3.30844791921314,-57.0434254998796));
#80618=CARTESIAN_POINT('Ctrl Pts',(-6.97972648593816,-4.76146745484501,
-56.7258978980166));
#80619=CARTESIAN_POINT('Ctrl Pts',(-1.00702533288646,-7.81027475648936,
-56.4612915631308));
#80620=CARTESIAN_POINT('Ctrl Pts',(3.7150507761986,-6.44413077085018,-56.249606495222));
#80621=CARTESIAN_POINT('Ctrl Pts',(6.35709703780464,-3.89264454526949,-56.0908426942905));
#80622=CARTESIAN_POINT('Ctrl Pts',(7.42822665373128,-0.387073605132157,
-55.9320788933591));
#80623=CARTESIAN_POINT('Ctrl Pts',(6.49974656903945,4.45372245075779,-55.7203938254502));
#80624=CARTESIAN_POINT('Ctrl Pts',(2.16082594048462,7.57919118758771,-55.5087087575417));
#80625=CARTESIAN_POINT('Ctrl Pts',(-2.71490966702803,6.91713221250367,-55.2970236896329));
#80626=CARTESIAN_POINT('Ctrl Pts',(-6.72165560441165,4.10264625103405,-55.0853386217243));
#80627=CARTESIAN_POINT('Ctrl Pts',(-8.08377338813595,-2.47924397858112,
-54.8207322868384));
#80628=CARTESIAN_POINT('Ctrl Pts',(-2.27412232409216,-8.13735018118491,
-54.5032046849754));
#80629=CARTESIAN_POINT('Ctrl Pts',(4.25872376383168,-6.62402727327916,-54.2385983500895));
#80630=CARTESIAN_POINT('Ctrl Pts',(6.9918664875298,-2.53815891362137,-54.0269132821809));
#80631=CARTESIAN_POINT('Ctrl Pts',(7.37031945951809,1.11523115162059,-53.8681494812492));
#80632=CARTESIAN_POINT('Ctrl Pts',(5.93252554039144,4.48703956948173,-53.7093856803178));
#80633=CARTESIAN_POINT('Ctrl Pts',(2.10506424181126,7.5928289382194,-53.497700612409));
#80634=CARTESIAN_POINT('Ctrl Pts',(-3.22716385688535,7.19018222171262,-53.2860155445004));
#80635=CARTESIAN_POINT('Ctrl Pts',(-6.53123957473593,3.54406024958424,-53.0743304765917));
#80636=CARTESIAN_POINT('Ctrl Pts',(-7.78446579669849,-1.1893072397415,-52.862645408683));
#80637=CARTESIAN_POINT('Ctrl Pts',(-4.58839864462092,-7.10215749873455,
-52.5980390737971));
#80638=CARTESIAN_POINT('Ctrl Pts',(3.49989180946896,-7.69017930427037,-52.2805114719342));
#80639=CARTESIAN_POINT('Ctrl Pts',(7.52366382706956,-2.32571449231829,-52.0159051370482));
#80640=CARTESIAN_POINT('Ctrl Pts',(6.98379687578907,2.56027906868629,-51.8042200691396));
#80641=CARTESIAN_POINT('Ctrl Pts',(4.92085603590594,5.59915398115555,-51.6454562682081));
#80642=CARTESIAN_POINT('Ctrl Pts',(1.64963450172886,7.25307447927886,-51.4866924672765));
#80643=CARTESIAN_POINT('Ctrl Pts',(-3.27860852967551,7.1647102426091,-51.275007399368));
#80644=CARTESIAN_POINT('Ctrl Pts',(-7.09898380706795,3.4231178539073,-51.0633223314591));
#80645=CARTESIAN_POINT('Ctrl Pts',(-7.27909505938493,-1.49406444114012,
-50.8516372635505));
#80646=CARTESIAN_POINT('Ctrl Pts',(-5.19001718959643,-5.92250631241772,
-50.6399521956417));
#80647=CARTESIAN_POINT('Ctrl Pts',(1.06267466412245,-8.38837086787587,-50.3753458607559));
#80648=CARTESIAN_POINT('Ctrl Pts',(7.62960423514155,-3.63004678007801,-50.0578182588929));
#80649=CARTESIAN_POINT('Ctrl Pts',(7.2538737309012,3.06525385218751,-49.793211924007));
#80650=CARTESIAN_POINT('Ctrl Pts',(3.69463468840507,6.45585952690713,-49.5815268560984));
#80651=CARTESIAN_POINT('Ctrl Pts',(0.159500605525881,7.45251024740165,-49.4227630551668));
#80652=CARTESIAN_POINT('Ctrl Pts',(-3.4082795814312,6.61150615866358,-49.2639992542353));
#80653=CARTESIAN_POINT('Ctrl Pts',(-7.12194181390246,3.3705031598894,-49.0523141863267));
#80654=CARTESIAN_POINT('Ctrl Pts',(-7.63559463672009,-1.95217864920896,
-48.8406291184179));
#80655=CARTESIAN_POINT('Ctrl Pts',(-4.60712245387128,-5.83025523737004,
-48.6289440505092));
#80656=CARTESIAN_POINT('Ctrl Pts',(-0.157220624807248,-7.87322304549216,
-48.4172589826005));
#80657=CARTESIAN_POINT('Ctrl Pts',(6.21448746908153,-5.73360172626448,-48.1526526477148));
#80658=CARTESIAN_POINT('Ctrl Pts',(8.17481410019929,2.13553619440853,-47.8351250458516));
#80659=CARTESIAN_POINT('Ctrl Pts',(3.57610490332985,7.01611993929612,-47.5705187109658));
#80660=CARTESIAN_POINT('Ctrl Pts',(-1.33032231780475,7.31838030186149,-47.3588336430571));
#80661=CARTESIAN_POINT('Ctrl Pts',(-4.67679060281408,5.80456536600457,-47.2000698421256));
#80662=CARTESIAN_POINT('Ctrl Pts',(-6.86493277211707,2.86375303152355,-47.041306041194));
#80663=CARTESIAN_POINT('Ctrl Pts',(-7.61927996110144,-2.00721688558928,
-46.8296209732854));
#80664=CARTESIAN_POINT('Ctrl Pts',(-4.58488852524102,-6.41031232826053,
-46.6179359053767));
#80665=CARTESIAN_POINT('Ctrl Pts',(0.229345415595273,-7.4273046334583,-46.406250837468));
#80666=CARTESIAN_POINT('Ctrl Pts',(4.94944054879081,-6.12498144510814,-46.1945657695593));
#80667=CARTESIAN_POINT('Ctrl Pts',(8.44664080559815,-0.385100454424842,
-45.9299594346735));
#80668=CARTESIAN_POINT('Ctrl Pts',(4.87937362857974,6.89781221860719,-45.6124318328105));
#80669=CARTESIAN_POINT('Ctrl Pts',(-1.78177167135614,7.67070759404643,-45.3478254979245));
#80670=CARTESIAN_POINT('Ctrl Pts',(-5.73027393610722,4.74261619036305,-45.1361404300159));
#80671=CARTESIAN_POINT('Ctrl Pts',(-7.31585540537817,1.4295485715389,-44.9773766290843));
#80672=CARTESIAN_POINT('Ctrl Pts',(-7.09633753032112,-2.22943424370471,
-44.8186128281528));
#80673=CARTESIAN_POINT('Ctrl Pts',(-4.53696604659435,-6.4419163176408,-44.6069277602442));
#80674=CARTESIAN_POINT('Ctrl Pts',(0.61986701687461,-7.856785081452,-44.3952426923354));
#80675=CARTESIAN_POINT('Ctrl Pts',(4.95806336722576,-5.53489485757584,-44.1835576244268));
#80676=CARTESIAN_POINT('Ctrl Pts',(7.7307802805699,-1.4991316494842,-43.971872556518));
#80677=CARTESIAN_POINT('Ctrl Pts',(6.71043554017164,5.14432678977491,-43.7072662216322));
#80678=CARTESIAN_POINT('Ctrl Pts',(-0.708469794309639,8.41939255296942,
-43.3897386197692));
#80679=CARTESIAN_POINT('Ctrl Pts',(-6.3025451773241,4.72148171340279,-43.1251322848833));
#80680=CARTESIAN_POINT('Ctrl Pts',(-7.43805686993446,-0.0613001757296944,
-42.9134472169747));
#80681=CARTESIAN_POINT('Ctrl Pts',(-6.51782155574628,-3.61709159384154,
-42.7546834160431));
#80682=CARTESIAN_POINT('Ctrl Pts',(-3.99377642814695,-6.27519985603844,
-42.5959196151115));
#80683=CARTESIAN_POINT('Ctrl Pts',(0.676882598949729,-7.85010679536756,
-42.384234547203));
#80684=CARTESIAN_POINT('Ctrl Pts',(5.53339973265141,-5.61202230336168,-42.1725494792941));
#80685=CARTESIAN_POINT('Ctrl Pts',(7.35740874754137,-1.04210842019799,-41.9608644113856));
#80686=CARTESIAN_POINT('Ctrl Pts',(6.88008342736724,3.83103269124661,-41.7491793434768));
#80687=CARTESIAN_POINT('Ctrl Pts',(1.82156696023834,8.25687211165112,-41.484573008591));
#80688=CARTESIAN_POINT('Ctrl Pts',(-5.96346347643551,5.98541592336455,-41.1670454067279));
#80689=CARTESIAN_POINT('Ctrl Pts',(-7.8622883821109,-0.445967127412303,
-40.9024390718421));
#80690=CARTESIAN_POINT('Ctrl Pts',(-5.6513290697449,-4.83641679938568,-40.6907540039334));
#80691=CARTESIAN_POINT('Ctrl Pts',(-2.65761733188299,-6.96436784985291,
-40.5319902030019));
#80692=CARTESIAN_POINT('Ctrl Pts',(0.985120771138287,-7.37278240947874,
-40.3732264020704));
#80693=CARTESIAN_POINT('Ctrl Pts',(5.57272164211232,-5.57019930083024,-40.1615413341616));
#80694=CARTESIAN_POINT('Ctrl Pts',(7.84725821905841,-0.7306472323605,-39.949856266253));
#80695=CARTESIAN_POINT('Ctrl Pts',(6.30013309195742,3.94027619101359,-39.7381711983442));
#80696=CARTESIAN_POINT('Ctrl Pts',(2.79702013649338,7.36132038461744,-39.5264861304356));
#80697=CARTESIAN_POINT('Ctrl Pts',(-3.92310111230352,7.49021501169607,-39.2618797955497));
#80698=CARTESIAN_POINT('Ctrl Pts',(-8.4167325287651,0.739401074974589,-38.9443521936867));
#80699=CARTESIAN_POINT('Ctrl Pts',(-5.72821052238303,-5.40389391952402,
-38.6797458588009));
#80700=CARTESIAN_POINT('Ctrl Pts',(-1.20952206795488,-7.33931223474337,
-38.4680607908921));
#80701=CARTESIAN_POINT('Ctrl Pts',(2.45117539507621,-7.0396795817255,-38.3092969899607));
#80702=CARTESIAN_POINT('Ctrl Pts',(5.50119344928266,-5.00652114994202,-38.150533189029));
#80703=CARTESIAN_POINT('Ctrl Pts',(7.85041243277023,-0.673328587573193,
-37.9388481211205));
#80704=CARTESIAN_POINT('Ctrl Pts',(6.47435703709748,4.49399687259815,-37.7271630532117));
#80705=CARTESIAN_POINT('Ctrl Pts',(2.2829603690937,7.07145991935139,-37.5154779853031));
#80706=CARTESIAN_POINT('Ctrl Pts',(-2.60012518698035,7.43314929629184,-37.3037929173943));
#80707=CARTESIAN_POINT('Ctrl Pts',(-7.82463741168122,3.2045425000323,-37.0391865825085));
#80708=CARTESIAN_POINT('Ctrl Pts',(-6.91569433641548,-4.85399549399435,
-36.7216589806454));
#80709=CARTESIAN_POINT('Ctrl Pts',(-0.902933400911396,-7.82299025665549,
-36.4570526457596));
#80710=CARTESIAN_POINT('Ctrl Pts',(3.80053655161767,-6.39408864747288,-36.2453675778509));
#80711=CARTESIAN_POINT('Ctrl Pts',(6.40836913874791,-3.80764420768715,-36.0866037769195));
#80712=CARTESIAN_POINT('Ctrl Pts',(7.43272289327584,-0.288121125605982,
-35.9278399759878));
#80713=CARTESIAN_POINT('Ctrl Pts',(6.43986165812585,4.53988200018871,-35.7161549080792));
#80714=CARTESIAN_POINT('Ctrl Pts',(2.05970576400102,7.60729380926465,-35.5044698401705));
#80715=CARTESIAN_POINT('Ctrl Pts',(-2.80678139359286,6.88036566226147,-35.2927847722618));
#80716=CARTESIAN_POINT('Ctrl Pts',(-6.77569267976859,4.01277312569048,-35.0810997043531));
#80717=CARTESIAN_POINT('Ctrl Pts',(-8.05004163744785,-2.58667216595958,
-34.8164933694672));
#80718=CARTESIAN_POINT('Ctrl Pts',(-2.16555916694153,-8.16691214014953,
-34.4989657676043));
#80719=CARTESIAN_POINT('Ctrl Pts',(4.34655538185322,-6.56672837832442,-34.2343594327183));
#80720=CARTESIAN_POINT('Ctrl Pts',(7.02504606785724,-2.44482626303123,-34.0226743648097));
#80721=CARTESIAN_POINT('Ctrl Pts',(7.3548148961523,1.21327955316404,-33.8639105638781));
#80722=CARTESIAN_POINT('Ctrl Pts',(5.87224758552886,4.56564252712561,-33.7051467629467));
#80723=CARTESIAN_POINT('Ctrl Pts',(2.00376723902932,7.62018789815773,-33.4934616950379));
#80724=CARTESIAN_POINT('Ctrl Pts',(-3.32262618525587,7.14656995822387,-33.2817766271293));
#80725=CARTESIAN_POINT('Ctrl Pts',(-6.57785513861537,3.45677236931173,-33.0700915592206));
#80726=CARTESIAN_POINT('Ctrl Pts',(-7.76793807460959,-1.29286407559497,
-32.8584064913119));
#80727=CARTESIAN_POINT('Ctrl Pts',(-4.4934155018909,-7.1626294324194,-32.5938001564261));
#80728=CARTESIAN_POINT('Ctrl Pts',(3.60198819584529,-7.6428909090368,-32.2762725545629));
#80729=CARTESIAN_POINT('Ctrl Pts',(7.55396722120535,-2.22531896661211,-32.0116662196771));
#80730=CARTESIAN_POINT('Ctrl Pts',(6.94908352259376,2.65305218718735,-31.7999811517684));
#80731=CARTESIAN_POINT('Ctrl Pts',(4.84585824796351,5.66418637329614,-31.6412173508369));
#80732=CARTESIAN_POINT('Ctrl Pts',(1.55290224233197,7.27439880794334,-31.4824535499054));
#80733=CARTESIAN_POINT('Ctrl Pts',(-3.37372709777454,7.12041517196706,-31.2707684819967));
#80734=CARTESIAN_POINT('Ctrl Pts',(-7.14393849288627,3.32828029838134,-31.059083414088));
#80735=CARTESIAN_POINT('Ctrl Pts',(-7.25855383130227,-1.59086445555011,
-30.8473983461793));
#80736=CARTESIAN_POINT('Ctrl Pts',(-5.11068959523401,-5.99109433326673,
-30.6357132782707));
#80737=CARTESIAN_POINT('Ctrl Pts',(1.1742846652758,-8.37347590810965,-30.3711069433848));
#80738=CARTESIAN_POINT('Ctrl Pts',(7.67726745228539,-3.52812483856874,-30.0535793415218));
#80739=CARTESIAN_POINT('Ctrl Pts',(7.21241190414664,3.16157868906219,-29.7889730066358));
#80740=CARTESIAN_POINT('Ctrl Pts',(3.60833725949656,6.50448690779315,-29.5772879387272));
#80741=CARTESIAN_POINT('Ctrl Pts',(0.0602446772548879,7.45397343768087,
-29.4185241377956));
#80742=CARTESIAN_POINT('Ctrl Pts',(-3.49601987738074,6.56553336814352,-29.2597603368642));
#80743=CARTESIAN_POINT('Ctrl Pts',(-7.16619381742337,3.2753645480404,-29.0480752689555));
#80744=CARTESIAN_POINT('Ctrl Pts',(-7.60892129361871,-2.05368539028039,
-28.8363902010468));
#80745=CARTESIAN_POINT('Ctrl Pts',(-4.52907501116952,-5.89108928646016,
-28.6247051331381));
#80746=CARTESIAN_POINT('Ctrl Pts',(-0.0523624522946749,-7.87461856997043,
-28.4130200652294));
#80747=CARTESIAN_POINT('Ctrl Pts',(6.290288275216,-5.65033774861951,-28.1484137303435));
#80748=CARTESIAN_POINT('Ctrl Pts',(8.14565125349276,2.24420722459355,-27.8308861284805));
#80749=CARTESIAN_POINT('Ctrl Pts',(3.48235724405825,7.06311923352307,-27.5662797935946));
#80750=CARTESIAN_POINT('Ctrl Pts',(-1.42765999532561,7.30001607187756,-27.354594725686));
#80751=CARTESIAN_POINT('Ctrl Pts',(-4.7536727468681,5.74177192567531,-27.1958309247544));
#80752=CARTESIAN_POINT('Ctrl Pts',(-6.90245939693678,2.77208182867794,-27.0370671238229));
#80753=CARTESIAN_POINT('Ctrl Pts',(-7.59187514474007,-2.1085014911341,-26.8253820559143));
#80754=CARTESIAN_POINT('Ctrl Pts',(-4.49911869007206,-6.47079886469823,
-26.6136969880055));
#80755=CARTESIAN_POINT('Ctrl Pts',(0.32823121314369,-7.42359196808149,-26.4020119200969));
#80756=CARTESIAN_POINT('Ctrl Pts',(5.030565356491,-6.05852883487454,-26.1903268521881));
#80757=CARTESIAN_POINT('Ctrl Pts',(8.45102006051422,-0.272586125069461,
-25.9257205173023));
#80758=CARTESIAN_POINT('Ctrl Pts',(4.78708586102741,6.96217705675442,-25.6081929154392));
#80759=CARTESIAN_POINT('Ctrl Pts',(-1.88376110602854,7.6463003719199,-25.3435865805534));
#80760=CARTESIAN_POINT('Ctrl Pts',(-5.79292116067826,4.66588814033186,-25.1319015126447));
#80761=CARTESIAN_POINT('Ctrl Pts',(-7.33424338023445,1.33199980115504,-24.9731377117132));
#80762=CARTESIAN_POINT('Ctrl Pts',(-7.0660199125409,-2.32373535214808,-24.8143739107817));
#80763=CARTESIAN_POINT('Ctrl Pts',(-4.45077960431779,-6.5017618893055,-24.602688842873));
#80764=CARTESIAN_POINT('Ctrl Pts',(0.724437388474664,-7.84783393076815,
-24.3910037749643));
#80765=CARTESIAN_POINT('Ctrl Pts',(5.03132948803849,-5.4683797436389,-24.1793187070556));
#80766=CARTESIAN_POINT('Ctrl Pts',(7.75005807142993,-1.39605133802358,-23.9676336391469));
#80767=CARTESIAN_POINT('Ctrl Pts',(6.64133580419396,5.23323055050373,-23.7030273042611));
#80768=CARTESIAN_POINT('Ctrl Pts',(-0.820524304628543,8.40921163224948,
-23.385499702398));
#80769=CARTESIAN_POINT('Ctrl Pts',(-6.36486022052054,4.63713485413607,-23.1208933675121));
#80770=CARTESIAN_POINT('Ctrl Pts',(-7.43658103535925,-0.160344056511672,
-22.9092082996035));
#80771=CARTESIAN_POINT('Ctrl Pts',(-6.46907641488485,-3.70356581812319,
-22.7504444986719));
#80772=CARTESIAN_POINT('Ctrl Pts',(-3.90985823955037,-6.3278267942373,-22.5916806977405));
#80773=CARTESIAN_POINT('Ctrl Pts',(0.781358983234233,-7.84039698553307,
-22.3799956298317));
#80774=CARTESIAN_POINT('Ctrl Pts',(5.60764191090731,-5.53783885046969,-22.168310561923));
#80775=CARTESIAN_POINT('Ctrl Pts',(7.37063366861889,-0.944040656363546,
-21.9566254940144));
#80776=CARTESIAN_POINT('Ctrl Pts',(6.82845720595584,3.92231202677236,-21.7449404261057));
#80777=CARTESIAN_POINT('Ctrl Pts',(1.71145232624966,8.28039698286071,-21.4803340912198));
#80778=CARTESIAN_POINT('Ctrl Pts',(-6.04263983906747,5.90547239310807,-21.1628064893568));
#80779=CARTESIAN_POINT('Ctrl Pts',(-7.85565249142942,-0.550626203615014,
-20.8982001544709));
#80780=CARTESIAN_POINT('Ctrl Pts',(-5.58642354525344,-4.9112442094607,-20.6865150865622));
#80781=CARTESIAN_POINT('Ctrl Pts',(-2.56464027395697,-6.99914063982059,
-20.5277512856307));
#80782=CARTESIAN_POINT('Ctrl Pts',(1.0832135062605,-7.35901025214003,-20.3689874846992));
#80783=CARTESIAN_POINT('Ctrl Pts',(5.64640339528061,-5.49549592386352,-20.1573024167905));
#80784=CARTESIAN_POINT('Ctrl Pts',(7.85629211453692,-0.626083976636307,
-19.9456173488818));
#80785=CARTESIAN_POINT('Ctrl Pts',(6.24710354692251,4.0238228976775,-19.7339322809731));
#80786=CARTESIAN_POINT('Ctrl Pts',(2.69874467633993,7.39791434262794,-19.5222472130645));
#80787=CARTESIAN_POINT('Ctrl Pts',(-4.02249713685988,7.43730865587472,-19.2576408781786));
#80788=CARTESIAN_POINT('Ctrl Pts',(-8.42583250041413,0.627253605339702,
-18.9401132763156));
#80789=CARTESIAN_POINT('Ctrl Pts',(-5.65574133884476,-5.47969480813399,
-18.6755069414297));
#80790=CARTESIAN_POINT('Ctrl Pts',(-1.11168044293459,-7.35476813398764,
-18.463821873521));
#80791=CARTESIAN_POINT('Ctrl Pts',(2.54470235302645,-7.00641415884697,-18.3050580725895));
#80792=CARTESIAN_POINT('Ctrl Pts',(5.56737529197671,-4.93282026325047,-18.146294271658));
#80793=CARTESIAN_POINT('Ctrl Pts',(7.85868276150516,-0.568728410982657,
-17.9346092037493));
#80794=CARTESIAN_POINT('Ctrl Pts',(6.41393839013896,4.57981454452449,-17.7229241358406));
#80795=CARTESIAN_POINT('Ctrl Pts',(2.18859043397245,7.10123407234051,-17.5112390679319));
#80796=CARTESIAN_POINT('Ctrl Pts',(-2.69887859996051,7.39786548617967,-17.2995540000232));
#80797=CARTESIAN_POINT('Ctrl Pts',(-7.86661708291787,3.10006111706502,-17.0349476651374));
#80798=CARTESIAN_POINT('Ctrl Pts',(-6.85044261384541,-4.94565833887236,
-16.7174200632743));
#80799=CARTESIAN_POINT('Ctrl Pts',(-0.798678034425534,-7.83432056272497,
-16.4528137283885));
#80800=CARTESIAN_POINT('Ctrl Pts',(3.88534681350714,-6.34291162248799,-16.2411286604798));
#80801=CARTESIAN_POINT('Ctrl Pts',(6.45850562839871,-3.72196916681638,-16.0823648595482));
#80802=CARTESIAN_POINT('Ctrl Pts',(7.43590062071016,-0.189117292095101,
-15.9236010586167));
#80803=CARTESIAN_POINT('Ctrl Pts',(6.37883503788212,4.62523624379607,-15.7119159907081));
#80804=CARTESIAN_POINT('Ctrl Pts',(1.9582201615972,7.6340474673302,-15.5002309227993));
#80805=CARTESIAN_POINT('Ctrl Pts',(-2.898155307152,6.84237891770634,-15.2885458548907));
#80806=CARTESIAN_POINT('Ctrl Pts',(-6.82852821024978,3.9221884109201,-15.076860786982));
#80807=CARTESIAN_POINT('Ctrl Pts',(-8.01488227586511,-2.69364165449249,
-14.8122544520961));
#80808=CARTESIAN_POINT('Ctrl Pts',(-2.05661198859221,-8.19502578024167,
-14.4947268502331));
#80809=CARTESIAN_POINT('Ctrl Pts',(4.43361619564124,-6.50826495403781,-14.2301205153472));
#80810=CARTESIAN_POINT('Ctrl Pts',(7.05697983290556,-2.35106004812461,-14.0184354474385));
#80811=CARTESIAN_POINT('Ctrl Pts',(7.33800604231056,1.31111279217438,-13.859671646507));
#80812=CARTESIAN_POINT('Ctrl Pts',(5.81092825366935,4.64343582080709,-13.7009078455755));
#80813=CARTESIAN_POINT('Ctrl Pts',(1.90211489177139,7.64619550429748,-13.4892227776668));
#80814=CARTESIAN_POINT('Ctrl Pts',(-3.41749928418853,7.10169033240024,-13.2775377097581));
#80815=CARTESIAN_POINT('Ctrl Pts',(-6.62330419485259,3.36887146983878,-13.0658526418494));
#80816=CARTESIAN_POINT('Ctrl Pts',(-7.7500327975144,-1.39619163669753,-12.8541675739407));
#80817=CARTESIAN_POINT('Ctrl Pts',(-4.3976355031666,-7.22183115560607,-12.5895612390549));
#80818=CARTESIAN_POINT('Ctrl Pts',(3.70344581070873,-7.59424713435049,-12.2720336371918));
#80819=CARTESIAN_POINT('Ctrl Pts',(7.58293100553107,-2.12452880600961,-12.007427302306));
#80820=CARTESIAN_POINT('Ctrl Pts',(6.91313782877864,2.74535481718361,-11.7957422343973));
#80821=CARTESIAN_POINT('Ctrl Pts',(4.77000110240001,5.7282142866597,-11.6369784334658));
#80822=CARTESIAN_POINT('Ctrl Pts',(1.45589459345264,7.29443310504678,-11.4782146325342));
#80823=CARTESIAN_POINT('Ctrl Pts',(-3.46824737389549,7.07485737700085,-11.2665295646256));
#80824=CARTESIAN_POINT('Ctrl Pts',(-7.18762628279014,3.23285251035057,-11.0548444967169));
#80825=CARTESIAN_POINT('Ctrl Pts',(-7.23672538158249,-1.68738234831527,
-10.8431594288082));
#80826=CARTESIAN_POINT('Ctrl Pts',(-5.03045567843081,-6.05861990194769,
-10.6314743608995));
#80827=CARTESIAN_POINT('Ctrl Pts',(1.28568642045295,-8.3570960080076,-10.3668680260136));
#80828=CARTESIAN_POINT('Ctrl Pts',(7.72356919371295,-3.42557722440691,-10.0493404241506));
#80829=CARTESIAN_POINT('Ctrl Pts',(7.16967103849924,3.25734285605831,-9.78473408926473));
#80830=CARTESIAN_POINT('Ctrl Pts',(3.52139993317844,6.55196079220062,-9.57304902135602));
#80831=CARTESIAN_POINT('Ctrl Pts',(-0.0390219347217104,7.45411475088761,
-9.41428522042451));
#80832=CARTESIAN_POINT('Ctrl Pts',(-3.583140194126,6.51839625525219,-9.255521419493));
#80833=CARTESIAN_POINT('Ctrl Pts',(-7.20917497830124,3.17964508769009,-9.0438363515843));
#80834=CARTESIAN_POINT('Ctrl Pts',(-7.58089859521199,-2.15482793369875,
-8.83215128367564));
#80835=CARTESIAN_POINT('Ctrl Pts',(-4.45022438873187,-5.95087861813555,
-8.62046621576692));
#80836=CARTESIAN_POINT('Ctrl Pts',(0.0525050061010802,-7.87461762076525,
-8.40878114785824));
#80837=CARTESIAN_POINT('Ctrl Pts',(6.36497357055341,-5.5660717480959,-8.14417481297238));
#80838=CARTESIAN_POINT('Ctrl Pts',(8.11504386855144,2.35248027025413,-7.82664721110936));
#80839=CARTESIAN_POINT('Ctrl Pts',(3.38799202849415,7.10886596420688,-7.56204087622348));
#80840=CARTESIAN_POINT('Ctrl Pts',(-1.52474449364832,7.2803572674027,-7.3503558083148));
#80841=CARTESIAN_POINT('Ctrl Pts',(-4.82971188134325,5.67796024765845,-7.19159200738328));
#80842=CARTESIAN_POINT('Ctrl Pts',(-6.93876194940002,2.67991902877748,-7.03282820645175));
#80843=CARTESIAN_POINT('Ctrl Pts',(-7.56312399601624,-2.20941217802357,
-6.82114313854308));
#80844=CARTESIAN_POINT('Ctrl Pts',(-4.41255098757272,-6.53013787883321,
-6.60945807063438));
#80845=CARTESIAN_POINT('Ctrl Pts',(0.427058802627542,-7.41856281345515,
-6.39777300272569));
#80846=CARTESIAN_POINT('Ctrl Pts',(5.11079805088555,-5.99100181369613,-6.186087934817));
#80847=CARTESIAN_POINT('Ctrl Pts',(8.45390062348955,-0.160023455758246,
-5.92148159993113));
#80848=CARTESIAN_POINT('Ctrl Pts',(4.6939491585227,7.02530723244401,-5.60395399806812));
#80849=CARTESIAN_POINT('Ctrl Pts',(-1.98541647728356,7.62053716549387,-5.33934766318224));
#80850=CARTESIAN_POINT('Ctrl Pts',(-5.85454107668646,4.58833264865286,-5.12766259527357));
#80851=CARTESIAN_POINT('Ctrl Pts',(-7.35133071109141,1.23421481508714,-4.96889879434203));
#80852=CARTESIAN_POINT('Ctrl Pts',(-7.03444921622923,-2.41762437130216,
-4.81013499341053));
#80853=CARTESIAN_POINT('Ctrl Pts',(-4.36380386843999,-6.56045445084411,
-4.59844992550183));
#80854=CARTESIAN_POINT('Ctrl Pts',(0.82887929194248,-7.83749105040353,-4.38676485759314));
#80855=CARTESIAN_POINT('Ctrl Pts',(5.10370335701861,-5.40089488195087,-4.17507978968447));
#80856=CARTESIAN_POINT('Ctrl Pts',(7.7679614850053,-1.29272343653906,-3.96339472177576));
#80857=CARTESIAN_POINT('Ctrl Pts',(6.57105828821083,5.32120622293475,-3.69878838688992));
#80858=CARTESIAN_POINT('Ctrl Pts',(-0.932433277993894,8.39753949490707,
-3.38126078502686));
#80859=CARTESIAN_POINT('Ctrl Pts',(-6.42604657304033,4.55196554858829,-3.11665445014101));
#80860=CARTESIAN_POINT('Ctrl Pts',(-7.43378634629405,-0.259359358977234,
-2.90496938223232));
#80861=CARTESIAN_POINT('Ctrl Pts',(-6.41918419191598,-3.78938356951557,
-2.7462055813008));
#80862=CARTESIAN_POINT('Ctrl Pts',(-3.82524643111245,-6.37933098263298,
-2.58744178036929));
#80863=CARTESIAN_POINT('Ctrl Pts',(0.885696229427913,-7.82929809871447,
-2.37575671246058));
#80864=CARTESIAN_POINT('Ctrl Pts',(5.68089073662934,-5.4626707788536,-2.16407164455192));
#80865=CARTESIAN_POINT('Ctrl Pts',(7.38255020742661,-0.845808454586203,
-1.95238657664321));
#80866=CARTESIAN_POINT('Ctrl Pts',(6.775623039718,4.01290274686232,-1.74070150873454));
#80867=CARTESIAN_POINT('Ctrl Pts',(1.6010277902956,8.30243859911855,-1.47609517384866));
#80868=CARTESIAN_POINT('Ctrl Pts',(-6.12073333244397,5.82450772649672,-1.15856757198564));
#80869=CARTESIAN_POINT('Ctrl Pts',(-7.84764258678692,-0.655231887258009,
-0.893961237099761));
#80870=CARTESIAN_POINT('Ctrl Pts',(-5.52050089002332,-4.98513938774051,
-0.682276169191086));
#80871=CARTESIAN_POINT('Ctrl Pts',(-2.47126608679663,-7.03280588366045,
-0.523512368259554));
#80872=CARTESIAN_POINT('Ctrl Pts',(1.18122166265399,-7.34368389283164,-0.364748567328037));
#80873=CARTESIAN_POINT('Ctrl Pts',(5.71883850865417,-5.42038649664947,-0.153063499419362));
#80874=CARTESIAN_POINT('Ctrl Pts',(7.86440313102783,-0.520319605577109,
0.0586215684893359));
#80875=CARTESIAN_POINT('Ctrl Pts',(6.19241647359457,4.10538175951475,0.270306636398015));
#80876=CARTESIAN_POINT('Ctrl Pts',(2.601272284163,7.43617310821803,0.48199170430671));
#80877=CARTESIAN_POINT('Ctrl Pts',(-4.12386344860959,7.37678467612258,0.74659803919257));
#80878=CARTESIAN_POINT('Ctrl Pts',(-8.42894816866634,0.525894078781797,
1.06412564105561));
#80879=CARTESIAN_POINT('Ctrl Pts',(-5.02020791058217,-6.79126235295692,
1.38165324291864));
#80880=CARTESIAN_POINT('Ctrl Pts',(2.99431082191942,-7.90299339506185,1.69918084478167));
#80881=CARTESIAN_POINT('Ctrl Pts',(7.36643365261397,-2.79265881077084,1.96378717966754));
#80882=CARTESIAN_POINT('Ctrl Pts',(7.12687393130928,2.09948782826333,2.17547224757623));
#80883=CARTESIAN_POINT('Ctrl Pts',(4.66127205797912,6.35547888838997,2.38715731548491));
#80884=CARTESIAN_POINT('Ctrl Pts',(-0.470419877862721,7.86539311157671,
2.59884238339361));
#80885=CARTESIAN_POINT('Ctrl Pts',(-4.86213645379484,5.62890813913654,2.81052745130229));
#80886=CARTESIAN_POINT('Ctrl Pts',(-6.97398870797767,2.63267851626443,2.96929125223381));
#80887=CARTESIAN_POINT('Ctrl Pts',(-7.36810642574136,-1.01909395587376,
3.12805505316534));
#80888=CARTESIAN_POINT('Ctrl Pts',(-5.55045257799891,-5.58634936030821,
3.339740121074));
#80889=CARTESIAN_POINT('Ctrl Pts',(0.521240305046402,-8.43306440905713,
3.60434645595989));
#80890=CARTESIAN_POINT('Ctrl Pts',(7.3861046083072,-4.11573023807145,3.9218740578229));
#80891=CARTESIAN_POINT('Ctrl Pts',(7.43128453774611,2.60546850896112,4.18648039270878));
#80892=CARTESIAN_POINT('Ctrl Pts',(4.10208550089539,6.19599338688865,4.39816546061746));
#80893=CARTESIAN_POINT('Ctrl Pts',(-0.5272052621981,7.86354539703132,4.60985052852616));
#80894=CARTESIAN_POINT('Ctrl Pts',(-5.42403478710137,5.71508645233573,4.82153559643483));
#80895=CARTESIAN_POINT('Ctrl Pts',(-7.34480133401163,1.17569868955459,5.03322066434353));
#80896=CARTESIAN_POINT('Ctrl Pts',(-7.03084851288744,-2.476393085818,5.19198446527505));
#80897=CARTESIAN_POINT('Ctrl Pts',(-4.98112867333205,-5.52420164903002,
5.35074826620655));
#80898=CARTESIAN_POINT('Ctrl Pts',(-0.649401219666167,-7.84810441892272,
5.56243333411527));
#80899=CARTESIAN_POINT('Ctrl Pts',(5.82899312617974,-6.11644835843352,5.8270396690011));
#80900=CARTESIAN_POINT('Ctrl Pts',(8.30127062559556,1.60715546686924,6.14456727086416));
#80901=CARTESIAN_POINT('Ctrl Pts',(4.00789879630099,6.77857704496396,6.40917360575001));
#80902=CARTESIAN_POINT('Ctrl Pts',(-0.85124868288478,7.38192584372215,6.62085867365872));
#80903=CARTESIAN_POINT('Ctrl Pts',(-5.46686056367904,5.67686026101199,6.83254374156738));
#80904=CARTESIAN_POINT('Ctrl Pts',(-7.82994770275829,0.879923732992005,
7.04422880947609));
#80905=CARTESIAN_POINT('Ctrl Pts',(-6.37650933343722,-3.82994935958821,
7.25591387738476));
#80906=CARTESIAN_POINT('Ctrl Pts',(-3.78464912651592,-6.42197636423389,
7.41467767831628));
#80907=CARTESIAN_POINT('Ctrl Pts',(-0.253878226009082,-7.43397562275133,
7.5734414792478));
#80908=CARTESIAN_POINT('Ctrl Pts',(4.5567025757456,-6.42268844917267,7.78512654715649));
#80909=CARTESIAN_POINT('Ctrl Pts',(8.39822466880191,-0.926241234967016,
8.04973288204236));
#80910=CARTESIAN_POINT('Ctrl Pts',(5.31635972703513,6.57498003882823,8.36726048390539));
#80911=CARTESIAN_POINT('Ctrl Pts',(-1.29845070622145,7.76700619364757,8.63186681879125));
#80912=CARTESIAN_POINT('Ctrl Pts',(-5.40465655583919,5.09971969342482,8.84355188669994));
#80913=CARTESIAN_POINT('Ctrl Pts',(-7.83810008915857,0.823100192463282,
9.05523695460863));
#80914=CARTESIAN_POINT('Ctrl Pts',(-6.55723507065759,-4.36863994621369,
9.26692202251733));
#80915=CARTESIAN_POINT('Ctrl Pts',(-2.41243695628078,-7.03622990835402,
9.47860709042599));
#80916=CARTESIAN_POINT('Ctrl Pts',(1.23963488792975,-7.35041868027973,9.63737089135754));
#80917=CARTESIAN_POINT('Ctrl Pts',(4.59264817040183,-5.85115633826675,9.79613469228902));
#80918=CARTESIAN_POINT('Ctrl Pts',(7.62199901511133,-1.97979703400137,10.0078197601977));
#80919=CARTESIAN_POINT('Ctrl Pts',(7.0218443005315,4.69912790095596,10.2724260950835));
#80920=CARTESIAN_POINT('Ctrl Pts',(-0.166256785307518,8.4537803342726,10.5899536969466));
#80921=CARTESIAN_POINT('Ctrl Pts',(-5.99476856532561,5.10637927470297,10.8545600318324));
#80922=CARTESIAN_POINT('Ctrl Pts',(-7.41887568305574,0.421588706218421,
11.0662450997412));
#80923=CARTESIAN_POINT('Ctrl Pts',(-6.52688256694344,-4.41736469991614,
11.2779301676499));
#80924=CARTESIAN_POINT('Ctrl Pts',(-2.20383500679938,-7.56475102129884,
11.4896152355585));
#80925=CARTESIAN_POINT('Ctrl Pts',(2.68503450571567,-6.93678405994906,11.7013003034672));
#80926=CARTESIAN_POINT('Ctrl Pts',(5.68151982913352,-4.82552399869201,11.8600641043987));
#80927=CARTESIAN_POINT('Ctrl Pts',(7.28147953878471,-1.5193760028984,12.0188279053302));
#80928=CARTESIAN_POINT('Ctrl Pts',(7.10636594014363,3.39323273693023,12.230512973239));
#80929=CARTESIAN_POINT('Ctrl Pts',(2.34649610924198,8.1167762331949,12.4951193081248));
#80930=CARTESIAN_POINT('Ctrl Pts',(-5.57076336512423,6.36086777009108,12.8126469099879));
#80931=CARTESIAN_POINT('Ctrl Pts',(-7.8746541940651,0.0466987454495366,
13.0772532448737));
#80932=CARTESIAN_POINT('Ctrl Pts',(-5.94759568570367,-4.45461098158359,
13.2889383127824));
#80933=CARTESIAN_POINT('Ctrl Pts',(-2.14923767145121,-7.58248536868689,
13.5006233806911));
#80934=CARTESIAN_POINT('Ctrl Pts',(3.18495981430195,-7.20682854886377,13.7123084485998));
#80935=CARTESIAN_POINT('Ctrl Pts',(6.52103646492693,-3.57833296582929,13.9239935165085));
#80936=CARTESIAN_POINT('Ctrl Pts',(7.45414149692743,-0.0335257300303479,
14.08275731744));
#80937=CARTESIAN_POINT('Ctrl Pts',(6.54936255294715,3.52622997859995,14.2415211183715));
#80938=CARTESIAN_POINT('Ctrl Pts',(3.25205550737496,7.17207084872711,14.4532061862802));
#80939=CARTESIAN_POINT('Ctrl Pts',(-3.43127116601776,7.72104128959961,14.7178125211661));
#80940=CARTESIAN_POINT('Ctrl Pts',(-8.35804172035165,1.27952407544949,15.0353401230291));
#80941=CARTESIAN_POINT('Ctrl Pts',(-6.05490911427058,-5.03492155518401,
15.299946457915));
#80942=CARTESIAN_POINT('Ctrl Pts',(-1.6820459847554,-7.23796758372227,15.5116315258236));
#80943=CARTESIAN_POINT('Ctrl Pts',(3.23815133384991,-7.18524062741268,15.7233165937323));
#80944=CARTESIAN_POINT('Ctrl Pts',(7.07741272069182,-3.46302987749542,15.935001661641));
#80945=CARTESIAN_POINT('Ctrl Pts',(7.29335763733033,1.46127265260201,16.1466867295497));
#80946=CARTESIAN_POINT('Ctrl Pts',(5.72469563157511,4.7742234296914,16.3054505304812));
#80947=CARTESIAN_POINT('Ctrl Pts',(2.74025675908468,6.91516020105205,16.4642143314127));
#80948=CARTESIAN_POINT('Ctrl Pts',(-2.13011940355835,7.58136245069402,16.6758993993214));
#80949=CARTESIAN_POINT('Ctrl Pts',(-7.5969757573475,3.69784528512499,16.9405057342073));
#80950=CARTESIAN_POINT('Ctrl Pts',(-7.21858665341493,-4.40295923055548,
17.2580333360703));
#80951=CARTESIAN_POINT('Ctrl Pts',(-1.39047687177878,-7.75106015445512,
17.5226396709562));
#80952=CARTESIAN_POINT('Ctrl Pts',(3.37375416084809,-6.62081840107444,17.7343247388649));
#80953=CARTESIAN_POINT('Ctrl Pts',(7.10420825035649,-3.41226201665443,17.9460098067736));
#80954=CARTESIAN_POINT('Ctrl Pts',(7.64479092625569,1.90775219703075,18.1576948746822));
#80955=CARTESIAN_POINT('Ctrl Pts',(4.63914994657131,5.81435045077905,18.3693799425909));
#80956=CARTESIAN_POINT('Ctrl Pts',(1.30570185292558,7.3389707794797,18.5281437435225));
#80957=CARTESIAN_POINT('Ctrl Pts',(-2.356262780872,7.05524439118878,18.6869075444539));
#80958=CARTESIAN_POINT('Ctrl Pts',(-6.5115322538303,4.42881620633961,18.8985926123627));
#80959=CARTESIAN_POINT('Ctrl Pts',(-8.19350713659474,-2.06265392468485,
19.1631989472485));
#80960=CARTESIAN_POINT('Ctrl Pts',(-2.687731253583,-8.01686621862352,19.4807265491116));
#80961=CARTESIAN_POINT('Ctrl Pts',(3.92722227076492,-6.82563437967056,19.7453328839974));
#80962=CARTESIAN_POINT('Ctrl Pts',(6.84451397465846,-2.89310938067519,19.9570179519061));
#80963=CARTESIAN_POINT('Ctrl Pts',(7.63260152410329,1.96384849440906,20.1687030198148));
#80964=CARTESIAN_POINT('Ctrl Pts',(4.62053163586282,6.38224366139593,20.3803880877235));
#80965=CARTESIAN_POINT('Ctrl Pts',(-0.194600004819961,7.43575915622415,
20.5920731556322));
#80966=CARTESIAN_POINT('Ctrl Pts',(-3.72673024977302,6.45575952744647,20.7508369565637));
#80967=CARTESIAN_POINT('Ctrl Pts',(-6.34577470796605,3.88066889436112,20.9096007574952));
#80968=CARTESIAN_POINT('Ctrl Pts',(-7.83372953828914,-0.804454351188343,
21.1212858254039));
#80969=CARTESIAN_POINT('Ctrl Pts',(-4.9406059101558,-6.85408736820449,21.3858921602898));
#80970=CARTESIAN_POINT('Ctrl Pts',(3.10586062165327,-7.86432915496657,21.7034197621528));
#80971=CARTESIAN_POINT('Ctrl Pts',(7.39985345805689,-2.69342314689265,21.9680260970386));
#80972=CARTESIAN_POINT('Ctrl Pts',(7.09961841344044,2.19382584116961,22.1797111649474));
#80973=CARTESIAN_POINT('Ctrl Pts',(4.5750840659402,6.41731351301429,22.391396232856));
#80974=CARTESIAN_POINT('Ctrl Pts',(-0.574522753402311,7.85826128079608,
22.6030813007648));
#80975=CARTESIAN_POINT('Ctrl Pts',(-4.93692395375169,5.56373662803334,22.8147663686734));
#80976=CARTESIAN_POINT('Ctrl Pts',(-7.00828855729298,2.53953557338866,22.973530169605));
#80977=CARTESIAN_POINT('Ctrl Pts',(-7.35394645167502,-1.11710308289776,
23.1322939705364));
#80978=CARTESIAN_POINT('Ctrl Pts',(-5.47552313161862,-5.65978018277373,
23.3439790384452));
#80979=CARTESIAN_POINT('Ctrl Pts',(0.633466112297581,-8.42536771274805,
23.6085853733309));
#80980=CARTESIAN_POINT('Ctrl Pts',(7.44027256985801,-4.01701224108319,23.9261129751941));
#80981=CARTESIAN_POINT('Ctrl Pts',(7.3959224475177,2.70419869817981,24.1907193100799));
#80982=CARTESIAN_POINT('Ctrl Pts',(4.01921558372116,6.25006876197528,24.4024043779886));
#80983=CARTESIAN_POINT('Ctrl Pts',(-0.631876540752792,7.85582834410108,
24.6140894458972));
#80984=CARTESIAN_POINT('Ctrl Pts',(-5.49965773175034,5.64234982831051,24.825774513806));
#80985=CARTESIAN_POINT('Ctrl Pts',(-7.35980694503976,1.07778714178239,25.0374595817147));
#80986=CARTESIAN_POINT('Ctrl Pts',(-6.99724773323839,-2.56980030167315,
25.1962233826462));
#80987=CARTESIAN_POINT('Ctrl Pts',(-4.90712379803821,-5.59004326840594,
25.3549871835777));
#80988=CARTESIAN_POINT('Ctrl Pts',(-0.544833791248015,-7.85605635303897,
25.5666722514863));
#80989=CARTESIAN_POINT('Ctrl Pts',(5.90992624931247,-6.03828387359638,25.8312785863723));
#80990=CARTESIAN_POINT('Ctrl Pts',(8.27913281497273,1.71755730350853,26.1488061882353));
#80991=CARTESIAN_POINT('Ctrl Pts',(3.91727608688812,6.83134741526356,26.4134125231212));
#80992=CARTESIAN_POINT('Ctrl Pts',(-0.949475040141325,7.36993558899901,
26.6250975910298));
#80993=CARTESIAN_POINT('Ctrl Pts',(-5.54197206657227,5.60355713347054,26.8367826589385));
#80994=CARTESIAN_POINT('Ctrl Pts',(-7.84097097908883,0.775577756594261,
27.0484677268472));
#80995=CARTESIAN_POINT('Ctrl Pts',(-6.32494219125582,-3.91452291710228,
27.2601527947559));
#80996=CARTESIAN_POINT('Ctrl Pts',(-3.69879492243045,-6.47180543222624,
27.4189165956874));
#80997=CARTESIAN_POINT('Ctrl Pts',(-0.154860747096868,-7.43669724144609,
27.5776803966189));
#80998=CARTESIAN_POINT('Ctrl Pts',(4.6418266401032,-6.36143935956612,27.7893654645276));
#80999=CARTESIAN_POINT('Ctrl Pts',(8.40981434922058,-0.814323659296858,
28.0539717994135));
#81000=CARTESIAN_POINT('Ctrl Pts',(5.22833222578838,6.64519265300687,28.3714994012766));
#81001=CARTESIAN_POINT('Ctrl Pts',(-1.40176536255414,7.74902660450176,28.6361057361623));
#81002=CARTESIAN_POINT('Ctrl Pts',(-5.47208804219018,5.0272960820271,28.8477908040711));
#81003=CARTESIAN_POINT('Ctrl Pts',(-7.84836595190842,0.718650693773629,
29.0594758719798));
#81004=CARTESIAN_POINT('Ctrl Pts',(-6.49847839774445,-4.45557238359858,
29.2711609398884));
#81005=CARTESIAN_POINT('Ctrl Pts',(-2.3185246830527,-7.06773136765416,29.4828460077972));
#81006=CARTESIAN_POINT('Ctrl Pts',(1.33740724756926,-7.33325925390194,29.6416098087286));
#81007=CARTESIAN_POINT('Ctrl Pts',(4.67015820669236,-5.78947925433603,29.8003736096602));
#81008=CARTESIAN_POINT('Ctrl Pts',(7.64768726003397,-1.87812269432075,30.0120586775688));
#81009=CARTESIAN_POINT('Ctrl Pts',(6.95864546901471,4.79221802999488,30.2766650124548));
#81010=CARTESIAN_POINT('Ctrl Pts',(-0.278817300155773,8.45081677543235,
30.5941926143177));
#81011=CARTESIAN_POINT('Ctrl Pts',(-6.06223640958164,5.02609681196815,30.8587989492036));
#81012=CARTESIAN_POINT('Ctrl Pts',(-7.4238319670998,0.322757435410584,31.0704840171123));
#81013=CARTESIAN_POINT('Ctrl Pts',(-6.46747973936085,-4.50388862603115,
31.282169085021));
#81014=CARTESIAN_POINT('Ctrl Pts',(-2.10290314806414,-7.59342775703431,
31.4938541529297));
#81015=CARTESIAN_POINT('Ctrl Pts',(2.777170513354,-6.90041356231668,31.7055392208384));
#81016=CARTESIAN_POINT('Ctrl Pts',(5.74527542334076,-4.74943783418069,31.8643030217699));
#81017=CARTESIAN_POINT('Ctrl Pts',(7.30106675393053,-1.42227703580339,32.0230668227014));
#81018=CARTESIAN_POINT('Ctrl Pts',(7.06054964293635,3.4875641960886,32.2347518906101));
#81019=CARTESIAN_POINT('Ctrl Pts',(2.23820052505865,8.14730377610127,32.499358225496));
#81020=CARTESIAN_POINT('Ctrl Pts',(-5.6549742745155,6.28612036262135,32.8168858273589));
#81021=CARTESIAN_POINT('Ctrl Pts',(-7.87457782062009,-0.058168685139664,
33.0814921622449));
#81022=CARTESIAN_POINT('Ctrl Pts',(-5.88774823080518,-4.5334174977048,33.2931772301535));
#81023=CARTESIAN_POINT('Ctrl Pts',(-2.04807449335629,-7.61043348334377,
33.5048622980623));
#81024=CARTESIAN_POINT('Ctrl Pts',(3.28064755703563,-7.16377682217656,33.7165473659709));
#81025=CARTESIAN_POINT('Ctrl Pts',(6.56810932797811,-3.4911779168318,33.9282324338796));
#81026=CARTESIAN_POINT('Ctrl Pts',(7.45392699082019,0.0657407507670758,
34.0869962348112));
#81027=CARTESIAN_POINT('Ctrl Pts',(6.50182457934332,3.61313227703756,34.2457600357426));
#81028=CARTESIAN_POINT('Ctrl Pts',(3.15625985199202,7.21474109229927,34.4574451036513));
#81029=CARTESIAN_POINT('Ctrl Pts',(-3.53378461232003,7.67466394861541,34.7220514385372));
#81030=CARTESIAN_POINT('Ctrl Pts',(-8.37433947537304,1.16811027304956,35.0395790404002));
#81031=CARTESIAN_POINT('Ctrl Pts',(-5.98732440451525,-5.11510566108166,
35.3041853752861));
#81032=CARTESIAN_POINT('Ctrl Pts',(-1.5855120233048,-7.25972486130166,35.5158704431948));
#81033=CARTESIAN_POINT('Ctrl Pts',(3.33354688331943,-7.14148248695229,35.7275555111035));
#81034=CARTESIAN_POINT('Ctrl Pts',(7.12290080998369,-3.36847603562356,35.9392405790121));
#81035=CARTESIAN_POINT('Ctrl Pts',(7.27325181835091,1.55826550308438,36.1509256469209));
#81036=CARTESIAN_POINT('Ctrl Pts',(5.66061180334153,4.85003334448958,36.3096894478524));
#81037=CARTESIAN_POINT('Ctrl Pts',(2.64792765009157,6.95103782695821,36.4684532487839));
#81038=CARTESIAN_POINT('Ctrl Pts',(-2.23088818069513,7.55232435793397,36.6801383166926));
#81039=CARTESIAN_POINT('Ctrl Pts',(-7.64554471036468,3.59635183098948,36.9447446515784));
#81040=CARTESIAN_POINT('Ctrl Pts',(-7.15931432419098,-4.49869555162702,
37.2622722534414));
#81041=CARTESIAN_POINT('Ctrl Pts',(-1.28713613654189,-7.76888923945637,
37.5268785883273));
#81042=CARTESIAN_POINT('Ctrl Pts',(3.46162152515911,-6.57530454461241,37.738563656236));
#81043=CARTESIAN_POINT('Ctrl Pts',(7.14901791054088,-3.31735585210594,37.9502487241447));
#81044=CARTESIAN_POINT('Ctrl Pts',(7.61870837515603,2.00938534028792,38.1619337920533));
#81045=CARTESIAN_POINT('Ctrl Pts',(4.56131146102861,5.87561240610175,38.3736188599621));
#81046=CARTESIAN_POINT('Ctrl Pts',(1.20785624672071,7.35570749269215,38.5323826608936));
#81047=CARTESIAN_POINT('Ctrl Pts',(-2.45000542434561,7.02324149752807,38.6911464618251));
#81048=CARTESIAN_POINT('Ctrl Pts',(-6.56993146907149,4.34171230897587,38.9028315297338));
#81049=CARTESIAN_POINT('Ctrl Pts',(-8.16531317336679,-2.17158034419366,
39.1674378646196));
#81050=CARTESIAN_POINT('Ctrl Pts',(-2.58073586983221,-8.05194669809458,
39.4849654664827));
#81051=CARTESIAN_POINT('Ctrl Pts',(4.01776800332386,-6.77273207209629,39.7495718013686));
#81052=CARTESIAN_POINT('Ctrl Pts',(6.88243333552675,-2.80170748292457,39.9612568692772));
#81053=CARTESIAN_POINT('Ctrl Pts',(7.60577304422771,2.06531434276588,40.172941937186));
#81054=CARTESIAN_POINT('Ctrl Pts',(4.53513241827669,6.44320733021469,40.3846270050946));
#81055=CARTESIAN_POINT('Ctrl Pts',(-0.293601468362634,7.43250843047103,
40.5963120730034));
#81056=CARTESIAN_POINT('Ctrl Pts',(-3.81236829986945,6.4055598800527,40.7550758739348));
#81057=CARTESIAN_POINT('Ctrl Pts',(-6.39688918530141,3.79582092081505,40.9138396748664));
#81058=CARTESIAN_POINT('Ctrl Pts',(-7.82232236396769,-0.908701335081412,
41.125524742775));
#81059=CARTESIAN_POINT('Ctrl Pts',(-4.8488949776899,-6.91927148663638,41.3901310776609));
#81060=CARTESIAN_POINT('Ctrl Pts',(3.21031102305723,-7.82227245715925,41.7076586795239));
#81061=CARTESIAN_POINT('Ctrl Pts',(7.43506444403943,-2.59464374470073,41.9722650144098));
#81062=CARTESIAN_POINT('Ctrl Pts',(7.06977468610669,2.28817379705533,42.1839500823185));
#81063=CARTESIAN_POINT('Ctrl Pts',(4.48922186844248,6.47766886701024,42.3956351502272));
#81064=CARTESIAN_POINT('Ctrl Pts',(-0.679116803540349,7.84991382873632,
42.6073202181359));
#81065=CARTESIAN_POINT('Ctrl Pts',(-5.01057602209241,5.49750046094407,42.8190052860445));
#81066=CARTESIAN_POINT('Ctrl Pts',(-7.04148501024886,2.44598411303715,42.9777690869761));
#81067=CARTESIAN_POINT('Ctrl Pts',(-7.33841841438875,-1.21493328511627,
43.1365328879076));
#81068=CARTESIAN_POINT('Ctrl Pts',(-5.3996688294086,-5.73219345581792,43.3482179558163));
#81069=CARTESIAN_POINT('Ctrl Pts',(0.745606841701872,-8.41618505310172,
43.6128242907021));
#81070=CARTESIAN_POINT('Ctrl Pts',(7.49310562293818,-3.91757723373606,43.9303518925652));
#81071=CARTESIAN_POINT('Ctrl Pts',(7.35925603732857,2.80244714954233,44.1949582274511));
#81072=CARTESIAN_POINT('Ctrl Pts',(3.93562979912596,6.30303669052284,44.4066432953597));
#81073=CARTESIAN_POINT('Ctrl Pts',(-0.736433107028406,7.84671735272832,
44.6183283632685));
#81074=CARTESIAN_POINT('Ctrl Pts',(-5.57430676013242,5.56861301361288,44.8300134311771));
#81075=CARTESIAN_POINT('Ctrl Pts',(-7.37350677123859,0.979684278604959,
45.0416984990858));
#81076=CARTESIAN_POINT('Ctrl Pts',(-6.96240639730474,-2.66275169506281,
45.2004623000174));
#81077=CARTESIAN_POINT('Ctrl Pts',(-4.83224855106344,-5.65489360224126,
45.3592261009488));
#81078=CARTESIAN_POINT('Ctrl Pts',(-0.440169850607679,-7.86261507291464,
45.5709111688576));
#81079=CARTESIAN_POINT('Ctrl Pts',(5.98981137818155,-5.95904858716997,45.8355175037433));
#81080=CARTESIAN_POINT('Ctrl Pts',(8.2555267585719,1.82765456180822,46.1530451056065));
#81081=CARTESIAN_POINT('Ctrl Pts',(3.82595871025544,6.88290631901628,46.4176514404922));
#81082=CARTESIAN_POINT('Ctrl Pts',(-1.04753302609511,7.35663836253256,46.629336508401));
#81083=CARTESIAN_POINT('Ctrl Pts',(-5.61610075779896,5.52926027719673,46.8410215763096));
#81084=CARTESIAN_POINT('Ctrl Pts',(-7.85060375198737,0.671094241308602,
47.0527066442183));
#81085=CARTESIAN_POINT('Ctrl Pts',(-6.27225339138328,-3.998402279102,47.264391712127));
#81086=CARTESIAN_POINT('Ctrl Pts',(-3.61228478006291,-6.52048679919805,
47.4231555130585));
#81087=CARTESIAN_POINT('Ctrl Pts',(-0.0558158050509224,-7.43810004690919,
47.5819193139901));
#81088=CARTESIAN_POINT('Ctrl Pts',(4.72612752925907,-6.29906214125468,47.7936043818987));
#81089=CARTESIAN_POINT('Ctrl Pts',(8.41991264524431,-0.702261672669268,
48.0582107167846));
#81090=CARTESIAN_POINT('Ctrl Pts',(5.1393775394395,6.71422681817487,48.3757383186477));
#81091=CARTESIAN_POINT('Ctrl Pts',(-1.50483143176698,7.72967281396177,48.6403446535335));
#81092=CARTESIAN_POINT('Ctrl Pts',(-5.53854911622968,4.95398093708056,48.8520297214422));
#81093=CARTESIAN_POINT('Ctrl Pts',(-7.85723999656229,0.61407375058509,49.0637147893509));
#81094=CARTESIAN_POINT('Ctrl Pts',(-6.43856929390096,-4.54171467609673,
49.2753998572596));
#81095=CARTESIAN_POINT('Ctrl Pts',(-2.22420124594441,-7.09797944550326,
49.4870849251683));
#81096=CARTESIAN_POINT('Ctrl Pts',(1.43494243330327,-7.31479935773328,49.6458487260998));
#81097=CARTESIAN_POINT('Ctrl Pts',(4.74684004375429,-5.72677547236965,49.8046125270314));
#81098=CARTESIAN_POINT('Ctrl Pts',(7.67201927494928,-1.77611529102583,50.01629759494));
#81099=CARTESIAN_POINT('Ctrl Pts',(6.89421260118454,4.88445831388825,50.2809039298258));
#81100=CARTESIAN_POINT('Ctrl Pts',(-0.391328369939513,8.4463545607366,50.598431531689));
#81101=CARTESIAN_POINT('Ctrl Pts',(-6.12862918543473,4.94492302835666,50.8630378665747));
#81102=CARTESIAN_POINT('Ctrl Pts',(-7.42747171931677,0.223868927257572,
51.0747229344835));
#81103=CARTESIAN_POINT('Ctrl Pts',(-6.40692997809917,-4.58961383892871,
51.2864080023921));
#81104=CARTESIAN_POINT('Ctrl Pts',(-2.00159836346711,-7.62075788506456,
51.4980930703008));
#81105=CARTESIAN_POINT('Ctrl Pts',(2.86881402151197,-6.86281935513654,51.7097781382095));
#81106=CARTESIAN_POINT('Ctrl Pts',(5.80801215856054,-4.6725094110997,51.868541939141));
#81107=CARTESIAN_POINT('Ctrl Pts',(7.31935920825085,-1.32492584412404,52.0273057400726));
#81108=CARTESIAN_POINT('Ctrl Pts',(7.01348123788996,3.58127717557574,52.2389908079812));
#81109=CARTESIAN_POINT('Ctrl Pts',(2.12950802153738,8.17638648768663,52.5035971428671));
#81110=CARTESIAN_POINT('Ctrl Pts',(-5.73818233873579,6.21025818353877,52.8211247447302));
#81111=CARTESIAN_POINT('Ctrl Pts',(-7.873104980814,-0.163025800264569,53.0857310796159));
#81112=CARTESIAN_POINT('Ctrl Pts',(-5.82685665086243,-4.61142006388278,
53.2974161475247));
#81113=CARTESIAN_POINT('Ctrl Pts',(-1.94654811296497,-7.63703197482712,
53.5091012154332));
#81114=CARTESIAN_POINT('Ctrl Pts',(3.37575351505398,-7.11945468085971,53.7207862833422));
#81115=CARTESIAN_POINT('Ctrl Pts',(6.6140174110158,-3.40340374805446,53.9324713512506));
#81116=CARTESIAN_POINT('Ctrl Pts',(7.45239061759393,0.164995574769106,54.0912351521824));
#81117=CARTESIAN_POINT('Ctrl Pts',(6.45313357826351,3.6993938248483,54.2499989531137));
#81118=CARTESIAN_POINT('Ctrl Pts',(3.05990447673085,7.25613189013641,54.4616840210225));
#81119=CARTESIAN_POINT('Ctrl Pts',(-3.63567139626818,7.62692558076465,54.7262903559084));
#81120=CARTESIAN_POINT('Ctrl Pts',(-8.38915211246843,1.05648934208145,55.0438179577714));
#81121=CARTESIAN_POINT('Ctrl Pts',(-5.91867795214696,-5.19438269905205,
55.3084242926573));
#81122=CARTESIAN_POINT('Ctrl Pts',(-1.48869683481292,-7.280194659444,55.5201093605659));
#81123=CARTESIAN_POINT('Ctrl Pts',(3.42835112574471,-7.09645801521317,55.7317944284747));
#81124=CARTESIAN_POINT('Ctrl Pts',(7.16712601997843,-3.27332457050499,55.9434794963832));
#81125=CARTESIAN_POINT('Ctrl Pts',(7.25185581801874,1.65498168861816,56.155164564292));
#81126=CARTESIAN_POINT('Ctrl Pts',(5.59552486519911,4.92498383619882,56.3139283652234));
#81127=CARTESIAN_POINT('Ctrl Pts',(2.55512762082478,6.98568153459991,56.4726921661551));
#81128=CARTESIAN_POINT('Ctrl Pts',(-2.33125843887759,7.52194960659085,56.6843772340637));
#81129=CARTESIAN_POINT('Ctrl Pts',(-7.69276380499366,3.49421510251371,56.9489835689495));
#81130=CARTESIAN_POINT('Ctrl Pts',(-7.09876190604784,-4.59362446876616,
57.2665111708127));
#81131=CARTESIAN_POINT('Ctrl Pts',(-1.18358469634226,-7.78535672122115,
57.5311175056984));
#81132=CARTESIAN_POINT('Ctrl Pts',(3.54889838194794,-6.52860316985953,57.7428025736072));
#81133=CARTESIAN_POINT('Ctrl Pts',(7.19249959080346,-3.22191666131488,57.9544876415158));
#81134=CARTESIAN_POINT('Ctrl Pts',(7.59139710526208,2.11077452177849,58.1661727094246));
#81135=CARTESIAN_POINT('Ctrl Pts',(4.48251286310495,5.93569352038678,58.3778577773332));
#81136=CARTESIAN_POINT('Ctrl Pts',(1.11011110261031,7.37142872296306,58.5366215782647));
#81137=CARTESIAN_POINT('Ctrl Pts',(-2.54388752560662,6.98946603881242,58.6953853791963));
#81138=CARTESIAN_POINT('Ctrl Pts',(-6.62592548180662,4.2549773013165,58.9070704471049));
#81139=CARTESIAN_POINT('Ctrl Pts',(-8.13823691959708,-2.28247792862617,
59.1716767819908));
#81140=CARTESIAN_POINT('Ctrl Pts',(-2.46879882883055,-8.08148114908733,
59.4892043838539));
#81141=CARTESIAN_POINT('Ctrl Pts',(4.10006641658602,-6.72554991167464,59.7538107187397));
#81142=CARTESIAN_POINT('Ctrl Pts',(6.92927008283139,-2.70048724128809,59.9654957866484));
#81143=CARTESIAN_POINT('Ctrl Pts',(7.39449643883256,0.930216882217807,60.1242595875799));
#81144=CARTESIAN_POINT('Ctrl Pts',(6.03812441791351,4.36307444356796,60.2830880368553));
#81145=CARTESIAN_POINT('Ctrl Pts',(4.15875444436768,5.93146837941342,60.3889952191537));
#81146=CARTESIAN_POINT('Ctrl Pts',(3.08588518346614,6.44513774759855,60.4419811344748));
#81147=CARTESIAN_POINT('Ctrl Pts',(3.92310195780859,-5.50507296558183,-59.9960106818844));
#81148=CARTESIAN_POINT('Ctrl Pts',(4.83892195707862,-4.85243511881996,-59.94305719595));
#81149=CARTESIAN_POINT('Ctrl Pts',(6.33530927587413,-3.08625648992924,-59.8371824430386));
#81150=CARTESIAN_POINT('Ctrl Pts',(7.04247861132623,0.332438649457811,-59.6783864231499));
#81151=CARTESIAN_POINT('Ctrl Pts',(6.0199900274931,3.64075869155507,-59.5196226222184));
#81152=CARTESIAN_POINT('Ctrl Pts',(2.73033299632717,6.93317850862972,-59.3079375543098));
#81153=CARTESIAN_POINT('Ctrl Pts',(-3.61171668904582,7.1314192372823,-59.0433312194238));
#81154=CARTESIAN_POINT('Ctrl Pts',(-7.95497482546268,0.807220027998837,
-58.7258036175609));
#81155=CARTESIAN_POINT('Ctrl Pts',(-5.48513671916016,-5.04032525277668,
-58.461197282675));
#81156=CARTESIAN_POINT('Ctrl Pts',(-1.23718245068589,-6.92673261012629,
-58.2495122147664));
#81157=CARTESIAN_POINT('Ctrl Pts',(2.23026237868773,-6.69003737759096,-58.0907484138348));
#81158=CARTESIAN_POINT('Ctrl Pts',(5.14043011189061,-4.80494102070203,-57.9319846129032));
#81159=CARTESIAN_POINT('Ctrl Pts',(7.41747518458126,-0.735891892932647,
-57.7202995449947));
#81160=CARTESIAN_POINT('Ctrl Pts',(6.18074115598698,4.16942168380601,-57.5086144770858));
#81161=CARTESIAN_POINT('Ctrl Pts',(2.24859475984408,6.66022634333414,-57.2969294091773));
#81162=CARTESIAN_POINT('Ctrl Pts',(-2.36587839035156,7.06389668382096,-57.0852443412685));
#81163=CARTESIAN_POINT('Ctrl Pts',(-7.36106375900914,3.12978898030585,-56.8206380063827));
#81164=CARTESIAN_POINT('Ctrl Pts',(-6.60281545143133,-4.50434425269732,
-56.5031104045197));
#81165=CARTESIAN_POINT('Ctrl Pts',(-0.95264512747938,-7.38851342469737,
-56.2385040696336));
#81166=CARTESIAN_POINT('Ctrl Pts',(3.51443494488682,-6.09614235035376,-56.0268190017251));
#81167=CARTESIAN_POINT('Ctrl Pts',(6.01380851126865,-3.68243850274338,-55.8680552007936));
#81168=CARTESIAN_POINT('Ctrl Pts',(7.02709623719541,-0.366171308569067,
-55.709291399862));
#81169=CARTESIAN_POINT('Ctrl Pts',(6.14875484919133,4.21321773474829,-55.4976063319533));
#81170=CARTESIAN_POINT('Ctrl Pts',(2.04413954277891,7.16990856068301,-55.2859212640447));
#81171=CARTESIAN_POINT('Ctrl Pts',(-2.56830228731816,6.54360132081494,-55.0742361961359));
#81172=CARTESIAN_POINT('Ctrl Pts',(-6.35868061211583,3.88109994176148,-54.8625511282274));
#81173=CARTESIAN_POINT('Ctrl Pts',(-7.64724290279666,-2.34536274202442,
-54.5979447933414));
#81174=CARTESIAN_POINT('Ctrl Pts',(-2.15131782745559,-7.69792650446685,
-54.2804171914784));
#81175=CARTESIAN_POINT('Ctrl Pts',(4.02874913907503,-6.26632429205159,-54.0158108565925));
#81176=CARTESIAN_POINT('Ctrl Pts',(6.61429988284118,-2.40109622158015,-53.8041257886839));
#81177=CARTESIAN_POINT('Ctrl Pts',(6.97231607962482,1.05500774201836,-53.6453619877523));
#81178=CARTESIAN_POINT('Ctrl Pts',(5.61216422778529,4.244735701355,-53.4865981868208));
#81179=CARTESIAN_POINT('Ctrl Pts',(1.99138902220475,7.18280986143957,-53.2749131189121));
#81180=CARTESIAN_POINT('Ctrl Pts',(-3.05289432493803,6.80190640246115,-53.0632280510034));
#81181=CARTESIAN_POINT('Ctrl Pts',(-6.17854720639058,3.35267804890413,-52.8515429830947));
#81182=CARTESIAN_POINT('Ctrl Pts',(-7.36409817019778,-1.12508365977983,
-52.639857915186));
#81183=CARTESIAN_POINT('Ctrl Pts',(-4.34062130214816,-6.71863508772395,
-52.3752515803003));
#81184=CARTESIAN_POINT('Ctrl Pts',(3.31089474128444,-7.27490322676852,-52.057723978437));
#81185=CARTESIAN_POINT('Ctrl Pts',(7.11737972380877,-2.20012397569399,-51.7931176435514));
#81186=CARTESIAN_POINT('Ctrl Pts',(6.6066660368453,2.42202186987603,-51.5814325756425));
#81187=CARTESIAN_POINT('Ctrl Pts',(4.65512571783568,5.29679500997594,-51.422668774711));
#81188=CARTESIAN_POINT('Ctrl Pts',(1.56055286681731,6.86140242581805,-51.2639049737795));
#81189=CARTESIAN_POINT('Ctrl Pts',(-3.10156094261667,6.77780993141143,-51.052219905871));
#81190=CARTESIAN_POINT('Ctrl Pts',(-6.71563277804662,3.2382666431682,-50.8405348379621));
#81191=CARTESIAN_POINT('Ctrl Pts',(-6.88601787296009,-1.4133837188701,-50.6288497700535));
#81192=CARTESIAN_POINT('Ctrl Pts',(-4.90975194539534,-5.60268604645359,
-50.4171647021448));
#81193=CARTESIAN_POINT('Ctrl Pts',(1.0052893485505,-7.93539186533052,-50.152558367259));
#81194=CARTESIAN_POINT('Ctrl Pts',(7.2175992617459,-3.43402123524581,-49.8350307653958));
#81195=CARTESIAN_POINT('Ctrl Pts',(6.86215851718836,2.89972759513651,-49.5704244305101));
#81196=CARTESIAN_POINT('Ctrl Pts',(3.49512134281254,6.10723774382978,-49.3587393626013));
#81197=CARTESIAN_POINT('Ctrl Pts',(0.150887440188818,7.0500684966136,-49.1999755616699));
#81198=CARTESIAN_POINT('Ctrl Pts',(-3.22422964974452,6.25447932803763,-49.0412117607383));
#81199=CARTESIAN_POINT('Ctrl Pts',(-6.73735103342042,3.18849318638109,-48.8295266928297));
#81200=CARTESIAN_POINT('Ctrl Pts',(-7.2232661766579,-1.8467593787403,-48.6178416249209));
#81201=CARTESIAN_POINT('Ctrl Pts',(-4.35833401012841,-5.51541660617352,
-48.4061565570123));
#81202=CARTESIAN_POINT('Ctrl Pts',(-0.148730580325022,-7.44806245374694,
-48.1944714891035));
#81203=CARTESIAN_POINT('Ctrl Pts',(5.87889997784911,-5.4239824650442,-47.9298651542178));
#81204=CARTESIAN_POINT('Ctrl Pts',(7.73336734070007,2.02021546402088,-47.6123375523546));
#81205=CARTESIAN_POINT('Ctrl Pts',(3.38299226469952,6.63724362804317,-47.3477312174689));
#81206=CARTESIAN_POINT('Ctrl Pts',(-1.25848380636106,6.9231816796737,-47.1360461495601));
#81207=CARTESIAN_POINT('Ctrl Pts',(-4.42424002109247,5.49111400922566,-46.9772823486285));
#81208=CARTESIAN_POINT('Ctrl Pts',(-6.49422069361746,2.70910798635499,-46.8185185476971));
#81209=CARTESIAN_POINT('Ctrl Pts',(-7.20783250708978,-1.89882550458687,
-46.6068334797883));
#81210=CARTESIAN_POINT('Ctrl Pts',(-4.33730073213373,-6.06415013178661,
-46.3951484118797));
#81211=CARTESIAN_POINT('Ctrl Pts',(0.216960572431575,-7.02622400678393,
-46.183463343971));
#81212=CARTESIAN_POINT('Ctrl Pts',(4.68216664325364,-5.79422735360303,-45.9717782760624));
#81213=CARTESIAN_POINT('Ctrl Pts',(7.99051517795909,-0.364304709640845,
-45.7071719411764));
#81214=CARTESIAN_POINT('Ctrl Pts',(4.61588339500148,6.52532462265482,-45.3896443393135));
#81215=CARTESIAN_POINT('Ctrl Pts',(-1.68555451940014,7.25648300508906,-45.1250380044276));
#81216=CARTESIAN_POINT('Ctrl Pts',(-5.4208343783223,4.48651097217447,-44.9133529365189));
#81217=CARTESIAN_POINT('Ctrl Pts',(-6.92079312970003,1.35235175987873,-44.7545891355874));
#81218=CARTESIAN_POINT('Ctrl Pts',(-6.71312940244499,-2.1090429405705,-44.5958253346557));
#81219=CARTESIAN_POINT('Ctrl Pts',(-4.29196610718577,-6.09404747945881,
-44.3841402667472));
#81220=CARTESIAN_POINT('Ctrl Pts',(0.586393682488183,-7.43251215343463,
-44.1724551988384));
#81221=CARTESIAN_POINT('Ctrl Pts',(4.6903238223225,-5.23600593250722,-43.9607701309298));
#81222=CARTESIAN_POINT('Ctrl Pts',(7.3133117165843,-1.41817729375046,-43.7490850630211));
#81223=CARTESIAN_POINT('Ctrl Pts',(6.34806644067571,4.86652886515926,-43.4844787281352));
#81224=CARTESIAN_POINT('Ctrl Pts',(-0.67021183626058,7.9647383536317,-43.1669511262723));
#81225=CARTESIAN_POINT('Ctrl Pts',(-5.96220249661876,4.46651777454531,-42.9023447913863));
#81226=CARTESIAN_POINT('Ctrl Pts',(-7.03639561354893,-0.0579899152633749,
-42.6906597234777));
#81227=CARTESIAN_POINT('Ctrl Pts',(-6.16585377158498,-3.42176563983885,
-42.5318959225461));
#81228=CARTESIAN_POINT('Ctrl Pts',(-3.77810917984525,-5.93633384542265,
-42.3731321216146));
#81229=CARTESIAN_POINT('Ctrl Pts',(0.6403303757177,-7.42619450035234,-42.1614470537058));
#81230=CARTESIAN_POINT('Ctrl Pts',(5.23459154557155,-5.30896843208227,-41.9497619857972));
#81231=CARTESIAN_POINT('Ctrl Pts',(6.96010255683114,-0.985833698901345,
-41.7380769178885));
#81232=CARTESIAN_POINT('Ctrl Pts',(6.50855320088531,3.62415374007287,-41.5263918499799));
#81233=CARTESIAN_POINT('Ctrl Pts',(1.72320082959013,7.81099415129477,-41.2617855150938));
#81234=CARTESIAN_POINT('Ctrl Pts',(-5.64143148955485,5.66219848609485,-40.9442579132311));
#81235=CARTESIAN_POINT('Ctrl Pts',(-7.43771827128143,-0.421884531670146,
-40.679651578345));
#81236=CARTESIAN_POINT('Ctrl Pts',(-5.34615260039369,-4.57524627030576,
-40.4679665104363));
#81237=CARTESIAN_POINT('Ctrl Pts',(-2.51410378591528,-6.58828619446641,
-40.3092027095049));
#81238=CARTESIAN_POINT('Ctrl Pts',(0.931923430280503,-6.97464602823941,
-40.1504389085732));
#81239=CARTESIAN_POINT('Ctrl Pts',(5.2717900392219,-5.26940390646711,-39.9387538406647));
#81240=CARTESIAN_POINT('Ctrl Pts',(7.42349974953265,-0.691191674214921,
-39.7270687727558));
#81241=CARTESIAN_POINT('Ctrl Pts',(5.95992066586817,3.72749800000675,-39.5153837048473));
#81242=CARTESIAN_POINT('Ctrl Pts',(2.64597872315084,6.96380296225215,-39.3036986369385));
#81243=CARTESIAN_POINT('Ctrl Pts',(-3.71125038982958,7.08573717228143,-39.0390923020528));
#81244=CARTESIAN_POINT('Ctrl Pts',(-7.96222197294639,0.699472802048286,
-38.7215647001897));
#81245=CARTESIAN_POINT('Ctrl Pts',(-5.41888239065558,-5.11207915404871,
-38.4569583653038));
#81246=CARTESIAN_POINT('Ctrl Pts',(-1.14420687045995,-6.94298327077308,
-38.2452732973951));
#81247=CARTESIAN_POINT('Ctrl Pts',(2.31880988537035,-6.65953103018969,-38.0865094964637));
#81248=CARTESIAN_POINT('Ctrl Pts',(5.20412442828714,-4.73616484447559,-37.9277456955321));
#81249=CARTESIAN_POINT('Ctrl Pts',(7.42648363308103,-0.636968283911715,
-37.7160606276233));
#81250=CARTESIAN_POINT('Ctrl Pts',(6.12473637308791,4.2513173043175,-37.5043755597148));
#81251=CARTESIAN_POINT('Ctrl Pts',(2.15967861067737,6.68959520315537,-37.2926904918059));
#81252=CARTESIAN_POINT('Ctrl Pts',(-2.45971626464659,7.03175305296422,-37.0810054238974));
#81253=CARTESIAN_POINT('Ctrl Pts',(-7.40210048456495,3.03149454016741,-36.8163990890115));
#81254=CARTESIAN_POINT('Ctrl Pts',(-6.54224109123133,-4.59187570078724,
-36.4988714871485));
#81255=CARTESIAN_POINT('Ctrl Pts',(-0.854174246392727,-7.40054227728048,
-36.2342651522626));
#81256=CARTESIAN_POINT('Ctrl Pts',(3.59530441734421,-6.04880254325333,-36.022580084354));
#81257=CARTESIAN_POINT('Ctrl Pts',(6.06231187612364,-3.60202825407587,-35.8638162834224));
#81258=CARTESIAN_POINT('Ctrl Pts',(7.03134967606554,-0.272562345225122,
-35.7050524824909));
#81259=CARTESIAN_POINT('Ctrl Pts',(6.09210377326671,4.29472459686056,-35.4933674145823));
#81260=CARTESIAN_POINT('Ctrl Pts',(1.94847993991589,7.19649361741958,-35.2816823466735));
#81261=CARTESIAN_POINT('Ctrl Pts',(-2.65521286424894,6.50882019486048,-35.0699972787649));
#81262=CARTESIAN_POINT('Ctrl Pts',(-6.40979964046684,3.79608003992402,-34.8583122108561));
#81263=CARTESIAN_POINT('Ctrl Pts',(-7.6153326946967,-2.4469897179483,-34.5937058759703));
#81264=CARTESIAN_POINT('Ctrl Pts',(-2.04861717107107,-7.72589209306399,
-34.2761782741073));
#81265=CARTESIAN_POINT('Ctrl Pts',(4.11183777668357,-6.21211958507354,-34.0115719392213));
#81266=CARTESIAN_POINT('Ctrl Pts',(6.64568773823915,-2.31280361173633,-33.7998868713127));
#81267=CARTESIAN_POINT('Ctrl Pts',(6.9576487755742,1.14776144834246,-33.6411230703812));
#81268=CARTESIAN_POINT('Ctrl Pts',(5.55514133261181,4.31909403392073,-33.4823592694497));
#81269=CARTESIAN_POINT('Ctrl Pts',(1.89556214181054,7.20869141478983,-33.2706742015409));
#81270=CARTESIAN_POINT('Ctrl Pts',(-3.14320160819109,6.76064923746827,-33.0589891336322));
#81271=CARTESIAN_POINT('Ctrl Pts',(-6.22264549105552,3.27010378675402,-32.8473040657235));
#81272=CARTESIAN_POINT('Ctrl Pts',(-7.34846295884596,-1.22304834038044,
-32.6356189978149));
#81273=CARTESIAN_POINT('Ctrl Pts',(-4.25076732811253,-6.77584148670202,
-32.3710126629291));
#81274=CARTESIAN_POINT('Ctrl Pts',(3.40747783789418,-7.2301684442021,-32.053485061066));
#81275=CARTESIAN_POINT('Ctrl Pts',(7.14604670946127,-2.1051498918638,-31.7888787261801));
#81276=CARTESIAN_POINT('Ctrl Pts',(6.57382723358979,2.5097851628289,-31.5771936582715));
#81277=CARTESIAN_POINT('Ctrl Pts',(4.5841778728095,5.35831559886071,-31.4184298573399));
#81278=CARTESIAN_POINT('Ctrl Pts',(1.46904422986937,6.88157522300156,-31.2596660564085));
#81279=CARTESIAN_POINT('Ctrl Pts',(-3.19154302893877,6.73590683141938,-31.0479809884997));
#81280=CARTESIAN_POINT('Ctrl Pts',(-6.75815987344691,3.14855039450655,-30.8362959205911));
#81281=CARTESIAN_POINT('Ctrl Pts',(-6.86658588827577,-1.50495645200409,
-30.6246108526823));
#81282=CARTESIAN_POINT('Ctrl Pts',(-4.83470810709648,-5.6675702571397,-30.4129257847737));
#81283=CARTESIAN_POINT('Ctrl Pts',(1.11087231682787,-7.92130124577817,-30.1483194498878));
#81284=CARTESIAN_POINT('Ctrl Pts',(7.26268862552777,-3.33760316333525,-29.8307918480246));
#81285=CARTESIAN_POINT('Ctrl Pts',(6.82293566355775,2.99085081071726,-29.5661855131389));
#81286=CARTESIAN_POINT('Ctrl Pts',(3.41348404682912,6.15323920570995,-29.3545004452302));
#81287=CARTESIAN_POINT('Ctrl Pts',(0.0569914145846386,7.05145267340099,
-29.1957366442987));
#81288=CARTESIAN_POINT('Ctrl Pts',(-3.30723189674889,6.21098910643613,-29.036972843367));
#81289=CARTESIAN_POINT('Ctrl Pts',(-6.77921339195171,3.09849213868819,-28.8252877754586));
#81290=CARTESIAN_POINT('Ctrl Pts',(-7.19803321626531,-1.94278467138195,
-28.6136027075498));
#81291=CARTESIAN_POINT('Ctrl Pts',(-4.28450119423596,-5.57296556602382,
-28.4019176396412));
#81292=CARTESIAN_POINT('Ctrl Pts',(-0.049534836327076,-7.44938261874288,
-28.1902325717324));
#81293=CARTESIAN_POINT('Ctrl Pts',(5.95060747741717,-5.3452148114335,-27.9256262368466));
#81294=CARTESIAN_POINT('Ctrl Pts',(7.70577931196721,2.12301816820624,-27.6080986349835));
#81295=CARTESIAN_POINT('Ctrl Pts',(3.29430705698815,6.68170492129775,-27.3434923000977));
#81296=CARTESIAN_POINT('Ctrl Pts',(-1.35056516835081,6.90580913338042,-27.131807232189));
#81297=CARTESIAN_POINT('Ctrl Pts',(-4.4969704654332,5.43171146689254,-26.9730434312574));
#81298=CARTESIAN_POINT('Ctrl Pts',(-6.52972084949016,2.62238710469586,-26.814279630326));
#81299=CARTESIAN_POINT('Ctrl Pts',(-7.18190757360148,-1.99464065720506,
-26.6025945624171));
#81300=CARTESIAN_POINT('Ctrl Pts',(-4.25616253938917,-6.12137034495673,
-26.3909094945086));
#81301=CARTESIAN_POINT('Ctrl Pts',(0.310506454680001,-7.02271182842488,
-26.1792244265999));
#81302=CARTESIAN_POINT('Ctrl Pts',(4.75891064387549,-5.73136323958333,-25.9675393586912));
#81303=CARTESIAN_POINT('Ctrl Pts',(7.99465794946795,-0.257866247636377,
-25.7029330238053));
#81304=CARTESIAN_POINT('Ctrl Pts',(4.5285792436425,6.58621370601699,-25.3854054219423));
#81305=CARTESIAN_POINT('Ctrl Pts',(-1.78203643978692,7.23339379325415,-25.1207990870564));
#81306=CARTESIAN_POINT('Ctrl Pts',(-5.48009860066973,4.41392630065121,-24.9091140191477));
#81307=CARTESIAN_POINT('Ctrl Pts',(-6.93818813862285,1.26007070421613,-24.7503502182163));
#81308=CARTESIAN_POINT('Ctrl Pts',(-6.68444896123671,-2.19825171073812,
-24.5915864172847));
#81309=CARTESIAN_POINT('Ctrl Pts',(-4.21043380446389,-6.15066134048668,
-24.379901349376));
#81310=CARTESIAN_POINT('Ctrl Pts',(0.685317167062233,-7.42404437233138,
-24.1682162814673));
#81311=CARTESIAN_POINT('Ctrl Pts',(4.75963351168402,-5.17308269003613,-23.9565312135587));
#81312=CARTESIAN_POINT('Ctrl Pts',(7.33154849070669,-1.32066340482921,-23.74484614565));
#81313=CARTESIAN_POINT('Ctrl Pts',(6.28269814790344,4.9506317488773,-23.4802398107641));
#81314=CARTESIAN_POINT('Ctrl Pts',(-0.776215309838923,7.955107211097,-23.162712208901));
#81315=CARTESIAN_POINT('Ctrl Pts',(-6.02115247566208,4.38672571582093,-22.8981058740152));
#81316=CARTESIAN_POINT('Ctrl Pts',(-7.03499947526807,-0.151685344119284,
-22.6864208061065));
#81317=CARTESIAN_POINT('Ctrl Pts',(-6.11974090886601,-3.50357018409825,
-22.527657005175));
#81318=CARTESIAN_POINT('Ctrl Pts',(-3.69872264321837,-5.98611888519477,
-22.3688932042435));
#81319=CARTESIAN_POINT('Ctrl Pts',(0.739164948369388,-7.41700902832348,
-22.1572081363348));
#81320=CARTESIAN_POINT('Ctrl Pts',(5.30482458446264,-5.23879094733663,-21.9455230684261));
#81321=CARTESIAN_POINT('Ctrl Pts',(6.97261332117276,-0.893061675866078,
-21.7338380005174));
#81322=CARTESIAN_POINT('Ctrl Pts',(6.45971483836194,3.71050391557333,-21.5221529326087));
#81323=CARTESIAN_POINT('Ctrl Pts',(1.61903247740699,7.83324865989599,-21.2575465977228));
#81324=CARTESIAN_POINT('Ctrl Pts',(-5.71633226276247,5.58657197295241,-20.9400189958598));
#81325=CARTESIAN_POINT('Ctrl Pts',(-7.4314407242151,-0.520891930724535,
-20.6754126609739));
#81326=CARTESIAN_POINT('Ctrl Pts',(-5.28475202819951,-4.64603293801106,
-20.4637275930653));
#81327=CARTESIAN_POINT('Ctrl Pts',(-2.42614756643601,-6.62118122485914,
-20.3049637921337));
#81328=CARTESIAN_POINT('Ctrl Pts',(1.02471907613325,-6.96161757884978,-20.1461999912023));
#81329=CARTESIAN_POINT('Ctrl Pts',(5.34149291644613,-5.19873457397912,-19.9345149232935));
#81330=CARTESIAN_POINT('Ctrl Pts',(7.43204580714285,-0.592274921253531,
-19.7228298553849));
#81331=CARTESIAN_POINT('Ctrl Pts',(5.90975476036394,3.80653311503425,-19.5111447874762));
#81332=CARTESIAN_POINT('Ctrl Pts',(2.55301021957051,6.99842081609893,-19.2994597195675));
#81333=CARTESIAN_POINT('Ctrl Pts',(-3.80527894640322,7.03568780367081,-19.0348533846816));
#81334=CARTESIAN_POINT('Ctrl Pts',(-7.97083053855895,0.593381389034304,
-18.7173257828186));
#81335=CARTESIAN_POINT('Ctrl Pts',(-5.35032660329299,-5.1837867316385,-18.4527194479327));
#81336=CARTESIAN_POINT('Ctrl Pts',(-1.05164877455481,-6.95760453860522,
-18.241034380024));
#81337=CARTESIAN_POINT('Ctrl Pts',(2.40728630981526,-6.62806196780977,-18.0822705790925));
#81338=CARTESIAN_POINT('Ctrl Pts',(5.26673239643959,-4.66644386695429,-17.923506778161));
#81339=CARTESIAN_POINT('Ctrl Pts',(7.43430735718676,-0.538016603841439,
-17.7118217102523));
#81340=CARTESIAN_POINT('Ctrl Pts',(6.06758038330864,4.33250075059474,-17.5001366423436));
#81341=CARTESIAN_POINT('Ctrl Pts',(2.07040473052971,6.71776152712322,-17.2884515744349));
#81342=CARTESIAN_POINT('Ctrl Pts',(-2.55313691120353,6.99837459793973,-17.0767665065262));
#81343=CARTESIAN_POINT('Ctrl Pts',(-7.44181321864497,2.932655238766,-16.8121601716404));
#81344=CARTESIAN_POINT('Ctrl Pts',(-6.48051301594269,-4.678588675816,-16.4946325697774));
#81345=CARTESIAN_POINT('Ctrl Pts',(-0.755548756394746,-7.41126073740003,
-16.2300262348915));
#81346=CARTESIAN_POINT('Ctrl Pts',(3.67553485456433,-6.00038912017591,-16.0183411669828));
#81347=CARTESIAN_POINT('Ctrl Pts',(6.10974095364035,-3.52097973665857,-15.8595773660513));
#81348=CARTESIAN_POINT('Ctrl Pts',(7.03435580357583,-0.17890480105438,-15.7008135651198));
#81349=CARTESIAN_POINT('Ctrl Pts',(6.03437264126526,4.37546964033347,-15.4891284972111));
#81350=CARTESIAN_POINT('Ctrl Pts',(1.85247464443622,7.22180255570149,-15.2774434293024));
#81351=CARTESIAN_POINT('Ctrl Pts',(-2.74165251049031,6.47288476610073,-15.0657583613937));
#81352=CARTESIAN_POINT('Ctrl Pts',(-6.4597820083646,3.71038697508052,-14.854073293485));
#81353=CARTESIAN_POINT('Ctrl Pts',(-7.58207196787757,-2.54818276514574,
-14.589466958599));
#81354=CARTESIAN_POINT('Ctrl Pts',(-1.94555323095193,-7.75248757321215,
-14.2719393567361));
#81355=CARTESIAN_POINT('Ctrl Pts',(4.19419723412819,-6.15681323431598,-14.0073330218502));
#81356=CARTESIAN_POINT('Ctrl Pts',(6.67589705341909,-2.22410085040965,-13.7956479539416));
#81357=CARTESIAN_POINT('Ctrl Pts',(6.94174761381799,1.24031161108916,-13.63688415301));
#81358=CARTESIAN_POINT('Ctrl Pts',(5.49713329566522,4.39268642505134,-13.4781203520784));
#81359=CARTESIAN_POINT('Ctrl Pts',(1.79939910583755,7.23329458857038,-13.2664352841698));
#81360=CARTESIAN_POINT('Ctrl Pts',(-3.23295148088592,6.71819314876056,-13.054750216261));
#81361=CARTESIAN_POINT('Ctrl Pts',(-6.265640260461,3.18694960895007,-12.8430651483524));
#81362=CARTESIAN_POINT('Ctrl Pts',(-7.33152458160375,-1.32079612725738,
-12.6313800804438));
#81363=CARTESIAN_POINT('Ctrl Pts',(-4.16015952896897,-6.83184626760507,
-12.3667737455578));
#81364=CARTESIAN_POINT('Ctrl Pts',(3.50345665718391,-7.18415147380051,-12.0492461436949));
#81365=CARTESIAN_POINT('Ctrl Pts',(7.17344642534743,-2.00980248374984,-11.784639808809));
#81366=CARTESIAN_POINT('Ctrl Pts',(6.53982263713274,2.59710337404747,-11.5729547409003));
#81367=CARTESIAN_POINT('Ctrl Pts',(4.51241707618843,5.41888595165771,-11.4141909399688));
#81368=CARTESIAN_POINT('Ctrl Pts',(1.37727507470006,6.90052765140112,-11.2554271390373));
#81369=CARTESIAN_POINT('Ctrl Pts',(-3.28095913154713,6.69280919526674,-11.0437420711286));
#81370=CARTESIAN_POINT('Ctrl Pts',(-6.79948848636568,3.05827578638617,-10.8320570032198));
#81371=CARTESIAN_POINT('Ctrl Pts',(-6.84593619299317,-1.59626229829667,
-10.6203719353112));
#81372=CARTESIAN_POINT('Ctrl Pts',(-4.75880688852233,-5.73144938895834,
-10.4086868674024));
#81373=CARTESIAN_POINT('Ctrl Pts',(1.21625828458495,-7.90580587390299,-10.1440805325167));
#81374=CARTESIAN_POINT('Ctrl Pts',(7.30649003441419,-3.24059320561566,-9.82655293065358));
#81375=CARTESIAN_POINT('Ctrl Pts',(6.78250284019818,3.08144363305912,-9.56194659576771));
#81376=CARTESIAN_POINT('Ctrl Pts',(3.33124140842834,6.19814946088065,-9.35026152785902));
#81377=CARTESIAN_POINT('Ctrl Pts',(-0.0369147177961642,7.05158635557704,
-9.19149772692751));
#81378=CARTESIAN_POINT('Ctrl Pts',(-3.38964764394158,6.16639743683966,-9.03273392599598));
#81379=CARTESIAN_POINT('Ctrl Pts',(-6.8198735343995,3.00794160879609,-8.82104885808732));
#81380=CARTESIAN_POINT('Ctrl Pts',(-7.17152376687591,-2.03846543334665,
-8.60936379017862));
#81381=CARTESIAN_POINT('Ctrl Pts',(-4.2099085709813,-5.62952622406857,-8.39767872226993));
#81382=CARTESIAN_POINT('Ctrl Pts',(0.0496696921086477,-7.44938172079558,
-8.18599365436123));
#81383=CARTESIAN_POINT('Ctrl Pts',(6.02125970469887,-5.26549924501289,-7.92138731947539));
#81384=CARTESIAN_POINT('Ctrl Pts',(7.6768247512655,2.22544437936245,-7.60385971761233));
#81385=CARTESIAN_POINT('Ctrl Pts',(3.20503764153763,6.72498129048212,-7.33925338272649));
#81386=CARTESIAN_POINT('Ctrl Pts',(-1.44240702302965,6.88721192069529,-7.12756831481779));
#81387=CARTESIAN_POINT('Ctrl Pts',(-4.56890342341336,5.37134567255369,-6.96880451388627));
#81388=CARTESIAN_POINT('Ctrl Pts',(-6.56406303393157,2.53520117263162,-6.81004071295475));
#81389=CARTESIAN_POINT('Ctrl Pts',(-7.15470901081791,-2.09010208308626,
-6.59835564504608));
#81390=CARTESIAN_POINT('Ctrl Pts',(-4.17426956481358,-6.17750500298273,
-6.38667057713737));
#81391=CARTESIAN_POINT('Ctrl Pts',(0.403997272147747,-7.01795425233056,
-6.17498550922869));
#81392=CARTESIAN_POINT('Ctrl Pts',(4.83481070605209,-5.66748273370333,-5.96330044131999));
#81393=CARTESIAN_POINT('Ctrl Pts',(7.99738295964715,-0.151382056073881,
-5.69869410643413));
#81394=CARTESIAN_POINT('Ctrl Pts',(4.44047200052455,6.64593479972095,-5.38116650457111));
#81395=CARTESIAN_POINT('Ctrl Pts',(-1.87820233645865,7.20902182139955,-5.11656016968524));
#81396=CARTESIAN_POINT('Ctrl Pts',(-5.53839098997102,4.34055887001719,-4.90487510177656));
#81397=CARTESIAN_POINT('Ctrl Pts',(-6.95435273940389,1.16756618871284,-4.74611130084502));
#81398=CARTESIAN_POINT('Ctrl Pts',(-6.65458310877973,-2.28707064478078,
-4.58734749991352));
#81399=CARTESIAN_POINT('Ctrl Pts',(-4.1281548306516,-6.2061844548941,-4.37566243200482));
#81400=CARTESIAN_POINT('Ctrl Pts',(0.784119120890008,-7.41426001610747,
-4.16397736409614));
#81401=CARTESIAN_POINT('Ctrl Pts',(4.82809913155386,-5.10924206699896,-3.95229229618746));
#81402=CARTESIAN_POINT('Ctrl Pts',(7.34848510506071,-1.22291529595122,-3.74060722827875));
#81403=CARTESIAN_POINT('Ctrl Pts',(6.21621567622543,5.0338566618374,-3.47600089339291));
#81404=CARTESIAN_POINT('Ctrl Pts',(-0.88208110558023,7.94406537887752,-3.15847329152986));
#81405=CARTESIAN_POINT('Ctrl Pts',(-6.07903471426388,4.30615562359862,-2.893866956644));
#81406=CARTESIAN_POINT('Ctrl Pts',(-7.03235570173644,-0.245353737911625,
-2.68218188873531));
#81407=CARTESIAN_POINT('Ctrl Pts',(-6.07254290742731,-3.58475370555032,
-2.5234180878038));
#81408=CARTESIAN_POINT('Ctrl Pts',(-3.61867994279838,-6.03484180458674,
-2.36465428687228));
#81409=CARTESIAN_POINT('Ctrl Pts',(0.83786789650287,-7.40650949062282,-2.15296921896358));
#81410=CARTESIAN_POINT('Ctrl Pts',(5.37411791268271,-5.16768201409678,-1.94128415105492));
#81411=CARTESIAN_POINT('Ctrl Pts',(6.98388635697521,-0.800134094673566,
-1.7295990831462));
#81412=CARTESIAN_POINT('Ctrl Pts',(6.40973376103728,3.79620266144416,-1.51791401523753));
#81413=CARTESIAN_POINT('Ctrl Pts',(1.51457095822232,7.85410001054634,-1.25330768035165));
#81414=CARTESIAN_POINT('Ctrl Pts',(-5.79020864255492,5.50997946566744,-0.935780078488634));
#81415=CARTESIAN_POINT('Ctrl Pts',(-7.42386336108424,-0.61984882046184,
-0.671173743602752));
#81416=CARTESIAN_POINT('Ctrl Pts',(-5.2223892511724,-4.7159377152133,-0.45948867569408));
#81417=CARTESIAN_POINT('Ctrl Pts',(-2.33781566303131,-6.65302851753602,
-0.300724874762546));
#81418=CARTESIAN_POINT('Ctrl Pts',(1.11743471057894,-6.94711885568928,-0.14196107383103));
#81419=CARTESIAN_POINT('Ctrl Pts',(5.41001647346126,-5.12768111829485,0.0697239940776447));
#81420=CARTESIAN_POINT('Ctrl Pts',(7.43971882199819,-0.492221914184057,
0.281409061986343));
#81421=CARTESIAN_POINT('Ctrl Pts',(5.85802083447291,3.88368773050881,0.493094129895022));
#81422=CARTESIAN_POINT('Ctrl Pts',(2.46080141762815,7.03461357653157,0.704779197803715));
#81423=CARTESIAN_POINT('Ctrl Pts',(-3.9011713930233,6.97843216915639,0.969385532689581));
#81424=CARTESIAN_POINT('Ctrl Pts',(-7.9737779581346,0.497495361200036,1.28691313455261));
#81425=CARTESIAN_POINT('Ctrl Pts',(-4.74911250865948,-6.42452853835538,
1.60444073641564));
#81426=CARTESIAN_POINT('Ctrl Pts',(2.83261554749834,-7.47622517968333,1.92196833827868));
#81427=CARTESIAN_POINT('Ctrl Pts',(6.96864010952473,-2.64185291264415,2.18657467316454));
#81428=CARTESIAN_POINT('Ctrl Pts',(6.74201681238604,1.986113739625,2.39825974107324));
#81429=CARTESIAN_POINT('Ctrl Pts',(4.40955949058423,6.01227774326799,2.60994480898192));
#81430=CARTESIAN_POINT('Ctrl Pts',(-0.445016813261593,7.44065534277421,
2.82162987689062));
#81431=CARTESIAN_POINT('Ctrl Pts',(-4.59957704198864,5.32494241868321,3.0333149447993));
#81432=CARTESIAN_POINT('Ctrl Pts',(-6.59738751825183,2.49051168707897,3.19207874573082));
#81433=CARTESIAN_POINT('Ctrl Pts',(-6.97022255151235,-0.964062034788524,
3.35084254666235));
#81434=CARTESIAN_POINT('Ctrl Pts',(-5.25072352308984,-5.28468184930254,
3.56252761457101));
#81435=CARTESIAN_POINT('Ctrl Pts',(0.493092895115608,-7.97767191812129,
3.82713394945689));
#81436=CARTESIAN_POINT('Ctrl Pts',(6.9872488172523,-3.8934773826184,4.14466155131991));
#81437=CARTESIAN_POINT('Ctrl Pts',(7.02998899293067,2.46477104279695,4.40926788620579));
#81438=CARTESIAN_POINT('Ctrl Pts',(3.88056947259661,5.8614045914742,4.62095295411446));
#81439=CARTESIAN_POINT('Ctrl Pts',(-0.49873573962075,7.43890740635084,4.83263802202317));
#81440=CARTESIAN_POINT('Ctrl Pts',(-5.13113239802791,5.40646703130468,5.04432308993184));
#81441=CARTESIAN_POINT('Ctrl Pts',(-6.9481759541162,1.11220998262044,5.25600815784053));
#81442=CARTESIAN_POINT('Ctrl Pts',(-6.65117684641269,-2.34266579984132,
5.41477195877206));
#81443=CARTESIAN_POINT('Ctrl Pts',(-4.71214358271871,-5.22589016611478,
5.57353575970356));
#81444=CARTESIAN_POINT('Ctrl Pts',(-0.614333013769389,-7.4243002539006,
5.78522082761227));
#81445=CARTESIAN_POINT('Ctrl Pts',(5.51422265003698,-5.7861550607049,6.04982716249811));
#81446=CARTESIAN_POINT('Ctrl Pts',(7.85299510856503,1.52036773516451,6.36735476436117));
#81447=CARTESIAN_POINT('Ctrl Pts',(3.79146892837499,6.41252824754307,6.63196109924701));
#81448=CARTESIAN_POINT('Ctrl Pts',(-0.805280546119295,6.98329570943009,
6.84364616715573));
#81449=CARTESIAN_POINT('Ctrl Pts',(-5.17164554705694,5.37030508610091,7.05533123506437));
#81450=CARTESIAN_POINT('Ctrl Pts',(-7.40712401550797,0.83240711967557,7.26701630297311));
#81451=CARTESIAN_POINT('Ctrl Pts',(-6.03217252679437,-3.62312890922495,
7.47870137088176));
#81452=CARTESIAN_POINT('Ctrl Pts',(-3.58027492641036,-6.07518430011776,
7.6374651718133));
#81453=CARTESIAN_POINT('Ctrl Pts',(-0.240168590682506,-7.03253475710761,
7.7962289727448));
#81454=CARTESIAN_POINT('Ctrl Pts',(4.31063684734961,-6.07585793187805,8.00791404065352));
#81455=CARTESIAN_POINT('Ctrl Pts',(7.94471355281213,-0.876223438026825,
8.27252037553935));
#81456=CARTESIAN_POINT('Ctrl Pts',(5.0292718807473,6.21992564904773,8.59004797740241));
#81457=CARTESIAN_POINT('Ctrl Pts',(-1.22833328830734,7.34758140023083,8.85465431228825));
#81458=CARTESIAN_POINT('Ctrl Pts',(-5.11280060736866,4.82433058910742,9.06633938019695));
#81459=CARTESIAN_POINT('Ctrl Pts',(-7.41483616626323,0.778652097589249,
9.27802444810563));
#81460=CARTESIAN_POINT('Ctrl Pts',(-6.20313892391525,-4.13272975620328,
9.48970951601433));
#81461=CARTESIAN_POINT('Ctrl Pts',(-2.28216335448501,-6.65626764204876,
9.70139458392301));
#81462=CARTESIAN_POINT('Ctrl Pts',(1.172693573114,-6.95348995901458,9.86015838485453));
#81463=CARTESIAN_POINT('Ctrl Pts',(4.34464135000243,-5.5351890302411,10.0189221857861));
#81464=CARTESIAN_POINT('Ctrl Pts',(7.21040472992183,-1.87288634778747,10.2306072536948));
#81465=CARTESIAN_POINT('Ctrl Pts',(6.64265886901188,4.44537108655917,10.4952135885806));
#81466=CARTESIAN_POINT('Ctrl Pts',(-0.157278780643135,7.99726916614796,
10.8127411904437));
#81467=CARTESIAN_POINT('Ctrl Pts',(-5.67104607761196,4.83063054745853,11.0773475253295));
#81468=CARTESIAN_POINT('Ctrl Pts',(-7.0182502267125,0.398822565494279,11.2890325932382));
#81469=CARTESIAN_POINT('Ctrl Pts',(-6.1744254806425,-4.1788233326868,11.5007176611469));
#81470=CARTESIAN_POINT('Ctrl Pts',(-2.08482608374679,-7.15624817538203,
11.7124027290556));
#81471=CARTESIAN_POINT('Ctrl Pts',(2.54004040956054,-6.56219195215601,11.9240877969643));
#81472=CARTESIAN_POINT('Ctrl Pts',(5.37471303366855,-4.56494168990841,12.0828515978958));
#81473=CARTESIAN_POINT('Ctrl Pts',(6.88827358848924,-1.43732843524527,12.2416153988273));
#81474=CARTESIAN_POINT('Ctrl Pts',(6.72261626979761,3.20999534735937,12.453300466736));
#81475=CARTESIAN_POINT('Ctrl Pts',(2.21978336802205,7.67846356677739,12.7179068016219));
#81476=CARTESIAN_POINT('Ctrl Pts',(-5.2699375108196,6.01737562087635,13.0354344034849));
#81477=CARTESIAN_POINT('Ctrl Pts',(-7.4494163191068,0.0441769743614518,
13.3000407383708));
#81478=CARTESIAN_POINT('Ctrl Pts',(-5.62642057271849,-4.21405828417065,
13.5117258062795));
#81479=CARTESIAN_POINT('Ctrl Pts',(-2.03317704990997,-7.17302485326342,
13.7234108741881));
#81480=CARTESIAN_POINT('Ctrl Pts',(3.01296933575057,-6.81765381410323,13.9350959420969));
#81481=CARTESIAN_POINT('Ctrl Pts',(6.16889507299606,-3.38510000997113,14.1467810100055));
#81482=CARTESIAN_POINT('Ctrl Pts',(7.05161165730847,-0.0317153127294182,
14.305544810937));
#81483=CARTESIAN_POINT('Ctrl Pts',(6.19569152870785,3.33581062737987,14.4643086118686));
#81484=CARTESIAN_POINT('Ctrl Pts',(3.07644180560223,6.78477305867776,14.6759936797772));
#81485=CARTESIAN_POINT('Ctrl Pts',(-3.24597966964378,7.30409863922549,14.9406000146631));
#81486=CARTESIAN_POINT('Ctrl Pts',(-7.90670051699391,1.21042871133698,15.2581276165262));
#81487=CARTESIAN_POINT('Ctrl Pts',(-5.72793898690211,-4.76303160421653,
15.5227339514119));
#81488=CARTESIAN_POINT('Ctrl Pts',(-1.59121410280738,-6.84711131518423,
15.7344190193207));
#81489=CARTESIAN_POINT('Ctrl Pts',(3.06328846900944,-6.79723165836278,15.9461040872294));
#81490=CARTESIAN_POINT('Ctrl Pts',(6.69522654827307,-3.27602338429213,16.1577891551381));
#81491=CARTESIAN_POINT('Ctrl Pts',(6.89951025983584,1.38236271418235,16.3694742230468));
#81492=CARTESIAN_POINT('Ctrl Pts',(5.41555730687422,4.51641139429432,16.5282380239783));
#81493=CARTESIAN_POINT('Ctrl Pts',(2.59228061532602,6.54173579962135,16.6870018249098));
#81494=CARTESIAN_POINT('Ctrl Pts',(-2.01509118438118,7.17196257377617,16.8986868928185));
#81495=CARTESIAN_POINT('Ctrl Pts',(-7.18673274888623,3.49815856463975,17.1632932277044));
#81496=CARTESIAN_POINT('Ctrl Pts',(-6.82877697123075,-4.16519577065104,
17.4808208295674));
#81497=CARTESIAN_POINT('Ctrl Pts',(-1.3153899643973,-7.33249646041519,17.7454271644533));
#81498=CARTESIAN_POINT('Ctrl Pts',(3.19156863058387,-6.26328870161434,17.9571122323619));
#81499=CARTESIAN_POINT('Ctrl Pts',(6.72057509705298,-3.22799703015457,18.1687973002706));
#81500=CARTESIAN_POINT('Ctrl Pts',(7.23196585891104,1.80473199192428,18.3804823681793));
#81501=CARTESIAN_POINT('Ctrl Pts',(4.38863199158892,5.5003706912847,18.592167436088));
#81502=CARTESIAN_POINT('Ctrl Pts',(1.23519286706014,6.94266025437761,18.7509312370195));
#81503=CARTESIAN_POINT('Ctrl Pts',(-2.22902263126149,6.6742553269984,18.909695037951));
#81504=CARTESIAN_POINT('Ctrl Pts',(-6.15990409720221,4.18965644824107,19.1213801058598));
#81505=CARTESIAN_POINT('Ctrl Pts',(-7.75105093758523,-1.95126889747041,
19.3859864407454));
#81506=CARTESIAN_POINT('Ctrl Pts',(-2.54259153080113,-7.58394877607694,
19.7035140426087));
#81507=CARTESIAN_POINT('Ctrl Pts',(3.71514900230698,-6.45704444704349,19.9681203774944));
#81508=CARTESIAN_POINT('Ctrl Pts',(6.47490452820166,-2.73687906824002,20.1798054454032));
#81509=CARTESIAN_POINT('Ctrl Pts',(7.22043469461147,1.85779904259507,20.3914905133118));
#81510=CARTESIAN_POINT('Ctrl Pts',(4.37101908514151,6.03759719627431,20.6031755812206));
#81511=CARTESIAN_POINT('Ctrl Pts',(-0.184091442732042,7.03422197828974,
20.8148606491293));
#81512=CARTESIAN_POINT('Ctrl Pts',(-3.52548371717569,6.10714314442349,20.9736244500608));
#81513=CARTESIAN_POINT('Ctrl Pts',(-6.00309759665687,3.67110954694288,21.1323882509922));
#81514=CARTESIAN_POINT('Ctrl Pts',(-7.41070162877531,-0.761013147248125,
21.344073318901));
#81515=CARTESIAN_POINT('Ctrl Pts',(-4.67380908245231,-6.48396095053497,
21.6086796537869));
#81516=CARTESIAN_POINT('Ctrl Pts',(2.93814156528294,-7.43964884070595,21.9262072556498));
#81517=CARTESIAN_POINT('Ctrl Pts',(7.00025521768217,-2.54797605713872,22.1908135905358));
#81518=CARTESIAN_POINT('Ctrl Pts',(6.71623311514751,2.07535742138385,22.4024986584444));
#81519=CARTESIAN_POINT('Ctrl Pts',(4.32802572178841,6.07077324674158,22.614183726353));
#81520=CARTESIAN_POINT('Ctrl Pts',(-0.543498046951198,7.43390863678652,
22.8258687942618));
#81521=CARTESIAN_POINT('Ctrl Pts',(-4.67032595475534,5.26329022337551,23.0375538621705));
#81522=CARTESIAN_POINT('Ctrl Pts',(-6.62983514718073,2.40239854057519,23.196317663102));
#81523=CARTESIAN_POINT('Ctrl Pts',(-6.95682722782088,-1.05677858744988,
23.3550814640335));
#81524=CARTESIAN_POINT('Ctrl Pts',(-5.17984032912462,-5.35414734629062,
23.5667665319422));
#81525=CARTESIAN_POINT('Ctrl Pts',(0.599258415449432,-7.9703908498134,23.831372866828));
#81526=CARTESIAN_POINT('Ctrl Pts',(7.03849166383386,-3.80009023956034,24.1489004686911));
#81527=CARTESIAN_POINT('Ctrl Pts',(6.99653648498133,2.55816971969485,24.413506803577));
#81528=CARTESIAN_POINT('Ctrl Pts',(3.80217459986353,5.91255985133764,24.6251918714857));
#81529=CARTESIAN_POINT('Ctrl Pts',(-0.597754682089963,7.43160708069626,
24.8368769393942));
#81530=CARTESIAN_POINT('Ctrl Pts',(-5.20267164077861,5.33765824546381,25.0485620073031));
#81531=CARTESIAN_POINT('Ctrl Pts',(-6.96237124967031,1.01958573985015,25.2602470752116));
#81532=CARTESIAN_POINT('Ctrl Pts',(-6.61939053680676,-2.43102894836384,
25.4190108761433));
#81533=CARTESIAN_POINT('Ctrl Pts',(-4.64213503223238,-5.2881762832912,25.5777746770747));
#81534=CARTESIAN_POINT('Ctrl Pts',(-0.515412313442996,-7.43182277696184,
25.7894597449835));
#81535=CARTESIAN_POINT('Ctrl Pts',(5.59078531721744,-5.71221152304974,26.0540660798693));
#81536=CARTESIAN_POINT('Ctrl Pts',(7.83205275812538,1.62480778081629,26.3715936817324));
#81537=CARTESIAN_POINT('Ctrl Pts',(3.70573992063129,6.46244897396321,26.6362000166182));
#81538=CARTESIAN_POINT('Ctrl Pts',(-0.898202598399992,6.97195293843298,
26.8478850845269));
#81539=CARTESIAN_POINT('Ctrl Pts',(-5.24270096633202,5.3009603884048,27.0595701524356));
#81540=CARTESIAN_POINT('Ctrl Pts',(-7.41755202574982,0.733695912776324,
27.2712552203442));
#81541=CARTESIAN_POINT('Ctrl Pts',(-5.98339005317347,-3.70313542430281,
27.482940288253));
#81542=CARTESIAN_POINT('Ctrl Pts',(-3.49905692074093,-6.1223225570012,27.6417040891845));
#81543=CARTESIAN_POINT('Ctrl Pts',(-0.146498137973434,-7.03510940612958,
27.800467890116));
#81544=CARTESIAN_POINT('Ctrl Pts',(4.39116414144362,-6.01791634404437,28.0121529580247));
#81545=CARTESIAN_POINT('Ctrl Pts',(7.95567738085036,-0.770349504512316,
28.2767592929106));
#81546=CARTESIAN_POINT('Ctrl Pts',(4.94599793777059,6.28634672367265,28.5942868947736));
#81547=CARTESIAN_POINT('Ctrl Pts',(-1.32606886728268,7.33057272385053,28.8588932296594));
#81548=CARTESIAN_POINT('Ctrl Pts',(-5.17659073738139,4.75581791295187,29.0705782975681));
#81549=CARTESIAN_POINT('Ctrl Pts',(-7.42454766388758,0.679842958687934,
29.2822633654768));
#81550=CARTESIAN_POINT('Ctrl Pts',(-6.14755516020086,-4.21496776967729,
29.4939484333855));
#81551=CARTESIAN_POINT('Ctrl Pts',(-2.19332242210769,-6.68606799635041,
29.7056335012942));
#81552=CARTESIAN_POINT('Ctrl Pts',(1.26518614402654,-6.93725715593081,29.8643973022256));
#81553=CARTESIAN_POINT('Ctrl Pts',(4.41796577987675,-5.47684256013266,30.0231611031572));
#81554=CARTESIAN_POINT('Ctrl Pts',(7.23470578825659,-1.7767025070009,30.234846171066));
#81555=CARTESIAN_POINT('Ctrl Pts',(6.58287282695247,4.53343427121724,30.4994525059518));
#81556=CARTESIAN_POINT('Ctrl Pts',(-0.263760934085454,7.99446564194957,
30.8169801078149));
#81557=CARTESIAN_POINT('Ctrl Pts',(-5.73487060217261,4.75468340447343,31.0815864427006));
#81558=CARTESIAN_POINT('Ctrl Pts',(-7.02293886729659,0.305328265497105,
31.2932715106094));
#81559=CARTESIAN_POINT('Ctrl Pts',(-6.11823045514813,-4.26067489483924,
31.504956578518));
#81560=CARTESIAN_POINT('Ctrl Pts',(-1.98934462931711,-7.18337634354049,
31.7166416464268));
#81561=CARTESIAN_POINT('Ctrl Pts',(2.62720099616708,-6.52778549164112,31.9283267143354));
#81562=CARTESIAN_POINT('Ctrl Pts',(5.43502577277014,-4.49296424155314,32.087090515267));
#81563=CARTESIAN_POINT('Ctrl Pts',(6.90680307772866,-1.34547289311988,32.2458543161984));
#81564=CARTESIAN_POINT('Ctrl Pts',(6.67927409073989,3.29923282927815,32.4575393841072));
#81565=CARTESIAN_POINT('Ctrl Pts',(2.11733583544207,7.70734259698044,32.722145718993));
#81566=CARTESIAN_POINT('Ctrl Pts',(-5.34960096107483,5.94666463556916,33.039673320856));
#81567=CARTESIAN_POINT('Ctrl Pts',(-7.44934406989137,-0.0550275277693012,
33.3042796557419));
#81568=CARTESIAN_POINT('Ctrl Pts',(-5.56980493015303,-4.28860918288662,
33.5159647236506));
#81569=CARTESIAN_POINT('Ctrl Pts',(-1.93747676755842,-7.1994637464875,33.7276497915593));
#81570=CARTESIAN_POINT('Ctrl Pts',(3.10348986080373,-6.77692691645844,33.939334859468));
#81571=CARTESIAN_POINT('Ctrl Pts',(6.21342596229719,-3.30265140609674,34.1510199273767));
#81572=CARTESIAN_POINT('Ctrl Pts',(7.05140873470941,0.0621906955560119,
34.3097837283081));
#81573=CARTESIAN_POINT('Ctrl Pts',(6.1507206452107,3.4180201294348,34.4685475292397));
#81574=CARTESIAN_POINT('Ctrl Pts',(2.98581919527262,6.82513907361293,34.6802325971484));
#81575=CARTESIAN_POINT('Ctrl Pts',(-3.34295730459666,7.26022571322132,34.9448389320343));
#81576=CARTESIAN_POINT('Ctrl Pts',(-7.9221181796911,1.10503134691718,35.2623665338973));
#81577=CARTESIAN_POINT('Ctrl Pts',(-5.6640039076763,-4.83888570171544,35.5269728687832));
#81578=CARTESIAN_POINT('Ctrl Pts',(-1.49989305555173,-6.86769368168124,
35.7386579366918));
#81579=CARTESIAN_POINT('Ctrl Pts',(3.15353257947768,-6.75583649387605,35.9503430046006));
#81580=CARTESIAN_POINT('Ctrl Pts',(6.73825824291578,-3.18657552851134,36.1620280725092));
#81581=CARTESIAN_POINT('Ctrl Pts',(6.88049017180109,1.47411787008045,36.3737131404179));
#81582=CARTESIAN_POINT('Ctrl Pts',(5.35493405865668,4.58812751065068,36.5324769413494));
#81583=CARTESIAN_POINT('Ctrl Pts',(2.50493735499844,6.57567600389313,36.691240742281));
#81584=CARTESIAN_POINT('Ctrl Pts',(-2.11041836375434,7.14449256217294,36.9029258101897));
#81585=CARTESIAN_POINT('Ctrl Pts',(-7.23267893805106,3.40214584142843,37.1675321450755));
#81586=CARTESIAN_POINT('Ctrl Pts',(-6.77270539707515,-4.25576225077142,
37.4850597469385));
#81587=CARTESIAN_POINT('Ctrl Pts',(-1.21762971480025,-7.3493627599999,37.7496660818244));
#81588=CARTESIAN_POINT('Ctrl Pts',(3.27469108415253,-6.2202326312501,37.9613511497331));
#81589=CARTESIAN_POINT('Ctrl Pts',(6.76296499832418,-3.13821587741466,38.1730362176418));
#81590=CARTESIAN_POINT('Ctrl Pts',(7.20729178726076,1.90087686092851,38.3847212855504));
#81591=CARTESIAN_POINT('Ctrl Pts',(4.31499684899518,5.55832445007519,38.5964063534592));
#81592=CARTESIAN_POINT('Ctrl Pts',(1.14263100495772,6.95849317115852,38.7551701543905));
#81593=CARTESIAN_POINT('Ctrl Pts',(-2.31770309403215,6.64398061620866,38.9139339553223));
#81594=CARTESIAN_POINT('Ctrl Pts',(-6.21514970625623,4.10725623376965,39.1256190232308));
#81595=CARTESIAN_POINT('Ctrl Pts',(-7.72437947181739,-2.05431319974369,
39.3902253581168));
#81596=CARTESIAN_POINT('Ctrl Pts',(-2.4413739867491,-7.61713488048403,39.7077529599797));
#81597=CARTESIAN_POINT('Ctrl Pts',(3.80080519001087,-6.40699890807125,39.9723592948657));
#81598=CARTESIAN_POINT('Ctrl Pts',(6.51077621204975,-2.65041294897678,40.1840443627743));
#81599=CARTESIAN_POINT('Ctrl Pts',(7.19505497495942,1.9537856507627,40.3957294306831));
#81600=CARTESIAN_POINT('Ctrl Pts',(4.29023149632212,6.09526877628013,40.6074144985916));
#81601=CARTESIAN_POINT('Ctrl Pts',(-0.277746744914853,7.03114679443056,
40.8190995665004));
#81602=CARTESIAN_POINT('Ctrl Pts',(-3.60649724135123,6.05965431973448,40.9778633674319));
#81603=CARTESIAN_POINT('Ctrl Pts',(-6.05145184970988,3.59084343452698,41.1366271683635));
#81604=CARTESIAN_POINT('Ctrl Pts',(-7.39991045135328,-0.859630707320278,
41.3483122362721));
#81605=CARTESIAN_POINT('Ctrl Pts',(-4.58705061660543,-6.54562507236513,
41.612918571158));
#81606=CARTESIAN_POINT('Ctrl Pts',(3.03695155815124,-7.39986323955413,41.930446173021));
#81607=CARTESIAN_POINT('Ctrl Pts',(7.03356478114057,-2.45453082480906,42.1950525079069));
#81608=CARTESIAN_POINT('Ctrl Pts',(6.68800097390752,2.16461050919299,42.4067375758155));
#81609=CARTESIAN_POINT('Ctrl Pts',(4.24680015435768,6.12786936143086,42.6184226437243));
#81610=CARTESIAN_POINT('Ctrl Pts',(-0.642443931402486,7.42601195407965,
42.8301077116328));
#81611=CARTESIAN_POINT('Ctrl Pts',(-4.74000075015738,5.20063086439034,43.0417927795416));
#81612=CARTESIAN_POINT('Ctrl Pts',(-6.66123896407119,2.31389893687908,43.200556580473));
#81613=CARTESIAN_POINT('Ctrl Pts',(-6.94213771746103,-1.14932587739404,
43.3593203814047));
#81614=CARTESIAN_POINT('Ctrl Pts',(-5.10808222231357,-5.42265024237231,
43.5710054493132));
#81615=CARTESIAN_POINT('Ctrl Pts',(0.705343452210856,-7.96170406142419,
43.8356117841993));
#81616=CARTESIAN_POINT('Ctrl Pts',(7.08847168811231,-3.70602480529903,44.1531393860622));
#81617=CARTESIAN_POINT('Ctrl Pts',(6.96185009143382,2.65111267298142,44.4177457209481));
#81618=CARTESIAN_POINT('Ctrl Pts',(3.72310251714552,5.96266746769607,44.6294307888568));
#81619=CARTESIAN_POINT('Ctrl Pts',(-0.696665106838566,7.42298809043423,
44.8411158567655));
#81620=CARTESIAN_POINT('Ctrl Pts',(-5.27328955955073,5.26790328007862,45.0528009246742));
#81621=CARTESIAN_POINT('Ctrl Pts',(-6.97533127386178,0.926780512865594,
45.2644859925829));
#81622=CARTESIAN_POINT('Ctrl Pts',(-6.5864306619872,-2.51896088921308,45.4232497935144));
#81623=CARTESIAN_POINT('Ctrl Pts',(-4.57130311085973,-5.34952464517057,
45.582013594446));
#81624=CARTESIAN_POINT('Ctrl Pts',(-0.41640031263465,-7.43802732051007,
45.7936986623545));
#81625=CARTESIAN_POINT('Ctrl Pts',(5.66635658269597,-5.63725500798157,46.0583049972405));
#81626=CARTESIAN_POINT('Ctrl Pts',(7.80972144840075,1.72895969561206,46.3758325991034));
#81627=CARTESIAN_POINT('Ctrl Pts',(3.61935375827535,6.51122365403746,46.6404389339895));
#81628=CARTESIAN_POINT('Ctrl Pts',(-0.990965371568293,6.95937377325353,
46.8521240018979));
#81629=CARTESIAN_POINT('Ctrl Pts',(-5.31282664658784,5.23067562415428,47.0638090698067));
#81630=CARTESIAN_POINT('Ctrl Pts',(-7.42666462090135,0.634854594203452,
47.2754941377155));
#81631=CARTESIAN_POINT('Ctrl Pts',(-5.9335464923095,-3.78248523100134,47.4871792056241));
#81632=CARTESIAN_POINT('Ctrl Pts',(-3.41721839800217,-6.16837508967364,
47.6459430065556));
#81633=CARTESIAN_POINT('Ctrl Pts',(-0.0528017051626853,-7.03643645893111,
47.8047068074872));
#81634=CARTESIAN_POINT('Ctrl Pts',(4.47091271248134,-5.958907547394,48.0163918753957));
#81635=CARTESIAN_POINT('Ctrl Pts',(7.96523036049119,-0.66433895835216,48.2809982102817));
#81636=CARTESIAN_POINT('Ctrl Pts',(4.86184687845832,6.35165298651348,48.5985258121447));
#81637=CARTESIAN_POINT('Ctrl Pts',(-1.42356928304938,7.31226405409412,48.8631321470306));
#81638=CARTESIAN_POINT('Ctrl Pts',(-5.23946285815445,4.68646184680054,49.0748172149392));
#81639=CARTESIAN_POINT('Ctrl Pts',(-7.43294250275057,0.580913257396659,
49.2865022828479));
#81640=CARTESIAN_POINT('Ctrl Pts',(-6.09088119778471,-4.29645830674553,
49.4981873507567));
#81641=CARTESIAN_POINT('Ctrl Pts',(-2.10409252904161,-6.71468265284166,
49.7098724186654));
#81642=CARTESIAN_POINT('Ctrl Pts',(1.35745434862167,-6.91979410950631,49.8686362195968));
#81643=CARTESIAN_POINT('Ctrl Pts',(4.49050673396954,-5.41752483453627,50.0274000205284));
#81644=CARTESIAN_POINT('Ctrl Pts',(7.25772385413221,-1.68020358831217,50.2390850884371));
#81645=CARTESIAN_POINT('Ctrl Pts',(6.52191938756684,4.62069350307433,50.5036914233229));
#81646=CARTESIAN_POINT('Ctrl Pts',(-0.370196312537869,7.99024439055812,
50.821219025186));
#81647=CARTESIAN_POINT('Ctrl Pts',(-5.7976781129181,4.67789307268023,51.0858253600718));
#81648=CARTESIAN_POINT('Ctrl Pts',(-7.02638206986709,0.211779819018986,
51.2975104279806));
#81649=CARTESIAN_POINT('Ctrl Pts',(-6.06095043134714,-4.34177087495216,
51.5091954958891));
#81650=CARTESIAN_POINT('Ctrl Pts',(-1.8935103873323,-7.20923062192969,51.720880563798));
#81651=CARTESIAN_POINT('Ctrl Pts',(2.71389567867474,-6.49222140291163,51.9325656317066));
#81652=CARTESIAN_POINT('Ctrl Pts',(5.49437467211685,-4.4201900172914,52.091329432638));
#81653=CARTESIAN_POINT('Ctrl Pts',(6.92410772430388,-1.25337874674743,52.2500932335697));
#81654=CARTESIAN_POINT('Ctrl Pts',(6.63474741870759,3.38788522994228,52.4617783014783));
#81655=CARTESIAN_POINT('Ctrl Pts',(2.01451281749849,7.73485481795531,52.7263846363642));
#81656=CARTESIAN_POINT('Ctrl Pts',(-5.4283157206323,5.87489907724322,53.0439122382272));
#81657=CARTESIAN_POINT('Ctrl Pts',(-7.44795076465959,-0.154222271479397,
53.3085185731131));
#81658=CARTESIAN_POINT('Ctrl Pts',(-5.51220154616398,-4.36239954562491,
53.5202036410217));
#81659=CARTESIAN_POINT('Ctrl Pts',(-1.8414328961365,-7.22462589731171,53.7318887089303));
#81660=CARTESIAN_POINT('Ctrl Pts',(3.19346001799998,-6.73499820763055,53.9435737768392));
#81661=CARTESIAN_POINT('Ctrl Pts',(6.25685497067417,-3.21961711542544,54.1552588447478));
#81662=CARTESIAN_POINT('Ctrl Pts',(7.04995532691501,0.156085676522665,54.3140226456793));
#81663=CARTESIAN_POINT('Ctrl Pts',(6.10465899868012,3.4996234819296,54.4727864466108));
#81664=CARTESIAN_POINT('Ctrl Pts',(2.89466709040366,6.8642947339467,54.6844715145196));
#81665=CARTESIAN_POINT('Ctrl Pts',(-3.43934211748364,7.21506525693325,54.9490778494054));
#81666=CARTESIAN_POINT('Ctrl Pts',(-7.93613092206531,0.999438039044138,
55.2666054512683));
#81667=CARTESIAN_POINT('Ctrl Pts',(-5.59906442082156,-4.9138817137095,55.5312117861543));
#81668=CARTESIAN_POINT('Ctrl Pts',(-1.40830596774888,-6.88705809370141,
55.742896854063));
#81669=CARTESIAN_POINT('Ctrl Pts',(3.24321731397379,-6.71324338105273,55.9545819219718));
#81670=CARTESIAN_POINT('Ctrl Pts',(6.78009525479357,-3.09656232163611,56.1662669898803));
#81671=CARTESIAN_POINT('Ctrl Pts',(6.86024957327956,1.56561130116725,56.3779520577891));
#81672=CARTESIAN_POINT('Ctrl Pts',(5.29336186929955,4.65903061347959,56.5367158587205));
#81673=CARTESIAN_POINT('Ctrl Pts',(2.41714860448358,6.60844892251285,56.6954796596521));
#81674=CARTESIAN_POINT('Ctrl Pts',(-2.2053685445281,7.11575807266166,56.9071647275608));
#81675=CARTESIAN_POINT('Ctrl Pts',(-7.27734816230319,3.30552458122617,57.1717710624466));
#81676=CARTESIAN_POINT('Ctrl Pts',(-6.71542285986649,-4.34556492744316,
57.4892986643097));
#81677=CARTESIAN_POINT('Ctrl Pts',(-1.11967013848367,-7.36494098405521,
57.7539049991955));
#81678=CARTESIAN_POINT('Ctrl Pts',(3.35725491809626,-6.17605316957025,57.9655900671042));
#81679=CARTESIAN_POINT('Ctrl Pts',(6.80409863169368,-3.04793048229254,58.177275135013));
#81680=CARTESIAN_POINT('Ctrl Pts',(7.18145534865284,1.99679094230443,58.3889602029215));
#81681=CARTESIAN_POINT('Ctrl Pts',(4.24045344088747,5.61516113422602,58.6006452708304));
#81682=CARTESIAN_POINT('Ctrl Pts',(1.05016417991309,6.97336544192119,58.7594090717617));
#81683=CARTESIAN_POINT('Ctrl Pts',(-2.4065154837537,6.61202906035096,58.9181728726935));
#81684=CARTESIAN_POINT('Ctrl Pts',(-6.26811999573962,4.0252049886518,59.1298579406019));
#81685=CARTESIAN_POINT('Ctrl Pts',(-7.69876535826759,-2.15922222239559,
59.3944642754879));
#81686=CARTESIAN_POINT('Ctrl Pts',(-2.3354816390472,-7.64507444656264,59.7119918773507));
#81687=CARTESIAN_POINT('Ctrl Pts',(3.87865942051839,-6.36236462354854,59.9765982122369));
#81688=CARTESIAN_POINT('Ctrl Pts',(6.55508373605099,-2.55465868456236,60.1882832801454));
#81689=CARTESIAN_POINT('Ctrl Pts',(6.99518748195096,0.879984397019229,60.347047081077));
#81690=CARTESIAN_POINT('Ctrl Pts',(5.71206067810625,4.12746479532865,60.5058755303524));
#81691=CARTESIAN_POINT('Ctrl Pts',(3.93417824599609,5.61116415437882,60.6117827126507));
#81692=CARTESIAN_POINT('Ctrl Pts',(2.91924481736993,6.09709494952001,60.6647686279718));
#81693=CARTESIAN_POINT('Ctrl Pts',(3.93301173192297,-5.51252654933401,60.));
#81694=CARTESIAN_POINT('Ctrl Pts',(4.08943068438299,-5.42065063936855,60.0000000000001));
#81695=CARTESIAN_POINT('Ctrl Pts',(4.24173339265253,-5.32238226638426,60.));
#81696=CARTESIAN_POINT('Ctrl Pts',(4.38947572522442,-5.21781239717694,60.));
#81697=CARTESIAN_POINT('Ctrl Pts',(4.53944789002314,-5.11166428522596,60.));
#81698=CARTESIAN_POINT('Ctrl Pts',(4.6847220474222,-4.99902354735396,60.));
#81699=CARTESIAN_POINT('Ctrl Pts',(4.82511408164218,-4.88038463662292,60.));
#81700=CARTESIAN_POINT('Ctrl Pts',(4.96550611586215,-4.76174572589187,60.));
#81701=CARTESIAN_POINT('Ctrl Pts',(5.10101645190341,-4.63710808992744,60.));
#81702=CARTESIAN_POINT('Ctrl Pts',(5.23143491853015,-4.50691912389382,59.9999999999999));
#81703=CARTESIAN_POINT('Ctrl Pts',(5.25943563992776,-4.47896767605638,59.9999999999999));
#81704=CARTESIAN_POINT('Ctrl Pts',(5.28720153910478,-4.45076018096386,59.9999999999999));
#81705=CARTESIAN_POINT('Ctrl Pts',(5.31473034986051,-4.42230082168352,59.9999999999999));
#81706=CARTESIAN_POINT('Ctrl Pts',(5.33559713591147,-4.40072868162566,59.9999999999999));
#81707=CARTESIAN_POINT('Ctrl Pts',(5.3563286782172,-4.37901069779888,59.9999999999999));
#81708=CARTESIAN_POINT('Ctrl Pts',(5.37691127712948,-4.35716240021337,59.9999999999999));
#81709=CARTESIAN_POINT('Ctrl Pts',(5.50477144804138,-4.22143964356225,59.9999999999999));
#81710=CARTESIAN_POINT('Ctrl Pts',(5.62699841484352,-4.08057724269767,59.9999999999999));
#81711=CARTESIAN_POINT('Ctrl Pts',(5.74340953646046,-3.93507696910473,59.9999999999999));
#81712=CARTESIAN_POINT('Ctrl Pts',(5.86128096626322,-3.78775148124004,60.));
#81713=CARTESIAN_POINT('Ctrl Pts',(5.97319021681194,-3.63567053260053,60.));
#81714=CARTESIAN_POINT('Ctrl Pts',(6.07891840170064,-3.47931011242737,59.9999999999999));
#81715=CARTESIAN_POINT('Ctrl Pts',(6.18542930740369,-3.32179213378919,59.9999999999999));
#81716=CARTESIAN_POINT('Ctrl Pts',(6.28566780084611,-3.15993050846068,59.9999999999999));
#81717=CARTESIAN_POINT('Ctrl Pts',(6.37937298743066,-2.99417480689384,60.));
#81718=CARTESIAN_POINT('Ctrl Pts',(6.39382678116988,-2.96860739906009,60.));
#81719=CARTESIAN_POINT('Ctrl Pts',(6.4081250523425,-2.94294728093287,60.));
#81720=CARTESIAN_POINT('Ctrl Pts',(6.42226675335339,-2.91719603854252,60.));
#81721=CARTESIAN_POINT('Ctrl Pts',(6.43451668575209,-2.89488960042585,60.));
#81722=CARTESIAN_POINT('Ctrl Pts',(6.44664514426399,-2.8725220233613,59.9999999999999));
#81723=CARTESIAN_POINT('Ctrl Pts',(6.45864972514055,-2.85009817405855,59.9999999999999));
#81724=CARTESIAN_POINT('Ctrl Pts',(6.50694144611864,-2.75989208648933,59.9999999999999));
#81725=CARTESIAN_POINT('Ctrl Pts',(6.55323905636916,-2.66875676359713,60.));
#81726=CARTESIAN_POINT('Ctrl Pts',(6.59751447498518,-2.57677045843172,60.));
#81727=CARTESIAN_POINT('Ctrl Pts',(6.68196077380915,-2.40132540886417,60.));
#81728=CARTESIAN_POINT('Ctrl Pts',(6.75905350802381,-2.22278690146021,60.));
#81729=CARTESIAN_POINT('Ctrl Pts',(6.82877465833766,-2.04163087927507,60.));
#81730=CARTESIAN_POINT('Ctrl Pts',(6.89802150956567,-1.86170722539323,60.));
#81731=CARTESIAN_POINT('Ctrl Pts',(6.95999692380297,-1.67920088449624,60.));
#81732=CARTESIAN_POINT('Ctrl Pts',(7.01464054137877,-1.49454522797912,60.));
#81733=CARTESIAN_POINT('Ctrl Pts',(7.06984557259439,-1.30799240196921,60.));
#81734=CARTESIAN_POINT('Ctrl Pts',(7.1175677183855,-1.11924526300582,60.));
#81735=CARTESIAN_POINT('Ctrl Pts',(7.15769680819296,-0.928726386214075,
60.0000000000001));
#81736=CARTESIAN_POINT('Ctrl Pts',(7.19782589800042,-0.738207509422325,
60.0000000000001));
#81737=CARTESIAN_POINT('Ctrl Pts',(7.23036220953441,-0.545916226512543,
60.));
#81738=CARTESIAN_POINT('Ctrl Pts',(7.25514335619632,-0.352260600144331,
60.));
#81739=CARTESIAN_POINT('Ctrl Pts',(7.25810700464038,-0.32910076805098,60.));
#81740=CARTESIAN_POINT('Ctrl Pts',(7.26095967090388,-0.305921412473712,
60.));
#81741=CARTESIAN_POINT('Ctrl Pts',(7.2637010242391,-0.282723224613104,60.));
#81742=CARTESIAN_POINT('Ctrl Pts',(7.26647943597639,-0.259211436983195,
60.));
#81743=CARTESIAN_POINT('Ctrl Pts',(7.26914233841631,-0.235690110937071,
60.0000000000001));
#81744=CARTESIAN_POINT('Ctrl Pts',(7.27168943529372,-0.212162315957714,
60.));
#81745=CARTESIAN_POINT('Ctrl Pts',(7.29297172671287,-0.0155756083033903,
60.0000000000001));
#81746=CARTESIAN_POINT('Ctrl Pts',(7.30617899232667,0.181512276274655,60.0000000000001));
#81747=CARTESIAN_POINT('Ctrl Pts',(7.31126922514826,0.378646193900632,60.0000000000001));
#81748=CARTESIAN_POINT('Ctrl Pts',(7.31596526012799,0.5605136654503,60.));
#81749=CARTESIAN_POINT('Ctrl Pts',(7.3137524527044,0.74242103248043,60.));
#81750=CARTESIAN_POINT('Ctrl Pts',(7.30456172141971,0.924026543563235,60.));
#81751=CARTESIAN_POINT('Ctrl Pts',(7.29474439159223,1.11801341420085,60.));
#81752=CARTESIAN_POINT('Ctrl Pts',(7.27696618509513,1.31165628281886,60.));
#81753=CARTESIAN_POINT('Ctrl Pts',(7.25145299411574,1.50450172189991,60.));
#81754=CARTESIAN_POINT('Ctrl Pts',(7.22565302124297,1.69951484671629,60.));
#81755=CARTESIAN_POINT('Ctrl Pts',(7.19194313577524,1.89371321377546,60.));
#81756=CARTESIAN_POINT('Ctrl Pts',(7.15050363732496,2.08662930880182,60.));
#81757=CARTESIAN_POINT('Ctrl Pts',(7.1179488313502,2.2381838950748,60.));
#81758=CARTESIAN_POINT('Ctrl Pts',(7.08062249907401,2.38894725733733,60.));
#81759=CARTESIAN_POINT('Ctrl Pts',(7.03858982148013,2.53868895506453,59.9999999999999));
#81760=CARTESIAN_POINT('Ctrl Pts',(7.03300180162727,2.55859631351987,59.9999999999999));
#81761=CARTESIAN_POINT('Ctrl Pts',(7.02733083309508,2.57848457739548,59.9999999999999));
#81762=CARTESIAN_POINT('Ctrl Pts',(7.02157995933159,2.5983435215292,59.9999999999999));
#81763=CARTESIAN_POINT('Ctrl Pts',(6.9659804061741,2.79034015811396,59.9999999999999));
#81764=CARTESIAN_POINT('Ctrl Pts',(6.9028482219688,2.9798404774229,59.9999999999999));
#81765=CARTESIAN_POINT('Ctrl Pts',(6.8324580727966,3.16637611832398,59.9999999999999));
#81766=CARTESIAN_POINT('Ctrl Pts',(6.76136569194129,3.35477269059982,59.9999999999999));
#81767=CARTESIAN_POINT('Ctrl Pts',(6.68286970430263,3.54014584826076,59.9999999999999));
#81768=CARTESIAN_POINT('Ctrl Pts',(6.59719965578521,3.72201525869361,59.9999999999999));
#81769=CARTESIAN_POINT('Ctrl Pts',(6.51129089759076,3.90439142719392,60.));
#81770=CARTESIAN_POINT('Ctrl Pts',(6.41816787659654,4.08324503974194,59.9999999999999));
#81771=CARTESIAN_POINT('Ctrl Pts',(6.3180107511728,4.2580829378152,59.9999999999999));
#81772=CARTESIAN_POINT('Ctrl Pts',(6.27742617235638,4.32892884542708,59.9999999999999));
#81773=CARTESIAN_POINT('Ctrl Pts',(6.23568606124396,4.39911523202738,60.));
#81774=CARTESIAN_POINT('Ctrl Pts',(6.19280011122803,4.46860844401259,60.));
#81775=CARTESIAN_POINT('Ctrl Pts',(6.08722571743203,4.63968320685557,60.));
#81776=CARTESIAN_POINT('Ctrl Pts',(5.97471037226409,4.80655917740463,59.9999999999999));
#81777=CARTESIAN_POINT('Ctrl Pts',(5.85558066445649,4.96895350572671,60.));
#81778=CARTESIAN_POINT('Ctrl Pts',(5.81668657376114,5.02197285623473,60.0000000000001));
#81779=CARTESIAN_POINT('Ctrl Pts',(5.7770870938084,5.07451426995668,60.));
#81780=CARTESIAN_POINT('Ctrl Pts',(5.73679261859994,5.12656719766218,60.));
#81781=CARTESIAN_POINT('Ctrl Pts',(5.71566740085255,5.15385702899708,60.));
#81782=CARTESIAN_POINT('Ctrl Pts',(5.69434724576312,5.18101737942238,60.));
#81783=CARTESIAN_POINT('Ctrl Pts',(5.67285512479792,5.20801998658619,60.));
#81784=CARTESIAN_POINT('Ctrl Pts',(5.54699632712769,5.36614843175431,60.));
#81785=CARTESIAN_POINT('Ctrl Pts',(5.41513767804764,5.51901110932468,60.));
#81786=CARTESIAN_POINT('Ctrl Pts',(5.27770276549599,5.66637944969325,60.));
#81787=CARTESIAN_POINT('Ctrl Pts',(5.13773272163551,5.81646615387973,60.));
#81788=CARTESIAN_POINT('Ctrl Pts',(4.99197850428412,5.96085449177701,60.));
#81789=CARTESIAN_POINT('Ctrl Pts',(4.84083762292807,6.0992821473738,60.));
#81790=CARTESIAN_POINT('Ctrl Pts',(4.68918631562009,6.23817729440803,60.));
#81791=CARTESIAN_POINT('Ctrl Pts',(4.5321114673821,6.37107194887579,60.0000000000001));
#81792=CARTESIAN_POINT('Ctrl Pts',(4.36997047171315,6.49767239337633,60.0000000000001));
#81793=CARTESIAN_POINT('Ctrl Pts',(4.20894762566035,6.62339978144942,60.));
#81794=CARTESIAN_POINT('Ctrl Pts',(4.04292777468119,6.74291993626482,60.));
#81795=CARTESIAN_POINT('Ctrl Pts',(3.87222449617968,6.8559096253412,60.));
#81796=CARTESIAN_POINT('Ctrl Pts',(3.7251270308196,6.95327446227263,60.));
#81797=CARTESIAN_POINT('Ctrl Pts',(3.57455113397834,7.04578972027165,60.));
#81798=CARTESIAN_POINT('Ctrl Pts',(3.4206796250975,7.13322310757506,60.));
#81799=CARTESIAN_POINT('Ctrl Pts',(3.4248577137498,7.13737126555389,-60.));
#81800=CARTESIAN_POINT('Ctrl Pts',(3.60861991098295,7.03458684113382,-60.));
#81801=CARTESIAN_POINT('Ctrl Pts',(3.78767901468881,6.92437773889514,-60.));
#81802=CARTESIAN_POINT('Ctrl Pts',(3.96154458364234,6.80675795931553,-60.));
#81803=CARTESIAN_POINT('Ctrl Pts',(4.13076522420728,6.69228046636872,-60.));
#81804=CARTESIAN_POINT('Ctrl Pts',(4.29506657128387,6.57078249333906,-60.));
#81805=CARTESIAN_POINT('Ctrl Pts',(4.45418747522949,6.44274262314797,-60.));
#81806=CARTESIAN_POINT('Ctrl Pts',(4.61440833160287,6.31381765387451,-60.));
#81807=CARTESIAN_POINT('Ctrl Pts',(4.76937730965001,6.17825938241126,-60.));
#81808=CARTESIAN_POINT('Ctrl Pts',(4.91878898868684,6.03651990623725,-60.));
#81809=CARTESIAN_POINT('Ctrl Pts',(5.0675274265728,5.89541910067236,-60.));
#81810=CARTESIAN_POINT('Ctrl Pts',(5.21075889024205,5.74819197850466,-60.));
#81811=CARTESIAN_POINT('Ctrl Pts',(5.34813792788795,5.595258661849,-60.));
#81812=CARTESIAN_POINT('Ctrl Pts',(5.46090011722494,5.46972935327202,-60.));
#81813=CARTESIAN_POINT('Ctrl Pts',(5.56971864085314,5.34035497301831,-60.));
#81814=CARTESIAN_POINT('Ctrl Pts',(5.67437750866333,5.20735958609987,-60.));
#81815=CARTESIAN_POINT('Ctrl Pts',(5.69455286498308,5.18172172687107,-60.));
#81816=CARTESIAN_POINT('Ctrl Pts',(5.71457658133583,5.15594526087748,-60.));
#81817=CARTESIAN_POINT('Ctrl Pts',(5.73442860333554,5.13005609206325,-60.));
#81818=CARTESIAN_POINT('Ctrl Pts',(5.85765046658865,4.96936154823243,-60.));
#81819=CARTESIAN_POINT('Ctrl Pts',(5.97438553496247,4.80417296037974,-60.));
#81820=CARTESIAN_POINT('Ctrl Pts',(6.08437659315306,4.63494157400739,-60.));
#81821=CARTESIAN_POINT('Ctrl Pts',(6.19442667221929,4.46561937857496,-60.));
#81822=CARTESIAN_POINT('Ctrl Pts',(6.29772586482784,4.29224936825753,-60.));
#81823=CARTESIAN_POINT('Ctrl Pts',(6.39397171685177,4.11525752541809,-60.));
#81824=CARTESIAN_POINT('Ctrl Pts',(6.42699095565242,4.05453661327915,-60.));
#81825=CARTESIAN_POINT('Ctrl Pts',(6.45917961583643,3.99338923911971,-60.));
#81826=CARTESIAN_POINT('Ctrl Pts',(6.49052415144755,3.93183211822112,-60.));
#81827=CARTESIAN_POINT('Ctrl Pts',(6.58200931504942,3.75216560964246,-60.));
#81828=CARTESIAN_POINT('Ctrl Pts',(6.66630731358913,3.56900914058539,-60.));
#81829=CARTESIAN_POINT('Ctrl Pts',(6.7432492526404,3.38277223025193,-60.));
#81830=CARTESIAN_POINT('Ctrl Pts',(6.81951943947852,3.19816128695583,-60.));
#81831=CARTESIAN_POINT('Ctrl Pts',(6.88856152296434,3.01052281825039,-60.));
#81832=CARTESIAN_POINT('Ctrl Pts',(6.95016018173248,2.82025301605453,-60.));
#81833=CARTESIAN_POINT('Ctrl Pts',(6.96705468955314,2.76806820025631,-60.));
#81834=CARTESIAN_POINT('Ctrl Pts',(6.98338898298803,2.71568546353412,-60.));
#81835=CARTESIAN_POINT('Ctrl Pts',(6.99915793217927,2.66311304111913,-60.));
#81836=CARTESIAN_POINT('Ctrl Pts',(7.00922467652644,2.62955131612756,-60.));
#81837=CARTESIAN_POINT('Ctrl Pts',(7.01906101322371,2.59591228702048,-60.));
#81838=CARTESIAN_POINT('Ctrl Pts',(7.02866554329771,2.56219810720566,-60.));
#81839=CARTESIAN_POINT('Ctrl Pts',(7.03567914496781,2.53757870094282,-60.));
#81840=CARTESIAN_POINT('Ctrl Pts',(7.04256711476104,2.51292621131787,-60.));
#81841=CARTESIAN_POINT('Ctrl Pts',(7.0493270299122,2.48824942657131,-60.));
#81842=CARTESIAN_POINT('Ctrl Pts',(7.06363748749976,2.43600970556635,-60.));
#81843=CARTESIAN_POINT('Ctrl Pts',(7.07737720041661,2.38365021216742,-60.));
#81844=CARTESIAN_POINT('Ctrl Pts',(7.09054441676118,2.3311792008664,-60.));
#81845=CARTESIAN_POINT('Ctrl Pts',(7.13858283449617,2.139747367904,-60.));
#81846=CARTESIAN_POINT('Ctrl Pts',(7.17900498375673,1.94683219772224,-60.));
#81847=CARTESIAN_POINT('Ctrl Pts',(7.21169252079291,1.75283065323041,-60.));
#81848=CARTESIAN_POINT('Ctrl Pts',(7.24420959030436,1.55984083877647,-60.));
#81849=CARTESIAN_POINT('Ctrl Pts',(7.2690725791835,1.36577531784115,-60.));
#81850=CARTESIAN_POINT('Ctrl Pts',(7.28611380189689,1.17102122652283,-60.));
#81851=CARTESIAN_POINT('Ctrl Pts',(7.30289509392125,0.979237729861928,-60.));
#81852=CARTESIAN_POINT('Ctrl Pts',(7.31209139548342,0.78678594030478,-60.));
#81853=CARTESIAN_POINT('Ctrl Pts',(7.31349255663583,0.594040875125159,-60.));
#81854=CARTESIAN_POINT('Ctrl Pts',(7.31410769614461,0.50942169730248,-60.));
#81855=CARTESIAN_POINT('Ctrl Pts',(7.31321974938026,0.424746113772566,-60.));
#81856=CARTESIAN_POINT('Ctrl Pts',(7.31080782602045,0.340046611414358,-60.));
#81857=CARTESIAN_POINT('Ctrl Pts',(7.30678229620877,0.198682098155049,-60.));
#81858=CARTESIAN_POINT('Ctrl Pts',(7.29851215479959,0.057250540439187,-60.));
#81859=CARTESIAN_POINT('Ctrl Pts',(7.2860244774147,-0.0840501440206062,
-60.));
#81860=CARTESIAN_POINT('Ctrl Pts',(7.28245939678781,-0.124389777821812,
-60.));
#81861=CARTESIAN_POINT('Ctrl Pts',(7.27855049671512,-0.164718701457005,
-60.));
#81862=CARTESIAN_POINT('Ctrl Pts',(7.27429822708433,-0.20503219790969,-60.));
#81863=CARTESIAN_POINT('Ctrl Pts',(7.27144834789734,-0.232050379838477,
-60.));
#81864=CARTESIAN_POINT('Ctrl Pts',(7.26844391232975,-0.259064365716766,
-60.));
#81865=CARTESIAN_POINT('Ctrl Pts',(7.26528611071862,-0.28606362287843,-60.));
#81866=CARTESIAN_POINT('Ctrl Pts',(7.26002333336482,-0.331060458227003,
-60.));
#81867=CARTESIAN_POINT('Ctrl Pts',(7.25433702839529,-0.375996037536274,
-60.));
#81868=CARTESIAN_POINT('Ctrl Pts',(7.24823054744924,-0.420859007874808,
-60.));
#81869=CARTESIAN_POINT('Ctrl Pts',(7.22223958985405,-0.611808847883335,
-60.));
#81870=CARTESIAN_POINT('Ctrl Pts',(7.18863664734709,-0.801478953923177,
-60.));
#81871=CARTESIAN_POINT('Ctrl Pts',(7.14759919930349,-0.98939764097146,-60.));
#81872=CARTESIAN_POINT('Ctrl Pts',(7.10643012046813,-1.17791909175732,-60.));
#81873=CARTESIAN_POINT('Ctrl Pts',(7.05777850127931,-1.36467859587107,-60.));
#81874=CARTESIAN_POINT('Ctrl Pts',(7.00177368720448,-1.54918517106434,-60.));
#81875=CARTESIAN_POINT('Ctrl Pts',(6.94620176777722,-1.73226558477193,-60.));
#81876=CARTESIAN_POINT('Ctrl Pts',(6.88338955967928,-1.91312842201592,-60.));
#81877=CARTESIAN_POINT('Ctrl Pts',(6.81341899657811,-2.09126921993615,-60.));
#81878=CARTESIAN_POINT('Ctrl Pts',(6.74495504259696,-2.26557428267148,-60.));
#81879=CARTESIAN_POINT('Ctrl Pts',(6.66963730643464,-2.4372737762835,-60.));
#81880=CARTESIAN_POINT('Ctrl Pts',(6.58750516330558,-2.60586284078176,-60.));
#81881=CARTESIAN_POINT('Ctrl Pts',(6.53702924311811,-2.70947255848659,-60.));
#81882=CARTESIAN_POINT('Ctrl Pts',(6.48397884068404,-2.81190681635542,-60.));
#81883=CARTESIAN_POINT('Ctrl Pts',(6.42835674087745,-2.91304091849508,-60.));
#81884=CARTESIAN_POINT('Ctrl Pts',(6.40310580363065,-2.95895308066658,-60.));
#81885=CARTESIAN_POINT('Ctrl Pts',(6.37734514144749,-3.00456010758804,-60.));
#81886=CARTESIAN_POINT('Ctrl Pts',(6.35108059795691,-3.04984579985723,-60.));
#81887=CARTESIAN_POINT('Ctrl Pts',(6.34509772234999,-3.06016155743805,-60.));
#81888=CARTESIAN_POINT('Ctrl Pts',(6.33908864170211,-3.07046074555373,-60.));
#81889=CARTESIAN_POINT('Ctrl Pts',(6.33305338320512,-3.08074324429301,-60.));
#81890=CARTESIAN_POINT('Ctrl Pts',(6.23708789041981,-3.24424329306003,-60.));
#81891=CARTESIAN_POINT('Ctrl Pts',(6.13450706082851,-3.40352647237428,-60.));
#81892=CARTESIAN_POINT('Ctrl Pts',(6.02564607812735,-3.55828730005497,-60.));
#81893=CARTESIAN_POINT('Ctrl Pts',(5.91677903996887,-3.71305673639935,-60.));
#81894=CARTESIAN_POINT('Ctrl Pts',(5.80163059279153,-3.8633037709451,-60.));
#81895=CARTESIAN_POINT('Ctrl Pts',(5.68050054265185,-4.00868504968493,-60.));
#81896=CARTESIAN_POINT('Ctrl Pts',(5.57662125738459,-4.1333618190689,-60.));
#81897=CARTESIAN_POINT('Ctrl Pts',(5.46834202505428,-4.2544596084174,-60.));
#81898=CARTESIAN_POINT('Ctrl Pts',(5.35583581478516,-4.37173590025246,-60.));
#81899=CARTESIAN_POINT('Ctrl Pts',(5.33669698721178,-4.39168618319691,-60.));
#81900=CARTESIAN_POINT('Ctrl Pts',(5.31743557941832,-4.41152596850129,-60.));
#81901=CARTESIAN_POINT('Ctrl Pts',(5.29806298900613,-4.43124345790525,-60.));
#81902=CARTESIAN_POINT('Ctrl Pts',(5.16723317262104,-4.56440249670221,-60.));
#81903=CARTESIAN_POINT('Ctrl Pts',(5.03121965193352,-4.69210870498326,-60.));
#81904=CARTESIAN_POINT('Ctrl Pts',(4.89032787541421,-4.8140473373547,-60.));
#81905=CARTESIAN_POINT('Ctrl Pts',(4.75110811375755,-4.93453887884054,-60.));
#81906=CARTESIAN_POINT('Ctrl Pts',(4.60712461558511,-5.04939924921015,-60.));
#81907=CARTESIAN_POINT('Ctrl Pts',(4.45864629338521,-5.15828165385862,-60.));
#81908=CARTESIAN_POINT('Ctrl Pts',(4.31072242009514,-5.26675746898168,-60.));
#81909=CARTESIAN_POINT('Ctrl Pts',(4.15833671963038,-5.3693002495206,-60.));
#81910=CARTESIAN_POINT('Ctrl Pts',(4.00173737932556,-5.46551877007183,-60.));
#81911=CARTESIAN_POINT('Ctrl Pts',(3.97755260405217,-5.48037849612265,-60.));
#81912=CARTESIAN_POINT('Ctrl Pts',(3.9532673039551,-5.49508728270992,-60.));
#81913=CARTESIAN_POINT('Ctrl Pts',(3.92888236737297,-5.50964357679758,-60.));
#81914=CARTESIAN_POINT('Origin',(-15.3358035470651,3.40523243981596E-15,
65.));
#81915=CARTESIAN_POINT('',(-13.3358035470651,3.65016179964543E-15,65.));
#81916=CARTESIAN_POINT('Origin',(-15.3358035470651,3.40523243981596E-15,
65.));
#81917=CARTESIAN_POINT('',(-13.3358035470651,3.65016179964543E-15,60.));
#81918=CARTESIAN_POINT('',(-13.3358035470651,3.16030307998649E-15,65.));
#81919=CARTESIAN_POINT('Origin',(-15.3358035470651,3.40523243981596E-15,
60.));
#81920=CARTESIAN_POINT('Origin',(0.,-15.3358035470651,65.));
#81921=CARTESIAN_POINT('',(2.,-15.3358035470651,65.));
#81922=CARTESIAN_POINT('Origin',(0.,-15.3358035470651,65.));
#81923=CARTESIAN_POINT('',(2.,-15.3358035470651,60.));
#81924=CARTESIAN_POINT('',(2.,-15.3358035470651,65.));
#81925=CARTESIAN_POINT('Origin',(0.,-15.3358035470651,60.));
#81926=CARTESIAN_POINT('Origin',(1.87809427262659E-15,15.3358035470651,
65.));
#81927=CARTESIAN_POINT('',(2.,15.3358035470651,65.));
#81928=CARTESIAN_POINT('Origin',(1.87809427262659E-15,15.3358035470651,
65.));
#81929=CARTESIAN_POINT('',(2.,15.3358035470651,60.));
#81930=CARTESIAN_POINT('',(2.,15.3358035470651,65.));
#81931=CARTESIAN_POINT('Origin',(1.87809427262659E-15,15.3358035470651,
60.));
#81932=CARTESIAN_POINT('Origin',(15.3358035470651,3.40523243981596E-15,
65.));
#81933=CARTESIAN_POINT('',(17.3358035470651,3.65016179964543E-15,65.));
#81934=CARTESIAN_POINT('Origin',(15.3358035470651,3.40523243981596E-15,
65.));
#81935=CARTESIAN_POINT('',(17.3358035470651,3.65016179964543E-15,60.));
#81936=CARTESIAN_POINT('',(17.3358035470651,3.16030307998649E-15,65.));
#81937=CARTESIAN_POINT('Origin',(15.3358035470651,3.40523243981596E-15,
60.));
#81938=CARTESIAN_POINT('Origin',(0.,0.,61.));
#81939=CARTESIAN_POINT('',(20.,-2.44929359829471E-15,61.));
#81940=CARTESIAN_POINT('',(-20.,-2.44929359829471E-15,61.));
#81941=CARTESIAN_POINT('Origin',(0.,0.,61.));
#81942=CARTESIAN_POINT('',(-19.,-2.32682891837997E-15,60.));
#81943=CARTESIAN_POINT('Origin',(-19.,-2.32682891837997E-15,61.));
#81944=CARTESIAN_POINT('Origin',(0.,0.,60.));
#81945=CARTESIAN_POINT('Origin',(0.,0.,61.));
#81946=CARTESIAN_POINT('Origin',(0.,0.,60.));
#81947=CARTESIAN_POINT('',(-20.,-2.44929359829471E-15,64.));
#81948=CARTESIAN_POINT('',(20.,2.44929359829471E-15,64.));
#81949=CARTESIAN_POINT('Origin',(0.,0.,64.));
#81950=CARTESIAN_POINT('Origin',(0.,0.,64.));
#81951=CARTESIAN_POINT('',(20.,2.44929359829471E-15,60.));
#81952=CARTESIAN_POINT('Origin',(0.,0.,60.));
#81953=CARTESIAN_POINT('Origin',(0.,0.,64.));
#81954=CARTESIAN_POINT('',(-19.,-2.32682891837997E-15,65.));
#81955=CARTESIAN_POINT('Origin',(0.,0.,65.));
#81956=CARTESIAN_POINT('Origin',(-19.,-2.32682891837997E-15,64.));
#81957=CARTESIAN_POINT('Origin',(0.,0.,65.));
#81958=CARTESIAN_POINT('Origin',(0.,0.,-60.));
#81959=CARTESIAN_POINT('',(0.,0.,0.));
#81960=CARTESIAN_POINT('Origin',(-31.4159265358979,26.,7.7715611723761E-15));
#81961=CARTESIAN_POINT('',(-13.2129142961191,30.2426811775992,-4.2426001962529));
#81962=CARTESIAN_POINT('',(-15.0614191220869,30.2426782484473,-4.24260312545867));
#81963=CARTESIAN_POINT('',(-31.4159265358979,30.2426406871193,-4.24264068711928));
#81964=CARTESIAN_POINT('',(-14.7837106730077,21.7573593180495,-4.24264068195052));
#81965=CARTESIAN_POINT('Ctrl Pts',(-13.2129142961191,30.2426811775992,-4.2426001962529));
#81966=CARTESIAN_POINT('Ctrl Pts',(-13.2410017129647,30.1234962961936,-4.36178735262007));
#81967=CARTESIAN_POINT('Ctrl Pts',(-13.2690891298103,29.999287665009,-4.47594744906339));
#81968=CARTESIAN_POINT('Ctrl Pts',(-13.2971765466559,29.8705004317943,-4.5846729880636));
#81969=CARTESIAN_POINT('Ctrl Pts',(-13.3252684134104,29.741692794729,-4.6934157525263));
#81970=CARTESIAN_POINT('Ctrl Pts',(-13.3533602801649,29.6083053406003,-4.79672204033205));
#81971=CARTESIAN_POINT('Ctrl Pts',(-13.3814521469194,29.4708168269235,-4.89422420348155));
#81972=CARTESIAN_POINT('Ctrl Pts',(-13.4000726886277,29.3796833103903,-4.95885298416863));
#81973=CARTESIAN_POINT('Ctrl Pts',(-13.4186932303359,29.286748621905,-5.02093247673682));
#81974=CARTESIAN_POINT('Ctrl Pts',(-13.4373137720442,29.1921594803238,-5.08036591715385));
#81975=CARTESIAN_POINT('Ctrl Pts',(-13.4652952223468,29.0500185369615,-5.16967770439425));
#81976=CARTESIAN_POINT('Ctrl Pts',(-13.4932766726495,28.9041139043336,-5.2530287541782));
#81977=CARTESIAN_POINT('Ctrl Pts',(-13.5212581229522,28.7549640208624,-5.33011943991441));
#81978=CARTESIAN_POINT('Ctrl Pts',(-13.5492367727318,28.6058290650555,-5.40720241003029));
#81979=CARTESIAN_POINT('Ctrl Pts',(-13.5772154225113,28.453449784519,-5.47802612351747));
#81980=CARTESIAN_POINT('Ctrl Pts',(-13.6051940722909,28.2983686959519,-5.54233717284218));
#81981=CARTESIAN_POINT('Ctrl Pts',(-13.6331753283905,28.1432731609781,-5.60665421299133));
#81982=CARTESIAN_POINT('Ctrl Pts',(-13.6611565844901,27.9854756029791,-5.66445725473928));
#81983=CARTESIAN_POINT('Ctrl Pts',(-13.6891378405898,27.8255386914581,-5.71554096179788));
#81984=CARTESIAN_POINT('Ctrl Pts',(-13.7171188027312,27.6656034601607,-5.76662413219454));
#81985=CARTESIAN_POINT('Ctrl Pts',(-13.7450997648726,27.5035292189573,-5.81098801655115));
#81986=CARTESIAN_POINT('Ctrl Pts',(-13.773080727014,27.3398942132321,-5.84847702375132));
#81987=CARTESIAN_POINT('Ctrl Pts',(-13.8010671071371,27.176227522697,-5.88597328998547));
#81988=CARTESIAN_POINT('Ctrl Pts',(-13.8290534872602,27.0109997688288,-5.91659195041649));
#81989=CARTESIAN_POINT('Ctrl Pts',(-13.8570398673834,26.8448005976496,-5.94022827425098));
#81990=CARTESIAN_POINT('Ctrl Pts',(-13.8667308191079,26.7872501699964,-5.94841291521625));
#81991=CARTESIAN_POINT('Ctrl Pts',(-13.8764217708324,26.7295833399769,-5.95576078735063));
#81992=CARTESIAN_POINT('Ctrl Pts',(-13.8861127225569,26.6718247952912,-5.96226898457557));
#81993=CARTESIAN_POINT('Ctrl Pts',(-13.9139899859855,26.5056749463158,-5.98099064717824));
#81994=CARTESIAN_POINT('Ctrl Pts',(-13.9418672494142,26.338713434746,-5.99276609931421));
#81995=CARTESIAN_POINT('Ctrl Pts',(-13.9697445128428,26.1715325455289,-5.99754754760846));
#81996=CARTESIAN_POINT('Ctrl Pts',(-13.9976163987277,26.0043839056231,-6.00232807355797));
#81997=CARTESIAN_POINT('Ctrl Pts',(-14.0254882846126,25.8370162900367,-6.00011727873267));
#81998=CARTESIAN_POINT('Ctrl Pts',(-14.0533601704975,25.6700239306005,-5.99091944476168));
#81999=CARTESIAN_POINT('Ctrl Pts',(-14.0812318269964,25.5030329455137,-5.98172168648899));
#82000=CARTESIAN_POINT('Ctrl Pts',(-14.1091034834953,25.336417527901,-5.96553701791644));
#82001=CARTESIAN_POINT('Ctrl Pts',(-14.1369751399941,25.1707694209928,-5.94242178298034));
#82002=CARTESIAN_POINT('Ctrl Pts',(-14.1648451281333,25.0051312295563,-5.91930793169096));
#82003=CARTESIAN_POINT('Ctrl Pts',(-14.1927151162726,24.8404605476793,-5.88926438829303));
#82004=CARTESIAN_POINT('Ctrl Pts',(-14.2205851044118,24.6773417948699,-5.85239910399162));
#82005=CARTESIAN_POINT('Ctrl Pts',(-14.2484593155124,24.5141983257171,-5.815528233729));
#82006=CARTESIAN_POINT('Ctrl Pts',(-14.276333526613,24.3526075654144,-5.77183362777214));
#82007=CARTESIAN_POINT('Ctrl Pts',(-14.3042077377136,24.1931422948714,-5.7214740437598));
#82008=CARTESIAN_POINT('Ctrl Pts',(-14.3144423828323,24.1345910251376,-5.70298338697199));
#82009=CARTESIAN_POINT('Ctrl Pts',(-14.324677027951,24.0763261658875,-5.68359467421659));
#82010=CARTESIAN_POINT('Ctrl Pts',(-14.3349116730697,24.0183755413334,-5.66331744693994));
#82011=CARTESIAN_POINT('Ctrl Pts',(-14.3630440790537,23.8590841855444,-5.60758056663204));
#82012=CARTESIAN_POINT('Ctrl Pts',(-14.3911764850377,23.7021323444495,-5.54511432266296));
#82013=CARTESIAN_POINT('Ctrl Pts',(-14.4193088910216,23.5480833323248,-5.47613957590351));
#82014=CARTESIAN_POINT('Ctrl Pts',(-14.4474378260405,23.3940533267062,-5.40717333922098));
#82015=CARTESIAN_POINT('Ctrl Pts',(-14.4755667610593,23.2429257136142,-5.33170032765871));
#82016=CARTESIAN_POINT('Ctrl Pts',(-14.5036956960782,23.0952427019562,-5.24998905136581));
#82017=CARTESIAN_POINT('Ctrl Pts',(-14.5318247858119,22.9475588780117,-5.16827732564439));
#82018=CARTESIAN_POINT('Ctrl Pts',(-14.5599538755456,22.8033199617192,-5.08032741225067));
#82019=CARTESIAN_POINT('Ctrl Pts',(-14.5880829652792,22.6630431588223,-4.98645355339013));
#82020=CARTESIAN_POINT('Ctrl Pts',(-14.6162099061363,22.5227770721466,-4.8925868658724));
#82021=CARTESIAN_POINT('Ctrl Pts',(-14.6443368469933,22.3864727472703,-4.79279730773824));
#82022=CARTESIAN_POINT('Ctrl Pts',(-14.6724637878503,22.254618346355,-4.68744240162367));
#82023=CARTESIAN_POINT('Ctrl Pts',(-14.7005922972612,22.1227565923209,-4.58208162018649));
#82024=CARTESIAN_POINT('Ctrl Pts',(-14.7287208066722,21.9953454967693,-4.47115506104073));
#82025=CARTESIAN_POINT('Ctrl Pts',(-14.7568493160831,21.8728406817017,-4.35506095954851));
#82026=CARTESIAN_POINT('Ctrl Pts',(-14.7658030852496,21.8338453755561,-4.31810628942479));
#82027=CARTESIAN_POINT('Ctrl Pts',(-14.7747568544161,21.7953469382496,-4.28062831248813));
#82028=CARTESIAN_POINT('Ctrl Pts',(-14.7837106235826,21.7573593128807,-4.24264068711927));
#82029=CARTESIAN_POINT('',(-17.341,27.1984341265848,5.87909479803116));
#82030=CARTESIAN_POINT('Ctrl Pts',(-14.783710716403,21.7573593128807,-4.24264068711927));
#82031=CARTESIAN_POINT('Ctrl Pts',(-14.811635381255,21.6388849936053,-4.12416636784387));
#82032=CARTESIAN_POINT('Ctrl Pts',(-14.839560046107,21.5253639382053,-4.0007141031509));
#82033=CARTESIAN_POINT('Ctrl Pts',(-14.8674847109591,21.4172023830087,-3.87272074925351));
#82034=CARTESIAN_POINT('Ctrl Pts',(-14.8954064382147,21.3090522061044,-3.74474085989806));
#82035=CARTESIAN_POINT('Ctrl Pts',(-14.9233281654703,21.2062606072779,-3.61222107567854));
#82036=CARTESIAN_POINT('Ctrl Pts',(-14.9512498927259,21.1091941405294,-3.47563203532363));
#82037=CARTESIAN_POINT('Ctrl Pts',(-14.9791745175235,21.0121176008308,-3.33902882061339));
#82038=CARTESIAN_POINT('Ctrl Pts',(-15.0070991423211,20.920767565003,-3.19835576152329));
#82039=CARTESIAN_POINT('Ctrl Pts',(-15.0350237671187,20.8354682159095,-3.05411385693448));
#82040=CARTESIAN_POINT('Ctrl Pts',(-15.0629484025602,20.7501688343031,-2.90987189736591));
#82041=CARTESIAN_POINT('Ctrl Pts',(-15.0908730380016,20.6709203017243,-2.76206136256888));
#82042=CARTESIAN_POINT('Ctrl Pts',(-15.1187976734431,20.598001758941,-2.61120949056086));
#82043=CARTESIAN_POINT('Ctrl Pts',(-15.1467285765726,20.5250668495812,-2.46032375983055));
#82044=CARTESIAN_POINT('Ctrl Pts',(-15.1746594797021,20.4584649048534,-2.30639561238042));
#82045=CARTESIAN_POINT('Ctrl Pts',(-15.2025903828316,20.3984280066064,-2.14997469818332));
#82046=CARTESIAN_POINT('Ctrl Pts',(-15.2125634775264,20.3769910459532,-2.09412256256521));
#82047=CARTESIAN_POINT('Ctrl Pts',(-15.2225365722211,20.3563906424098,-2.03795279762032));
#82048=CARTESIAN_POINT('Ctrl Pts',(-15.2325096669158,20.3366358561963,-1.98149099787989));
#82049=CARTESIAN_POINT('Ctrl Pts',(-15.2605103911617,20.2811717963202,-1.82296735668836));
#82050=CARTESIAN_POINT('Ctrl Pts',(-15.2885111154076,20.2323602403577,-1.66209219433237));
#82051=CARTESIAN_POINT('Ctrl Pts',(-15.3165118396535,20.1903798098822,-1.49943764344352));
#82052=CARTESIAN_POINT('Ctrl Pts',(-15.3445078536952,20.1484064412384,-1.33681045385234));
#82053=CARTESIAN_POINT('Ctrl Pts',(-15.3725038677369,20.1132619825743,-1.17240477502853));
#82054=CARTESIAN_POINT('Ctrl Pts',(-15.4004998817785,20.0850746867121,-1.00680610756265));
#82055=CARTESIAN_POINT('Ctrl Pts',(-15.4284955428502,20.0568877462315,-0.841209527942798));
#82056=CARTESIAN_POINT('Ctrl Pts',(-15.4564912039218,20.0356578486871,-0.674420296689421));
#82057=CARTESIAN_POINT('Ctrl Pts',(-15.4844868649934,20.0214619223184,-0.507032990752785));
#82058=CARTESIAN_POINT('Ctrl Pts',(-15.5124804766443,20.0072670351617,-0.339657938394383));
#82059=CARTESIAN_POINT('Ctrl Pts',(-15.5404740882952,20.0001051156435,-0.171685209709194));
#82060=CARTESIAN_POINT('Ctrl Pts',(-15.568467699946,20.0000011493054,-0.00371371286646238));
#82061=CARTESIAN_POINT('Ctrl Pts',(-15.5964640728379,19.9998971727122,0.164274352391451));
#82062=CARTESIAN_POINT('Ctrl Pts',(-15.6244604457297,20.0068525404938,0.332260873623216));
#82063=CARTESIAN_POINT('Ctrl Pts',(-15.6524568186215,20.0208401175802,0.499646975835977));
#82064=CARTESIAN_POINT('Ctrl Pts',(-15.6620740848906,20.0256451062057,0.557147164197301));
#82065=CARTESIAN_POINT('Ctrl Pts',(-15.6716913511596,20.0312794776917,0.614576523478925));
#82066=CARTESIAN_POINT('Ctrl Pts',(-15.6813086174286,20.0377407166053,0.67191088514314));
#82067=CARTESIAN_POINT('Ctrl Pts',(-15.7092296642895,20.0564991194029,0.838365192841986));
#82068=CARTESIAN_POINT('Ctrl Pts',(-15.7371507111504,20.0822345347245,1.00405202747329));
#82069=CARTESIAN_POINT('Ctrl Pts',(-15.7650717580113,20.1148590193363,1.16838163187921));
#82070=CARTESIAN_POINT('Ctrl Pts',(-15.7929896016934,20.147479761178,1.33269238394361));
#82071=CARTESIAN_POINT('Ctrl Pts',(-15.8209074453755,20.1869879332608,1.49564590721416));
#82072=CARTESIAN_POINT('Ctrl Pts',(-15.8488252890575,20.2332444334929,1.65666237844633));
#82073=CARTESIAN_POINT('Ctrl Pts',(-15.8767456944143,20.279505178111,1.81769362416544));
#82074=CARTESIAN_POINT('Ctrl Pts',(-15.904666099771,20.3325154035155,1.97678715868852));
#82075=CARTESIAN_POINT('Ctrl Pts',(-15.9325865051277,20.3920858482281,2.13337733801519));
#82076=CARTESIAN_POINT('Ctrl Pts',(-15.9605067427245,20.4516559350112,2.28996657646851));
#82077=CARTESIAN_POINT('Ctrl Pts',(-15.9884269803213,20.5177860473033,2.44405219594104));
#82078=CARTESIAN_POINT('Ctrl Pts',(-16.016347217918,20.5902383170795,2.59508738465685));
#82079=CARTESIAN_POINT('Ctrl Pts',(-16.044273509623,20.6627062971045,2.74615532321488));
#82080=CARTESIAN_POINT('Ctrl Pts',(-16.072199801328,20.7414990361101,2.89417122539148));
#82081=CARTESIAN_POINT('Ctrl Pts',(-16.1001260930329,20.8263317951561,3.03861108175881));
#82082=CARTESIAN_POINT('Ctrl Pts',(-16.1101199180024,20.8566904175805,3.09030096090228));
#82083=CARTESIAN_POINT('Ctrl Pts',(-16.1201137429719,20.8878221425343,3.14153310276232));
#82084=CARTESIAN_POINT('Ctrl Pts',(-16.1301075679414,20.9197125236784,3.19228431658747));
#82085=CARTESIAN_POINT('Ctrl Pts',(-16.1580655556408,21.0089267020812,3.33426216952963));
#82086=CARTESIAN_POINT('Ctrl Pts',(-16.1860235433401,21.1041101501299,3.47251987290981));
#82087=CARTESIAN_POINT('Ctrl Pts',(-16.2139815310394,21.2049286144706,3.60656213140395));
#82088=CARTESIAN_POINT('Ctrl Pts',(-16.2419342515229,21.3057280848616,3.74057913666768));
#82089=CARTESIAN_POINT('Ctrl Pts',(-16.2698869720064,21.412160264276,3.8703820310855));
#82090=CARTESIAN_POINT('Ctrl Pts',(-16.29783969249,21.5238489995523,3.99550650371025));
#82091=CARTESIAN_POINT('Ctrl Pts',(-16.3257916397405,21.6355346452756,4.12062751512036));
#82092=CARTESIAN_POINT('Ctrl Pts',(-16.3537435869911,21.7524763497601,4.24107012682793));
#82093=CARTESIAN_POINT('Ctrl Pts',(-16.3816955342416,21.874258829291,4.35640445692514));
#82094=CARTESIAN_POINT('Ctrl Pts',(-16.4096453034429,21.996031819385,4.47172980003287));
#82095=CARTESIAN_POINT('Ctrl Pts',(-16.4375950726441,22.1226446022546,4.58194744159069));
#82096=CARTESIAN_POINT('Ctrl Pts',(-16.4655448418454,22.2536460936716,4.68666538260823));
#82097=CARTESIAN_POINT('Ctrl Pts',(-16.4934975117503,22.3846611807822,4.79139419154048));
#82098=CARTESIAN_POINT('Ctrl Pts',(-16.5214501816551,22.5200656411934,4.89062196341714));
#82099=CARTESIAN_POINT('Ctrl Pts',(-16.54940285156,22.6593759004737,4.98399745441991));
#82100=CARTESIAN_POINT('Ctrl Pts',(-16.5592374071914,22.7083892684126,5.01684964578496));
#82101=CARTESIAN_POINT('Ctrl Pts',(-16.5690719628228,22.7578858352419,5.04897780417467));
#82102=CARTESIAN_POINT('Ctrl Pts',(-16.5789065184543,22.8078436787338,5.08036790209136));
#82103=CARTESIAN_POINT('Ctrl Pts',(-16.6068879338741,22.9499844347187,5.1696794483162));
#82104=CARTESIAN_POINT('Ctrl Pts',(-16.634869349294,23.0958888484545,5.25303026571069));
#82105=CARTESIAN_POINT('Ctrl Pts',(-16.6628507647138,23.2450384808978,5.33012073299153));
#82106=CARTESIAN_POINT('Ctrl Pts',(-16.6908293844766,23.3941732116208,5.40720349807049));
#82107=CARTESIAN_POINT('Ctrl Pts',(-16.7188080042394,23.5465522360667,5.47802701828067));
#82108=CARTESIAN_POINT('Ctrl Pts',(-16.7467866240022,23.701633037362,5.54233789163512));
#82109=CARTESIAN_POINT('Ctrl Pts',(-16.7747678577677,23.8567283276367,5.60665477346327));
#82110=CARTESIAN_POINT('Ctrl Pts',(-16.8027490915333,24.0145256112291,5.66445767062608));
#82111=CARTESIAN_POINT('Ctrl Pts',(-16.8307303252988,24.1744622187945,5.7155412525317));
#82112=CARTESIAN_POINT('Ctrl Pts',(-16.8587112697084,24.3343971724438,5.76662430617822));
#82113=CARTESIAN_POINT('Ctrl Pts',(-16.8866922141179,24.4964711071497,5.81098809101212));
#82114=CARTESIAN_POINT('Ctrl Pts',(-16.9146731585274,24.6601057782571,5.84847702180149));
#82115=CARTESIAN_POINT('Ctrl Pts',(-16.942659527978,24.8237721754128,5.88597322107268));
#82116=CARTESIAN_POINT('Ctrl Pts',(-16.9706458974285,24.9889996085543,5.91659183419624));
#82117=CARTESIAN_POINT('Ctrl Pts',(-16.998632266879,25.1551984328592,5.94022813637292));
#82118=CARTESIAN_POINT('Ctrl Pts',(-17.0083233342417,25.2127494490705,5.94841287062382));
#82119=CARTESIAN_POINT('Ctrl Pts',(-17.0180144016044,25.270416867388,5.95576081851139));
#82120=CARTESIAN_POINT('Ctrl Pts',(-17.0277054689671,25.3281759992757,5.96226907410684));
#82121=CARTESIAN_POINT('Ctrl Pts',(-17.0556148056643,25.4945167127237,5.98101222075169));
#82122=CARTESIAN_POINT('Ctrl Pts',(-17.0835241423614,25.6616705311091,5.99279315081194));
#82123=CARTESIAN_POINT('Ctrl Pts',(-17.1114334790586,25.8290438172005,5.9975640041239));
#82124=CARTESIAN_POINT('Ctrl Pts',(-17.1393368213947,25.9963811548955,6.00233383275307));
#82125=CARTESIAN_POINT('Ctrl Pts',(-17.1672401637309,26.1639375501269,6.0000965807107));
#82126=CARTESIAN_POINT('Ctrl Pts',(-17.195143506067,26.3311174488523,5.99085646924258));
#82127=CARTESIAN_POINT('Ctrl Pts',(-17.2230459518635,26.498291976056,5.98161665466098));
#82128=CARTESIAN_POINT('Ctrl Pts',(-17.25094839766,26.6650897149014,5.96537444428861));
#82129=CARTESIAN_POINT('Ctrl Pts',(-17.2788508434566,26.8309176112471,5.94218612324787));
#82130=CARTESIAN_POINT('Ctrl Pts',(-17.299567228971,26.9540378084802,5.92496977592058));
#82131=CARTESIAN_POINT('Ctrl Pts',(-17.3202836144855,27.0766234122808,5.90392551126519));
#82132=CARTESIAN_POINT('Ctrl Pts',(-17.341,27.1984341265848,5.87909479803116));
#82133=CARTESIAN_POINT('',(-17.341,20.0176003675788,-0.459232662172854));
#82134=CARTESIAN_POINT('Origin',(-17.341,26.,7.7715611723761E-15));
#82135=CARTESIAN_POINT('',(-16.6322154976385,21.7573593077119,-4.24264069228803));
#82136=CARTESIAN_POINT('Ctrl Pts',(-17.341,20.0176003675788,-0.459232662172852));
#82137=CARTESIAN_POINT('Ctrl Pts',(-17.2225531007737,20.0719950524366,-1.16782934856558));
#82138=CARTESIAN_POINT('Ctrl Pts',(-17.105980663342,20.2518558191926,-1.86116408950255));
#82139=CARTESIAN_POINT('Ctrl Pts',(-16.8692219591851,20.8456854082936,-3.15245663059683));
#82140=CARTESIAN_POINT('Ctrl Pts',(-16.7506405280734,21.2549246444944,-3.74020601873292));
#82141=CARTESIAN_POINT('Ctrl Pts',(-16.6322155410337,21.7573593128806,-4.24264068711921));
#82142=CARTESIAN_POINT('Ctrl Pts',(-16.6322154482133,21.7573593128807,-4.24264068711927));
#82143=CARTESIAN_POINT('Ctrl Pts',(-16.6040873150048,21.876696875284,-4.36197824952258));
#82144=CARTESIAN_POINT('Ctrl Pts',(-16.5759591817962,22.001078300101,-4.47628330412854));
#82145=CARTESIAN_POINT('Ctrl Pts',(-16.5478310485877,22.1300590992214,-4.58514530025829));
#82146=CARTESIAN_POINT('Ctrl Pts',(-16.5197046961868,22.2590317324958,-4.69400040427467));
#82147=CARTESIAN_POINT('Ctrl Pts',(-16.491578343786,22.3926029250832,-4.79741294130875));
#82148=CARTESIAN_POINT('Ctrl Pts',(-16.4634519913852,22.5302945345852,-4.89501215353657));
#82149=CARTESIAN_POINT('Ctrl Pts',(-16.4353229896715,22.6679991137089,-4.99262055895245));
#82150=CARTESIAN_POINT('Ctrl Pts',(-16.4071939879578,22.8098246372677,-5.08441436719853));
#82151=CARTESIAN_POINT('Ctrl Pts',(-16.3790649862441,22.9552626926979,-5.17006525389408));
#82152=CARTESIAN_POINT('Ctrl Pts',(-16.3509366819145,23.1006971423768,-5.25571401710279));
#82153=CARTESIAN_POINT('Ctrl Pts',(-16.3228083775849,23.2497436806413,-5.33522001016744));
#82154=CARTESIAN_POINT('Ctrl Pts',(-16.2946800732553,23.401867650476,-5.4082999449325));
#82155=CARTESIAN_POINT('Ctrl Pts',(-16.2665481067811,23.5540114259828,-5.48138939428771));
#82156=CARTESIAN_POINT('Ctrl Pts',(-16.2384161403069,23.7092331581346,-5.5480509819099));
#82157=CARTESIAN_POINT('Ctrl Pts',(-16.2102841738328,23.8669757466507,-5.60804846043824));
#82158=CARTESIAN_POINT('Ctrl Pts',(-16.2013282817887,23.917193551183,-5.62714882944768));
#82159=CARTESIAN_POINT('Ctrl Pts',(-16.1923723897446,23.9676666892194,-5.64557416629127));
#82160=CARTESIAN_POINT('Ctrl Pts',(-16.1834164977005,24.0183767844616,-5.66331788191683));
#82161=CARTESIAN_POINT('Ctrl Pts',(-16.1555420242995,24.1762077625514,-5.71854372952689));
#82162=CARTESIAN_POINT('Ctrl Pts',(-16.1276675508985,24.33637074922,-5.76717526848675));
#82163=CARTESIAN_POINT('Ctrl Pts',(-16.0997930774975,24.4982984770211,-5.80903542215768));
#82164=CARTESIAN_POINT('Ctrl Pts',(-16.0719226239925,24.660202852538,-5.85088953899838));
#82165=CARTESIAN_POINT('Ctrl Pts',(-16.0440521704875,24.8238711537045,-5.88597413996263));
#82166=CARTESIAN_POINT('Ctrl Pts',(-16.0161817169824,24.9887227670212,-5.9141625238117));
#82167=CARTESIAN_POINT('Ctrl Pts',(-15.988309486411,25.1535848915505,-5.94235270499893));
#82168=CARTESIAN_POINT('Ctrl Pts',(-15.9604372558396,25.3196301662181,-5.96364573398776));
#82169=CARTESIAN_POINT('Ctrl Pts',(-15.9325650252682,25.4862689201503,-5.97796624092144));
#82170=CARTESIAN_POINT('Ctrl Pts',(-15.9046933029176,25.6529046356006,-5.99228648673578));
#82171=CARTESIAN_POINT('Ctrl Pts',(-15.8768215805669,25.8201334918203,-5.999634440016));
#82172=CARTESIAN_POINT('Ctrl Pts',(-15.8489498582162,25.9873616309338,-5.99998668928751));
#82173=CARTESIAN_POINT('Ctrl Pts',(-15.821072225014,26.154625234691,-6.00033901326173));
#82174=CARTESIAN_POINT('Ctrl Pts',(-15.7931945918118,26.3218878031738,-5.99369266936041));
#82175=CARTESIAN_POINT('Ctrl Pts',(-15.7653169586096,26.4885556433562,-5.98007636935723));
#82176=CARTESIAN_POINT('Ctrl Pts',(-15.7550838214689,26.5497349713554,-5.97507818804572));
#82177=CARTESIAN_POINT('Ctrl Pts',(-15.7448506843283,26.6108341930809,-5.96914136077459));
#82178=CARTESIAN_POINT('Ctrl Pts',(-15.7346175471877,26.6718240929007,-5.96226906372046));
#82179=CARTESIAN_POINT('Ctrl Pts',(-15.7066311888463,26.8386238892982,-5.94347418534225));
#82180=CARTESIAN_POINT('Ctrl Pts',(-15.6786448305049,27.0046583179452,-5.91767274678865));
#82181=CARTESIAN_POINT('Ctrl Pts',(-15.6506584721634,27.1693349785026,-5.88495163175113));
#82182=CARTESIAN_POINT('Ctrl Pts',(-15.6226770670896,27.3339824931617,-5.85223630797928));
#82183=CARTESIAN_POINT('Ctrl Pts',(-15.5946956620157,27.4972724128116,-5.81260381282124));
#82184=CARTESIAN_POINT('Ctrl Pts',(-15.5667142569418,27.6586221159657,-5.7661922163963));
#82185=CARTESIAN_POINT('Ctrl Pts',(-15.5387334249018,27.8199685148236,-5.71978157043898));
#82186=CARTESIAN_POINT('Ctrl Pts',(-15.5107525928619,27.9793744752583,-5.66659218393378));
#82187=CARTESIAN_POINT('Ctrl Pts',(-15.4827717608219,28.1362714456714,-5.60681231275037));
#82188=CARTESIAN_POINT('Ctrl Pts',(-15.4547930658108,28.2931564331184,-5.54703700723933));
#82189=CARTESIAN_POINT('Ctrl Pts',(-15.4268143707998,28.4475325216267,-5.48067233496891));
#82190=CARTESIAN_POINT('Ctrl Pts',(-15.3988356757887,28.5988497756167,-5.40795523685032));
#82191=CARTESIAN_POINT('Ctrl Pts',(-15.3708542344006,28.7501818828451,-5.33523100085181));
#82192=CARTESIAN_POINT('Ctrl Pts',(-15.3428727930126,28.8984542738177,-5.25615322852832));
#82193=CARTESIAN_POINT('Ctrl Pts',(-15.3148913516245,29.0431396447295,-5.17100581151051));
#82194=CARTESIAN_POINT('Ctrl Pts',(-15.3052004333079,29.0932490758935,-5.14151638486731));
#82195=CARTESIAN_POINT('Ctrl Pts',(-15.2955095149914,29.1429284743663,-5.11129932464418));
#82196=CARTESIAN_POINT('Ctrl Pts',(-15.2858185966749,29.1921566655501,-5.08036768576688));
#82197=CARTESIAN_POINT('Ctrl Pts',(-15.2577278232719,29.3348529424569,-4.99070707463563));
#82198=CARTESIAN_POINT('Ctrl Pts',(-15.229637049869,29.4737825802179,-4.89502244371932));
#82199=CARTESIAN_POINT('Ctrl Pts',(-15.201546276466,29.608446748013,-4.79365331107231));
#82200=CARTESIAN_POINT('Ctrl Pts',(-15.1734574449732,29.7431016064979,-4.69229118605549));
#82201=CARTESIAN_POINT('Ctrl Pts',(-15.1453686134805,29.8734913370775,-4.58524552703901));
#82202=CARTESIAN_POINT('Ctrl Pts',(-15.1172797819877,29.9991481915547,-4.47289768963977));
#82203=CARTESIAN_POINT('Ctrl Pts',(-15.0986595620208,30.0824467179217,-4.39842177398193));
#82204=CARTESIAN_POINT('Ctrl Pts',(-15.0800393420538,30.1636660601329,-4.32161671282728));
#82205=CARTESIAN_POINT('Ctrl Pts',(-15.0614191220869,30.2426782484473,-4.24260312545867));
#82206=CARTESIAN_POINT('Origin',(-31.4159265358979,26.,7.7715611723761E-15));
#82207=CARTESIAN_POINT('',(-6.9297288961107,30.2426857292706,-4.24259564448975));
#82208=CARTESIAN_POINT('',(-8.77823372208692,30.2426826788146,-4.24259869500835));
#82209=CARTESIAN_POINT('',(-31.4159265358979,30.2426406871193,-4.24264068711928));
#82210=CARTESIAN_POINT('',(-8.5005252730077,21.7573593180495,-4.24264068195053));
#82211=CARTESIAN_POINT('Ctrl Pts',(-6.92972889611913,30.2426857292348,-4.24259564452553));
#82212=CARTESIAN_POINT('Ctrl Pts',(-6.95781684444987,30.1234985386172,-4.36178536589192));
#82213=CARTESIAN_POINT('Ctrl Pts',(-6.98590479278062,29.9992874203363,-4.47594779443039));
#82214=CARTESIAN_POINT('Ctrl Pts',(-7.01399274111136,29.8704975466977,-4.58467542373584));
#82215=CARTESIAN_POINT('Ctrl Pts',(-7.0420851505798,29.7416872176896,-4.69342032197528));
#82216=CARTESIAN_POINT('Ctrl Pts',(-7.07017756004824,29.6082969145932,-4.79672849740392));
#82217=CARTESIAN_POINT('Ctrl Pts',(-7.09826996951668,29.4708054188974,-4.89423229364448));
#82218=CARTESIAN_POINT('Ctrl Pts',(-7.11688943702581,29.3796769437922,-4.95885717988492));
#82219=CARTESIAN_POINT('Ctrl Pts',(-7.13550890453494,29.2867475157265,-5.02093305892931));
#82220=CARTESIAN_POINT('Ctrl Pts',(-7.15412837204407,29.1921638262116,-5.08036318648836));
#82221=CARTESIAN_POINT('Ctrl Pts',(-7.18210991041342,29.0500224284525,-5.16967542883757));
#82222=CARTESIAN_POINT('Ctrl Pts',(-7.21009144878276,28.9041172855606,-5.25302690670604));
#82223=CARTESIAN_POINT('Ctrl Pts',(-7.23807298715211,28.7549668361744,-5.33011798477098));
#82224=CARTESIAN_POINT('Ctrl Pts',(-7.2660517174012,28.6058313549574,-5.40720132626995));
#82225=CARTESIAN_POINT('Ctrl Pts',(-7.29403044765029,28.4534514951217,-5.47802537878091));
#82226=CARTESIAN_POINT('Ctrl Pts',(-7.32200917789939,28.2983697742659,-5.54233672567274));
#82227=CARTESIAN_POINT('Ctrl Pts',(-7.34999050219416,28.1432736750211,-5.60665403518583));
#82228=CARTESIAN_POINT('Ctrl Pts',(-7.37797182648893,27.9854755021155,-5.66445731054565));
#82229=CARTESIAN_POINT('Ctrl Pts',(-7.40595315078371,27.8255379264614,-5.71554120613708));
#82230=CARTESIAN_POINT('Ctrl Pts',(-7.43393417369507,27.6656020734754,-5.76662455151013));
#82231=CARTESIAN_POINT('Ctrl Pts',(-7.46191519660644,27.5035271624844,-5.81098856932182));
#82232=CARTESIAN_POINT('Ctrl Pts',(-7.4898962195178,27.3398914411849,-5.84847765883048));
#82233=CARTESIAN_POINT('Ctrl Pts',(-7.51788264881145,27.1762241028402,-5.88597399183237));
#82234=CARTESIAN_POINT('Ctrl Pts',(-7.5458690781051,27.0109956566457,-5.91659267356233));
#82235=CARTESIAN_POINT('Ctrl Pts',(-7.57385550739876,26.8447957516834,-5.94022896342705));
#82236=CARTESIAN_POINT('Ctrl Pts',(-7.58354611245147,26.7872472297949,-5.94841328546352));
#82237=CARTESIAN_POINT('Ctrl Pts',(-7.59323671750418,26.7295823093205,-5.9557608948509));
#82238=CARTESIAN_POINT('Ctrl Pts',(-7.60292732255689,26.67182567535,-5.96226888541102));
#82239=CARTESIAN_POINT('Ctrl Pts',(-7.63080398612794,26.5056789543317,-5.98099022039282));
#82240=CARTESIAN_POINT('Ctrl Pts',(-7.65868064969899,26.338720625094,-5.99276560336772));
#82241=CARTESIAN_POINT('Ctrl Pts',(-7.68655731327004,26.1715429512646,-5.99754724999073));
#82242=CARTESIAN_POINT('Ctrl Pts',(-7.71442860956402,26.0043974652504,-6.00232797597192));
#82243=CARTESIAN_POINT('Ctrl Pts',(-7.74229990585801,25.8370330364648,-6.00011764348317));
#82244=CARTESIAN_POINT('Ctrl Pts',(-7.77017120215199,25.6700438745741,-5.99092054322988));
#82245=CARTESIAN_POINT('Ctrl Pts',(-7.79804228889752,25.5030559681801,-5.98172351212437));
#82246=CARTESIAN_POINT('Ctrl Pts',(-7.82591337564304,25.3364436405639,-5.96553983216607));
#82247=CARTESIAN_POINT('Ctrl Pts',(-7.85378446238856,25.1707986121721,-5.94242585636743));
#82248=CARTESIAN_POINT('Ctrl Pts',(-7.88165389348992,25.0051634236989,-5.91931325362322));
#82249=CARTESIAN_POINT('Ctrl Pts',(-7.90952332459129,24.8404957342096,-5.88927122297676));
#82250=CARTESIAN_POINT('Ctrl Pts',(-7.93739275569265,24.6773799389868,-5.85240772453572));
#82251=CARTESIAN_POINT('Ctrl Pts',(-7.96526643215482,24.5142392962743,-5.81553861066426));
#82252=CARTESIAN_POINT('Ctrl Pts',(-7.99314010861698,24.3526513301256,-5.7718460233064));
#82253=CARTESIAN_POINT('Ctrl Pts',(-8.02101378507914,24.1931887960309,-5.72148872874986));
#82254=CARTESIAN_POINT('Ctrl Pts',(-8.031251281076,24.1346210984163,-5.7029934074694));
#82255=CARTESIAN_POINT('Ctrl Pts',(-8.04148877707287,24.0763399740661,-5.68359953185717));
#82256=CARTESIAN_POINT('Ctrl Pts',(-8.05172627306973,24.0183732706507,-5.66331665241563));
#82257=CARTESIAN_POINT('Ctrl Pts',(-8.07985938912929,23.8590780684571,-5.60757835454219));
#82258=CARTESIAN_POINT('Ctrl Pts',(-8.10799250518886,23.7021225204538,-5.54511037539292));
#82259=CARTESIAN_POINT('Ctrl Pts',(-8.13612562124842,23.5480699659983,-5.47613359117183));
#82260=CARTESIAN_POINT('Ctrl Pts',(-8.16425526800264,23.3940364089177,-5.40716531299486));
#82261=CARTESIAN_POINT('Ctrl Pts',(-8.19238491475685,23.2429054092286,-5.33168995691243));
#82262=CARTESIAN_POINT('Ctrl Pts',(-8.22051456151107,23.0952192005546,-5.24997604824758));
#82263=CARTESIAN_POINT('Ctrl Pts',(-8.24864435841876,22.9475322035451,-5.16826170340138));
#82264=CARTESIAN_POINT('Ctrl Pts',(-8.27677415532646,22.8032903026227,-5.08030888503684));
#82265=CARTESIAN_POINT('Ctrl Pts',(-8.30490395223415,22.6630107280007,-4.98643185038779));
#82266=CARTESIAN_POINT('Ctrl Pts',(-8.33303159546407,22.5227418934848,-4.89256200316648));
#82267=CARTESIAN_POINT('Ctrl Pts',(-8.36115923869398,22.386435032278,-4.79276901652899));
#82268=CARTESIAN_POINT('Ctrl Pts',(-8.3892868819239,22.2545783311889,-4.68741042824289));
#82269=CARTESIAN_POINT('Ctrl Pts',(-8.41741608128806,22.1227143352573,-4.58204601109636));
#82270=CARTESIAN_POINT('Ctrl Pts',(-8.44554528065223,21.9953012300267,-4.47111556744834));
#82271=CARTESIAN_POINT('Ctrl Pts',(-8.4736744800164,21.872794662332,-4.35501734792463));
#82272=CARTESIAN_POINT('Ctrl Pts',(-8.48262472787178,21.8338150905857,-4.31807680699938));
#82273=CARTESIAN_POINT('Ctrl Pts',(-8.49157497572716,21.7953319985918,-4.28061337283033));
#82274=CARTESIAN_POINT('Ctrl Pts',(-8.50052522358255,21.7573593128807,-4.24264068711927));
#82275=CARTESIAN_POINT('',(-11.6421179699928,30.2426406871193,4.24264068711929));
#82276=CARTESIAN_POINT('Ctrl Pts',(-8.50052531640296,21.7573593128807,-4.24264068711927));
#82277=CARTESIAN_POINT('Ctrl Pts',(-8.52845069909252,21.6388819480786,-4.12416332231719));
#82278=CARTESIAN_POINT('Ctrl Pts',(-8.55637608178207,21.5253581562297,-4.00070781090067));
#82279=CARTESIAN_POINT('Ctrl Pts',(-8.58430146447163,21.4171941806491,-3.87271104294179));
#82280=CARTESIAN_POINT('Ctrl Pts',(-8.61222392419931,21.3090415266385,-3.74472767245994));
#82281=CARTESIAN_POINT('Ctrl Pts',(-8.64014638392699,21.2062477723132,-3.61220423501525));
#82282=CARTESIAN_POINT('Ctrl Pts',(-8.66806884365467,21.1091794775264,-3.47561140189052));
#82283=CARTESIAN_POINT('Ctrl Pts',(-8.69599421623101,21.0121010566528,-3.33900431951072));
#82284=CARTESIAN_POINT('Ctrl Pts',(-8.72391958880735,20.9207494733936,-3.19832724871925));
#82285=CARTESIAN_POINT('Ctrl Pts',(-8.75184496138369,20.8354489157695,-3.05408122000282));
#82286=CARTESIAN_POINT('Ctrl Pts',(-8.77977035175856,20.7501483037783,-2.90983509934969));
#82287=CARTESIAN_POINT('Ctrl Pts',(-8.80769574213342,20.6708988827886,-2.76202028919063));
#82288=CARTESIAN_POINT('Ctrl Pts',(-8.83562113250829,20.5979797981118,-2.61116405811506));
#82289=CARTESIAN_POINT('Ctrl Pts',(-8.86355279570316,20.5250443337788,-2.46027394053079));
#82290=CARTESIAN_POINT('Ctrl Pts',(-8.89148445889802,20.4584421829795,-2.30634132137571));
#82291=CARTESIAN_POINT('Ctrl Pts',(-8.91941612209289,20.3984054317556,-2.14991588045076));
#82292=CARTESIAN_POINT('Ctrl Pts',(-8.92938550370053,20.3769770878987,-2.09408444274354));
#82293=CARTESIAN_POINT('Ctrl Pts',(-8.93935488530816,20.3563846777811,-2.03793562245308));
#82294=CARTESIAN_POINT('Ctrl Pts',(-8.9493242669158,20.3366372511112,-1.981494984727));
#82295=CARTESIAN_POINT('Ctrl Pts',(-8.97732492365711,20.2811733379547,-1.82297212087967));
#82296=CARTESIAN_POINT('Ctrl Pts',(-9.00532558039843,20.2323618582529,-1.66209773342208));
#82297=CARTESIAN_POINT('Ctrl Pts',(-9.03332623713976,20.190381437133,-1.4994439482659));
#82298=CARTESIAN_POINT('Ctrl Pts',(-9.0613221792703,20.1484080844668,-1.33681754994193));
#82299=CARTESIAN_POINT('Ctrl Pts',(-9.08931812140085,20.1132635727499,-1.17241265378827));
#82300=CARTESIAN_POINT('Ctrl Pts',(-9.1173140635314,20.0850761584985,-1.00681475418157));
#82301=CARTESIAN_POINT('Ctrl Pts',(-9.14530964735303,20.0568891050067,-0.84121897399644));
#82302=CARTESIAN_POINT('Ctrl Pts',(-9.17330523117467,20.0356590264685,-0.674430527827274));
#82303=CARTESIAN_POINT('Ctrl Pts',(-9.2013008149963,20.0214628548888,-0.507043986776435));
#82304=CARTESIAN_POINT('Ctrl Pts',(-9.22929434665013,20.007267723935,-0.339669715706182));
#82305=CARTESIAN_POINT('Ctrl Pts',(-9.25728787830396,20.000105495034,-0.171697748236844));
#82306=CARTESIAN_POINT('Ctrl Pts',(-9.28528140995779,20.0000011575362,-0.00372698713702113));
#82307=CARTESIAN_POINT('Ctrl Pts',(-9.31327769979149,19.9998968097581,0.164260323985088));
#82308=CARTESIAN_POINT('Ctrl Pts',(-9.34127398962519,20.0068517430295,0.332246116553286));
#82309=CARTESIAN_POINT('Ctrl Pts',(-9.3692702794589,20.0208388260907,0.499631520638411));
#82310=CARTESIAN_POINT('Ctrl Pts',(-9.37888792544881,20.0256438489745,0.557133910059677));
#82311=CARTESIAN_POINT('Ctrl Pts',(-9.38850557143871,20.0312783181165,0.614565467986606));
#82312=CARTESIAN_POINT('Ctrl Pts',(-9.39812321742862,20.0377397179013,0.671902022997967));
#82313=CARTESIAN_POINT('Ctrl Pts',(-9.42604429401234,20.0564978670804,0.838356303515164));
#82314=CARTESIAN_POINT('Ctrl Pts',(-9.45396537059607,20.0822330307513,1.00404317010695));
#82315=CARTESIAN_POINT('Ctrl Pts',(-9.48188644717979,20.1148572786045,1.16837286377507));
#82316=CARTESIAN_POINT('Ctrl Pts',(-9.50980430841761,20.1474777695023,1.33268363350215));
#82317=CARTESIAN_POINT('Ctrl Pts',(-9.53772216965544,20.1869856995438,1.49563723290372));
#82318=CARTESIAN_POINT('Ctrl Pts',(-9.56564003089326,20.2332419793214,1.65665383557911));
#82319=CARTESIAN_POINT('Ctrl Pts',(-9.59356043576381,20.2795024735689,1.81768510868707));
#82320=CARTESIAN_POINT('Ctrl Pts',(-9.62148084063436,20.3325124614835,1.97677872842205));
#82321=CARTESIAN_POINT('Ctrl Pts',(-9.64940124550491,20.3920826940288,2.13336904669319));
#82322=CARTESIAN_POINT('Ctrl Pts',(-9.67732147215226,20.4516525463218,2.28995836540765));
#82323=CARTESIAN_POINT('Ctrl Pts',(-9.70524169879962,20.5177824445448,2.44404412074397));
#82324=CARTESIAN_POINT('Ctrl Pts',(-9.73316192544697,20.5902345326086,2.5950794954721));
#82325=CARTESIAN_POINT('Ctrl Pts',(-9.76108819095282,20.6627022913155,2.74614753760182));
#82326=CARTESIAN_POINT('Ctrl Pts',(-9.78901445645868,20.7414948344809,2.89416359684659));
#82327=CARTESIAN_POINT('Ctrl Pts',(-9.81694072196453,20.8263274346028,3.03860365728353));
#82328=CARTESIAN_POINT('Ctrl Pts',(-9.82693453729016,20.8566859993395,3.0902936080694));
#82329=CARTESIAN_POINT('Ctrl Pts',(-9.8369283526158,20.8878176712821,3.14152582759828));
#82330=CARTESIAN_POINT('Ctrl Pts',(-9.84692216794143,20.9197080045832,3.19227712476596));
#82331=CARTESIAN_POINT('Ctrl Pts',(-9.87487991362713,21.0089213629666,3.33425411885685));
#82332=CARTESIAN_POINT('Ctrl Pts',(-9.90283765931282,21.1041039105059,3.47251101870401));
#82333=CARTESIAN_POINT('Ctrl Pts',(-9.93079540499851,21.2049213976204,3.60655253628739));
#82334=CARTESIAN_POINT('Ctrl Pts',(-9.95874788641887,21.3057199014445,3.74056881470723));
#82335=CARTESIAN_POINT('Ctrl Pts',(-9.98670036783922,21.4121510387671,3.87037104399797));
#82336=CARTESIAN_POINT('Ctrl Pts',(-10.0146528492596,21.5238386602809,3.99549492063299));
#82337=CARTESIAN_POINT('Ctrl Pts',(-10.0426045636081,21.6355232168635,4.12061536361926));
#82338=CARTESIAN_POINT('Ctrl Pts',(-10.0705562779566,21.7524637628468,4.2410574739713));
#82339=CARTESIAN_POINT('Ctrl Pts',(-10.0985079923051,21.8742450184155,4.35639137726755));
#82340=CARTESIAN_POINT('Ctrl Pts',(-10.1264575326743,21.996016802296,4.47171631032632));
#82341=CARTESIAN_POINT('Ctrl Pts',(-10.1544070730436,22.1226283148942,4.58193361489443));
#82342=CARTESIAN_POINT('Ctrl Pts',(-10.1823566134128,22.2536284761326,4.68665129971874));
#82343=CARTESIAN_POINT('Ctrl Pts',(-10.2103090618765,22.384642267679,4.79137988021132));
#82344=CARTESIAN_POINT('Ctrl Pts',(-10.2382615103402,22.5200453749241,4.89060750154165));
#82345=CARTESIAN_POINT('Ctrl Pts',(-10.2662139588039,22.6593542278063,4.98398292781231));
#82346=CARTESIAN_POINT('Ctrl Pts',(-10.2760496786874,22.7083732915929,5.016839245855));
#82347=CARTESIAN_POINT('Ctrl Pts',(-10.2858853985708,22.7578756697644,5.04897135862553));
#82348=CARTESIAN_POINT('Ctrl Pts',(-10.2957211184543,22.8078394319699,5.08036523371242));
#82349=CARTESIAN_POINT('Ctrl Pts',(-10.323702586032,22.9499804657511,5.1696771202131));
#82350=CARTESIAN_POINT('Ctrl Pts',(-10.3516840536097,23.0958852012862,5.25302826428355));
#82351=CARTESIAN_POINT('Ctrl Pts',(-10.3796655211874,23.245035200224,5.33011903731945));
#82352=CARTESIAN_POINT('Ctrl Pts',(-10.4076441864509,23.3941702619481,5.40720208979644));
#82353=CARTESIAN_POINT('Ctrl Pts',(-10.4356228517144,23.5465496605457,5.47802587945846));
#82354=CARTESIAN_POINT('Ctrl Pts',(-10.4636015169779,23.7016308792268,5.54233699667174));
#82355=CARTESIAN_POINT('Ctrl Pts',(-10.4915827856967,23.8567265284392,5.60665409812732));
#82356=CARTESIAN_POINT('Ctrl Pts',(-10.5195640544154,24.0145242121799,5.66445719422693));
#82357=CARTESIAN_POINT('Ctrl Pts',(-10.5475453231341,24.1744612607334,5.71554094652789));
#82358=CARTESIAN_POINT('Ctrl Pts',(-10.5755262961688,24.3343966191982,5.766624159016));
#82359=CARTESIAN_POINT('Ctrl Pts',(-10.6035072692035,24.4964709985975,5.81098807718157));
#82360=CARTESIAN_POINT('Ctrl Pts',(-10.6314882422382,24.660106153123,5.84847710768379));
#82361=CARTESIAN_POINT('Ctrl Pts',(-10.6594746305795,24.8237729768308,5.88597339363759));
#82362=CARTESIAN_POINT('Ctrl Pts',(-10.6874610189208,24.9890008741831,5.91659206459093));
#82363=CARTESIAN_POINT('Ctrl Pts',(-10.7154474072621,25.1552001985585,5.94022838748516));
#82364=CARTESIAN_POINT('Ctrl Pts',(-10.7251382944971,25.2127502793841,5.94841297125584));
#82365=CARTESIAN_POINT('Ctrl Pts',(-10.7348291817321,25.2704167621195,5.95576079644968));
#82366=CARTESIAN_POINT('Ctrl Pts',(-10.7445200689671,25.3281749595449,5.96226895695066));
#82367=CARTESIAN_POINT('Ctrl Pts',(-10.7723971906407,25.4943240703769,5.98099054329845));
#82368=CARTESIAN_POINT('Ctrl Pts',(-10.8002743123142,25.6612848310749,5.99276598017385));
#82369=CARTESIAN_POINT('Ctrl Pts',(-10.8281514339878,25.8284649617233,5.99754747631426));
#82370=CARTESIAN_POINT('Ctrl Pts',(-10.856023180526,25.9956128574863,6.00232805050909));
#82371=CARTESIAN_POINT('Ctrl Pts',(-10.8838949270642,26.1629797212672,6.00011736581946));
#82372=CARTESIAN_POINT('Ctrl Pts',(-10.9117666736025,26.3299713264642,5.9909197059977));
#82373=CARTESIAN_POINT('Ctrl Pts',(-10.9396381954146,26.4969615852309,5.9817221203354));
#82374=CARTESIAN_POINT('Ctrl Pts',(-10.9675097172268,26.6635762739584,5.96553768605322));
#82375=CARTESIAN_POINT('Ctrl Pts',(-10.995381239039,26.82922365479,5.94242274921069));
#82376=CARTESIAN_POINT('Ctrl Pts',(-11.0232510954796,26.9948611379049,5.91930919352551));
#82377=CARTESIAN_POINT('Ctrl Pts',(-11.0511209519203,27.1595311140562,5.88926600805049));
#82378=CARTESIAN_POINT('Ctrl Pts',(-11.0789908083609,27.3226491694477,5.85240114607324));
#82379=CARTESIAN_POINT('Ctrl Pts',(-11.1068648930307,27.4857919720246,5.81553069120456));
#82380=CARTESIAN_POINT('Ctrl Pts',(-11.1347389777004,27.6473820734677,5.77183656247926));
#82381=CARTESIAN_POINT('Ctrl Pts',(-11.1626130623701,27.8068466988594,5.72147751955919));
#82382=CARTESIAN_POINT('Ctrl Pts',(-11.1728483814067,27.8654018526975,5.70298576003517));
#82383=CARTESIAN_POINT('Ctrl Pts',(-11.1830837004433,27.9236705575847,5.68359582672217));
#82384=CARTESIAN_POINT('Ctrl Pts',(-11.1933190194799,27.9816249837635,5.66331726320576));
#82385=CARTESIAN_POINT('Ctrl Pts',(-11.2214515954767,28.1409172630754,5.60758004317469));
#82386=CARTESIAN_POINT('Ctrl Pts',(-11.2495841714735,28.2978699939995,5.54511338331285));
#82387=CARTESIAN_POINT('Ctrl Pts',(-11.2777167474703,28.4519198562624,5.47613814822693));
#82388=CARTESIAN_POINT('Ctrl Pts',(-11.3058458529672,28.6059507145766,5.40717142208619));
#82389=CARTESIAN_POINT('Ctrl Pts',(-11.3339749584641,28.7570791405905,5.33169784842252));
#82390=CARTESIAN_POINT('Ctrl Pts',(-11.362104063961,28.9047629194926,5.2499859410803));
#82391=CARTESIAN_POINT('Ctrl Pts',(-11.390233323177,29.0524475054531,5.16827358720107));
#82392=CARTESIAN_POINT('Ctrl Pts',(-11.4183625823931,29.1966871383346,5.08032297713911));
#82393=CARTESIAN_POINT('Ctrl Pts',(-11.4464918416091,29.3369646065521,4.98644835675844));
#82394=CARTESIAN_POINT('Ctrl Pts',(-11.4746189508543,29.4772313531051,4.89258091138735));
#82395=CARTESIAN_POINT('Ctrl Pts',(-11.5027460600994,29.6135362869088,4.79279053100786));
#82396=CARTESIAN_POINT('Ctrl Pts',(-11.5308731693445,29.7453912399233,4.68743474193568));
#82397=CARTESIAN_POINT('Ctrl Pts',(-11.5590018442466,29.8772535324625,4.58207308837832));
#82398=CARTESIAN_POINT('Ctrl Pts',(-11.5871305191486,30.0046651106096,4.47114559753712));
#82399=CARTESIAN_POINT('Ctrl Pts',(-11.6152591940506,30.127170346444,4.3550505084825));
#82400=CARTESIAN_POINT('Ctrl Pts',(-11.6242121193646,30.1661618819794,4.31809922424115));
#82401=CARTESIAN_POINT('Ctrl Pts',(-11.6331650446787,30.2046566419131,4.2806247323255));
#82402=CARTESIAN_POINT('Ctrl Pts',(-11.6421179699928,30.2426406871193,4.24264068711928));
#82403=CARTESIAN_POINT('Ctrl Pts',(-11.6421179699928,30.2426406871193,4.24264068711928));
#82404=CARTESIAN_POINT('Ctrl Pts',(-11.6700431543099,30.3611172102982,4.12416416394038));
#82405=CARTESIAN_POINT('Ctrl Pts',(-11.6979683386269,30.4746402455888,4.00070955009656));
#82406=CARTESIAN_POINT('Ctrl Pts',(-11.725893522944,30.5828035516995,3.87271372638496));
#82407=CARTESIAN_POINT('Ctrl Pts',(-11.7538157803785,30.6909555210438,3.74473131811725));
#82408=CARTESIAN_POINT('Ctrl Pts',(-11.781738037813,30.7937486792756,3.61220889083677));
#82409=CARTESIAN_POINT('Ctrl Pts',(-11.8096602952475,30.8908164682605,3.47561710690225));
#82410=CARTESIAN_POINT('Ctrl Pts',(-11.8375854614852,30.9878943692896,3.33901109350855));
#82411=CARTESIAN_POINT('Ctrl Pts',(-11.865510627723,31.0792455246564,3.19833513191561));
#82412=CARTESIAN_POINT('Ctrl Pts',(-11.8934357939607,31.1645457478722,3.05409024394096));
#82413=CARTESIAN_POINT('Ctrl Pts',(-11.9213609761272,31.2498460197439,2.90984527368792));
#82414=CARTESIAN_POINT('Ctrl Pts',(-11.9492861582937,31.329095194901,2.76203164595643));
#82415=CARTESIAN_POINT('Ctrl Pts',(-11.9772113404601,31.4020141294016,2.61117662094029));
#82416=CARTESIAN_POINT('Ctrl Pts',(-12.0051427941856,31.4749494403542,2.46028771624566));
#82417=CARTESIAN_POINT('Ctrl Pts',(-12.0330742479111,31.5415515340173,2.30635633389469));
#82418=CARTESIAN_POINT('Ctrl Pts',(-12.0610057016366,31.6015883256266,2.1499321454883));
#82419=CARTESIAN_POINT('Ctrl Pts',(-12.0709761079263,31.6230190470833,2.09409499761674));
#82420=CARTESIAN_POINT('Ctrl Pts',(-12.0809465142159,31.6436136628225,2.03794039915355));
#82421=CARTESIAN_POINT('Ctrl Pts',(-12.0909169205055,31.6633631202419,1.98149392335291));
#82422=CARTESIAN_POINT('Ctrl Pts',(-12.1189176009114,31.7188270832263,1.82297082178452));
#82423=CARTESIAN_POINT('Ctrl Pts',(-12.1469182813172,31.7676385913327,1.66209619658588));
#82424=CARTESIAN_POINT('Ctrl Pts',(-12.1749189617231,31.8096190203628,1.49944217569028));
#82425=CARTESIAN_POINT('Ctrl Pts',(-12.2029149287158,31.8515923827395,1.33681553468645));
#82426=CARTESIAN_POINT('Ctrl Pts',(-12.2309108957085,31.8867368830954,1.17241039769987));
#82427=CARTESIAN_POINT('Ctrl Pts',(-12.2589068627012,31.9149242658821,1.00681226098963));
#82428=CARTESIAN_POINT('Ctrl Pts',(-12.2869024727919,31.9431112893265,0.841216235380474));
#82429=CARTESIAN_POINT('Ctrl Pts',(-12.3148980828826,31.9643413170165,0.674427547395076));
#82430=CARTESIAN_POINT('Ctrl Pts',(-12.3428936929732,31.9785374179344,0.507040769917742));
#82431=CARTESIAN_POINT('Ctrl Pts',(-12.3708872516044,31.9927324785918,0.339666258191626));
#82432=CARTESIAN_POINT('Ctrl Pts',(-12.3988808102356,31.9998946170303,0.171694055423287));
#82433=CARTESIAN_POINT('Ctrl Pts',(-12.4268743688668,31.9999988448982,0.00372306604439232));
#82434=CARTESIAN_POINT('Ctrl Pts',(-12.4548706864185,32.0001030830383,-0.16426447780736));
#82435=CARTESIAN_POINT('Ctrl Pts',(-12.4828670039702,31.9931480205866,-0.332250496085683));
#82436=CARTESIAN_POINT('Ctrl Pts',(-12.5108633215219,31.9791607898017,-0.499636117287159));
#82437=CARTESIAN_POINT('Ctrl Pts',(-12.5204808380207,31.9743557856222,-0.557137750157443));
#82438=CARTESIAN_POINT('Ctrl Pts',(-12.5300983545196,31.9687213569753,-0.614568552568057));
#82439=CARTESIAN_POINT('Ctrl Pts',(-12.5397158710184,31.9622600194022,-0.671904354084557));
#82440=CARTESIAN_POINT('Ctrl Pts',(-12.5676369379214,31.9435018047756,-0.838358630535872));
#82441=CARTESIAN_POINT('Ctrl Pts',(-12.5955580048243,31.9177665771291,-1.00404547747855));
#82442=CARTESIAN_POINT('Ctrl Pts',(-12.6234790717273,31.8851422701962,-1.16837513648239));
#82443=CARTESIAN_POINT('Ctrl Pts',(-12.6513969265305,31.8525217164338,-1.33268589064812));
#82444=CARTESIAN_POINT('Ctrl Pts',(-12.6793147813338,31.8130137268255,-1.49563945916178));
#82445=CARTESIAN_POINT('Ctrl Pts',(-12.707232636137,31.7667573941392,-1.65665601654091));
#82446=CARTESIAN_POINT('Ctrl Pts',(-12.7351530394038,31.720496838973,-1.81768727221378));
#82447=CARTESIAN_POINT('Ctrl Pts',(-12.7630734426706,31.6674867944667,-1.97678085943301));
#82448=CARTESIAN_POINT('Ctrl Pts',(-12.7909938459374,31.6079165129524,-2.13337113127463));
#82449=CARTESIAN_POINT('Ctrl Pts',(-12.8189140737873,31.5483466057032,-2.28996041929891));
#82450=CARTESIAN_POINT('Ctrl Pts',(-12.8468343016373,31.4822166588321,-2.44404612952963));
#82451=CARTESIAN_POINT('Ctrl Pts',(-12.8747545294872,31.4097645315886,-2.59508144626834));
#82452=CARTESIAN_POINT('Ctrl Pts',(-12.9026808002997,31.3372967230442,-2.74614945259596));
#82453=CARTESIAN_POINT('Ctrl Pts',(-12.9306070711122,31.2585041376586,-2.89416546225386));
#82454=CARTESIAN_POINT('Ctrl Pts',(-12.9585333419248,31.1736715059612,-3.0386054611294));
#82455=CARTESIAN_POINT('Ctrl Pts',(-12.9685271684603,31.1433129016411,-3.09029543804178));
#82456=CARTESIAN_POINT('Ctrl Pts',(-12.9785209949957,31.112181190035,-3.14152768131535));
#82457=CARTESIAN_POINT('Ctrl Pts',(-12.9885148215312,31.0802908171608,-3.19227899987956));
#82458=CARTESIAN_POINT('Ctrl Pts',(-13.0169030324834,30.9897038303564,-3.33644191209172));
#82459=CARTESIAN_POINT('Ctrl Pts',(-13.0452912434355,30.892967802122,-3.47676099978773));
#82460=CARTESIAN_POINT('Ctrl Pts',(-13.0736794543876,30.7904285700081,-3.61272668709525));
#82461=CARTESIAN_POINT('Ctrl Pts',(-13.1020615285156,30.6879115043224,-3.74866298200747));
#82462=CARTESIAN_POINT('Ctrl Pts',(-13.1304436026435,30.5795939149887,-3.88024752181972));
#82463=CARTESIAN_POINT('Ctrl Pts',(-13.1588256767714,30.4658634811698,-4.00700179280647));
#82464=CARTESIAN_POINT('Ctrl Pts',(-13.176855216554,30.3936169155458,-4.08752167169423));
#82465=CARTESIAN_POINT('Ctrl Pts',(-13.1948847563365,30.3191869158306,-4.16609299770538));
#82466=CARTESIAN_POINT('Ctrl Pts',(-13.2129142961191,30.2426811775992,-4.2426001962529));
#82467=CARTESIAN_POINT('',(-13.4906227946235,30.2426406871193,4.24264068711929));
#82468=CARTESIAN_POINT('Ctrl Pts',(-15.0614191220869,30.2426782484473,-4.24260312545867));
#82469=CARTESIAN_POINT('Ctrl Pts',(-15.0330386320433,30.3631067196343,-4.12217252186706));
#82470=CARTESIAN_POINT('Ctrl Pts',(-15.0046581419997,30.4783899337406,-3.99662567453541));
#82471=CARTESIAN_POINT('Ctrl Pts',(-14.976277651956,30.5881149555321,-3.86641968167225));
#82472=CARTESIAN_POINT('Ctrl Pts',(-14.9478886092434,30.6978730437644,-3.73617445027738));
#82473=CARTESIAN_POINT('Ctrl Pts',(-14.9194995665308,30.8020694046409,-3.60126749182685));
#82474=CARTESIAN_POINT('Ctrl Pts',(-14.8911105238182,30.9003311423157,-3.46218929229054));
#82475=CARTESIAN_POINT('Ctrl Pts',(-14.8730802312661,30.9627385963071,-3.37385871169863));
#82476=CARTESIAN_POINT('Ctrl Pts',(-14.8550499387141,31.0227530197161,-3.28384622751062));
#82477=CARTESIAN_POINT('Ctrl Pts',(-14.837019646162,31.080287834931,-3.19228374588672));
#82478=CARTESIAN_POINT('Ctrl Pts',(-14.8090933737951,31.1694008049856,-3.05046692327928));
#82479=CARTESIAN_POINT('Ctrl Pts',(-14.7811671014282,31.2525866330839,-2.90489286188319));
#82480=CARTESIAN_POINT('Ctrl Pts',(-14.7532408290614,31.3295444076921,-2.75607627006915));
#82481=CARTESIAN_POINT('Ctrl Pts',(-14.7253200369762,31.4064870800239,-2.60728888218287));
#82482=CARTESIAN_POINT('Ctrl Pts',(-14.6973992448909,31.4772039929293,-2.45526051379136));
#82483=CARTESIAN_POINT('Ctrl Pts',(-14.6694784528057,31.5414403126701,-2.30053021304105));
#82484=CARTESIAN_POINT('Ctrl Pts',(-14.6415584660166,31.6056747796963,-2.14580437504755));
#82485=CARTESIAN_POINT('Ctrl Pts',(-14.6136384792275,31.6634289028201,-1.98837705042711));
#82486=CARTESIAN_POINT('Ctrl Pts',(-14.5857184924384,31.7144958357582,-1.82880762878485));
#82487=CARTESIAN_POINT('Ctrl Pts',(-14.5578006231568,31.7655588956783,-1.66925030920596));
#82488=CARTESIAN_POINT('Ctrl Pts',(-14.5298827538752,31.809935683519,-1.5075515179884));
#82489=CARTESIAN_POINT('Ctrl Pts',(-14.5019648845936,31.8474690148528,-1.3442864725705));
#82490=CARTESIAN_POINT('Ctrl Pts',(-14.4740437955224,31.8850066749349,-1.18100259766807));
#82491=CARTESIAN_POINT('Ctrl Pts',(-14.4461227064512,31.9156992309195,-1.01615241518673));
#82492=CARTESIAN_POINT('Ctrl Pts',(-14.4182016173801,31.9394403141167,-0.850322735816167));
#82493=CARTESIAN_POINT('Ctrl Pts',(-14.4082079768031,31.947937828371,-0.790968238274906));
#82494=CARTESIAN_POINT('Ctrl Pts',(-14.3982143362261,31.9555452682394,-0.731488341091311));
#82495=CARTESIAN_POINT('Ctrl Pts',(-14.3882206956492,31.962259361791,-0.671910189486545));
#82496=CARTESIAN_POINT('Ctrl Pts',(-14.3602243452432,31.9810683347855,-0.505006967780993));
#82497=CARTESIAN_POINT('Ctrl Pts',(-14.3322279948373,31.992866437625,-0.337298389795841));
#82498=CARTESIAN_POINT('Ctrl Pts',(-14.3042316444314,31.9976086632807,-0.169382177752417));
#82499=CARTESIAN_POINT('Ctrl Pts',(-14.276238095147,32.0023504144621,-0.00148276624575069));
#82500=CARTESIAN_POINT('Ctrl Pts',(-14.2482445458626,32.0000376891145,0.166623926130821));
#82501=CARTESIAN_POINT('Ctrl Pts',(-14.2202509965782,31.9906775694119,0.334338540022986));
#82502=CARTESIAN_POINT('Ctrl Pts',(-14.192254980999,31.9813166250617,0.502067929951041));
#82503=CARTESIAN_POINT('Ctrl Pts',(-14.1642589654198,31.9649070607109,0.669404860761526));
#82504=CARTESIAN_POINT('Ctrl Pts',(-14.1362629498405,31.9415080128943,0.835752674367886));
#82505=CARTESIAN_POINT('Ctrl Pts',(-14.1082673487604,31.9181093115157,1.00209802508714));
#82506=CARTESIAN_POINT('Ctrl Pts',(-14.0802717476803,31.8877213796004,1.16745397934408));
#82507=CARTESIAN_POINT('Ctrl Pts',(-14.0522761466002,31.8504549319236,1.33123141847328));
#82508=CARTESIAN_POINT('Ctrl Pts',(-14.0242754155985,31.8131816555328,1.49503886822536));
#82509=CARTESIAN_POINT('Ctrl Pts',(-13.9962746845967,31.7690274150913,1.65726692091452));
#82510=CARTESIAN_POINT('Ctrl Pts',(-13.968273953595,31.7181536977392,1.81733824287937));
#82511=CARTESIAN_POINT('Ctrl Pts',(-13.9586565507755,31.7006801170433,1.87231789262844));
#82512=CARTESIAN_POINT('Ctrl Pts',(-13.9490391479559,31.6824142643844,1.92704323551223));
#82513=CARTESIAN_POINT('Ctrl Pts',(-13.9394217451364,31.6633640359077,1.98149130626074));
#82514=CARTESIAN_POINT('Ctrl Pts',(-13.9114908001388,31.6080381965145,2.13961986735324));
#82515=CARTESIAN_POINT('Ctrl Pts',(-13.8835598551412,31.5460761816123,2.29545653429214));
#82516=CARTESIAN_POINT('Ctrl Pts',(-13.8556289101436,31.4776927529954,2.44844483372244));
#82517=CARTESIAN_POINT('Ctrl Pts',(-13.8277036153902,31.4093231578906,2.60140218463854));
#82518=CARTESIAN_POINT('Ctrl Pts',(-13.7997783206368,31.3345348698172,2.75151203023619));
#82519=CARTESIAN_POINT('Ctrl Pts',(-13.7718530258833,31.2535904151959,2.8982387322927));
#82520=CARTESIAN_POINT('Ctrl Pts',(-13.7439288447544,31.1726491885345,3.04495958307862));
#82521=CARTESIAN_POINT('Ctrl Pts',(-13.7160046636256,31.0855524349579,3.18829728220577));
#82522=CARTESIAN_POINT('Ctrl Pts',(-13.6880804824967,30.9926085091711,3.32774101668878));
#82523=CARTESIAN_POINT('Ctrl Pts',(-13.6601586138252,30.8996722802569,3.46717320355674));
#82524=CARTESIAN_POINT('Ctrl Pts',(-13.6322367451537,30.8008900220586,3.60271180823876));
#82525=CARTESIAN_POINT('Ctrl Pts',(-13.6043148764822,30.6966134401082,3.73387495695766));
#82526=CARTESIAN_POINT('Ctrl Pts',(-13.5763901169249,30.5923260619,3.86505168563023));
#82527=CARTESIAN_POINT('Ctrl Pts',(-13.5484653573676,30.4825434194855,3.99185180642084));
#82528=CARTESIAN_POINT('Ctrl Pts',(-13.5205405978103,30.3676579772534,4.11382593138488));
#82529=CARTESIAN_POINT('Ctrl Pts',(-13.510567996748,30.3266296317491,4.15738581542576));
#82530=CARTESIAN_POINT('Ctrl Pts',(-13.5005953956858,30.2849508501425,4.20033052409612));
#82531=CARTESIAN_POINT('Ctrl Pts',(-13.4906227946235,30.2426406871193,4.24264068711928));
#82532=CARTESIAN_POINT('',(-10.3490300976385,21.7573593077119,-4.24264069228803));
#82533=CARTESIAN_POINT('Ctrl Pts',(-13.4906227946235,30.2426406871193,4.24264068711928));
#82534=CARTESIAN_POINT('Ctrl Pts',(-13.4624945102889,30.1233024835425,4.36197889069605));
#82535=CARTESIAN_POINT('Ctrl Pts',(-13.4343662259543,29.9989203714952,4.47628452432291));
#82536=CARTESIAN_POINT('Ctrl Pts',(-13.4062379416198,29.8699388455358,4.58514703491752));
#82537=CARTESIAN_POINT('Ctrl Pts',(-13.3781114359764,29.7409654757192,4.69400266159471));
#82538=CARTESIAN_POINT('Ctrl Pts',(-13.3499849303329,29.6073935062869,4.7974156559258));
#82539=CARTESIAN_POINT('Ctrl Pts',(-13.3218584246895,29.4697010859089,4.89501525783557));
#82540=CARTESIAN_POINT('Ctrl Pts',(-13.2937292681557,29.3319956881806,4.99262405839415));
#82541=CARTESIAN_POINT('Ctrl Pts',(-13.2656001116219,29.1901693115166,5.08441819351467));
#82542=CARTESIAN_POINT('Ctrl Pts',(-13.2374709550881,29.0447303746263,5.17006933665578));
#82543=CARTESIAN_POINT('Ctrl Pts',(-13.2093424954878,28.8992950411596,5.25571835768733));
#82544=CARTESIAN_POINT('Ctrl Pts',(-13.1812140358875,28.7502475906313,5.3352245379556));
#82545=CARTESIAN_POINT('Ctrl Pts',(-13.1530855762872,28.5981226861008,5.40830458720368));
#82546=CARTESIAN_POINT('Ctrl Pts',(-13.124953455114,28.445977978978,5.48139414951888));
#82547=CARTESIAN_POINT('Ctrl Pts',(-13.0968213339409,28.2907552928954,5.54805577763542));
#82548=CARTESIAN_POINT('Ctrl Pts',(-13.0686892127677,28.1330117341137,5.60805322212025));
#82549=CARTESIAN_POINT('Ctrl Pts',(-13.059734089882,28.0827982097007,5.62715183487265));
#82550=CARTESIAN_POINT('Ctrl Pts',(-13.0507789669963,28.0323293967946,5.64557553127911));
#82551=CARTESIAN_POINT('Ctrl Pts',(-13.0418238441107,27.9816236668424,5.66331772400333));
#82552=CARTESIAN_POINT('Ctrl Pts',(-13.0139494836753,27.8237933600043,5.71854335085626));
#82553=CARTESIAN_POINT('Ctrl Pts',(-12.98607512324,27.6636310460951,5.76717473111242));
#82554=CARTESIAN_POINT('Ctrl Pts',(-12.9582007628047,27.5017039866551,5.80903478526892));
#82555=CARTESIAN_POINT('Ctrl Pts',(-12.9303304260567,27.339800301522,5.85088879689147));
#82556=CARTESIAN_POINT('Ctrl Pts',(-12.9024600893088,27.1761326868282,5.88597335365304));
#82557=CARTESIAN_POINT('Ctrl Pts',(-12.8745897525608,27.0112817505993,5.91416175133085));
#82558=CARTESIAN_POINT('Ctrl Pts',(-12.8467176433771,26.8464203305474,5.94235194167167));
#82559=CARTESIAN_POINT('Ctrl Pts',(-12.8188455341935,26.6803757513683,5.96364504013599));
#82560=CARTESIAN_POINT('Ctrl Pts',(-12.7909734250098,26.5137376787702,5.97796567382349));
#82561=CARTESIAN_POINT('Ctrl Pts',(-12.7631018264686,26.3471026591335,5.99228604514393));
#82562=CARTESIAN_POINT('Ctrl Pts',(-12.7352302279274,26.1798744846817,5.99963418241472));
#82563=CARTESIAN_POINT('Ctrl Pts',(-12.7073586293862,26.0126470084994,5.99998667108321));
#82564=CARTESIAN_POINT('Ctrl Pts',(-12.6794811226982,25.845384083885,6.00033923447129));
#82565=CARTESIAN_POINT('Ctrl Pts',(-12.6516036160103,25.6781221757056,5.99369318675545));
#82566=CARTESIAN_POINT('Ctrl Pts',(-12.6237261093223,25.5114549724733,5.98007723663156));
#82567=CARTESIAN_POINT('Ctrl Pts',(-12.6134923707475,25.45027200493,5.97507886731628));
#82568=CARTESIAN_POINT('Ctrl Pts',(-12.6032586321727,25.3891691506621,5.9691417404092));
#82569=CARTESIAN_POINT('Ctrl Pts',(-12.5930248935979,25.3281756306373,5.96226903256893));
#82570=CARTESIAN_POINT('Ctrl Pts',(-12.565038533079,25.161375723814,5.94347413391556));
#82571=CARTESIAN_POINT('Ctrl Pts',(-12.53705217256,24.9953411938198,5.91767266664919));
#82572=CARTESIAN_POINT('Ctrl Pts',(-12.5090658120411,24.8306644414388,5.88495151649395));
#82573=CARTESIAN_POINT('Ctrl Pts',(-12.4810844029258,24.6660168240021,5.85223615543083));
#82574=CARTESIAN_POINT('Ctrl Pts',(-12.4531029938104,24.5027268112747,5.81260361565926));
#82575=CARTESIAN_POINT('Ctrl Pts',(-12.425121584695,24.3413770249947,5.76619196929694));
#82576=CARTESIAN_POINT('Ctrl Pts',(-12.3971407460117,24.1800305280088,5.71978126908746));
#82577=CARTESIAN_POINT('Ctrl Pts',(-12.3691599073283,24.0206244797569,5.66659182174747));
#82578=CARTESIAN_POINT('Ctrl Pts',(-12.341179068645,23.8637274319567,5.60681188511132));
#82579=CARTESIAN_POINT('Ctrl Pts',(-12.313200365528,23.7068423589246,5.54703651102683));
#82580=CARTESIAN_POINT('Ctrl Pts',(-12.285221662411,23.5524661955205,5.48067176487843));
#82581=CARTESIAN_POINT('Ctrl Pts',(-12.2572429592941,23.4011488772566,5.40795458947422));
#82582=CARTESIAN_POINT('Ctrl Pts',(-12.229261507797,23.2498166949191,5.33523027097856));
#82583=CARTESIAN_POINT('Ctrl Pts',(-12.2012800563,23.1015442398978,5.25615241184179));
#82584=CARTESIAN_POINT('Ctrl Pts',(-12.1732986048029,22.956858815793,5.1710049055269));
#82585=CARTESIAN_POINT('Ctrl Pts',(-12.1636077175636,22.9067495450027,5.14151555317889));
#82586=CARTESIAN_POINT('Ctrl Pts',(-12.1539168303243,22.8570703051347,5.11129857214482));
#82587=CARTESIAN_POINT('Ctrl Pts',(-12.144225943085,22.8078422705457,5.08036701728184));
#82588=CARTESIAN_POINT('Ctrl Pts',(-12.1162733741538,22.6658480448137,4.99114748576642));
#82589=CARTESIAN_POINT('Ctrl Pts',(-12.0883208052225,22.5275823738739,4.89596231205403));
#82590=CARTESIAN_POINT('Ctrl Pts',(-12.0603682362912,22.3935393131819,4.79514768431963));
#82591=CARTESIAN_POINT('Ctrl Pts',(-12.0324186026479,22.2595103282974,4.69434364308838));
#82592=CARTESIAN_POINT('Ctrl Pts',(-12.0044689690045,22.1297033193408,4.58791151666546));
#82593=CARTESIAN_POINT('Ctrl Pts',(-11.9765193353612,22.0045811655867,4.47622925436303));
#82594=CARTESIAN_POINT('Ctrl Pts',(-11.9485670282336,21.8794470434428,4.3645363092454));
#82595=CARTESIAN_POINT('Ctrl Pts',(-11.9206147211059,21.758998907872,4.24759243207913));
#82596=CARTESIAN_POINT('Ctrl Pts',(-11.8926624139783,21.6436650824415,4.12581459666584));
#82597=CARTESIAN_POINT('Ctrl Pts',(-11.8647102876227,21.5283320028931,4.00403754880902));
#82598=CARTESIAN_POINT('Ctrl Pts',(-11.8367581612671,21.4181133811633,3.87742683525044));
#82599=CARTESIAN_POINT('Ctrl Pts',(-11.8088060349114,21.3133994780108,3.74643504511826));
#82600=CARTESIAN_POINT('Ctrl Pts',(-11.7808481081224,21.2086638453477,3.61541607246872));
#82601=CARTESIAN_POINT('Ctrl Pts',(-11.7528901813333,21.1094354088864,3.48001445278672));
#82602=CARTESIAN_POINT('Ctrl Pts',(-11.7249322545442,21.0160635480069,3.34071510944811));
#82603=CARTESIAN_POINT('Ctrl Pts',(-11.7150971672202,20.9832170350203,3.29171214809656));
#82604=CARTESIAN_POINT('Ctrl Pts',(-11.7052620798962,20.9510948904246,3.24222711380554));
#82605=CARTESIAN_POINT('Ctrl Pts',(-11.6954269925722,20.9197110486641,3.19228196920867));
#82606=CARTESIAN_POINT('Ctrl Pts',(-11.6675007278284,20.8305981160787,3.05046509613738));
#82607=CARTESIAN_POINT('Ctrl Pts',(-11.6395744630847,20.747412334659,2.90489099532772));
#82608=CARTESIAN_POINT('Ctrl Pts',(-11.611648198341,20.670454613249,2.75607437681959));
#82609=CARTESIAN_POINT('Ctrl Pts',(-11.5837274109289,20.5935119859795,2.60728694653193));
#82610=CARTESIAN_POINT('Ctrl Pts',(-11.5558066235168,20.5227951259649,2.45525854777079));
#82611=CARTESIAN_POINT('Ctrl Pts',(-11.5278858361047,20.4585588640983,2.30052823006726));
#82612=CARTESIAN_POINT('Ctrl Pts',(-11.4999658496265,20.3943244449088,2.14580235094729));
#82613=CARTESIAN_POINT('Ctrl Pts',(-11.4720458631482,20.3365703766266,1.98837499777321));
#82614=CARTESIAN_POINT('Ctrl Pts',(-11.44412587667,20.2855035025929,1.82880556132206));
#82615=CARTESIAN_POINT('Ctrl Pts',(-11.4162080051734,20.2344404969532,1.66924821250002));
#82616=CARTESIAN_POINT('Ctrl Pts',(-11.3882901336769,20.1900637686612,1.50754940539573));
#82617=CARTESIAN_POINT('Ctrl Pts',(-11.3603722621804,20.1525304990906,1.34428435828654));
#82618=CARTESIAN_POINT('Ctrl Pts',(-11.3324511672218,20.1149928958417,1.1810004602169));
#82619=CARTESIAN_POINT('Ctrl Pts',(-11.3045300722631,20.0843004007024,1.01615026835585));
#82620=CARTESIAN_POINT('Ctrl Pts',(-11.2766089773045,20.0605593792441,0.850320593961511));
#82621=CARTESIAN_POINT('Ctrl Pts',(-11.2666153322228,20.052061885049,0.790966083962213));
#82622=CARTESIAN_POINT('Ctrl Pts',(-11.2566216871411,20.0444544657807,0.731486176094842));
#82623=CARTESIAN_POINT('Ctrl Pts',(-11.2466280420594,20.0377403932269,0.671908015610335));
#82624=CARTESIAN_POINT('Ctrl Pts',(-11.2186317076778,20.0189314982998,0.505004939793092));
#82625=CARTESIAN_POINT('Ctrl Pts',(-11.1906353732962,20.007133461194,0.337296513475724));
#82626=CARTESIAN_POINT('Ctrl Pts',(-11.1626390389146,20.0023912881466,0.169380457846953));
#82627=CARTESIAN_POINT('Ctrl Pts',(-11.1346455050256,19.997649589462,0.00148119897672991));
#82628=CARTESIAN_POINT('Ctrl Pts',(-11.1066519711366,19.9999623544989,-0.166625336025476));
#82629=CARTESIAN_POINT('Ctrl Pts',(-11.0786584372476,20.0093225002884,-0.33433978891192));
#82630=CARTESIAN_POINT('Ctrl Pts',(-11.0506624358882,20.0186834711215,-0.502069024871426));
#82631=CARTESIAN_POINT('Ctrl Pts',(-11.0226664345287,20.0350930489421,-0.669405798047149));
#82632=CARTESIAN_POINT('Ctrl Pts',(-10.9946704331693,20.0584920964223,-0.835753451517604));
#82633=CARTESIAN_POINT('Ctrl Pts',(-10.9666748455537,20.0818907980955,-1.00209864658985));
#82634=CARTESIAN_POINT('Ctrl Pts',(-10.9386792579381,20.1122787168752,-1.16745444264423));
#82635=CARTESIAN_POINT('Ctrl Pts',(-10.9106836703225,20.1495451372064,-1.33123172228389));
#82636=CARTESIAN_POINT('Ctrl Pts',(-10.8826829514969,20.1868183879651,-1.49503902006914));
#82637=CARTESIAN_POINT('Ctrl Pts',(-10.8546822326712,20.2309725891922,-1.65726691935743));
#82638=CARTESIAN_POINT('Ctrl Pts',(-10.8266815138456,20.2818462529875,-1.81733808784359));
#82639=CARTESIAN_POINT('Ctrl Pts',(-10.8170640397459,20.2993199523933,-1.87231811627087));
#82640=CARTESIAN_POINT('Ctrl Pts',(-10.8074465656462,20.3175859345044,-1.92704383383409));
#82641=CARTESIAN_POINT('Ctrl Pts',(-10.7978290915466,20.336636302958,-1.9814922747834));
#82642=CARTESIAN_POINT('Ctrl Pts',(-10.769897967176,20.3919624941248,-2.13962175453832));
#82643=CARTESIAN_POINT('Ctrl Pts',(-10.7419668428055,20.4539249378764,-2.29545931101644));
#82644=CARTESIAN_POINT('Ctrl Pts',(-10.714035718435,20.522308869905,-2.44844846449311));
#82645=CARTESIAN_POINT('Ctrl Pts',(-10.6861102453204,20.5906789659313,-2.60140666393984));
#82646=CARTESIAN_POINT('Ctrl Pts',(-10.6581847722058,20.6654678290136,-2.75151732279546));
#82647=CARTESIAN_POINT('Ctrl Pts',(-10.6302592990912,20.7464129302101,-2.89824479644781));
#82648=CARTESIAN_POINT('Ctrl Pts',(-10.6023349425737,20.8273547948253,-3.04496640321761));
#82649=CARTESIAN_POINT('Ctrl Pts',(-10.5744105860562,20.9144522566137,-3.18830481739469));
#82650=CARTESIAN_POINT('Ctrl Pts',(-10.5464862295387,21.0073969583467,-3.32774921958888));
#82651=CARTESIAN_POINT('Ctrl Pts',(-10.5185641876098,21.1003339560975,-3.46718206354282));
#82652=CARTESIAN_POINT('Ctrl Pts',(-10.4906421456808,21.1991170499757,-3.60272127857529));
#82653=CARTESIAN_POINT('Ctrl Pts',(-10.4627201037519,21.3033945318271,-3.73388498434647));
#82654=CARTESIAN_POINT('Ctrl Pts',(-10.4347951752472,21.4076827938663,-3.86506224979871));
#82655=CARTESIAN_POINT('Ctrl Pts',(-10.4068702467424,21.5174663826501,-3.99186285542055));
#82656=CARTESIAN_POINT('Ctrl Pts',(-10.3789453182376,21.6323528310669,-4.1138374065719));
#82657=CARTESIAN_POINT('Ctrl Pts',(-10.368973592503,21.6733776864767,-4.15739335589082));
#82658=CARTESIAN_POINT('Ctrl Pts',(-10.3590018667683,21.7150528635581,-4.20033423779668));
#82659=CARTESIAN_POINT('Ctrl Pts',(-10.3490301410337,21.7573593128807,-4.24264068711927));
#82660=CARTESIAN_POINT('Ctrl Pts',(-10.3490300482133,21.7573593128807,-4.24264068711927));
#82661=CARTESIAN_POINT('Ctrl Pts',(-10.3209012858048,21.8766995447535,-4.36198091899205));
#82662=CARTESIAN_POINT('Ctrl Pts',(-10.2927725233962,22.0010838302075,-4.47628838371058));
#82663=CARTESIAN_POINT('Ctrl Pts',(-10.2646437609877,22.1300676541458,-4.5851525207469));
#82664=CARTESIAN_POINT('Ctrl Pts',(-10.2365167703473,22.2590433536801,-4.69400980067342));
#82665=CARTESIAN_POINT('Ctrl Pts',(-10.208389779707,22.3926177796726,-4.79742424096074));
#82666=CARTESIAN_POINT('Ctrl Pts',(-10.1802627890666,22.5303127634901,-4.89502507458337));
#82667=CARTESIAN_POINT('Ctrl Pts',(-10.1521331422088,22.6680207507538,-4.99263512529695));
#82668=CARTESIAN_POINT('Ctrl Pts',(-10.1240034953511,22.8098498254159,-5.08443029412364));
#82669=CARTESIAN_POINT('Ctrl Pts',(-10.0958738484933,22.9552915492135,-5.17008224786698));
#82670=CARTESIAN_POINT('Ctrl Pts',(-10.067744896948,23.100729677963,-5.25573208445378));
#82671=CARTESIAN_POINT('Ctrl Pts',(-10.0396159454026,23.2497800131169,-5.3352388564859));
#82672=CARTESIAN_POINT('Ctrl Pts',(-10.0114869938573,23.4019078724027,-5.40831926725084));
#82673=CARTESIAN_POINT('Ctrl Pts',(-9.98335438226454,23.554055526069,-5.48140918700032));
#82674=CARTESIAN_POINT('Ctrl Pts',(-9.95522177067182,23.7092812285162,-5.54807094298151));
#82675=CARTESIAN_POINT('Ctrl Pts',(-9.9270891590791,23.8670278544895,-5.60806827940568));
#82676=CARTESIAN_POINT('Ctrl Pts',(-9.91813647195288,23.9172278219863,-5.62716133017494));
#82677=CARTESIAN_POINT('Ctrl Pts',(-9.90918378482667,23.967682935363,-5.64557983134726));
#82678=CARTESIAN_POINT('Ctrl Pts',(-9.90023109770045,24.01837483853,-5.66331720102528));
#82679=CARTESIAN_POINT('Ctrl Pts',(-9.8723571003697,24.1762029803656,-5.7185421170856));
#82680=CARTESIAN_POINT('Ctrl Pts',(-9.84448310303895,24.336363124577,-5.76717298671253));
#82681=CARTESIAN_POINT('Ctrl Pts',(-9.8166091057082,24.4982880286785,-5.80903272113263));
#82682=CARTESIAN_POINT('Ctrl Pts',(-9.78873914432011,24.6601894872864,-5.85088639458181));
#82683=CARTESIAN_POINT('Ctrl Pts',(-9.76086918293202,24.82385488824,-5.88597080996578));
#82684=CARTESIAN_POINT('Ctrl Pts',(-9.73299922154392,24.9887036411706,-5.91415925340351));
#82685=CARTESIAN_POINT('Ctrl Pts',(-9.70512750269832,25.1535627893319,-5.94234947438196));
#82686=CARTESIAN_POINT('Ctrl Pts',(-9.67725578385272,25.3196051257821,-5.96364279802991));
#82687=CARTESIAN_POINT('Ctrl Pts',(-9.64938406500712,25.4862410014732,-5.97796384159628));
#82688=CARTESIAN_POINT('Ctrl Pts',(-9.62151286463947,25.6528737773544,-5.99228461875837));
#82689=CARTESIAN_POINT('Ctrl Pts',(-9.59364166427182,25.8200997535212,-5.99963335046843));
#82690=CARTESIAN_POINT('Ctrl Pts',(-9.56577046390418,25.9873250923379,-5.99998661221137));
#82691=CARTESIAN_POINT('Ctrl Pts',(-9.53789336415152,26.1545858270703,-6.00033994872781));
#82692=CARTESIAN_POINT('Ctrl Pts',(-9.51001626439885,26.3218456062963,-5.99369485719773));
#82693=CARTESIAN_POINT('Ctrl Pts',(-9.48213916464618,26.4885107560557,-5.98008003635552));
#82694=CARTESIAN_POINT('Ctrl Pts',(-9.47190349216001,26.5497054249033,-5.9750810641405));
#82695=CARTESIAN_POINT('Ctrl Pts',(-9.46166781967383,26.6108199580132,-5.96914297538562));
#82696=CARTESIAN_POINT('Ctrl Pts',(-9.45143214718766,26.6718251172582,-5.96226894829653));
#82697=CARTESIAN_POINT('Ctrl Pts',(-9.42344576703072,26.8386254501595,-5.9434739804442));
#82698=CARTESIAN_POINT('Ctrl Pts',(-9.39545938687379,27.004660375534,-5.91767241102094));
#82699=CARTESIAN_POINT('Ctrl Pts',(-9.36747300671686,27.1693374907124,-5.88495113257657));
#82700=CARTESIAN_POINT('Ctrl Pts',(-9.3394915717959,27.333985507194,-5.8522356360319));
#82701=CARTESIAN_POINT('Ctrl Pts',(-9.31151013687494,27.4972758858009,-5.81260293161189));
#82702=CARTESIAN_POINT('Ctrl Pts',(-9.28352870195398,27.6586260035525,-5.76619109814611));
#82703=CARTESIAN_POINT('Ctrl Pts',(-9.25554782894945,27.8199728811099,-5.71978019671158));
#82704=CARTESIAN_POINT('Ctrl Pts',(-9.22756695594493,27.9793792743505,-5.66659052157172));
#82705=CARTESIAN_POINT('Ctrl Pts',(-9.19958608294041,28.1362766307547,-5.60681033716064));
#82706=CARTESIAN_POINT('Ctrl Pts',(-9.17160734074356,28.2931620390651,-5.54703470514777));
#82707=CARTESIAN_POINT('Ctrl Pts',(-9.14362859854671,28.4475385005199,-5.48066967886209));
#82708=CARTESIAN_POINT('Ctrl Pts',(-9.11564985634986,28.5988560794148,-5.40795220748931));
#82709=CARTESIAN_POINT('Ctrl Pts',(-9.08766835933929,28.7501885571833,-5.33522757628474));
#82710=CARTESIAN_POINT('Ctrl Pts',(-9.05968686232871,28.8984612688081,-5.25614938568914));
#82711=CARTESIAN_POINT('Ctrl Pts',(-9.03170536531814,29.0431469109443,-5.17100153533239));
#82712=CARTESIAN_POINT('Ctrl Pts',(-9.02201464243703,29.0932553258832,-5.14151261194071));
#82713=CARTESIAN_POINT('Ctrl Pts',(-9.01232391955593,29.1429337212672,-5.11129608540006));
#82714=CARTESIAN_POINT('Ctrl Pts',(-9.00263319667482,29.1921609239478,-5.08036501007758));
#82715=CARTESIAN_POINT('Ctrl Pts',(-8.97454195866122,29.3348595733893,-4.99070274137374));
#82716=CARTESIAN_POINT('Ctrl Pts',(-8.94645072064762,29.473791457817,-4.89501624427522));
#82717=CARTESIAN_POINT('Ctrl Pts',(-8.91835948263403,29.6084577278052,-4.79364504595855));
#82718=CARTESIAN_POINT('Ctrl Pts',(-8.8902701958346,29.7431146438897,-4.69228088887367));
#82719=CARTESIAN_POINT('Ctrl Pts',(-8.86218090903517,29.8735062904475,-4.58523300206302));
#82720=CARTESIAN_POINT('Ctrl Pts',(-8.83409162223575,29.9991649005209,-4.47288275035703));
#82721=CARTESIAN_POINT('Ctrl Pts',(-8.81547232218614,30.0824591251654,-4.39841012091293));
#82722=CARTESIAN_POINT('Ctrl Pts',(-8.79685302213653,30.1636743680789,-4.3216085697427));
#82723=CARTESIAN_POINT('Ctrl Pts',(-8.77823372208692,30.2426826788146,-4.24259869500835));
#82724=CARTESIAN_POINT('Origin',(-31.4159265358979,26.,7.7715611723761E-15));
#82725=CARTESIAN_POINT('',(-0.646543496119136,30.2426884810913,-4.2425928926089));
#82726=CARTESIAN_POINT('',(-2.4950483220781,30.2426872863809,-4.24259408734582));
#82727=CARTESIAN_POINT('',(-31.4159265358979,30.2426406871193,-4.24264068711928));
#82728=CARTESIAN_POINT('',(-2.21733987300771,21.7573593180495,-4.24264068195053));
#82729=CARTESIAN_POINT('Ctrl Pts',(-0.646543496119133,30.2426884810913,
-4.24259289260889));
#82730=CARTESIAN_POINT('Ctrl Pts',(-0.674631828671807,30.1234996154242,
-4.36178444368155));
#82731=CARTESIAN_POINT('Ctrl Pts',(-0.702720161224486,29.9992866956845,
-4.47594853295759));
#82732=CARTESIAN_POINT('Ctrl Pts',(-0.730808493777161,29.8704949120925,
-4.58467764793407));
#82733=CARTESIAN_POINT('Ctrl Pts',(-0.758901295988709,29.7416826340358,
-4.69342406482951));
#82734=CARTESIAN_POINT('Ctrl Pts',(-0.78699409820026,29.6082902705929,-4.79673358053653));
#82735=CARTESIAN_POINT('Ctrl Pts',(-0.81508690041181,29.470796620725,-4.89423853296546));
#82736=CARTESIAN_POINT('Ctrl Pts',(-0.8337055909559,29.3796717945368,-4.95886058533744));
#82737=CARTESIAN_POINT('Ctrl Pts',(-0.852324281499978,29.2867461748589,
-5.02093383373948));
#82738=CARTESIAN_POINT('Ctrl Pts',(-0.870942972044066,29.1921664334504,
-5.0803615482712));
#82739=CARTESIAN_POINT('Ctrl Pts',(-0.898924591431005,29.0500246260263,
-5.16967414977368));
#82740=CARTESIAN_POINT('Ctrl Pts',(-0.926906210817951,28.9041190310538,
-5.25302596012802));
#82741=CARTESIAN_POINT('Ctrl Pts',(-0.954887830204889,28.7549680880225,
-5.33011733773072));
#82742=CARTESIAN_POINT('Ctrl Pts',(-0.982866636230461,28.6058321411033,
-5.40720096432014));
#82743=CARTESIAN_POINT('Ctrl Pts',(-1.01084544225603,28.4534517752157,-5.47802527131782));
#82744=CARTESIAN_POINT('Ctrl Pts',(-1.0388242482816,28.2983695092723,-5.54233683556378));
#82745=CARTESIAN_POINT('Ctrl Pts',(-1.06680563972006,28.1432729127786,-5.6066543425918));
#82746=CARTESIAN_POINT('Ctrl Pts',(-1.09478703115852,27.9854742052433,-5.66445778234588));
#82747=CARTESIAN_POINT('Ctrl Pts',(-1.12276842259697,27.8255360592375,-5.71554180252613));
#82748=CARTESIAN_POINT('Ctrl Pts',(-1.15074950738818,27.6655996659891,-5.7666252628781));
#82749=CARTESIAN_POINT('Ctrl Pts',(-1.17873059217939,27.5035241798124,-5.81098935838577));
#82750=CARTESIAN_POINT('Ctrl Pts',(-1.2067116769706,27.3398878506923,-5.84847848141439));
#82751=CARTESIAN_POINT('Ctrl Pts',(-1.23469815980102,27.1762199532706,-5.88597483674862));
#82752=CARTESIAN_POINT('Ctrl Pts',(-1.26268464263146,27.0109909162775,-5.91659350071789));
#82753=CARTESIAN_POINT('Ctrl Pts',(-1.29067112546188,26.8447903916065,-5.94022972571342));
#82754=CARTESIAN_POINT('Ctrl Pts',(-1.30036139116022,26.7872437805148,-5.94841372302741));
#82755=CARTESIAN_POINT('Ctrl Pts',(-1.31005165685856,26.7295807759789,-5.95576106384891));
#82756=CARTESIAN_POINT('Ctrl Pts',(-1.3197419225569,26.6718260604999,-5.9622688420125));
#82757=CARTESIAN_POINT('Ctrl Pts',(-1.34761817735919,26.5056814763528,-5.98098994708151));
#82758=CARTESIAN_POINT('Ctrl Pts',(-1.37549443216149,26.3387253218434,-5.99276527668446));
#82759=CARTESIAN_POINT('Ctrl Pts',(-1.4033706869638,26.1715498460393,-5.99754705278115));
#82760=CARTESIAN_POINT('Ctrl Pts',(-1.43124158161395,26.0044065153706,-6.00232790941976));
#82761=CARTESIAN_POINT('Ctrl Pts',(-1.45911247626411,25.8370442651252,-6.0001178868363));
#82762=CARTESIAN_POINT('Ctrl Pts',(-1.48698337091426,25.6700572898176,-5.99092128207319));
#82763=CARTESIAN_POINT('Ctrl Pts',(-1.51485406973379,25.5030714878188,-5.98172474192863));
#82764=CARTESIAN_POINT('Ctrl Pts',(-1.54272476855332,25.3364612730271,-5.96554173164693));
#82765=CARTESIAN_POINT('Ctrl Pts',(-1.57059546737285,25.1708183503036,-5.94242861057722));
#82766=CARTESIAN_POINT('Ctrl Pts',(-1.59846451933102,25.0051852153121,-5.91931685524672));
#82767=CARTESIAN_POINT('Ctrl Pts',(-1.62633357128919,24.8405195727728,-5.88927585270327));
#82768=CARTESIAN_POINT('Ctrl Pts',(-1.65420262324735,24.6774058013829,-5.85241356927074));
#82769=CARTESIAN_POINT('Ctrl Pts',(-1.68207593600995,24.514267092084,-5.81554565008924));
#82770=CARTESIAN_POINT('Ctrl Pts',(-1.70994924877255,24.3526810379655,-5.7718544368111));
#82771=CARTESIAN_POINT('Ctrl Pts',(-1.73782256153514,24.1932203771043,-5.72149870176414));
#82772=CARTESIAN_POINT('Ctrl Pts',(-1.74806199871334,24.134641497974,-5.70300020501327));
#82773=CARTESIAN_POINT('Ctrl Pts',(-1.75830143589153,24.0763493030335,-5.68360281467021));
#82774=CARTESIAN_POINT('Ctrl Pts',(-1.76854087306972,24.0183716559267,-5.66331608741428));
#82775=CARTESIAN_POINT('Ctrl Pts',(-1.79667445855355,23.8590739267015,-5.60757685433833));
#82776=CARTESIAN_POINT('Ctrl Pts',(-1.82480804403738,23.7021159420866,-5.54510773076916));
#82777=CARTESIAN_POINT('Ctrl Pts',(-1.85294162952121,23.5480610580687,-5.47612960265194));
#82778=CARTESIAN_POINT('Ctrl Pts',(-1.88107174638236,23.3940251676578,-5.40715997892888));
#82779=CARTESIAN_POINT('Ctrl Pts',(-1.90920186324351,23.242891941793,-5.33168307752339));
#82780=CARTESIAN_POINT('Ctrl Pts',(-1.93733198010466,23.0952036305205,-5.24996743340936));
#82781=CARTESIAN_POINT('Ctrl Pts',(-1.96546224351292,22.9475145498487,-5.16825136358818));
#82782=CARTESIAN_POINT('Ctrl Pts',(-1.9935925069212,22.803270687939,-5.08029663171037));
#82783=CARTESIAN_POINT('Ctrl Pts',(-2.02172277032946,22.662989291288,-4.98641750457591));
#82784=CARTESIAN_POINT('Ctrl Pts',(-2.04985087654862,22.5227186522149,-4.89254557662859));
#82785=CARTESIAN_POINT('Ctrl Pts',(-2.07797898276777,22.3864101243919,-4.79275033176879));
#82786=CARTESIAN_POINT('Ctrl Pts',(-2.10610708898693,22.2545519110613,-4.68738931742023));
#82787=CARTESIAN_POINT('Ctrl Pts',(-2.13423674266047,22.1226864436138,-4.58202250668559));
#82788=CARTESIAN_POINT('Ctrl Pts',(-2.162366396334,21.99527201849,-4.47108950501785));
#82789=CARTESIAN_POINT('Ctrl Pts',(-2.19049605000754,21.8727642991052,-4.3549885728047));
#82790=CARTESIAN_POINT('Ctrl Pts',(-2.19944397453254,21.8337951088156,-4.31805735456851));
#82791=CARTESIAN_POINT('Ctrl Pts',(-2.20839189905755,21.7953221415358,-4.28060351577433));
#82792=CARTESIAN_POINT('Ctrl Pts',(-2.21733982358255,21.7573593128807,-4.24264068711927));
#82793=CARTESIAN_POINT('',(-5.35893256999276,30.2426406871193,4.24264068711929));
#82794=CARTESIAN_POINT('Ctrl Pts',(-2.21733991640297,21.7573593128807,-4.24264068711927));
#82795=CARTESIAN_POINT('Ctrl Pts',(-2.24526622497855,21.6388780198769,-4.12415939411543));
#82796=CARTESIAN_POINT('Ctrl Pts',(-2.27319253355414,21.5253506939012,-4.00069969038654));
#82797=CARTESIAN_POINT('Ctrl Pts',(-2.30111884212972,21.4171835885019,-3.87269850859888));
#82798=CARTESIAN_POINT('Ctrl Pts',(-2.329042244992,21.309027737816,-3.74471064524665));
#82799=CARTESIAN_POINT('Ctrl Pts',(-2.35696564785428,21.206231197651,-3.61218248780336));
#82800=CARTESIAN_POINT('Ctrl Pts',(-2.38488905071656,21.1091605367417,-3.47558474859055));
#82801=CARTESIAN_POINT('Ctrl Pts',(-2.4128153837417,21.012079689651,-3.33897267539329));
#82802=CARTESIAN_POINT('Ctrl Pts',(-2.44074171676684,20.9207261070017,-3.19829042261256));
#82803=CARTESIAN_POINT('Ctrl Pts',(-2.46866804979198,20.8354239848706,-3.0540390606458));
#82804=CARTESIAN_POINT('Ctrl Pts',(-2.49659440842889,20.7501217845073,-2.90978756638336));
#82805=CARTESIAN_POINT('Ctrl Pts',(-2.52452076706581,20.6708712133814,-2.76196722932661));
#82806=CARTESIAN_POINT('Ctrl Pts',(-2.55244712570272,20.5979514241649,-2.61110535680167));
#82807=CARTESIAN_POINT('Ctrl Pts',(-2.58037976170836,20.5250152438246,-2.46020957310296));
#82808=CARTESIAN_POINT('Ctrl Pts',(-2.608312397714,20.4584128247526,-2.30627117225125));
#82809=CARTESIAN_POINT('Ctrl Pts',(-2.63624503371964,20.3983762599628,-2.14983987195589));
#82810=CARTESIAN_POINT('Ctrl Pts',(-2.64620964478503,20.3769589824201,-2.09403500393051));
#82811=CARTESIAN_POINT('Ctrl Pts',(-2.65617425585041,20.3563768384129,-2.03791306921283));
#82812=CARTESIAN_POINT('Ctrl Pts',(-2.6661388669158,20.3366388642348,-1.98149959523188));
#82813=CARTESIAN_POINT('Ctrl Pts',(-2.69413936958568,20.2811752645975,-1.82297804145962));
#82814=CARTESIAN_POINT('Ctrl Pts',(-2.72213987225557,20.232363981333,-1.66210497024651));
#82815=CARTESIAN_POINT('Ctrl Pts',(-2.75014037492545,20.1903836434445,-1.49945249662752));
#82816=CARTESIAN_POINT('Ctrl Pts',(-2.77813615756997,20.1484103821525,-1.33682744122351));
#82817=CARTESIAN_POINT('Ctrl Pts',(-2.80613194021447,20.1132658459979,-1.17242388398358));
#82818=CARTESIAN_POINT('Ctrl Pts',(-2.83412772285899,20.0850782955521,-1.0068273090513));
#82819=CARTESIAN_POINT('Ctrl Pts',(-2.86212314122732,20.0568911118777,-0.841232888832398));
#82820=CARTESIAN_POINT('Ctrl Pts',(-2.89011855959567,20.0356607884437,-0.674445788908477));
#82821=CARTESIAN_POINT('Ctrl Pts',(-2.918113977964,20.021464261399,-0.507060570613027));
#82822=CARTESIAN_POINT('Ctrl Pts',(-2.94610734130233,20.0072687764636,-0.339687639386882));
#82823=CARTESIAN_POINT('Ctrl Pts',(-2.97410070464067,20.0001060815898,-0.171716988407973));
#82824=CARTESIAN_POINT('Ctrl Pts',(-3.002094067979,20.0000011703201,-0.00374751118958749));
#82825=CARTESIAN_POINT('Ctrl Pts',(-3.030090186961,19.9998962487231,0.164238500805971));
#82826=CARTESIAN_POINT('Ctrl Pts',(-3.05808630594298,20.0068504990882,0.332223026852808));
#82827=CARTESIAN_POINT('Ctrl Pts',(-3.08608242492498,20.0208367943488,0.499607205900024));
#82828=CARTESIAN_POINT('Ctrl Pts',(-3.09570088909286,20.0256419846644,0.55711441714853));
#82829=CARTESIAN_POINT('Ctrl Pts',(-3.10531935326074,20.0312767601218,0.614550788877512));
#82830=CARTESIAN_POINT('Ctrl Pts',(-3.11493781742862,20.0377386045537,0.67189214340621));
#82831=CARTESIAN_POINT('Ctrl Pts',(-3.14285895277454,20.0564964883302,0.838346547432625));
#82832=CARTESIAN_POINT('Ctrl Pts',(-3.17078008812047,20.0822314018542,1.00403360360904));
#82833=CARTESIAN_POINT('Ctrl Pts',(-3.19870122346638,20.1148554295047,1.16836354974373));
#82834=CARTESIAN_POINT('Ctrl Pts',(-3.22661912933023,20.1474756837158,1.33267448874964));
#82835=CARTESIAN_POINT('Ctrl Pts',(-3.25453703519406,20.1869834000549,1.49562832166912));
#82836=CARTESIAN_POINT('Ctrl Pts',(-3.28245494105791,20.2332395035258,1.65664521739113));
#82837=CARTESIAN_POINT('Ctrl Pts',(-3.31037536935724,20.279499786323,1.81767666129358));
#82838=CARTESIAN_POINT('Ctrl Pts',(-3.33829579765657,20.3325095899557,1.97677051430215));
#82839=CARTESIAN_POINT('Ctrl Pts',(-3.3662162259559,20.3920796795207,2.1333611225378));
#82840=CARTESIAN_POINT('Ctrl Pts',(-3.39413646367448,20.4516493624691,2.28995066190891));
#82841=CARTESIAN_POINT('Ctrl Pts',(-3.42205670139307,20.5177791268602,2.44403669680262));
#82842=CARTESIAN_POINT('Ctrl Pts',(-3.44997693911165,20.590231130146,2.59507240260436));
#82843=CARTESIAN_POINT('Ctrl Pts',(-3.47790319748545,20.6626987568135,2.74614067739491));
#82844=CARTESIAN_POINT('Ctrl Pts',(-3.50582945585924,20.7414912087847,2.89415702481168));
#82845=CARTESIAN_POINT('Ctrl Pts',(-3.53375571423304,20.8263237715149,3.03859742032546));
#82846=CARTESIAN_POINT('Ctrl Pts',(-3.54374939880251,20.8566819334211,3.09028682792646));
#82847=CARTESIAN_POINT('Ctrl Pts',(-3.55374308337198,20.8878131895755,3.14151852200135));
#82848=CARTESIAN_POINT('Ctrl Pts',(-3.56373676794145,20.9197030952441,3.19226931187323));
#82849=CARTESIAN_POINT('Ctrl Pts',(-3.59169420490673,21.0089154394363,3.33424517662241));
#82850=CARTESIAN_POINT('Ctrl Pts',(-3.61965164187199,21.104096867155,3.47250101481236));
#82851=CARTESIAN_POINT('Ctrl Pts',(-3.64760907883727,21.2049131331077,3.60654154820884));
#82852=CARTESIAN_POINT('Ctrl Pts',(-3.67556125585628,21.3057104313651,3.74055686305599));
#82853=CARTESIAN_POINT('Ctrl Pts',(-3.7035134328753,21.4121402635245,3.87035820492312));
#82854=CARTESIAN_POINT('Ctrl Pts',(-3.73146560989431,21.523826484711,3.99548128027463));
#82855=CARTESIAN_POINT('Ctrl Pts',(-3.75941702854489,21.6355096757468,4.12060096092133));
#82856=CARTESIAN_POINT('Ctrl Pts',(-3.78736844719548,21.7524487642828,4.24104239215249));
#82857=CARTESIAN_POINT('Ctrl Pts',(-3.81531986584607,21.8742284750283,4.35637570966201));
#82858=CARTESIAN_POINT('Ctrl Pts',(-3.8432691162056,21.9959987388882,4.47170008035548));
#82859=CARTESIAN_POINT('Ctrl Pts',(-3.87121836656512,22.1226086460514,4.58191691380431));
#82860=CARTESIAN_POINT('Ctrl Pts',(-3.89916761692465,22.2536071213404,4.6866342292448));
#82861=CARTESIAN_POINT('Ctrl Pts',(-3.92711978554461,22.3846192745514,4.79136247851691));
#82862=CARTESIAN_POINT('Ctrl Pts',(-3.95507195416456,22.5200206661178,4.89058986636883));
#82863=CARTESIAN_POINT('Ctrl Pts',(-3.98302412278452,22.6593277312072,4.98396516766709));
#82864=CARTESIAN_POINT('Ctrl Pts',(-3.9928613213411,22.7083540260272,5.0168267102415));
#82865=CARTESIAN_POINT('Ctrl Pts',(-4.00269851989769,22.7578637813317,5.04896382869954));
#82866=CARTESIAN_POINT('Ctrl Pts',(-4.01253571845427,22.8078350564425,5.08036248442202));
#82867=CARTESIAN_POINT('Ctrl Pts',(-4.04051728858883,22.9499766154631,5.16967487170139));
#82868=CARTESIAN_POINT('Ctrl Pts',(-4.06849885872339,23.0958819368552,5.25302648415614));
#82869=CARTESIAN_POINT('Ctrl Pts',(-4.09648042885795,23.2450325816891,5.3301176838833));
#82870=CARTESIAN_POINT('Ctrl Pts',(-4.12445918870059,23.3941682467756,5.40720114105794));
#82871=CARTESIAN_POINT('Ctrl Pts',(-4.15243794854322,23.546548306925,5.47802529729181));
#82872=CARTESIAN_POINT('Ctrl Pts',(-4.18041670838586,23.7016302440552,5.54233673327037));
#82873=CARTESIAN_POINT('Ctrl Pts',(-4.20839805871158,23.8567265398323,5.60665412368324));
#82874=CARTESIAN_POINT('Ctrl Pts',(-4.23637940903731,24.014524924548,5.66445746696233));
#82875=CARTESIAN_POINT('Ctrl Pts',(-4.26436075936304,24.1744627266629,5.71554141474429));
#82876=CARTESIAN_POINT('Ctrl Pts',(-4.29234180613671,24.3343987937134,5.76662480834867));
#82877=CARTESIAN_POINT('Ctrl Pts',(-4.32032285291038,24.4964739330904,5.81098885970217));
#82878=CARTESIAN_POINT('Ctrl Pts',(-4.34830389968406,24.6601098962103,5.84847796522877));
#82879=CARTESIAN_POINT('Ctrl Pts',(-4.3762903494129,24.8237774563529,5.88597430965383));
#82880=CARTESIAN_POINT('Ctrl Pts',(-4.40427679914175,24.9890061374045,5.91659298696035));
#82881=CARTESIAN_POINT('Ctrl Pts',(-4.4322632488706,25.1552062891796,5.94022925367014));
#82882=CARTESIAN_POINT('Ctrl Pts',(-4.4419537222361,25.212754072472,5.94841345049504));
#82883=CARTESIAN_POINT('Ctrl Pts',(-4.4516441956016,25.2704182524461,5.95576095638831));
#82884=CARTESIAN_POINT('Ctrl Pts',(-4.4613346689671,25.3281741450144,5.96226886516979));
#82885=CARTESIAN_POINT('Ctrl Pts',(-4.48921116242423,25.4943199771698,5.98099010506423));
#82886=CARTESIAN_POINT('Ctrl Pts',(-4.51708765588136,25.6612774018721,5.9927654663902));
#82887=CARTESIAN_POINT('Ctrl Pts',(-4.54496414933848,25.8284541615509,5.99754716741027));
#82888=CARTESIAN_POINT('Ctrl Pts',(-4.57283527846951,25.9955987510912,6.00232794827861));
#82889=CARTESIAN_POINT('Ctrl Pts',(-4.60070640760054,26.1629622738299,6.00011774523284));
#82890=CARTESIAN_POINT('Ctrl Pts',(-4.62857753673157,26.3299505264023,5.99092085159927));
#82891=CARTESIAN_POINT('Ctrl Pts',(-4.65644846200135,26.4969375575519,5.98172402523568));
#82892=CARTESIAN_POINT('Ctrl Pts',(-4.68431938727114,26.663549006492,5.96554062434815));
#82893=CARTESIAN_POINT('Ctrl Pts',(-4.71219031254093,26.8291931592569,5.9424270045699));
#82894=CARTESIAN_POINT('Ctrl Pts',(-4.74005958580881,26.9948274937451,5.91931475481234));
#82895=CARTESIAN_POINT('Ctrl Pts',(-4.76792885907669,27.1594943320396,5.88927315229279));
#82896=CARTESIAN_POINT('Ctrl Pts',(-4.79579813234457,27.3226092857528,5.85241015968981));
#82897=CARTESIAN_POINT('Ctrl Pts',(-4.82367165738117,27.485749124473,5.81554154322584));
#82898=CARTESIAN_POINT('Ctrl Pts',(-4.85154518241778,27.6473362955952,5.77184952786816));
#82899=CARTESIAN_POINT('Ctrl Pts',(-4.87941870745439,27.8067980508674,5.72149288240244));
#82900=CARTESIAN_POINT('Ctrl Pts',(-4.8896570114629,27.8653704031646,5.70299623928142));
#82901=CARTESIAN_POINT('Ctrl Pts',(-4.89989531547142,27.9236561360343,5.68360090060498));
#82902=CARTESIAN_POINT('Ctrl Pts',(-4.91013361947993,27.9816273951573,5.66331641944561));
#82903=CARTESIAN_POINT('Ctrl Pts',(-4.93826693235807,28.1409236584338,5.60757772927263));
#82904=CARTESIAN_POINT('Ctrl Pts',(-4.96640024523622,28.2978802294315,5.5451092700294));
#82905=CARTESIAN_POINT('Ctrl Pts',(-4.99453355811436,28.4519337618254,5.47613192204322));
#82906=CARTESIAN_POINT('Ctrl Pts',(-5.02266340201436,28.6059682986485,5.40716307930892));
#82907=CARTESIAN_POINT('Ctrl Pts',(-5.05079324591437,28.7571002329714,5.33168707485302));
#82908=CARTESIAN_POINT('Ctrl Pts',(-5.07892308981437,28.9047873242932,5.24997243808246));
#82909=CARTESIAN_POINT('Ctrl Pts',(-5.10705308241398,29.0524751963166,5.16825736935306));
#82910=CARTESIAN_POINT('Ctrl Pts',(-5.1351830750136,29.196717920631,5.08030374801303));
#82911=CARTESIAN_POINT('Ctrl Pts',(-5.16331306761321,29.3369982602062,4.98642583534348));
#82912=CARTESIAN_POINT('Ctrl Pts',(-5.19144090509611,29.4772678525157,4.89255511492108));
#82913=CARTESIAN_POINT('Ctrl Pts',(-5.21956874257901,29.6135754134946,4.79276118064227));
#82914=CARTESIAN_POINT('Ctrl Pts',(-5.24769658006191,29.7454327494578,4.68740157435749));
#82915=CARTESIAN_POINT('Ctrl Pts',(-5.27582597008618,29.8772973634057,4.58203615265417));
#82916=CARTESIAN_POINT('Ctrl Pts',(-5.30395536011045,30.0047110228937,4.47110463550279));
#82917=CARTESIAN_POINT('Ctrl Pts',(-5.33208475013472,30.1272180741514,4.35500527765449));
#82918=CARTESIAN_POINT('Ctrl Pts',(-5.34103402342074,30.1661932911832,4.31806864728964));
#82919=CARTESIAN_POINT('Ctrl Pts',(-5.34998329670675,30.2046721361559,4.28060923808268));
#82920=CARTESIAN_POINT('Ctrl Pts',(-5.35893256999276,30.2426406871193,4.24264068711928));
#82921=CARTESIAN_POINT('Ctrl Pts',(-5.35893256999276,30.2426406871193,4.24264068711928));
#82922=CARTESIAN_POINT('Ctrl Pts',(-5.38685862009565,30.3611208835163,4.12416049072224));
#82923=CARTESIAN_POINT('Ctrl Pts',(-5.41478467019854,30.4746472224472,4.00070195778111));
#82924=CARTESIAN_POINT('Ctrl Pts',(-5.44271072030143,30.5828134533402,3.87270200917711));
#82925=CARTESIAN_POINT('Ctrl Pts',(-5.47063386003537,30.6909684114738,3.74471540034279));
#82926=CARTESIAN_POINT('Ctrl Pts',(-5.4985569997693,30.7937641733863,3.61218856132808));
#82927=CARTESIAN_POINT('Ctrl Pts',(-5.52648013950324,30.8908341729529,3.47559219309117));
#82928=CARTESIAN_POINT('Ctrl Pts',(-5.55440620480455,30.987914342752,3.33898151335911));
#82929=CARTESIAN_POINT('Ctrl Pts',(-5.58233227010586,31.0792673669068,3.19830070794058));
#82930=CARTESIAN_POINT('Ctrl Pts',(-5.61025833540717,31.1645690517271,3.05405083617519));
#82931=CARTESIAN_POINT('Ctrl Pts',(-5.6381844242778,31.2498708085412,2.90980084266435));
#82932=CARTESIAN_POINT('Ctrl Pts',(-5.66611051314844,31.3291210581777,2.76198204972899));
#82933=CARTESIAN_POINT('Ctrl Pts',(-5.69403660201908,31.4020406501665,2.61112175394955));
#82934=CARTESIAN_POINT('Ctrl Pts',(-5.7219689671916,31.4749766306075,2.46022755278642));
#82935=CARTESIAN_POINT('Ctrl Pts',(-5.74990133236411,31.5415789745469,2.30629076733826));
#82936=CARTESIAN_POINT('Ctrl Pts',(-5.77783369753662,31.6016155910704,2.14986110478715));
#82937=CARTESIAN_POINT('Ctrl Pts',(-5.78779963852627,31.623035953213,2.09404883194927));
#82938=CARTESIAN_POINT('Ctrl Pts',(-5.79776557951593,31.643620958814,2.03791940446808));
#82939=CARTESIAN_POINT('Ctrl Pts',(-5.80773152050558,31.6633615678493,1.98149836028398));
#82940=CARTESIAN_POINT('Ctrl Pts',(-5.83573207289206,31.7188252674645,1.82297640987132));
#82941=CARTESIAN_POINT('Ctrl Pts',(-5.86373262527855,31.7676366153877,1.66210293936009));
#82942=CARTESIAN_POINT('Ctrl Pts',(-5.89173317766504,31.8096169836266,1.49945006704371));
#82943=CARTESIAN_POINT('Ctrl Pts',(-5.91972901151066,31.8515902775021,1.33682460433745));
#82944=CARTESIAN_POINT('Ctrl Pts',(-5.94772484535629,31.8867348112181,1.17242064020356));
#82945=CARTESIAN_POINT('Ctrl Pts',(-5.97572067920192,31.9149223252641,1.00682366186531));
#82946=CARTESIAN_POINT('Ctrl Pts',(-6.00371615034491,31.9431094741242,0.841228828934126));
#82947=CARTESIAN_POINT('Ctrl Pts',(-6.03171162148791,31.9643397280031,0.674441319648803));
#82948=CARTESIAN_POINT('Ctrl Pts',(-6.0597070926309,31.9785361518375,0.507055698293729));
#82949=CARTESIAN_POINT('Ctrl Pts',(-6.08770050947458,31.9927315339425,0.33968235964562));
#82950=CARTESIAN_POINT('Ctrl Pts',(-6.11569392631826,31.9998940919681,0.171711307511174));
#82951=CARTESIAN_POINT('Ctrl Pts',(-6.14368734316193,31.9999988334699,0.00374143821752759));
#82952=CARTESIAN_POINT('Ctrl Pts',(-6.17168351621534,32.0001035852844,-0.164244969256905));
#82953=CARTESIAN_POINT('Ctrl Pts',(-6.19967968926875,31.9931491319286,-0.332229881703685));
#82954=CARTESIAN_POINT('Ctrl Pts',(-6.22767586232215,31.9791626015674,-0.499614435357538));
#82955=CARTESIAN_POINT('Ctrl Pts',(-6.23729406522091,31.9743574702873,-0.5571201021531));
#82956=CARTESIAN_POINT('Ctrl Pts',(-6.24691226811966,31.9687227983511,-0.61455493216058));
#82957=CARTESIAN_POINT('Ctrl Pts',(-6.25653047101842,31.9622611017402,-0.671894749700876));
#82958=CARTESIAN_POINT('Ctrl Pts',(-6.28445158780701,31.9435031500081,-0.838349102871839));
#82959=CARTESIAN_POINT('Ctrl Pts',(-6.3123727045956,31.9177681741016,-1.00403609077342));
#82960=CARTESIAN_POINT('Ctrl Pts',(-6.34029382138419,31.8851440935428,-1.16836595219074));
#82961=CARTESIAN_POINT('Ctrl Pts',(-6.3682117124807,31.8525237820036,-1.33267682878248));
#82962=CARTESIAN_POINT('Ctrl Pts',(-6.39612960357722,31.8130160159444,-1.49563058248121));
#82963=CARTESIAN_POINT('Ctrl Pts',(-6.42404749467373,31.7667598741885,-1.65664738355812));
#82964=CARTESIAN_POINT('Ctrl Pts',(-6.45196791391568,31.72049954364,-1.81767876574686));
#82965=CARTESIAN_POINT('Ctrl Pts',(-6.47988833315764,31.6674897009362,-1.97677254082257));
#82966=CARTESIAN_POINT('Ctrl Pts',(-6.50780875239959,31.6079195847332,-2.13336305657655));
#82967=CARTESIAN_POINT('Ctrl Pts',(-6.53572898439683,31.5483498680295,-2.28995252217631));
#82968=CARTESIAN_POINT('Ctrl Pts',(-6.56364921639407,31.4822200807533,-2.44403846815317));
#82969=CARTESIAN_POINT('Ctrl Pts',(-6.59156944839131,31.4097680690463,-2.59507407199231));
#82970=CARTESIAN_POINT('Ctrl Pts',(-6.61949570597962,31.3373004211442,-2.74614227150561));
#82971=CARTESIAN_POINT('Ctrl Pts',(-6.64742196356792,31.2585079601768,-2.89415852951629));
#82972=CARTESIAN_POINT('Ctrl Pts',(-6.67534822115623,31.173675404125,-3.03859882392392));
#82973=CARTESIAN_POINT('Ctrl Pts',(-6.68534195461456,31.1433170952435,-3.09028844966017));
#82974=CARTESIAN_POINT('Ctrl Pts',(-6.6953356880729,31.1121856865101,-3.14152035587315));
#82975=CARTESIAN_POINT('Ctrl Pts',(-6.70532942153124,31.0802956230202,-3.19227135167446));
#82976=CARTESIAN_POINT('Ctrl Pts',(-6.73371647244484,30.9897123730567,-3.33642879871208));
#82977=CARTESIAN_POINT('Ctrl Pts',(-6.76210352335846,30.8929805450667,-3.47674274232387));
#82978=CARTESIAN_POINT('Ctrl Pts',(-6.79049057427206,30.7904459474236,-3.61270364475314));
#82979=CARTESIAN_POINT('Ctrl Pts',(-6.81887149804735,30.6879334811271,-3.74863520101128));
#82980=CARTESIAN_POINT('Ctrl Pts',(-6.84725242182265,30.5796209213999,-3.88021535828063));
#82981=CARTESIAN_POINT('Ctrl Pts',(-6.87563334559794,30.4658959184947,-4.00696564062785));
#82982=CARTESIAN_POINT('Ctrl Pts',(-6.89366519576886,30.3936406166832,-4.08749656761606));
#82983=CARTESIAN_POINT('Ctrl Pts',(-6.91169704593979,30.3192013059224,-4.16607844315121));
#82984=CARTESIAN_POINT('Ctrl Pts',(-6.92972889611071,30.2426857292706,-4.24259564448975));
#82985=CARTESIAN_POINT('',(-7.20743739462351,30.2426406871193,4.24264068711929));
#82986=CARTESIAN_POINT('Ctrl Pts',(-8.77823372208692,30.2426826788146,-4.24259869500835));
#82987=CARTESIAN_POINT('Ctrl Pts',(-8.74985421405489,30.3631070225411,-4.12217196743755));
#82988=CARTESIAN_POINT('Ctrl Pts',(-8.72147470602285,30.4783864730919,-3.99662931378174));
#82989=CARTESIAN_POINT('Ctrl Pts',(-8.69309519799082,30.5881081168997,-3.86642779677049));
#82990=CARTESIAN_POINT('Ctrl Pts',(-8.66470714486868,30.6978627979726,-3.7361870759896));
#82991=CARTESIAN_POINT('Ctrl Pts',(-8.63631909174654,30.8020561403102,-3.60128491292457));
#82992=CARTESIAN_POINT('Ctrl Pts',(-8.6079310386244,30.9003152694159,-3.46221175844709));
#82993=CARTESIAN_POINT('Ctrl Pts',(-8.58989877447026,30.9627300663717,-3.37387164412164));
#82994=CARTESIAN_POINT('Ctrl Pts',(-8.57186651031613,31.0227513077197,-3.28384924170612));
#82995=CARTESIAN_POINT('Ctrl Pts',(-8.55383424616199,31.080292384334,-3.19227650583059));
#82996=CARTESIAN_POINT('Ctrl Pts',(-8.52590799899587,31.1694052275134,-3.0504594364998));
#82997=CARTESIAN_POINT('Ctrl Pts',(-8.49798175182974,31.2525908867869,-2.90488517280906));
#82998=CARTESIAN_POINT('Ctrl Pts',(-8.47005550466362,31.3295484618057,-2.75606843043945));
#82999=CARTESIAN_POINT('Ctrl Pts',(-8.44213472535204,31.4064909688196,-2.60728082583033));
#83000=CARTESIAN_POINT('Ctrl Pts',(-8.41421394604047,31.4772076801296,-2.4552522895582));
#83001=CARTESIAN_POINT('Ctrl Pts',(-8.38629316672889,31.5414437738368,-2.3005218758806));
#83002=CARTESIAN_POINT('Ctrl Pts',(-8.35837317440489,31.6056780569567,-2.14579582350367));
#83003=CARTESIAN_POINT('Ctrl Pts',(-8.33045318208088,31.6634319632521,-1.98836833591238));
#83004=CARTESIAN_POINT('Ctrl Pts',(-8.30253318975688,31.714498658686,-1.82879880792706));
#83005=CARTESIAN_POINT('Ctrl Pts',(-8.27461530435817,31.765561500476,-1.66924132153077));
#83006=CARTESIAN_POINT('Ctrl Pts',(-8.24669741895945,31.8099380444609,-1.50754241849642));
#83007=CARTESIAN_POINT('Ctrl Pts',(-8.21877953356073,31.8474711189296,-1.34427732008116));
#83008=CARTESIAN_POINT('Ctrl Pts',(-8.19085841304085,31.8850085427264,-1.18099330252613));
#83009=CARTESIAN_POINT('Ctrl Pts',(-8.16293729252096,31.9157008419118,-1.01614303450835));
#83010=CARTESIAN_POINT('Ctrl Pts',(-8.13501617200108,31.9394416607826,-0.850313329402882));
#83011=CARTESIAN_POINT('Ctrl Pts',(-8.12502254655044,31.9479390579955,-0.790958979342547));
#83012=CARTESIAN_POINT('Ctrl Pts',(-8.11502892109981,31.9555463845614,-0.731479237943481));
#83013=CARTESIAN_POINT('Ctrl Pts',(-8.10503529564917,31.9622603691794,-0.671901250268776));
#83014=CARTESIAN_POINT('Ctrl Pts',(-8.07703903409974,31.981069005778,-0.504998764902671));
#83015=CARTESIAN_POINT('Ctrl Pts',(-8.04904277255031,31.9928668345532,-0.337290946922631));
#83016=CARTESIAN_POINT('Ctrl Pts',(-8.02104651100088,31.9976088514911,-0.169375513328665));
#83017=CARTESIAN_POINT('Ctrl Pts',(-7.99305304819962,32.0023503943761,-0.00147686601206276));
#83018=CARTESIAN_POINT('Ctrl Pts',(-7.96505958539836,32.0000375248769,0.166629043762389));
#83019=CARTESIAN_POINT('Ctrl Pts',(-7.93706612259709,31.990677328194,0.334342862137911));
#83020=CARTESIAN_POINT('Ctrl Pts',(-7.90907018876753,31.9813163052714,0.502071484883777));
#83021=CARTESIAN_POINT('Ctrl Pts',(-7.88107425493798,31.9649067271477,0.66940763545621));
#83022=CARTESIAN_POINT('Ctrl Pts',(-7.85307832110842,31.9415077333789,0.835754661488181));
#83023=CARTESIAN_POINT('Ctrl Pts',(-7.82508279866994,31.9181090834506,1.0020992431051));
#83024=CARTESIAN_POINT('Ctrl Pts',(-7.79708727623145,31.8877212692587,1.16745442069838));
#83025=CARTESIAN_POINT('Ctrl Pts',(-7.76909175379297,31.8504550085453,1.33123108173894));
#83026=CARTESIAN_POINT('Ctrl Pts',(-7.74109109595693,31.8131819118435,1.49503778537888));
#83027=CARTESIAN_POINT('Ctrl Pts',(-7.7130904381209,31.7690279176645,1.65726508990603));
#83028=CARTESIAN_POINT('Ctrl Pts',(-7.68508978028486,31.7181545160358,1.81733566815265));
#83029=CARTESIAN_POINT('Ctrl Pts',(-7.67547196856869,31.7006802552133,1.87231754364606));
#83030=CARTESIAN_POINT('Ctrl Pts',(-7.66585415685251,31.6824136591051,1.9270450898491));
#83031=CARTESIAN_POINT('Ctrl Pts',(-7.65623634513634,31.6633626250509,1.98149533867154));
#83032=CARTESIAN_POINT('Ctrl Pts',(-7.62830462513129,31.6080352632026,2.13962788994163));
#83033=CARTESIAN_POINT('Ctrl Pts',(-7.60037290512624,31.5460713918224,2.29546841885858));
#83034=CARTESIAN_POINT('Ctrl Pts',(-7.57244118512119,31.4776857840826,2.44846042460541));
#83035=CARTESIAN_POINT('Ctrl Pts',(-7.54451511922803,31.4093140193814,2.6014214607622));
#83036=CARTESIAN_POINT('Ctrl Pts',(-7.51658905333486,31.3345232408874,2.75153483678904));
#83037=CARTESIAN_POINT('Ctrl Pts',(-7.4886629874417,31.2535759864111,2.89826488696343));
#83038=CARTESIAN_POINT('Ctrl Pts',(-7.46073804729851,31.1726319950643,3.04498902218538));
#83039=CARTESIAN_POINT('Ctrl Pts',(-7.43281310715533,31.0855321727043,3.18832982641012));
#83040=CARTESIAN_POINT('Ctrl Pts',(-7.40488816701215,30.9925848854212,3.32777645911853));
#83041=CARTESIAN_POINT('Ctrl Pts',(-7.37696554812668,30.8996453243716,3.46721150034027));
#83042=CARTESIAN_POINT('Ctrl Pts',(-7.34904292924121,30.8008594450044,3.60275275499733));
#83043=CARTESIAN_POINT('Ctrl Pts',(-7.32112031035573,30.6965789646336,3.73391832114218));
#83044=CARTESIAN_POINT('Ctrl Pts',(-7.29319481863296,30.5922877552959,3.86509738234394));
#83045=CARTESIAN_POINT('Ctrl Pts',(-7.26526932691019,30.4825010115459,3.99189960876678));
#83046=CARTESIAN_POINT('Ctrl Pts',(-7.23734383518741,30.3676112099624,4.1138755837544));
#83047=CARTESIAN_POINT('Ctrl Pts',(-7.22737502166611,30.3265979659038,4.15741844275942));
#83048=CARTESIAN_POINT('Ctrl Pts',(-7.21740620814481,30.2849347809671,4.20034659327151));
#83049=CARTESIAN_POINT('Ctrl Pts',(-7.20743739462351,30.2426406871193,4.24264068711928));
#83050=CARTESIAN_POINT('',(-4.06584469763847,21.7573593077119,-4.24264069228803));
#83051=CARTESIAN_POINT('Ctrl Pts',(-7.20743739462351,30.2426406871193,4.24264068711928));
#83052=CARTESIAN_POINT('Ctrl Pts',(-7.17930845867346,30.1232997189722,4.36198165526634));
#83053=CARTESIAN_POINT('Ctrl Pts',(-7.15117952272342,29.9989146447901,4.47628978445081));
#83054=CARTESIAN_POINT('Ctrl Pts',(-7.12305058677337,29.8699299871777,4.58515451150155));
#83055=CARTESIAN_POINT('Ctrl Pts',(-7.09492341999255,29.7409534420544,4.69401239150605));
#83056=CARTESIAN_POINT('Ctrl Pts',(-7.06679625321173,29.6073781246749,4.79742735642718));
#83057=CARTESIAN_POINT('Ctrl Pts',(-7.03866908643091,29.4696822109658,4.89502863678119));
#83058=CARTESIAN_POINT('Ctrl Pts',(-7.0105392613718,29.3319732837149,4.99263914136195));
#83059=CARTESIAN_POINT('Ctrl Pts',(-6.98240943631269,29.190143229949,5.08443468530025));
#83060=CARTESIAN_POINT('Ctrl Pts',(-6.95427961125358,29.0447004950714,5.17008693305169));
#83061=CARTESIAN_POINT('Ctrl Pts',(-6.92615048084451,28.8992613518196,5.25573706566954));
#83062=CARTESIAN_POINT('Ctrl Pts',(-6.89802135043545,28.7502099700108,5.33524405234749));
#83063=CARTESIAN_POINT('Ctrl Pts',(-6.86989222002639,28.5980810389268,5.40832459410204));
#83064=CARTESIAN_POINT('Ctrl Pts',(-6.84175943001676,28.4459323158652,5.48141464363687));
#83065=CARTESIAN_POINT('Ctrl Pts',(-6.81362664000713,28.2907055189682,5.5480764459443));
#83066=CARTESIAN_POINT('Ctrl Pts',(-6.7854938499975,28.1329577804145,5.60807374300387));
#83067=CARTESIAN_POINT('Ctrl Pts',(-6.77654204803523,28.0827627405679,5.62716477241705));
#83068=CARTESIAN_POINT('Ctrl Pts',(-6.76759024607297,28.0323126066951,5.64558138550073));
#83069=CARTESIAN_POINT('Ctrl Pts',(-6.7586384441107,27.9816257293069,5.66331700233609));
#83070=CARTESIAN_POINT('Ctrl Pts',(-6.73076458085901,27.8237983896352,5.71854165547708));
#83071=CARTESIAN_POINT('Ctrl Pts',(-6.70289071760731,27.6636390492527,5.76717233636074));
#83072=CARTESIAN_POINT('Ctrl Pts',(-6.67501685435562,27.5017149435815,5.80903195276322));
#83073=CARTESIAN_POINT('Ctrl Pts',(-6.64714703160113,27.3398143098593,5.85088550134291));
#83074=CARTESIAN_POINT('Ctrl Pts',(-6.61927720884665,27.1761497289779,5.88596986477678));
#83075=CARTESIAN_POINT('Ctrl Pts',(-6.59140738609216,27.0113017847623,5.91415832558926));
#83076=CARTESIAN_POINT('Ctrl Pts',(-6.56353581145049,26.8464434782633,5.9423485583184));
#83077=CARTESIAN_POINT('Ctrl Pts',(-6.53566423680882,26.6804019725943,5.96364196579702));
#83078=CARTESIAN_POINT('Ctrl Pts',(-6.50779266216716,26.5137669106297,5.97796316160799));
#83079=CARTESIAN_POINT('Ctrl Pts',(-6.47992160891878,26.3471349659057,5.99228408951247));
#83080=CARTESIAN_POINT('Ctrl Pts',(-6.45205055567041,26.1799098039722,5.99963304183077));
#83081=CARTESIAN_POINT('Ctrl Pts',(-6.42417950242203,26.0126852567424,5.99998659034014));
#83082=CARTESIAN_POINT('Ctrl Pts',(-6.39630255305344,25.8454253331661,6.00034021364268));
#83083=CARTESIAN_POINT('Ctrl Pts',(-6.36842560368486,25.6781663424463,5.99369547670465));
#83084=CARTESIAN_POINT('Ctrl Pts',(-6.34054865431628,25.5115019531542,5.98008107455308));
#83085=CARTESIAN_POINT('Ctrl Pts',(-6.33031226741014,25.4503029621989,5.97508188019804));
#83086=CARTESIAN_POINT('Ctrl Pts',(-6.32007588050399,25.3891841152585,5.96914343670092));
#83087=CARTESIAN_POINT('Ctrl Pts',(-6.30983949359785,25.3281746568008,5.96226892283763));
#83088=CARTESIAN_POINT('Ctrl Pts',(-6.28185310161256,25.1613741406751,5.9434739279385));
#83089=CARTESIAN_POINT('Ctrl Pts',(-6.25386670962727,24.995339043989,5.91767231717653));
#83090=CARTESIAN_POINT('Ctrl Pts',(-6.22588031764197,24.8306617702719,5.88495098573441));
#83091=CARTESIAN_POINT('Ctrl Pts',(-6.19789886854471,24.6660135814516,5.85223543345373));
#83092=CARTESIAN_POINT('Ctrl Pts',(-6.16991741944744,24.5027230435007,5.81260266048362));
#83093=CARTESIAN_POINT('Ctrl Pts',(-6.14193597035018,24.3413727800146,5.76619074824303));
#83094=CARTESIAN_POINT('Ctrl Pts',(-6.11395507996023,24.1800257382191,5.71977976271195));
#83095=CARTESIAN_POINT('Ctrl Pts',(-6.08597418957029,24.0206191947924,5.66658999169828));
#83096=CARTESIAN_POINT('Ctrl Pts',(-6.05799329918034,23.863721702701,5.60680970218266));
#83097=CARTESIAN_POINT('Ctrl Pts',(-6.03001453781447,23.706836148705,5.54703396125978));
#83098=CARTESIAN_POINT('Ctrl Pts',(-6.00203577644859,23.5524595563791,5.48066881599614));
#83099=CARTESIAN_POINT('Ctrl Pts',(-5.97405701508271,23.4011418616442,5.40795121804017));
#83100=CARTESIAN_POINT('Ctrl Pts',(-5.94607549652134,23.2498092551532,5.33522645405453));
#83101=CARTESIAN_POINT('Ctrl Pts',(-5.91809397795996,23.1015364303583,5.25614812199193));
#83102=CARTESIAN_POINT('Ctrl Pts',(-5.89011245939859,22.9568506906527,5.17100012386571));
#83103=CARTESIAN_POINT('Ctrl Pts',(-5.8804218206274,22.9067427154278,5.14151142795663));
#83104=CARTESIAN_POINT('Ctrl Pts',(-5.87073118185622,22.8570647534989,5.11129514189335));
#83105=CARTESIAN_POINT('Ctrl Pts',(-5.86104054308503,22.8078379774101,5.08036431976434));
#83106=CARTESIAN_POINT('Ctrl Pts',(-5.83308821337882,22.6658449562999,4.99114537778861));
#83107=CARTESIAN_POINT('Ctrl Pts',(-5.8051358836726,22.5275804084579,4.89596087443907));
#83108=CARTESIAN_POINT('Ctrl Pts',(-5.77718355396639,22.3935383858232,4.79514698684719));
#83109=CARTESIAN_POINT('Ctrl Pts',(-5.74923416624616,22.2595104711272,4.69434370992882));
#83110=CARTESIAN_POINT('Ctrl Pts',(-5.72128477852594,22.1297044453186,4.5879124202907));
#83111=CARTESIAN_POINT('Ctrl Pts',(-5.69333539080571,22.004583184726,4.47623105661738));
#83112=CARTESIAN_POINT('Ctrl Pts',(-5.66538333752667,21.8794499912037,4.36453904178971));
#83113=CARTESIAN_POINT('Ctrl Pts',(-5.63743128424762,21.7590026916137,4.2475961597402));
#83114=CARTESIAN_POINT('Ctrl Pts',(-5.60947923096859,21.6436696069346,4.12581937394926));
#83115=CARTESIAN_POINT('Ctrl Pts',(-5.5815273625192,21.528337284882,4.00404339339295));
#83116=CARTESIAN_POINT('Ctrl Pts',(-5.55357549406982,21.4181193239461,3.87743380304682));
#83117=CARTESIAN_POINT('Ctrl Pts',(-5.52562362562044,21.3134059826887,3.74644318212646));
#83118=CARTESIAN_POINT('Ctrl Pts',(-5.49766596098341,21.2086709277424,3.6154253985776));
#83119=CARTESIAN_POINT('Ctrl Pts',(-5.46970829634638,21.1094429684166,3.48002501533422));
#83120=CARTESIAN_POINT('Ctrl Pts',(-5.44175063170935,21.0160714821414,3.34072694617136));
#83121=CARTESIAN_POINT('Ctrl Pts',(-5.4319142853303,20.9832205880179,3.29171770037032));
#83122=CARTESIAN_POINT('Ctrl Pts',(-5.42207793895126,20.9510942486745,3.24222625381832));
#83123=CARTESIAN_POINT('Ctrl Pts',(-5.4122415925722,20.9197064041771,3.19227457782702));
#83124=CARTESIAN_POINT('Ctrl Pts',(-5.38431534913912,20.8305935819466,3.05045742236428));
#83125=CARTESIAN_POINT('Ctrl Pts',(-5.35638910570604,20.7474079569722,2.90488308404311));
#83126=CARTESIAN_POINT('Ctrl Pts',(-5.32846286227296,20.6704504265211,2.75606628073979));
#83127=CARTESIAN_POINT('Ctrl Pts',(-5.30054208319254,20.5935079544178,2.60727859655151));
#83128=CARTESIAN_POINT('Ctrl Pts',(-5.27262130411212,20.5227912898402,2.45524999358071));
#83129=CARTESIAN_POINT('Ctrl Pts',(-5.2447005250317,20.4585552514206,2.30051952794176));
#83130=CARTESIAN_POINT('Ctrl Pts',(-5.21678052781217,20.3943210117919,2.14579339519407));
#83131=CARTESIAN_POINT('Ctrl Pts',(-5.18886053059263,20.3365671599187,1.98836584097777));
#83132=CARTESIAN_POINT('Ctrl Pts',(-5.1609405333731,20.2855005264566,1.82879626171768));
#83133=CARTESIAN_POINT('Ctrl Pts',(-5.13302264012483,20.2344377412302,1.66923870716541));
#83134=CARTESIAN_POINT('Ctrl Pts',(-5.10510474687656,20.1900612627682,1.50753975087095));
#83135=CARTESIAN_POINT('Ctrl Pts',(-5.07718685362829,20.1525282592692,1.34427461530531));
#83136=CARTESIAN_POINT('Ctrl Pts',(-5.04926572100557,20.1149909007333,1.18099053572748));
#83137=CARTESIAN_POINT('Ctrl Pts',(-5.02134458838285,20.0842986743378,1.01614022132391));
#83138=CARTESIAN_POINT('Ctrl Pts',(-4.99342345576012,20.0605579321982,0.85031048636718));
#83139=CARTESIAN_POINT('Ctrl Pts',(-4.98342985119321,20.0520605838895,0.790956275383463));
#83140=CARTESIAN_POINT('Ctrl Pts',(-4.97343624662629,20.0444533022396,0.731476675806575));
#83141=CARTESIAN_POINT('Ctrl Pts',(-4.96344264205937,20.0377393583589,0.67189883251683));
#83142=CARTESIAN_POINT('Ctrl Pts',(-4.93544641569036,20.0189308202128,0.504996612587124));
#83143=CARTESIAN_POINT('Ctrl Pts',(-4.90745018932134,20.0071330673888,0.337289066390713));
#83144=CARTESIAN_POINT('Ctrl Pts',(-4.87945396295232,20.0023911032032,0.169373909041591));
#83145=CARTESIAN_POINT('Ctrl Pts',(-4.85146053479445,19.997649612975,0.00147553474236162));
#83146=CARTESIAN_POINT('Ctrl Pts',(-4.82346710663657,19.9999625122051,-0.166630097560031));
#83147=CARTESIAN_POINT('Ctrl Pts',(-4.79547367847869,20.0093227149932,-0.334343635955789));
#83148=CARTESIAN_POINT('Ctrl Pts',(-4.76747777806289,20.0186837444339,-0.502071986082449));
#83149=CARTESIAN_POINT('Ctrl Pts',(-4.73948187764708,20.0350933060655,-0.669407861490774));
#83150=CARTESIAN_POINT('Ctrl Pts',(-4.71148597723127,20.0584922596335,-0.835754611811684));
#83151=CARTESIAN_POINT('Ctrl Pts',(-4.68349048736598,20.0818908700636,-1.00209892271317));
#83152=CARTESIAN_POINT('Ctrl Pts',(-4.65549499750069,20.1122786214671,-1.16745382898266));
#83153=CARTESIAN_POINT('Ctrl Pts',(-4.6274995076354,20.1495447954169,-1.33123022019737));
#83154=CARTESIAN_POINT('Ctrl Pts',(-4.59949888080676,20.1868178074314,-1.49503666315689));
#83155=CARTESIAN_POINT('Ctrl Pts',(-4.57149825397813,20.2309716937099,-1.65726370832291));
#83156=CARTESIAN_POINT('Ctrl Pts',(-4.5434976271495,20.2818449635609,-1.81733403072898));
#83157=CARTESIAN_POINT('Ctrl Pts',(-4.53387964861519,20.2993195015557,-1.87231683287499));
#83158=CARTESIAN_POINT('Ctrl Pts',(-4.52426167008086,20.3175864012626,-1.92704529676114));
#83159=CARTESIAN_POINT('Ctrl Pts',(-4.51464369154655,20.3366377648732,-1.98149645312302));
#83160=CARTESIAN_POINT('Ctrl Pts',(-4.48671174395061,20.3919655749844,-2.13963018575835));
#83161=CARTESIAN_POINT('Ctrl Pts',(-4.45877979635468,20.4539299931781,-2.29547185730847));
#83162=CARTESIAN_POINT('Ctrl Pts',(-4.43084784875875,20.5223162427038,-2.44846495891884));
#83163=CARTESIAN_POINT('Ctrl Pts',(-4.40292155618005,20.5906886469572,-2.60142708601074));
#83164=CARTESIAN_POINT('Ctrl Pts',(-4.37499526360135,20.6654801595467,-2.7515415064063));
#83165=CARTESIAN_POINT('Ctrl Pts',(-4.34706897102266,20.7464282390894,-2.89827254635629));
#83166=CARTESIAN_POINT('Ctrl Pts',(-4.31914380742579,20.8273730461278,-3.04499765438114));
#83167=CARTESIAN_POINT('Ctrl Pts',(-4.29121864382891,20.914473773728,-3.18833937760928));
#83168=CARTESIAN_POINT('Ctrl Pts',(-4.26329348023204,21.0074220522362,-3.3277868674996));
#83169=CARTESIAN_POINT('Ctrl Pts',(-4.23537064029043,21.1003625965102,-3.4672227539523));
#83170=CARTESIAN_POINT('Ctrl Pts',(-4.20744780034882,21.1991495440843,-3.60276479269939));
#83171=CARTESIAN_POINT('Ctrl Pts',(-4.17952496040721,21.3034311739776,-3.73393107360522));
#83172=CARTESIAN_POINT('Ctrl Pts',(-4.15159925266601,21.4077235140571,-3.86511082587024));
#83173=CARTESIAN_POINT('Ctrl Pts',(-4.12367354492482,21.5175114678987,-3.99191367560493));
#83174=CARTESIAN_POINT('Ctrl Pts',(-4.09574783718362,21.6324025551485,-4.11389019782085));
#83175=CARTESIAN_POINT('Ctrl Pts',(-4.08578013846699,21.6734113544078,-4.15742804600068));
#83176=CARTESIAN_POINT('Ctrl Pts',(-4.07581243975035,21.7150699487486,-4.20035132298714));
#83177=CARTESIAN_POINT('Ctrl Pts',(-4.06584474103372,21.7573593128807,-4.24264068711927));
#83178=CARTESIAN_POINT('Ctrl Pts',(-4.06584464821331,21.7573593128807,-4.24264068711927));
#83179=CARTESIAN_POINT('Ctrl Pts',(-4.03771516188517,21.8767026160842,-4.36198399032277));
#83180=CARTESIAN_POINT('Ctrl Pts',(-4.00958567555705,22.0010901908825,-4.47629422602707));
#83181=CARTESIAN_POINT('Ctrl Pts',(-3.98145618922891,22.1300774906703,-4.58516082289194));
#83182=CARTESIAN_POINT('Ctrl Pts',(-3.95332846351848,22.2590567171744,-4.69402060582301));
#83183=CARTESIAN_POINT('Ctrl Pts',(-3.92520073780805,22.3926348602974,-4.79743723369757));
#83184=CARTESIAN_POINT('Ctrl Pts',(-3.89707301209762,22.5303337208148,-4.89503992946789));
#83185=CARTESIAN_POINT('Ctrl Pts',(-3.86894262111681,22.6680456291235,-4.99265187367786));
#83186=CARTESIAN_POINT('Ctrl Pts',(-3.84081223013601,22.8098787870859,-5.08444860681414));
#83187=CARTESIAN_POINT('Ctrl Pts',(-3.8126818391552,22.9553247265007,-5.17010178612975));
#83188=CARTESIAN_POINT('Ctrl Pts',(-3.78455214045757,23.1007670865208,-5.25575285753813));
#83189=CARTESIAN_POINT('Ctrl Pts',(-3.75642244175993,23.2498217860661,-5.33526052436333));
#83190=CARTESIAN_POINT('Ctrl Pts',(-3.7282927430623,23.4019541134999,-5.40834148067964));
#83191=CARTESIAN_POINT('Ctrl Pts',(-3.70015938579756,23.5541062273644,-5.48143194195318));
#83192=CARTESIAN_POINT('Ctrl Pts',(-3.67202602853282,23.7093364934794,-5.54809389086397));
#83193=CARTESIAN_POINT('Ctrl Pts',(-3.64389267126808,23.8670877576044,-5.60809106258438));
#83194=CARTESIAN_POINT('Ctrl Pts',(-3.63494368007888,23.9172671464152,-5.62717567292969));
#83195=CARTESIAN_POINT('Ctrl Pts',(-3.62599468888967,23.9677014644956,-5.64558629009007));
#83196=CARTESIAN_POINT('Ctrl Pts',(-3.61704569770047,24.0183723790421,-5.66331634043665));
#83197=CARTESIAN_POINT('Ctrl Pts',(-3.58917226838873,24.1761971131281,-5.71854014103948));
#83198=CARTESIAN_POINT('Ctrl Pts',(-3.56129883907699,24.3363538428541,-5.76717021039578));
#83199=CARTESIAN_POINT('Ctrl Pts',(-3.53342540976525,24.4982753557587,-5.80902944500011));
#83200=CARTESIAN_POINT('Ctrl Pts',(-3.50555603581229,24.6601733103914,-5.85088258942398));
#83201=CARTESIAN_POINT('Ctrl Pts',(-3.47768666185932,24.8238352281641,-5.88596678558931));
#83202=CARTESIAN_POINT('Ctrl Pts',(-3.44981728790635,24.9886805465176,-5.91415530426856));
#83203=CARTESIAN_POINT('Ctrl Pts',(-3.42194618026319,25.1535361195224,-5.94234557649128));
#83204=CARTESIAN_POINT('Ctrl Pts',(-3.39407507262003,25.3195749273882,-5.96363925759899));
#83205=CARTESIAN_POINT('Ctrl Pts',(-3.36620396497687,25.4862073472971,-5.97796094918898));
#83206=CARTESIAN_POINT('Ctrl Pts',(-3.33833338825653,25.6528365929886,-5.99228236796194));
#83207=CARTESIAN_POINT('Ctrl Pts',(-3.31046281153618,25.8200591112097,-5.99963203804457));
#83208=CARTESIAN_POINT('Ctrl Pts',(-3.28259223481584,25.9872810886311,-5.99998651909265));
#83209=CARTESIAN_POINT('Ctrl Pts',(-3.25471577267068,26.1545383782883,-6.00034107499643));
#83210=CARTESIAN_POINT('Ctrl Pts',(-3.22683931052552,26.3217948090041,-5.99369749083168));
#83211=CARTESIAN_POINT('Ctrl Pts',(-3.19896284838036,26.4884567296998,-5.98008444950495));
#83212=CARTESIAN_POINT('Ctrl Pts',(-3.18872414798279,26.5496697152214,-5.9750845377185));
#83213=CARTESIAN_POINT('Ctrl Pts',(-3.17848544758522,26.6108025300056,-5.96914494737047));
#83214=CARTESIAN_POINT('Ctrl Pts',(-3.16824674718765,26.6718259090464,-5.96226885907822));
#83215=CARTESIAN_POINT('Ctrl Pts',(-3.14026030146104,26.838627106392,-5.94347377138838));
#83216=CARTESIAN_POINT('Ctrl Pts',(-3.11227385573443,27.0046628436322,-5.91767201436493));
#83217=CARTESIAN_POINT('Ctrl Pts',(-3.08428741000782,27.1693407138992,-5.8849504921297));
#83218=CARTESIAN_POINT('Ctrl Pts',(-3.05630589929474,27.333989545555,-5.8522347398717));
#83219=CARTESIAN_POINT('Ctrl Pts',(-3.02832438858165,27.4972806815948,-5.81260171851936));
#83220=CARTESIAN_POINT('Ctrl Pts',(-3.00034287786857,27.6586314959111,-5.76618951828429));
#83221=CARTESIAN_POINT('Ctrl Pts',(-2.97236191520299,27.8199791500009,-5.7197782270813));
#83222=CARTESIAN_POINT('Ctrl Pts',(-2.94438095253741,27.9793862569935,-5.66658810562624));
#83223=CARTESIAN_POINT('Ctrl Pts',(-2.91639998987183,28.1362842619755,-5.6068074295481));
#83224=CARTESIAN_POINT('Ctrl Pts',(-2.88842115033735,28.2931703618977,-5.54703128949018));
#83225=CARTESIAN_POINT('Ctrl Pts',(-2.86044231080287,28.447547448432,-5.48066570620433));
#83226=CARTESIAN_POINT('Ctrl Pts',(-2.83246347126839,28.5988655844751,-5.4079476397087));
#83227=CARTESIAN_POINT('Ctrl Pts',(-2.80448186676361,28.7501986743246,-5.33522238695025));
#83228=CARTESIAN_POINT('Ctrl Pts',(-2.77650026225883,28.8984719278766,-5.25614353206902));
#83229=CARTESIAN_POINT('Ctrl Pts',(-2.74851865775405,29.0431580411126,-5.1709949851853));
#83230=CARTESIAN_POINT('Ctrl Pts',(-2.73882837072764,29.0932641730091,-5.14150726016784));
#83231=CARTESIAN_POINT('Ctrl Pts',(-2.72913808370123,29.1429403188547,-5.1112919991724));
#83232=CARTESIAN_POINT('Ctrl Pts',(-2.71944779667482,29.1921653085973,-5.08036225505503));
#83233=CARTESIAN_POINT('Ctrl Pts',(-2.69135596545285,29.3348669747074,-4.99069791909505));
#83234=CARTESIAN_POINT('Ctrl Pts',(-2.66326413423087,29.4738017201919,-4.89500908884372));
#83235=CARTESIAN_POINT('Ctrl Pts',(-2.6351723030089,29.6084706716364,-4.79363530235036));
#83236=CARTESIAN_POINT('Ctrl Pts',(-2.60708243574623,29.7431302080898,-4.69226860311273));
#83237=CARTESIAN_POINT('Ctrl Pts',(-2.57899256848356,29.8735242993192,-4.5852179242781));
#83238=CARTESIAN_POINT('Ctrl Pts',(-2.55090270122089,29.9991851541301,-4.47286464170168));
#83239=CARTESIAN_POINT('Ctrl Pts',(-2.5322845748429,30.0824738950045,-4.39839623662062));
#83240=CARTESIAN_POINT('Ctrl Pts',(-2.51366644846492,30.1636839143914,-4.32159919483766));
#83241=CARTESIAN_POINT('Ctrl Pts',(-2.49504832208693,30.2426872863434,-4.24259408738332));
#83242=CARTESIAN_POINT('Origin',(-31.4159265358979,26.,7.7715611723761E-15));
#83243=CARTESIAN_POINT('',(5.63664190388931,30.2426838347204,-4.24259753907934));
#83244=CARTESIAN_POINT('',(3.78813707791307,30.2426869010466,-4.2425944726886));
#83245=CARTESIAN_POINT('',(-31.4159265358979,30.2426406871193,-4.24264068711928));
#83246=CARTESIAN_POINT('',(4.06584552699229,21.7573593180495,-4.24264068195053));
#83247=CARTESIAN_POINT('Ctrl Pts',(5.63664190388088,30.2426838346846,-4.24259753911516));
#83248=CARTESIAN_POINT('Ctrl Pts',(5.6085541904248,30.1234976659262,-4.36178613215216));
#83249=CARTESIAN_POINT('Ctrl Pts',(5.58046647696872,29.9992876476353,-4.47594753544482));
#83250=CARTESIAN_POINT('Ctrl Pts',(5.55237876351264,29.8704989412251,-4.58467424644055));
#83251=CARTESIAN_POINT('Ctrl Pts',(5.52428659397689,29.7416898026521,-4.69341820678932));
#83252=CARTESIAN_POINT('Ctrl Pts',(5.49619442444114,29.6083007588941,-4.79672555322897));
#83253=CARTESIAN_POINT('Ctrl Pts',(5.4681022549054,29.4708105808102,-4.894228633006));
#83254=CARTESIAN_POINT('Ctrl Pts',(5.4494823125889,29.3796798768698,-4.9588552443049));
#83255=CARTESIAN_POINT('Ctrl Pts',(5.43086237027242,29.2867481229324,-5.02093272423811));
#83256=CARTESIAN_POINT('Ctrl Pts',(5.41224242795593,29.1921620225893,-5.08036431976472));
#83257=CARTESIAN_POINT('Ctrl Pts',(5.38426093251302,29.0500208445595,-5.16967635366504));
#83258=CARTESIAN_POINT('Ctrl Pts',(5.35627943707011,28.9041159465853,-5.25302763668842));
#83259=CARTESIAN_POINT('Ctrl Pts',(5.3282979416272,28.7549657670488,-5.33011853736753));
#83260=CARTESIAN_POINT('Ctrl Pts',(5.30031925100227,28.6058305380751,-5.40720171058461));
#83261=CARTESIAN_POINT('Ctrl Pts',(5.27234056037734,28.4534509546491,-5.47802561079631));
#83262=CARTESIAN_POINT('Ctrl Pts',(5.2443618697524,28.2983695338176,-5.54233682538501));
#83263=CARTESIAN_POINT('Ctrl Pts',(5.21638057970836,28.1432737048206,-5.60665401494237));
#83264=CARTESIAN_POINT('Ctrl Pts',(5.18839928966432,27.9854758247472,-5.66445718784532));
#83265=CARTESIAN_POINT('Ctrl Pts',(5.16041799962029,27.8255385637381,-5.71554100259154));
#83266=CARTESIAN_POINT('Ctrl Pts',(5.13243700769939,27.6656030067604,-5.76662427307167));
#83267=CARTESIAN_POINT('Ctrl Pts',(5.10445601577849,27.5035284130956,-5.81098823603987));
#83268=CARTESIAN_POINT('Ctrl Pts',(5.07647502385759,27.3398930292745,-5.84847729499751));
#83269=CARTESIAN_POINT('Ctrl Pts',(5.0484886204334,27.1762259984904,-5.88597360431161));
#83270=CARTESIAN_POINT('Ctrl Pts',(5.02050221700923,27.010997879448,-5.91659228413978));
#83271=CARTESIAN_POINT('Ctrl Pts',(4.99251581358505,26.844798319737,-5.94022859820811));
#83272=CARTESIAN_POINT('Ctrl Pts',(4.98282503487107,26.7872488328984,-5.94841308285869));
#83273=CARTESIAN_POINT('Ctrl Pts',(4.97313425615709,26.7295829452508,-5.95576082645302));
#83274=CARTESIAN_POINT('Ctrl Pts',(4.96344347744311,26.671825343199,-5.96226892283763));
#83275=CARTESIAN_POINT('Ctrl Pts',(4.9355665537412,26.5056772643785,-5.98099040144252));
#83276=CARTESIAN_POINT('Ctrl Pts',(4.90768963003929,26.3387175535921,-5.99276581585045));
#83277=CARTESIAN_POINT('Ctrl Pts',(4.87981270633737,26.1715384837214,-5.99754737777056));
#83278=CARTESIAN_POINT('Ctrl Pts',(4.85194115438949,26.0043916284828,-6.00232801830583));
#83279=CARTESIAN_POINT('Ctrl Pts',(4.8240696024416,25.8370258160442,-6.00011748649615));
#83280=CARTESIAN_POINT('Ctrl Pts',(4.79619805049373,25.670035265695,-5.99092006908079));
#83281=CARTESIAN_POINT('Ctrl Pts',(4.76832671673624,25.5030460226191,-5.98172272366673));
#83282=CARTESIAN_POINT('Ctrl Pts',(4.74045538297876,25.3364323532721,-5.96553861588635));
#83283=CARTESIAN_POINT('Ctrl Pts',(4.71258404922128,25.170785987995,-5.9424240947861));
#83284=CARTESIAN_POINT('Ctrl Pts',(4.68471437664526,25.0051494955382,-5.91931095135276));
#83285=CARTESIAN_POINT('Ctrl Pts',(4.65684470406925,24.8404805065169,-5.88926826528848));
#83286=CARTESIAN_POINT('Ctrl Pts',(4.62897503149323,24.6773634267367,-5.85240399281066));
#83287=CARTESIAN_POINT('Ctrl Pts',(4.60110112330571,24.5142215565475,-5.81553411772893));
#83288=CARTESIAN_POINT('Ctrl Pts',(4.57322721511818,24.3526323768021,-5.77184065528646));
#83289=CARTESIAN_POINT('Ctrl Pts',(4.54535330693066,24.1931686540343,-5.72148236799133));
#83290=CARTESIAN_POINT('Ctrl Pts',(4.53511704693053,24.134608077747,-5.70298906886563));
#83291=CARTESIAN_POINT('Ctrl Pts',(4.52488078693041,24.0763340041334,-5.68359743145589));
#83292=CARTESIAN_POINT('Ctrl Pts',(4.51464452693028,24.0183742706934,-5.66331700233619));
#83293=CARTESIAN_POINT('Ctrl Pts',(4.4865117157702,23.8590807166286,-5.6075793127247));
#83294=CARTESIAN_POINT('Ctrl Pts',(4.45837890461014,23.7021267572523,-5.54511207805169));
#83295=CARTESIAN_POINT('Ctrl Pts',(4.43024609345007,23.5480757211417,-5.47613616802442));
#83296=CARTESIAN_POINT('Ctrl Pts',(4.4021167522165,23.3940436858259,-5.40716876554857));
#83297=CARTESIAN_POINT('Ctrl Pts',(4.37398741098292,23.242914137515,-5.33169441516217));
#83298=CARTESIAN_POINT('Ctrl Pts',(4.34585806974934,23.0952292992012,-5.24998163575655));
#83299=CARTESIAN_POINT('Ctrl Pts',(4.31772857627372,22.9475436615853,-5.16826841410376));
#83300=CARTESIAN_POINT('Ctrl Pts',(4.28959908279809,22.8033030395622,-5.080316841577));
#83301=CARTESIAN_POINT('Ctrl Pts',(4.26146958932246,22.6630246528152,-4.98644116903836));
#83302=CARTESIAN_POINT('Ctrl Pts',(4.23334224738877,22.5227569955479,-4.89257267677286));
#83303=CARTESIAN_POINT('Ctrl Pts',(4.20521490545508,22.3864512211851,-4.79278116046609));
#83304=CARTESIAN_POINT('Ctrl Pts',(4.17708756352139,22.2545955059214,-4.68742415146482));
#83305=CARTESIAN_POINT('Ctrl Pts',(4.1489586600171,22.1227324703069,-4.58206129326496));
#83306=CARTESIAN_POINT('Ctrl Pts',(4.1208297565128,21.9953202260986,-4.47113251538342));
#83307=CARTESIAN_POINT('Ctrl Pts',(4.0927008530085,21.8728144094322,-4.35503606196433));
#83308=CARTESIAN_POINT('Ctrl Pts',(4.08374909414482,21.8338280859864,-4.31808945806355));
#83309=CARTESIAN_POINT('Ctrl Pts',(4.07479733528114,21.795338409257,-4.28061978349561));
#83310=CARTESIAN_POINT('Ctrl Pts',(4.06584557641746,21.7573593128807,-4.24264068711927));
#83311=CARTESIAN_POINT('',(0.924252830007244,30.2426406871193,4.24264068711929));
#83312=CARTESIAN_POINT('Ctrl Pts',(4.06584548359704,21.7573593128807,-4.24264068711927));
#83313=CARTESIAN_POINT('Ctrl Pts',(4.03791880226835,21.6388764384194,-4.12415781265794));
#83314=CARTESIAN_POINT('Ctrl Pts',(4.00999212093965,21.5253476884487,-4.00069641994847));
#83315=CARTESIAN_POINT('Ctrl Pts',(3.98206543961095,21.4171793209539,-3.87269345852562));
#83316=CARTESIAN_POINT('Ctrl Pts',(3.9541416574735,21.3090221828915,-3.74470378565145));
#83317=CARTESIAN_POINT('Ctrl Pts',(3.92621787533605,21.206224519716,-3.61217372590949));
#83318=CARTESIAN_POINT('Ctrl Pts',(3.8982940931986,21.1091529040836,-3.47557400789661));
#83319=CARTESIAN_POINT('Ctrl Pts',(3.87036737455777,21.0120710802665,-3.33895992486932));
#83320=CARTESIAN_POINT('Ctrl Pts',(3.84244065591694,20.9207166917825,-3.19827558389406));
#83321=CARTESIAN_POINT('Ctrl Pts',(3.81451393727611,20.8354139383164,-3.05402207121422));
#83322=CARTESIAN_POINT('Ctrl Pts',(3.7865871902451,20.7501110981319,-2.90976841188688));
#83323=CARTESIAN_POINT('Ctrl Pts',(3.75866044321409,20.6708600628755,-2.76194584652404));
#83324=CARTESIAN_POINT('Ctrl Pts',(3.73073369618308,20.5979399885723,-2.61108169786646));
#83325=CARTESIAN_POINT('Ctrl Pts',(3.70280067048967,20.525003519931,-2.46018363100646));
#83326=CARTESIAN_POINT('Ctrl Pts',(3.67486764479626,20.4584009922193,-2.30624289886807));
#83327=CARTESIAN_POINT('Ctrl Pts',(3.64693461910284,20.3983645016636,-2.14980923427589));
#83328=CARTESIAN_POINT('Ctrl Pts',(3.6369719237633,20.3769516668628,-2.09401503001439));
#83329=CARTESIAN_POINT('Ctrl Pts',(3.62700922842375,20.3563736444569,-2.03790388561375));
#83330=CARTESIAN_POINT('Ctrl Pts',(3.6170465330842,20.336639465377,-1.98150131336679));
#83331=CARTESIAN_POINT('Ctrl Pts',(3.58904611033923,20.2811760252203,-1.82298036968697));
#83332=CARTESIAN_POINT('Ctrl Pts',(3.56104568759426,20.2323648472564,-1.6621079135492));
#83333=CARTESIAN_POINT('Ctrl Pts',(3.53304526484928,20.1903845618598,-1.49945605501576));
#83334=CARTESIAN_POINT('Ctrl Pts',(3.50504956423739,20.1484113562312,-1.33683162691539));
#83335=CARTESIAN_POINT('Ctrl Pts',(3.47705386362551,20.1132668219182,-1.1724286972628));
#83336=CARTESIAN_POINT('Ctrl Pts',(3.44905816301361,20.0850792209348,-1.00683274548563));
#83337=CARTESIAN_POINT('Ctrl Pts',(3.42106282883359,20.0568919888949,-0.841238961171053));
#83338=CARTESIAN_POINT('Ctrl Pts',(3.39306749465355,20.0356615636487,-0.674452492907592));
#83339=CARTESIAN_POINT('Ctrl Pts',(3.36507216047352,20.0214648828223,-0.507067897497593));
#83340=CARTESIAN_POINT('Ctrl Pts',(3.33707888229296,20.0072692446113,-0.339695594944594));
#83341=CARTESIAN_POINT('Ctrl Pts',(3.30908560411241,20.0001063440121,-0.171725563911534));
#83342=CARTESIAN_POINT('Ctrl Pts',(3.28109232593185,20.0000011760623,-0.00375669357035702));
#83343=CARTESIAN_POINT('Ctrl Pts',(3.25309629274952,19.9998959977622,0.164228707687036));
#83344=CARTESIAN_POINT('Ctrl Pts',(3.22510025956719,20.0068499401413,0.332212636062041));
#83345=CARTESIAN_POINT('Ctrl Pts',(3.19710422638486,20.0208358776276,0.499596234708716));
#83346=CARTESIAN_POINT('Ctrl Pts',(3.1874853451137,20.0256411681226,0.557105916585281));
#83347=CARTESIAN_POINT('Ctrl Pts',(3.17786646384254,20.031276114924,0.614544754401049));
#83348=CARTESIAN_POINT('Ctrl Pts',(3.16824758257138,20.0377382015578,0.671888567276623));
#83349=CARTESIAN_POINT('Ctrl Pts',(3.14032641770501,20.0564959948186,0.838343065282123));
#83350=CARTESIAN_POINT('Ctrl Pts',(3.11240525283864,20.0822308275213,1.00403023929455));
#83351=CARTESIAN_POINT('Ctrl Pts',(3.08448408797227,20.1148547894252,1.16836032560507));
#83352=CARTESIAN_POINT('Ctrl Pts',(3.05656615786135,20.1474749717396,1.33267137375424));
#83353=CARTESIAN_POINT('Ctrl Pts',(3.02864822775042,20.1869826286598,1.49562533866357));
#83354=CARTESIAN_POINT('Ctrl Pts',(3.0007302976395,20.2332386904674,1.65664238714261));
#83355=CARTESIAN_POINT('Ctrl Pts',(2.97280985307306,20.2794989183721,1.81767393777864));
#83356=CARTESIAN_POINT('Ctrl Pts',(2.94488940850663,20.3325086810178,1.9767679193988));
#83357=CARTESIAN_POINT('Ctrl Pts',(2.9169689639402,20.392078748676,2.13335867564475));
#83358=CARTESIAN_POINT('Ctrl Pts',(2.88904871462632,20.4516483997502,2.28994833682409));
#83359=CARTESIAN_POINT('Ctrl Pts',(2.86112846531243,20.517778149159,2.44403451376054));
#83360=CARTESIAN_POINT('Ctrl Pts',(2.83320821599856,20.5902301593064,2.59507037876083));
#83361=CARTESIAN_POINT('Ctrl Pts',(2.80528195296983,20.6626977748205,2.7461387752265));
#83362=CARTESIAN_POINT('Ctrl Pts',(2.77735568994111,20.7414902343532,2.89415526299696));
#83363=CARTESIAN_POINT('Ctrl Pts',(2.74942942691238,20.8263228280928,3.0385958140046));
#83364=CARTESIAN_POINT('Ctrl Pts',(2.73943582862777,20.8566807339251,3.09028482235108));
#83365=CARTESIAN_POINT('Ctrl Pts',(2.72944223034316,20.8878117233957,3.14151612715943));
#83366=CARTESIAN_POINT('Ctrl Pts',(2.71944863205855,20.9197013523565,3.19226653817505));
#83367=CARTESIAN_POINT('Ctrl Pts',(2.69149131753093,21.0089133020105,3.33424194710808));
#83368=CARTESIAN_POINT('Ctrl Pts',(2.66353400300332,21.1040942925657,3.47249735556752));
#83369=CARTESIAN_POINT('Ctrl Pts',(2.6355766884757,21.2049100802888,3.60653748932186));
#83370=CARTESIAN_POINT('Ctrl Pts',(2.60762463203012,21.3057069070462,3.74055241342958));
#83371=CARTESIAN_POINT('Ctrl Pts',(2.57967257558453,21.4121362273927,3.87035339407639));
#83372=CARTESIAN_POINT('Ctrl Pts',(2.55172051913895,21.5238218980808,3.99547614182584));
#83373=CARTESIAN_POINT('Ctrl Pts',(2.52376921738104,21.6355045533272,4.120595511341));
#83374=CARTESIAN_POINT('Ctrl Pts',(2.49581791562314,21.7524430687688,4.24103666382374));
#83375=CARTESIAN_POINT('Ctrl Pts',(2.46786661386523,21.8742221707881,4.35636973912725));
#83376=CARTESIAN_POINT('Ctrl Pts',(2.43991747800799,21.995991836344,4.47169387745935));
#83377=CARTESIAN_POINT('Ctrl Pts',(2.41196834215075,22.122601110396,4.58191051421212));
#83378=CARTESIAN_POINT('Ctrl Pts',(2.38401920629351,22.2535989196033,4.68662767294378));
#83379=CARTESIAN_POINT('Ctrl Pts',(2.35606714794483,22.3846104265499,4.79135578138786));
#83380=CARTESIAN_POINT('Ctrl Pts',(2.32811508959615,22.5200111402011,4.89058306673688));
#83381=CARTESIAN_POINT('Ctrl Pts',(2.30016303124748,22.6593174977051,4.98395830829879));
#83382=CARTESIAN_POINT('Ctrl Pts',(2.29032524801356,22.7083466508048,5.01682191263311));
#83383=CARTESIAN_POINT('Ctrl Pts',(2.28048746477965,22.7578593220079,5.04896100631227));
#83384=CARTESIAN_POINT('Ctrl Pts',(2.27064968154573,22.8078335665496,5.0803615482712));
#83385=CARTESIAN_POINT('Ctrl Pts',(2.24266806215881,22.9499753739736,5.1696741497736));
#83386=CARTESIAN_POINT('Ctrl Pts',(2.2146864427719,23.0958809689459,5.25302596012788));
#83387=CARTESIAN_POINT('Ctrl Pts',(2.18670482338498,23.2450319119771,5.33011733773052));
#83388=CARTESIAN_POINT('Ctrl Pts',(2.15872601735941,23.3941678588963,5.40720096431996));
#83389=CARTESIAN_POINT('Ctrl Pts',(2.13074721133383,23.5465482247839,5.47802527131766));
#83390=CARTESIAN_POINT('Ctrl Pts',(2.10276840530826,23.7016304907273,5.54233683556363));
#83391=CARTESIAN_POINT('Ctrl Pts',(2.07478701386981,23.8567270872209,5.60665434259165));
#83392=CARTESIAN_POINT('Ctrl Pts',(2.04680562243137,24.0145257947562,5.66445778234574));
#83393=CARTESIAN_POINT('Ctrl Pts',(2.01882423099292,24.1744639407621,5.71554180252599));
#83394=CARTESIAN_POINT('Ctrl Pts',(1.99084314620162,24.3344003340109,5.76662526287813));
#83395=CARTESIAN_POINT('Ctrl Pts',(1.96286206141032,24.4964758201881,5.81098935838593));
#83396=CARTESIAN_POINT('Ctrl Pts',(1.93488097661903,24.6601121493087,5.84847848141463));
#83397=CARTESIAN_POINT('Ctrl Pts',(1.90689449378863,24.8237800467303,5.88597483674879));
#83398=CARTESIAN_POINT('Ctrl Pts',(1.87890801095822,24.9890090837231,5.91659350071802));
#83399=CARTESIAN_POINT('Ctrl Pts',(1.85092152812782,25.155209608394,5.94022972571351));
#83400=CARTESIAN_POINT('Ctrl Pts',(1.84123126242951,25.2127562194855,5.94841372302747));
#83401=CARTESIAN_POINT('Ctrl Pts',(1.83154099673121,25.2704192240213,5.95576106384894));
#83402=CARTESIAN_POINT('Ctrl Pts',(1.8218507310329,25.3281739395001,5.96226884201251));
#83403=CARTESIAN_POINT('Ctrl Pts',(1.79397447623059,25.4943185236473,5.98098994708153));
#83404=CARTESIAN_POINT('Ctrl Pts',(1.76609822142828,25.6612746781566,5.99276527668448));
#83405=CARTESIAN_POINT('Ctrl Pts',(1.73822196662597,25.8284501539608,5.99754705278116));
#83406=CARTESIAN_POINT('Ctrl Pts',(1.71035107197587,25.9955934846291,6.00232790941977));
#83407=CARTESIAN_POINT('Ctrl Pts',(1.68248017732578,26.1629557348742,6.00011788683632));
#83408=CARTESIAN_POINT('Ctrl Pts',(1.65460928267568,26.3299427101814,5.99092128207325));
#83409=CARTESIAN_POINT('Ctrl Pts',(1.62673858385612,26.4969285121805,5.98172474192871));
#83410=CARTESIAN_POINT('Ctrl Pts',(1.59886788503655,26.6635387269724,5.96554173164701));
#83411=CARTESIAN_POINT('Ctrl Pts',(1.57099718621698,26.8291816496961,5.94242861057728));
#83412=CARTESIAN_POINT('Ctrl Pts',(1.54312813425875,26.994814784688,5.91931685524672));
#83413=CARTESIAN_POINT('Ctrl Pts',(1.51525908230051,27.1594804272277,5.88927585270319));
#83414=CARTESIAN_POINT('Ctrl Pts',(1.48739003034228,27.3225941986181,5.85241356927054));
#83415=CARTESIAN_POINT('Ctrl Pts',(1.45951671757968,27.485732907917,5.81554565008901));
#83416=CARTESIAN_POINT('Ctrl Pts',(1.43164340481709,27.6473189620354,5.77185443681084));
#83417=CARTESIAN_POINT('Ctrl Pts',(1.40377009205449,27.8067796228967,5.72149870176385));
#83418=CARTESIAN_POINT('Ctrl Pts',(1.39353065487635,27.8653585020267,5.70300020501307));
#83419=CARTESIAN_POINT('Ctrl Pts',(1.38329121769821,27.9236506969668,5.68360281467011));
#83420=CARTESIAN_POINT('Ctrl Pts',(1.37305178052007,27.9816283440733,5.66331608741429));
#83421=CARTESIAN_POINT('Ctrl Pts',(1.34491819503623,28.1409260732985,5.60757685433833));
#83422=CARTESIAN_POINT('Ctrl Pts',(1.3167846095524,28.2978840579134,5.54510773076915));
#83423=CARTESIAN_POINT('Ctrl Pts',(1.28865102406856,28.4519389419314,5.47612960265192));
#83424=CARTESIAN_POINT('Ctrl Pts',(1.26052090720747,28.605974832342,5.40715997892899));
#83425=CARTESIAN_POINT('Ctrl Pts',(1.23239079034638,28.7571080582065,5.33168307752366));
#83426=CARTESIAN_POINT('Ctrl Pts',(1.20426067348529,28.9047963694786,5.24996743340983));
#83427=CARTESIAN_POINT('Ctrl Pts',(1.17613041007705,29.0524854501504,5.16825136358875));
#83428=CARTESIAN_POINT('Ctrl Pts',(1.1480001466688,29.19672931206,5.08029663171104));
#83429=CARTESIAN_POINT('Ctrl Pts',(1.11986988326057,29.3370107087109,4.9864175045767));
#83430=CARTESIAN_POINT('Ctrl Pts',(1.0917417770414,29.4772813477841,4.89254557662939));
#83431=CARTESIAN_POINT('Ctrl Pts',(1.06361367082224,29.6135898756071,4.79275033176959));
#83432=CARTESIAN_POINT('Ctrl Pts',(1.03548556460307,29.7454480889377,4.68738931742103));
#83433=CARTESIAN_POINT('Ctrl Pts',(1.00735591092944,29.8773135563857,4.58202250668605));
#83434=CARTESIAN_POINT('Ctrl Pts',(0.979226257255812,30.0047279815099,4.47108950501795));
#83435=CARTESIAN_POINT('Ctrl Pts',(0.951096603582176,30.1272357008951,4.35498857280439));
#83436=CARTESIAN_POINT('Ctrl Pts',(0.942148679057198,30.1662048911846,4.3180573545683));
#83437=CARTESIAN_POINT('Ctrl Pts',(0.933200754532215,30.2046778584644,4.28060351577423));
#83438=CARTESIAN_POINT('Ctrl Pts',(0.924252830007237,30.2426406871193,4.24264068711928));
#83439=CARTESIAN_POINT('Ctrl Pts',(0.924252830007237,30.2426406871193,4.24264068711928));
#83440=CARTESIAN_POINT('Ctrl Pts',(0.89632614867855,30.3611235615806,4.12415781265799));
#83441=CARTESIAN_POINT('Ctrl Pts',(0.868399467349873,30.4746523115512,4.00069641994855));
#83442=CARTESIAN_POINT('Ctrl Pts',(0.840472786021184,30.582820679046,3.87269345852573));
#83443=CARTESIAN_POINT('Ctrl Pts',(0.812549003883679,30.6909778171086,3.74470378565134));
#83444=CARTESIAN_POINT('Ctrl Pts',(0.784625221746176,30.7937754802843,3.61217372590913));
#83445=CARTESIAN_POINT('Ctrl Pts',(0.756701439608673,30.8908470959168,3.475574007896));
#83446=CARTESIAN_POINT('Ctrl Pts',(0.728774720967817,30.987928919734,3.33895992486855));
#83447=CARTESIAN_POINT('Ctrl Pts',(0.70084800232696,31.0792833082181,3.19827558389312));
#83448=CARTESIAN_POINT('Ctrl Pts',(0.672921283686104,31.1645860616843,3.05402207121311));
#83449=CARTESIAN_POINT('Ctrl Pts',(0.644994536655131,31.2498889018687,2.90976841188593));
#83450=CARTESIAN_POINT('Ctrl Pts',(0.617067789624155,31.3291399371249,2.76194584652326));
#83451=CARTESIAN_POINT('Ctrl Pts',(0.58914104259318,31.402060011428,2.61108169786585));
#83452=CARTESIAN_POINT('Ctrl Pts',(0.561208016899777,31.4749964800692,2.46018363100591));
#83453=CARTESIAN_POINT('Ctrl Pts',(0.533274991206372,31.5415990077809,2.30624289886759));
#83454=CARTESIAN_POINT('Ctrl Pts',(0.505341965512969,31.6016354983365,2.14980923427548));
#83455=CARTESIAN_POINT('Ctrl Pts',(0.49537927017345,31.6230483331373,2.09401503001411));
#83456=CARTESIAN_POINT('Ctrl Pts',(0.485416574833935,31.6436263555431,2.03790388561361));
#83457=CARTESIAN_POINT('Ctrl Pts',(0.475453879494417,31.663360534623,1.98150131336679));
#83458=CARTESIAN_POINT('Ctrl Pts',(0.447453456749435,31.7188239747797,1.82298036968693));
#83459=CARTESIAN_POINT('Ctrl Pts',(0.419453034004449,31.7676351527436,1.66210791354913));
#83460=CARTESIAN_POINT('Ctrl Pts',(0.391452611259467,31.8096154381402,1.49945605501565));
#83461=CARTESIAN_POINT('Ctrl Pts',(0.363456910647587,31.8515886437689,1.33683162691534));
#83462=CARTESIAN_POINT('Ctrl Pts',(0.335461210035708,31.8867331780818,1.17242869726283));
#83463=CARTESIAN_POINT('Ctrl Pts',(0.307465509423828,31.9149207790652,1.00683274548574));
#83464=CARTESIAN_POINT('Ctrl Pts',(0.279470175243799,31.9431080111051,0.841238961171152));
#83465=CARTESIAN_POINT('Ctrl Pts',(0.251474841063771,31.9643384363513,0.674452492907679));
#83466=CARTESIAN_POINT('Ctrl Pts',(0.223479506883741,31.9785351171777,0.50706789749767));
#83467=CARTESIAN_POINT('Ctrl Pts',(0.195486228703238,31.9927307553886,0.339695594944983));
#83468=CARTESIAN_POINT('Ctrl Pts',(0.167492950522737,31.9998936559878,0.171725563912239));
#83469=CARTESIAN_POINT('Ctrl Pts',(0.139499672342232,31.9999988239377,0.00375669357137531));
#83470=CARTESIAN_POINT('Ctrl Pts',(0.111503639159925,32.0001040022378,-0.164228707685864));
#83471=CARTESIAN_POINT('Ctrl Pts',(0.0835076059776147,31.9931500598587,
-0.332212636060722));
#83472=CARTESIAN_POINT('Ctrl Pts',(0.0555115727953073,31.9791641223725,
-0.499596234707248));
#83473=CARTESIAN_POINT('Ctrl Pts',(0.045892691524066,31.9743588318775,-0.557105916584305));
#83474=CARTESIAN_POINT('Ctrl Pts',(0.0362738102528267,31.9687238850761,
-0.614544754400563));
#83475=CARTESIAN_POINT('Ctrl Pts',(0.0266549289815856,31.9622617984422,
-0.671888567276625));
#83476=CARTESIAN_POINT('Ctrl Pts',(-0.00126623588478278,31.9435040051814,
-0.838343065282101));
#83477=CARTESIAN_POINT('Ctrl Pts',(-0.0291874007511589,31.9177691724787,
-1.0040302392945));
#83478=CARTESIAN_POINT('Ctrl Pts',(-0.0571085656175256,31.8851452105749,
-1.168360325605));
#83479=CARTESIAN_POINT('Ctrl Pts',(-0.0850264957284651,31.8525250282604,
-1.33267137375427));
#83480=CARTESIAN_POINT('Ctrl Pts',(-0.112944425839412,31.8130173713401,
-1.4956253386637));
#83481=CARTESIAN_POINT('Ctrl Pts',(-0.14086235595035,31.7667613095326,-1.65664238714284));
#83482=CARTESIAN_POINT('Ctrl Pts',(-0.168782800516778,31.7205010816279,
-1.81767393777883));
#83483=CARTESIAN_POINT('Ctrl Pts',(-0.196703245083203,31.6674913189821,
-1.97676791939895));
#83484=CARTESIAN_POINT('Ctrl Pts',(-0.224623689649633,31.607921251324,-2.13335867564485));
#83485=CARTESIAN_POINT('Ctrl Pts',(-0.252543938963529,31.5483516002497,
-2.2899483368243));
#83486=CARTESIAN_POINT('Ctrl Pts',(-0.280464188277424,31.4822218508408,
-2.44403451376085));
#83487=CARTESIAN_POINT('Ctrl Pts',(-0.308384437591322,31.4097698406934,
-2.59507037876124));
#83488=CARTESIAN_POINT('Ctrl Pts',(-0.336310700620064,31.3373022251793,
-2.746138775227));
#83489=CARTESIAN_POINT('Ctrl Pts',(-0.364236963648801,31.2585097656465,
-2.89415526299755));
#83490=CARTESIAN_POINT('Ctrl Pts',(-0.392163226677543,31.1736771719068,
-3.03859581400527));
#83491=CARTESIAN_POINT('Ctrl Pts',(-0.402156824962108,31.1433192660746,
-3.09028482235153));
#83492=CARTESIAN_POINT('Ctrl Pts',(-0.412150423246673,31.1121882766042,
-3.14151612715966));
#83493=CARTESIAN_POINT('Ctrl Pts',(-0.422144021531238,31.0802986476434,
-3.19226653817506));
#83494=CARTESIAN_POINT('Ctrl Pts',(-0.450530238418072,30.989718068122,-3.33642003856181));
#83495=CARTESIAN_POINT('Ctrl Pts',(-0.478916455304906,30.8929892453202,
-3.47673026481364));
#83496=CARTESIAN_POINT('Ctrl Pts',(-0.507302672191738,30.7904579669258,
-3.61268770683503));
#83497=CARTESIAN_POINT('Ctrl Pts',(-0.535682769382887,30.6879487929289,
-3.74861583821688));
#83498=CARTESIAN_POINT('Ctrl Pts',(-0.564062866574028,30.5796398364838,
-3.88019282519102));
#83499=CARTESIAN_POINT('Ctrl Pts',(-0.592442963765176,30.4659187273337,
-4.00694021927577));
#83500=CARTESIAN_POINT('Ctrl Pts',(-0.610476474549829,30.3936571408251,
-4.08747907306331));
#83501=CARTESIAN_POINT('Ctrl Pts',(-0.628509985334481,30.3192111329926,
-4.16606851660056));
#83502=CARTESIAN_POINT('Ctrl Pts',(-0.646543496119133,30.2426884810913,
-4.24259289260889));
#83503=CARTESIAN_POINT('',(-0.924251994623517,30.2426406871193,4.24264068711929));
#83504=CARTESIAN_POINT('Ctrl Pts',(-2.49504832207809,30.2426872863809,-4.24259408734582));
#83505=CARTESIAN_POINT('Ctrl Pts',(-2.46667006335947,30.3631063921147,-4.12217233630957));
#83506=CARTESIAN_POINT('Ctrl Pts',(-2.43829180464085,30.4783810719969,-3.99663506167176));
#83507=CARTESIAN_POINT('Ctrl Pts',(-2.40991354592223,30.5880984395498,-3.86643928039754));
#83508=CARTESIAN_POINT('Ctrl Pts',(-2.38152675269319,30.6978488036309,-3.73620434389315));
#83509=CARTESIAN_POINT('Ctrl Pts',(-2.35313995946415,30.8020383276375,-3.60130832543165));
#83510=CARTESIAN_POINT('Ctrl Pts',(-2.32475316623511,30.9002941637225,-3.46224163064734));
#83511=CARTESIAN_POINT('Ctrl Pts',(-2.30671839287741,30.962718324161,-3.37388940636458));
#83512=CARTESIAN_POINT('Ctrl Pts',(-2.2886836195197,31.022748262084,-3.28385440346218));
#83513=CARTESIAN_POINT('Ctrl Pts',(-2.270648846162,31.0802973280948,-3.19226863815583));
#83514=CARTESIAN_POINT('Ctrl Pts',(-2.24272260406513,31.1694101280169,-3.05045115013736));
#83515=CARTESIAN_POINT('Ctrl Pts',(-2.21479636196826,31.2525956824996,-2.90487651342687));
#83516=CARTESIAN_POINT('Ctrl Pts',(-2.18687011987139,31.3295531040625,-2.75605945345486));
#83517=CARTESIAN_POINT('Ctrl Pts',(-2.15894933075943,31.4064954986247,-2.60727145207154));
#83518=CARTESIAN_POINT('Ctrl Pts',(-2.13102854164748,31.477212042224,-2.45524257097675));
#83519=CARTESIAN_POINT('Ctrl Pts',(-2.10310775253553,31.541447926615,-2.30051187273918));
#83520=CARTESIAN_POINT('Ctrl Pts',(-2.07518772874498,31.6056820502715,-2.14578541573972));
#83521=CARTESIAN_POINT('Ctrl Pts',(-2.04726770495442,31.6634357454588,-1.98835757959765));
#83522=CARTESIAN_POINT('Ctrl Pts',(-2.01934768116386,31.7145021922793,-1.82878776637276));
#83523=CARTESIAN_POINT('Ctrl Pts',(-1.99142975184323,31.7655648082602,-1.66922992355936));
#83524=CARTESIAN_POINT('Ctrl Pts',(-1.96351182252259,31.8099410829883,-1.50753072550295));
#83525=CARTESIAN_POINT('Ctrl Pts',(-1.93559389320195,31.8474738594471,-1.34426539904996));
#83526=CARTESIAN_POINT('Ctrl Pts',(-1.90767271091177,31.8850110091879,-1.18098104908242));
#83527=CARTESIAN_POINT('Ctrl Pts',(-1.8797515286216,31.9157029968264,-1.01613051365243));
#83528=CARTESIAN_POINT('Ctrl Pts',(-1.85183034633142,31.9394434816715,-0.850300610390311));
#83529=CARTESIAN_POINT('Ctrl Pts',(-1.84183686277067,31.9479406198857,-0.790947163429956));
#83530=CARTESIAN_POINT('Ctrl Pts',(-1.83184337920992,31.9555477137923,-0.731468338095572));
#83531=CARTESIAN_POINT('Ctrl Pts',(-1.82184989564917,31.9622614929435,-0.671891278231294));
#83532=CARTESIAN_POINT('Ctrl Pts',(-1.79385381433342,31.9810696999027,-0.504990096839036));
#83533=CARTESIAN_POINT('Ctrl Pts',(-1.76585773301767,31.9928672096575,-0.337283608813402));
#83534=CARTESIAN_POINT('Ctrl Pts',(-1.73786165170193,31.9976090206897,-0.169369521879895));
#83535=CARTESIAN_POINT('Ctrl Pts',(-1.70986836725733,32.0023503580043,-0.00147220993925742));
#83536=CARTESIAN_POINT('Ctrl Pts',(-1.68187508281275,32.0000373950918,0.166632347773044));
#83537=CARTESIAN_POINT('Ctrl Pts',(-1.65388179836815,31.9906772196565,0.334344806882151));
#83538=CARTESIAN_POINT('Ctrl Pts',(-1.62588603799567,31.9813162163397,0.50207209969018));
#83539=CARTESIAN_POINT('Ctrl Pts',(-1.59789027762319,31.9649067700317,0.669406912970671));
#83540=CARTESIAN_POINT('Ctrl Pts',(-1.56989451725071,31.9415080227897,0.83575260401952));
#83541=CARTESIAN_POINT('Ctrl Pts',(-1.54189916480914,31.9181096164948,1.00209587121748));
#83542=CARTESIAN_POINT('Ctrl Pts',(-1.51390381236757,31.8877221589244,1.16744973644604));
#83543=CARTESIAN_POINT('Ctrl Pts',(-1.485908459926,31.8504563702668,1.33122509727129));
#83544=CARTESIAN_POINT('Ctrl Pts',(-1.45790796537159,31.8131837367269,1.49503053992486));
#83545=CARTESIAN_POINT('Ctrl Pts',(-1.42990747081718,31.7690303178787,1.6572565948491));
#83546=CARTESIAN_POINT('Ctrl Pts',(-1.40190697626278,31.7181576061116,1.81732594535721));
#83547=CARTESIAN_POINT('Ctrl Pts',(-1.39228829922063,31.7006819081808,1.87231266653428));
#83548=CARTESIAN_POINT('Ctrl Pts',(-1.38266962217848,31.6824137366426,1.92704501227138));
#83549=CARTESIAN_POINT('Ctrl Pts',(-1.37305094513634,31.6633609912275,1.98150000833774));
#83550=CARTESIAN_POINT('Ctrl Pts',(-1.34511823087734,31.608031667746,2.13963774790754));
#83551=CARTESIAN_POINT('Ctrl Pts',(-1.31718551661833,31.5460654028897,2.29548329282442));
#83552=CARTESIAN_POINT('Ctrl Pts',(-1.28925280235933,31.4776769861386,2.4484801072354));
#83553=CARTESIAN_POINT('Ctrl Pts',(-1.26132574550914,31.4093024205739,2.60144593412696));
#83554=CARTESIAN_POINT('Ctrl Pts',(-1.23339868865894,31.3345084272542,2.75156389430813));
#83555=CARTESIAN_POINT('Ctrl Pts',(-1.20547163180875,31.253557560246,2.89829828713029));
#83556=CARTESIAN_POINT('Ctrl Pts',(-1.17754571388895,31.1726099946025,3.04502669578233));
#83557=CARTESIAN_POINT('Ctrl Pts',(-1.14961979596914,31.0855062060404,3.18837153517099));
#83558=CARTESIAN_POINT('Ctrl Pts',(-1.12169387804934,30.9925545768458,3.32782192991391));
#83559=CARTESIAN_POINT('Ctrl Pts',(-1.09377029132843,30.8996107070644,3.46726068362119));
#83560=CARTESIAN_POINT('Ctrl Pts',(-1.06584670460752,30.8008201474129,3.60280538045999));
#83561=CARTESIAN_POINT('Ctrl Pts',(-1.03792311788661,30.6965346318148,3.73397408295295));
#83562=CARTESIAN_POINT('Ctrl Pts',(-1.00999667958778,30.5922384665005,3.86515618049359));
#83563=CARTESIAN_POINT('Ctrl Pts',(-0.98207024128895,30.4824464201251,3.99196114407935));
#83564=CARTESIAN_POINT('Ctrl Pts',(-0.954143802990121,30.3675509863158,
4.11393952093755));
#83565=CARTESIAN_POINT('Ctrl Pts',(-0.944179866867919,30.3265571885763,
4.15746045770362));
#83566=CARTESIAN_POINT('Ctrl Pts',(-0.934215930745716,30.2849140879152,
4.20036728632337));
#83567=CARTESIAN_POINT('Ctrl Pts',(-0.924251994623514,30.2426406871193,
4.24264068711928));
#83568=CARTESIAN_POINT('',(2.21734070236153,21.7573593077119,-4.24264069228803));
#83569=CARTESIAN_POINT('Ctrl Pts',(-0.924251994623514,30.2426406871193,
4.24264068711928));
#83570=CARTESIAN_POINT('Ctrl Pts',(-0.896122308120024,30.1232965346437,
4.3619848395949));
#83571=CARTESIAN_POINT('Ctrl Pts',(-0.867992621616533,29.998908050666,4.47629584114187));
#83572=CARTESIAN_POINT('Ctrl Pts',(-0.839862935113043,29.8699197905936,
4.58516311753156));
#83573=CARTESIAN_POINT('Ctrl Pts',(-0.811735005997595,29.7409395889981,
4.69402359249282));
#83574=CARTESIAN_POINT('Ctrl Pts',(-0.783607076882148,29.6073604186198,
4.79744082484517));
#83575=CARTESIAN_POINT('Ctrl Pts',(-0.7554791477667,29.4696604872218,4.89504403487973));
#83576=CARTESIAN_POINT('Ctrl Pts',(-0.727348550661214,29.3319474947114,
4.99265650277294));
#83577=CARTESIAN_POINT('Ctrl Pts',(-0.699217953555737,29.1901132081159,
5.08445366825331));
#83578=CARTESIAN_POINT('Ctrl Pts',(-0.671087356450254,29.0446661039873,
5.17010718604854));
#83579=CARTESIAN_POINT('Ctrl Pts',(-0.642957450664213,28.8992225742731,
5.25575859887807));
#83580=CARTESIAN_POINT('Ctrl Pts',(-0.614827544878162,28.7501666686984,
5.33526651284798));
#83581=CARTESIAN_POINT('Ctrl Pts',(-0.586697639092119,28.5980331070789,
5.40834761960824));
#83582=CARTESIAN_POINT('Ctrl Pts',(-0.55856407496633,28.4458797602437,5.48143823068464));
#83583=CARTESIAN_POINT('Ctrl Pts',(-0.530430510840543,28.2906482330414,
5.54810023279348));
#83584=CARTESIAN_POINT('Ctrl Pts',(-0.502296946714754,28.132895687777,5.60809735873605));
#83585=CARTESIAN_POINT('Ctrl Pts',(-0.493348979180065,28.0827220003185,
5.62717963116725));
#83586=CARTESIAN_POINT('Ctrl Pts',(-0.484401011645379,28.0322934436315,
5.64558806450506));
#83587=CARTESIAN_POINT('Ctrl Pts',(-0.47545304411069,27.9816283440737,5.66331608741415));
#83588=CARTESIAN_POINT('Ctrl Pts',(-0.447579776163769,27.8238045824141,
5.71853957037812));
#83589=CARTESIAN_POINT('Ctrl Pts',(-0.419706508216854,27.6636488268566,
5.76716941207883));
#83590=CARTESIAN_POINT('Ctrl Pts',(-0.391833240269932,27.501728281285,5.80902850476642));
#83591=CARTESIAN_POINT('Ctrl Pts',(-0.363964033260086,27.3398313263864,
5.85088149888166));
#83592=CARTESIAN_POINT('Ctrl Pts',(-0.336094826250237,27.1761704022288,
5.88596563316397));
#83593=CARTESIAN_POINT('Ctrl Pts',(-0.308225619240392,27.0113260634304,
5.9141541739649));
#83594=CARTESIAN_POINT('Ctrl Pts',(-0.280354685379861,26.8464715104353,
5.9423444614033));
#83595=CARTESIAN_POINT('Ctrl Pts',(-0.252483751519326,26.6804337091038,
5.96363824511411));
#83596=CARTESIAN_POINT('Ctrl Pts',(-0.224612817658794,26.5138022747661,
5.97796012218593));
#83597=CARTESIAN_POINT('Ctrl Pts',(-0.196742418305686,26.3471740360781,
5.99228172459349));
#83598=CARTESIAN_POINT('Ctrl Pts',(-0.168872018952584,26.1799525040583,
5.99963166297465));
#83599=CARTESIAN_POINT('Ctrl Pts',(-0.141001619599475,26.0127314851022,
5.9999864924254));
#83600=CARTESIAN_POINT('Ctrl Pts',(-0.113125338855247,25.84547517809,6.00034139675454));
#83601=CARTESIAN_POINT('Ctrl Pts',(-0.0852490581110152,25.6782197022789,
5.99369824315483));
#83602=CARTESIAN_POINT('Ctrl Pts',(-0.0573727773667869,25.5115587022245,
5.98008570997336));
#83603=CARTESIAN_POINT('Ctrl Pts',(-0.0471332161104769,25.4503405097852,
5.97508553191359));
#83604=CARTESIAN_POINT('Ctrl Pts',(-0.0368936548541687,25.3892024979934,
5.9691455154932));
#83605=CARTESIAN_POINT('Ctrl Pts',(-0.026654093597859,25.3281739395,5.9622688420125));
#83606=CARTESIAN_POINT('Ctrl Pts',(0.00133237775107972,25.16137245641,5.94347371783423));
#83607=CARTESIAN_POINT('Ctrl Pts',(0.0293188491000237,24.9953364493688,
5.91767190179122));
#83608=CARTESIAN_POINT('Ctrl Pts',(0.0573053204489611,24.830658326687,5.88495030149394));
#83609=CARTESIAN_POINT('Ctrl Pts',(0.0852868598251298,24.6660092247418,
5.85223446762714));
#83610=CARTESIAN_POINT('Ctrl Pts',(0.113268399201294,24.5027178360857,5.81260134412805));
#83611=CARTESIAN_POINT('Ctrl Pts',(0.141249938577463,24.3413667879488,5.76618902464018));
#83612=CARTESIAN_POINT('Ctrl Pts',(0.169230933987283,24.1800188765065,5.71977760741647));
#83613=CARTESIAN_POINT('Ctrl Pts',(0.197211929397112,24.0206115315198,5.66658734086016));
#83614=CARTESIAN_POINT('Ctrl Pts',(0.225192924806933,23.8637133088066,5.60680650397623));
#83615=CARTESIAN_POINT('Ctrl Pts',(0.253171799331124,23.7068269785648,5.54703019832201));
#83616=CARTESIAN_POINT('Ctrl Pts',(0.281150673855311,23.5524496823706,5.4806644326814));
#83617=CARTESIAN_POINT('Ctrl Pts',(0.309129548379502,23.4011313579394,5.40794617034175));
#83618=CARTESIAN_POINT('Ctrl Pts',(0.337111190803452,23.2497980638583,5.33522071411514));
#83619=CARTESIAN_POINT('Ctrl Pts',(0.365092833227402,23.1015246279873,5.25614164094682));
#83620=CARTESIAN_POINT('Ctrl Pts',(0.393074475651353,22.9568383547437,5.17099286412591));
#83621=CARTESIAN_POINT('Ctrl Pts',(0.402764602739227,22.9067330623395,5.14150558613592));
#83622=CARTESIAN_POINT('Ctrl Pts',(0.412454729827095,22.8570577432985,5.11129079675859));
#83623=CARTESIAN_POINT('Ctrl Pts',(0.422144856914969,22.807833566549,5.08036154827086));
#83624=CARTESIAN_POINT('Ctrl Pts',(0.45009688294762,22.6658420882681,4.99114340375536));
#83625=CARTESIAN_POINT('Ctrl Pts',(0.478048908980264,22.5275789742579,4.89595980073667));
#83626=CARTESIAN_POINT('Ctrl Pts',(0.506000935012917,22.3935382722901,4.79514690145816));
#83627=CARTESIAN_POINT('Ctrl Pts',(0.533950009814166,22.2595117226105,4.69434464620932));
#83628=CARTESIAN_POINT('Ctrl Pts',(0.561899084615418,22.1297069458922,4.58791446993937));
#83629=CARTESIAN_POINT('Ctrl Pts',(0.589848159416665,22.0045868150917,4.47623429702482));
#83630=CARTESIAN_POINT('Ctrl Pts',(0.617799888666578,21.8794548010727,4.36454351734464));
#83631=CARTESIAN_POINT('Ctrl Pts',(0.645751617916485,21.7590085579661,4.24760195201275));
#83632=CARTESIAN_POINT('Ctrl Pts',(0.673703347166398,21.6436764038817,4.12582655063237));
#83633=CARTESIAN_POINT('Ctrl Pts',(0.701654885842154,21.5283450361289,4.00405197951348));
#83634=CARTESIAN_POINT('Ctrl Pts',(0.729606424517915,21.4181279015186,3.87744386828778));
#83635=CARTESIAN_POINT('Ctrl Pts',(0.757557963193673,21.3134152563028,3.74645478287737));
#83636=CARTESIAN_POINT('Ctrl Pts',(0.785515291843235,21.2086809205647,3.61543856395628));
#83637=CARTESIAN_POINT('Ctrl Pts',(0.813472620492793,21.1094535477017,3.48003980368646));
#83638=CARTESIAN_POINT('Ctrl Pts',(0.841429949142356,21.0160825131925,3.34074340300097));
#83639=CARTESIAN_POINT('Ctrl Pts',(0.851267901904173,20.9832260182699,3.29172615149555));
#83640=CARTESIAN_POINT('Ctrl Pts',(0.86110585466598,20.9510943155683,3.24222653576395));
#83641=CARTESIAN_POINT('Ctrl Pts',(0.870943807427796,20.9197013523558,3.19226653817392));
#83642=CARTESIAN_POINT('Ctrl Pts',(0.898870053403839,20.8305885426266,3.05044890442022));
#83643=CARTESIAN_POINT('Ctrl Pts',(0.926796299379875,20.7474029982992,2.90487413347756));
#83644=CARTESIAN_POINT('Ctrl Pts',(0.954722545355917,20.6704456032832,2.75605695377225));
#83645=CARTESIAN_POINT('Ctrl Pts',(0.982643342595285,20.5935032235535,2.6072688100364));
#83646=CARTESIAN_POINT('Ctrl Pts',(1.01056413983465,20.5227867130616,2.45523980009785));
#83647=CARTESIAN_POINT('Ctrl Pts',(1.03848493707402,20.4585508762575,2.30050898910937));
#83648=CARTESIAN_POINT('Ctrl Pts',(1.06640497513163,20.3943167860609,2.14578238533637));
#83649=CARTESIAN_POINT('Ctrl Pts',(1.09432501318922,20.3365631416576,1.98835441732583));
#83650=CARTESIAN_POINT('Ctrl Pts',(1.12224505124682,20.285496759011,1.82878448941532));
#83651=CARTESIAN_POINT('Ctrl Pts',(1.15016299834979,20.2344342007678,1.6692265118281));
#83652=CARTESIAN_POINT('Ctrl Pts',(1.17808094545276,20.190057998844,1.50752719563975));
#83653=CARTESIAN_POINT('Ctrl Pts',(1.20599889255573,20.1525253061649,1.34426176950714));
#83654=CARTESIAN_POINT('Ctrl Pts',(1.23392009762376,20.1149882335004,1.18097729064647));
#83655=CARTESIAN_POINT('Ctrl Pts',(1.26184130269178,20.0842963363596,1.01612664422016));
#83656=CARTESIAN_POINT('Ctrl Pts',(1.28976250775981,20.0605559512525,0.850296649292306));
#83657=CARTESIAN_POINT('Ctrl Pts',(1.29975592448675,20.0520589124945,0.790943614883419));
#83658=CARTESIAN_POINT('Ctrl Pts',(1.30974934121368,20.0444519058687,0.73146520645205));
#83659=CARTESIAN_POINT('Ctrl Pts',(1.31974275794062,20.0377382015577,0.671888567275174));
#83660=CARTESIAN_POINT('Ctrl Pts',(1.34773877292647,20.0189301230358,0.504987843651186));
#83661=CARTESIAN_POINT('Ctrl Pts',(1.37573478791231,20.007132702851,0.337281820351));
#83662=CARTESIAN_POINT('Ctrl Pts',(1.40373080289816,20.0023909420332,0.169368201840285));
#83663=CARTESIAN_POINT('Ctrl Pts',(1.43172402135423,19.9976496548712,0.00147135626790321));
#83664=CARTESIAN_POINT('Ctrl Pts',(1.45971723981031,19.9999626287568,-0.166632731380683));
#83665=CARTESIAN_POINT('Ctrl Pts',(1.48771045826638,20.009322775496,-0.334344720024882));
#83666=CARTESIAN_POINT('Ctrl Pts',(1.51570615389444,20.0186837505319,-0.502071549814969));
#83667=CARTESIAN_POINT('Ctrl Pts',(1.5437018495225,20.0350931295111,-0.669405899637445));
#83668=CARTESIAN_POINT('Ctrl Pts',(1.57169754515055,20.0584917698864,-0.835751130117129));
#83669=CARTESIAN_POINT('Ctrl Pts',(1.59969283378329,20.0818900700973,-1.0020939423061));
#83670=CARTESIAN_POINT('Ctrl Pts',(1.627688122416,20.1122773825116,-1.16744735534482));
#83671=CARTESIAN_POINT('Ctrl Pts',(1.65568341104874,20.1495429864649,-1.33122227023831));
#83672=CARTESIAN_POINT('Ctrl Pts',(1.68368384374439,20.186815437878,-1.49502727835492));
#83673=CARTESIAN_POINT('Ctrl Pts',(1.71168427644005,20.2309686359984,-1.65725290477794));
#83674=CARTESIAN_POINT('Ctrl Pts',(1.7396847091357,20.2818410879826,-1.81732183636135));
#83675=CARTESIAN_POINT('Ctrl Pts',(1.74930370890828,20.2993173216317,-1.87231038004687));
#83676=CARTESIAN_POINT('Ctrl Pts',(1.75892270868087,20.3175860809654,-1.92704453122915));
#83677=CARTESIAN_POINT('Ctrl Pts',(1.76854170845345,20.3366394653772,-1.98150131336752));
#83678=CARTESIAN_POINT('Ctrl Pts',(1.79647472012914,20.3919693771996,-2.13964061758363));
#83679=CARTESIAN_POINT('Ctrl Pts',(1.82440773180482,20.4539363601836,-2.29548767417718));
#83680=CARTESIAN_POINT('Ctrl Pts',(1.85234074348051,20.5223256196587,-2.4484859368501));
#83681=CARTESIAN_POINT('Ctrl Pts',(1.88026809706484,20.5907010262531,-2.60145320830169));
#83682=CARTESIAN_POINT('Ctrl Pts',(1.90819545064917,20.6654959848677,-2.75157254979298));
#83683=CARTESIAN_POINT('Ctrl Pts',(1.9361228042335,20.7464479362731,-2.89830825029203));
#83684=CARTESIAN_POINT('Ctrl Pts',(1.96404901537803,20.827396576132,-3.04503794819205));
#83685=CARTESIAN_POINT('Ctrl Pts',(1.99197522652255,20.9145015564675,-3.18838400406016));
#83686=CARTESIAN_POINT('Ctrl Pts',(2.01990143766708,21.0074544898585,-3.3278355321689));
#83687=CARTESIAN_POINT('Ctrl Pts',(2.04782531488487,21.1003996547292,-3.46727540564799));
#83688=CARTESIAN_POINT('Ctrl Pts',(2.07574919210266,21.1991916207523,-3.60282113992212));
#83689=CARTESIAN_POINT('Ctrl Pts',(2.10367306932045,21.3034786487632,-3.73399078699681));
#83690=CARTESIAN_POINT('Ctrl Pts',(2.131599792102,21.407776304073,-3.86517380082534));
#83691=CARTESIAN_POINT('Ctrl Pts',(2.15952651488354,21.5175699441395,-3.99197958972882));
#83692=CARTESIAN_POINT('Ctrl Pts',(2.18745323766509,21.6324670699787,-4.11395869026166));
#83693=CARTESIAN_POINT('Ctrl Pts',(2.19741571143215,21.6734550373473,-4.15747305457479));
#83694=CARTESIAN_POINT('Ctrl Pts',(2.20737818519921,21.7150921163322,-4.20037349057077));
#83695=CARTESIAN_POINT('Ctrl Pts',(2.21734065896628,21.7573593128807,-4.24264068711927));
#83696=CARTESIAN_POINT('Ctrl Pts',(2.2173407517867,21.7573593128807,-4.24264068711927));
#83697=CARTESIAN_POINT('Ctrl Pts',(2.24547017450468,21.8767023462092,-4.36198372044778));
#83698=CARTESIAN_POINT('Ctrl Pts',(2.27359959722266,22.0010896320607,-4.47629371275351));
#83699=CARTESIAN_POINT('Ctrl Pts',(2.30172901994065,22.1300766266187,-4.58516009362348));
#83700=CARTESIAN_POINT('Ctrl Pts',(2.3298566810282,22.25905554325,-4.69401965663829));
#83701=CARTESIAN_POINT('Ctrl Pts',(2.35798434211575,22.3926333598853,-4.79743609238731));
#83702=CARTESIAN_POINT('Ctrl Pts',(2.3861120032033,22.5303318800058,-4.89503862467868));
#83703=CARTESIAN_POINT('Ctrl Pts',(2.41424232871702,22.6680434437826,-4.99265040248606));
#83704=CARTESIAN_POINT('Ctrl Pts',(2.44237265423074,22.8098762430537,-5.08444699821573));
#83705=CARTESIAN_POINT('Ctrl Pts',(2.47050297974446,22.955321812265,-5.17010006993391));
#83706=CARTESIAN_POINT('Ctrl Pts',(2.4986326126804,23.100763800559,-5.25575103284557));
#83707=CARTESIAN_POINT('Ctrl Pts',(2.52676224561635,23.2498181167879,-5.33525862110907));
#83708=CARTESIAN_POINT('Ctrl Pts',(2.55489187855229,23.4019500519087,-5.40833952958048));
#83709=CARTESIAN_POINT('Ctrl Pts',(2.58302517014452,23.5541017739375,-5.48142994325679));
#83710=CARTESIAN_POINT('Ctrl Pts',(2.61115846173675,23.7093316392366,-5.54809187524892));
#83711=CARTESIAN_POINT('Ctrl Pts',(2.63929175332897,23.8670824961232,-5.60808906149463));
#83712=CARTESIAN_POINT('Ctrl Pts',(2.64824106965249,23.9172636956446,-5.62717441439312));
#83713=CARTESIAN_POINT('Ctrl Pts',(2.657190385976,23.9676998435017,-5.64558572516249));
#83714=CARTESIAN_POINT('Ctrl Pts',(2.66613970229952,24.018372604843,-5.66331641944571));
#83715=CARTESIAN_POINT('Ctrl Pts',(2.69401318247694,24.1761976450724,-5.71854032010687));
#83716=CARTESIAN_POINT('Ctrl Pts',(2.72188666265437,24.3363546815082,-5.76717046119709));
#83717=CARTESIAN_POINT('Ctrl Pts',(2.74976014283179,24.4982764989898,-5.80902974054304));
#83718=CARTESIAN_POINT('Ctrl Pts',(2.77762956940271,24.6601747683773,-5.85088293234464));
#83719=CARTESIAN_POINT('Ctrl Pts',(2.80549899597363,24.8238369989971,-5.88596714805142));
#83720=CARTESIAN_POINT('Ctrl Pts',(2.83336842254456,24.9886826257904,-5.91415565982344));
#83721=CARTESIAN_POINT('Ctrl Pts',(2.86123958495308,25.1535385199364,-5.94234592730716));
#83722=CARTESIAN_POINT('Ctrl Pts',(2.88911074736159,25.3195776447197,-5.9636395761651));
#83723=CARTESIAN_POINT('Ctrl Pts',(2.91698190977011,25.4862103749654,-5.97796120940967));
#83724=CARTESIAN_POINT('Ctrl Pts',(2.94485254238088,25.6528399377204,-5.99228257041697));
#83725=CARTESIAN_POINT('Ctrl Pts',(2.97272317499164,25.8200627664747,-5.99963215607798));
#83726=CARTESIAN_POINT('Ctrl Pts',(3.00059380760241,25.987285045716,-5.99998652747966));
#83727=CARTESIAN_POINT('Ctrl Pts',(3.02847032690278,26.1545426447746,-6.00034097372983));
#83728=CARTESIAN_POINT('Ctrl Pts',(3.05634684620316,26.3217993761771,-5.99369725404841));
#83729=CARTESIAN_POINT('Ctrl Pts',(3.08422336550353,26.4884615867904,-5.98008405277301));
#83730=CARTESIAN_POINT('Ctrl Pts',(3.09446179460647,26.5496729313316,-5.97508422497456));
#83731=CARTESIAN_POINT('Ctrl Pts',(3.10470022370941,26.6108041082623,-5.96914476897286));
#83732=CARTESIAN_POINT('Ctrl Pts',(3.11493865281235,26.6718258549855,-5.96226886516978));
#83733=CARTESIAN_POINT('Ctrl Pts',(3.14292509107457,26.8386269657956,-5.94347378876235));
#83734=CARTESIAN_POINT('Ctrl Pts',(3.17091152933679,27.0046626214334,-5.91767204983508));
#83735=CARTESIAN_POINT('Ctrl Pts',(3.19889796759901,27.1693404154645,-5.88495055142872));
#83736=CARTESIAN_POINT('Ctrl Pts',(3.2268794699022,27.3339891653265,-5.85223482410241));
#83737=CARTESIAN_POINT('Ctrl Pts',(3.2548609722054,27.4972802250278,-5.81260183387949));
#83738=CARTESIAN_POINT('Ctrl Pts',(3.28284247450859,27.6586309687947,-5.76618966990811));
#83739=CARTESIAN_POINT('Ctrl Pts',(3.31082342749156,27.8199785449967,-5.71977841707938));
#83740=CARTESIAN_POINT('Ctrl Pts',(3.33880438047452,27.9793855800658,-5.66658833974861));
#83741=CARTESIAN_POINT('Ctrl Pts',(3.36678533345749,28.1362835193544,-5.60680771249868));
#83742=CARTESIAN_POINT('Ctrl Pts',(3.39476416260806,28.2931695496517,-5.54703162276515));
#83743=CARTESIAN_POINT('Ctrl Pts',(3.42274299175863,28.4475465729151,-5.48066609483681));
#83744=CARTESIAN_POINT('Ctrl Pts',(3.4507218209092,28.5988646522158,-5.40794808771897));
#83745=CARTESIAN_POINT('Ctrl Pts',(3.47870341411161,28.7501976803556,-5.33522289672862));
#83746=CARTESIAN_POINT('Ctrl Pts',(3.50668500731404,28.8984708789272,-5.25614410805264));
#83747=CARTESIAN_POINT('Ctrl Pts',(3.53466660051646,29.0431569440202,-5.17099563082988));
#83748=CARTESIAN_POINT('Ctrl Pts',(3.54435693478603,29.0932633237662,-5.14150777426415));
#83749=CARTESIAN_POINT('Ctrl Pts',(3.5540472690556,29.1429397137401,-5.11129237445318));
#83750=CARTESIAN_POINT('Ctrl Pts',(3.56373760332517,29.1921649435568,-5.08036248442241));
#83751=CARTESIAN_POINT('Ctrl Pts',(3.59182937948356,29.3348663302056,-4.99069833835923));
#83752=CARTESIAN_POINT('Ctrl Pts',(3.61992115564195,29.4738008104779,-4.89500972265669));
#83753=CARTESIAN_POINT('Ctrl Pts',(3.64801293180034,29.6084695131929,-4.79363617438342));
#83754=CARTESIAN_POINT('Ctrl Pts',(3.67610274521235,29.7431288067304,-4.69226970898605));
#83755=CARTESIAN_POINT('Ctrl Pts',(3.70419255862436,29.8735226711554,-4.58521928717258));
#83756=CARTESIAN_POINT('Ctrl Pts',(3.73228237203637,29.999183317532,-4.47286628380213));
#83757=CARTESIAN_POINT('Ctrl Pts',(3.7509006073286,30.0824725671577,-4.39839748538549));
#83758=CARTESIAN_POINT('Ctrl Pts',(3.76951884262084,30.1636830710683,-4.32160002382929));
#83759=CARTESIAN_POINT('Ctrl Pts',(3.78813707791307,30.2426869010466,-4.2425944726886));
#83760=CARTESIAN_POINT('Origin',(-31.4159265358979,26.,7.7715611723761E-15));
#83761=CARTESIAN_POINT('',(11.9198273038894,30.2426793568795,-4.24260201700658));
#83762=CARTESIAN_POINT('',(10.0713224779131,30.2426823068249,-4.24259906700534));
#83763=CARTESIAN_POINT('',(-31.4159265358979,30.2426406871193,-4.24264068711928));
#83764=CARTESIAN_POINT('',(10.3490309269923,21.7573593180495,-4.24264068195052));
#83765=CARTESIAN_POINT('Ctrl Pts',(11.9198273038809,30.2426793568436,-4.24260201704246));
#83766=CARTESIAN_POINT('Ctrl Pts',(11.8917400717272,30.123495274846,-4.36178827168631));
#83767=CARTESIAN_POINT('Ctrl Pts',(11.8636528395734,29.999287505876,-4.47594754696579));
#83768=CARTESIAN_POINT('Ctrl Pts',(11.8355656074197,29.8705011892402,-4.58467234860792));
#83769=CARTESIAN_POINT('Ctrl Pts',(11.8074739290482,29.7416944856895,-4.69341436142083));
#83770=CARTESIAN_POINT('Ctrl Pts',(11.7793822506767,29.608308020656,-4.7967199828174));
#83771=CARTESIAN_POINT('Ctrl Pts',(11.7512905723051,29.470820543405,-4.89422156787753));
#83772=CARTESIAN_POINT('Ctrl Pts',(11.7326696575221,29.379685276805,-4.95885169366101));
#83773=CARTESIAN_POINT('Ctrl Pts',(11.714048742739,29.2867487626982,-5.02093243374107));
#83774=CARTESIAN_POINT('Ctrl Pts',(11.6954278279559,29.1921577294537,-5.08036701728221));
#83775=CARTESIAN_POINT('Ctrl Pts',(11.6674463996327,29.0500169029914,-5.16967866274384));
#83776=CARTESIAN_POINT('Ctrl Pts',(11.6394649713094,28.9041124055508,-5.25302957654197));
#83777=CARTESIAN_POINT('Ctrl Pts',(11.6114835429862,28.7549626758259,-5.3301201351195));
#83778=CARTESIAN_POINT('Ctrl Pts',(11.5835049124322,28.6058278590825,-5.40720298567047));
#83779=CARTESIAN_POINT('Ctrl Pts',(11.5555262818782,28.4534487355297,-5.47802658718929));
#83780=CARTESIAN_POINT('Ctrl Pts',(11.5275476513242,28.2983678218862,-5.54233753531108));
#83781=CARTESIAN_POINT('Ctrl Pts',(11.4995664100833,28.1432724376382,-5.60665448428929));
#83782=CARTESIAN_POINT('Ctrl Pts',(11.4715851688425,27.9854750474674,-5.66445744360215));
#83783=CARTESIAN_POINT('Ctrl Pts',(11.4436039276017,27.8255383207092,-5.71554108021472));
#83784=CARTESIAN_POINT('Ctrl Pts',(11.4156229776983,27.6656032591937,-5.76662418495037));
#83785=CARTESIAN_POINT('Ctrl Pts',(11.3876420277949,27.5035292043085,-5.8109880143795));
#83786=CARTESIAN_POINT('Ctrl Pts',(11.3596610778915,27.3398944009461,-5.84847698074578));
#83787=CARTESIAN_POINT('Ctrl Pts',(11.3316747059724,27.1762278892077,-5.88597321154614));
#83788=CARTESIAN_POINT('Ctrl Pts',(11.3036883340533,27.0110003297392,-5.91659184866189));
#83789=CARTESIAN_POINT('Ctrl Pts',(11.2757019621341,26.8448013678039,-5.94022816472201));
#83790=CARTESIAN_POINT('Ctrl Pts',(11.2660109339038,26.7872505414007,-5.94841287000865));
#83791=CARTESIAN_POINT('Ctrl Pts',(11.2563199056734,26.7295833125003,-5.9557607946252));
#83792=CARTESIAN_POINT('Ctrl Pts',(11.2466288774431,26.6718243693625,-5.96226903256894));
#83793=CARTESIAN_POINT('Ctrl Pts',(11.2187513961962,26.505673387662,-5.98099081078629));
#83794=CARTESIAN_POINT('Ctrl Pts',(11.1908739149493,26.3387107239503,-5.99276628493694));
#83795=CARTESIAN_POINT('Ctrl Pts',(11.1629964337025,26.1715286708957,-5.99754765842346));
#83796=CARTESIAN_POINT('Ctrl Pts',(11.1351243336815,26.0043788892069,-6.00232810895532));
#83797=CARTESIAN_POINT('Ctrl Pts',(11.1072522336605,25.8370101201943,-6.00011714374969));
#83798=CARTESIAN_POINT('Ctrl Pts',(11.0793801336396,25.6700166037108,-5.99091904119672));
#83799=CARTESIAN_POINT('Ctrl Pts',(11.0515082701352,25.5030245042977,-5.98172101669682));
#83800=CARTESIAN_POINT('Ctrl Pts',(11.0236364066307,25.3364079685368,-5.96553598726629));
#83801=CARTESIAN_POINT('Ctrl Pts',(10.9957645431263,25.1707587479012,-5.94242029360239));
#83802=CARTESIAN_POINT('Ctrl Pts',(10.9678943525553,25.005119469913,-5.91930598739562));
#83803=CARTESIAN_POINT('Ctrl Pts',(10.9400241619842,24.8404477055799,-5.88926189348273));
#83804=CARTESIAN_POINT('Ctrl Pts',(10.9121539714132,24.6773278831695,-5.8523959598919));
#83805=CARTESIAN_POINT('Ctrl Pts',(10.8842795659469,24.5141833916432,-5.81552445095176));
#83806=CARTESIAN_POINT('Ctrl Pts',(10.8564051604806,24.3525916209166,-5.77182911146859));
#83807=CARTESIAN_POINT('Ctrl Pts',(10.8285307550143,24.1931253610869,-5.72146869599517));
#83808=CARTESIAN_POINT('Ctrl Pts',(10.818297145653,24.134580061838,-5.70297973414616));
#83809=CARTESIAN_POINT('Ctrl Pts',(10.8080635362916,24.076321113965,-5.68359289742881));
#83810=CARTESIAN_POINT('Ctrl Pts',(10.7978299269303,24.0183763331579,-5.6633177240034));
#83811=CARTESIAN_POINT('Ctrl Pts',(10.7696977847909,23.8590864138009,-5.60758137130871));
#83812=CARTESIAN_POINT('Ctrl Pts',(10.7415656426516,23.702135956483,-5.54511577331444));
#83813=CARTESIAN_POINT('Ctrl Pts',(10.7134335005122,23.5480882661828,-5.47614178501336));
#83814=CARTESIAN_POINT('Ctrl Pts',(10.6853048301441,23.3940595868179,-5.40717630875183));
#83815=CARTESIAN_POINT('Ctrl Pts',(10.6571761597759,23.2429332378814,-5.33170417045805));
#83816=CARTESIAN_POINT('Ctrl Pts',(10.6290474894078,23.0952514191351,-5.24999387446911));
#83817=CARTESIAN_POINT('Ctrl Pts',(10.6009186628996,22.9475687806187,-5.16828312491282));
#83818=CARTESIAN_POINT('Ctrl Pts',(10.5727898363915,22.8033309788704,-5.08033429409392));
#83819=CARTESIAN_POINT('Ctrl Pts',(10.5446610098833,22.6630552105896,-4.98646161846521));
#83820=CARTESIAN_POINT('Ctrl Pts',(10.5165343306218,22.5227901504224,-4.89259610871617));
#83821=CARTESIAN_POINT('Ctrl Pts',(10.4884076513603,22.3864867726021,-4.79280782832261));
#83822=CARTESIAN_POINT('Ctrl Pts',(10.4602809720987,22.2546332301958,-4.68745429413948));
#83823=CARTESIAN_POINT('Ctrl Pts',(10.4321527198829,22.1227723140219,-4.58209486817321));
#83824=CARTESIAN_POINT('Ctrl Pts',(10.404024467667,21.9953619691791,-4.47116975696246));
#83825=CARTESIAN_POINT('Ctrl Pts',(10.3758962154512,21.872857808516,-4.35507719004761));
#83826=CARTESIAN_POINT('Ctrl Pts',(10.3669411357733,21.8338566465811,-4.31811726168941));
#83827=CARTESIAN_POINT('Ctrl Pts',(10.3579860560953,21.7953524982787,-4.28063387251726));
#83828=CARTESIAN_POINT('Ctrl Pts',(10.3490309764174,21.7573593128807,-4.24264068711927));
#83829=CARTESIAN_POINT('',(7.20743823000724,30.2426406871193,4.24264068711929));
#83830=CARTESIAN_POINT('Ctrl Pts',(10.349030883597,21.7573593128807,-4.24264068711927));
#83831=CARTESIAN_POINT('Ctrl Pts',(10.3211052174972,21.6388807456707,-4.12416211990928));
#83832=CARTESIAN_POINT('Ctrl Pts',(10.2931795513974,21.5253558725309,-4.00070532573603));
#83833=CARTESIAN_POINT('Ctrl Pts',(10.2652538852976,21.4171909397775,-3.87270720782532));
#83834=CARTESIAN_POINT('Ctrl Pts',(10.2373311367051,21.3090373074524,-3.74472246239618));
#83835=CARTESIAN_POINT('Ctrl Pts',(10.2094083881127,21.2062427009957,-3.61219758103455));
#83836=CARTESIAN_POINT('Ctrl Pts',(10.1814856395203,21.1091736828357,-3.47560324768711));
#83837=CARTESIAN_POINT('Ctrl Pts',(10.1535599725185,21.0120945192872,-3.33899463787312));
#83838=CARTESIAN_POINT('Ctrl Pts',(10.1256343055166,20.9207423243946,-3.19831598171024));
#83839=CARTESIAN_POINT('Ctrl Pts',(10.0977086385148,20.8354412884937,-3.05406832199351));
#83840=CARTESIAN_POINT('Ctrl Pts',(10.0697829511709,20.7501401904563,-2.90982055720133));
#83841=CARTESIAN_POINT('Ctrl Pts',(10.0418572638269,20.6708904178689,-2.76200405661509));
#83842=CARTESIAN_POINT('Ctrl Pts',(10.013931576483,20.5979711181347,-2.61114610075604));
#83843=CARTESIAN_POINT('Ctrl Pts',(9.98599961470421,20.5250354346536,-2.46025424963762));
#83844=CARTESIAN_POINT('Ctrl Pts',(9.95806765292542,20.4584332020016,-2.30631986222864));
#83845=CARTESIAN_POINT('Ctrl Pts',(9.93013569114663,20.3983965081866,-2.14989262999431));
#83846=CARTESIAN_POINT('Ctrl Pts',(9.92016777179247,20.376971556836,-2.09406933881071));
#83847=CARTESIAN_POINT('Ctrl Pts',(9.91019985243831,20.3563822938692,-2.03792876199266));
#83848=CARTESIAN_POINT('Ctrl Pts',(9.90023193308415,20.3366377648729,-1.98149645312239));
#83849=CARTESIAN_POINT('Ctrl Pts',(9.87223131619321,20.2811739341101,-1.82297395662084));
#83850=CARTESIAN_POINT('Ctrl Pts',(9.84423069930227,20.2323625038322,-1.66209993737829));
#83851=CARTESIAN_POINT('Ctrl Pts',(9.81623008241133,20.1903821004303,-1.49944651821894));
#83852=CARTESIAN_POINT('Ctrl Pts',(9.78823418181804,20.1484087680182,-1.33682049566804));
#83853=CARTESIAN_POINT('Ctrl Pts',(9.76023828122473,20.1132642440369,-1.1724159732874));
#83854=CARTESIAN_POINT('Ctrl Pts',(9.73224238063144,20.0850767863215,-1.00681844256419));
#83855=CARTESIAN_POINT('Ctrl Pts',(9.70424684027408,20.0568896913069,-0.841223042659437));
#83856=CARTESIAN_POINT('Ctrl Pts',(9.67625129991674,20.0356595390914,-0.674434972048046));
#83857=CARTESIAN_POINT('Ctrl Pts',(9.64825575955938,20.0214632630262,-0.507048799085849));
#83858=CARTESIAN_POINT('Ctrl Pts',(9.62026227232045,20.0072680280781,-0.33967490178013));
#83859=CARTESIAN_POINT('Ctrl Pts',(9.59226878508153,20.0001056639017,-0.171703300650773));
#83860=CARTESIAN_POINT('Ctrl Pts',(9.56427529784261,20.0000011612094,-0.00373289588396664));
#83861=CARTESIAN_POINT('Ctrl Pts',(9.53627905335459,19.999896648224,0.164254053311281));
#83862=CARTESIAN_POINT('Ctrl Pts',(9.50828280886656,20.006851385897,0.332239493958736));
#83863=CARTESIAN_POINT('Ctrl Pts',(9.48028656437853,20.0208382443311,0.499624558589952));
#83864=CARTESIAN_POINT('Ctrl Pts',(9.47066870377616,20.0256433050506,0.557128207668029));
#83865=CARTESIAN_POINT('Ctrl Pts',(9.46105084317377,20.0312778483098,0.61456102333078));
#83866=CARTESIAN_POINT('Ctrl Pts',(9.45143298257139,20.037739358359,0.671898832518114));
#83867=CARTESIAN_POINT('Ctrl Pts',(9.42351189031721,20.0564974196,0.83835313313213));
#83868=CARTESIAN_POINT('Ctrl Pts',(9.39559079806303,20.0822324985814,1.00404004116379));
#83869=CARTESIAN_POINT('Ctrl Pts',(9.36766970580884,20.1148566697071,1.16836979672944));
#83870=CARTESIAN_POINT('Ctrl Pts',(9.33975183339789,20.1474770786335,1.33268060188844));
#83871=CARTESIAN_POINT('Ctrl Pts',(9.31183396098695,20.1869849324514,1.49563425761114));
#83872=CARTESIAN_POINT('Ctrl Pts',(9.283916088576,20.233241146378,1.65665093612744));
#83873=CARTESIAN_POINT('Ctrl Pts',(9.25599567924702,20.2795015636414,1.81768224635024));
#83874=CARTESIAN_POINT('Ctrl Pts',(9.22807526991804,20.3325114817047,1.97677592365439));
#83875=CARTESIAN_POINT('Ctrl Pts',(9.20015486058906,20.3920816560673,2.1333663182358));
#83876=CARTESIAN_POINT('Ctrl Pts',(9.17223463338991,20.4516514418429,2.28995569134995));
#83877=CARTESIAN_POINT('Ctrl Pts',(9.14431440619078,20.5177812833871,2.44404152052552));
#83878=CARTESIAN_POINT('Ctrl Pts',(9.11639417899164,20.5902333289587,2.59507698631285));
#83879=CARTESIAN_POINT('Ctrl Pts',(9.08846791866522,20.6627010302915,2.74614508851758));
#83880=CARTESIAN_POINT('Ctrl Pts',(9.06054165833879,20.7414935276847,2.89416122631526));
#83881=CARTESIAN_POINT('Ctrl Pts',(9.03261539801237,20.8263260977992,3.03860138117629));
#83882=CARTESIAN_POINT('Ctrl Pts',(9.0226216093611,20.8566845763982,3.09029123737493));
#83883=CARTESIAN_POINT('Ctrl Pts',(9.01262782070982,20.8878161603781,3.14152336661647));
#83884=CARTESIAN_POINT('Ctrl Pts',(9.00263403205854,20.9197064041777,3.19227457782808));
#83885=CARTESIAN_POINT('Ctrl Pts',(8.97467638145488,21.0089194468914,3.33425122755296));
#83886=CARTESIAN_POINT('Ctrl Pts',(8.94671873085123,21.1041016465399,3.47250780419374));
#83887=CARTESIAN_POINT('Ctrl Pts',(8.91876108024757,21.2049187549211,3.60654902269362));
#83888=CARTESIAN_POINT('Ctrl Pts',(8.89080869264064,21.3057168845933,3.74056500808271));
#83889=CARTESIAN_POINT('Ctrl Pts',(8.86285630503372,21.412147617434,3.8703669680771));
#83890=CARTESIAN_POINT('Ctrl Pts',(8.8349039174268,21.5238348055542,3.99549060217045));
#83891=CARTESIAN_POINT('Ctrl Pts',(8.8069522943046,21.6355189390821,4.12061081419089));
#83892=CARTESIAN_POINT('Ctrl Pts',(8.77900067118241,21.752459034069,4.24105271946324));
#83893=CARTESIAN_POINT('Ctrl Pts',(8.75104904806022,21.8742398121431,4.35638644662011));
#83894=CARTESIAN_POINT('Ctrl Pts',(8.7230995972203,21.9960111259288,4.4717112105261));
#83895=CARTESIAN_POINT('Ctrl Pts',(8.69515014638039,22.1226221425189,4.58192837425858));
#83896=CARTESIAN_POINT('Ctrl Pts',(8.66720069554047,22.2536217833888,4.6866459497279));
#83897=CARTESIAN_POINT('Ctrl Pts',(8.63924833355655,22.3846350688493,4.7913744323146));
#83898=CARTESIAN_POINT('Ctrl Pts',(8.61129597157264,22.5200376465994,4.89060198602177));
#83899=CARTESIAN_POINT('Ctrl Pts',(8.58334360958872,22.6593459482259,4.9839773781956));
#83900=CARTESIAN_POINT('Ctrl Pts',(8.57350743357439,22.7083672429503,5.01683530960609));
#83901=CARTESIAN_POINT('Ctrl Pts',(8.56367125756006,22.7578718971903,5.04896896823911));
#83902=CARTESIAN_POINT('Ctrl Pts',(8.55383508154573,22.8078379774106,5.08036431976468));
#83903=CARTESIAN_POINT('Ctrl Pts',(8.52585358610291,22.9499791554399,5.16967635366472));
#83904=CARTESIAN_POINT('Ctrl Pts',(8.49787209066009,23.0958840534137,5.25302763668785));
#83905=CARTESIAN_POINT('Ctrl Pts',(8.46989059521728,23.2450342329497,5.33011853736677));
#83906=CARTESIAN_POINT('Ctrl Pts',(8.44191190459252,23.3941694619224,5.40720171058341));
#83907=CARTESIAN_POINT('Ctrl Pts',(8.41393321396774,23.5465490453474,5.47802561079475));
#83908=CARTESIAN_POINT('Ctrl Pts',(8.38595452334298,23.7016304661779,5.54233682538317));
#83909=CARTESIAN_POINT('Ctrl Pts',(8.35797323329905,23.8567262951743,5.60665401494042));
#83910=CARTESIAN_POINT('Ctrl Pts',(8.32999194325513,24.0145241752471,5.66445718784331));
#83911=CARTESIAN_POINT('Ctrl Pts',(8.3020106532112,24.1744614362556,5.71554100258952));
#83912=CARTESIAN_POINT('Ctrl Pts',(8.27402966129036,24.3343969932329,5.76662427306973));
#83913=CARTESIAN_POINT('Ctrl Pts',(8.24604866936951,24.4964715868972,5.81098823603804));
#83914=CARTESIAN_POINT('Ctrl Pts',(8.21806767744866,24.660106970718,5.84847729499581));
#83915=CARTESIAN_POINT('Ctrl Pts',(8.19008127402464,24.8237740015011,5.88597360430991));
#83916=CARTESIAN_POINT('Ctrl Pts',(8.16209487060061,24.9890021205426,5.91659228413816));
#83917=CARTESIAN_POINT('Ctrl Pts',(8.13410846717658,25.1552016802526,5.94022859820664));
#83918=CARTESIAN_POINT('Ctrl Pts',(8.12441768846202,25.2127511670947,5.94841308285782));
#83919=CARTESIAN_POINT('Ctrl Pts',(8.11472690974746,25.2704170547458,5.95576082645265));
#83920=CARTESIAN_POINT('Ctrl Pts',(8.1050361310329,25.328174656801,5.96226892283765));
#83921=CARTESIAN_POINT('Ctrl Pts',(8.07715920733096,25.4943227356217,5.98099040144255));
#83922=CARTESIAN_POINT('Ctrl Pts',(8.049282283629,25.6612824464083,5.99276581585049));
#83923=CARTESIAN_POINT('Ctrl Pts',(8.02140535992706,25.8284615162792,5.99754737777059));
#83924=CARTESIAN_POINT('Ctrl Pts',(7.99353380797928,25.9956083715171,6.00232801830583));
#83925=CARTESIAN_POINT('Ctrl Pts',(7.96566225603151,26.1629741839552,6.00011748649617));
#83926=CARTESIAN_POINT('Ctrl Pts',(7.93779070408373,26.3299647343038,5.99092006908087));
#83927=CARTESIAN_POINT('Ctrl Pts',(7.90991937032615,26.4969539773803,5.98172272366681));
#83928=CARTESIAN_POINT('Ctrl Pts',(7.88204803656856,26.6635676467278,5.96553861588639));
#83929=CARTESIAN_POINT('Ctrl Pts',(7.85417670281099,26.8292140120055,5.94242409478605));
#83930=CARTESIAN_POINT('Ctrl Pts',(7.82630703023503,26.9948505044619,5.91931095135275));
#83931=CARTESIAN_POINT('Ctrl Pts',(7.79843735765908,27.1595194934828,5.88926826528854));
#83932=CARTESIAN_POINT('Ctrl Pts',(7.77056768508313,27.3226365732627,5.85240399281082));
#83933=CARTESIAN_POINT('Ctrl Pts',(7.7426937768956,27.4857784434519,5.8155341177291));
#83934=CARTESIAN_POINT('Ctrl Pts',(7.71481986870808,27.6473676231973,5.77184065528664));
#83935=CARTESIAN_POINT('Ctrl Pts',(7.68694596052055,27.8068313459651,5.72148236799152));
#83936=CARTESIAN_POINT('Ctrl Pts',(7.67670970052039,27.8653919222526,5.70298906886577));
#83937=CARTESIAN_POINT('Ctrl Pts',(7.66647344052023,27.9236659958665,5.68359743145597));
#83938=CARTESIAN_POINT('Ctrl Pts',(7.65623718052007,27.9816257293065,5.66331700233621));
#83939=CARTESIAN_POINT('Ctrl Pts',(7.62810436935998,28.1409192833715,5.60757931272468));
#83940=CARTESIAN_POINT('Ctrl Pts',(7.59997155819989,28.2978732427479,5.54511207805163));
#83941=CARTESIAN_POINT('Ctrl Pts',(7.5718387470398,28.4519242788586,5.4761361680243));
#83942=CARTESIAN_POINT('Ctrl Pts',(7.5437094058063,28.6059563141739,5.40716876554863));
#83943=CARTESIAN_POINT('Ctrl Pts',(7.5155800645728,28.7570858624845,5.33169441516243));
#83944=CARTESIAN_POINT('Ctrl Pts',(7.4874507233393,28.9047707007979,5.24998163575705));
#83945=CARTESIAN_POINT('Ctrl Pts',(7.45932122986369,29.0524563384138,5.16826841410433));
#83946=CARTESIAN_POINT('Ctrl Pts',(7.43119173638808,29.1966969604368,5.08031684157763));
#83947=CARTESIAN_POINT('Ctrl Pts',(7.40306224291247,29.3369753471838,4.98644116903908));
#83948=CARTESIAN_POINT('Ctrl Pts',(7.37493490097868,29.4772430044515,4.8925726767733));
#83949=CARTESIAN_POINT('Ctrl Pts',(7.34680755904491,29.6135487788148,4.79278116046622));
#83950=CARTESIAN_POINT('Ctrl Pts',(7.31868021711113,29.7454044940789,4.68742415146459));
#83951=CARTESIAN_POINT('Ctrl Pts',(7.29055131360684,29.8772675296933,4.58206129326477));
#83952=CARTESIAN_POINT('Ctrl Pts',(7.26242241010255,30.0046797739015,4.47113251538327));
#83953=CARTESIAN_POINT('Ctrl Pts',(7.23429350659826,30.1271855905679,4.35503606196422));
#83954=CARTESIAN_POINT('Ctrl Pts',(7.22534174773459,30.1661719140137,4.31808945806348));
#83955=CARTESIAN_POINT('Ctrl Pts',(7.21638998887092,30.204661590743,4.28061978349558));
#83956=CARTESIAN_POINT('Ctrl Pts',(7.20743823000725,30.2426406871193,4.24264068711928));
#83957=CARTESIAN_POINT('Ctrl Pts',(7.20743823000725,30.2426406871193,4.24264068711928));
#83958=CARTESIAN_POINT('Ctrl Pts',(7.17951256390743,30.3611192543293,4.1241621199093));
#83959=CARTESIAN_POINT('Ctrl Pts',(7.15158689780761,30.4746441274691,4.00070532573605));
#83960=CARTESIAN_POINT('Ctrl Pts',(7.1236612317078,30.5828090602225,3.87270720782535));
#83961=CARTESIAN_POINT('Ctrl Pts',(7.09573848311536,30.6909626925476,3.74472246239618));
#83962=CARTESIAN_POINT('Ctrl Pts',(7.06781573452291,30.7937572990044,3.61219758103451));
#83963=CARTESIAN_POINT('Ctrl Pts',(7.03989298593048,30.8908263171644,3.47560324768702));
#83964=CARTESIAN_POINT('Ctrl Pts',(7.01196731892867,30.9879054807129,3.33899463787309));
#83965=CARTESIAN_POINT('Ctrl Pts',(6.98404165192688,31.0792576756054,3.19831598171026));
#83966=CARTESIAN_POINT('Ctrl Pts',(6.95611598492507,31.1645587115063,3.05406832199359));
#83967=CARTESIAN_POINT('Ctrl Pts',(6.92819029758115,31.2498598095437,2.90982055720145));
#83968=CARTESIAN_POINT('Ctrl Pts',(6.90026461023721,31.329109582131,2.76200405661523));
#83969=CARTESIAN_POINT('Ctrl Pts',(6.87233892289328,31.4020288818652,2.61114610075623));
#83970=CARTESIAN_POINT('Ctrl Pts',(6.84440696111448,31.4749645653464,2.46025424963772));
#83971=CARTESIAN_POINT('Ctrl Pts',(6.81647499933569,31.5415667979984,2.30631986222865));
#83972=CARTESIAN_POINT('Ctrl Pts',(6.78854303755689,31.6016034918134,2.14989262999423));
#83973=CARTESIAN_POINT('Ctrl Pts',(6.77857511820273,31.6230284431641,2.09406933881066));
#83974=CARTESIAN_POINT('Ctrl Pts',(6.76860719884858,31.6436177061308,2.03792876199264));
#83975=CARTESIAN_POINT('Ctrl Pts',(6.75863927949442,31.6633622351271,1.9814964531224));
#83976=CARTESIAN_POINT('Ctrl Pts',(6.73063866260346,31.71882606589,1.82297395662076));
#83977=CARTESIAN_POINT('Ctrl Pts',(6.70263804571251,31.7676374961679,1.66209993737812));
#83978=CARTESIAN_POINT('Ctrl Pts',(6.67463742882156,31.8096178995698,1.49944651821868));
#83979=CARTESIAN_POINT('Ctrl Pts',(6.64664152822826,31.8515912319819,1.33682049566777));
#83980=CARTESIAN_POINT('Ctrl Pts',(6.61864562763495,31.8867357559632,1.17241597328713));
#83981=CARTESIAN_POINT('Ctrl Pts',(6.59064972704165,31.9149232136785,1.0068184425639));
#83982=CARTESIAN_POINT('Ctrl Pts',(6.56265418668425,31.9431103086931,0.841223042658928));
#83983=CARTESIAN_POINT('Ctrl Pts',(6.53465864632685,31.9643404609087,0.67443497204731));
#83984=CARTESIAN_POINT('Ctrl Pts',(6.50666310596945,31.9785367369739,0.507048799084887));
#83985=CARTESIAN_POINT('Ctrl Pts',(6.4786696187305,31.992731971922,0.339674901779049));
#83986=CARTESIAN_POINT('Ctrl Pts',(6.45067613149154,31.9998943360983,0.171703300649576));
#83987=CARTESIAN_POINT('Ctrl Pts',(6.42268264425259,31.9999988387906,0.00373289588265302));
#83988=CARTESIAN_POINT('Ctrl Pts',(6.39468639976459,32.000103351776,-0.164254053312412));
#83989=CARTESIAN_POINT('Ctrl Pts',(6.3666901552766,31.9931486141029,-0.332239493959689));
#83990=CARTESIAN_POINT('Ctrl Pts',(6.3386939107886,31.9791617556689,-0.499624558590723));
#83991=CARTESIAN_POINT('Ctrl Pts',(6.32907605018627,31.9743566949493,-0.557128207668544));
#83992=CARTESIAN_POINT('Ctrl Pts',(6.31945818958392,31.9687221516902,-0.614561023331037));
#83993=CARTESIAN_POINT('Ctrl Pts',(6.30984032898158,31.962260641641,-0.671898832518117));
#83994=CARTESIAN_POINT('Ctrl Pts',(6.28191923672742,31.9435025804001,-0.838353133131996));
#83995=CARTESIAN_POINT('Ctrl Pts',(6.25399814447326,31.9177675014186,-1.00404004116352));
#83996=CARTESIAN_POINT('Ctrl Pts',(6.2260770522191,31.8851433302929,-1.16836979672903));
#83997=CARTESIAN_POINT('Ctrl Pts',(6.19815917980828,31.8525229213668,-1.33268060188732));
#83998=CARTESIAN_POINT('Ctrl Pts',(6.17024130739745,31.8130150675491,-1.49563425760931));
#83999=CARTESIAN_POINT('Ctrl Pts',(6.14232343498663,31.7667588536228,-1.65665093612492));
#84000=CARTESIAN_POINT('Ctrl Pts',(6.11440302565763,31.7204984363593,-1.81768224634783));
#84001=CARTESIAN_POINT('Ctrl Pts',(6.08648261632864,31.6674885182961,-1.97677592365209));
#84002=CARTESIAN_POINT('Ctrl Pts',(6.05856220699964,31.6079183439335,-2.1333663182336));
#84003=CARTESIAN_POINT('Ctrl Pts',(6.03064197980054,31.5483485581581,-2.28995569134754));
#84004=CARTESIAN_POINT('Ctrl Pts',(6.00272175260146,31.482218716614,-2.44404152052291));
#84005=CARTESIAN_POINT('Ctrl Pts',(5.97480152540236,31.4097666710427,-2.59507698631006));
#84006=CARTESIAN_POINT('Ctrl Pts',(5.94687526507597,31.3372989697099,-2.74614508851467));
#84007=CARTESIAN_POINT('Ctrl Pts',(5.91894900474958,31.2585064723169,-2.89416122631225));
#84008=CARTESIAN_POINT('Ctrl Pts',(5.89102274442319,31.1736739022026,-3.03860138117318));
#84009=CARTESIAN_POINT('Ctrl Pts',(5.88102895577172,31.1433154236031,-3.09029123737288));
#84010=CARTESIAN_POINT('Ctrl Pts',(5.87103516712024,31.1121838396226,-3.14152336661546));
#84011=CARTESIAN_POINT('Ctrl Pts',(5.86104137846877,31.0802935958222,-3.19227457782808));
#84012=CARTESIAN_POINT('Ctrl Pts',(5.83265381532736,30.9897086994383,-3.33643444182407));
#84013=CARTESIAN_POINT('Ctrl Pts',(5.80426625218595,30.8929750200676,-3.47675066095956));
#84014=CARTESIAN_POINT('Ctrl Pts',(5.77587868904454,30.7904383789029,-3.61271368059163));
#84015=CARTESIAN_POINT('Ctrl Pts',(5.74749725742285,30.6879238849523,-3.7486473331402));
#84016=CARTESIAN_POINT('Ctrl Pts',(5.71911582580117,30.5796091072431,-3.88022942977747));
#84017=CARTESIAN_POINT('Ctrl Pts',(5.69073439417949,30.4658817087328,-4.00698147782166));
#84018=CARTESIAN_POINT('Ctrl Pts',(5.67270356408276,30.3936302653519,-4.08750752996593));
#84019=CARTESIAN_POINT('Ctrl Pts',(5.65467273398604,30.3191950666548,-4.16608475088474));
#84020=CARTESIAN_POINT('Ctrl Pts',(5.63664190388932,30.2426838347204,-4.24259753907934));
#84021=CARTESIAN_POINT('',(5.35893340537649,30.2426406871193,4.24264068711929));
#84022=CARTESIAN_POINT('Ctrl Pts',(3.78813707791307,30.2426869010466,-4.24259447268859));
#84023=CARTESIAN_POINT('Ctrl Pts',(3.816515452064,30.3631064902981,-4.12217225999875));
#84024=CARTESIAN_POINT('Ctrl Pts',(3.84489382621493,30.4783816103409,-3.99663448658121));
#84025=CARTESIAN_POINT('Ctrl Pts',(3.87327220036586,30.5880993722131,-3.86643817365513));
#84026=CARTESIAN_POINT('Ctrl Pts',(3.90165911004251,30.6978501345234,-3.73620270084018));
#84027=CARTESIAN_POINT('Ctrl Pts',(3.93004601971916,30.8020400105107,-3.60130611285029));
#84028=CARTESIAN_POINT('Ctrl Pts',(3.95843292939582,30.9002961498858,-3.46223881952335));
#84029=CARTESIAN_POINT('Ctrl Pts',(3.97646747087655,30.9627194443367,-3.37388771337318));
#84030=CARTESIAN_POINT('Ctrl Pts',(3.99450201235727,31.0227485778494,-3.28385387398067));
#84031=CARTESIAN_POINT('Ctrl Pts',(4.012536553838,31.0802969047552,-3.19226931187434));
#84032=CARTESIAN_POINT('Ctrl Pts',(4.04046279521554,31.1694097036452,-3.05045186724619));
#84033=CARTESIAN_POINT('Ctrl Pts',(4.06838903659308,31.252595263152,-2.90487727016411));
#84034=CARTESIAN_POINT('Ctrl Pts',(4.09631527797061,31.3295526946622,-2.75606024513595));
#84035=CARTESIAN_POINT('Ctrl Pts',(4.12423606502702,31.4064950954872,-2.60727228581099));
#84036=CARTESIAN_POINT('Ctrl Pts',(4.15215685208344,31.4772116508648,-2.45524344240145));
#84037=CARTESIAN_POINT('Ctrl Pts',(4.18007763913985,31.5414475513461,-2.30051277668276));
#84038=CARTESIAN_POINT('Ctrl Pts',(4.20799765893873,31.6056816866379,-2.14578636293118));
#84039=CARTESIAN_POINT('Ctrl Pts',(4.23591767873761,31.6634353986696,-1.98835856524518));
#84040=CARTESIAN_POINT('Ctrl Pts',(4.26383769853649,31.7145018662962,-1.82878878498768));
#84041=CARTESIAN_POINT('Ctrl Pts',(4.29175562275567,31.7655645010513,-1.66923098148356));
#84042=CARTESIAN_POINT('Ctrl Pts',(4.31967354697488,31.8099407990447,-1.50753181741852));
#84043=CARTESIAN_POINT('Ctrl Pts',(4.34759147119407,31.8474736019631,-1.34426651908945));
#84044=CARTESIAN_POINT('Ctrl Pts',(4.37551264680177,31.8850107760418,-1.18098220649159));
#84045=CARTESIAN_POINT('Ctrl Pts',(4.40343382240945,31.9157027919866,-1.01613170273964));
#84046=CARTESIAN_POINT('Ctrl Pts',(4.43135499801715,31.939443307781,-0.8503018250333));
#84047=CARTESIAN_POINT('Ctrl Pts',(4.44134850012838,31.9479404748791,-0.790948262839224));
#84048=CARTESIAN_POINT('Ctrl Pts',(4.45134200223961,31.9555475942772,-0.731469320963337));
#84049=CARTESIAN_POINT('Ctrl Pts',(4.46133550435084,31.9622613954461,-0.671892143407596));
#84050=CARTESIAN_POINT('Ctrl Pts',(4.48933160516719,31.9810696422743,-0.504990825867469));
#84051=CARTESIAN_POINT('Ctrl Pts',(4.51732770598352,31.992867180341,-0.337284199462853));
#84052=CARTESIAN_POINT('Ctrl Pts',(4.54532380679987,31.9976090079534,-0.169369972888486));
#84053=CARTESIAN_POINT('Ctrl Pts',(4.57331711061984,32.0023503618258,-0.00147252206045653));
#84054=CARTESIAN_POINT('Ctrl Pts',(4.60131041443981,32.0000374038039,0.166632175800177));
#84055=CARTESIAN_POINT('Ctrl Pts',(4.62930371825977,31.9906772214171,0.334344775336205));
#84056=CARTESIAN_POINT('Ctrl Pts',(4.65729949760172,31.9813162112846,0.502072206141611));
#84057=CARTESIAN_POINT('Ctrl Pts',(4.68529527694368,31.9649067465216,0.669407157710664));
#84058=CARTESIAN_POINT('Ctrl Pts',(4.71329105628564,31.9415079690106,0.835752986344446));
#84059=CARTESIAN_POINT('Ctrl Pts',(4.74128642739747,31.918109532697,1.00209638934909));
#84060=CARTESIAN_POINT('Ctrl Pts',(4.76928179850931,31.8877220334429,1.16745038970294));
#84061=CARTESIAN_POINT('Ctrl Pts',(4.79727716962114,31.8504561912662,1.33122588394137));
#84062=CARTESIAN_POINT('Ctrl Pts',(4.82527768223529,31.8131835050147,1.49503145644092));
#84063=CARTESIAN_POINT('Ctrl Pts',(4.85327819484944,31.7690300219162,1.65725763956866));
#84064=CARTESIAN_POINT('Ctrl Pts',(4.88127870746359,31.7181572341969,1.81732711557434));
#84065=CARTESIAN_POINT('Ctrl Pts',(4.89089728993028,31.7006816932762,1.87231330374087));
#84066=CARTESIAN_POINT('Ctrl Pts',(4.90051587239697,31.6824136939749,1.92704512147826));
#84067=CARTESIAN_POINT('Ctrl Pts',(4.91013445486366,31.6633611357654,1.98149959523123));
#84068=CARTESIAN_POINT('Ctrl Pts',(4.93806707679286,31.6080319947938,2.13963685017107));
#84069=CARTESIAN_POINT('Ctrl Pts',(4.96599969872205,31.5460659526854,2.2954819267778));
#84070=CARTESIAN_POINT('Ctrl Pts',(4.99393232065124,31.4776777973362,2.44847829244406));
#84071=CARTESIAN_POINT('Ctrl Pts',(5.02185928540985,31.4093034925831,2.60144367188414));
#84072=CARTESIAN_POINT('Ctrl Pts',(5.04978625016845,31.334509798614,2.75156120412281));
#84073=CARTESIAN_POINT('Ctrl Pts',(5.07771321492705,31.2535592679187,2.89829519174042));
#84074=CARTESIAN_POINT('Ctrl Pts',(5.10563904188241,31.1726120353182,3.04502320110693));
#84075=CARTESIAN_POINT('Ctrl Pts',(5.13356486883776,31.0855086162654,3.18836766367047));
#84076=CARTESIAN_POINT('Ctrl Pts',(5.16149069579312,30.9925573914775,3.32781770726749));
#84077=CARTESIAN_POINT('Ctrl Pts',(5.18941419241778,30.8996139232046,3.46725611415569));
#84078=CARTESIAN_POINT('Ctrl Pts',(5.21733768904245,30.8008237995959,3.60280048960743));
#84079=CARTESIAN_POINT('Ctrl Pts',(5.24526118566711,30.6965387529717,3.73396889941992));
#84080=CARTESIAN_POINT('Ctrl Pts',(5.27318753576663,30.5922430495604,3.86515071320411));
#84081=CARTESIAN_POINT('Ctrl Pts',(5.30111388586613,30.4824514972791,3.99195542114597));
#84082=CARTESIAN_POINT('Ctrl Pts',(5.32904023596565,30.3675565881145,4.11393357379745));
#84083=CARTESIAN_POINT('Ctrl Pts',(5.33900462576926,30.3265609815534,4.15745654963257));
#84084=CARTESIAN_POINT('Ctrl Pts',(5.34896901557288,30.2849160127224,4.20036536151615));
#84085=CARTESIAN_POINT('Ctrl Pts',(5.35893340537649,30.2426406871193,4.24264068711928));
#84086=CARTESIAN_POINT('',(8.50052610236153,21.7573593077119,-4.24264069228803));
#84087=CARTESIAN_POINT('Ctrl Pts',(5.35893340537649,30.2426406871193,4.24264068711928));
#84088=CARTESIAN_POINT('Ctrl Pts',(5.3870628280945,30.1232976537907,4.3619837204479));
#84089=CARTESIAN_POINT('Ctrl Pts',(5.41519225081251,29.9989103679391,4.47629371275373));
#84090=CARTESIAN_POINT('Ctrl Pts',(5.44332167353052,29.8699233733809,4.58516009362379));
#84091=CARTESIAN_POINT('Ctrl Pts',(5.47144933461812,29.7409444567494,4.69401965663878));
#84092=CARTESIAN_POINT('Ctrl Pts',(5.49957699570573,29.6073666401139,4.79743609238796));
#84093=CARTESIAN_POINT('Ctrl Pts',(5.52770465679333,29.4696681199931,4.89503862467947));
#84094=CARTESIAN_POINT('Ctrl Pts',(5.55583498230706,29.3319565562162,4.99265040248689));
#84095=CARTESIAN_POINT('Ctrl Pts',(5.58396530782079,29.1901237569449,5.08444699821659));
#84096=CARTESIAN_POINT('Ctrl Pts',(5.61209563333453,29.0446781877336,5.17010006993478));
#84097=CARTESIAN_POINT('Ctrl Pts',(5.64022526627055,28.8992361994392,5.25575103284663));
#84098=CARTESIAN_POINT('Ctrl Pts',(5.66835489920657,28.7501818832098,5.33525862111028));
#84099=CARTESIAN_POINT('Ctrl Pts',(5.69648453214259,28.5980499480886,5.40833952958181));
#84100=CARTESIAN_POINT('Ctrl Pts',(5.72461782373482,28.4458982260597,5.48142994325803));
#84101=CARTESIAN_POINT('Ctrl Pts',(5.75275111532705,28.2906683607607,5.54809187525009));
#84102=CARTESIAN_POINT('Ctrl Pts',(5.78088440691927,28.1329175038741,5.60808906149571));
#84103=CARTESIAN_POINT('Ctrl Pts',(5.78983372324263,28.0827363043535,5.62717441439382));
#84104=CARTESIAN_POINT('Ctrl Pts',(5.79878303956597,28.0323001564974,5.64558572516284));
#84105=CARTESIAN_POINT('Ctrl Pts',(5.80773235588932,27.981627395157,5.66331641944572));
#84106=CARTESIAN_POINT('Ctrl Pts',(5.83560583606672,27.8238023549277,5.71854032010687));
#84107=CARTESIAN_POINT('Ctrl Pts',(5.86347931624414,27.6636453184919,5.76717046119707));
#84108=CARTESIAN_POINT('Ctrl Pts',(5.89135279642155,27.5017235010104,5.80902974054302));
#84109=CARTESIAN_POINT('Ctrl Pts',(5.91922222299253,27.3398252316225,5.85088293234471));
#84110=CARTESIAN_POINT('Ctrl Pts',(5.94709164956352,27.1761630010024,5.88596714805155));
#84111=CARTESIAN_POINT('Ctrl Pts',(5.97496107613449,27.0113173742088,5.9141556598236));
#84112=CARTESIAN_POINT('Ctrl Pts',(6.00283223854301,26.8464614800627,5.9423459273073));
#84113=CARTESIAN_POINT('Ctrl Pts',(6.03070340095152,26.6804223552794,5.96363957616521));
#84114=CARTESIAN_POINT('Ctrl Pts',(6.05857456336004,26.5137896250338,5.97796120940976));
#84115=CARTESIAN_POINT('Ctrl Pts',(6.08644519597083,26.3471600622786,5.99228257041705));
#84116=CARTESIAN_POINT('Ctrl Pts',(6.11431582858164,26.1799372335241,5.99963215607804));
#84117=CARTESIAN_POINT('Ctrl Pts',(6.14218646119243,26.0127149542826,5.99998652747968));
#84118=CARTESIAN_POINT('Ctrl Pts',(6.17006298049281,25.845457355224,6.0003409737298));
#84119=CARTESIAN_POINT('Ctrl Pts',(6.19793949979319,25.6782006238214,5.99369725404834));
#84120=CARTESIAN_POINT('Ctrl Pts',(6.22581601909357,25.511538413208,5.9800840527729));
#84121=CARTESIAN_POINT('Ctrl Pts',(6.23605444819643,25.4503270686674,5.97508422497447));
#84122=CARTESIAN_POINT('Ctrl Pts',(6.24629287729929,25.3891958917371,5.96914476897281));
#84123=CARTESIAN_POINT('Ctrl Pts',(6.25653130640214,25.3281741450145,5.96226886516979));
#84124=CARTESIAN_POINT('Ctrl Pts',(6.28451774466434,25.1613730342045,5.94347378876237));
#84125=CARTESIAN_POINT('Ctrl Pts',(6.31250418292654,24.9953373785667,5.91767204983512));
#84126=CARTESIAN_POINT('Ctrl Pts',(6.34049062118875,24.8306595845358,5.8849505514288));
#84127=CARTESIAN_POINT('Ctrl Pts',(6.36847212349185,24.6660108346743,5.8522348241026));
#84128=CARTESIAN_POINT('Ctrl Pts',(6.39645362579495,24.5027197749735,5.81260183387982));
#84129=CARTESIAN_POINT('Ctrl Pts',(6.42443512809806,24.341369031207,5.76618966990863));
#84130=CARTESIAN_POINT('Ctrl Pts',(6.45241608108101,24.1800214550052,5.71977841707999));
#84131=CARTESIAN_POINT('Ctrl Pts',(6.48039703406395,24.0206144199361,5.66658833974929));
#84132=CARTESIAN_POINT('Ctrl Pts',(6.5083779870469,23.8637164806476,5.60680771249946));
#84133=CARTESIAN_POINT('Ctrl Pts',(6.53635681619747,23.7068304503503,5.547031622766));
#84134=CARTESIAN_POINT('Ctrl Pts',(6.56433564534805,23.5524534270869,5.48066609483771));
#84135=CARTESIAN_POINT('Ctrl Pts',(6.59231447449862,23.4011353477862,5.40794808771993));
#84136=CARTESIAN_POINT('Ctrl Pts',(6.62029606770103,23.2498023196464,5.33522289672965));
#84137=CARTESIAN_POINT('Ctrl Pts',(6.64827766090344,23.1015291210748,5.25614410805374));
#84138=CARTESIAN_POINT('Ctrl Pts',(6.67625925410585,22.9568430559818,5.17099563083105));
#84139=CARTESIAN_POINT('Ctrl Pts',(6.68594958837556,22.906736676235,5.14150777426493));
#84140=CARTESIAN_POINT('Ctrl Pts',(6.69563992264525,22.8570602862605,5.11129237445357));
#84141=CARTESIAN_POINT('Ctrl Pts',(6.70533025691496,22.8078350564431,5.08036248442237));
#84142=CARTESIAN_POINT('Ctrl Pts',(6.73328239323225,22.6658430161469,4.99114404485486));
#84143=CARTESIAN_POINT('Ctrl Pts',(6.76123452954954,22.5275793803426,4.89596010939473));
#84144=CARTESIAN_POINT('Ctrl Pts',(6.78918666586683,22.3935381982795,4.79514684579429));
#84145=CARTESIAN_POINT('Ctrl Pts',(6.8171358543992,22.2595111519723,4.69434421378974));
#84146=CARTESIAN_POINT('Ctrl Pts',(6.84508504293158,22.1297059213547,4.58791362749829));
#84147=CARTESIAN_POINT('Ctrl Pts',(6.87303423146396,22.004585380564,4.47623301658856));
#84148=CARTESIAN_POINT('Ctrl Pts',(6.90098607860559,21.8794529379384,4.36454178228968));
#84149=CARTESIAN_POINT('Ctrl Pts',(6.92893792574723,21.759006311528,4.2475997328004));
#84150=CARTESIAN_POINT('Ctrl Pts',(6.95688977288886,21.6436738204348,4.12582382285462));
#84151=CARTESIAN_POINT('Ctrl Pts',(6.98484143161379,21.5283421067702,4.00404873377111));
#84152=CARTESIAN_POINT('Ctrl Pts',(7.0127930903387,21.4181246733265,3.87744007942548));
#84153=CARTESIAN_POINT('Ctrl Pts',(7.04074474906362,21.3134117771372,3.74645043065086));
#84154=CARTESIAN_POINT('Ctrl Pts',(7.0687022001181,21.2086771816417,3.61543363732567));
#84155=CARTESIAN_POINT('Ctrl Pts',(7.09665965117257,21.1094495978143,3.48003428166612));
#84156=CARTESIAN_POINT('Ctrl Pts',(7.12461710222705,21.0160784017799,3.34073726934573));
#84157=CARTESIAN_POINT('Ctrl Pts',(7.13445447062729,20.9832239455002,3.29172292878301));
#84158=CARTESIAN_POINT('Ctrl Pts',(7.14429183902755,20.951094195107,3.24222628351));
#84159=CARTESIAN_POINT('Ctrl Pts',(7.1541292074278,20.9197030952448,3.19226931187431));
#84160=CARTESIAN_POINT('Ctrl Pts',(7.18205544880533,20.8305902963548,3.05045186724616));
#84161=CARTESIAN_POINT('Ctrl Pts',(7.20998169018287,20.747404736848,2.9048772701641));
#84162=CARTESIAN_POINT('Ctrl Pts',(7.2379079315604,20.6704473053378,2.75606024513595));
#84163=CARTESIAN_POINT('Ctrl Pts',(7.26582871861674,20.593504904513,2.60727228581136));
#84164=CARTESIAN_POINT('Ctrl Pts',(7.29374950567309,20.5227883491355,2.4552434424022));
#84165=CARTESIAN_POINT('Ctrl Pts',(7.32167029272943,20.4585524486544,2.30051277668391));
#84166=CARTESIAN_POINT('Ctrl Pts',(7.34959031252838,20.3943183133624,2.145786362932));
#84167=CARTESIAN_POINT('Ctrl Pts',(7.37751033232731,20.3365646013306,1.98835856524566));
#84168=CARTESIAN_POINT('Ctrl Pts',(7.40543035212626,20.2854981337038,1.8287887849878));
#84169=CARTESIAN_POINT('Ctrl Pts',(7.43334827634547,20.2344354989487,1.66923098148351));
#84170=CARTESIAN_POINT('Ctrl Pts',(7.46126620056469,20.1900592009552,1.50753181741829));
#84171=CARTESIAN_POINT('Ctrl Pts',(7.48918412478391,20.1525263980368,1.34426651908904));
#84172=CARTESIAN_POINT('Ctrl Pts',(7.51710530039168,20.114989223958,1.18098220649074));
#84173=CARTESIAN_POINT('Ctrl Pts',(7.54502647599945,20.0842972080132,1.01613170273834));
#84174=CARTESIAN_POINT('Ctrl Pts',(7.57294765160723,20.0605566922187,0.850301825031545));
#84175=CARTESIAN_POINT('Ctrl Pts',(7.58294115371836,20.0520595251207,0.790948262838054));
#84176=CARTESIAN_POINT('Ctrl Pts',(7.59293465582949,20.0444524057227,0.731469320962755));
#84177=CARTESIAN_POINT('Ctrl Pts',(7.60292815794062,20.0377386045539,0.671892143407602));
#84178=CARTESIAN_POINT('Ctrl Pts',(7.63092425875694,20.0189303577257,0.504990825867639));
#84179=CARTESIAN_POINT('Ctrl Pts',(7.65892035957326,20.0071328196591,0.33728419946319));
#84180=CARTESIAN_POINT('Ctrl Pts',(7.68691646038959,20.0023909920466,0.169369972888987));
#84181=CARTESIAN_POINT('Ctrl Pts',(7.71490976420946,19.9976496381742,0.00147252206147364));
#84182=CARTESIAN_POINT('Ctrl Pts',(7.74290306802933,19.9999625961961,-0.166632175798642));
#84183=CARTESIAN_POINT('Ctrl Pts',(7.77089637184921,20.0093227785828,-0.33434477533416));
#84184=CARTESIAN_POINT('Ctrl Pts',(7.79889215119115,20.0186837887153,-0.502072206139494));
#84185=CARTESIAN_POINT('Ctrl Pts',(7.8268879305331,20.0350932534782,-0.669407157708479));
#84186=CARTESIAN_POINT('Ctrl Pts',(7.85488370987504,20.0584920309891,-0.835752986342195));
#84187=CARTESIAN_POINT('Ctrl Pts',(7.88287908098689,20.0818904673027,-1.00209638934693));
#84188=CARTESIAN_POINT('Ctrl Pts',(7.91087445209875,20.1122779665567,-1.16745038970086));
#84189=CARTESIAN_POINT('Ctrl Pts',(7.9388698232106,20.1495438087334,-1.33122588393938));
#84190=CARTESIAN_POINT('Ctrl Pts',(7.96687033582474,20.1868164949848,-1.49503145643893));
#84191=CARTESIAN_POINT('Ctrl Pts',(7.99487084843889,20.2309699780832,-1.65725763956667));
#84192=CARTESIAN_POINT('Ctrl Pts',(8.02287136105303,20.2818427658025,-1.81732711557235));
#84193=CARTESIAN_POINT('Ctrl Pts',(8.03248994351984,20.2993183067234,-1.87231330373955));
#84194=CARTESIAN_POINT('Ctrl Pts',(8.04210852598664,20.3175863060249,-1.92704512147761));
#84195=CARTESIAN_POINT('Ctrl Pts',(8.05172710845345,20.3366388642346,-1.98149959523124));
#84196=CARTESIAN_POINT('Ctrl Pts',(8.07965973038267,20.3919680052063,-2.13963685017114));
#84197=CARTESIAN_POINT('Ctrl Pts',(8.10759235231187,20.4539340473147,-2.29548192677793));
#84198=CARTESIAN_POINT('Ctrl Pts',(8.13552497424108,20.5223222026639,-2.44847829244425));
#84199=CARTESIAN_POINT('Ctrl Pts',(8.16345193899964,20.5906965074169,-2.60144367188407));
#84200=CARTESIAN_POINT('Ctrl Pts',(8.1913789037582,20.6654902013859,-2.75156120412248));
#84201=CARTESIAN_POINT('Ctrl Pts',(8.21930586851675,20.746440732081,-2.89829519173985));
#84202=CARTESIAN_POINT('Ctrl Pts',(8.24723169547209,20.8273879646814,-3.04502320110628));
#84203=CARTESIAN_POINT('Ctrl Pts',(8.27515752242742,20.9144913837342,-3.18836766366975));
#84204=CARTESIAN_POINT('Ctrl Pts',(8.30308334938276,21.0074426085219,-3.3278177072667));
#84205=CARTESIAN_POINT('Ctrl Pts',(8.33100684600741,21.1003860767948,-3.46725611415485));
#84206=CARTESIAN_POINT('Ctrl Pts',(8.35893034263206,21.1991762004034,-3.60280048960655));
#84207=CARTESIAN_POINT('Ctrl Pts',(8.38685383925671,21.3034612470276,-3.73396889941901));
#84208=CARTESIAN_POINT('Ctrl Pts',(8.4147801893562,21.4077569504388,-3.86515071320316));
#84209=CARTESIAN_POINT('Ctrl Pts',(8.44270653945571,21.51754850272,-3.99195542114498));
#84210=CARTESIAN_POINT('Ctrl Pts',(8.47063288955521,21.6324434118846,-4.11393357379643));
#84211=CARTESIAN_POINT('Ctrl Pts',(8.4805972793589,21.673439018446,-4.1574565496319));
#84212=CARTESIAN_POINT('Ctrl Pts',(8.49056166916259,21.7150839872773,-4.20036536151581));
#84213=CARTESIAN_POINT('Ctrl Pts',(8.50052605896628,21.7573593128807,-4.24264068711927));
#84214=CARTESIAN_POINT('Ctrl Pts',(8.50052615178669,21.7573593128807,-4.24264068711927));
#84215=CARTESIAN_POINT('Ctrl Pts',(8.52865485901884,21.8766993106599,-4.36198068489846));
#84216=CARTESIAN_POINT('Ctrl Pts',(8.55678356625099,22.0010833453181,-4.47628793832941));
#84217=CARTESIAN_POINT('Ctrl Pts',(8.58491227348314,22.1300669041397,-4.58515188773124));
#84218=CARTESIAN_POINT('Ctrl Pts',(8.61303920813034,22.2590423348126,-4.69400897686049));
#84219=CARTESIAN_POINT('Ctrl Pts',(8.64116614277755,22.392616477355,-4.79742325031555));
#84220=CARTESIAN_POINT('Ctrl Pts',(8.66929307742474,22.5303111654473,-4.89502394185975));
#84221=CARTESIAN_POINT('Ctrl Pts',(8.69742266764845,22.6680188538464,-4.99263384827602));
#84222=CARTESIAN_POINT('Ctrl Pts',(8.72555225787215,22.8098476171784,-5.08442889782456));
#84223=CARTESIAN_POINT('Ctrl Pts',(8.75368184809586,22.9552890194459,-5.17008075806301));
#84224=CARTESIAN_POINT('Ctrl Pts',(8.78181074280473,23.1007268256194,-5.25573050052658));
#84225=CARTESIAN_POINT('Ctrl Pts',(8.80993963751361,23.2497768279433,-5.33523720429478));
#84226=CARTESIAN_POINT('Ctrl Pts',(8.83806853222248,23.4019043463697,-5.40831757338522));
#84227=CARTESIAN_POINT('Ctrl Pts',(8.86620108713286,23.554051660006,-5.48140745187444));
#84228=CARTESIAN_POINT('Ctrl Pts',(8.89433364204323,23.7092770144246,-5.54806919311663));
#84229=CARTESIAN_POINT('Ctrl Pts',(8.92246619695361,23.8670232865689,-5.60806654204109));
#84230=CARTESIAN_POINT('Ctrl Pts',(8.93141916540225,23.9172248200556,-5.62716023522444));
#84231=CARTESIAN_POINT('Ctrl Pts',(8.94037213385088,23.9676815158992,-5.64557933645468));
#84232=CARTESIAN_POINT('Ctrl Pts',(8.94932510229951,24.0183750162368,-5.66331726320585));
#84233=CARTESIAN_POINT('Ctrl Pts',(8.97719914199932,24.1762034112589,-5.71854226229871));
#84234=CARTESIAN_POINT('Ctrl Pts',(9.00507318169912,24.3363638091913,-5.76717319154773));
#84235=CARTESIAN_POINT('Ctrl Pts',(9.03294722139892,24.4982889653192,-5.8090329632666));
#84236=CARTESIAN_POINT('Ctrl Pts',(9.06081722659187,24.6601906842935,-5.85088667617456));
#84237=CARTESIAN_POINT('Ctrl Pts',(9.08868723178481,24.8238563441035,-5.88597110800244));
#84238=CARTESIAN_POINT('Ctrl Pts',(9.11655723697776,24.9887053523151,-5.91415954600176));
#84239=CARTESIAN_POINT('Ctrl Pts',(9.14442900138379,25.1535647661413,-5.94234976331433));
#84240=CARTESIAN_POINT('Ctrl Pts',(9.17230076578983,25.3196073648312,-5.96364306054573));
#84241=CARTESIAN_POINT('Ctrl Pts',(9.20017253019587,25.4862434973884,-5.97796405610006));
#84242=CARTESIAN_POINT('Ctrl Pts',(9.22804377704257,25.6528765356282,-5.99228478572342));
#84243=CARTESIAN_POINT('Ctrl Pts',(9.25591502388926,25.8201027688212,-5.99963344784175));
#84244=CARTESIAN_POINT('Ctrl Pts',(9.28378627073596,25.9873283575251,-5.99998661910815));
#84245=CARTESIAN_POINT('Ctrl Pts',(9.31166341799586,26.1545893483077,-6.00033986514181));
#84246=CARTESIAN_POINT('Ctrl Pts',(9.33954056525577,26.3218493764439,-5.99369466172522));
#84247=CARTESIAN_POINT('Ctrl Pts',(9.36741771251567,26.4885147662724,-5.98007970876089));
#84248=CARTESIAN_POINT('Ctrl Pts',(9.37765315928123,26.5497080694948,-5.97508080679352));
#84249=CARTESIAN_POINT('Ctrl Pts',(9.38788860604678,26.6108212395971,-5.96914283018167));
#84250=CARTESIAN_POINT('Ctrl Pts',(9.39812405281234,26.6718250404551,-5.96226895695066));
#84251=CARTESIAN_POINT('Ctrl Pts',(9.42611042972821,26.8386253182754,-5.94347399748075));
#84252=CARTESIAN_POINT('Ctrl Pts',(9.45409680664407,27.0046601922689,-5.91767244072537));
#84253=CARTESIAN_POINT('Ctrl Pts',(9.48208318355993,27.1693372600206,-5.88495117841495));
#84254=CARTESIAN_POINT('Ctrl Pts',(9.51006461450599,27.3339852247624,-5.85223569886003));
#84255=CARTESIAN_POINT('Ctrl Pts',(9.53804604545205,27.4972755556528,-5.81260301525687));
#84256=CARTESIAN_POINT('Ctrl Pts',(9.56602747639812,27.6586256298888,-5.76619120562924));
#84257=CARTESIAN_POINT('Ctrl Pts',(9.59400834442122,27.819972458127,-5.71978032970201));
#84258=CARTESIAN_POINT('Ctrl Pts',(9.62198921244433,27.979378806388,-5.66659068357769));
#84259=CARTESIAN_POINT('Ctrl Pts',(9.64997008046744,28.1362761222771,-5.60681053089799));
#84260=CARTESIAN_POINT('Ctrl Pts',(9.67794881712259,28.2931614869319,-5.54703493181189));
#84261=CARTESIAN_POINT('Ctrl Pts',(9.70592755377774,28.4475379092945,-5.48066994143182));
#84262=CARTESIAN_POINT('Ctrl Pts',(9.73390629043289,28.5988554537139,-5.40795250817734));
#84263=CARTESIAN_POINT('Ctrl Pts',(9.76188778115008,28.750187892941,-5.33522791704707));
#84264=CARTESIAN_POINT('Ctrl Pts',(9.78986927186726,28.8984605708052,-5.25614976907949));
#84265=CARTESIAN_POINT('Ctrl Pts',(9.81785076258445,29.0431461839619,-5.17100196316323));
#84266=CARTESIAN_POINT('Ctrl Pts',(9.82754150949802,29.0932547244006,-5.14151297539912));
#84267=CARTESIAN_POINT('Ctrl Pts',(9.8372322564116,29.1429332435305,-5.11129638076745));
#84268=CARTESIAN_POINT('Ctrl Pts',(9.84692300332517,29.1921605680295,-5.08036523371278));
#84269=CARTESIAN_POINT('Ctrl Pts',(9.87501419887874,29.3348590010206,-4.99070311495582));
#84270=CARTESIAN_POINT('Ctrl Pts',(9.90310539443231,29.4737906803365,-4.89501678685941));
#84271=CARTESIAN_POINT('Ctrl Pts',(9.93119658998587,29.60845675826,-4.79364577579194));
#84272=CARTESIAN_POINT('Ctrl Pts',(9.95928583520492,29.7431134864959,-4.69228180277956));
#84273=CARTESIAN_POINT('Ctrl Pts',(9.98737508042397,29.8735049579827,-4.58523411793288));
#84274=CARTESIAN_POINT('Ctrl Pts',(10.015464325643,29.9991634074874,-4.47288408526466));
#84275=CARTESIAN_POINT('Ctrl Pts',(10.034083709733,30.0824580249553,-4.39841115463005));
#84276=CARTESIAN_POINT('Ctrl Pts',(10.0527030938231,30.1636736421363,-4.32160928184441));
#84277=CARTESIAN_POINT('Ctrl Pts',(10.0713224779131,30.2426823068249,-4.24259906700534));
#84278=CARTESIAN_POINT('Origin',(-31.4159265358979,26.,7.7715611723761E-15));
#84279=CARTESIAN_POINT('',(17.341,30.2426406871193,-4.24264068711928));
#84280=CARTESIAN_POINT('',(16.354507877922,30.2426778922245,-4.24260348168784));
#84281=CARTESIAN_POINT('',(-31.4159265358979,30.2426406871193,-4.24264068711928));
#84282=CARTESIAN_POINT('',(17.341,25.540762340228,-5.98239924878364));
#84283=CARTESIAN_POINT('Origin',(17.341,26.,7.7715611723761E-15));
#84284=CARTESIAN_POINT('',(16.6322163269923,21.7573593180495,-4.24264068195053));
#84285=CARTESIAN_POINT('Ctrl Pts',(17.341,25.540762340228,-5.98239924878364));
#84286=CARTESIAN_POINT('Ctrl Pts',(17.2225532411293,24.8321665389389,-5.92800403643227));
#84287=CARTESIAN_POINT('Ctrl Pts',(17.1059809364002,24.1388327450978,-5.748143051765));
#84288=CARTESIAN_POINT('Ctrl Pts',(16.8692225121782,22.847541981894,-5.15431362704027));
#84289=CARTESIAN_POINT('Ctrl Pts',(16.750641223211,22.2597933862528,-4.74507476049141));
#84290=CARTESIAN_POINT('Ctrl Pts',(16.6322163764174,21.7573593128807,-4.24264068711927));
#84291=CARTESIAN_POINT('',(13.4906236300072,30.2426406871193,4.24264068711929));
#84292=CARTESIAN_POINT('Ctrl Pts',(16.632216283597,21.7573593128807,-4.24264068711927));
#84293=CARTESIAN_POINT('Ctrl Pts',(16.6042913968638,21.6388840522434,-4.12416542648196));
#84294=CARTESIAN_POINT('Ctrl Pts',(16.5763665101307,21.5253621514006,-4.00071215862345));
#84295=CARTESIAN_POINT('Ctrl Pts',(16.5484416233975,21.4171998487376,-3.87271775031295));
#84296=CARTESIAN_POINT('Ctrl Pts',(16.5205196696009,21.3090489063057,-3.74473678518948));
#84297=CARTESIAN_POINT('Ctrl Pts',(16.4925977158043,21.2062566416934,-3.6122158724385));
#84298=CARTESIAN_POINT('Ctrl Pts',(16.4646757620076,21.1091896105983,-3.47562566093074));
#84299=CARTESIAN_POINT('Ctrl Pts',(16.436750905734,21.0121124894206,-3.33902125092011));
#84300=CARTESIAN_POINT('Ctrl Pts',(16.4088260494604,20.9207619755784,-3.19834695246211));
#84301=CARTESIAN_POINT('Ctrl Pts',(16.3809011931868,20.8354622534116,-3.05410377427876));
#84302=CARTESIAN_POINT('Ctrl Pts',(16.3529763239393,20.7501624916145,-2.90986052907979));
#84303=CARTESIAN_POINT('Ctrl Pts',(16.3250514546917,20.6709136847872,-2.76204867382332));
#84304=CARTESIAN_POINT('Ctrl Pts',(16.2971265854442,20.5979949749762,-2.61119545603485));
#84305=CARTESIAN_POINT('Ctrl Pts',(16.2691954467488,20.5250598940929,-2.46030836999875));
#84306=CARTESIAN_POINT('Ctrl Pts',(16.2412643080534,20.4584578858779,-2.30637884153029));
#84307=CARTESIAN_POINT('Ctrl Pts',(16.213333169358,20.398421033345,-2.14995652986948));
#84308=CARTESIAN_POINT('Ctrl Pts',(16.2033612239334,20.3769867401194,-2.09411080255835));
#84309=CARTESIAN_POINT('Ctrl Pts',(16.1933892785088,20.3563888110039,-2.0379475223848));
#84310=CARTESIAN_POINT('Ctrl Pts',(16.1834173330842,20.3366363029578,-1.98149227478286));
#84311=CARTESIAN_POINT('Ctrl Pts',(16.1554166241976,20.2811722782334,-1.82296884872001));
#84312=CARTESIAN_POINT('Ctrl Pts',(16.127415915311,20.2323607377876,-1.66209389997231));
#84313=CARTESIAN_POINT('Ctrl Pts',(16.0994152064245,20.1903803043503,-1.49943955927496));
#84314=CARTESIAN_POINT('Ctrl Pts',(16.0714192091262,20.1484069348241,-1.33681258789509));
#84315=CARTESIAN_POINT('Ctrl Pts',(16.043423211828,20.1132624561311,-1.17240712404425));
#84316=CARTESIAN_POINT('Ctrl Pts',(16.0154272145297,20.0850751222934,-1.00680866657375));
#84317=CARTESIAN_POINT('Ctrl Pts',(15.987431571927,20.0568881455754,-0.84121230715428));
#84318=CARTESIAN_POINT('Ctrl Pts',(15.9594359293243,20.0356581929918,-0.674423291272229));
#84319=CARTESIAN_POINT('Ctrl Pts',(15.9314402867215,20.0214621940045,-0.507036194252439));
#84320=CARTESIAN_POINT('Ctrl Pts',(15.9034466944445,20.0072672346939,-0.339661356213942));
#84321=CARTESIAN_POINT('Ctrl Pts',(15.8754531021674,20.0001052249912,-0.171688835435331));
#84322=CARTESIAN_POINT('Ctrl Pts',(15.8474595098903,20.0000011516745,-0.00371753860386348));
#84323=CARTESIAN_POINT('Ctrl Pts',(15.8194631574341,19.9998970680962,0.164270320263236));
#84324=CARTESIAN_POINT('Ctrl Pts',(15.7914668049778,20.0068523115617,0.332256642999523));
#84325=CARTESIAN_POINT('Ctrl Pts',(15.7634704525216,20.0208397482382,0.499642555985247));
#84326=CARTESIAN_POINT('Ctrl Pts',(15.7538530958715,20.0256447372934,0.557143261689614));
#84327=CARTESIAN_POINT('Ctrl Pts',(15.7442357392215,20.0312791241108,0.614573137971777));
#84328=CARTESIAN_POINT('Ctrl Pts',(15.7346183825714,20.037740393227,0.671908015611504));
#84329=CARTESIAN_POINT('Ctrl Pts',(15.7066973281163,20.0564987125248,0.838362302272619));
#84330=CARTESIAN_POINT('Ctrl Pts',(15.6787762736612,20.0822340439421,1.00404913498184));
#84331=CARTESIAN_POINT('Ctrl Pts',(15.6508552192062,20.1148584484018,1.16837875607722));
#84332=CARTESIAN_POINT('Ctrl Pts',(15.6229373718183,20.1474791055584,1.3326895019496));
#84333=CARTESIAN_POINT('Ctrl Pts',(15.5950195244303,20.1869871947943,1.49564303801235));
#84334=CARTESIAN_POINT('Ctrl Pts',(15.5671016770424,20.2332436180977,1.65665954009544));
#84335=CARTESIAN_POINT('Ctrl Pts',(15.5391812737269,20.2795042762573,1.81769078352007));
#84336=CARTESIAN_POINT('Ctrl Pts',(15.5112608704114,20.3325144183481,1.97678433460715));
#84337=CARTESIAN_POINT('Ctrl Pts',(15.4833404670958,20.3920847868941,2.13337454813151));
#84338=CARTESIAN_POINT('Ctrl Pts',(15.4554202348681,20.4516547904109,2.28996380211851));
#84339=CARTESIAN_POINT('Ctrl Pts',(15.4275000026403,20.5177848250248,2.44404945535309));
#84340=CARTESIAN_POINT('Ctrl Pts',(15.3995797704125,20.5902370265517,2.59508469439968));
#84341=CARTESIAN_POINT('Ctrl Pts',(15.3716534889113,20.6627049257695,2.74615265715181));
#84342=CARTESIAN_POINT('Ctrl Pts',(15.3437272074102,20.7414975912157,2.89416860115279));
#84343=CARTESIAN_POINT('Ctrl Pts',(15.315800925909,20.8263302876324,3.03860851498343));
#84344=CARTESIAN_POINT('Ctrl Pts',(15.3058070946255,20.8566889179167,3.09029846623458));
#84345=CARTESIAN_POINT('Ctrl Pts',(15.295813263342,20.887820653669,3.14153068128663));
#84346=CARTESIAN_POINT('Ctrl Pts',(15.2858194320586,20.9197110486647,3.19228196920965));
#84347=CARTESIAN_POINT('Ctrl Pts',(15.2578615192377,21.0089249705158,3.33425955949041));
#84348=CARTESIAN_POINT('Ctrl Pts',(15.2299036064168,21.1041081373684,3.4725170175672));
#84349=CARTESIAN_POINT('Ctrl Pts',(15.2019456935959,21.2049262970795,3.60655905033598));
#84350=CARTESIAN_POINT('Ctrl Pts',(15.1739930471236,21.3057254659747,3.74057583400706));
#84351=CARTESIAN_POINT('Ctrl Pts',(15.1460404006513,21.4121573208104,3.87037852614376));
#84352=CARTESIAN_POINT('Ctrl Pts',(15.118087754179,21.5238457096574,3.99550281805025));
#84353=CARTESIAN_POINT('Ctrl Pts',(15.090135879103,21.6355310162916,4.12062365695957));
#84354=CARTESIAN_POINT('Ctrl Pts',(15.062184004027,21.7524723605252,4.24106611711228));
#84355=CARTESIAN_POINT('Ctrl Pts',(15.0342321289509,21.8742544598873,4.3564003188688));
#84356=CARTESIAN_POINT('Ctrl Pts',(15.0062824307059,21.9960270751254,4.4717255386496));
#84357=CARTESIAN_POINT('Ctrl Pts',(14.9783327324608,22.1226394636412,4.58194307964691));
#84358=CARTESIAN_POINT('Ctrl Pts',(14.9503830342157,22.2536405425231,4.68666094521177));
#84359=CARTESIAN_POINT('Ctrl Pts',(14.9224304330414,22.384655227522,4.79138968704997));
#84360=CARTESIAN_POINT('Ctrl Pts',(14.8944778318671,22.5200592683346,4.89061741606617));
#84361=CARTESIAN_POINT('Ctrl Pts',(14.8665252306927,22.6593690919098,4.9839928908369));
#84362=CARTESIAN_POINT('Ctrl Pts',(14.8566903143104,22.7083842249757,5.01684636235471));
#84363=CARTESIAN_POINT('Ctrl Pts',(14.8468553979281,22.7578825927692,5.04897574751083));
#84364=CARTESIAN_POINT('Ctrl Pts',(14.8370204815457,22.8078422705463,5.0803670172822));
#84365=CARTESIAN_POINT('Ctrl Pts',(14.8090390532225,22.9499830970086,5.1696786627439));
#84366=CARTESIAN_POINT('Ctrl Pts',(14.7810576248992,23.0958875944494,5.25302957654209));
#84367=CARTESIAN_POINT('Ctrl Pts',(14.753076196576,23.2450373241744,5.33012013511967));
#84368=CARTESIAN_POINT('Ctrl Pts',(14.725097566022,23.3941721409177,5.40720298567058));
#84369=CARTESIAN_POINT('Ctrl Pts',(14.697118935468,23.5465512644704,5.47802658718934));
#84370=CARTESIAN_POINT('Ctrl Pts',(14.669140304914,23.7016321781138,5.54233753531108));
#84371=CARTESIAN_POINT('Ctrl Pts',(14.6411590636731,23.8567275623619,5.60665448428935));
#84372=CARTESIAN_POINT('Ctrl Pts',(14.6131778224323,24.0145249525328,5.66445744360224));
#84373=CARTESIAN_POINT('Ctrl Pts',(14.5851965811914,24.1744616792911,5.71554108021484));
#84374=CARTESIAN_POINT('Ctrl Pts',(14.557215631288,24.3343967408066,5.76662418495049));
#84375=CARTESIAN_POINT('Ctrl Pts',(14.5292346813846,24.496470795692,5.81098801437962));
#84376=CARTESIAN_POINT('Ctrl Pts',(14.5012537314812,24.6601055990544,5.8484769807459));
#84377=CARTESIAN_POINT('Ctrl Pts',(14.4732673595621,24.8237721107926,5.88597321154622));
#84378=CARTESIAN_POINT('Ctrl Pts',(14.445280987643,24.988999670261,5.91659184866194));
#84379=CARTESIAN_POINT('Ctrl Pts',(14.4172946157239,25.1551986321962,5.94022816472204));
#84380=CARTESIAN_POINT('Ctrl Pts',(14.4076035874936,25.2127494585993,5.94841287000867));
#84381=CARTESIAN_POINT('Ctrl Pts',(14.3979125592632,25.2704166874997,5.95576079462521));
#84382=CARTESIAN_POINT('Ctrl Pts',(14.3882215310329,25.3281756306374,5.96226903256895));
#84383=CARTESIAN_POINT('Ctrl Pts',(14.360344049786,25.4943266123377,5.98099081078627));
#84384=CARTESIAN_POINT('Ctrl Pts',(14.3324665685392,25.6612892760491,5.99276628493692));
#84385=CARTESIAN_POINT('Ctrl Pts',(14.3045890872924,25.8284713291035,5.99754765842345));
#84386=CARTESIAN_POINT('Ctrl Pts',(14.2767169872715,25.9956211107917,6.00232810895532));
#84387=CARTESIAN_POINT('Ctrl Pts',(14.2488448872507,26.1629898798038,6.00011714374974));
#84388=CARTESIAN_POINT('Ctrl Pts',(14.2209727872298,26.3299833962866,5.99091904119687));
#84389=CARTESIAN_POINT('Ctrl Pts',(14.1931009237254,26.4969754956996,5.98172101669706));
#84390=CARTESIAN_POINT('Ctrl Pts',(14.165229060221,26.6635920314603,5.96553598726662));
#84391=CARTESIAN_POINT('Ctrl Pts',(14.1373571967166,26.8292412520957,5.94242029360283));
#84392=CARTESIAN_POINT('Ctrl Pts',(14.1094870061456,26.9948805300838,5.91930598739617));
#84393=CARTESIAN_POINT('Ctrl Pts',(14.0816168155746,27.1595522944168,5.88926189348339));
#84394=CARTESIAN_POINT('Ctrl Pts',(14.0537466250035,27.3226721168271,5.85239595989269));
#84395=CARTESIAN_POINT('Ctrl Pts',(14.0258722195373,27.4858166083534,5.81552445095265));
#84396=CARTESIAN_POINT('Ctrl Pts',(13.997997814071,27.64740837908,5.7718291114696));
#84397=CARTESIAN_POINT('Ctrl Pts',(13.9701234086047,27.8068746389096,5.72146869599629));
#84398=CARTESIAN_POINT('Ctrl Pts',(13.9598897992432,27.8654199381597,5.70297973414695));
#84399=CARTESIAN_POINT('Ctrl Pts',(13.9496561898816,27.9236788860339,5.68359289742922));
#84400=CARTESIAN_POINT('Ctrl Pts',(13.9394225805201,27.9816236668422,5.66331772400341));
#84401=CARTESIAN_POINT('Ctrl Pts',(13.9112904383807,28.140913586199,5.60758137130876));
#84402=CARTESIAN_POINT('Ctrl Pts',(13.8831582962414,28.2978640435168,5.54511577331456));
#84403=CARTESIAN_POINT('Ctrl Pts',(13.8550261541021,28.4519117338169,5.47614178501354));
#84404=CARTESIAN_POINT('Ctrl Pts',(13.826897483734,28.6059404131814,5.40717630875217));
#84405=CARTESIAN_POINT('Ctrl Pts',(13.7987688133659,28.7570667621176,5.33170417045857));
#84406=CARTESIAN_POINT('Ctrl Pts',(13.7706401429978,28.9047485808636,5.24999387446985));
#84407=CARTESIAN_POINT('Ctrl Pts',(13.7425113164897,29.0524312193798,5.16828312491369));
#84408=CARTESIAN_POINT('Ctrl Pts',(13.7143824899816,29.196669021128,5.08033429409493));
#84409=CARTESIAN_POINT('Ctrl Pts',(13.6862536634735,29.3369447894087,4.98646161846638));
#84410=CARTESIAN_POINT('Ctrl Pts',(13.6581269842118,29.4772098495769,4.89259610871675));
#84411=CARTESIAN_POINT('Ctrl Pts',(13.63000030495,29.613513227398,4.79280782832254));
#84412=CARTESIAN_POINT('Ctrl Pts',(13.6018736256883,29.7453667698052,4.68745429413868));
#84413=CARTESIAN_POINT('Ctrl Pts',(13.5737453734725,29.8772276859791,4.58209486817239));
#84414=CARTESIAN_POINT('Ctrl Pts',(13.5456171212566,30.0046380308218,4.47116975696162));
#84415=CARTESIAN_POINT('Ctrl Pts',(13.5174888690408,30.1271421914849,4.35507719004676));
#84416=CARTESIAN_POINT('Ctrl Pts',(13.5085337893629,30.1661433534195,4.31811726168885));
#84417=CARTESIAN_POINT('Ctrl Pts',(13.4995787096851,30.2046475017216,4.28063387251699));
#84418=CARTESIAN_POINT('Ctrl Pts',(13.4906236300072,30.2426406871193,4.24264068711928));
#84419=CARTESIAN_POINT('Ctrl Pts',(13.4906236300072,30.2426406871193,4.24264068711928));
#84420=CARTESIAN_POINT('Ctrl Pts',(13.4626987432741,30.3611159477566,4.12416542648202));
#84421=CARTESIAN_POINT('Ctrl Pts',(13.4347738565409,30.4746378485994,4.00071215862355));
#84422=CARTESIAN_POINT('Ctrl Pts',(13.4068489698078,30.5828001512623,3.8727177503131));
#84423=CARTESIAN_POINT('Ctrl Pts',(13.3789270160111,30.6909510936942,3.74473678518955));
#84424=CARTESIAN_POINT('Ctrl Pts',(13.3510050622145,30.7937433583066,3.61221587243848));
#84425=CARTESIAN_POINT('Ctrl Pts',(13.3230831084178,30.8908103894018,3.47562566093063));
#84426=CARTESIAN_POINT('Ctrl Pts',(13.2951582521442,30.9878875105796,3.3390212509199));
#84427=CARTESIAN_POINT('Ctrl Pts',(13.2672333958706,31.0792380244218,3.1983469524618));
#84428=CARTESIAN_POINT('Ctrl Pts',(13.2393085395969,31.1645377465886,3.05410377427835));
#84429=CARTESIAN_POINT('Ctrl Pts',(13.2113836703494,31.2498375083858,2.90986052907932));
#84430=CARTESIAN_POINT('Ctrl Pts',(13.1834588011019,31.3290863152131,2.76204867382277));
#84431=CARTESIAN_POINT('Ctrl Pts',(13.1555339318543,31.4020050250242,2.61119545603423));
#84432=CARTESIAN_POINT('Ctrl Pts',(13.1276027931589,31.4749401059074,2.46030836999807));
#84433=CARTESIAN_POINT('Ctrl Pts',(13.0996716544635,31.5415421141224,2.30637884152955));
#84434=CARTESIAN_POINT('Ctrl Pts',(13.071740515768,31.6015789666553,2.14995652986867));
#84435=CARTESIAN_POINT('Ctrl Pts',(13.0617685703435,31.6230132598808,2.09411080255781));
#84436=CARTESIAN_POINT('Ctrl Pts',(13.0517966249189,31.6436111889962,2.03794752238453));
#84437=CARTESIAN_POINT('Ctrl Pts',(13.0418246794944,31.6633636970422,1.98149227478286));
#84438=CARTESIAN_POINT('Ctrl Pts',(13.0138239706077,31.7188277217667,1.82296884871973));
#84439=CARTESIAN_POINT('Ctrl Pts',(12.9858232617211,31.7676392622126,1.66209389997174));
#84440=CARTESIAN_POINT('Ctrl Pts',(12.9578225528345,31.80961969565,1.49943955927409));
#84441=CARTESIAN_POINT('Ctrl Pts',(12.9298265555361,31.8515930651763,1.3368125878935));
#84442=CARTESIAN_POINT('Ctrl Pts',(12.9018305582378,31.8867375438694,1.17240712404193));
#84443=CARTESIAN_POINT('Ctrl Pts',(12.8738345609394,31.9149248777071,1.00680866657069));
#84444=CARTESIAN_POINT('Ctrl Pts',(12.8458389183366,31.943111854425,0.841212307151039));
#84445=CARTESIAN_POINT('Ctrl Pts',(12.8178432757339,31.9643418070086,0.674423291268812));
#84446=CARTESIAN_POINT('Ctrl Pts',(12.7898476331311,31.9785378059958,0.507036194248846));
#84447=CARTESIAN_POINT('Ctrl Pts',(12.761854040854,31.9927327653063,0.339661356210217));
#84448=CARTESIAN_POINT('Ctrl Pts',(12.7338604485769,31.9998947750089,0.171688835431475));
#84449=CARTESIAN_POINT('Ctrl Pts',(12.7058668562998,31.9999988483255,0.00371753859988222));
#84450=CARTESIAN_POINT('Ctrl Pts',(12.6778705038436,32.0001029319037,-0.164270320267365));
#84451=CARTESIAN_POINT('Ctrl Pts',(12.6498741513873,31.9931476884381,-0.33225664300379));
#84452=CARTESIAN_POINT('Ctrl Pts',(12.621877798931,31.9791602517615,-0.49964255598965));
#84453=CARTESIAN_POINT('Ctrl Pts',(12.6122604422812,31.9743552627063,-0.557143261692545));
#84454=CARTESIAN_POINT('Ctrl Pts',(12.6026430856314,31.9687208758891,-0.614573137973243));
#84455=CARTESIAN_POINT('Ctrl Pts',(12.5930257289816,31.962259606773,-0.671908015611506));
#84456=CARTESIAN_POINT('Ctrl Pts',(12.5651046745265,31.9435012874752,-0.838362302272481));
#84457=CARTESIAN_POINT('Ctrl Pts',(12.5371836200715,31.9177659560579,-1.00404913498156));
#84458=CARTESIAN_POINT('Ctrl Pts',(12.5092625656164,31.8851415515983,-1.16837875607681));
#84459=CARTESIAN_POINT('Ctrl Pts',(12.4813447182285,31.8525208944417,-1.33268950194925));
#84460=CARTESIAN_POINT('Ctrl Pts',(12.4534268708406,31.8130128052057,-1.49564303801208));
#84461=CARTESIAN_POINT('Ctrl Pts',(12.4255090234527,31.7667563819023,-1.65665954009523));
#84462=CARTESIAN_POINT('Ctrl Pts',(12.3975886201371,31.7204957237428,-1.81769078351988));
#84463=CARTESIAN_POINT('Ctrl Pts',(12.3696682168216,31.667485581652,-1.97678433460697));
#84464=CARTESIAN_POINT('Ctrl Pts',(12.3417478135061,31.607915213106,-2.13337454813135));
#84465=CARTESIAN_POINT('Ctrl Pts',(12.3138275812784,31.5483452095893,-2.28996380211801));
#84466=CARTESIAN_POINT('Ctrl Pts',(12.2859073490507,31.4822151749755,-2.44404945535227));
#84467=CARTESIAN_POINT('Ctrl Pts',(12.2579871168229,31.4097629734489,-2.59508469439855));
#84468=CARTESIAN_POINT('Ctrl Pts',(12.2300608353218,31.3372950742311,-2.74615265715067));
#84469=CARTESIAN_POINT('Ctrl Pts',(12.2021345538206,31.2585024087849,-2.89416860115163));
#84470=CARTESIAN_POINT('Ctrl Pts',(12.1742082723194,31.1736697123683,-3.03860851498227));
#84471=CARTESIAN_POINT('Ctrl Pts',(12.1642144410358,31.1433110820838,-3.09029846623381));
#84472=CARTESIAN_POINT('Ctrl Pts',(12.1542206097523,31.1121793463313,-3.14153068128624));
#84473=CARTESIAN_POINT('Ctrl Pts',(12.1442267784688,31.0802889513353,-3.19228196920963));
#84474=CARTESIAN_POINT('Ctrl Pts',(12.1158381645934,30.9897006589988,-3.33644677204223));
#84475=CARTESIAN_POINT('Ctrl Pts',(12.087449550718,30.8929631649647,-3.47676763811165));
#84476=CARTESIAN_POINT('Ctrl Pts',(12.0590609368427,30.7904223170505,-3.6127349784207));
#84477=CARTESIAN_POINT('Ctrl Pts',(12.0306784629411,30.6879036469758,-3.74867291130908));
#84478=CARTESIAN_POINT('Ctrl Pts',(12.0022959890396,30.5795843045573,-3.88025896473511));
#84479=CARTESIAN_POINT('Ctrl Pts',(11.9739135151381,30.4658519791244,-4.00701461197116));
#84480=CARTESIAN_POINT('Ctrl Pts',(11.9558847780552,30.3936084460142,-4.08753064611678));
#84481=CARTESIAN_POINT('Ctrl Pts',(11.9378560409723,30.3191816788964,-4.16609830040219));
#84482=CARTESIAN_POINT('Ctrl Pts',(11.9198273038894,30.2426793568795,-4.24260201700657));
#84483=CARTESIAN_POINT('',(11.6421188053765,30.2426406871193,4.24264068711929));
#84484=CARTESIAN_POINT('Ctrl Pts',(10.0713224779131,30.2426823068249,-4.24259906700533));
#84485=CARTESIAN_POINT('Ctrl Pts',(10.099702075706,30.3631070273837,-4.12217198371286));
#84486=CARTESIAN_POINT('Ctrl Pts',(10.1280816734989,30.4783868213669,-3.99662894535352));
#84487=CARTESIAN_POINT('Ctrl Pts',(10.1564612712918,30.5881087732421,-3.86642701791961));
#84488=CARTESIAN_POINT('Ctrl Pts',(10.1848494148972,30.6978637651638,-3.73618588340214));
#84489=CARTESIAN_POINT('Ctrl Pts',(10.2132375585026,30.8020573826946,-3.60128328063448));
#84490=CARTESIAN_POINT('Ctrl Pts',(10.2416257021081,30.900316749403,-3.46220966371485));
#84491=CARTESIAN_POINT('Ctrl Pts',(10.259657786018,30.9627308744707,-3.37387042023291));
#84492=CARTESIAN_POINT('Ctrl Pts',(10.277689869928,31.0227514918882,-3.28384892384956));
#84493=CARTESIAN_POINT('Ctrl Pts',(10.295721953838,31.0802919954162,-3.19227712476694));
#84494=CARTESIAN_POINT('Ctrl Pts',(10.3236482024984,31.1694048465757,-3.05046008108918));
#84495=CARTESIAN_POINT('Ctrl Pts',(10.3515744511589,31.2525905179036,-2.90488583932461));
#84496=CARTESIAN_POINT('Ctrl Pts',(10.3795006998193,31.3295481080712,-2.75606911447355));
#84497=CARTESIAN_POINT('Ctrl Pts',(10.4074214795192,31.406490627184,-2.60728153327165));
#84498=CARTESIAN_POINT('Ctrl Pts',(10.4353422592191,31.4772073541776,-2.45525301625694));
#84499=CARTESIAN_POINT('Ctrl Pts',(10.463263038919,31.5414434661153,-2.30052261711299));
#84500=CARTESIAN_POINT('Ctrl Pts',(10.4911830300089,31.6056777637326,-2.14579658826009));
#84501=CARTESIAN_POINT('Ctrl Pts',(10.5191030210989,31.6634316878239,-1.98836911978285));
#84502=CARTESIAN_POINT('Ctrl Pts',(10.5470230121888,31.714498403278,-1.82879960600742));
#84503=CARTESIAN_POINT('Ctrl Pts',(10.5749408954179,31.7655612633752,-1.66924213916772));
#84504=CARTESIAN_POINT('Ctrl Pts',(10.6028587786469,31.8099378283379,-1.50754325092965));
#84505=CARTESIAN_POINT('Ctrl Pts',(10.630776661876,31.8474709253391,-1.34427816217983));
#84506=CARTESIAN_POINT('Ctrl Pts',(10.6586977788765,31.8850083698569,-1.18099416218284));
#84507=CARTESIAN_POINT('Ctrl Pts',(10.686618895877,31.9157006919787,-1.01614390674221));
#84508=CARTESIAN_POINT('Ctrl Pts',(10.7145400128776,31.9394415348614,-0.850314208962638));
#84509=CARTESIAN_POINT('Ctrl Pts',(10.7245336433687,31.9479389460255,-0.79095982410671));
#84510=CARTESIAN_POINT('Ctrl Pts',(10.7345272738598,31.9555462855579,-0.731480047082945));
#84511=CARTESIAN_POINT('Ctrl Pts',(10.7445209043508,31.9622602820985,-0.671902022999215));
#84512=CARTESIAN_POINT('Ctrl Pts',(10.7725171760834,31.9810689494521,-0.504999459108853));
#84513=CARTESIAN_POINT('Ctrl Pts',(10.8005134478159,31.992866802328,-0.337291560570467));
#84514=CARTESIAN_POINT('Ctrl Pts',(10.8285097195484,31.9976088364781,-0.169376044941714));
#84515=CARTESIAN_POINT('Ctrl Pts',(10.8565031923509,32.0023503965428,-0.00147731668325168));
#84516=CARTESIAN_POINT('Ctrl Pts',(10.8844966651534,32.0000375374273,0.166628675507197));
#84517=CARTESIAN_POINT('Ctrl Pts',(10.9124901379559,31.9906773440968,0.334342577194388));
#84518=CARTESIAN_POINT('Ctrl Pts',(10.9404860813889,31.9813163246602,0.502071280870899));
#84519=CARTESIAN_POINT('Ctrl Pts',(10.9684820248219,31.9649067431905,0.669407513281637));
#84520=CARTESIAN_POINT('Ctrl Pts',(10.9964779682549,31.9415077390088,0.835754621463946));
#84521=CARTESIAN_POINT('Ctrl Pts',(11.0244735000281,31.9181090788924,1.00209928363357));
#84522=CARTESIAN_POINT('Ctrl Pts',(11.0524690318012,31.8877212475795,1.16745454211118));
#84523=CARTESIAN_POINT('Ctrl Pts',(11.0804645635743,31.850454962582,1.331231283737));
#84524=CARTESIAN_POINT('Ctrl Pts',(11.1084652302525,31.8131818422495,1.49503806508595));
#84525=CARTESIAN_POINT('Ctrl Pts',(11.1364658969307,31.7690278175163,1.65726544707923));
#84526=CARTESIAN_POINT('Ctrl Pts',(11.1644665636089,31.7181543781866,1.81733610188789));
#84527=CARTESIAN_POINT('Ctrl Pts',(11.1740843273605,31.7006801970778,1.87231771211886));
#84528=CARTESIAN_POINT('Ctrl Pts',(11.1837020911121,31.6824136882439,1.92704499564975));
#84529=CARTESIAN_POINT('Ctrl Pts',(11.1933198548636,31.663362748889,1.98149498472647));
#84530=CARTESIAN_POINT('Ctrl Pts',(11.2212515038255,31.6080355268652,2.13962716806498));
#84531=CARTESIAN_POINT('Ctrl Pts',(11.2491831527874,31.5460718260323,2.29546734104631));
#84532=CARTESIAN_POINT('Ctrl Pts',(11.2771148017493,31.4776864184661,2.44845900536477));
#84533=CARTESIAN_POINT('Ctrl Pts',(11.3050407969019,31.4093148531923,2.60141970174108));
#84534=CARTESIAN_POINT('Ctrl Pts',(11.3329667920545,31.3345243036091,2.75153275242724));
#84535=CARTESIAN_POINT('Ctrl Pts',(11.3608927872071,31.2535773064315,2.89826249421055));
#84536=CARTESIAN_POINT('Ctrl Pts',(11.3888176576472,31.1726335693742,3.04498632648999));
#84537=CARTESIAN_POINT('Ctrl Pts',(11.4167425280873,31.0855340292351,3.18832684446721));
#84538=CARTESIAN_POINT('Ctrl Pts',(11.4446673985274,30.9925870510111,3.32777321013268));
#84539=CARTESIAN_POINT('Ctrl Pts',(11.4725899484745,30.8996477964689,3.4672079881233));
#84540=CARTESIAN_POINT('Ctrl Pts',(11.5005124984216,30.8008622501275,3.60274899853689));
#84541=CARTESIAN_POINT('Ctrl Pts',(11.5284350483687,30.6965821281744,3.73391434198922));
#84542=CARTESIAN_POINT('Ctrl Pts',(11.5563604727484,30.5922912713068,3.86509318800296));
#84543=CARTESIAN_POINT('Ctrl Pts',(11.5842858971281,30.4825049047961,3.99189522028912));
#84544=CARTESIAN_POINT('Ctrl Pts',(11.6122113215079,30.3676155040598,4.11387102480096));
#84545=CARTESIAN_POINT('Ctrl Pts',(11.6221804827974,30.3266008734198,4.15741544697571));
#84546=CARTESIAN_POINT('Ctrl Pts',(11.632149644087,30.2849362564227,4.20034511781583));
#84547=CARTESIAN_POINT('Ctrl Pts',(11.6421188053765,30.2426406871193,4.24264068711928));
#84548=CARTESIAN_POINT('',(14.7837115023615,21.757359307712,-4.24264069228803));
#84549=CARTESIAN_POINT('Ctrl Pts',(11.6421188053765,30.2426406871193,4.24264068711928));
#84550=CARTESIAN_POINT('Ctrl Pts',(11.6702475126086,30.1233006893401,4.36198068489844));
#84551=CARTESIAN_POINT('Ctrl Pts',(11.6983762198408,29.998916654682,4.47628793832936));
#84552=CARTESIAN_POINT('Ctrl Pts',(11.7265049270729,29.8699330958604,4.58515188773117));
#84553=CARTESIAN_POINT('Ctrl Pts',(11.7546318617202,29.7409576651872,4.69400897686061));
#84554=CARTESIAN_POINT('Ctrl Pts',(11.7827587963674,29.6073835226446,4.79742325031584));
#84555=CARTESIAN_POINT('Ctrl Pts',(11.8108857310146,29.4696888345521,4.8950239418602));
#84556=CARTESIAN_POINT('Ctrl Pts',(11.8390153212383,29.3319811461531,4.99263384827642));
#84557=CARTESIAN_POINT('Ctrl Pts',(11.8671449114621,29.1901523828211,5.08442889782491));
#84558=CARTESIAN_POINT('Ctrl Pts',(11.8952745016858,29.0447109805536,5.17008075806332));
#84559=CARTESIAN_POINT('Ctrl Pts',(11.9234033963947,28.8992731743799,5.25573050052698));
#84560=CARTESIAN_POINT('Ctrl Pts',(11.9515322911036,28.7502231720558,5.33523720429525));
#84561=CARTESIAN_POINT('Ctrl Pts',(11.9796611858125,28.5980956536292,5.40831757338576));
#84562=CARTESIAN_POINT('Ctrl Pts',(12.0077937407229,28.445948339993,5.48140745187494));
#84563=CARTESIAN_POINT('Ctrl Pts',(12.0359262956333,28.2907229855743,5.54806919311709));
#84564=CARTESIAN_POINT('Ctrl Pts',(12.0640588505436,28.13297671343,5.60806654204151));
#84565=CARTESIAN_POINT('Ctrl Pts',(12.0730118189922,28.0827751799437,5.62716023522472));
#84566=CARTESIAN_POINT('Ctrl Pts',(12.0819647874408,28.0323184841005,5.64557933645482));
#84567=CARTESIAN_POINT('Ctrl Pts',(12.0909177558893,27.9816249837632,5.66331726320586));
#84568=CARTESIAN_POINT('Ctrl Pts',(12.1187917955891,27.8237965887412,5.71854226229868));
#84569=CARTESIAN_POINT('Ctrl Pts',(12.1466658352889,27.663636190809,5.76717319154767));
#84570=CARTESIAN_POINT('Ctrl Pts',(12.1745398749887,27.5017110346811,5.80903296326652));
#84571=CARTESIAN_POINT('Ctrl Pts',(12.2024098801815,27.3398093157074,5.85088667617435));
#84572=CARTESIAN_POINT('Ctrl Pts',(12.2302798853744,27.176143655898,5.88597110800216));
#84573=CARTESIAN_POINT('Ctrl Pts',(12.2581498905672,27.0112946476869,5.91415954600145));
#84574=CARTESIAN_POINT('Ctrl Pts',(12.2860216549733,26.8464352338608,5.94234976331403));
#84575=CARTESIAN_POINT('Ctrl Pts',(12.3138934193793,26.6803926351711,5.96364306054548));
#84576=CARTESIAN_POINT('Ctrl Pts',(12.3417651837853,26.5137565026141,5.97796405609986));
#84577=CARTESIAN_POINT('Ctrl Pts',(12.3696364306319,26.3471234643744,5.99228478572329));
#84578=CARTESIAN_POINT('Ctrl Pts',(12.3975076774786,26.1798972311815,5.99963344784168));
#84579=CARTESIAN_POINT('Ctrl Pts',(12.4253789243253,26.0126716424776,5.99998661910816));
#84580=CARTESIAN_POINT('Ctrl Pts',(12.4532560715852,25.845410651695,6.0003398651419));
#84581=CARTESIAN_POINT('Ctrl Pts',(12.4811332188451,25.6781506235587,5.99369466172538));
#84582=CARTESIAN_POINT('Ctrl Pts',(12.509010366105,25.5114852337302,5.98007970876112));
#84583=CARTESIAN_POINT('Ctrl Pts',(12.5192458128707,25.4502919305069,5.97508080679371));
#84584=CARTESIAN_POINT('Ctrl Pts',(12.5294812596364,25.3891787604038,5.96914283018179));
#84585=CARTESIAN_POINT('Ctrl Pts',(12.5397167064021,25.3281749595449,5.96226895695067));
#84586=CARTESIAN_POINT('Ctrl Pts',(12.567703083318,25.1613746817244,5.94347399748075));
#84587=CARTESIAN_POINT('Ctrl Pts',(12.5956894602339,24.9953398077307,5.91767244072533));
#84588=CARTESIAN_POINT('Ctrl Pts',(12.6236758371498,24.8306627399789,5.88495117841487));
#84589=CARTESIAN_POINT('Ctrl Pts',(12.6516572680958,24.6660147752372,5.85223569885995));
#84590=CARTESIAN_POINT('Ctrl Pts',(12.6796386990419,24.5027244443468,5.8126030152568));
#84591=CARTESIAN_POINT('Ctrl Pts',(12.7076201299879,24.341374370111,5.76619120562919));
#84592=CARTESIAN_POINT('Ctrl Pts',(12.735600998011,24.1800275418727,5.71978032970193));
#84593=CARTESIAN_POINT('Ctrl Pts',(12.7635818660341,24.0206211936116,5.66659068357758));
#84594=CARTESIAN_POINT('Ctrl Pts',(12.7915627340573,23.8637238777225,5.60681053089786));
#84595=CARTESIAN_POINT('Ctrl Pts',(12.8195414707123,23.7068385130682,5.54703493181191));
#84596=CARTESIAN_POINT('Ctrl Pts',(12.8475202073674,23.5524620907059,5.48066994143202));
#84597=CARTESIAN_POINT('Ctrl Pts',(12.8754989440225,23.401144546287,5.40795250817776));
#84598=CARTESIAN_POINT('Ctrl Pts',(12.9034804347397,23.2498121070596,5.3352279170474));
#84599=CARTESIAN_POINT('Ctrl Pts',(12.931461925457,23.1015394291952,5.25614976907973));
#84600=CARTESIAN_POINT('Ctrl Pts',(12.9594434161742,22.9568538160383,5.17100196316335));
#84601=CARTESIAN_POINT('Ctrl Pts',(12.9691341630878,22.9067452755995,5.1415129753992));
#84602=CARTESIAN_POINT('Ctrl Pts',(12.9788249100014,22.8570667564696,5.11129638076749));
#84603=CARTESIAN_POINT('Ctrl Pts',(12.988515656915,22.8078394319705,5.08036523371278));
#84604=CARTESIAN_POINT('Ctrl Pts',(13.0164680731131,22.6658459741917,4.99114607406818));
#84605=CARTESIAN_POINT('Ctrl Pts',(13.0444204893112,22.5275810196469,4.89596132380272));
#84606=CARTESIAN_POINT('Ctrl Pts',(13.0723729055094,22.3935386215211,4.79514716411706));
#84607=CARTESIAN_POINT('Ctrl Pts',(13.1003223822074,22.2595103194088,4.69434360613489));
#84608=CARTESIAN_POINT('Ctrl Pts',(13.1282718589055,22.1297039381378,4.5879120092559));
#84609=CARTESIAN_POINT('Ctrl Pts',(13.1562213356036,22.0045823550702,4.47623031607892));
#84610=CARTESIAN_POINT('Ctrl Pts',(13.1841734808165,21.879448825847,4.36453795993828));
#84611=CARTESIAN_POINT('Ctrl Pts',(13.2121256260294,21.7590012245333,4.24759471320073));
#84612=CARTESIAN_POINT('Ctrl Pts',(13.2400777712423,21.6436678730077,4.12581754314647));
#84613=CARTESIAN_POINT('Ctrl Pts',(13.2680297331437,21.5283352778435,4.00404117171243));
#84614=CARTESIAN_POINT('Ctrl Pts',(13.2959816950452,21.4181170792243,3.87743117038718));
#84615=CARTESIAN_POINT('Ctrl Pts',(13.3239336569466,21.3134035364645,3.7464401220327));
#84616=CARTESIAN_POINT('Ctrl Pts',(13.3518914166417,21.2086682740303,3.61542190352579));
#84617=CARTESIAN_POINT('Ctrl Pts',(13.3798491763368,21.1094401440338,3.48002106836329));
#84618=CARTESIAN_POINT('Ctrl Pts',(13.4078069360319,21.0160685245648,3.34072253384904));
#84619=CARTESIAN_POINT('Ctrl Pts',(13.4176428264972,20.9832192179079,3.29171556253219));
#84620=CARTESIAN_POINT('Ctrl Pts',(13.4274787169625,20.9510943985716,3.24222643678125));
#84621=CARTESIAN_POINT('Ctrl Pts',(13.4373146074278,20.9197080045838,3.19227712476694));
#84622=CARTESIAN_POINT('Ctrl Pts',(13.4652408560882,20.8305951534243,3.05046008108928));
#84623=CARTESIAN_POINT('Ctrl Pts',(13.4931671047486,20.7474094820965,2.90488583932483));
#84624=CARTESIAN_POINT('Ctrl Pts',(13.521093353409,20.670451891929,2.75606911447389));
#84625=CARTESIAN_POINT('Ctrl Pts',(13.5490141331088,20.5935093728166,2.60728153327268));
#84626=CARTESIAN_POINT('Ctrl Pts',(13.5769349128086,20.5227926458232,2.45525301625869));
#84627=CARTESIAN_POINT('Ctrl Pts',(13.6048556925083,20.4585565338858,2.30052261711549));
#84628=CARTESIAN_POINT('Ctrl Pts',(13.6327756835982,20.3943222362684,2.14579658826282));
#84629=CARTESIAN_POINT('Ctrl Pts',(13.6606956746882,20.3365683121772,1.98836911978582));
#84630=CARTESIAN_POINT('Ctrl Pts',(13.6886156657781,20.285501596723,1.82879960601062));
#84631=CARTESIAN_POINT('Ctrl Pts',(13.716533549007,20.2344387366259,1.66924213917137));
#84632=CARTESIAN_POINT('Ctrl Pts',(13.744451432236,20.1900621716632,1.50754325093376));
#84633=CARTESIAN_POINT('Ctrl Pts',(13.772369315465,20.1525290746619,1.3442781621844));
#84634=CARTESIAN_POINT('Ctrl Pts',(13.8002904324655,20.114991630144,1.18099416218751));
#84635=CARTESIAN_POINT('Ctrl Pts',(13.828211549466,20.0842993080221,1.01614390674698));
#84636=CARTESIAN_POINT('Ctrl Pts',(13.8561326664665,20.0605584651393,0.850314208967497));
#84637=CARTESIAN_POINT('Ctrl Pts',(13.8661262969579,20.0520610539749,0.790959824109951));
#84638=CARTESIAN_POINT('Ctrl Pts',(13.8761199274493,20.0444537144423,0.731480047084558));
#84639=CARTESIAN_POINT('Ctrl Pts',(13.8861135579406,20.0377397179015,0.671902022999197));
#84640=CARTESIAN_POINT('Ctrl Pts',(13.9141098296732,20.0189310505478,0.504999459108637));
#84641=CARTESIAN_POINT('Ctrl Pts',(13.9421061014057,20.007133197672,0.337291560570052));
#84642=CARTESIAN_POINT('Ctrl Pts',(13.9701023731383,20.0023911635219,0.169376044941101));
#84643=CARTESIAN_POINT('Ctrl Pts',(13.9980958459408,19.9976496034572,0.00147731668254816));
#84644=CARTESIAN_POINT('Ctrl Pts',(14.0260893187433,19.9999624625727,-0.166628675507993));
#84645=CARTESIAN_POINT('Ctrl Pts',(14.0540827915458,20.0093226559032,-0.334342577195271));
#84646=CARTESIAN_POINT('Ctrl Pts',(14.0820787349788,20.0186836753399,-0.502071280871779));
#84647=CARTESIAN_POINT('Ctrl Pts',(14.1100746784119,20.0350932568096,-0.669407513282511));
#84648=CARTESIAN_POINT('Ctrl Pts',(14.1380706218449,20.0584922609913,-0.835754621464816));
#84649=CARTESIAN_POINT('Ctrl Pts',(14.166066153618,20.0818909211078,-1.00209928363457));
#84650=CARTESIAN_POINT('Ctrl Pts',(14.1940616853912,20.1122787524207,-1.1674545421123));
#84651=CARTESIAN_POINT('Ctrl Pts',(14.2220572171643,20.1495450374183,-1.33123128373824));
#84652=CARTESIAN_POINT('Ctrl Pts',(14.2500578838426,20.1868181577509,-1.49503806508736));
#84653=CARTESIAN_POINT('Ctrl Pts',(14.2780585505208,20.2309721824841,-1.65726544708081));
#84654=CARTESIAN_POINT('Ctrl Pts',(14.3060592171991,20.2818456218139,-1.81733610188963));
#84655=CARTESIAN_POINT('Ctrl Pts',(14.3156769809505,20.2993198029226,-1.87231771212));
#84656=CARTESIAN_POINT('Ctrl Pts',(14.325294744702,20.3175863117563,-1.92704499565031));
#84657=CARTESIAN_POINT('Ctrl Pts',(14.3349125084534,20.336637251111,-1.98149498472645));
#84658=CARTESIAN_POINT('Ctrl Pts',(14.3628441574153,20.3919644731347,-2.13962716806488));
#84659=CARTESIAN_POINT('Ctrl Pts',(14.3907758063772,20.4539281739677,-2.29546734104614));
#84660=CARTESIAN_POINT('Ctrl Pts',(14.418707455339,20.5223135815338,-2.44845900536453));
#84661=CARTESIAN_POINT('Ctrl Pts',(14.4466334504916,20.5906851468074,-2.60141970174059));
#84662=CARTESIAN_POINT('Ctrl Pts',(14.4745594456442,20.6654756963905,-2.75153275242649));
#84663=CARTESIAN_POINT('Ctrl Pts',(14.5024854407967,20.7464226935679,-2.89826249420958));
#84664=CARTESIAN_POINT('Ctrl Pts',(14.5304103112368,20.8273664306252,-3.04498632648893));
#84665=CARTESIAN_POINT('Ctrl Pts',(14.5583351816769,20.9144659707642,-3.18832684446607));
#84666=CARTESIAN_POINT('Ctrl Pts',(14.586260052117,21.0074129489881,-3.32777321013146));
#84667=CARTESIAN_POINT('Ctrl Pts',(14.614182602064,21.10035220353,-3.46720798812171));
#84668=CARTESIAN_POINT('Ctrl Pts',(14.642105152011,21.1991377498711,-3.60274899853495));
#84669=CARTESIAN_POINT('Ctrl Pts',(14.670027701958,21.3034178718238,-3.73391434198695));
#84670=CARTESIAN_POINT('Ctrl Pts',(14.6979531263377,21.4077087286912,-3.86509318800059));
#84671=CARTESIAN_POINT('Ctrl Pts',(14.7258785507174,21.5174950952018,-3.99189522028667));
#84672=CARTESIAN_POINT('Ctrl Pts',(14.7538039750971,21.6323844959379,-4.11387102479843));
#84673=CARTESIAN_POINT('Ctrl Pts',(14.7637731363868,21.6733991265786,-4.15741544697404));
#84674=CARTESIAN_POINT('Ctrl Pts',(14.7737422976766,21.7150637435764,-4.200345117815));
#84675=CARTESIAN_POINT('Ctrl Pts',(14.7837114589663,21.7573593128807,-4.24264068711927));
#84676=CARTESIAN_POINT('Ctrl Pts',(14.7837115517867,21.7573593128807,-4.24264068711927));
#84677=CARTESIAN_POINT('Ctrl Pts',(14.8118396368998,21.8766966712322,-4.36197804547074));
#84678=CARTESIAN_POINT('Ctrl Pts',(14.8399677220128,22.0010778773211,-4.47628291578594));
#84679=CARTESIAN_POINT('Ctrl Pts',(14.8680958071259,22.130058445085,-4.58514474815595));
#84680=CARTESIAN_POINT('Ctrl Pts',(14.8962221107649,22.2590308439481,-4.69399968583229));
#84681=CARTESIAN_POINT('Ctrl Pts',(14.9243484144039,22.3926017892773,-4.7974120773116));
#84682=CARTESIAN_POINT('Ctrl Pts',(14.9524747180429,22.5302931406659,-4.89501116549187));
#84683=CARTESIAN_POINT('Ctrl Pts',(14.9806036705035,22.6679974592694,-4.99261944515966));
#84684=CARTESIAN_POINT('Ctrl Pts',(15.0087326229641,22.8098227113067,-5.08441314936828));
#84685=CARTESIAN_POINT('Ctrl Pts',(15.0368615754247,22.9552604861664,-5.17006395443035));
#84686=CARTESIAN_POINT('Ctrl Pts',(15.064989830364,23.1006946545664,-5.25571263558638));
#84687=CARTESIAN_POINT('Ctrl Pts',(15.0931180853034,23.2497409024661,-5.33521856906017));
#84688=CARTESIAN_POINT('Ctrl Pts',(15.1212463402428,23.4018645747706,-5.40829846737105));
#84689=CARTESIAN_POINT('Ctrl Pts',(15.1493782575177,23.5540080537758,-5.48138788078008));
#84690=CARTESIAN_POINT('Ctrl Pts',(15.1775101747925,23.7092294822999,-5.54804945550753));
#84691=CARTESIAN_POINT('Ctrl Pts',(15.2056420920674,23.8669717619628,-5.60804694485841));
#84692=CARTESIAN_POINT('Ctrl Pts',(15.2145982288115,23.9171909280855,-5.62714787259382));
#84693=CARTESIAN_POINT('Ctrl Pts',(15.2235543655555,23.96766544203,-5.64557373131554));
#84694=CARTESIAN_POINT('Ctrl Pts',(15.2325105022996,24.018376925954,-5.66331793142573));
#84695=CARTESIAN_POINT('Ctrl Pts',(15.2603850114755,24.1762081163835,-5.71854384890847));
#84696=CARTESIAN_POINT('Ctrl Pts',(15.2882595206514,24.3363713158732,-5.76717543811175));
#84697=CARTESIAN_POINT('Ctrl Pts',(15.3161340298273,24.4982992551085,-5.80903562330205));
#84698=CARTESIAN_POINT('Ctrl Pts',(15.3440045203059,24.6602038490224,-5.85088977346538));
#84699=CARTESIAN_POINT('Ctrl Pts',(15.3718750107844,24.8238723673531,-5.88597438845085));
#84700=CARTESIAN_POINT('Ctrl Pts',(15.399745501263,24.9887241948697,-5.91416276796285));
#84701=CARTESIAN_POINT('Ctrl Pts',(15.4276177702719,25.1535865422579,-5.94235294629101));
#84702=CARTESIAN_POINT('Ctrl Pts',(15.4554900392808,25.3196320369453,-5.96364595333837));
#84703=CARTESIAN_POINT('Ctrl Pts',(15.4833623082898,25.4862710064242,-5.9779664202101));
#84704=CARTESIAN_POINT('Ctrl Pts',(15.5112340698435,25.6529069419985,-5.99228662635691));
#84705=CARTESIAN_POINT('Ctrl Pts',(15.5391058313972,25.8201360139034,-5.99963452146785));
#84706=CARTESIAN_POINT('Ctrl Pts',(15.566977592951,25.9873643627478,-5.99998669504118));
#84707=CARTESIAN_POINT('Ctrl Pts',(15.594855266211,26.1546281813588,-6.00033894331185));
#84708=CARTESIAN_POINT('Ctrl Pts',(15.622732939471,26.32189095874,-5.99369250574667));
#84709=CARTESIAN_POINT('Ctrl Pts',(15.650610612731,26.4885590004376,-5.98007609509204));
#84710=CARTESIAN_POINT('Ctrl Pts',(15.6608435594248,26.5497371759023,-5.97507797336611));
#84711=CARTESIAN_POINT('Ctrl Pts',(15.6710765061185,26.6108352473121,-5.96914124102974));
#84712=CARTESIAN_POINT('Ctrl Pts',(15.6813094528123,26.6718240007242,-5.96226907410684));
#84713=CARTESIAN_POINT('Ctrl Pts',(15.7092958108749,26.8386237644539,-5.94347420202107));
#84714=CARTESIAN_POINT('Ctrl Pts',(15.7372821689374,27.004658163261,-5.91767277224285));
#84715=CARTESIAN_POINT('Ctrl Pts',(15.765268527,27.1693347969323,-5.88495166782899));
#84716=CARTESIAN_POINT('Ctrl Pts',(15.79324993121,27.3339822812672,-5.85223635536303));
#84717=CARTESIAN_POINT('Ctrl Pts',(15.8212313354199,27.4972721736021,-5.81260387364708));
#84718=CARTESIAN_POINT('Ctrl Pts',(15.8492127396299,27.6586218525161,-5.76619229217652));
#84719=CARTESIAN_POINT('Ctrl Pts',(15.8771935699863,27.8199682224078,-5.71978166253284));
#84720=CARTESIAN_POINT('Ctrl Pts',(15.9051744003426,27.9793741570644,-5.66659229425009));
#84721=CARTESIAN_POINT('Ctrl Pts',(15.933155230699,28.1362711049113,-5.60681244258456));
#84722=CARTESIAN_POINT('Ctrl Pts',(15.9611339235647,28.2931560672036,-5.54703715757685));
#84723=CARTESIAN_POINT('Ctrl Pts',(15.9891126164303,28.447532133851,-5.480672507322));
#84724=CARTESIAN_POINT('Ctrl Pts',(16.017091309296,28.5988493692395,-5.40795543213917));
#84725=CARTESIAN_POINT('Ctrl Pts',(16.0450727479037,28.7501814544316,-5.33523122072833));
#84726=CARTESIAN_POINT('Ctrl Pts',(16.0730541865114,28.8984538267661,-5.25615347420067));
#84727=CARTESIAN_POINT('Ctrl Pts',(16.1010356251191,29.0431391823601,-5.17100608361514));
#84728=CARTESIAN_POINT('Ctrl Pts',(16.1107265511878,29.0932486532825,-5.14151663960646));
#84729=CARTESIAN_POINT('Ctrl Pts',(16.1204174772565,29.1429280911377,-5.11129956078575));
#84730=CARTESIAN_POINT('Ctrl Pts',(16.1301084033251,29.1921563212657,-5.0803679020917));
#84731=CARTESIAN_POINT('Ctrl Pts',(16.1581991428504,29.334852424818,-4.99070741337258));
#84732=CARTESIAN_POINT('Ctrl Pts',(16.1862898823756,29.4737818985722,-4.89502292008477));
#84733=CARTESIAN_POINT('Ctrl Pts',(16.2143806219008,29.6084459130554,-4.79365393959071));
#84734=CARTESIAN_POINT('Ctrl Pts',(16.2424694201627,29.7431006213289,-4.69229196439055));
#84735=CARTESIAN_POINT('Ctrl Pts',(16.2705582184246,29.8734902121934,-4.58524646945369));
#84736=CARTESIAN_POINT('Ctrl Pts',(16.2986470166865,29.9991469388092,-4.4728988096997));
#84737=CARTESIAN_POINT('Ctrl Pts',(16.317267303762,30.0824457791775,-4.39842265527768));
#84738=CARTESIAN_POINT('Ctrl Pts',(16.3358875908376,30.1636654206877,-4.32161733901386));
#84739=CARTESIAN_POINT('Ctrl Pts',(16.3545078779131,30.2426778921868,-4.24260348172551));
#84740=CARTESIAN_POINT('Origin',(-31.4159265358979,26.,7.7715611723761E-15));
#84741=CARTESIAN_POINT('',(17.341,31.8790943677938,1.19843623717527));
#84742=CARTESIAN_POINT('Ctrl Pts',(16.354507877922,30.2426778922245,-4.24260348168784));
#84743=CARTESIAN_POINT('Ctrl Pts',(16.382888439425,30.3631066642285,-4.12217259749732));
#84744=CARTESIAN_POINT('Ctrl Pts',(16.4112690009281,30.4783901528095,-3.99662544639589));
#84745=CARTESIAN_POINT('Ctrl Pts',(16.4396495624311,30.5881154211411,-3.86641912915385));
#84746=CARTESIAN_POINT('Ctrl Pts',(16.4680386771246,30.6978737579205,-3.73617357098893));
#84747=CARTESIAN_POINT('Ctrl Pts',(16.4964277918181,30.8020703391995,-3.6012662649802));
#84748=CARTESIAN_POINT('Ctrl Pts',(16.5248169065115,30.9003322675621,-3.46218769963297));
#84749=CARTESIAN_POINT('Ctrl Pts',(16.5428470556204,30.9627391879337,-3.37385781340274));
#84750=CARTESIAN_POINT('Ctrl Pts',(16.5608772047292,31.0227531159613,-3.28384605151104));
#84751=CARTESIAN_POINT('Ctrl Pts',(16.578907353838,31.080287476321,-3.1922843165884));
#84752=CARTESIAN_POINT('Ctrl Pts',(16.6068336288268,31.1694004591925,-3.05046750894783));
#84753=CARTESIAN_POINT('Ctrl Pts',(16.6347599038155,31.2525863029309,-2.90489345895294));
#84754=CARTESIAN_POINT('Ctrl Pts',(16.6626861788043,31.3295440951455,-2.75607687445397));
#84755=CARTESIAN_POINT('Ctrl Pts',(16.6906069725765,31.4064867825055,-2.60728949886027));
#84756=CARTESIAN_POINT('Ctrl Pts',(16.7185277663487,31.4772037128205,-2.45526113889313));
#84757=CARTESIAN_POINT('Ctrl Pts',(16.746448560121,31.5414400514461,-2.30053084226862));
#84758=CARTESIAN_POINT('Ctrl Pts',(16.7743685472131,31.6056745341725,-2.14580501607051));
#84759=CARTESIAN_POINT('Ctrl Pts',(16.8022885343052,31.6634286751131,-1.98837769921453));
#84760=CARTESIAN_POINT('Ctrl Pts',(16.8302085213973,31.7144956270484,-1.82880828094286));
#84761=CARTESIAN_POINT('Ctrl Pts',(16.8581263901798,31.765558704497,-1.66925096931824));
#84762=CARTESIAN_POINT('Ctrl Pts',(16.8860442589624,31.8099355114292,-1.50755218178439));
#84763=CARTESIAN_POINT('Ctrl Pts',(16.9139621277449,31.8474688624454,-1.34428713552236));
#84764=CARTESIAN_POINT('Ctrl Pts',(16.9418832151492,31.8850065406423,-1.18100326660467));
#84765=CARTESIAN_POINT('Ctrl Pts',(16.9698043025534,31.9156991159039,-1.01615308570994));
#84766=CARTESIAN_POINT('Ctrl Pts',(16.9977253899577,31.9394402185479,-0.850323403356513));
#84767=CARTESIAN_POINT('Ctrl Pts',(17.0077190280888,31.9479377381903,-0.790968915731159));
#84768=CARTESIAN_POINT('Ctrl Pts',(17.0177126662198,31.9555451837976,-0.731489027925986));
#84769=CARTESIAN_POINT('Ctrl Pts',(17.0277063043508,31.9622592833946,-0.671910885144261));
#84770=CARTESIAN_POINT('Ctrl Pts',(17.0556074415748,31.9810043101541,-0.505575270875629));
#84771=CARTESIAN_POINT('Ctrl Pts',(17.0835085787988,31.9927864702583,-0.338435950515601));
#84772=CARTESIAN_POINT('Ctrl Pts',(17.1114097160228,31.9975602832382,-0.171086670796819));
#84773=CARTESIAN_POINT('Ctrl Pts',(17.1393069093683,32.0023334214305,-0.00376104621528817));
#84774=CARTESIAN_POINT('Ctrl Pts',(17.1672041027137,32.0001001819432,0.163774162066368));
#84775=CARTESIAN_POINT('Ctrl Pts',(17.1951012960592,31.9908671824224,0.330923560016396));
#84776=CARTESIAN_POINT('Ctrl Pts',(17.2230008709851,31.9816333946815,0.498087227492853));
#84777=CARTESIAN_POINT('Ctrl Pts',(17.250900445911,31.9653986681724,0.664864702559548));
#84778=CARTESIAN_POINT('Ctrl Pts',(17.278800020837,31.9422216809555,0.830663285803638));
#84779=CARTESIAN_POINT('Ctrl Pts',(17.2995333472246,31.9249979045387,0.95387506054006));
#84780=CARTESIAN_POINT('Ctrl Pts',(17.3202666736123,31.903941282576,1.0765462673785));
#84781=CARTESIAN_POINT('Ctrl Pts',(17.341,31.8790943677938,1.19843623717527));
#84782=CARTESIAN_POINT('Origin',(17.341,26.,7.7715611723761E-15));
#84783=CARTESIAN_POINT('Origin',(-17.341,26.,-5.55111512312578E-14));
#84784=CARTESIAN_POINT('',(-17.341094308639,36.2772926947297,2.14768526278092));
#84785=CARTESIAN_POINT('',(-17.341,31.8402307203765,5.84023072037652));
#84786=CARTESIAN_POINT('Ctrl Pts',(-17.341,36.2776062547427,2.14782924427302));
#84787=CARTESIAN_POINT('Ctrl Pts',(-17.341,36.1615316286314,2.33343382237898));
#84788=CARTESIAN_POINT('Ctrl Pts',(-17.341,36.0393803151467,2.51488353100729));
#84789=CARTESIAN_POINT('Ctrl Pts',(-17.341,35.9113297455572,2.6918644841006));
#84790=CARTESIAN_POINT('Ctrl Pts',(-17.341,35.785655731614,2.86556075767459));
#84791=CARTESIAN_POINT('Ctrl Pts',(-17.341,35.6542987314585,3.03495263305023));
#84792=CARTESIAN_POINT('Ctrl Pts',(-17.341,35.5174264520561,3.19969356394901));
#84793=CARTESIAN_POINT('Ctrl Pts',(-17.341,35.3824035821343,3.36220852593145));
#84794=CARTESIAN_POINT('Ctrl Pts',(-17.341,35.2420128499351,3.52019737874567));
#84795=CARTESIAN_POINT('Ctrl Pts',(-17.341,35.0964247300032,3.67327830325533));
#84796=CARTESIAN_POINT('Ctrl Pts',(-17.341,34.954049320268,3.82298117296687));
#84797=CARTESIAN_POINT('Ctrl Pts',(-17.341,34.8067028384009,3.96799019837233));
#84798=CARTESIAN_POINT('Ctrl Pts',(-17.341,34.6545622767166,4.10790209060223));
#84799=CARTESIAN_POINT('Ctrl Pts',(-17.341,34.550707649757,4.20340914811465));
#84800=CARTESIAN_POINT('Ctrl Pts',(-17.341,34.444619466998,4.29654011779324));
#84801=CARTESIAN_POINT('Ctrl Pts',(-17.341,34.3363608382622,4.38715446085138));
#84802=CARTESIAN_POINT('Ctrl Pts',(-17.341,34.3064917774342,4.41215538092857));
#84803=CARTESIAN_POINT('Ctrl Pts',(-17.341,34.2764559097218,4.43696598947311));
#84804=CARTESIAN_POINT('Ctrl Pts',(-17.341,34.2462598533269,4.46157896982436));
#84805=CARTESIAN_POINT('Ctrl Pts',(-17.341,34.2238656295209,4.47983263127309));
#84806=CARTESIAN_POINT('Ctrl Pts',(-17.341,34.201386247286,4.49797519500983));
#84807=CARTESIAN_POINT('Ctrl Pts',(-17.341,34.1788257701953,4.51600289953751));
#84808=CARTESIAN_POINT('Ctrl Pts',(-17.341,34.0263322655447,4.63785793980052));
#84809=CARTESIAN_POINT('Ctrl Pts',(-17.341,33.8700735855436,4.75451722463535));
#84810=CARTESIAN_POINT('Ctrl Pts',(-17.341,33.7102131419073,4.86568485778385));
#84811=CARTESIAN_POINT('Ctrl Pts',(-17.341,33.5537632563168,4.97448077434605));
#84812=CARTESIAN_POINT('Ctrl Pts',(-17.341,33.3938630916286,5.07801666714861));
#84813=CARTESIAN_POINT('Ctrl Pts',(-17.341,33.2306846425595,5.17596932344744));
#84814=CARTESIAN_POINT('Ctrl Pts',(-17.341,33.0697047439569,5.27260223526146));
#84815=CARTESIAN_POINT('Ctrl Pts',(-17.341,32.905533764824,5.36380114677409));
#84816=CARTESIAN_POINT('Ctrl Pts',(-17.341,32.7383634686604,5.44921344499573));
#84817=CARTESIAN_POINT('Ctrl Pts',(-17.341,32.5748642160718,5.5327500973891));
#84818=CARTESIAN_POINT('Ctrl Pts',(-17.341,32.408495487699,5.61075117905066));
#84819=CARTESIAN_POINT('Ctrl Pts',(-17.341,32.2394694502253,5.68284993327241));
#84820=CARTESIAN_POINT('Ctrl Pts',(-17.341,32.1079590152306,5.73894625234844));
#84821=CARTESIAN_POINT('Ctrl Pts',(-17.341,31.9748405139997,5.79146876643761));
#84822=CARTESIAN_POINT('Ctrl Pts',(-17.341,31.8402307203765,5.84023072037652));
#84823=CARTESIAN_POINT('',(-17.341,22.5935394840313,-9.9320706176077));
#84824=CARTESIAN_POINT('Ctrl Pts',(-17.341,22.5935394840313,-9.9320706176077));
#84825=CARTESIAN_POINT('Ctrl Pts',(-17.341,22.8358088333483,-10.0151631573662));
#84826=CARTESIAN_POINT('Ctrl Pts',(-17.341,23.080781809034,-10.0890669438635));
#84827=CARTESIAN_POINT('Ctrl Pts',(-17.341,23.3279547104505,-10.1538369902452));
#84828=CARTESIAN_POINT('Ctrl Pts',(-17.341,23.5907422034553,-10.2226987384906));
#84829=CARTESIAN_POINT('Ctrl Pts',(-17.341,23.8560168656464,-10.2812369185677));
#84830=CARTESIAN_POINT('Ctrl Pts',(-17.341,24.1231943750741,-10.3294578205659));
#84831=CARTESIAN_POINT('Ctrl Pts',(-17.341,24.3779390436958,-10.3754348106445));
#84832=CARTESIAN_POINT('Ctrl Pts',(-17.341,24.6344143202987,-10.4120320079489));
#84833=CARTESIAN_POINT('Ctrl Pts',(-17.341,24.8921223713494,-10.4392020733278));
#84834=CARTESIAN_POINT('Ctrl Pts',(-17.341,25.0304094986267,-10.4537816344779));
#84835=CARTESIAN_POINT('Ctrl Pts',(-17.341,25.1690516819469,-10.4656458282875));
#84836=CARTESIAN_POINT('Ctrl Pts',(-17.341,25.3079720394225,-10.4747811465506));
#84837=CARTESIAN_POINT('Ctrl Pts',(-17.341,25.3442642541695,-10.4771677005317));
#84838=CARTESIAN_POINT('Ctrl Pts',(-17.341,25.3805764111684,-10.4793680417995));
#84839=CARTESIAN_POINT('Ctrl Pts',(-17.341,25.4169041904599,-10.4813817179015));
#84840=CARTESIAN_POINT('Ctrl Pts',(-17.341,25.5258995833598,-10.4874234144263));
#84841=CARTESIAN_POINT('Ctrl Pts',(-17.341,25.6349403439897,-10.4917796357836));
#84842=CARTESIAN_POINT('Ctrl Pts',(-17.341,25.7439841375295,-10.4944519751268));
#84843=CARTESIAN_POINT('Ctrl Pts',(-17.341,26.0159511590823,-10.501117078643));
#84844=CARTESIAN_POINT('Ctrl Pts',(-17.341,26.2879465285844,-10.4973124016406));
#84845=CARTESIAN_POINT('Ctrl Pts',(-17.341,26.559393029141,-10.4830228194042));
#84846=CARTESIAN_POINT('Ctrl Pts',(-17.341,26.8181381329473,-10.4694018685668));
#84847=CARTESIAN_POINT('Ctrl Pts',(-17.341,27.0763852070207,-10.4462538416015));
#84848=CARTESIAN_POINT('Ctrl Pts',(-17.341,27.3335713168633,-10.4136535248962));
#84849=CARTESIAN_POINT('Ctrl Pts',(-17.341,27.6028277744426,-10.3795231988167));
#84850=CARTESIAN_POINT('Ctrl Pts',(-17.341,27.8709222300644,-10.3350328829493));
#84851=CARTESIAN_POINT('Ctrl Pts',(-17.341,28.1371965948931,-10.2802081881677));
#84852=CARTESIAN_POINT('Ctrl Pts',(-17.341,28.1827018784682,-10.2708388548316));
#84853=CARTESIAN_POINT('Ctrl Pts',(-17.341,28.2281549242296,-10.2611673443991));
#84854=CARTESIAN_POINT('Ctrl Pts',(-17.341,28.2735493716128,-10.2511942711831));
#84855=CARTESIAN_POINT('Ctrl Pts',(-17.341,28.3081605165915,-10.2435902688687));
#84856=CARTESIAN_POINT('Ctrl Pts',(-17.341,28.3427305407739,-10.235812482136));
#84857=CARTESIAN_POINT('Ctrl Pts',(-17.341,28.3772488537953,-10.2278633236637));
#84858=CARTESIAN_POINT('Ctrl Pts',(-17.341,28.6304099297094,-10.1695633276522));
#84859=CARTESIAN_POINT('Ctrl Pts',(-17.341,28.8809513566271,-10.1020141715181));
#84860=CARTESIAN_POINT('Ctrl Pts',(-17.341,29.1283233348882,-10.0253414139435));
#84861=CARTESIAN_POINT('Ctrl Pts',(-17.341,29.3750732479331,-9.94886146501217));
#84862=CARTESIAN_POINT('Ctrl Pts',(-17.341,29.6186702931669,-9.86330361846533));
#84863=CARTESIAN_POINT('Ctrl Pts',(-17.341,29.8585620425732,-9.76874141915599));
#84864=CARTESIAN_POINT('Ctrl Pts',(-17.341,30.0573570415716,-9.6903790229356));
#84865=CARTESIAN_POINT('Ctrl Pts',(-17.341,30.2536075928598,-9.60583221153325));
#84866=CARTESIAN_POINT('Ctrl Pts',(-17.341,30.4469909186711,-9.51511701868236));
#84867=CARTESIAN_POINT('Ctrl Pts',(-17.341,30.6809973108109,-9.40534573978716));
#84868=CARTESIAN_POINT('Ctrl Pts',(-17.341,30.9108063750555,-9.28654330808442));
#84869=CARTESIAN_POINT('Ctrl Pts',(-17.341,31.1360653900894,-9.15912023482861));
#84870=CARTESIAN_POINT('Ctrl Pts',(-17.341,31.3624225939535,-9.03107594516669));
#84871=CARTESIAN_POINT('Ctrl Pts',(-17.341,31.5841857695078,-8.89432631678317));
#84872=CARTESIAN_POINT('Ctrl Pts',(-17.341,31.8009651035927,-8.74924628711789));
#84873=CARTESIAN_POINT('Ctrl Pts',(-17.341,31.8443517478387,-8.72020968332513));
#84874=CARTESIAN_POINT('Ctrl Pts',(-17.341,31.8875386396169,-8.69083926973578));
#84875=CARTESIAN_POINT('Ctrl Pts',(-17.341,31.930522473861,-8.6611378774681));
#84876=CARTESIAN_POINT('Ctrl Pts',(-17.341,31.9566250905296,-8.64310123484369));
#84877=CARTESIAN_POINT('Ctrl Pts',(-17.341,31.9826551439777,-8.62494089745138));
#84878=CARTESIAN_POINT('Ctrl Pts',(-17.341,32.0086040372382,-8.6066630275424));
#84879=CARTESIAN_POINT('Ctrl Pts',(-17.341,32.0559898745325,-8.57328541251676));
#84880=CARTESIAN_POINT('Ctrl Pts',(-17.341,32.1030883056765,-8.5395277586763));
#84881=CARTESIAN_POINT('Ctrl Pts',(-17.341,32.1498919137234,-8.50539854264918));
#84882=CARTESIAN_POINT('Ctrl Pts',(-17.341,32.3589826980336,-8.3529294308696));
#84883=CARTESIAN_POINT('Ctrl Pts',(-17.341,32.5622213807345,-8.19302739276201));
#84884=CARTESIAN_POINT('Ctrl Pts',(-17.341,32.7592977225623,-8.02615983750127));
#84885=CARTESIAN_POINT('Ctrl Pts',(-17.341,32.9580802244621,-7.85784765039154));
#84886=CARTESIAN_POINT('Ctrl Pts',(-17.341,33.1505937118948,-7.682448388491));
#84887=CARTESIAN_POINT('Ctrl Pts',(-17.341,33.3364921131307,-7.50039575408498));
#84888=CARTESIAN_POINT('Ctrl Pts',(-17.341,33.5226147373004,-7.31812353534938));
#84889=CARTESIAN_POINT('Ctrl Pts',(-17.341,33.7021067751131,-7.12918140070557));
#84890=CARTESIAN_POINT('Ctrl Pts',(-17.341,33.8745861108141,-6.9339657231966));
#84891=CARTESIAN_POINT('Ctrl Pts',(-17.341,34.0459474637866,-6.74001540164983));
#84892=CARTESIAN_POINT('Ctrl Pts',(-17.341,34.2103871455161,-6.53987209449813));
#84893=CARTESIAN_POINT('Ctrl Pts',(-17.341,34.3674895883909,-6.33389361035062));
#84894=CARTESIAN_POINT('Ctrl Pts',(-17.341,34.517366833392,-6.13738815080077));
#84895=CARTESIAN_POINT('Ctrl Pts',(-17.341,34.6605662781383,-5.93557133757178));
#84896=CARTESIAN_POINT('Ctrl Pts',(-17.341,34.7966867681353,-5.72873359083955));
#84897=CARTESIAN_POINT('Ctrl Pts',(-17.341,34.8194088706324,-5.6942069117067));
#84898=CARTESIAN_POINT('Ctrl Pts',(-17.341,34.8419351844103,-5.65953767929054));
#84899=CARTESIAN_POINT('Ctrl Pts',(-17.341,34.8642455796673,-5.62475603283737));
#84900=CARTESIAN_POINT('Ctrl Pts',(-17.341,35.0050863633287,-5.40518689087187));
#84901=CARTESIAN_POINT('Ctrl Pts',(-17.341,35.137490961629,-5.18089281592262));
#84902=CARTESIAN_POINT('Ctrl Pts',(-17.341,35.2611152866583,-4.95229237399867));
#84903=CARTESIAN_POINT('Ctrl Pts',(-17.341,35.3838450176568,-4.72534617439922));
#84904=CARTESIAN_POINT('Ctrl Pts',(-17.341,35.4979214784785,-4.49415518369225));
#84905=CARTESIAN_POINT('Ctrl Pts',(-17.341,35.6029675828494,-4.25909790208043));
#84906=CARTESIAN_POINT('Ctrl Pts',(-17.341,35.6765857757336,-4.0943655457481));
#84907=CARTESIAN_POINT('Ctrl Pts',(-17.341,35.7457679170749,-3.9277336259582));
#84908=CARTESIAN_POINT('Ctrl Pts',(-17.341,35.8103706829352,-3.75932527825395));
#84909=CARTESIAN_POINT('Ctrl Pts',(-17.341,35.9028113585593,-3.51834826689536));
#84910=CARTESIAN_POINT('Ctrl Pts',(-17.341,35.9858779941333,-3.27373439840514));
#84911=CARTESIAN_POINT('Ctrl Pts',(-17.341,36.0596175129558,-3.02603073497669));
#84912=CARTESIAN_POINT('Ctrl Pts',(-17.341,36.1201532965813,-2.82268067774835));
#84913=CARTESIAN_POINT('Ctrl Pts',(-17.341,36.1744021874915,-2.61724776464813));
#84914=CARTESIAN_POINT('Ctrl Pts',(-17.341,36.222364326136,-2.41002990804256));
#84915=CARTESIAN_POINT('Ctrl Pts',(-17.341,36.243347761793,-2.31937209577762));
#84916=CARTESIAN_POINT('Ctrl Pts',(-17.341,36.2631275735294,-2.2283726039198));
#84917=CARTESIAN_POINT('Ctrl Pts',(-17.341,36.2817023711122,-2.13705632026244));
#84918=CARTESIAN_POINT('Ctrl Pts',(-17.341,36.2945135782287,-2.07407464749687));
#84919=CARTESIAN_POINT('Ctrl Pts',(-17.341,36.3067515439926,-2.01094227700125));
#84920=CARTESIAN_POINT('Ctrl Pts',(-17.341,36.3184155754271,-1.94766738554708));
#84921=CARTESIAN_POINT('Ctrl Pts',(-17.341,36.3246021142257,-1.91410672745434));
#84922=CARTESIAN_POINT('Ctrl Pts',(-17.341,36.3306268079126,-1.88050770831468));
#84923=CARTESIAN_POINT('Ctrl Pts',(-17.341,36.3364864178808,-1.84689081480382));
#84924=CARTESIAN_POINT('Ctrl Pts',(-17.341,36.380510407315,-1.59432284991413));
#84925=CARTESIAN_POINT('Ctrl Pts',(-17.341,36.4152740876249,-1.34045762649642));
#84926=CARTESIAN_POINT('Ctrl Pts',(-17.341,36.4408913376544,-1.08583872086898));
#84927=CARTESIAN_POINT('Ctrl Pts',(-17.341,36.4669799578256,-0.82653470073817));
#84928=CARTESIAN_POINT('Ctrl Pts',(-17.341,36.4835825777201,-0.566448386721993));
#84929=CARTESIAN_POINT('Ctrl Pts',(-17.341,36.4907673755878,-0.306138836329885));
#84930=CARTESIAN_POINT('Ctrl Pts',(-17.341,36.4979550685448,-0.0457243951114861));
#84931=CARTESIAN_POINT('Ctrl Pts',(-17.341,36.4957173304509,0.214914140407855));
#84932=CARTESIAN_POINT('Ctrl Pts',(-17.341,36.4840701763494,0.475222111787335));
#84933=CARTESIAN_POINT('Ctrl Pts',(-17.341,36.4724300591827,0.735372811253935));
#84934=CARTESIAN_POINT('Ctrl Pts',(-17.341,36.451391878011,0.995194022519522));
#84935=CARTESIAN_POINT('Ctrl Pts',(-17.341,36.4209197011799,1.25412700844002));
#84936=CARTESIAN_POINT('Ctrl Pts',(-17.341,36.3904475243488,1.51305999436052));
#84937=CARTESIAN_POINT('Ctrl Pts',(-17.341,36.350541354477,1.77110543783372));
#84938=CARTESIAN_POINT('Ctrl Pts',(-17.341,36.3011134072668,2.02768932866362));
#84939=CARTESIAN_POINT('Ctrl Pts',(-17.341,36.2934016269672,2.06772171329963));
#84940=CARTESIAN_POINT('Ctrl Pts',(-17.341,36.285457960639,2.10771847797819));
#84941=CARTESIAN_POINT('Ctrl Pts',(-17.341,36.2772819608986,2.14767739224408));
#84942=CARTESIAN_POINT('',(-17.3410000124526,19.8194155612307,-6.18058438813164));
#84943=CARTESIAN_POINT('Origin',(-17.3410000000001,27.3621811742135,-4.63182998232183));
#84944=CARTESIAN_POINT('Ctrl Pts',(-17.341,20.0176003675788,-0.459232662172889));
#84945=CARTESIAN_POINT('Ctrl Pts',(-17.341,19.9517322064179,-0.581001446356886));
#84946=CARTESIAN_POINT('Ctrl Pts',(-17.341,19.8905997935081,-0.705156493938228));
#84947=CARTESIAN_POINT('Ctrl Pts',(-17.341,19.8341231382621,-0.831315420025));
#84948=CARTESIAN_POINT('Ctrl Pts',(-17.341,19.775995155109,-0.961163122553425));
#84949=CARTESIAN_POINT('Ctrl Pts',(-17.341,19.7227985260101,-1.09313356461186));
#84950=CARTESIAN_POINT('Ctrl Pts',(-17.341,19.6744339467518,-1.22686438721676));
#84951=CARTESIAN_POINT('Ctrl Pts',(-17.341,19.6385288680426,-1.32614397953659));
#84952=CARTESIAN_POINT('Ctrl Pts',(-17.341,19.6052866062593,-1.42639494775124));
#84953=CARTESIAN_POINT('Ctrl Pts',(-17.341,19.574665475194,-1.52748750025652));
#84954=CARTESIAN_POINT('Ctrl Pts',(-17.341,19.5542445293948,-1.59490517764461));
#84955=CARTESIAN_POINT('Ctrl Pts',(-17.341,19.5349891052483,-1.66269819855154));
#84956=CARTESIAN_POINT('Ctrl Pts',(-17.341,19.516887615846,-1.73082984977366));
#84957=CARTESIAN_POINT('Ctrl Pts',(-17.341,19.5050712366903,-1.7753051636802));
#84958=CARTESIAN_POINT('Ctrl Pts',(-17.341,19.4937484932404,-1.81991806378669));
#84959=CARTESIAN_POINT('Ctrl Pts',(-17.341,19.4829189525045,-1.86464426777467));
#84960=CARTESIAN_POINT('Ctrl Pts',(-17.341,19.4469174164301,-2.01333127912788));
#84961=CARTESIAN_POINT('Ctrl Pts',(-17.341,19.4163550630892,-2.16330885224486));
#84962=CARTESIAN_POINT('Ctrl Pts',(-17.341,19.3910863712414,-2.31419943608681));
#84963=CARTESIAN_POINT('Ctrl Pts',(-17.341,19.3651542274392,-2.46905178626642));
#84964=CARTESIAN_POINT('Ctrl Pts',(-17.341,19.3447967764344,-2.62486586549222));
#84965=CARTESIAN_POINT('Ctrl Pts',(-17.341,19.3298623828192,-2.781288963794));
#84966=CARTESIAN_POINT('Ctrl Pts',(-17.341,19.317433960963,-2.91146447033498));
#84967=CARTESIAN_POINT('Ctrl Pts',(-17.341,19.3087612989332,-3.04206287948856));
#84968=CARTESIAN_POINT('Ctrl Pts',(-17.341,19.3037641109837,-3.17290743017106));
#84969=CARTESIAN_POINT('Ctrl Pts',(-17.341,19.3019398254421,-3.22067385889559));
#84970=CARTESIAN_POINT('Ctrl Pts',(-17.341,19.3006054749907,-3.2684782057861));
#84971=CARTESIAN_POINT('Ctrl Pts',(-17.341,19.2997576672998,-3.31628153991435));
#84972=CARTESIAN_POINT('Ctrl Pts',(-17.341,19.2967922872302,-3.48348343700968));
#84973=CARTESIAN_POINT('Ctrl Pts',(-17.341,19.2997749992745,-3.65073112523236));
#84974=CARTESIAN_POINT('Ctrl Pts',(-17.341,19.3085060414163,-3.81763388962603));
#84975=CARTESIAN_POINT('Ctrl Pts',(-17.341,19.3174019514415,-3.9876882715531));
#84976=CARTESIAN_POINT('Ctrl Pts',(-17.341,19.3322648327157,-4.15738486193371));
#84977=CARTESIAN_POINT('Ctrl Pts',(-17.341,19.3528972700962,-4.32636292421868));
#84978=CARTESIAN_POINT('Ctrl Pts',(-17.341,19.3741185543832,-4.50016359700939));
#84979=CARTESIAN_POINT('Ctrl Pts',(-17.341,19.4014428903213,-4.67320444045425));
#84980=CARTESIAN_POINT('Ctrl Pts',(-17.341,19.4346780013984,-4.84514365891977));
#84981=CARTESIAN_POINT('Ctrl Pts',(-17.341,19.4683919621552,-5.01956016832891));
#84982=CARTESIAN_POINT('Ctrl Pts',(-17.341,19.5081877984253,-5.19284357814337));
#84983=CARTESIAN_POINT('Ctrl Pts',(-17.341,19.5538951091161,-5.36468229142512));
#84984=CARTESIAN_POINT('Ctrl Pts',(-17.341,19.6004418917034,-5.53967703748047));
#84985=CARTESIAN_POINT('Ctrl Pts',(-17.341,19.6531188357664,-5.71317409403076));
#84986=CARTESIAN_POINT('Ctrl Pts',(-17.341,19.7117841117731,-5.88488284291019));
#84987=CARTESIAN_POINT('Ctrl Pts',(-17.341,19.7456696241611,-5.98406313035338));
#84988=CARTESIAN_POINT('Ctrl Pts',(-17.341,19.781553769508,-6.08264744949897));
#84989=CARTESIAN_POINT('Ctrl Pts',(-17.341,19.8194156939928,-6.18058430600717));
#84990=CARTESIAN_POINT('Ctrl Pts',(-17.341,31.8402307203765,5.84023072037652));
#84991=CARTESIAN_POINT('Ctrl Pts',(-17.341,31.6772449817606,5.89927176683509));
#84992=CARTESIAN_POINT('Ctrl Pts',(-17.341,31.5124860737517,5.95267777531149));
#84993=CARTESIAN_POINT('Ctrl Pts',(-17.341,31.3462177804631,6.00028119451195));
#84994=CARTESIAN_POINT('Ctrl Pts',(-17.341,31.1839939581346,6.04672666205036));
#84995=CARTESIAN_POINT('Ctrl Pts',(-17.341,31.0203328080484,6.0876479752421));
#84996=CARTESIAN_POINT('Ctrl Pts',(-17.341,30.8555135488753,6.12285427372568));
#84997=CARTESIAN_POINT('Ctrl Pts',(-17.341,30.6932702801199,6.15751032651596));
#84998=CARTESIAN_POINT('Ctrl Pts',(-17.341,30.5299043691695,6.18662820695463));
#84999=CARTESIAN_POINT('Ctrl Pts',(-17.341,30.3657226044152,6.20999729895849));
#85000=CARTESIAN_POINT('Ctrl Pts',(-17.341,30.2057956270301,6.23276077853254));
#85001=CARTESIAN_POINT('Ctrl Pts',(-17.341,30.0450942444858,6.25006910703489));
#85002=CARTESIAN_POINT('Ctrl Pts',(-17.341,29.8839459666204,6.26170670088772));
#85003=CARTESIAN_POINT('Ctrl Pts',(-17.341,29.7384970744284,6.27221053720602));
#85004=CARTESIAN_POINT('Ctrl Pts',(-17.341,29.5926844366067,6.27809422970468));
#85005=CARTESIAN_POINT('Ctrl Pts',(-17.341,29.4467839047476,6.27918890117428));
#85006=CARTESIAN_POINT('Ctrl Pts',(-17.341,29.4214408789879,6.27937904638416));
#85007=CARTESIAN_POINT('Ctrl Pts',(-17.341,29.3960942595598,6.2794246753895));
#85008=CARTESIAN_POINT('Ctrl Pts',(-17.341,29.3707487936054,6.27932489687429));
#85009=CARTESIAN_POINT('Ctrl Pts',(-17.341,29.2195272607711,6.27872957698387));
#85010=CARTESIAN_POINT('Ctrl Pts',(-17.341,29.0685973566615,6.27296155917988));
#85011=CARTESIAN_POINT('Ctrl Pts',(-17.341,28.9182153028243,6.26188279249635));
#85012=CARTESIAN_POINT('Ctrl Pts',(-17.341,28.771341749382,6.25106249985473));
#85013=CARTESIAN_POINT('Ctrl Pts',(-17.341,28.6249904852149,6.23517583557146));
#85014=CARTESIAN_POINT('Ctrl Pts',(-17.341,28.4794453702235,6.21407478427408));
#85015=CARTESIAN_POINT('Ctrl Pts',(-17.341,28.3707028106173,6.19830934736062));
#85016=CARTESIAN_POINT('Ctrl Pts',(-17.341,28.2624111412361,6.17963269235642));
#85017=CARTESIAN_POINT('Ctrl Pts',(-17.341,28.1547072927676,6.15797858226784));
#85018=CARTESIAN_POINT('Ctrl Pts',(-17.341,28.0155058302988,6.12999180337691));
#85019=CARTESIAN_POINT('Ctrl Pts',(-17.341,27.877284360162,6.09703110233222));
#85020=CARTESIAN_POINT('Ctrl Pts',(-17.341,27.7404123010864,6.05902908146687));
#85021=CARTESIAN_POINT('Ctrl Pts',(-17.341,27.6071004973527,6.02201555232658));
#85022=CARTESIAN_POINT('Ctrl Pts',(-17.341,27.4750687666256,5.98021902236883));
#85023=CARTESIAN_POINT('Ctrl Pts',(-17.341,27.3447076507239,5.9335817990719));
#85024=CARTESIAN_POINT('Ctrl Pts',(-17.341,27.2957305755044,5.91606004975545));
#85025=CARTESIAN_POINT('Ctrl Pts',(-17.341,27.2469898227419,5.89785511112464));
#85026=CARTESIAN_POINT('Ctrl Pts',(-17.341,27.1985079825373,5.87896434107663));
#85027=CARTESIAN_POINT('',(-17.341,21.5,-6.08441629692198E-14));
#85028=CARTESIAN_POINT('Origin',(-17.341,26.,-6.02930719096035E-14));
#85029=CARTESIAN_POINT('Ctrl Pts',(-17.341,20.0176003675788,-0.459232662172788));
#85030=CARTESIAN_POINT('Ctrl Pts',(-17.1047385136779,20.1260993589114,-1.87264329110142));
#85031=CARTESIAN_POINT('Ctrl Pts',(-16.8684770273558,20.7549867182113,-3.24026809244986));
#85032=CARTESIAN_POINT('Ctrl Pts',(-16.6322155410337,21.7573593128807,-4.24264068711928));
#85033=CARTESIAN_POINT('Ctrl Pts',(-17.5772614863221,19.1067248030209,-0.529155073934297));
#85034=CARTESIAN_POINT('Ctrl Pts',(-17.341,19.2317437672835,-2.15777051759985));
#85035=CARTESIAN_POINT('Ctrl Pts',(-17.1047385136779,19.9563850319797,-3.7336288188102));
#85036=CARTESIAN_POINT('Ctrl Pts',(-16.8684770273558,21.1113781065848,-4.88862189341524));
#85037=CARTESIAN_POINT('Ctrl Pts',(-17.8135229726442,18.195849238463,-0.599077485695805));
#85038=CARTESIAN_POINT('Ctrl Pts',(-17.5772614863221,18.3373881756556,-2.44289774409829));
#85039=CARTESIAN_POINT('Ctrl Pts',(-17.341,19.1577833457481,-4.22698954517053));
#85040=CARTESIAN_POINT('Ctrl Pts',(-17.1047385136779,20.4653969002888,-5.53460309971121));
#85041=CARTESIAN_POINT('Ctrl Pts',(-18.0497844589663,17.2849736739051,-0.668999897457314));
#85042=CARTESIAN_POINT('Ctrl Pts',(-17.8135229726442,17.4430325840277,-2.72802497059672));
#85043=CARTESIAN_POINT('Ctrl Pts',(-17.5772614863221,18.3591816595165,-4.72035027153087));
#85044=CARTESIAN_POINT('Ctrl Pts',(-17.341,19.8194156939928,-6.18058430600717));
#85045=CARTESIAN_POINT('',(-16.6063537825981,21.8280699909994,-4.17193000900062));
#85046=CARTESIAN_POINT('Ctrl Pts',(-16.6324666134455,21.756063321237,-4.24050691752413));
#85047=CARTESIAN_POINT('Ctrl Pts',(-16.4827322162892,22.3910092147368,-4.87597515128349));
#85048=CARTESIAN_POINT('Ctrl Pts',(-16.1833981689618,23.9499461437912,-5.85575312624584));
#85049=CARTESIAN_POINT('Ctrl Pts',(-15.7344644714635,26.6949162487901,-6.1663874940781));
#85050=CARTESIAN_POINT('Ctrl Pts',(-15.2856655209507,29.3005941525251,-5.25296914865542));
#85051=CARTESIAN_POINT('Ctrl Pts',(-14.8368665704379,31.2541515525533,-3.30156178378519));
#85052=CARTESIAN_POINT('Ctrl Pts',(-14.3880676199251,32.164786766515,-0.694649642063505));
#85053=CARTESIAN_POINT('Ctrl Pts',(-13.9379057895215,31.8558977514204,2.05741712339704));
#85054=CARTESIAN_POINT('Ctrl Pts',(-13.6373436092891,30.8679132696699,3.62177982099857));
#85055=CARTESIAN_POINT('Ctrl Pts',(-13.4863810792274,30.2248412548482,4.25953100287412));
#85056=CARTESIAN_POINT('Ctrl Pts',(-17.0209601030214,20.6934232598663,-5.30228820036689));
#85057=CARTESIAN_POINT('Ctrl Pts',(-16.8712257058651,21.4873533688026,-6.09687143843352));
#85058=CARTESIAN_POINT('Ctrl Pts',(-16.5718916585378,23.4366327933644,-7.32197619516751));
#85059=CARTESIAN_POINT('Ctrl Pts',(-16.1229579610395,26.8689164521759,-7.71039035772407));
#85060=CARTESIAN_POINT('Ctrl Pts',(-15.6741590105267,30.1270305106238,-6.56826102999712));
#85061=CARTESIAN_POINT('Ctrl Pts',(-15.2253600600138,32.5697394962176,-4.12824042724765));
#85062=CARTESIAN_POINT('Ctrl Pts',(-14.776561109501,33.7083888237012,-0.868583089743648));
#85063=CARTESIAN_POINT('Ctrl Pts',(-14.3263992790975,33.3221570330652,2.57257416360736));
#85064=CARTESIAN_POINT('Ctrl Pts',(-14.025837098865,32.086790940846,4.52863791586972));
#85065=CARTESIAN_POINT('Ctrl Pts',(-13.8748745688034,31.2827000096214,5.32607572983823));
#85066=CARTESIAN_POINT('Ctrl Pts',(-17.4094535925974,19.6307831984957,-6.36406948320964));
#85067=CARTESIAN_POINT('Ctrl Pts',(-17.259719195441,20.5836975228685,-7.31776772558355));
#85068=CARTESIAN_POINT('Ctrl Pts',(-16.9603851481138,22.9233194429377,-8.78819926408918));
#85069=CARTESIAN_POINT('Ctrl Pts',(-16.5114514506154,27.0429166555619,-9.25439322137004));
#85070=CARTESIAN_POINT('Ctrl Pts',(-16.0626525001026,30.9534668687226,-7.88355291133882));
#85071=CARTESIAN_POINT('Ctrl Pts',(-15.6138535495898,33.885327439882,-4.95491907071012));
#85072=CARTESIAN_POINT('Ctrl Pts',(-15.1650545990769,35.2519908808874,-1.04251653742379));
#85073=CARTESIAN_POINT('Ctrl Pts',(-14.7148927686735,34.78841631471,3.08773120381769));
#85074=CARTESIAN_POINT('Ctrl Pts',(-14.4143305884409,33.3056686120219,5.43549601074087));
#85075=CARTESIAN_POINT('Ctrl Pts',(-14.2633680583793,32.3405587643947,6.39262045680234));
#85076=CARTESIAN_POINT('Ctrl Pts',(-17.7979470821733,18.568143137125,-7.4258507660524));
#85077=CARTESIAN_POINT('Ctrl Pts',(-17.648212685017,19.6800416769345,-8.53866401273357));
#85078=CARTESIAN_POINT('Ctrl Pts',(-17.3488786376897,22.4100060925109,-10.2544223330108));
#85079=CARTESIAN_POINT('Ctrl Pts',(-16.8999449401914,27.2169168589478,-10.798396085016));
#85080=CARTESIAN_POINT('Ctrl Pts',(-16.4511459896785,31.7799032268214,-9.19884479268053));
#85081=CARTESIAN_POINT('Ctrl Pts',(-16.0023470391657,35.2009153835464,-5.7815977141726));
#85082=CARTESIAN_POINT('Ctrl Pts',(-15.553548088653,36.7955929380736,-1.21644998510393));
#85083=CARTESIAN_POINT('Ctrl Pts',(-15.1033862582494,36.254675596355,3.60288824402801));
#85084=CARTESIAN_POINT('Ctrl Pts',(-14.8028240780169,34.5245462831979,6.34235410561202));
#85085=CARTESIAN_POINT('Ctrl Pts',(-14.6518615479552,33.398417519168,7.45916518376644));
#85086=CARTESIAN_POINT('',(-14.654401924225,33.4246212024587,7.42462120245876));
#85087=CARTESIAN_POINT('Ctrl Pts',(-17.341,22.5935394840313,-9.9320706176077));
#85088=CARTESIAN_POINT('Ctrl Pts',(-17.2130667582964,23.8641814749706,-10.3678701541508));
#85089=CARTESIAN_POINT('Ctrl Pts',(-16.9572002748893,26.5709740036708,-10.7394481103171));
#85090=CARTESIAN_POINT('Ctrl Pts',(-16.445467308075,31.8919112648329,-9.43120169534687));
#85091=CARTESIAN_POINT('Ctrl Pts',(-15.8058010995572,36.8227923782163,-4.14869947052776));
#85092=CARTESIAN_POINT('Ctrl Pts',(-15.1661348910393,36.6915650151942,3.0806737156604));
#85093=CARTESIAN_POINT('Ctrl Pts',(-14.7823351659286,34.3744770613104,6.47476534360713));
#85094=CARTESIAN_POINT('Ctrl Pts',(-14.654401924225,33.4246212024587,7.42462120245876));
#85095=CARTESIAN_POINT('',(-13.4647610361879,30.1719300090006,4.17193000900064));
#85096=CARTESIAN_POINT('Ctrl Pts',(-17.341,22.5935394840313,-9.9320706176077));
#85097=CARTESIAN_POINT('Ctrl Pts',(-17.2130667582964,23.8641814749706,-10.3678701541508));
#85098=CARTESIAN_POINT('Ctrl Pts',(-16.9572002748893,26.5709740036708,-10.7394481103171));
#85099=CARTESIAN_POINT('Ctrl Pts',(-16.445467308075,31.8919112648329,-9.43120169534687));
#85100=CARTESIAN_POINT('Ctrl Pts',(-15.8058010995572,36.8227923782163,-4.14869947052776));
#85101=CARTESIAN_POINT('Ctrl Pts',(-15.1661197260623,36.691561904103,3.08084510704696));
#85102=CARTESIAN_POINT('Ctrl Pts',(-14.7823048359745,34.3742939488486,6.47503356182392));
#85103=CARTESIAN_POINT('Ctrl Pts',(-14.6543564292939,33.4242834123465,7.42495897743765));
#85104=CARTESIAN_POINT('Ctrl Pts',(-18.0433842768097,22.5935394840313,-9.9320706176077));
#85105=CARTESIAN_POINT('Ctrl Pts',(-17.9154510351062,23.8641814749706,-10.3678701541508));
#85106=CARTESIAN_POINT('Ctrl Pts',(-17.659584551699,26.5709740036708,-10.7394481103171));
#85107=CARTESIAN_POINT('Ctrl Pts',(-17.1478515848848,31.8919112648329,-9.43120169534687));
#85108=CARTESIAN_POINT('Ctrl Pts',(-16.5081853763669,36.8227923782163,-4.14869947052775));
#85109=CARTESIAN_POINT('Ctrl Pts',(-15.868504002872,36.691561904103,3.08084510704696));
#85110=CARTESIAN_POINT('Ctrl Pts',(-15.4846891127842,34.3742939488486,6.47503356182392));
#85111=CARTESIAN_POINT('Ctrl Pts',(-15.3567407061037,33.4242834123465,7.42495897743765));
#85112=CARTESIAN_POINT('Ctrl Pts',(-18.7457685536195,22.5935394840313,-9.9320706176077));
#85113=CARTESIAN_POINT('Ctrl Pts',(-18.6178353119159,23.8641814749706,-10.3678701541508));
#85114=CARTESIAN_POINT('Ctrl Pts',(-18.3619688285088,26.5709740036708,-10.7394481103171));
#85115=CARTESIAN_POINT('Ctrl Pts',(-17.8502358616945,31.8919112648329,-9.43120169534687));
#85116=CARTESIAN_POINT('Ctrl Pts',(-17.2105696531766,36.8227923782163,-4.14869947052776));
#85117=CARTESIAN_POINT('Ctrl Pts',(-16.5708882796818,36.691561904103,3.08084510704696));
#85118=CARTESIAN_POINT('Ctrl Pts',(-16.1870733895941,34.3742939488486,6.47503356182392));
#85119=CARTESIAN_POINT('Ctrl Pts',(-16.0591249829134,33.4242834123465,7.42495897743765));
#85120=CARTESIAN_POINT('Ctrl Pts',(-19.4481528304293,22.5935394840313,-9.9320706176077));
#85121=CARTESIAN_POINT('Ctrl Pts',(-19.3202195887258,23.8641814749706,-10.3678701541508));
#85122=CARTESIAN_POINT('Ctrl Pts',(-19.0643531053186,26.5709740036708,-10.7394481103171));
#85123=CARTESIAN_POINT('Ctrl Pts',(-18.5526201385043,31.8919112648329,-9.43120169534687));
#85124=CARTESIAN_POINT('Ctrl Pts',(-17.9129539299865,36.8227923782163,-4.14869947052776));
#85125=CARTESIAN_POINT('Ctrl Pts',(-17.2732725564915,36.691561904103,3.08084510704696));
#85126=CARTESIAN_POINT('Ctrl Pts',(-16.8894576664038,34.3742939488486,6.47503356182392));
#85127=CARTESIAN_POINT('Ctrl Pts',(-16.7615092597232,33.4242834123465,7.42495897743765));
#85128=CARTESIAN_POINT('',(-16.7615242403913,33.4246212024587,7.42462120245876));
#85129=CARTESIAN_POINT('Ctrl Pts',(-17.341094308639,36.2772926947297,2.14768526278091));
#85130=CARTESIAN_POINT('Ctrl Pts',(-17.3074845396453,36.205660317479,2.49222032891058));
#85131=CARTESIAN_POINT('Ctrl Pts',(-17.273944378382,36.1161264432318,2.83269742905984));
#85132=CARTESIAN_POINT('Ctrl Pts',(-17.2404435591107,36.009671232445,3.16762466466842));
#85133=CARTESIAN_POINT('Ctrl Pts',(-17.208700986421,35.9088031838391,3.48497368338849));
#85134=CARTESIAN_POINT('Ctrl Pts',(-17.1769937344665,35.7927434822782,3.79734082231336));
#85135=CARTESIAN_POINT('Ctrl Pts',(-17.1452960571528,35.6622975920403,4.10348960834603));
#85136=CARTESIAN_POINT('Ctrl Pts',(-17.1082962555543,35.5100317963359,4.4608484214461));
#85137=CARTESIAN_POINT('Ctrl Pts',(-17.0712703535404,35.3379954474769,4.81011526676917));
#85138=CARTESIAN_POINT('Ctrl Pts',(-17.0342293500534,35.1473064814038,5.14906385221752));
#85139=CARTESIAN_POINT('Ctrl Pts',(-16.9969240103757,34.9552566992045,5.49043128082452));
#85140=CARTESIAN_POINT('Ctrl Pts',(-16.9596033529182,34.7442875207048,5.82133178564715));
#85141=CARTESIAN_POINT('Ctrl Pts',(-16.9222786137831,34.5155918346289,6.13950603627829));
#85142=CARTESIAN_POINT('Ctrl Pts',(-16.885276572442,34.2888733785379,6.45492945378458));
#85143=CARTESIAN_POINT('Ctrl Pts',(-16.848270519696,34.0447341171065,6.75784492409598));
#85144=CARTESIAN_POINT('Ctrl Pts',(-16.8112714027285,33.78437909671,7.04607825580267));
#85145=CARTESIAN_POINT('Ctrl Pts',(-16.7946872932033,33.6676801988014,7.1752730456687));
#85146=CARTESIAN_POINT('Ctrl Pts',(-16.7781045771455,33.5477239222676,7.30151848264989));
#85147=CARTESIAN_POINT('Ctrl Pts',(-16.7615242403913,33.4246212024587,7.42462120245876));
#85148=CARTESIAN_POINT('',(-16.7615242403913,33.4246212024587,7.42462120245876));
#85149=CARTESIAN_POINT('Origin',(17.341,26.,-5.55111512312578E-14));
#85150=CARTESIAN_POINT('',(17.341,31.8402330044652,5.84023300446519));
#85151=CARTESIAN_POINT('Ctrl Pts',(17.341,31.8402330044652,5.8402330044652));
#85152=CARTESIAN_POINT('Ctrl Pts',(17.341,31.8992685593566,5.67726250202317));
#85153=CARTESIAN_POINT('Ctrl Pts',(17.341,31.9526810918222,5.51251754969076));
#85154=CARTESIAN_POINT('Ctrl Pts',(17.341,32.0002995254776,5.3462623959511));
#85155=CARTESIAN_POINT('Ctrl Pts',(17.341,32.0467530017636,5.18407457814962));
#85156=CARTESIAN_POINT('Ctrl Pts',(17.341,32.0876919849256,5.0204490675178));
#85157=CARTESIAN_POINT('Ctrl Pts',(17.341,32.1229224002175,4.85566538347096));
#85158=CARTESIAN_POINT('Ctrl Pts',(17.341,32.1576023005175,4.69345663042466));
#85159=CARTESIAN_POINT('Ctrl Pts',(17.341,32.1867502430916,4.53012516617391));
#85160=CARTESIAN_POINT('Ctrl Pts',(17.341,32.2101525002504,4.36597803817485));
#85161=CARTESIAN_POINT('Ctrl Pts',(17.341,32.2329501218819,4.20607191926426));
#85162=CARTESIAN_POINT('Ctrl Pts',(17.341,32.2502946593677,4.04539145045367));
#85163=CARTESIAN_POINT('Ctrl Pts',(17.341,32.2619675366177,3.88426442880339));
#85164=CARTESIAN_POINT('Ctrl Pts',(17.341,32.2725061960161,3.73879362801657));
#85165=CARTESIAN_POINT('Ctrl Pts',(17.341,32.2784213451913,3.59295915344904));
#85166=CARTESIAN_POINT('Ctrl Pts',(17.341,32.2795417065118,3.44703729053366));
#85167=CARTESIAN_POINT('Ctrl Pts',(17.341,32.2797575956532,3.41891873170909));
#85168=CARTESIAN_POINT('Ctrl Pts',(17.341,32.2797954074234,3.39079437858622));
#85169=CARTESIAN_POINT('Ctrl Pts',(17.341,32.2796539422494,3.36267510215636));
#85170=CARTESIAN_POINT('Ctrl Pts',(17.341,32.2788934262934,3.21150603495092));
#85171=CARTESIAN_POINT('Ctrl Pts',(17.341,32.2729554998115,3.06063343258084));
#85172=CARTESIAN_POINT('Ctrl Pts',(17.341,32.2616992396755,2.91031447087161));
#85173=CARTESIAN_POINT('Ctrl Pts',(17.341,32.2507045736095,2.7634889029276));
#85174=CARTESIAN_POINT('Ctrl Pts',(17.341,32.2346353579727,2.61719124631499));
#85175=CARTESIAN_POINT('Ctrl Pts',(17.341,32.2133409878654,2.47170640449163));
#85176=CARTESIAN_POINT('Ctrl Pts',(17.341,32.1978029806876,2.36554949517109));
#85177=CARTESIAN_POINT('Ctrl Pts',(17.341,32.1794825144783,2.25982625781697));
#85178=CARTESIAN_POINT('Ctrl Pts',(17.341,32.1583169602484,2.15466449074636));
#85179=CARTESIAN_POINT('Ctrl Pts',(17.341,32.1302989771486,2.01545620068619));
#85180=CARTESIAN_POINT('Ctrl Pts',(17.341,32.0972951601529,1.87722976698276));
#85181=CARTESIAN_POINT('Ctrl Pts',(17.341,32.0592418386405,1.74035383175913));
#85182=CARTESIAN_POINT('Ctrl Pts',(17.341,32.022182235483,1.60705225282758));
#85183=CARTESIAN_POINT('Ctrl Pts',(17.341,31.9803328729637,1.47503151017727));
#85184=CARTESIAN_POINT('Ctrl Pts',(17.341,31.9336396253331,1.34468130064232));
#85185=CARTESIAN_POINT('Ctrl Pts',(17.341,31.9160986730874,1.29571347517094));
#85186=CARTESIAN_POINT('Ctrl Pts',(17.341,31.897874225919,1.24698191069875));
#85187=CARTESIAN_POINT('Ctrl Pts',(17.341,31.8789638354448,1.19850914458424));
#85188=CARTESIAN_POINT('',(17.341,28.1469046708622,10.2782246994423));
#85189=CARTESIAN_POINT('Ctrl Pts',(17.341,28.1469452949575,10.2781625741404));
#85190=CARTESIAN_POINT('Ctrl Pts',(17.341,28.3325279067454,10.1621292850198));
#85191=CARTESIAN_POINT('Ctrl Pts',(17.341,28.5139576804591,10.0400213276751));
#85192=CARTESIAN_POINT('Ctrl Pts',(17.341,28.6909209962493,9.91201604150413));
#85193=CARTESIAN_POINT('Ctrl Pts',(17.341,28.864524013336,9.78644140597534));
#85194=CARTESIAN_POINT('Ctrl Pts',(17.341,29.0338286034143,9.65519060909531));
#85195=CARTESIAN_POINT('Ctrl Pts',(17.341,29.1984889795133,9.51843103193587));
#85196=CARTESIAN_POINT('Ctrl Pts',(17.341,29.3609129200115,9.383528938613));
#85197=CARTESIAN_POINT('Ctrl Pts',(17.341,29.5188179436805,9.24326607244863));
#85198=CARTESIAN_POINT('Ctrl Pts',(17.341,29.6718231704292,9.09781251105125));
#85199=CARTESIAN_POINT('Ctrl Pts',(17.341,29.8213281162527,8.9556864721006));
#85200=CARTESIAN_POINT('Ctrl Pts',(17.341,29.9661547456581,8.80860398474598));
#85201=CARTESIAN_POINT('Ctrl Pts',(17.341,30.1059017960368,8.65674114496278));
#85202=CARTESIAN_POINT('Ctrl Pts',(17.341,30.2254261203405,8.52685430110651));
#85203=CARTESIAN_POINT('Ctrl Pts',(17.341,30.3412338611254,8.39347059630592));
#85204=CARTESIAN_POINT('Ctrl Pts',(17.341,30.4530475545969,8.25671513771186));
#85205=CARTESIAN_POINT('Ctrl Pts',(17.341,30.4741841444228,8.23086370623684));
#85206=CARTESIAN_POINT('Ctrl Pts',(17.341,30.495173125642,8.2048976877583));
#85207=CARTESIAN_POINT('Ctrl Pts',(17.341,30.5160086779073,8.17882334113199));
#85208=CARTESIAN_POINT('Ctrl Pts',(17.341,30.6378636386358,8.02632973579267));
#85209=CARTESIAN_POINT('Ctrl Pts',(17.341,30.754522841015,7.87007095642442));
#85210=CARTESIAN_POINT('Ctrl Pts',(17.341,30.8656903884429,7.71021041498222));
#85211=CARTESIAN_POINT('Ctrl Pts',(17.341,30.9744862217097,7.55376043281476));
#85212=CARTESIAN_POINT('Ctrl Pts',(17.341,31.0780220280316,7.39386017300758));
#85213=CARTESIAN_POINT('Ctrl Pts',(17.341,31.1759745943601,7.23068163057763));
#85214=CARTESIAN_POINT('Ctrl Pts',(17.341,31.2726074170979,7.06970164040195));
#85215=CARTESIAN_POINT('Ctrl Pts',(17.341,31.3638062361732,6.90553057142836));
#85216=CARTESIAN_POINT('Ctrl Pts',(17.341,31.4492184383387,6.73836018750939));
#85217=CARTESIAN_POINT('Ctrl Pts',(17.341,31.5327550010927,6.5748608406618));
#85218=CARTESIAN_POINT('Ctrl Pts',(17.341,31.6107559890823,6.40849201972888));
#85219=CARTESIAN_POINT('Ctrl Pts',(17.341,31.682854645339,6.23946589181676));
#85220=CARTESIAN_POINT('Ctrl Pts',(17.341,31.7389500478517,6.10795735653098));
#85221=CARTESIAN_POINT('Ctrl Pts',(17.341,31.7914717498238,5.97484080451409));
#85222=CARTESIAN_POINT('Ctrl Pts',(17.341,31.8402330044652,5.84023300446519));
#85223=CARTESIAN_POINT('',(17.341,16.0679265366941,-3.4064522188774));
#85224=CARTESIAN_POINT('Ctrl Pts',(17.341,16.0679265366941,-3.4064522188774));
#85225=CARTESIAN_POINT('Ctrl Pts',(17.341,15.9845961443224,-3.16348871151483));
#85226=CARTESIAN_POINT('Ctrl Pts',(17.341,15.9103740268908,-2.91768390374845));
#85227=CARTESIAN_POINT('Ctrl Pts',(17.341,15.8452640134803,-2.66959981594315));
#85228=CARTESIAN_POINT('Ctrl Pts',(17.341,15.7762851031214,-2.40677434321136));
#85229=CARTESIAN_POINT('Ctrl Pts',(17.341,15.717532718057,-2.14139009190298));
#85230=CARTESIAN_POINT('Ctrl Pts',(17.341,15.6690701999576,-1.87409349011832));
#85231=CARTESIAN_POINT('Ctrl Pts',(17.341,15.6229786729691,-1.61987416726227));
#85232=CARTESIAN_POINT('Ctrl Pts',(17.341,15.586195137224,-1.36392425427929));
#85233=CARTESIAN_POINT('Ctrl Pts',(17.341,15.5588262867574,-1.10679133129087));
#85234=CARTESIAN_POINT('Ctrl Pts',(17.341,15.5440859521401,-0.968304501870222));
#85235=CARTESIAN_POINT('Ctrl Pts',(17.341,15.5320774096911,-0.829474436419078));
#85236=CARTESIAN_POINT('Ctrl Pts',(17.341,15.522823606219,-0.690386720854866));
#85237=CARTESIAN_POINT('Ctrl Pts',(17.341,15.5204881459522,-0.655283983447918));
#85238=CARTESIAN_POINT('Ctrl Pts',(17.341,15.5183281478679,-0.620164434365577));
#85239=CARTESIAN_POINT('Ctrl Pts',(17.341,15.5163440946815,-0.58503067513978));
#85240=CARTESIAN_POINT('Ctrl Pts',(17.341,15.5118071418151,-0.504689981294506));
#85241=CARTESIAN_POINT('Ctrl Pts',(17.341,15.5081932973467,-0.424329734635187));
#85242=CARTESIAN_POINT('Ctrl Pts',(17.341,15.5055038583947,-0.343972754343596));
#85243=CARTESIAN_POINT('Ctrl Pts',(17.341,15.4968333929881,-0.0849103884541162));
#85244=CARTESIAN_POINT('Ctrl Pts',(17.341,15.4977656324917,0.174138796742486));
#85245=CARTESIAN_POINT('Ctrl Pts',(17.341,15.5083661305816,0.432621246943835));
#85246=CARTESIAN_POINT('Ctrl Pts',(17.341,15.5101320321375,0.47568097462022));
#85247=CARTESIAN_POINT('Ctrl Pts',(17.341,15.5121663553424,0.518724985663109));
#85248=CARTESIAN_POINT('Ctrl Pts',(17.341,15.5144695437764,0.561750729678525));
#85249=CARTESIAN_POINT('Ctrl Pts',(17.341,15.528277558698,0.819697542286757));
#85250=CARTESIAN_POINT('Ctrl Pts',(17.341,15.5517449206594,1.07698819160038));
#85251=CARTESIAN_POINT('Ctrl Pts',(17.341,15.5847062718016,1.33315042288893));
#85252=CARTESIAN_POINT('Ctrl Pts',(17.341,15.6193150905622,1.60211610326126));
#85253=CARTESIAN_POINT('Ctrl Pts',(17.341,15.6643903836506,1.86983854205682));
#85254=CARTESIAN_POINT('Ctrl Pts',(17.341,15.7198009821417,2.1357590308058));
#85255=CARTESIAN_POINT('Ctrl Pts',(17.341,15.7286446160712,2.1782004322866));
#85256=CARTESIAN_POINT('Ctrl Pts',(17.341,15.7377516426895,2.22059589419355));
#85257=CARTESIAN_POINT('Ctrl Pts',(17.341,15.7471216689552,2.26294309641981));
#85258=CARTESIAN_POINT('Ctrl Pts',(17.341,15.7550108842892,2.29859787343784));
#85259=CARTESIAN_POINT('Ctrl Pts',(17.341,15.7630852570301,2.33421241764003));
#85260=CARTESIAN_POINT('Ctrl Pts',(17.341,15.7713411716081,2.36977215384259));
#85261=CARTESIAN_POINT('Ctrl Pts',(17.341,15.829782966907,2.62149167012282));
#85262=CARTESIAN_POINT('Ctrl Pts',(17.341,15.8973609940489,2.87066335406102));
#85263=CARTESIAN_POINT('Ctrl Pts',(17.341,15.9738605229754,3.11682986990915));
#85264=CARTESIAN_POINT('Ctrl Pts',(17.341,16.050813888197,3.36445677775033));
#85265=CARTESIAN_POINT('Ctrl Pts',(17.341,16.1367950601888,3.60904335199101));
#85266=CARTESIAN_POINT('Ctrl Pts',(17.341,16.2316376645728,3.85011695443059));
#85267=CARTESIAN_POINT('Ctrl Pts',(17.341,16.3107225750279,4.05113720673006));
#85268=CARTESIAN_POINT('Ctrl Pts',(17.341,16.3959699274851,4.24971488739541));
#85269=CARTESIAN_POINT('Ctrl Pts',(17.341,16.4873097035077,4.44556767895105));
#85270=CARTESIAN_POINT('Ctrl Pts',(17.341,16.5966493783922,4.68001625640994));
#85271=CARTESIAN_POINT('Ctrl Pts',(17.341,16.7147183649624,4.91056122178516));
#85272=CARTESIAN_POINT('Ctrl Pts',(17.341,16.8412379141657,5.13669090393161));
#85273=CARTESIAN_POINT('Ctrl Pts',(17.341,16.9668462010638,5.36119187765551));
#85274=CARTESIAN_POINT('Ctrl Pts',(17.341,17.1007841394184,5.58134149474401));
#85275=CARTESIAN_POINT('Ctrl Pts',(17.341,17.2428193477291,5.79660754331022));
#85276=CARTESIAN_POINT('Ctrl Pts',(17.341,17.2761955888083,5.84719198373571));
#85277=CARTESIAN_POINT('Ctrl Pts',(17.341,17.3100191098424,5.89750660346259));
#85278=CARTESIAN_POINT('Ctrl Pts',(17.341,17.3442871876066,5.94754419044709));
#85279=CARTESIAN_POINT('Ctrl Pts',(17.341,17.3706168923142,5.98599031802523));
#85280=CARTESIAN_POINT('Ctrl Pts',(17.341,17.3972133137863,6.02427877787285));
#85281=CARTESIAN_POINT('Ctrl Pts',(17.341,17.4240491903923,6.06236977651445));
#85282=CARTESIAN_POINT('Ctrl Pts',(17.341,17.5735436314461,6.27456305175956));
#85283=CARTESIAN_POINT('Ctrl Pts',(17.341,17.7305971258366,6.48082832820043));
#85284=CARTESIAN_POINT('Ctrl Pts',(17.341,17.8948640063635,6.68069808976308));
#85285=CARTESIAN_POINT('Ctrl Pts',(17.341,18.0589715640803,6.88037399720268));
#85286=CARTESIAN_POINT('Ctrl Pts',(17.341,18.2302788952672,7.07366736772761));
#85287=CARTESIAN_POINT('Ctrl Pts',(17.341,18.4084863697564,7.26008663890563));
#85288=CARTESIAN_POINT('Ctrl Pts',(17.341,18.5489289706688,7.40700083192413));
#85289=CARTESIAN_POINT('Ctrl Pts',(17.341,18.6936580371364,7.54964527618223));
#85290=CARTESIAN_POINT('Ctrl Pts',(17.341,18.8425443966315,7.68776467945016));
#85291=CARTESIAN_POINT('Ctrl Pts',(17.341,19.0319051885732,7.86343154157266));
#85292=CARTESIAN_POINT('Ctrl Pts',(17.341,19.2279900886259,8.03178022504402));
#85293=CARTESIAN_POINT('Ctrl Pts',(17.341,19.43030103464,8.19265160060018));
#85294=CARTESIAN_POINT('Ctrl Pts',(17.341,19.6337043980953,8.35439163254851));
#85295=CARTESIAN_POINT('Ctrl Pts',(17.341,19.8434017995546,8.50857367461105));
#85296=CARTESIAN_POINT('Ctrl Pts',(17.341,20.0589140327271,8.65499096131215));
#85297=CARTESIAN_POINT('Ctrl Pts',(17.341,20.1170226522608,8.69446949244159));
#85298=CARTESIAN_POINT('Ctrl Pts',(17.341,20.1755541364194,8.73338325663078));
#85299=CARTESIAN_POINT('Ctrl Pts',(17.341,20.2344993406077,8.7717276020584));
#85300=CARTESIAN_POINT('Ctrl Pts',(17.341,20.2608991208657,8.78890087861871));
#85301=CARTESIAN_POINT('Ctrl Pts',(17.341,20.2873835813077,8.80596101132696));
#85302=CARTESIAN_POINT('Ctrl Pts',(17.341,20.3139465106913,8.82290412783024));
#85303=CARTESIAN_POINT('Ctrl Pts',(17.341,20.3744302829357,8.86148359265122));
#85304=CARTESIAN_POINT('Ctrl Pts',(17.341,20.4352834531749,8.89943257445888));
#85305=CARTESIAN_POINT('Ctrl Pts',(17.341,20.4964892231803,8.93674624652325));
#85306=CARTESIAN_POINT('Ctrl Pts',(17.341,20.7173534911754,9.0713946116361));
#85307=CARTESIAN_POINT('Ctrl Pts',(17.341,20.9428288522432,9.19778755624999));
#85308=CARTESIAN_POINT('Ctrl Pts',(17.341,21.1723828801861,9.31582124528712));
#85309=CARTESIAN_POINT('Ctrl Pts',(17.341,21.4038163979976,9.43482134351639));
#85310=CARTESIAN_POINT('Ctrl Pts',(17.341,21.6393962155438,9.54532502020363));
#85311=CARTESIAN_POINT('Ctrl Pts',(17.341,21.8786080889347,9.64718249239929));
#85312=CARTESIAN_POINT('Ctrl Pts',(17.341,22.118070891722,9.74914681144021));
#85313=CARTESIAN_POINT('Ctrl Pts',(17.341,22.361173983963,9.84244701763524));
#85314=CARTESIAN_POINT('Ctrl Pts',(17.341,22.6074238642972,9.92688573515372));
#85315=CARTESIAN_POINT('Ctrl Pts',(17.341,22.8521249582807,10.0107933761374));
#85316=CARTESIAN_POINT('Ctrl Pts',(17.341,23.0999339927884,10.0859508329837));
#85317=CARTESIAN_POINT('Ctrl Pts',(17.341,23.3503796394041,10.1521148249929));
#85318=CARTESIAN_POINT('Ctrl Pts',(17.341,23.5813869667577,10.2131435039404));
#85319=CARTESIAN_POINT('Ctrl Pts',(17.341,23.8146380016544,10.2665202226159));
#85320=CARTESIAN_POINT('Ctrl Pts',(17.341,24.0497660152581,10.3120140744538));
#85321=CARTESIAN_POINT('Ctrl Pts',(17.341,24.080163066604,10.3178954619118));
#85322=CARTESIAN_POINT('Ctrl Pts',(17.341,24.1105928674216,10.323645259904));
#85323=CARTESIAN_POINT('Ctrl Pts',(17.341,24.141036215458,10.3292596547578));
#85324=CARTESIAN_POINT('Ctrl Pts',(17.341,24.3979233185446,10.3766350494692));
#85325=CARTESIAN_POINT('Ctrl Pts',(17.341,24.6560576019166,10.4144296911714));
#85326=CARTESIAN_POINT('Ctrl Pts',(17.341,24.9149377889596,10.4424928180281));
#85327=CARTESIAN_POINT('Ctrl Pts',(17.341,25.171976331243,10.4703563069322));
#85328=CARTESIAN_POINT('Ctrl Pts',(17.341,25.4297503170471,10.4886263071145));
#85329=CARTESIAN_POINT('Ctrl Pts',(17.341,25.6877814236054,10.4971057263321));
#85330=CARTESIAN_POINT('Ctrl Pts',(17.341,25.8537611339476,10.5025601522128));
#85331=CARTESIAN_POINT('Ctrl Pts',(17.341,26.0198474887083,10.5039624655609));
#85332=CARTESIAN_POINT('Ctrl Pts',(17.341,26.1859144523977,10.5012488452782));
#85333=CARTESIAN_POINT('Ctrl Pts',(17.341,26.4435060609303,10.4970396648485));
#85334=CARTESIAN_POINT('Ctrl Pts',(17.341,26.7010514637349,10.4829300428959));
#85335=CARTESIAN_POINT('Ctrl Pts',(17.341,26.9580017760534,10.4591240892664));
#85336=CARTESIAN_POINT('Ctrl Pts',(17.341,27.2156042235232,10.4352577165658));
#85337=CARTESIAN_POINT('Ctrl Pts',(17.341,27.4726092240827,10.4016455486853));
#85338=CARTESIAN_POINT('Ctrl Pts',(17.341,27.7284529044781,10.3584422735481));
#85339=CARTESIAN_POINT('Ctrl Pts',(17.341,27.8681170757507,10.3348577565924));
#85340=CARTESIAN_POINT('Ctrl Pts',(17.341,28.0074349233039,10.3084141893606));
#85341=CARTESIAN_POINT('Ctrl Pts',(17.341,28.146312267496,10.2791306454767));
#85342=CARTESIAN_POINT('',(17.3409999839613,19.8194178862033,-6.18058216019384));
#85343=CARTESIAN_POINT('Origin',(17.3409999999995,21.3441513567948,1.29316405882314));
#85344=CARTESIAN_POINT('Ctrl Pts',(17.341,25.540762340228,-5.98239924878362));
#85345=CARTESIAN_POINT('Ctrl Pts',(17.341,25.4183996188332,-6.04858855516172));
#85346=CARTESIAN_POINT('Ctrl Pts',(17.341,25.293627346394,-6.10999579303368));
#85347=CARTESIAN_POINT('Ctrl Pts',(17.341,25.1668334048713,-6.16670216610432));
#85348=CARTESIAN_POINT('Ctrl Pts',(17.341,25.0371649034307,-6.22469413583013));
#85349=CARTESIAN_POINT('Ctrl Pts',(17.341,24.9053820043425,-6.27777033516398));
#85350=CARTESIAN_POINT('Ctrl Pts',(17.341,24.771845187989,-6.32602964024892));
#85351=CARTESIAN_POINT('Ctrl Pts',(17.341,24.6729857355588,-6.36175677981713));
#85352=CARTESIAN_POINT('Ctrl Pts',(17.341,24.5731638536018,-6.39484421795225));
#85353=CARTESIAN_POINT('Ctrl Pts',(17.341,24.4725076277925,-6.42533310314458));
#85354=CARTESIAN_POINT('Ctrl Pts',(17.341,24.4137637069362,-6.44312670353376));
#85355=CARTESIAN_POINT('Ctrl Pts',(17.341,24.3547359339088,-6.46003507521374));
#85356=CARTESIAN_POINT('Ctrl Pts',(17.341,24.2954455073458,-6.47606676524652));
#85357=CARTESIAN_POINT('Ctrl Pts',(17.341,24.2467280160254,-6.48923961228606));
#85358=CARTESIAN_POINT('Ctrl Pts',(17.341,24.1978356308289,-6.50181966029287));
#85359=CARTESIAN_POINT('Ctrl Pts',(17.341,24.1488067498374,-6.51380557918685));
#85360=CARTESIAN_POINT('Ctrl Pts',(17.341,24.0007014245001,-6.55001236957977));
#85361=CARTESIAN_POINT('Ctrl Pts',(17.341,23.8513020969686,-6.5808123761519));
#85362=CARTESIAN_POINT('Ctrl Pts',(17.341,23.7009841745541,-6.60634967722337));
#85363=CARTESIAN_POINT('Ctrl Pts',(17.341,23.5476129800787,-6.63240569440416));
#85364=CARTESIAN_POINT('Ctrl Pts',(17.341,23.3932853069637,-6.65298361480213));
#85365=CARTESIAN_POINT('Ctrl Pts',(17.341,23.2383461904164,-6.66823130644756));
#85366=CARTESIAN_POINT('Ctrl Pts',(17.341,23.1373547140553,-6.67816996444875));
#85367=CARTESIAN_POINT('Ctrl Pts',(17.341,23.0361023630569,-6.68584387994372));
#85368=CARTESIAN_POINT('Ctrl Pts',(17.341,22.934673477861,-6.69129118893674));
#85369=CARTESIAN_POINT('Ctrl Pts',(17.341,22.8806851312291,-6.69419067073187));
#85370=CARTESIAN_POINT('Ctrl Pts',(17.341,22.8266453434879,-6.69645930799709));
#85371=CARTESIAN_POINT('Ctrl Pts',(17.341,22.7725693409315,-6.69810238552906));
#85372=CARTESIAN_POINT('Ctrl Pts',(17.341,22.7271872751647,-6.69948130129744));
#85373=CARTESIAN_POINT('Ctrl Pts',(17.341,22.6817878595131,-6.70041931464329));
#85374=CARTESIAN_POINT('Ctrl Pts',(17.341,22.6363912203757,-6.70092013375722));
#85375=CARTESIAN_POINT('Ctrl Pts',(17.341,22.4688853069381,-6.70276807150637));
#85376=CARTESIAN_POINT('Ctrl Pts',(17.341,22.3013726898151,-6.69866601218014));
#85377=CARTESIAN_POINT('Ctrl Pts',(17.341,22.1342411971029,-6.68881383255924));
#85378=CARTESIAN_POINT('Ctrl Pts',(17.341,21.9639554414572,-6.67877571332584));
#85379=CARTESIAN_POINT('Ctrl Pts',(17.341,21.7940650425909,-6.66276887957955));
#85380=CARTESIAN_POINT('Ctrl Pts',(17.341,21.6249279438386,-6.64099010569175));
#85381=CARTESIAN_POINT('Ctrl Pts',(17.341,21.4510285893043,-6.61859812457362));
#85382=CARTESIAN_POINT('Ctrl Pts',(17.341,21.2779252433068,-6.59010512149647));
#85383=CARTESIAN_POINT('Ctrl Pts',(17.341,21.1059567043584,-6.55570169646653));
#85384=CARTESIAN_POINT('Ctrl Pts',(17.341,20.9315335584359,-6.52080721134196));
#85385=CARTESIAN_POINT('Ctrl Pts',(17.341,20.7582773397082,-6.47983282131137));
#85386=CARTESIAN_POINT('Ctrl Pts',(17.341,20.5864970100379,-6.43294640530162));
#85387=CARTESIAN_POINT('Ctrl Pts',(17.341,20.4116858195953,-6.38523273392849));
#85388=CARTESIAN_POINT('Ctrl Pts',(17.341,20.2384024855397,-6.33139701701376));
#85389=CARTESIAN_POINT('Ctrl Pts',(17.341,20.0669350139262,-6.27157747171442));
#85390=CARTESIAN_POINT('Ctrl Pts',(17.341,19.9839949222142,-6.24264231260461));
#85391=CARTESIAN_POINT('Ctrl Pts',(17.341,19.9014791913052,-6.21230648506642));
#85392=CARTESIAN_POINT('Ctrl Pts',(17.341,19.8194179780815,-6.18058202191849));
#85393=CARTESIAN_POINT('',(17.341,21.5,-6.08441629692198E-14));
#85394=CARTESIAN_POINT('Origin',(17.341,26.,-6.02930719096035E-14));
#85395=CARTESIAN_POINT('Ctrl Pts',(16.7615124374135,33.4249061655004,7.42433622827797));
#85396=CARTESIAN_POINT('Ctrl Pts',(16.8894584331897,32.474992220184,8.37432443882492));
#85397=CARTESIAN_POINT('Ctrl Pts',(17.1453376308892,30.2091713978346,9.89763205493));
#85398=CARTESIAN_POINT('Ctrl Pts',(17.6570832324356,24.8471265934024,11.0609731255039));
#85399=CARTESIAN_POINT('Ctrl Pts',(18.1688160401292,19.4649378970143,8.99752970904879));
#85400=CARTESIAN_POINT('Ctrl Pts',(18.6805488478228,16.2522102217688,4.55237376613912));
#85401=CARTESIAN_POINT('Ctrl Pts',(19.064348453593,15.2532613557681,0.57767028582841));
#85402=CARTESIAN_POINT('Ctrl Pts',(19.3202148574397,15.6321281971341,-2.13581025897831));
#85403=CARTESIAN_POINT('Ctrl Pts',(19.4481480593631,16.0679265366941,-3.4064522188774));
#85404=CARTESIAN_POINT('Ctrl Pts',(16.0591297509591,33.4249061655004,7.42433622827797));
#85405=CARTESIAN_POINT('Ctrl Pts',(16.1870757467353,32.474992220184,8.37432443882492));
#85406=CARTESIAN_POINT('Ctrl Pts',(16.4429549444349,30.2091713978346,9.89763205493));
#85407=CARTESIAN_POINT('Ctrl Pts',(16.9547005459813,24.8471265934024,11.0609731255039));
#85408=CARTESIAN_POINT('Ctrl Pts',(17.4664333536749,19.4649378970143,8.99752970904879));
#85409=CARTESIAN_POINT('Ctrl Pts',(17.9781661613684,16.2522102217688,4.55237376613912));
#85410=CARTESIAN_POINT('Ctrl Pts',(18.3619657671386,15.2532613557681,0.577670285828411));
#85411=CARTESIAN_POINT('Ctrl Pts',(18.6178321709854,15.6321281971341,-2.13581025897831));
#85412=CARTESIAN_POINT('Ctrl Pts',(18.7457653729088,16.0679265366941,-3.4064522188774));
#85413=CARTESIAN_POINT('Ctrl Pts',(15.3567470645047,33.4249061655004,7.42433622827797));
#85414=CARTESIAN_POINT('Ctrl Pts',(15.4846930602809,32.474992220184,8.37432443882493));
#85415=CARTESIAN_POINT('Ctrl Pts',(15.7405722579805,30.2091713978346,9.89763205493));
#85416=CARTESIAN_POINT('Ctrl Pts',(16.2523178595268,24.8471265934024,11.060973125504));
#85417=CARTESIAN_POINT('Ctrl Pts',(16.7640506672204,19.4649378970143,8.99752970904879));
#85418=CARTESIAN_POINT('Ctrl Pts',(17.275783474914,16.2522102217688,4.55237376613912));
#85419=CARTESIAN_POINT('Ctrl Pts',(17.6595830806842,15.2532613557681,0.577670285828411));
#85420=CARTESIAN_POINT('Ctrl Pts',(17.915449484531,15.6321281971341,-2.13581025897831));
#85421=CARTESIAN_POINT('Ctrl Pts',(18.0433826864543,16.0679265366941,-3.4064522188774));
#85422=CARTESIAN_POINT('Ctrl Pts',(14.6543643780503,33.4249061655004,7.42433622827796));
#85423=CARTESIAN_POINT('Ctrl Pts',(14.7823103738265,32.474992220184,8.37432443882492));
#85424=CARTESIAN_POINT('Ctrl Pts',(15.0381895715261,30.2091713978346,9.89763205493));
#85425=CARTESIAN_POINT('Ctrl Pts',(15.5499351730725,24.8471265934024,11.0609731255039));
#85426=CARTESIAN_POINT('Ctrl Pts',(16.0616679807661,19.4649378970143,8.99752970904879));
#85427=CARTESIAN_POINT('Ctrl Pts',(16.5734007884596,16.2522102217688,4.55237376613912));
#85428=CARTESIAN_POINT('Ctrl Pts',(16.9572003942298,15.2532613557681,0.57767028582841));
#85429=CARTESIAN_POINT('Ctrl Pts',(17.2130667980766,15.6321281971341,-2.13581025897831));
#85430=CARTESIAN_POINT('Ctrl Pts',(17.341,16.0679265366941,-3.4064522188774));
#85431=CARTESIAN_POINT('',(16.761525075775,33.4246212024587,7.42462120245876));
#85432=CARTESIAN_POINT('Ctrl Pts',(16.761525075775,33.4246212024587,7.42462120245875));
#85433=CARTESIAN_POINT('Ctrl Pts',(16.796415203332,33.1655752216426,7.68366718327491));
#85434=CARTESIAN_POINT('Ctrl Pts',(16.8312868468052,32.8928326264494,7.92856820410911));
#85435=CARTESIAN_POINT('Ctrl Pts',(16.8661515162646,32.6080803815643,8.15849134617175));
#85436=CARTESIAN_POINT('Ctrl Pts',(16.9013571533157,32.3205433322152,8.39066307803096));
#85437=CARTESIAN_POINT('Ctrl Pts',(16.9365556792779,32.0207598439169,8.60756302871267));
#85438=CARTESIAN_POINT('Ctrl Pts',(16.9717589452313,31.710429563843,8.80829510701351));
#85439=CARTESIAN_POINT('Ctrl Pts',(17.0068253488282,31.4013057778907,9.0082467842771));
#85440=CARTESIAN_POINT('Ctrl Pts',(17.0418964556319,31.0817162363085,9.19215646243076));
#85441=CARTESIAN_POINT('Ctrl Pts',(17.0769839790363,30.7533157721565,9.3590938754793));
#85442=CARTESIAN_POINT('Ctrl Pts',(17.0996969030388,30.5407349439604,9.46715612689669));
#85443=CARTESIAN_POINT('Ctrl Pts',(17.1224167060189,30.3244616354424,9.56810564435477));
#85444=CARTESIAN_POINT('Ctrl Pts',(17.1451465651708,30.1049414928425,9.66167885853807));
#85445=CARTESIAN_POINT('Ctrl Pts',(17.1720213888841,29.8453901645892,9.77231586770984));
#85446=CARTESIAN_POINT('Ctrl Pts',(17.1989367351104,29.5812233705055,9.87257656592876));
#85447=CARTESIAN_POINT('Ctrl Pts',(17.2258528491582,29.3134003424746,9.9620468904518));
#85448=CARTESIAN_POINT('Ctrl Pts',(17.252643297162,29.0468277274996,10.0510994956222));
#85449=CARTESIAN_POINT('Ctrl Pts',(17.2794345058345,28.7766335588408,10.1294624424491));
#85450=CARTESIAN_POINT('Ctrl Pts',(17.3061872747089,28.5037474425124,10.1967762920531));
#85451=CARTESIAN_POINT('Ctrl Pts',(17.3177998278266,28.3852959829343,10.2259951612382));
#85452=CARTESIAN_POINT('Ctrl Pts',(17.3294051382684,28.2663370545596,10.2531328098949));
#85453=CARTESIAN_POINT('Ctrl Pts',(17.341,28.1469452949575,10.2781625741404));
#85454=CARTESIAN_POINT('',(14.6544027596087,33.4246212024587,7.42462120245876));
#85455=CARTESIAN_POINT('',(14.6544027596087,33.4246212024587,7.42462120245876));
#85456=CARTESIAN_POINT('Ctrl Pts',(14.6544027596087,33.4246212024587,7.42462120245875));
#85457=CARTESIAN_POINT('Ctrl Pts',(14.7823359615321,32.4747656389599,8.37447676595761));
#85458=CARTESIAN_POINT('Ctrl Pts',(15.0382023653789,30.2090373444851,9.89766113894045));
#85459=CARTESIAN_POINT('Ctrl Pts',(15.5499351730725,24.8471265934024,11.0609731255039));
#85460=CARTESIAN_POINT('Ctrl Pts',(16.0616679807661,19.4649378970143,8.99752970904879));
#85461=CARTESIAN_POINT('Ctrl Pts',(16.5734007884596,16.2522102217688,4.55237376613912));
#85462=CARTESIAN_POINT('Ctrl Pts',(16.9572003942298,15.2532613557681,0.57767028582841));
#85463=CARTESIAN_POINT('Ctrl Pts',(17.2130667980766,15.6321281971341,-2.13581025897831));
#85464=CARTESIAN_POINT('Ctrl Pts',(17.341,16.0679265366941,-3.4064522188774));
#85465=CARTESIAN_POINT('Ctrl Pts',(17.341,31.8402330044652,5.84023300446519));
#85466=CARTESIAN_POINT('Ctrl Pts',(17.534158308075,30.7121434785588,6.96832253037151));
#85467=CARTESIAN_POINT('Ctrl Pts',(17.72731661615,29.250448427975,7.75863390468211));
#85468=CARTESIAN_POINT('Ctrl Pts',(17.920474924225,27.6887946776651,8.08483862730598));
#85469=CARTESIAN_POINT('Ctrl Pts',(17.147841691925,32.3683624037964,6.36836240379638));
#85470=CARTESIAN_POINT('Ctrl Pts',(17.341,31.1382602966705,7.59846451092218));
#85471=CARTESIAN_POINT('Ctrl Pts',(17.534158308075,29.5443848812828,8.460243354267));
#85472=CARTESIAN_POINT('Ctrl Pts',(17.72731661615,27.8415115500959,8.81594660958411));
#85473=CARTESIAN_POINT('Ctrl Pts',(16.95468338385,32.8964918031275,6.89649180312756));
#85474=CARTESIAN_POINT('Ctrl Pts',(17.147841691925,31.5643771147823,8.22860649147286));
#85475=CARTESIAN_POINT('Ctrl Pts',(17.341,29.8383213345905,9.1618528038519));
#85476=CARTESIAN_POINT('Ctrl Pts',(17.534158308075,27.9942284225267,9.54705459186225));
#85477=CARTESIAN_POINT('Ctrl Pts',(16.761525075775,33.4246212024587,7.42462120245875));
#85478=CARTESIAN_POINT('Ctrl Pts',(16.95468338385,31.990493932894,8.85874847202353));
#85479=CARTESIAN_POINT('Ctrl Pts',(17.147841691925,30.1322577878983,9.86346225343679));
#85480=CARTESIAN_POINT('Ctrl Pts',(17.341,28.1469452949574,10.2781625741404));
#85481=CARTESIAN_POINT('',(17.9511659638121,30.1719300090006,4.17193000900064));
#85482=CARTESIAN_POINT('Ctrl Pts',(14.7834604024327,21.7560634031344,-4.24050705242816));
#85483=CARTESIAN_POINT('Ctrl Pts',(14.9331947910706,22.3910092806787,-4.87597523762566));
#85484=CARTESIAN_POINT('Ctrl Pts',(15.2325288298794,23.9499464904882,-5.8557529849313));
#85485=CARTESIAN_POINT('Ctrl Pts',(15.6814625188592,26.6949161928493,-6.16638799654186));
#85486=CARTESIAN_POINT('Ctrl Pts',(16.1302614693721,29.3005937404032,-5.25296922685046));
#85487=CARTESIAN_POINT('Ctrl Pts',(16.5790604198849,31.2541512947311,-3.30156243078436));
#85488=CARTESIAN_POINT('Ctrl Pts',(17.0278593703977,32.1647858337878,-0.694650259068251));
#85489=CARTESIAN_POINT('Ctrl Pts',(17.4766583209106,31.8568326061558,2.04908452357241));
#85490=CARTESIAN_POINT('Ctrl Pts',(17.7758576212524,30.876857130788,3.60758722349281));
#85491=CARTESIAN_POINT('Ctrl Pts',(17.9254572714234,30.2422221771405,4.24222217714045));
#85492=CARTESIAN_POINT('Ctrl Pts',(14.3954830038832,20.6948350244358,-5.30087784765443));
#85493=CARTESIAN_POINT('Ctrl Pts',(14.5452173925211,21.4885539111445,-6.09524964898742));
#85494=CARTESIAN_POINT('Ctrl Pts',(14.84455143133,23.4373151369117,-7.32002821723511));
#85495=CARTESIAN_POINT('Ctrl Pts',(15.2934851203098,26.8686852320035,-7.70833985812943));
#85496=CARTESIAN_POINT('Ctrl Pts',(15.7422840708226,30.1259321176207,-6.56651383071689));
#85497=CARTESIAN_POINT('Ctrl Pts',(16.1910830213355,32.5679914835932,-4.12714303634316));
#85498=CARTESIAN_POINT('Ctrl Pts',(16.6398819718483,33.7063370624859,-0.868352799473312));
#85499=CARTESIAN_POINT('Ctrl Pts',(17.0886809223611,33.3213778058956,2.5614735749011));
#85500=CARTESIAN_POINT('Ctrl Pts',(17.387880222703,32.0963520661915,4.5096916383016));
#85501=CARTESIAN_POINT('Ctrl Pts',(17.5374798728739,31.3030218522465,5.30302185224656));
#85502=CARTESIAN_POINT('Ctrl Pts',(14.0075056053337,19.6336066457373,-6.3612486428807));
#85503=CARTESIAN_POINT('Ctrl Pts',(14.1572399939717,20.5860985416104,-7.31452406034918));
#85504=CARTESIAN_POINT('Ctrl Pts',(14.4565740327805,22.9246837833351,-8.78430344953894));
#85505=CARTESIAN_POINT('Ctrl Pts',(14.9055077217603,27.0424542711577,-9.250291719717));
#85506=CARTESIAN_POINT('Ctrl Pts',(15.3543066722731,30.9512704948381,-7.88005843458333));
#85507=CARTESIAN_POINT('Ctrl Pts',(15.8031056227859,33.8818316724552,-4.95272364190195));
#85508=CARTESIAN_POINT('Ctrl Pts',(16.2519045732988,35.2478882911839,-1.04205533987837));
#85509=CARTESIAN_POINT('Ctrl Pts',(16.7007035238116,34.7859230056355,3.0738626262298));
#85510=CARTESIAN_POINT('Ctrl Pts',(16.9999028241535,33.3158470015949,5.41179605311038));
#85511=CARTESIAN_POINT('Ctrl Pts',(17.1495024743244,32.3638215273526,6.36382152735266));
#85512=CARTESIAN_POINT('Ctrl Pts',(13.6195282067842,18.5723782670386,-7.42161943810697));
#85513=CARTESIAN_POINT('Ctrl Pts',(13.7692625954221,19.6836431720763,-8.53379847171094));
#85514=CARTESIAN_POINT('Ctrl Pts',(14.068596634231,22.4120524297584,-10.2485786818427));
#85515=CARTESIAN_POINT('Ctrl Pts',(14.5175303232108,27.2162233103119,-10.7922435813046));
#85516=CARTESIAN_POINT('Ctrl Pts',(14.9663292737237,31.7766088720556,-9.19360303844975));
#85517=CARTESIAN_POINT('Ctrl Pts',(15.4151282242365,35.1956718613173,-5.77830424746075));
#85518=CARTESIAN_POINT('Ctrl Pts',(15.8639271747493,36.7894395198819,-1.21575788028343));
#85519=CARTESIAN_POINT('Ctrl Pts',(16.3127261252621,36.2504682053753,3.58625167755849));
#85520=CARTESIAN_POINT('Ctrl Pts',(16.611925425604,34.5353419369983,6.31390046791915));
#85521=CARTESIAN_POINT('Ctrl Pts',(16.761525075775,33.4246212024587,7.42462120245876));
#85522=CARTESIAN_POINT('',(13.6199323608887,18.5753787991571,-7.42462120084289));
#85523=CARTESIAN_POINT('',(14.8095732174019,21.8280699909994,-4.17193000900062));
#85524=CARTESIAN_POINT('Ctrl Pts',(13.6199324221852,18.5753787975412,-7.42462120245874));
#85525=CARTESIAN_POINT('Ctrl Pts',(13.7695320723561,19.6860995320808,-8.53534193699833));
#85526=CARTESIAN_POINT('Ctrl Pts',(14.068731372698,22.4134943055532,-10.2487418519877));
#85527=CARTESIAN_POINT('Ctrl Pts',(14.5175303232108,27.2162233103119,-10.7922435813046));
#85528=CARTESIAN_POINT('Ctrl Pts',(14.9663292737237,31.7766088720556,-9.19360303844976));
#85529=CARTESIAN_POINT('Ctrl Pts',(15.4151282242365,35.1956718613173,-5.77830424746075));
#85530=CARTESIAN_POINT('Ctrl Pts',(15.8639271747493,36.7894395198819,-1.21575788028344));
#85531=CARTESIAN_POINT('Ctrl Pts',(16.3127261252621,36.2504682053753,3.58625167755849));
#85532=CARTESIAN_POINT('Ctrl Pts',(16.611925425604,34.5353419369983,6.31390046791915));
#85533=CARTESIAN_POINT('Ctrl Pts',(16.761525075775,33.4246212024587,7.42462120245876));
#85534=CARTESIAN_POINT('Origin',(-36.3408714641021,26.,7.7715611723761E-15));
#85535=CARTESIAN_POINT('',(-36.6591285358979,21.5,8.3226522319924E-15));
#85536=CARTESIAN_POINT('Origin',(-36.6591285358979,26.,7.7715611723761E-15));
#85537=CARTESIAN_POINT('',(-36.3408714641021,21.5,8.32265223199241E-15));
#85538=CARTESIAN_POINT('Origin',(36.3408714641021,26.,7.7715611723761E-15));
#85539=CARTESIAN_POINT('',(36.3408714641021,21.5,7.22047011275979E-15));
#85540=CARTESIAN_POINT('',(36.3408714641021,21.5,8.32265223199241E-15));
#85541=CARTESIAN_POINT('Origin',(36.3408714641021,26.,7.7715611723761E-15));
#85542=CARTESIAN_POINT('Origin',(36.3408714641021,26.,7.7715611723761E-15));
#85543=CARTESIAN_POINT('Ctrl Pts',(17.3410000905454,19.8194177305141,-6.18058226948589));
#85544=CARTESIAN_POINT('Ctrl Pts',(17.5772612984063,21.2796495627862,-7.64081410175804));
#85545=CARTESIAN_POINT('Ctrl Pts',(17.8135225062671,23.2719712067439,-8.55696250376816));
#85546=CARTESIAN_POINT('Ctrl Pts',(18.049783714128,25.3309930425917,-8.71502289559277));
#85547=CARTESIAN_POINT('Ctrl Pts',(17.1047388505631,20.465398263273,-5.53460173672703));
#85548=CARTESIAN_POINT('Ctrl Pts',(17.341000058424,21.7730099546209,-6.84221342807497));
#85549=CARTESIAN_POINT('Ctrl Pts',(17.5772612662848,23.5570986294383,-7.66260806336661));
#85550=CARTESIAN_POINT('Ctrl Pts',(17.8135224741457,25.4009161423779,-7.80414833917836));
#85551=CARTESIAN_POINT('Ctrl Pts',(16.8684776105808,21.1113787960318,-4.88862120396816));
#85552=CARTESIAN_POINT('Ctrl Pts',(17.1047388184417,22.2663703464555,-6.04361275439188));
#85553=CARTESIAN_POINT('Ctrl Pts',(17.3410000263025,23.8422260521326,-6.76825362296505));
#85554=CARTESIAN_POINT('Ctrl Pts',(17.5772612341634,25.470839242164,-6.89327378276394));
#85555=CARTESIAN_POINT('Ctrl Pts',(16.6322163705985,21.7573593287907,-4.24264067120929));
#85556=CARTESIAN_POINT('Ctrl Pts',(16.8684775784594,22.7597307382902,-5.24501208070881));
#85557=CARTESIAN_POINT('Ctrl Pts',(17.1047387863202,24.127353474827,-5.8738991825635));
#85558=CARTESIAN_POINT('Ctrl Pts',(17.3409999941811,25.5407623419502,-5.98239922634953));
#85559=CARTESIAN_POINT('',(17.7959954131985,18.5753787975412,-7.42462120245874));
#85560=CARTESIAN_POINT('Ctrl Pts',(11.5124058800916,18.5723781889139,-7.42161935992234));
#85561=CARTESIAN_POINT('Ctrl Pts',(11.6621402722384,19.6836431101435,-8.53379843028192));
#85562=CARTESIAN_POINT('Ctrl Pts',(11.961474314556,22.4120501365063,-10.2485800412561));
#85563=CARTESIAN_POINT('Ctrl Pts',(12.4104080070446,27.2162237256492,-10.7922402146103));
#85564=CARTESIAN_POINT('Ctrl Pts',(12.8592069575574,31.7766119901629,-9.19360275595219));
#85565=CARTESIAN_POINT('Ctrl Pts',(13.3080059080703,35.1956739272439,-5.77829971989694));
#85566=CARTESIAN_POINT('Ctrl Pts',(13.7568048585831,36.7894465571738,-1.21575346390194));
#85567=CARTESIAN_POINT('Ctrl Pts',(14.2057182183514,36.2503333440016,3.58748045005371));
#85568=CARTESIAN_POINT('Ctrl Pts',(14.5050319279488,34.5340300604887,6.31598641782465));
#85569=CARTESIAN_POINT('Ctrl Pts',(14.6547459873753,33.4220724221517,7.42716909445542));
#85570=CARTESIAN_POINT('Ctrl Pts',(11.1244284782739,19.6336065877144,-6.3612485669342));
#85571=CARTESIAN_POINT('Ctrl Pts',(11.2741628704205,20.5860984961286,-7.31452401456818));
#85572=CARTESIAN_POINT('Ctrl Pts',(11.5734969127382,22.9246818220518,-8.78430460238974));
#85573=CARTESIAN_POINT('Ctrl Pts',(12.0224306052268,27.0424546256895,-9.25028882105291));
#85574=CARTESIAN_POINT('Ctrl Pts',(12.4712295557397,30.9512731604903,-7.88005818138255));
#85575=CARTESIAN_POINT('Ctrl Pts',(12.9200285062525,33.8818334321429,-4.95271975426335));
#85576=CARTESIAN_POINT('Ctrl Pts',(13.3688274567653,35.2478943100302,-1.04205155302823));
#85577=CARTESIAN_POINT('Ctrl Pts',(13.8177408165336,34.785807400369,3.07491583239152));
#85578=CARTESIAN_POINT('Ctrl Pts',(14.117054526131,33.314722550393,5.41358396337687));
#85579=CARTESIAN_POINT('Ctrl Pts',(14.2667685855575,32.3616368974747,6.36600537796603));
#85580=CARTESIAN_POINT('Ctrl Pts',(10.736451076456,20.6948349865149,-5.30087777394604));
#85581=CARTESIAN_POINT('Ctrl Pts',(10.8861854686027,21.4885538821137,-6.09524959885446));
#85582=CARTESIAN_POINT('Ctrl Pts',(11.1855195109204,23.4373135075974,-7.3200291635234));
#85583=CARTESIAN_POINT('Ctrl Pts',(11.6344532034089,26.8686855257297,-7.7083374274955));
#85584=CARTESIAN_POINT('Ctrl Pts',(12.0832521539218,30.1259343308177,-6.5665136068129));
#85585=CARTESIAN_POINT('Ctrl Pts',(12.5320511044346,32.5679929370418,-4.12713978862975));
#85586=CARTESIAN_POINT('Ctrl Pts',(12.9808500549474,33.7063420628864,-0.86834964215453));
#85587=CARTESIAN_POINT('Ctrl Pts',(13.4297634147159,33.3212814567364,2.56235121472933));
#85588=CARTESIAN_POINT('Ctrl Pts',(13.7290771243132,32.0954150402973,4.51118150892909));
#85589=CARTESIAN_POINT('Ctrl Pts',(13.8787911837397,31.3012013727976,5.30484166147665));
#85590=CARTESIAN_POINT('Ctrl Pts',(10.3484736746382,21.7560633853155,-4.2405069809579));
#85591=CARTESIAN_POINT('Ctrl Pts',(10.498208066785,22.3910092680988,-4.87597518314072));
#85592=CARTESIAN_POINT('Ctrl Pts',(10.7975421091025,23.9499451931429,-5.85575372465707));
#85593=CARTESIAN_POINT('Ctrl Pts',(11.2464758015912,26.69491642577,-6.16638603393809));
#85594=CARTESIAN_POINT('Ctrl Pts',(11.695274752104,29.3005955011451,-5.25296903224326));
#85595=CARTESIAN_POINT('Ctrl Pts',(12.1440737026168,31.2541524419408,-3.30155982299616));
#85596=CARTESIAN_POINT('Ctrl Pts',(12.5928726531297,32.1647898157427,-0.694647731280824));
#85597=CARTESIAN_POINT('Ctrl Pts',(13.041786012898,31.856755513104,2.04978659706714));
#85598=CARTESIAN_POINT('Ctrl Pts',(13.3410997224955,30.8761075302016,3.60877905448131));
#85599=CARTESIAN_POINT('Ctrl Pts',(13.4908137819219,30.2407658481206,4.24367794498727));
#85600=CARTESIAN_POINT('',(14.6544027596087,33.4246212024587,7.42462120245876));
#85601=CARTESIAN_POINT('',(11.5128100581662,18.5753788014852,-7.42462119851477));
#85602=CARTESIAN_POINT('Ctrl Pts',(11.5128101060189,18.5753787975412,-7.42462120245874));
#85603=CARTESIAN_POINT('Ctrl Pts',(11.6624097561899,19.6860995320808,-8.53534193699833));
#85604=CARTESIAN_POINT('Ctrl Pts',(11.9616090565318,22.4134943055532,-10.2487418519877));
#85605=CARTESIAN_POINT('Ctrl Pts',(12.4104080070446,27.2162233103119,-10.7922435813046));
#85606=CARTESIAN_POINT('Ctrl Pts',(12.8592069575574,31.7766088720556,-9.19360303844976));
#85607=CARTESIAN_POINT('Ctrl Pts',(13.3080059080703,35.1956718613173,-5.77830424746075));
#85608=CARTESIAN_POINT('Ctrl Pts',(13.7568048585831,36.7894395198819,-1.21575788028344));
#85609=CARTESIAN_POINT('Ctrl Pts',(14.2056038090959,36.2504682053753,3.58625167755849));
#85610=CARTESIAN_POINT('Ctrl Pts',(14.5048031094378,34.5353419369983,6.31390046791915));
#85611=CARTESIAN_POINT('Ctrl Pts',(14.6544027596087,33.4246212024587,7.42462120245876));
#85612=CARTESIAN_POINT('',(11.5128100131985,18.5753787975412,-7.42462120245874));
#85613=CARTESIAN_POINT('Ctrl Pts',(13.6199324221852,18.5753787975412,-7.42462120245874));
#85614=CARTESIAN_POINT('Ctrl Pts',(13.7695320723561,19.6860995320808,-8.53534193699833));
#85615=CARTESIAN_POINT('Ctrl Pts',(14.068731372698,22.4134943055532,-10.2487418519877));
#85616=CARTESIAN_POINT('Ctrl Pts',(14.5175303232108,27.2162233103119,-10.7922435813046));
#85617=CARTESIAN_POINT('Ctrl Pts',(14.9663292737237,31.7766088720556,-9.19360303844976));
#85618=CARTESIAN_POINT('Ctrl Pts',(15.4151282242365,35.1956718613173,-5.77830424746075));
#85619=CARTESIAN_POINT('Ctrl Pts',(15.8639271747493,36.7894395198819,-1.21575788028344));
#85620=CARTESIAN_POINT('Ctrl Pts',(16.3127261252621,36.2504682053753,3.58625167755849));
#85621=CARTESIAN_POINT('Ctrl Pts',(16.611925425604,34.5353419369983,6.31390046791915));
#85622=CARTESIAN_POINT('Ctrl Pts',(16.761525075775,33.4246212024587,7.42462120245876));
#85623=CARTESIAN_POINT('Ctrl Pts',(12.9175583167964,18.5753787975412,-7.42462120245874));
#85624=CARTESIAN_POINT('Ctrl Pts',(13.0671579669674,19.6860995320808,-8.53534193699833));
#85625=CARTESIAN_POINT('Ctrl Pts',(13.3663572673093,22.4134943055532,-10.2487418519877));
#85626=CARTESIAN_POINT('Ctrl Pts',(13.8151562178221,27.2162233103119,-10.7922435813046));
#85627=CARTESIAN_POINT('Ctrl Pts',(14.2639551683349,31.7766088720556,-9.19360303844975));
#85628=CARTESIAN_POINT('Ctrl Pts',(14.7127541188477,35.1956718613173,-5.77830424746075));
#85629=CARTESIAN_POINT('Ctrl Pts',(15.1615530693606,36.7894395198819,-1.21575788028343));
#85630=CARTESIAN_POINT('Ctrl Pts',(15.6103520198734,36.2504682053753,3.58625167755849));
#85631=CARTESIAN_POINT('Ctrl Pts',(15.9095513202153,34.5353419369983,6.31390046791915));
#85632=CARTESIAN_POINT('Ctrl Pts',(16.0591509703862,33.4246212024587,7.42462120245876));
#85633=CARTESIAN_POINT('Ctrl Pts',(12.2151842114077,18.5753787975412,-7.42462120245874));
#85634=CARTESIAN_POINT('Ctrl Pts',(12.3647838615786,19.6860995320808,-8.53534193699833));
#85635=CARTESIAN_POINT('Ctrl Pts',(12.6639831619205,22.4134943055532,-10.2487418519877));
#85636=CARTESIAN_POINT('Ctrl Pts',(13.1127821124333,27.2162233103119,-10.7922435813046));
#85637=CARTESIAN_POINT('Ctrl Pts',(13.5615810629462,31.7766088720556,-9.19360303844976));
#85638=CARTESIAN_POINT('Ctrl Pts',(14.010380013459,35.1956718613173,-5.77830424746075));
#85639=CARTESIAN_POINT('Ctrl Pts',(14.4591789639718,36.7894395198819,-1.21575788028344));
#85640=CARTESIAN_POINT('Ctrl Pts',(14.9079779144847,36.2504682053753,3.5862516775585));
#85641=CARTESIAN_POINT('Ctrl Pts',(15.2071772148265,34.5353419369983,6.31390046791915));
#85642=CARTESIAN_POINT('Ctrl Pts',(15.3567768649975,33.4246212024587,7.42462120245876));
#85643=CARTESIAN_POINT('Ctrl Pts',(11.5128101060189,18.5753787975412,-7.42462120245874));
#85644=CARTESIAN_POINT('Ctrl Pts',(11.6624097561899,19.6860995320808,-8.53534193699833));
#85645=CARTESIAN_POINT('Ctrl Pts',(11.9616090565318,22.4134943055532,-10.2487418519877));
#85646=CARTESIAN_POINT('Ctrl Pts',(12.4104080070446,27.2162233103119,-10.7922435813046));
#85647=CARTESIAN_POINT('Ctrl Pts',(12.8592069575574,31.7766088720556,-9.19360303844976));
#85648=CARTESIAN_POINT('Ctrl Pts',(13.3080059080703,35.1956718613173,-5.77830424746075));
#85649=CARTESIAN_POINT('Ctrl Pts',(13.7568048585831,36.7894395198819,-1.21575788028344));
#85650=CARTESIAN_POINT('Ctrl Pts',(14.2056038090959,36.2504682053753,3.58625167755849));
#85651=CARTESIAN_POINT('Ctrl Pts',(14.5048031094378,34.5353419369983,6.31390046791915));
#85652=CARTESIAN_POINT('Ctrl Pts',(14.6544027596087,33.4246212024587,7.42462120245876));
#85653=CARTESIAN_POINT('',(11.5128100131985,18.5753787975412,-7.42462120245874));
#85654=CARTESIAN_POINT('Ctrl Pts',(8.50027478292078,21.7560622709221,-4.24050518741127));
#85655=CARTESIAN_POINT('Ctrl Pts',(8.65000928932408,22.3910083689704,-4.87597404391553));
#85656=CARTESIAN_POINT('Ctrl Pts',(8.94934344589831,23.9499417862674,-5.85575499156164));
#85657=CARTESIAN_POINT('Ctrl Pts',(9.39827725264349,26.6949167687136,-6.1663814341434));
#85658=CARTESIAN_POINT('Ctrl Pts',(9.84707620315632,29.3005989330943,-5.25296850297538));
#85659=CARTESIAN_POINT('Ctrl Pts',(10.2958751536691,31.2541543256308,-3.30155412730028));
#85660=CARTESIAN_POINT('Ctrl Pts',(10.7446741041819,32.164797852443,-0.694642440642849));
#85661=CARTESIAN_POINT('Ctrl Pts',(11.193587522373,31.8567579459617,2.0497923910259));
#85662=CARTESIAN_POINT('Ctrl Pts',(11.492901290393,30.8761067554945,3.60877937042535));
#85663=CARTESIAN_POINT('Ctrl Pts',(11.6426154082421,30.2407647654735,4.2436783491607));
#85664=CARTESIAN_POINT('Ctrl Pts',(8.11229733977657,20.6948333956204,-5.30087572958818));
#85665=CARTESIAN_POINT('Ctrl Pts',(8.26203184617986,21.488552589912,-6.09524840205955));
#85666=CARTESIAN_POINT('Ctrl Pts',(8.56136600275409,23.4373091532399,-7.32003102020338));
#85667=CARTESIAN_POINT('Ctrl Pts',(9.01029980949927,26.8686859868238,-7.70833196494417));
#85668=CARTESIAN_POINT('Ctrl Pts',(9.4590987600121,30.125938774815,-6.56651319007399));
#85669=CARTESIAN_POINT('Ctrl Pts',(9.90789771052492,32.5679955366945,-4.12713282258988));
#85670=CARTESIAN_POINT('Ctrl Pts',(10.3566966610378,33.7063523966073,-0.868343060934558));
#85671=CARTESIAN_POINT('Ctrl Pts',(10.8056100792287,33.3212847709717,2.56235855306593));
#85672=CARTESIAN_POINT('Ctrl Pts',(11.1049238472488,32.0954142991773,4.51118207210694));
#85673=CARTESIAN_POINT('Ctrl Pts',(11.254637965098,31.3012002171171,5.30484236454325));
#85674=CARTESIAN_POINT('Ctrl Pts',(7.72431989663235,19.6336045203188,-6.36124627176508));
#85675=CARTESIAN_POINT('Ctrl Pts',(7.87405440303564,20.5860968108534,-7.31452276020356));
#85676=CARTESIAN_POINT('Ctrl Pts',(8.17338855960988,22.9246765202122,-8.78430704884514));
#85677=CARTESIAN_POINT('Ctrl Pts',(8.62232236635506,27.042455204934,-9.25028249574493));
#85678=CARTESIAN_POINT('Ctrl Pts',(9.07112131686788,30.9512786165357,-7.88005787717262));
#85679=CARTESIAN_POINT('Ctrl Pts',(9.51992026738071,33.8818367477582,-4.95271151787948));
#85680=CARTESIAN_POINT('Ctrl Pts',(9.96871921789354,35.2479069407715,-1.04204368122627));
#85681=CARTESIAN_POINT('Ctrl Pts',(10.4176326360845,34.7858115959818,3.07492471510595));
#85682=CARTESIAN_POINT('Ctrl Pts',(10.7169464041046,33.3147218428599,5.41358477378853));
#85683=CARTESIAN_POINT('Ctrl Pts',(10.8666605219537,32.3616356687608,6.3660063799258));
#85684=CARTESIAN_POINT('Ctrl Pts',(7.33634245348814,18.572375645017,-7.42161681394198));
#85685=CARTESIAN_POINT('Ctrl Pts',(7.48607695989143,19.6836410317949,-8.53379711834756));
#85686=CARTESIAN_POINT('Ctrl Pts',(7.78541111646566,22.4120438871847,-10.2485830774869));
#85687=CARTESIAN_POINT('Ctrl Pts',(8.23434492321084,27.2162244230442,-10.7922330265457));
#85688=CARTESIAN_POINT('Ctrl Pts',(8.68314387372367,31.7766184582563,-9.19360256427123));
#85689=CARTESIAN_POINT('Ctrl Pts',(9.13194282423649,35.1956779588219,-5.77829021316908));
#85690=CARTESIAN_POINT('Ctrl Pts',(9.58074177474933,36.7894614849358,-1.21574430151798));
#85691=CARTESIAN_POINT('Ctrl Pts',(10.0296551929403,36.2503384209919,3.58749087714597));
#85692=CARTESIAN_POINT('Ctrl Pts',(10.3289689609603,34.5340293865426,6.31598747547012));
#85693=CARTESIAN_POINT('Ctrl Pts',(10.4786830788095,33.4220711204044,7.42717039530835));
#85694=CARTESIAN_POINT('',(7.33674696088869,18.5753787991571,-7.42462120084289));
#85695=CARTESIAN_POINT('',(8.52638781740187,21.8280699909994,-4.17193000900062));
#85696=CARTESIAN_POINT('',(10.478339675775,33.4246212024587,7.42462120245876));
#85697=CARTESIAN_POINT('Ctrl Pts',(7.33674702218519,18.5753787975412,-7.42462120245874));
#85698=CARTESIAN_POINT('Ctrl Pts',(7.48634667235613,19.6860995320808,-8.53534193699833));
#85699=CARTESIAN_POINT('Ctrl Pts',(7.78554597269801,22.4134870257429,-10.2487463857135));
#85700=CARTESIAN_POINT('Ctrl Pts',(8.23434492321084,27.2162244230442,-10.7922330265457));
#85701=CARTESIAN_POINT('Ctrl Pts',(8.68314387372367,31.7766184582563,-9.19360256427123));
#85702=CARTESIAN_POINT('Ctrl Pts',(9.13194282423649,35.1956779588219,-5.77829021316908));
#85703=CARTESIAN_POINT('Ctrl Pts',(9.58074177474933,36.7894614849358,-1.21574430151798));
#85704=CARTESIAN_POINT('Ctrl Pts',(10.0295407252621,36.250475891076,3.58626610827892));
#85705=CARTESIAN_POINT('Ctrl Pts',(10.328740025604,34.5353419369983,6.31390046791915));
#85706=CARTESIAN_POINT('Ctrl Pts',(10.478339675775,33.4246212024587,7.42462120245876));
#85707=CARTESIAN_POINT('',(11.6679805638121,30.1719300090006,4.17193000900064));
#85708=CARTESIAN_POINT('Ctrl Pts',(5.22922008610955,18.5723752649374,-7.42161643355513));
#85709=CARTESIAN_POINT('Ctrl Pts',(5.37895460958362,19.6836407231716,-8.53379692106834));
#85710=CARTESIAN_POINT('Ctrl Pts',(5.67828878322864,22.4120408496955,-10.2485849356457));
#85711=CARTESIAN_POINT('Ctrl Pts',(6.12722260704461,27.2162246994806,-10.7922291011963));
#85712=CARTESIAN_POINT('Ctrl Pts',(6.57602155755744,31.7766218825448,-9.19360269140816));
#85713=CARTESIAN_POINT('Ctrl Pts',(7.02482050807027,35.1956799398728,-5.77828511785068));
#85714=CARTESIAN_POINT('Ctrl Pts',(7.4736194585831,36.7894695685334,-1.21573946002377));
#85715=CARTESIAN_POINT('Ctrl Pts',(7.9225324577569,36.2503415768864,3.58749169207723));
#85716=CARTESIAN_POINT('Ctrl Pts',(8.22184580675976,34.5340341899288,6.31597983204138));
#85717=CARTESIAN_POINT('Ctrl Pts',(8.37155950559168,33.4220804567874,7.42716106543041));
#85718=CARTESIAN_POINT('Ctrl Pts',(4.84124263456142,19.6336042175304,-6.36124592275786));
#85719=CARTESIAN_POINT('Ctrl Pts',(4.99097715803549,20.5860965658729,-7.3145225647003));
#85720=CARTESIAN_POINT('Ctrl Pts',(5.29031133168052,22.9246739278113,-8.78430860980025));
#85721=CARTESIAN_POINT('Ctrl Pts',(5.73924515549648,27.0424554381102,-9.25027909783365));
#85722=CARTESIAN_POINT('Ctrl Pts',(6.18804410600931,30.9512815336981,-7.88005795769227));
#85723=CARTESIAN_POINT('Ctrl Pts',(6.63684305652214,33.8818384173056,-4.95270713267683));
#85724=CARTESIAN_POINT('Ctrl Pts',(7.08564200703497,35.2479138360262,-1.04203952770266));
#85725=CARTESIAN_POINT('Ctrl Pts',(7.53455500620877,34.785814269252,3.07492540250052));
#85726=CARTESIAN_POINT('Ctrl Pts',(7.83386835521163,33.3147259335466,5.41357820287516));
#85727=CARTESIAN_POINT('Ctrl Pts',(7.98358205404355,32.3616436482293,6.36599836007736));
#85728=CARTESIAN_POINT('Ctrl Pts',(4.45326518301329,20.6948331701234,-5.30087541196059));
#85729=CARTESIAN_POINT('Ctrl Pts',(4.60299970648736,21.4885524085742,-6.09524820833226));
#85730=CARTESIAN_POINT('Ctrl Pts',(4.90233388013239,23.437307005927,-7.32003228395488));
#85731=CARTESIAN_POINT('Ctrl Pts',(5.35126770394836,26.86868617674,-7.70832909447099));
#85732=CARTESIAN_POINT('Ctrl Pts',(5.80006665446118,30.1259411848514,-6.56651322397638));
#85733=CARTESIAN_POINT('Ctrl Pts',(6.24886560497401,32.5679968947386,-4.12712914750298));
#85734=CARTESIAN_POINT('Ctrl Pts',(6.69766455548684,33.7063581035188,-0.868339595381541));
#85735=CARTESIAN_POINT('Ctrl Pts',(7.14657755466065,33.3212869616176,2.56235911292381));
#85736=CARTESIAN_POINT('Ctrl Pts',(7.4458909036635,32.0954176771643,4.51117657370893));
#85737=CARTESIAN_POINT('Ctrl Pts',(7.59560460249543,31.3012068396711,5.3048356547243));
#85738=CARTESIAN_POINT('Ctrl Pts',(4.06528773146516,21.7560621227164,-4.24050490116332));
#85739=CARTESIAN_POINT('Ctrl Pts',(4.21502225493925,22.3910082512754,-4.87597385196422));
#85740=CARTESIAN_POINT('Ctrl Pts',(4.51435642858426,23.9499400840428,-5.8557559581095));
#85741=CARTESIAN_POINT('Ctrl Pts',(4.96329025240023,26.6949169153697,-6.16637909110834));
#85742=CARTESIAN_POINT('Ctrl Pts',(5.41208920291306,29.3006008360047,-5.25296849026049));
#85743=CARTESIAN_POINT('Ctrl Pts',(5.86088815342589,31.2541553721714,-3.30155116232912));
#85744=CARTESIAN_POINT('Ctrl Pts',(6.30968710393871,32.1648023710115,-0.694639663060422));
#85745=CARTESIAN_POINT('Ctrl Pts',(6.75860010311252,31.8567596539832,2.0497928233471));
#85746=CARTESIAN_POINT('Ctrl Pts',(7.05791345211538,30.876109420782,3.60877494454271));
#85747=CARTESIAN_POINT('Ctrl Pts',(7.2076271509473,30.2407700311129,4.24367294937125));
#85748=CARTESIAN_POINT('',(8.37121735960874,33.4246212024587,7.42462120245876));
#85749=CARTESIAN_POINT('',(8.37121735960875,33.4246212024587,7.42462120245876));
#85750=CARTESIAN_POINT('',(5.22962465816628,18.5753788014852,-7.42462119851477));
#85751=CARTESIAN_POINT('Ctrl Pts',(5.22962470601896,18.5753787975412,-7.42462120245874));
#85752=CARTESIAN_POINT('Ctrl Pts',(5.3792243561899,19.6860995320808,-8.53534193699833));
#85753=CARTESIAN_POINT('Ctrl Pts',(5.67842365653178,22.4134870257429,-10.2487463857135));
#85754=CARTESIAN_POINT('Ctrl Pts',(6.12722260704461,27.2162244230442,-10.7922330265457));
#85755=CARTESIAN_POINT('Ctrl Pts',(6.57602155755744,31.7766184582563,-9.19360256427123));
#85756=CARTESIAN_POINT('Ctrl Pts',(7.02482050807026,35.1956779588219,-5.77829021316908));
#85757=CARTESIAN_POINT('Ctrl Pts',(7.47361945858309,36.7894614849358,-1.21574430151798));
#85758=CARTESIAN_POINT('Ctrl Pts',(7.92241840909592,36.250475891076,3.58626610827892));
#85759=CARTESIAN_POINT('Ctrl Pts',(8.22161770943781,34.5353419369983,6.31390046791915));
#85760=CARTESIAN_POINT('Ctrl Pts',(8.37121735960875,33.4246212024587,7.42462120245876));
#85761=CARTESIAN_POINT('',(5.22962461319854,18.5753787975412,-7.42462120245874));
#85762=CARTESIAN_POINT('Ctrl Pts',(7.33674702218519,18.5753787975412,-7.42462120245874));
#85763=CARTESIAN_POINT('Ctrl Pts',(7.48634667235613,19.6860995320808,-8.53534193699833));
#85764=CARTESIAN_POINT('Ctrl Pts',(7.78554597269801,22.4134870257429,-10.2487463857135));
#85765=CARTESIAN_POINT('Ctrl Pts',(8.23434492321084,27.2162244230442,-10.7922330265457));
#85766=CARTESIAN_POINT('Ctrl Pts',(8.68314387372367,31.7766184582563,-9.19360256427123));
#85767=CARTESIAN_POINT('Ctrl Pts',(9.13194282423649,35.1956779588219,-5.77829021316908));
#85768=CARTESIAN_POINT('Ctrl Pts',(9.58074177474933,36.7894614849358,-1.21574430151798));
#85769=CARTESIAN_POINT('Ctrl Pts',(10.0295407252621,36.250475891076,3.58626610827892));
#85770=CARTESIAN_POINT('Ctrl Pts',(10.328740025604,34.5353419369983,6.31390046791915));
#85771=CARTESIAN_POINT('Ctrl Pts',(10.478339675775,33.4246212024587,7.42462120245876));
#85772=CARTESIAN_POINT('Ctrl Pts',(6.63437291679644,18.5753787975412,-7.42462120245874));
#85773=CARTESIAN_POINT('Ctrl Pts',(6.78397256696739,19.6860995320808,-8.53534193699833));
#85774=CARTESIAN_POINT('Ctrl Pts',(7.08317186730927,22.4134870257429,-10.2487463857135));
#85775=CARTESIAN_POINT('Ctrl Pts',(7.5319708178221,27.2162244230442,-10.7922330265457));
#85776=CARTESIAN_POINT('Ctrl Pts',(7.98076976833493,31.7766184582563,-9.19360256427123));
#85777=CARTESIAN_POINT('Ctrl Pts',(8.42956871884775,35.1956779588219,-5.77829021316908));
#85778=CARTESIAN_POINT('Ctrl Pts',(8.87836766936058,36.7894614849358,-1.21574430151798));
#85779=CARTESIAN_POINT('Ctrl Pts',(9.3271666198734,36.250475891076,3.58626610827891));
#85780=CARTESIAN_POINT('Ctrl Pts',(9.62636592021529,34.5353419369983,6.31390046791915));
#85781=CARTESIAN_POINT('Ctrl Pts',(9.77596557038624,33.4246212024587,7.42462120245876));
#85782=CARTESIAN_POINT('Ctrl Pts',(5.9319988114077,18.5753787975412,-7.42462120245874));
#85783=CARTESIAN_POINT('Ctrl Pts',(6.08159846157864,19.6860995320808,-8.53534193699833));
#85784=CARTESIAN_POINT('Ctrl Pts',(6.38079776192053,22.4134870257429,-10.2487463857135));
#85785=CARTESIAN_POINT('Ctrl Pts',(6.82959671243335,27.2162244230442,-10.7922330265457));
#85786=CARTESIAN_POINT('Ctrl Pts',(7.27839566294618,31.7766184582563,-9.19360256427123));
#85787=CARTESIAN_POINT('Ctrl Pts',(7.72719461345901,35.1956779588219,-5.77829021316908));
#85788=CARTESIAN_POINT('Ctrl Pts',(8.17599356397184,36.7894614849358,-1.21574430151798));
#85789=CARTESIAN_POINT('Ctrl Pts',(8.62479251448466,36.250475891076,3.58626610827892));
#85790=CARTESIAN_POINT('Ctrl Pts',(8.92399181482655,34.5353419369983,6.31390046791915));
#85791=CARTESIAN_POINT('Ctrl Pts',(9.07359146499749,33.4246212024587,7.42462120245876));
#85792=CARTESIAN_POINT('Ctrl Pts',(5.22962470601896,18.5753787975412,-7.42462120245874));
#85793=CARTESIAN_POINT('Ctrl Pts',(5.3792243561899,19.6860995320808,-8.53534193699833));
#85794=CARTESIAN_POINT('Ctrl Pts',(5.67842365653178,22.4134870257429,-10.2487463857135));
#85795=CARTESIAN_POINT('Ctrl Pts',(6.12722260704461,27.2162244230442,-10.7922330265457));
#85796=CARTESIAN_POINT('Ctrl Pts',(6.57602155755744,31.7766184582563,-9.19360256427123));
#85797=CARTESIAN_POINT('Ctrl Pts',(7.02482050807026,35.1956779588219,-5.77829021316908));
#85798=CARTESIAN_POINT('Ctrl Pts',(7.47361945858309,36.7894614849358,-1.21574430151798));
#85799=CARTESIAN_POINT('Ctrl Pts',(7.92241840909592,36.250475891076,3.58626610827892));
#85800=CARTESIAN_POINT('Ctrl Pts',(8.22161770943781,34.5353419369983,6.31390046791915));
#85801=CARTESIAN_POINT('Ctrl Pts',(8.37121735960875,33.4246212024587,7.42462120245876));
#85802=CARTESIAN_POINT('',(5.22962461319854,18.5753787975412,-7.42462120245874));
#85803=CARTESIAN_POINT('',(8.37121735960875,33.4246212024587,7.42462120245876));
#85804=CARTESIAN_POINT('Ctrl Pts',(2.21708909116458,21.7560607660849,-4.24050270859201));
#85805=CARTESIAN_POINT('Ctrl Pts',(2.36682375409141,22.3910071569996,-4.8759724572093));
#85806=CARTESIAN_POINT('Ctrl Pts',(2.66615806718916,23.9499357751967,-5.85575779538566));
#85807=CARTESIAN_POINT('Ctrl Pts',(3.11509203045787,26.6949170540957,-6.16637363300278));
#85808=CARTESIAN_POINT('Ctrl Pts',(3.5638909809707,29.3006045977601,-5.25296843898344));
#85809=CARTESIAN_POINT('Ctrl Pts',(4.01268993148352,31.2541569977362,-3.30154467940645));
#85810=CARTESIAN_POINT('Ctrl Pts',(4.46148888199635,32.1648116395084,-0.694633848166408));
#85811=CARTESIAN_POINT('Ctrl Pts',(4.91040191516051,31.856762106403,2.04979928901456));
#85812=CARTESIAN_POINT('Ctrl Pts',(5.20971529815371,30.8761087161373,3.60877493875489));
#85813=CARTESIAN_POINT('Ctrl Pts',(5.35942903097598,30.2407691812814,4.2436729644246));
#85814=CARTESIAN_POINT('Ctrl Pts',(1.82911158874891,20.6948312307416,-5.3008729144373));
#85815=CARTESIAN_POINT('Ctrl Pts',(1.97884625167573,21.4885508335847,-6.09524674458824));
#85816=CARTESIAN_POINT('Ctrl Pts',(2.27818056477349,23.4373015019899,-7.3200349166553));
#85817=CARTESIAN_POINT('Ctrl Pts',(2.72711452804219,26.8686863900293,-7.70832262534693));
#85818=CARTESIAN_POINT('Ctrl Pts',(3.17591347855502,30.1259460766487,-6.56651346128885));
#85819=CARTESIAN_POINT('Ctrl Pts',(3.62471242906785,32.5679992282681,-4.12712123291655));
#85820=CARTESIAN_POINT('Ctrl Pts',(4.07351137958068,33.7063700434066,-0.868332366286651));
#85821=CARTESIAN_POINT('Ctrl Pts',(4.52242441274482,33.3212903633405,2.56236731299668));
#85822=CARTESIAN_POINT('Ctrl Pts',(4.82173779573804,32.0954170761057,4.51117677354287));
#85823=CARTESIAN_POINT('Ctrl Pts',(4.9714515285603,31.3012060206651,5.30483591704091));
#85824=CARTESIAN_POINT('Ctrl Pts',(1.44113408633323,19.6336016953983,-6.36124312028259));
#85825=CARTESIAN_POINT('Ctrl Pts',(1.59086874926006,20.5860945101698,-7.31452103196718));
#85826=CARTESIAN_POINT('Ctrl Pts',(1.89020306235781,22.924667228783,-8.78431203792493));
#85827=CARTESIAN_POINT('Ctrl Pts',(2.33913702562652,27.042455725963,-9.25027161769108));
#85828=CARTESIAN_POINT('Ctrl Pts',(2.78793597613934,30.9512875555375,-7.88005848359427));
#85829=CARTESIAN_POINT('Ctrl Pts',(3.23673492665217,33.8818414587999,-4.95269778642664));
#85830=CARTESIAN_POINT('Ctrl Pts',(3.685533877165,35.2479284473048,-1.0420308844069));
#85831=CARTESIAN_POINT('Ctrl Pts',(4.13444691032915,34.7858186202782,3.07493533697882));
#85832=CARTESIAN_POINT('Ctrl Pts',(4.43376029332236,33.314725436074,5.41357860833083));
#85833=CARTESIAN_POINT('Ctrl Pts',(4.58347402614463,32.3616428600489,6.36599886965723));
#85834=CARTESIAN_POINT('Ctrl Pts',(1.05315658391756,18.5723721600548,-7.42161332612787));
#85835=CARTESIAN_POINT('Ctrl Pts',(1.20289124684438,19.683638186755,-8.53379531934611));
#85836=CARTESIAN_POINT('Ctrl Pts',(1.50222555994213,22.4120329555762,-10.2485891591946));
#85837=CARTESIAN_POINT('Ctrl Pts',(1.95115952321084,27.2162250618967,-10.7922206100352));
#85838=CARTESIAN_POINT('Ctrl Pts',(2.39995847372367,31.7766290344261,-9.19360350589968));
#85839=CARTESIAN_POINT('Ctrl Pts',(2.8487574242365,35.1956836893318,-5.77827433993674));
#85840=CARTESIAN_POINT('Ctrl Pts',(3.29755637474933,36.7894868512029,-1.21572940252715));
#85841=CARTESIAN_POINT('Ctrl Pts',(3.74646940791347,36.2503468772158,3.58750336096094));
#85842=CARTESIAN_POINT('Ctrl Pts',(4.04578279090669,34.5340337960423,6.31598044311881));
#85843=CARTESIAN_POINT('Ctrl Pts',(4.19549652372895,33.4220796994326,7.42716182227354));
#85844=CARTESIAN_POINT('',(1.05356156088868,18.5753787991571,-7.42462120084289));
#85845=CARTESIAN_POINT('',(2.24320241740187,21.8280699909994,-4.17193000900062));
#85846=CARTESIAN_POINT('',(4.19515427577498,33.4246212024587,7.42462120245876));
#85847=CARTESIAN_POINT('Ctrl Pts',(1.05356162218519,18.5753787975412,-7.42462120245874));
#85848=CARTESIAN_POINT('Ctrl Pts',(1.20316127235613,19.6860995320808,-8.53534193699833));
#85849=CARTESIAN_POINT('Ctrl Pts',(1.50236057269802,22.4134777721174,-10.2487526513479));
#85850=CARTESIAN_POINT('Ctrl Pts',(1.95115952321084,27.2162250618967,-10.7922206100352));
#85851=CARTESIAN_POINT('Ctrl Pts',(2.39995847372367,31.7766290344261,-9.19360350589968));
#85852=CARTESIAN_POINT('Ctrl Pts',(2.8487574242365,35.1956836893318,-5.77827433993674));
#85853=CARTESIAN_POINT('Ctrl Pts',(3.29755637474932,36.7894868512029,-1.21572940252715));
#85854=CARTESIAN_POINT('Ctrl Pts',(3.74635532526215,36.2504838893164,3.58628271132926));
#85855=CARTESIAN_POINT('Ctrl Pts',(4.04555462560404,34.5353419369983,6.31390046791915));
#85856=CARTESIAN_POINT('Ctrl Pts',(4.19515427577498,33.4246212024587,7.42462120245876));
#85857=CARTESIAN_POINT('',(5.38479516381208,30.1719300090006,4.17193000900064));
#85858=CARTESIAN_POINT('Ctrl Pts',(-1.0539654241159,18.5723702242316,-7.42161366308853));
#85859=CARTESIAN_POINT('Ctrl Pts',(-0.904230725318819,19.683636569112,-8.53379621253979));
#85860=CARTESIAN_POINT('Ctrl Pts',(-0.60489637635079,22.4120283617824,-10.2485932995738));
#85861=CARTESIAN_POINT('Ctrl Pts',(-0.155962377211819,27.2162253197193,
-10.7922175564503));
#85862=CARTESIAN_POINT('Ctrl Pts',(0.292836573301009,31.7766337359551,-9.19360566949464));
#85863=CARTESIAN_POINT('Ctrl Pts',(0.741635523813836,35.1956868609254,-5.77826939950743));
#85864=CARTESIAN_POINT('Ctrl Pts',(1.19043447432666,36.789497943561,-1.21572426912529));
#85865=CARTESIAN_POINT('Ctrl Pts',(1.63934707394011,36.2503516882648,3.58750543382354));
#85866=CARTESIAN_POINT('Ctrl Pts',(1.93866002338263,34.5340400726463,6.31597350110576));
#85867=CARTESIAN_POINT('Ctrl Pts',(2.08837332265419,33.4220904959639,7.42715330588487));
#85868=CARTESIAN_POINT('Ctrl Pts',(-1.44194308063557,19.6336002952009,-6.36124315026631));
#85869=CARTESIAN_POINT('Ctrl Pts',(-1.29220838183848,20.5860933439363,-7.31452149992352));
#85870=CARTESIAN_POINT('Ctrl Pts',(-0.992874032870451,22.9246634164647,
-8.78431522931743));
#85871=CARTESIAN_POINT('Ctrl Pts',(-0.54394003373148,27.0424559045324,-9.25026862400477));
#85872=CARTESIAN_POINT('Ctrl Pts',(-0.0951410832186525,30.9512913838673,
-7.88006001743081));
#85873=CARTESIAN_POINT('Ctrl Pts',(0.353657867294175,33.8818438565437,-4.95269335034525));
#85874=CARTESIAN_POINT('Ctrl Pts',(0.802456817807003,35.247937578541,-1.04202644204568));
#85875=CARTESIAN_POINT('Ctrl Pts',(1.25136941742045,34.7858223864565,3.07493698856269));
#85876=CARTESIAN_POINT('Ctrl Pts',(1.55068236686297,33.3147305182722,5.41357243789115));
#85877=CARTESIAN_POINT('Ctrl Pts',(1.70039566613453,32.3616518551653,6.3659913110293));
#85878=CARTESIAN_POINT('Ctrl Pts',(-1.82992073715523,20.69483036617,-5.30087263744408));
#85879=CARTESIAN_POINT('Ctrl Pts',(-1.68018603835815,21.4885501187606,-6.09524678730726));
#85880=CARTESIAN_POINT('Ctrl Pts',(-1.38085168939011,23.4372984711471,-7.32003715906107));
#85881=CARTESIAN_POINT('Ctrl Pts',(-0.931917690251141,26.8686864893455,
-7.70831969155928));
#85882=CARTESIAN_POINT('Ctrl Pts',(-0.483118739738314,30.1259490317793,
-6.566514365367));
#85883=CARTESIAN_POINT('Ctrl Pts',(-0.0343197892254864,32.5680008521621,
-4.12711730118307));
#85884=CARTESIAN_POINT('Ctrl Pts',(0.414479161287341,33.706377213521,-0.868328614966077));
#85885=CARTESIAN_POINT('Ctrl Pts',(0.863391760900794,33.3212930846483,2.56236854330184));
#85886=CARTESIAN_POINT('Ctrl Pts',(1.1627047103433,32.0954209638981,4.51117137467655));
#85887=CARTESIAN_POINT('Ctrl Pts',(1.31241800961487,31.3012132143666,5.30482931617372));
#85888=CARTESIAN_POINT('Ctrl Pts',(-2.21789839367489,21.7560604371392,-4.24050212462184));
#85889=CARTESIAN_POINT('Ctrl Pts',(-2.0681636948778,22.3910068935847,-4.87597207469099));
#85890=CARTESIAN_POINT('Ctrl Pts',(-1.76882934590978,23.9499335258294,-5.8557590888047));
#85891=CARTESIAN_POINT('Ctrl Pts',(-1.3198953467708,26.6949170741586,-6.16637075911378));
#85892=CARTESIAN_POINT('Ctrl Pts',(-0.871096396257976,29.3006066796915,
-5.25296871330317));
#85893=CARTESIAN_POINT('Ctrl Pts',(-0.422297445745148,31.2541578477804,
-3.30154125202089));
#85894=CARTESIAN_POINT('Ctrl Pts',(0.0265015047676796,32.164816848501,-0.694630787886463));
#85895=CARTESIAN_POINT('Ctrl Pts',(0.475414104381133,31.8567637828401,2.04980009804098));
#85896=CARTESIAN_POINT('Ctrl Pts',(0.774727053823643,30.8761114095239,3.60877031146195));
#85897=CARTESIAN_POINT('Ctrl Pts',(0.924440353095209,30.240774573568,4.24366732131814));
#85898=CARTESIAN_POINT('',(2.08803195960875,33.4246212024587,7.42462120245876));
#85899=CARTESIAN_POINT('',(2.08803195960875,33.4246212024587,7.42462120245876));
#85900=CARTESIAN_POINT('',(-1.05356074183372,18.5753788014852,-7.42462119851477));
#85901=CARTESIAN_POINT('Ctrl Pts',(-1.05356069398104,18.5753787975412,-7.42462120245874));
#85902=CARTESIAN_POINT('Ctrl Pts',(-0.923480593410918,19.5411742702521,
-8.39041667516965));
#85903=CARTESIAN_POINT('Ctrl Pts',(-0.793390386445168,20.6983162097813,
-9.16424028291836));
#85904=CARTESIAN_POINT('Ctrl Pts',(-0.514417007370215,23.4005592311826,
-10.293571643669));
#85905=CARTESIAN_POINT('Ctrl Pts',(-0.383476568361032,24.789559828435,-10.495214302546));
#85906=CARTESIAN_POINT('Ctrl Pts',(-0.10475646414209,27.7160925620855,-10.508047074406));
#85907=CARTESIAN_POINT('Ctrl Pts',(0.0293830968989478,29.0939459047543,
-10.0808266335395));
#85908=CARTESIAN_POINT('Ctrl Pts',(0.2550250052573,31.2849952676692,-9.17859210179942));
#85909=CARTESIAN_POINT('Ctrl Pts',(0.385396446792777,32.4450836887615,-8.40289350048829));
#85910=CARTESIAN_POINT('Ctrl Pts',(0.649104132018911,34.4038383988825,-6.44526974701288));
#85911=CARTESIAN_POINT('Ctrl Pts',(0.779361426258769,35.1789943402779,-5.28667072334708));
#85912=CARTESIAN_POINT('Ctrl Pts',(1.00998133826083,36.099849591882,-3.04686683603461));
#85913=CARTESIAN_POINT('Ctrl Pts',(1.14347962089245,36.5054107499014,-1.67135405526916));
#85914=CARTESIAN_POINT('Ctrl Pts',(1.4145748299214,36.4953815121046,1.17517952963133));
#85915=CARTESIAN_POINT('Ctrl Pts',(1.54629654869269,36.3052557276413,2.5745604504923));
#85916=CARTESIAN_POINT('Ctrl Pts',(1.82814073845306,35.1632292264153,5.30408588680117));
#85917=CARTESIAN_POINT('Ctrl Pts',(1.95809258149138,34.3893718642633,6.45987054065415));
#85918=CARTESIAN_POINT('Ctrl Pts',(2.08803195960875,33.4246212024587,7.42462120245876));
#85919=CARTESIAN_POINT('',(-1.05356078680146,18.5753787975412,-7.42462120245874));
#85920=CARTESIAN_POINT('Ctrl Pts',(1.05356162218519,18.5753787975412,-7.42462120245874));
#85921=CARTESIAN_POINT('Ctrl Pts',(1.20316127235613,19.6860995320808,-8.53534193699833));
#85922=CARTESIAN_POINT('Ctrl Pts',(1.50236057269802,22.4134777721174,-10.2487526513479));
#85923=CARTESIAN_POINT('Ctrl Pts',(1.95115952321084,27.2162250618967,-10.7922206100352));
#85924=CARTESIAN_POINT('Ctrl Pts',(2.39995847372367,31.7766290344261,-9.19360350589968));
#85925=CARTESIAN_POINT('Ctrl Pts',(2.8487574242365,35.1956836893318,-5.77827433993674));
#85926=CARTESIAN_POINT('Ctrl Pts',(3.29755637474932,36.7894868512029,-1.21572940252715));
#85927=CARTESIAN_POINT('Ctrl Pts',(3.74635532526215,36.2504838893164,3.58628271132926));
#85928=CARTESIAN_POINT('Ctrl Pts',(4.04555462560404,34.5353419369983,6.31390046791915));
#85929=CARTESIAN_POINT('Ctrl Pts',(4.19515427577498,33.4246212024587,7.42462120245876));
#85930=CARTESIAN_POINT('Ctrl Pts',(0.35118671899054,18.5753787975412,-7.42462120245874));
#85931=CARTESIAN_POINT('Ctrl Pts',(0.500786369161483,19.6860995320808,-8.53534193699833));
#85932=CARTESIAN_POINT('Ctrl Pts',(0.799985669503367,22.4134777721174,-10.2487526513479));
#85933=CARTESIAN_POINT('Ctrl Pts',(1.2487846200162,27.2162250618967,-10.7922206100352));
#85934=CARTESIAN_POINT('Ctrl Pts',(1.69758357052903,31.7766290344261,-9.19360350589968));
#85935=CARTESIAN_POINT('Ctrl Pts',(2.14638252104185,35.1956836893318,-5.77827433993674));
#85936=CARTESIAN_POINT('Ctrl Pts',(2.59518147155468,36.7894868512029,-1.21572940252715));
#85937=CARTESIAN_POINT('Ctrl Pts',(3.04398042206751,36.2504838893164,3.58628271132925));
#85938=CARTESIAN_POINT('Ctrl Pts',(3.34317972240939,34.5353419369983,6.31390046791915));
#85939=CARTESIAN_POINT('Ctrl Pts',(3.49277937258034,33.4246212024587,7.42462120245876));
#85940=CARTESIAN_POINT('Ctrl Pts',(-0.351188184204108,18.5753787975412,
-7.42462120245874));
#85941=CARTESIAN_POINT('Ctrl Pts',(-0.201588534033165,19.6860995320808,
-8.53534193699833));
#85942=CARTESIAN_POINT('Ctrl Pts',(0.0976107663087195,22.4134777721174,
-10.2487526513479));
#85943=CARTESIAN_POINT('Ctrl Pts',(0.546409716821547,27.2162250618966,-10.7922206100352));
#85944=CARTESIAN_POINT('Ctrl Pts',(0.995208667334374,31.7766290344261,-9.19360350589968));
#85945=CARTESIAN_POINT('Ctrl Pts',(1.4440076178472,35.1956836893318,-5.77827433993674));
#85946=CARTESIAN_POINT('Ctrl Pts',(1.89280656836003,36.7894868512029,-1.21572940252715));
#85947=CARTESIAN_POINT('Ctrl Pts',(2.34160551887286,36.2504838893164,3.58628271132926));
#85948=CARTESIAN_POINT('Ctrl Pts',(2.64080481921474,34.5353419369983,6.31390046791915));
#85949=CARTESIAN_POINT('Ctrl Pts',(2.79040446938568,33.4246212024587,7.42462120245876));
#85950=CARTESIAN_POINT('Ctrl Pts',(-1.05356308739875,18.5753787975412,-7.42462120245874));
#85951=CARTESIAN_POINT('Ctrl Pts',(-0.903963437227813,19.6860995320808,
-8.53534193699833));
#85952=CARTESIAN_POINT('Ctrl Pts',(-0.604764136885928,22.4134777721174,
-10.2487526513479));
#85953=CARTESIAN_POINT('Ctrl Pts',(-0.1559651863731,27.2162250618967,-10.7922206100352));
#85954=CARTESIAN_POINT('Ctrl Pts',(0.292833764139727,31.7766290344261,-9.19360350589968));
#85955=CARTESIAN_POINT('Ctrl Pts',(0.741632714652555,35.1956836893318,-5.77827433993674));
#85956=CARTESIAN_POINT('Ctrl Pts',(1.19043166516538,36.7894868512029,-1.21572940252715));
#85957=CARTESIAN_POINT('Ctrl Pts',(1.63923061567821,36.2504838893164,3.58628271132926));
#85958=CARTESIAN_POINT('Ctrl Pts',(1.9384299160201,34.5353419369983,6.31390046791915));
#85959=CARTESIAN_POINT('Ctrl Pts',(2.08802956619104,33.4246212024587,7.42462120245876));
#85960=CARTESIAN_POINT('',(-1.05356078680146,18.5753787975412,-7.42462120245874));
#85961=CARTESIAN_POINT('',(2.08803195960875,33.4246212024587,7.42462120245876));
#85962=CARTESIAN_POINT('Ctrl Pts',(-4.06609633692487,21.7560606212036,-4.24050246993839));
#85963=CARTESIAN_POINT('Ctrl Pts',(-3.91636165892841,22.3910070403042,-4.87597230443958));
#85964=CARTESIAN_POINT('Ctrl Pts',(-3.61702733076101,23.9499352084937,-5.8557580717418));
#85965=CARTESIAN_POINT('Ctrl Pts',(-3.16809335242267,26.694917060818,-6.16637292099771));
#85966=CARTESIAN_POINT('Ctrl Pts',(-2.71929440190984,29.3006050890309,-5.25296847347605));
#85967=CARTESIAN_POINT('Ctrl Pts',(-2.27049545139702,31.2541571927175,-3.30154384028647));
#85968=CARTESIAN_POINT('Ctrl Pts',(-1.82169650088419,32.1648128688101,-0.694633102948697));
#85969=CARTESIAN_POINT('Ctrl Pts',(-1.37278350126161,31.8567624461033,2.04979990866951));
#85970=CARTESIAN_POINT('Ctrl Pts',(-1.07347015180998,30.8761088818321,3.60877454888744));
#85971=CARTESIAN_POINT('Ctrl Pts',(-0.923756452529281,30.2407695615107,
4.24367249087768));
#85972=CARTESIAN_POINT('Ctrl Pts',(-4.45407384504702,20.6948310223133,-5.30087264340261));
#85973=CARTESIAN_POINT('Ctrl Pts',(-4.30433916705057,21.4885506644777,-6.0952465850039));
#85974=CARTESIAN_POINT('Ctrl Pts',(-4.00500483888317,23.437300780382,-7.32003529980991));
#85975=CARTESIAN_POINT('Ctrl Pts',(-3.55607086054484,26.8686864029058,-7.70832177499247));
#85976=CARTESIAN_POINT('Ctrl Pts',(-3.10727191003201,30.1259467120115,-6.56651353821995));
#85977=CARTESIAN_POINT('Ctrl Pts',(-2.65847295951918,32.5679995058269,-4.12712020522022));
#85978=CARTESIAN_POINT('Ctrl Pts',(-2.20967400900635,33.7063716197874,-0.868331439192896));
#85979=CARTESIAN_POINT('Ctrl Pts',(-1.76076100938378,33.3212908256856,2.56236810079568));
#85980=CARTESIAN_POINT('Ctrl Pts',(-1.46144765993214,32.0954173146212,4.51117630941575));
#85981=CARTESIAN_POINT('Ctrl Pts',(-1.31173396065144,31.3012065232716,5.30483535239647));
#85982=CARTESIAN_POINT('Ctrl Pts',(-4.84205135316919,19.6336014234231,-6.36124281686683));
#85983=CARTESIAN_POINT('Ctrl Pts',(-4.69231667517274,20.5860942886512,-7.31452086556822));
#85984=CARTESIAN_POINT('Ctrl Pts',(-4.39298234700534,22.9246663522705,-8.78431252787802));
#85985=CARTESIAN_POINT('Ctrl Pts',(-3.94404836866699,27.0424557449935,-9.25027062898723));
#85986=CARTESIAN_POINT('Ctrl Pts',(-3.49524941815416,30.9512883349922,-7.88005860296385));
#85987=CARTESIAN_POINT('Ctrl Pts',(-3.04645046764134,33.8818418189363,-4.95269657015396));
#85988=CARTESIAN_POINT('Ctrl Pts',(-2.59765151712851,35.2479303707647,-1.04202977543709));
#85989=CARTESIAN_POINT('Ctrl Pts',(-2.14873851750593,34.7858192052677,3.07493629292183));
#85990=CARTESIAN_POINT('Ctrl Pts',(-1.8494251680543,33.3147257474102,5.41357806994405));
#85991=CARTESIAN_POINT('Ctrl Pts',(-1.6997114687736,32.3616434850324,6.36599821391526));
#85992=CARTESIAN_POINT('Ctrl Pts',(-5.23002886129135,18.5723718245327,-7.42161299033105));
#85993=CARTESIAN_POINT('Ctrl Pts',(-5.0802941832949,19.6836379128248,-8.53379514613253));
#85994=CARTESIAN_POINT('Ctrl Pts',(-4.7809598551275,22.4120319241589,-10.2485897559461));
#85995=CARTESIAN_POINT('Ctrl Pts',(-4.33202587678916,27.2162250870813,-10.792219482982));
#85996=CARTESIAN_POINT('Ctrl Pts',(-3.88322692627633,31.7766299579729,-9.19360366770775));
#85997=CARTESIAN_POINT('Ctrl Pts',(-3.4344279757635,35.1956841320457,-5.77827293508771));
#85998=CARTESIAN_POINT('Ctrl Pts',(-2.98562902525068,36.7894891217421,-1.21572811168129));
#85999=CARTESIAN_POINT('Ctrl Pts',(-2.5367160256281,36.25034758485,3.58750448504799));
#86000=CARTESIAN_POINT('Ctrl Pts',(-2.23740267617646,34.5340341801993,6.31597983047236));
#86001=CARTESIAN_POINT('Ctrl Pts',(-2.08768897689577,33.4220804467933,7.42716107543405));
#86002=CARTESIAN_POINT('',(-5.22962383911132,18.5753787991571,-7.42462120084288));
#86003=CARTESIAN_POINT('',(-4.03998298259813,21.8280699909994,-4.17193000900062));
#86004=CARTESIAN_POINT('',(-2.08803112422502,33.4246212024587,7.42462120245876));
#86005=CARTESIAN_POINT('Ctrl Pts',(-5.22962377781481,18.5753787975412,-7.42462120245874));
#86006=CARTESIAN_POINT('Ctrl Pts',(-5.08002412764387,19.6860995320808,-8.53534193699833));
#86007=CARTESIAN_POINT('Ctrl Pts',(-4.93042391721014,21.0497898200314,-9.39204650881968));
#86008=CARTESIAN_POINT('Ctrl Pts',(-4.78082437558953,22.5320924911443,-9.91097757957131));
#86009=CARTESIAN_POINT('Ctrl Pts',(-4.63122483396892,24.0143951622573,-10.4299086503229));
#86010=CARTESIAN_POINT('Ctrl Pts',(-4.4816254109829,25.6153102292322,-10.6110638876134));
#86011=CARTESIAN_POINT('Ctrl Pts',(-4.33202591030011,27.1758341851912,-10.4352058503029));
#86012=CARTESIAN_POINT('Ctrl Pts',(-4.18242640961732,28.7363581411502,-10.2593478129924));
#86013=CARTESIAN_POINT('Ctrl Pts',(-4.03282683881772,30.2564924773674,-9.72647664573263));
#86014=CARTESIAN_POINT('Ctrl Pts',(-3.88322710462072,31.5864020319258,-8.89081910296247));
#86015=CARTESIAN_POINT('Ctrl Pts',(-3.73362737042372,32.9163115864842,-8.05516156019232));
#86016=CARTESIAN_POINT('Ctrl Pts',(-3.58402803875759,34.0559964457548,-6.91671962854987));
#86017=CARTESIAN_POINT('Ctrl Pts',(-3.4344283002626,34.8914722949544,-5.58707487977672));
#86018=CARTESIAN_POINT('Ctrl Pts',(-3.28482856176761,35.7269481441539,-4.25743013100356));
#86019=CARTESIAN_POINT('Ctrl Pts',(-3.13522807006066,36.258214271152,-2.73658183224548));
#86020=CARTESIAN_POINT('Ctrl Pts',(-2.98562808753307,36.4340142951492,-1.17582236661662));
#86021=CARTESIAN_POINT('Ctrl Pts',(-2.83602810500547,36.6098143191465,0.384937099012241));
#86022=CARTESIAN_POINT('Ctrl Pts',(-2.68642868171361,36.4301482037352,1.98560771006104));
#86023=CARTESIAN_POINT('Ctrl Pts',(-2.53682930086399,35.9115301168794,3.46784855547023));
#86024=CARTESIAN_POINT('Ctrl Pts',(-2.38722992001438,35.3929120300235,4.95008940087942));
#86025=CARTESIAN_POINT('Ctrl Pts',(-2.23763077439596,34.5353419369983,6.31390046791915));
#86026=CARTESIAN_POINT('Ctrl Pts',(-2.08803112422502,33.4246212024587,7.42462120245876));
#86027=CARTESIAN_POINT('',(-0.898390236187925,30.1719300090006,4.17193000900064));
#86028=CARTESIAN_POINT('Ctrl Pts',(-7.33715091171646,18.5723737967529,-7.42161496416937));
#86029=CARTESIAN_POINT('Ctrl Pts',(-7.18741632230038,19.6836395245258,-8.53379616319783));
#86030=CARTESIAN_POINT('Ctrl Pts',(-6.88808208271336,22.412036304676,-10.2485874615845));
#86031=CARTESIAN_POINT('Ctrl Pts',(-6.43914819295539,27.2162249558894,-10.7922239637205));
#86032=CARTESIAN_POINT('Ctrl Pts',(-5.99034924244256,31.7766262509208,-9.19360309786621));
#86033=CARTESIAN_POINT('Ctrl Pts',(-5.54155029192973,35.1956822959411,-5.77827855619686));
#86034=CARTESIAN_POINT('Ctrl Pts',(-5.09275134141691,36.7894800611825,-1.21573330540808));
#86035=CARTESIAN_POINT('Ctrl Pts',(-4.64383850166433,36.2503450657148,3.58749685357029));
#86036=CARTESIAN_POINT('Ctrl Pts',(-4.34452531208268,34.5340360157071,6.3159769203004));
#86037=CARTESIAN_POINT('Ctrl Pts',(-4.19481177267199,33.4220840089498,7.42715751574294));
#86038=CARTESIAN_POINT('Ctrl Pts',(-7.72512838823515,19.6336030274158,-6.36124459506567));
#86039=CARTESIAN_POINT('Ctrl Pts',(-7.57539379881907,20.5860955965676,-7.31452183663775));
#86040=CARTESIAN_POINT('Ctrl Pts',(-7.27605955923203,22.9246700651593,-8.7843106806011));
#86041=CARTESIAN_POINT('Ctrl Pts',(-6.82712566947407,27.0424556467005,-9.25027459513849));
#86042=CARTESIAN_POINT('Ctrl Pts',(-6.37832671896124,30.9512852248186,-7.8800582215364));
#86043=CARTESIAN_POINT('Ctrl Pts',(-5.92952776844841,33.8818403521886,-4.95270145539072));
#86044=CARTESIAN_POINT('Ctrl Pts',(-5.48072881793558,35.247922730312,-1.04203424125412));
#86045=CARTESIAN_POINT('Ctrl Pts',(-5.03181597818301,34.7858171653526,3.07492979355112));
#86046=CARTESIAN_POINT('Ctrl Pts',(-4.73250278860136,33.3147274199893,5.41357564907264));
#86047=CARTESIAN_POINT('Ctrl Pts',(-4.58278924919067,32.3616466246225,6.36599524925758));
#86048=CARTESIAN_POINT('Ctrl Pts',(-8.11310586475383,20.6948322580786,-5.30087422596197));
#86049=CARTESIAN_POINT('Ctrl Pts',(-7.96337127533775,21.4885516686094,-6.09524751007768));
#86050=CARTESIAN_POINT('Ctrl Pts',(-7.66403703575072,23.4373038256427,-7.32003389961774));
#86051=CARTESIAN_POINT('Ctrl Pts',(-7.21510314599275,26.8686863375116,-7.70832522655642));
#86052=CARTESIAN_POINT('Ctrl Pts',(-6.76630419547992,30.1259441987164,-6.56651334520659));
#86053=CARTESIAN_POINT('Ctrl Pts',(-6.3175052449671,32.5679984084359,-4.12712435458457));
#86054=CARTESIAN_POINT('Ctrl Pts',(-5.86870629445427,33.7063653994416,-0.868335177100162));
#86055=CARTESIAN_POINT('Ctrl Pts',(-5.41979345470168,33.3212892649903,2.56236273353193));
#86056=CARTESIAN_POINT('Ctrl Pts',(-5.12048026512005,32.0954188242716,4.51117437784488));
#86057=CARTESIAN_POINT('Ctrl Pts',(-4.97076672570934,31.301209240295,5.30483298277222));
#86058=CARTESIAN_POINT('Ctrl Pts',(-8.50108334127251,21.7560614887415,-4.24050385685827));
#86059=CARTESIAN_POINT('Ctrl Pts',(-8.35134875185642,22.3910077406511,-4.87597318351759));
#86060=CARTESIAN_POINT('Ctrl Pts',(-8.05201451226939,23.949937586126,-5.85575711863438));
#86061=CARTESIAN_POINT('Ctrl Pts',(-7.60308062251143,26.6949170283227,-6.16637585797436));
#86062=CARTESIAN_POINT('Ctrl Pts',(-7.1542816719986,29.3006031726142,-5.25296846887678));
#86063=CARTESIAN_POINT('Ctrl Pts',(-6.70548272148578,31.2541564646834,-3.30154725377842));
#86064=CARTESIAN_POINT('Ctrl Pts',(-6.25668377097295,32.1648080685711,-0.694636112946202));
#86065=CARTESIAN_POINT('Ctrl Pts',(-5.80777093122036,31.856761364628,2.04979567351274));
#86066=CARTESIAN_POINT('Ctrl Pts',(-5.50845774163872,30.8761102285537,3.60877310661714));
#86067=CARTESIAN_POINT('Ctrl Pts',(-5.35874420222803,30.2407718559677,4.24367071628685));
#86068=CARTESIAN_POINT('',(-4.19515344039126,33.4246212024587,7.42462120245876));
#86069=CARTESIAN_POINT('',(-4.19515344039125,33.4246212024587,7.42462120245876));
#86070=CARTESIAN_POINT('',(-7.33674614183372,18.5753788014852,-7.42462119851477));
#86071=CARTESIAN_POINT('Ctrl Pts',(-7.33674609398104,18.5753787975412,-7.42462120245874));
#86072=CARTESIAN_POINT('Ctrl Pts',(-7.1871464438101,19.6860995320808,-8.53534193699833));
#86073=CARTESIAN_POINT('Ctrl Pts',(-6.88794714346822,22.4134803337522,-10.2487508662659));
#86074=CARTESIAN_POINT('Ctrl Pts',(-6.43914819295539,27.2162249558894,-10.7922239637205));
#86075=CARTESIAN_POINT('Ctrl Pts',(-5.99034924244256,31.7766262509208,-9.19360309786621));
#86076=CARTESIAN_POINT('Ctrl Pts',(-5.54155029192973,35.1956822959411,-5.77827855619686));
#86077=CARTESIAN_POINT('Ctrl Pts',(-5.09275134141691,36.7894800611825,-1.21573330540808));
#86078=CARTESIAN_POINT('Ctrl Pts',(-4.64395239090408,36.250481844326,3.58627827351926));
#86079=CARTESIAN_POINT('Ctrl Pts',(-4.34475309056219,34.5353419369983,6.31390046791915));
#86080=CARTESIAN_POINT('Ctrl Pts',(-4.19515344039125,33.4246212024587,7.42462120245876));
#86081=CARTESIAN_POINT('',(-7.33674618680146,18.5753787975412,-7.42462120245874));
#86082=CARTESIAN_POINT('Ctrl Pts',(-5.22962377781481,18.5753787975412,-7.42462120245874));
#86083=CARTESIAN_POINT('Ctrl Pts',(-5.08002412764387,19.6860995320808,-8.53534193699833));
#86084=CARTESIAN_POINT('Ctrl Pts',(-4.78082482730198,22.4134803337522,-10.2487508662659));
#86085=CARTESIAN_POINT('Ctrl Pts',(-4.33202587678916,27.2162249558894,-10.7922239637205));
#86086=CARTESIAN_POINT('Ctrl Pts',(-3.88322692627633,31.7766262509208,-9.19360309786621));
#86087=CARTESIAN_POINT('Ctrl Pts',(-3.4344279757635,35.1956822959411,-5.77827855619686));
#86088=CARTESIAN_POINT('Ctrl Pts',(-2.98562902525067,36.7894800611825,-1.21573330540808));
#86089=CARTESIAN_POINT('Ctrl Pts',(-2.53683007473785,36.250481844326,3.58627827351926));
#86090=CARTESIAN_POINT('Ctrl Pts',(-2.23763077439596,34.5353419369983,6.31390046791915));
#86091=CARTESIAN_POINT('Ctrl Pts',(-2.08803112422502,33.4246212024587,7.42462120245876));
#86092=CARTESIAN_POINT('Ctrl Pts',(-5.93199788320355,18.5753787975412,-7.42462120245874));
#86093=CARTESIAN_POINT('Ctrl Pts',(-5.78239823303261,19.6860995320808,-8.53534193699833));
#86094=CARTESIAN_POINT('Ctrl Pts',(-5.48319893269072,22.4134803337522,-10.2487508662659));
#86095=CARTESIAN_POINT('Ctrl Pts',(-5.0343999821779,27.2162249558894,-10.7922239637205));
#86096=CARTESIAN_POINT('Ctrl Pts',(-4.58560103166507,31.7766262509208,-9.19360309786621));
#86097=CARTESIAN_POINT('Ctrl Pts',(-4.13680208115225,35.1956822959411,-5.77827855619686));
#86098=CARTESIAN_POINT('Ctrl Pts',(-3.68800313063942,36.7894800611825,-1.21573330540808));
#86099=CARTESIAN_POINT('Ctrl Pts',(-3.23920418012659,36.250481844326,3.58627827351926));
#86100=CARTESIAN_POINT('Ctrl Pts',(-2.94000487978471,34.5353419369983,6.31390046791915));
#86101=CARTESIAN_POINT('Ctrl Pts',(-2.79040522961376,33.4246212024587,7.42462120245876));
#86102=CARTESIAN_POINT('Ctrl Pts',(-6.6343719885923,18.5753787975412,-7.42462120245874));
#86103=CARTESIAN_POINT('Ctrl Pts',(-6.48477233842136,19.6860995320808,-8.53534193699833));
#86104=CARTESIAN_POINT('Ctrl Pts',(-6.18557303807947,22.4134803337522,-10.2487508662659));
#86105=CARTESIAN_POINT('Ctrl Pts',(-5.73677408756665,27.2162249558894,-10.7922239637205));
#86106=CARTESIAN_POINT('Ctrl Pts',(-5.28797513705382,31.7766262509208,-9.19360309786621));
#86107=CARTESIAN_POINT('Ctrl Pts',(-4.83917618654099,35.1956822959411,-5.77827855619686));
#86108=CARTESIAN_POINT('Ctrl Pts',(-4.39037723602816,36.7894800611825,-1.21573330540808));
#86109=CARTESIAN_POINT('Ctrl Pts',(-3.94157828551533,36.250481844326,3.58627827351927));
#86110=CARTESIAN_POINT('Ctrl Pts',(-3.64237898517345,34.5353419369983,6.31390046791915));
#86111=CARTESIAN_POINT('Ctrl Pts',(-3.49277933500251,33.4246212024587,7.42462120245876));
#86112=CARTESIAN_POINT('Ctrl Pts',(-7.33674609398104,18.5753787975412,-7.42462120245874));
#86113=CARTESIAN_POINT('Ctrl Pts',(-7.1871464438101,19.6860995320808,-8.53534193699833));
#86114=CARTESIAN_POINT('Ctrl Pts',(-6.88794714346822,22.4134803337522,-10.2487508662659));
#86115=CARTESIAN_POINT('Ctrl Pts',(-6.43914819295539,27.2162249558894,-10.7922239637205));
#86116=CARTESIAN_POINT('Ctrl Pts',(-5.99034924244256,31.7766262509208,-9.19360309786621));
#86117=CARTESIAN_POINT('Ctrl Pts',(-5.54155029192973,35.1956822959411,-5.77827855619686));
#86118=CARTESIAN_POINT('Ctrl Pts',(-5.09275134141691,36.7894800611825,-1.21573330540808));
#86119=CARTESIAN_POINT('Ctrl Pts',(-4.64395239090408,36.250481844326,3.58627827351926));
#86120=CARTESIAN_POINT('Ctrl Pts',(-4.34475309056219,34.5353419369983,6.31390046791915));
#86121=CARTESIAN_POINT('Ctrl Pts',(-4.19515344039125,33.4246212024587,7.42462120245876));
#86122=CARTESIAN_POINT('',(-7.33674618680146,18.5753787975412,-7.42462120245874));
#86123=CARTESIAN_POINT('',(-4.19515344039125,33.4246212024587,7.42462120245876));
#86124=CARTESIAN_POINT('Ctrl Pts',(-10.3492814380484,21.7560621627659,-4.2405050092528));
#86125=CARTESIAN_POINT('Ctrl Pts',(-10.1995469203954,22.3910082818704,-4.87597392987967));
#86126=CARTESIAN_POINT('Ctrl Pts',(-9.90021275257146,23.9499413459023,-5.85575518849289));
#86127=CARTESIAN_POINT('Ctrl Pts',(-9.45127893457658,26.6949168047227,-6.16638084397979));
#86128=CARTESIAN_POINT('Ctrl Pts',(-9.00247998406375,29.3005993803806,-5.25296846874784));
#86129=CARTESIAN_POINT('Ctrl Pts',(-8.55368103355092,31.254154562729,-3.30155339634265));
#86130=CARTESIAN_POINT('Ctrl Pts',(-8.1048820830381,32.1647989151806,-0.694641763526773));
#86131=CARTESIAN_POINT('Ctrl Pts',(-7.65596869508309,31.8567582889011,2.04979291948575));
#86132=CARTESIAN_POINT('Ctrl Pts',(-7.35665495729904,30.8761069131734,3.60877902517104));
#86133=CARTESIAN_POINT('Ctrl Pts',(-7.20694086968591,30.2407651154807,4.24367792953755));
#86134=CARTESIAN_POINT('Ctrl Pts',(-10.7372588854526,20.6948332400255,-5.30087552725679));
#86135=CARTESIAN_POINT('Ctrl Pts',(-10.5875243677996,21.4885524636896,-6.09524828293874));
#86136=CARTESIAN_POINT('Ctrl Pts',(-10.2881901999756,23.4373085929068,-7.32003129451753));
#86137=CARTESIAN_POINT('Ctrl Pts',(-9.83925638198077,26.8686860351764,-7.70833125683706));
#86138=CARTESIAN_POINT('Ctrl Pts',(-9.39045743146795,30.1259393498091,-6.56651317252976));
#86139=CARTESIAN_POINT('Ctrl Pts',(-8.94165848095512,32.5679958583287,-4.12713192471575));
#86140=CARTESIAN_POINT('Ctrl Pts',(-8.49285953044229,33.7063537547143,-0.868342217838437));
#86141=CARTESIAN_POINT('Ctrl Pts',(-8.04394614248728,33.3212852278094,2.56235922352107));
#86142=CARTESIAN_POINT('Ctrl Pts',(-7.74463240470322,32.0954145197162,4.51118165786049));
#86143=CARTESIAN_POINT('Ctrl Pts',(-7.59491831709011,31.3012006750246,5.30484186038235));
#86144=CARTESIAN_POINT('Ctrl Pts',(-11.1252363328568,19.6336043172851,-6.36124604526076));
#86145=CARTESIAN_POINT('Ctrl Pts',(-10.9755018152038,20.5860966455086,-7.31452263599781));
#86146=CARTESIAN_POINT('Ctrl Pts',(-10.6761676473798,22.9246758399115,-8.78430740054218));
#86147=CARTESIAN_POINT('Ctrl Pts',(-10.2272338293849,27.0424552656302,-9.25028166969433));
#86148=CARTESIAN_POINT('Ctrl Pts',(-9.77843487887213,30.9512793192374,-7.88005787631169));
#86149=CARTESIAN_POINT('Ctrl Pts',(-9.3296359283593,33.8818371539285,-4.95271045308884));
#86150=CARTESIAN_POINT('Ctrl Pts',(-8.88083697784648,35.247908594248,-1.0420426721501));
#86151=CARTESIAN_POINT('Ctrl Pts',(-8.43192358989148,34.7858121667177,3.0749255275564));
#86152=CARTESIAN_POINT('Ctrl Pts',(-8.13260985210742,33.314722126259,5.41358429054993));
#86153=CARTESIAN_POINT('Ctrl Pts',(-7.98289576449429,32.3616362345684,6.36600579122716));
#86154=CARTESIAN_POINT('Ctrl Pts',(-11.513213780261,18.5723753945447,-7.42161656326474));
#86155=CARTESIAN_POINT('Ctrl Pts',(-11.363479262608,19.6836408273278,-8.53379698905687));
#86156=CARTESIAN_POINT('Ctrl Pts',(-11.0641450947841,22.4120430869161,-10.2485835065668));
#86157=CARTESIAN_POINT('Ctrl Pts',(-10.6152112767892,27.2162244960841,-10.7922320825516));
#86158=CARTESIAN_POINT('Ctrl Pts',(-10.1664123262763,31.7766192886659,-9.1936025800936));
#86159=CARTESIAN_POINT('Ctrl Pts',(-9.7176133757635,35.1956784495283,-5.77828898146194));
#86160=CARTESIAN_POINT('Ctrl Pts',(-9.26881442525067,36.7894634337816,-1.21574312646176));
#86161=CARTESIAN_POINT('Ctrl Pts',(-8.81990103729567,36.250339105626,3.58749183159172));
#86162=CARTESIAN_POINT('Ctrl Pts',(-8.52058729951161,34.5340297328017,6.31598692323937));
#86163=CARTESIAN_POINT('Ctrl Pts',(-8.37087321189849,33.4220717941122,7.42716972207196));
#86164=CARTESIAN_POINT('',(-11.5128092391113,18.5753787991571,-7.42462120084288));
#86165=CARTESIAN_POINT('',(-10.3231683825981,21.8280699909994,-4.17193000900062));
#86166=CARTESIAN_POINT('',(-8.37121652422502,33.4246212024587,7.42462120245876));
#86167=CARTESIAN_POINT('Ctrl Pts',(-11.5128091778148,18.5753787975412,-7.42462120245874));
#86168=CARTESIAN_POINT('Ctrl Pts',(-11.3632095276439,19.6860995320808,-8.53534193699833));
#86169=CARTESIAN_POINT('Ctrl Pts',(-11.213609451507,21.0497941968264,-9.39204359968316));
#86170=CARTESIAN_POINT('Ctrl Pts',(-11.0640099052434,22.5320974583249,-9.91097616832263));
#86171=CARTESIAN_POINT('Ctrl Pts',(-10.9144103589797,24.0144007198234,-10.4299087369621));
#86172=CARTESIAN_POINT('Ctrl Pts',(-10.7648108479412,25.6153125949017,-10.6110701604612));
#86173=CARTESIAN_POINT('Ctrl Pts',(-10.615211325617,27.1758334271763,-10.4352130137814));
#86174=CARTESIAN_POINT('Ctrl Pts',(-10.4656118032928,28.7363542594509,-10.2593558671016));
#86175=CARTESIAN_POINT('Ctrl Pts',(-10.3160122275825,30.2564852600915,-9.72648007747699));
#86176=CARTESIAN_POINT('Ctrl Pts',(-10.1664125253831,31.5863940042371,-8.8908232015921));
#86177=CARTESIAN_POINT('Ctrl Pts',(-10.0168128231837,32.9163027483828,-8.05516632570722));
#86178=CARTESIAN_POINT('Ctrl Pts',(-9.8672134190413,34.0559892681328,-6.91672982584028));
#86179=CARTESIAN_POINT('Ctrl Pts',(-9.7176136600352,34.8914626930057,-5.58708752460106));
#86180=CARTESIAN_POINT('Ctrl Pts',(-9.56801390102909,35.7269361178786,-4.25744522336183));
#86181=CARTESIAN_POINT('Ctrl Pts',(-9.41841355447926,36.2581960188536,-2.73659663848387));
#86182=CARTESIAN_POINT('Ctrl Pts',(-9.26881361325665,36.4339956847859,-1.17583727852711));
#86183=CARTESIAN_POINT('Ctrl Pts',(-9.11921367203404,36.6097953507183,0.384922081429656));
#86184=CARTESIAN_POINT('Ctrl Pts',(-8.96961418003796,36.4301347482737,1.98559219616138));
#86185=CARTESIAN_POINT('Ctrl Pts',(-8.8200147653941,35.9115214019404,3.46783679709374));
#86186=CARTESIAN_POINT('Ctrl Pts',(-8.67041535075024,35.3929080556071,4.9500813980261));
#86187=CARTESIAN_POINT('Ctrl Pts',(-8.52081617439596,34.5353419369983,6.31390046791915));
#86188=CARTESIAN_POINT('Ctrl Pts',(-8.37121652422502,33.4246212024587,7.42462120245876));
#86189=CARTESIAN_POINT('',(-7.18157563618792,30.1719300090006,4.17193000900064));
#86190=CARTESIAN_POINT('Ctrl Pts',(-13.6203358688322,18.5723770836602,-7.42161825376526));
#86191=CARTESIAN_POINT('Ctrl Pts',(-13.4706014270443,19.683642207911,-8.53379785982716));
#86192=CARTESIAN_POINT('Ctrl Pts',(-13.1712673350853,22.4120465854243,-10.2485818670356));
#86193=CARTESIAN_POINT('Ctrl Pts',(-12.7223335929554,27.2162241792528,-10.7922358496953));
#86194=CARTESIAN_POINT('Ctrl Pts',(-12.2735346424426,31.776615948509,-9.19360257337038));
#86195=CARTESIAN_POINT('Ctrl Pts',(-11.8247356919297,35.1956764374484,-5.77829392033626));
#86196=CARTESIAN_POINT('Ctrl Pts',(-11.3759367414169,36.7894556396735,-1.21574785540399));
#86197=CARTESIAN_POINT('Ctrl Pts',(-10.9270235257324,36.2503366865871,3.5874848749837));
#86198=CARTESIAN_POINT('Ctrl Pts',(-10.6277099602189,34.5340317104571,6.31598378636594));
#86199=CARTESIAN_POINT('Ctrl Pts',(-10.4779960448763,33.4220756325766,7.42716588627459));
#86200=CARTESIAN_POINT('Ctrl Pts',(-14.008313289448,19.6336056917925,-6.36124756744431));
#86201=CARTESIAN_POINT('Ctrl Pts',(-13.85857884766,20.5860977665283,-7.31452346654261));
#86202=CARTESIAN_POINT('Ctrl Pts',(-13.559244755701,22.9246788031716,-8.78430609636367));
#86203=CARTESIAN_POINT('Ctrl Pts',(-13.1103110135711,27.0424550060647,-9.2502850050701));
#86204=CARTESIAN_POINT('Ctrl Pts',(-12.6615120630582,30.9512765132955,-7.88005796124472));
#86205=CARTESIAN_POINT('Ctrl Pts',(-12.2127131125454,33.8818355200426,-4.95271474332016));
#86206=CARTESIAN_POINT('Ctrl Pts',(-11.7639141620326,35.2479020201693,-1.04204673743367));
#86207=CARTESIAN_POINT('Ctrl Pts',(-11.3150009463482,34.7858101944217,3.0749196002712));
#86208=CARTESIAN_POINT('Ctrl Pts',(-11.0156873808346,33.314723905544,5.41358166416799));
#86209=CARTESIAN_POINT('Ctrl Pts',(-10.8659734654919,32.3616395978279,6.3660025767426));
#86210=CARTESIAN_POINT('Ctrl Pts',(-14.3962907100637,20.6948342999247,-5.30087688112336));
#86211=CARTESIAN_POINT('Ctrl Pts',(-14.2465562682757,21.4885533251457,-6.09524907325806));
#86212=CARTESIAN_POINT('Ctrl Pts',(-13.9472221763167,23.4373110209188,-7.32003032569173));
#86213=CARTESIAN_POINT('Ctrl Pts',(-13.4982884341868,26.8686858328766,-7.70833416044494));
#86214=CARTESIAN_POINT('Ctrl Pts',(-13.049489483674,30.1259370780819,-6.56651334911906));
#86215=CARTESIAN_POINT('Ctrl Pts',(-12.6006905331612,32.5679946026368,-4.12713556630407));
#86216=CARTESIAN_POINT('Ctrl Pts',(-12.1518915826484,33.7063484006651,-0.868345619463353));
#86217=CARTESIAN_POINT('Ctrl Pts',(-11.7029783669638,33.3212837022564,2.5623543255587));
#86218=CARTESIAN_POINT('Ctrl Pts',(-11.4036648014502,32.0954161006308,4.51117954197003));
#86219=CARTESIAN_POINT('Ctrl Pts',(-11.2539508861077,31.3012035630792,5.30483926721062));
#86220=CARTESIAN_POINT('Ctrl Pts',(-14.7842681306794,21.7560629080571,-4.24050619480241));
#86221=CARTESIAN_POINT('Ctrl Pts',(-14.6345336888914,22.3910088837629,-4.87597467997351));
#86222=CARTESIAN_POINT('Ctrl Pts',(-14.3351995969325,23.9499432386661,-5.8557545550198));
#86223=CARTESIAN_POINT('Ctrl Pts',(-13.8862658548025,26.6949166596885,-6.16638331581976));
#86224=CARTESIAN_POINT('Ctrl Pts',(-13.4374669042897,29.3005976428683,-5.2529687369934));
#86225=CARTESIAN_POINT('Ctrl Pts',(-12.9886679537769,31.254153685231,-3.30155638928797));
#86226=CARTESIAN_POINT('Ctrl Pts',(-12.539869003264,32.164794781161,-0.69464450149303));
#86227=CARTESIAN_POINT('Ctrl Pts',(-12.0909557875795,31.856757210091,2.04978905084621));
#86228=CARTESIAN_POINT('Ctrl Pts',(-11.7916422220659,30.8761082957176,3.60877741977209));
#86229=CARTESIAN_POINT('Ctrl Pts',(-11.6419283067234,30.2407675283306,4.24367595767864));
#86230=CARTESIAN_POINT('',(-10.4783388403913,33.4246212024587,7.42462120245876));
#86231=CARTESIAN_POINT('',(-10.4783388403913,33.4246212024587,7.42462120245876));
#86232=CARTESIAN_POINT('',(-13.6199315418337,18.5753788014852,-7.42462119851477));
#86233=CARTESIAN_POINT('Ctrl Pts',(-13.619931493981,18.5753787975412,-7.42462120245874));
#86234=CARTESIAN_POINT('Ctrl Pts',(-13.4703318438101,19.6860995320808,-8.53534193699833));
#86235=CARTESIAN_POINT('Ctrl Pts',(-13.1711325434682,22.4134890318387,-10.248745098249));
#86236=CARTESIAN_POINT('Ctrl Pts',(-12.7223335929554,27.2162241792528,-10.7922358496953));
#86237=CARTESIAN_POINT('Ctrl Pts',(-12.2735346424426,31.776615948509,-9.19360257337038));
#86238=CARTESIAN_POINT('Ctrl Pts',(-11.8247356919297,35.1956764374484,-5.77829392033626));
#86239=CARTESIAN_POINT('Ctrl Pts',(-11.3759367414169,36.7894556396735,-1.21574785540399));
#86240=CARTESIAN_POINT('Ctrl Pts',(-10.9271377909041,36.2504739124864,3.58626227294545));
#86241=CARTESIAN_POINT('Ctrl Pts',(-10.6279384905622,34.5353419369983,6.31390046791915));
#86242=CARTESIAN_POINT('Ctrl Pts',(-10.4783388403913,33.4246212024587,7.42462120245876));
#86243=CARTESIAN_POINT('',(-13.6199315868015,18.5753787975412,-7.42462120245874));
#86244=CARTESIAN_POINT('Ctrl Pts',(-11.5128091778148,18.5753787975412,-7.42462120245874));
#86245=CARTESIAN_POINT('Ctrl Pts',(-11.3632095276439,19.6860995320808,-8.53534193699833));
#86246=CARTESIAN_POINT('Ctrl Pts',(-11.064010227302,22.4134890318387,-10.248745098249));
#86247=CARTESIAN_POINT('Ctrl Pts',(-10.6152112767892,27.2162241792528,-10.7922358496953));
#86248=CARTESIAN_POINT('Ctrl Pts',(-10.1664123262763,31.776615948509,-9.19360257337038));
#86249=CARTESIAN_POINT('Ctrl Pts',(-9.71761337576351,35.1956764374484,-5.77829392033626));
#86250=CARTESIAN_POINT('Ctrl Pts',(-9.26881442525068,36.7894556396735,-1.21574785540399));
#86251=CARTESIAN_POINT('Ctrl Pts',(-8.82001547473785,36.2504739124864,3.58626227294545));
#86252=CARTESIAN_POINT('Ctrl Pts',(-8.52081617439596,34.5353419369983,6.31390046791915));
#86253=CARTESIAN_POINT('Ctrl Pts',(-8.37121652422502,33.4246212024587,7.42462120245876));
#86254=CARTESIAN_POINT('Ctrl Pts',(-12.2151832832036,18.5753787975412,-7.42462120245874));
#86255=CARTESIAN_POINT('Ctrl Pts',(-12.0655836330326,19.6860995320808,-8.53534193699833));
#86256=CARTESIAN_POINT('Ctrl Pts',(-11.7663843326907,22.4134890318387,-10.248745098249));
#86257=CARTESIAN_POINT('Ctrl Pts',(-11.3175853821779,27.2162241792528,-10.7922358496953));
#86258=CARTESIAN_POINT('Ctrl Pts',(-10.8687864316651,31.7766159485089,-9.19360257337038));
#86259=CARTESIAN_POINT('Ctrl Pts',(-10.4199874811522,35.1956764374484,-5.77829392033625));
#86260=CARTESIAN_POINT('Ctrl Pts',(-9.97118853063942,36.7894556396735,-1.21574785540399));
#86261=CARTESIAN_POINT('Ctrl Pts',(-9.52238958012659,36.2504739124864,3.58626227294544));
#86262=CARTESIAN_POINT('Ctrl Pts',(-9.22319027978471,34.5353419369983,6.31390046791915));
#86263=CARTESIAN_POINT('Ctrl Pts',(-9.07359062961376,33.4246212024587,7.42462120245876));
#86264=CARTESIAN_POINT('Ctrl Pts',(-12.9175573885923,18.5753787975412,-7.42462120245874));
#86265=CARTESIAN_POINT('Ctrl Pts',(-12.7679577384214,19.6860995320808,-8.53534193699833));
#86266=CARTESIAN_POINT('Ctrl Pts',(-12.4687584380795,22.4134890318387,-10.248745098249));
#86267=CARTESIAN_POINT('Ctrl Pts',(-12.0199594875667,27.2162241792528,-10.7922358496953));
#86268=CARTESIAN_POINT('Ctrl Pts',(-11.5711605370538,31.776615948509,-9.19360257337038));
#86269=CARTESIAN_POINT('Ctrl Pts',(-11.122361586541,35.1956764374484,-5.77829392033626));
#86270=CARTESIAN_POINT('Ctrl Pts',(-10.6735626360282,36.7894556396735,-1.21574785540399));
#86271=CARTESIAN_POINT('Ctrl Pts',(-10.2247636855153,36.2504739124864,3.58626227294545));
#86272=CARTESIAN_POINT('Ctrl Pts',(-9.92556438517345,34.5353419369983,6.31390046791915));
#86273=CARTESIAN_POINT('Ctrl Pts',(-9.77596473500251,33.4246212024587,7.42462120245876));
#86274=CARTESIAN_POINT('Ctrl Pts',(-13.619931493981,18.5753787975412,-7.42462120245874));
#86275=CARTESIAN_POINT('Ctrl Pts',(-13.4703318438101,19.6860995320808,-8.53534193699833));
#86276=CARTESIAN_POINT('Ctrl Pts',(-13.1711325434682,22.4134890318387,-10.248745098249));
#86277=CARTESIAN_POINT('Ctrl Pts',(-12.7223335929554,27.2162241792528,-10.7922358496953));
#86278=CARTESIAN_POINT('Ctrl Pts',(-12.2735346424426,31.776615948509,-9.19360257337038));
#86279=CARTESIAN_POINT('Ctrl Pts',(-11.8247356919297,35.1956764374484,-5.77829392033626));
#86280=CARTESIAN_POINT('Ctrl Pts',(-11.3759367414169,36.7894556396735,-1.21574785540399));
#86281=CARTESIAN_POINT('Ctrl Pts',(-10.9271377909041,36.2504739124864,3.58626227294545));
#86282=CARTESIAN_POINT('Ctrl Pts',(-10.6279384905622,34.5353419369983,6.31390046791915));
#86283=CARTESIAN_POINT('Ctrl Pts',(-10.4783388403913,33.4246212024587,7.42462120245876));
#86284=CARTESIAN_POINT('',(-13.6199315868015,18.5753787975412,-7.42462120245874));
#86285=CARTESIAN_POINT('',(-10.4783388403913,33.4246212024587,7.42462120245876));
#86286=CARTESIAN_POINT('Ctrl Pts',(-17.341,36.2781643676599,2.14693670874701));
#86287=CARTESIAN_POINT('Ctrl Pts',(-17.1478414134638,35.8634651076156,4.13225241019146));
#86288=CARTESIAN_POINT('Ctrl Pts',(-16.9546828269275,34.8587505394928,5.99049186542473));
#86289=CARTESIAN_POINT('Ctrl Pts',(-16.7615242403913,33.4246212024587,7.42462120245876));
#86290=CARTESIAN_POINT('Ctrl Pts',(-17.5341585865363,35.5470552038234,1.99422022691288));
#86291=CARTESIAN_POINT('Ctrl Pts',(-17.341,35.1618544435509,3.83831591566697));
#86292=CARTESIAN_POINT('Ctrl Pts',(-17.1478414134638,34.2286075034518,5.56437458007748));
#86293=CARTESIAN_POINT('Ctrl Pts',(-16.9546828269275,32.8964910417647,6.89649104176468));
#86294=CARTESIAN_POINT('Ctrl Pts',(-17.7273171730725,34.8159460399869,1.84150374507876));
#86295=CARTESIAN_POINT('Ctrl Pts',(-17.5341585865363,34.4602437794863,3.54437942114248));
#86296=CARTESIAN_POINT('Ctrl Pts',(-17.341,33.5984644674109,5.13825729473024));
#86297=CARTESIAN_POINT('Ctrl Pts',(-17.1478414134638,32.3683608810706,6.3683608810706));
#86298=CARTESIAN_POINT('Ctrl Pts',(-17.9204757596088,34.0848368761504,1.68878726324463));
#86299=CARTESIAN_POINT('Ctrl Pts',(-17.7273171730725,33.7586331154217,3.250442926618));
#86300=CARTESIAN_POINT('Ctrl Pts',(-17.5341585865363,32.96832143137,4.71214000938299));
#86301=CARTESIAN_POINT('Ctrl Pts',(-17.341,31.8402307203765,5.84023072037652));
#86302=CARTESIAN_POINT('',(-16.7615242403913,33.4246212024587,7.42462120245876));
#86303=CARTESIAN_POINT('Ctrl Pts',(14.6516813050447,33.4616240069009,7.39654333888314));
#86304=CARTESIAN_POINT('Ctrl Pts',(14.8027409813318,32.3443801052069,8.52379090131628));
#86305=CARTESIAN_POINT('Ctrl Pts',(15.1034003077898,29.6043323150422,10.2532339919884));
#86306=CARTESIAN_POINT('Ctrl Pts',(15.5536592844188,24.7830334023154,10.7988321378608));
#86307=CARTESIAN_POINT('Ctrl Pts',(16.0024582349316,20.2198596429615,9.19921822804673));
#86308=CARTESIAN_POINT('Ctrl Pts',(16.4512571854445,16.7987093355857,5.78182911764146));
#86309=CARTESIAN_POINT('Ctrl Pts',(16.9000561359573,15.2039632259476,1.21649604870047));
#86310=CARTESIAN_POINT('Ctrl Pts',(17.3489898284458,15.7434301636902,-3.58988937742563));
#86311=CARTESIAN_POINT('Ctrl Pts',(17.6483238707635,17.4609906653758,-6.32021516100136));
#86312=CARTESIAN_POINT('Ctrl Pts',(17.7980582629102,18.573847497101,-7.43215861796121));
#86313=CARTESIAN_POINT('Ctrl Pts',(14.2631510305718,32.3946700237951,6.33889538324544));
#86314=CARTESIAN_POINT('Ctrl Pts',(14.4142107068588,31.4371832781721,7.30495534421649));
#86315=CARTESIAN_POINT('Ctrl Pts',(14.7148700333168,29.0889409315559,8.78710157398526));
#86316=CARTESIAN_POINT('Ctrl Pts',(15.1651290099459,24.9570501254182,9.25468344426202));
#86317=CARTESIAN_POINT('Ctrl Pts',(15.6139279604586,21.0463745907998,7.88380183601246));
#86318=CARTESIAN_POINT('Ctrl Pts',(16.0627269109714,18.1144220698418,4.9550726902204));
#86319=CARTESIAN_POINT('Ctrl Pts',(16.5115258614844,16.7477122043441,1.04254661042898));
#86320=CARTESIAN_POINT('Ctrl Pts',(16.9604595539729,17.2100395813897,-3.07656322126833));
#86321=CARTESIAN_POINT('Ctrl Pts',(17.2597935962906,18.6820023396344,-5.41647373234195));
#86322=CARTESIAN_POINT('Ctrl Pts',(17.4095279884373,19.6357293320462,-6.36941795544942));
#86323=CARTESIAN_POINT('Ctrl Pts',(13.8746207560988,31.3277160406894,5.28124742760773));
#86324=CARTESIAN_POINT('Ctrl Pts',(14.0256804323859,30.5299864511372,6.08611978711668));
#86325=CARTESIAN_POINT('Ctrl Pts',(14.3263397588439,28.5735495480696,7.32096915598215));
#86326=CARTESIAN_POINT('Ctrl Pts',(14.7765987354728,25.131066848521,7.71053475066323));
#86327=CARTESIAN_POINT('Ctrl Pts',(15.2253976859856,21.8728895386381,6.56838544397819));
#86328=CARTESIAN_POINT('Ctrl Pts',(15.6741966364985,19.430134804098,4.12831626279934));
#86329=CARTESIAN_POINT('Ctrl Pts',(16.1229955870113,18.2914611827405,0.868597172157502));
#86330=CARTESIAN_POINT('Ctrl Pts',(16.5719292794999,18.6766489990893,-2.56323706511104));
#86331=CARTESIAN_POINT('Ctrl Pts',(16.8712633218176,19.9030140138931,-4.51273230368253));
#86332=CARTESIAN_POINT('Ctrl Pts',(17.0209977139643,20.6976111669914,-5.30667729293762));
#86333=CARTESIAN_POINT('Ctrl Pts',(13.4860904816258,30.2607620575836,4.22359947197002));
#86334=CARTESIAN_POINT('Ctrl Pts',(13.637150157913,29.6227896241023,4.86728423001688));
#86335=CARTESIAN_POINT('Ctrl Pts',(13.937809484371,28.0581581645833,5.85483673797904));
#86336=CARTESIAN_POINT('Ctrl Pts',(14.3880684609999,25.3050835716238,6.16638605706443));
#86337=CARTESIAN_POINT('Ctrl Pts',(14.8368674115127,22.6994044864765,5.25296905194393));
#86338=CARTESIAN_POINT('Ctrl Pts',(15.2856663620255,20.7458475383541,3.30155983537828));
#86339=CARTESIAN_POINT('Ctrl Pts',(15.7344653125384,19.835210161137,0.694647733886021));
#86340=CARTESIAN_POINT('Ctrl Pts',(16.183399005027,20.1432584167887,-2.04991090895374));
#86341=CARTESIAN_POINT('Ctrl Pts',(16.4827330473447,21.1240256881518,-3.60899087502311));
#86342=CARTESIAN_POINT('Ctrl Pts',(16.6324674394913,21.7594930019366,-4.24393663042583));
#86343=CARTESIAN_POINT('Ctrl Pts',(11.6418674365106,30.243937729078,4.2405051874113));
#86344=CARTESIAN_POINT('Ctrl Pts',(11.7916019429138,29.6089916310296,4.87597404391556));
#86345=CARTESIAN_POINT('Ctrl Pts',(12.0909360994881,28.0500582137326,5.85575499156165));
#86346=CARTESIAN_POINT('Ctrl Pts',(12.5398699062332,25.3050832312864,6.16638143414342));
#86347=CARTESIAN_POINT('Ctrl Pts',(12.9886688567461,22.6994010669056,5.25296850297539));
#86348=CARTESIAN_POINT('Ctrl Pts',(13.4374678072589,20.7458456743692,3.30155412730027));
#86349=CARTESIAN_POINT('Ctrl Pts',(13.8862667577717,19.8352021475569,0.694642440642844));
#86350=CARTESIAN_POINT('Ctrl Pts',(14.335200564517,20.1432560444607,-2.04991703657224));
#86351=CARTESIAN_POINT('Ctrl Pts',(14.6345347210911,21.124026847436,-3.6089917582658));
#86352=CARTESIAN_POINT('Ctrl Pts',(14.7842692274945,21.7594948113833,-4.24393772890585));
#86353=CARTESIAN_POINT('Ctrl Pts',(11.2538899933664,31.3051666043796,5.3008757295882));
#86354=CARTESIAN_POINT('Ctrl Pts',(11.4036244997697,30.511447410088,6.09524840205956));
#86355=CARTESIAN_POINT('Ctrl Pts',(11.7029586563439,28.5626908467601,7.3200310202034));
#86356=CARTESIAN_POINT('Ctrl Pts',(12.1518924630891,25.1313140131761,7.70833196494418));
#86357=CARTESIAN_POINT('Ctrl Pts',(12.6006914136019,21.874061225185,6.56651319007401));
#86358=CARTESIAN_POINT('Ctrl Pts',(13.0494903641148,19.4320044633055,4.12713282258986));
#86359=CARTESIAN_POINT('Ctrl Pts',(13.4982893146276,18.2936476033927,0.868343060934551));
#86360=CARTESIAN_POINT('Ctrl Pts',(13.9472231213727,18.6787327178621,-2.5625143671782));
#86361=CARTESIAN_POINT('Ctrl Pts',(14.246557277947,19.9047527121812,-4.51144756914065));
#86362=CARTESIAN_POINT('Ctrl Pts',(14.3962917843502,20.699124268905,-5.30516660416449));
#86363=CARTESIAN_POINT('Ctrl Pts',(10.8659125502221,32.3663954796812,6.3612462717651));
#86364=CARTESIAN_POINT('Ctrl Pts',(11.0156470566255,31.4139031891465,7.31452276020357));
#86365=CARTESIAN_POINT('Ctrl Pts',(11.3149812131996,29.0753234797877,8.78430704884515));
#86366=CARTESIAN_POINT('Ctrl Pts',(11.7639150199449,24.957544795066,9.25028249574495));
#86367=CARTESIAN_POINT('Ctrl Pts',(12.2127139704577,21.0487213834643,7.88005787717263));
#86368=CARTESIAN_POINT('Ctrl Pts',(12.6615129209705,18.1181632522417,4.95271151787947));
#86369=CARTESIAN_POINT('Ctrl Pts',(13.1103118714834,16.7520930592284,1.04204368122625));
#86370=CARTESIAN_POINT('Ctrl Pts',(13.5592456782285,17.2142093912634,-3.07511169778416));
#86371=CARTESIAN_POINT('Ctrl Pts',(13.8585798348028,18.6854785769265,-5.4139033800155));
#86372=CARTESIAN_POINT('Ctrl Pts',(14.008314341206,19.6387537264267,-6.36639547942313));
#86373=CARTESIAN_POINT('Ctrl Pts',(10.477935107078,33.4276243549829,7.421616813942));
#86374=CARTESIAN_POINT('Ctrl Pts',(10.6276696134812,32.316358968205,8.53379711834758));
#86375=CARTESIAN_POINT('Ctrl Pts',(10.9270037700554,29.5879561128153,10.2485830774869));
#86376=CARTESIAN_POINT('Ctrl Pts',(11.3759375768006,24.7837755769558,10.7922330265457));
#86377=CARTESIAN_POINT('Ctrl Pts',(11.8247365273135,20.2233815417436,9.19360256427124));
#86378=CARTESIAN_POINT('Ctrl Pts',(12.2735354778263,16.804322041178,5.77829021316907));
#86379=CARTESIAN_POINT('Ctrl Pts',(12.7223344283391,15.2105385150642,1.21574430151796));
#86380=CARTESIAN_POINT('Ctrl Pts',(13.1712682350843,15.7496860646647,-3.58770902839013));
#86381=CARTESIAN_POINT('Ctrl Pts',(13.4706023916585,17.4662044416717,-6.31635919089035));
#86382=CARTESIAN_POINT('Ctrl Pts',(13.6203368980619,18.5783831839484,-7.42762435468178));
#86383=CARTESIAN_POINT('Ctrl Pts',(10.478339675775,33.4246212024587,7.42462120245875));
#86384=CARTESIAN_POINT('Ctrl Pts',(10.6279393259459,32.3139004679191,8.53534193699834));
#86385=CARTESIAN_POINT('Ctrl Pts',(10.9271386262878,29.5865129742571,10.2487463857135));
#86386=CARTESIAN_POINT('Ctrl Pts',(11.3759375768006,24.7837755769558,10.7922330265457));
#86387=CARTESIAN_POINT('Ctrl Pts',(11.8247365273135,20.2233815417436,9.19360256427124));
#86388=CARTESIAN_POINT('Ctrl Pts',(12.2735354778263,16.804322041178,5.77829021316907));
#86389=CARTESIAN_POINT('Ctrl Pts',(12.7223344283391,15.2105385150642,1.21574430151797));
#86390=CARTESIAN_POINT('Ctrl Pts',(13.1711333788519,15.7495241089239,-3.58626610827894));
#86391=CARTESIAN_POINT('Ctrl Pts',(13.4703326791938,17.4646580630017,-6.31390046791915));
#86392=CARTESIAN_POINT('Ctrl Pts',(13.6199323293648,18.5753787975412,-7.42462120245874));
#86393=CARTESIAN_POINT('Ctrl Pts',(8.37081273969933,33.4276247350626,7.42161643355506));
#86394=CARTESIAN_POINT('Ctrl Pts',(8.52054726317341,32.3163592768284,8.53379692106831));
#86395=CARTESIAN_POINT('Ctrl Pts',(8.81988143681844,29.5879591503046,10.2485849356456));
#86396=CARTESIAN_POINT('Ctrl Pts',(9.2688152606344,24.7837753005194,10.7922291011963));
#86397=CARTESIAN_POINT('Ctrl Pts',(9.71761421114723,20.2233781174552,9.19360269140817));
#86398=CARTESIAN_POINT('Ctrl Pts',(10.1664131616601,16.8043200601272,5.77828511785067));
#86399=CARTESIAN_POINT('Ctrl Pts',(10.6152121121729,15.2105304314665,1.21573946002376));
#86400=CARTESIAN_POINT('Ctrl Pts',(11.0641459359888,15.7496834327425,-3.58771450934957));
#86401=CARTESIAN_POINT('Ctrl Pts',(11.3634801096339,17.4662046398477,-6.31635949733812));
#86402=CARTESIAN_POINT('Ctrl Pts',(11.5132146331079,18.5783835643338,-7.42762473476445));
#86403=CARTESIAN_POINT('Ctrl Pts',(7.98283529009083,32.3663957877751,6.36124592805898));
#86404=CARTESIAN_POINT('Ctrl Pts',(8.13256981356493,31.4139034386388,7.31452257079588));
#86405=CARTESIAN_POINT('Ctrl Pts',(8.43190398720995,29.0753260747516,8.7843086171207));
#86406=CARTESIAN_POINT('Ctrl Pts',(8.88083781102592,24.957544561021,9.25027910554244));
#86407=CARTESIAN_POINT('Ctrl Pts',(9.32963676153874,21.0487184621757,7.88005796425917));
#86408=CARTESIAN_POINT('Ctrl Pts',(9.77843571205157,18.118161576126,4.95270713680419));
#86409=CARTESIAN_POINT('Ctrl Pts',(10.2272346625643,16.752086156267,1.04203952857104));
#86410=CARTESIAN_POINT('Ctrl Pts',(10.6761684863804,17.2142071597807,-3.07511638710569));
#86411=CARTESIAN_POINT('Ctrl Pts',(10.9755026600254,18.6854787671028,-5.41390362764302));
#86412=CARTESIAN_POINT('Ctrl Pts',(11.1252371834995,19.6387540701316,-6.36639578751951));
#86413=CARTESIAN_POINT('Ctrl Pts',(7.59485784048235,31.3051668404876,5.3008754225629));
#86414=CARTESIAN_POINT('Ctrl Pts',(7.74459236395643,30.5114476004492,6.09524822052343));
#86415=CARTESIAN_POINT('Ctrl Pts',(8.04392653760145,28.5626929991986,7.32003229859578));
#86416=CARTESIAN_POINT('Ctrl Pts',(8.49286036141743,25.1313138215225,7.70832910988854));
#86417=CARTESIAN_POINT('Ctrl Pts',(8.94165931193025,21.8740588068962,6.56651323711017));
#86418=CARTESIAN_POINT('Ctrl Pts',(9.39045826244308,19.4320030921246,4.1271291557577));
#86419=CARTESIAN_POINT('Ctrl Pts',(9.83925721295591,18.2936418810676,0.868339597118319));
#86420=CARTESIAN_POINT('Ctrl Pts',(10.2881910367718,18.6787308868189,-2.56251826486181));
#86421=CARTESIAN_POINT('Ctrl Pts',(10.5875252104169,19.9047528943578,-4.51144775794791));
#86422=CARTESIAN_POINT('Ctrl Pts',(10.737259733891,20.6991245759293,-5.30516684027456));
#86423=CARTESIAN_POINT('Ctrl Pts',(7.20688039087386,30.2439378932,4.24050491706681));
#86424=CARTESIAN_POINT('Ctrl Pts',(7.35661491434794,29.6089917622597,4.87597387025098));
#86425=CARTESIAN_POINT('Ctrl Pts',(7.65594908799297,28.0500599236457,5.85575598007085));
#86426=CARTESIAN_POINT('Ctrl Pts',(8.10488291180894,25.3050830820241,6.16637911423465));
#86427=CARTESIAN_POINT('Ctrl Pts',(8.55368186232177,22.6993991516167,5.25296850996117));
#86428=CARTESIAN_POINT('Ctrl Pts',(9.0024808128346,20.7458446081234,3.30155117471121));
#86429=CARTESIAN_POINT('Ctrl Pts',(9.45127976334742,19.8351976058681,0.694639665665589));
#86430=CARTESIAN_POINT('Ctrl Pts',(9.9002135871634,20.143254613857,-2.04992014261793));
#86431=CARTESIAN_POINT('Ctrl Pts',(10.1995477608084,21.124027021613,-3.6089918882528));
#86432=CARTESIAN_POINT('Ctrl Pts',(10.3492822842825,21.759495081727,-4.24393789302962));
#86433=CARTESIAN_POINT('Ctrl Pts',(8.37121735960875,33.4246212024587,7.42462120245875));
#86434=CARTESIAN_POINT('Ctrl Pts',(8.52081700977969,32.3139004679191,8.53534193699834));
#86435=CARTESIAN_POINT('Ctrl Pts',(8.82001631012158,29.5865129742571,10.2487463857135));
#86436=CARTESIAN_POINT('Ctrl Pts',(9.2688152606344,24.7837755769558,10.7922330265457));
#86437=CARTESIAN_POINT('Ctrl Pts',(9.71761421114723,20.2233815417436,9.19360256427124));
#86438=CARTESIAN_POINT('Ctrl Pts',(10.1664131616601,16.804322041178,5.77829021316907));
#86439=CARTESIAN_POINT('Ctrl Pts',(10.6152121121729,15.2105385150642,1.21574430151797));
#86440=CARTESIAN_POINT('Ctrl Pts',(11.0640110626857,15.7495241089239,-3.58626610827894));
#86441=CARTESIAN_POINT('Ctrl Pts',(11.3632103630276,17.4646580630017,-6.31390046791915));
#86442=CARTESIAN_POINT('Ctrl Pts',(11.5128100131985,18.5753787975412,-7.42462120245874));
#86443=CARTESIAN_POINT('Ctrl Pts',(10.478339675775,33.4246212024587,7.42462120245875));
#86444=CARTESIAN_POINT('Ctrl Pts',(10.6279393259459,32.3139004679191,8.53534193699834));
#86445=CARTESIAN_POINT('Ctrl Pts',(10.9271386262878,29.5865129742571,10.2487463857135));
#86446=CARTESIAN_POINT('Ctrl Pts',(11.3759375768006,24.7837755769558,10.7922330265457));
#86447=CARTESIAN_POINT('Ctrl Pts',(11.8247365273135,20.2233815417436,9.19360256427124));
#86448=CARTESIAN_POINT('Ctrl Pts',(12.2735354778263,16.804322041178,5.77829021316907));
#86449=CARTESIAN_POINT('Ctrl Pts',(12.7223344283391,15.2105385150642,1.21574430151797));
#86450=CARTESIAN_POINT('Ctrl Pts',(13.1711333788519,15.7495241089239,-3.58626610827894));
#86451=CARTESIAN_POINT('Ctrl Pts',(13.4703326791938,17.4646580630017,-6.31390046791915));
#86452=CARTESIAN_POINT('Ctrl Pts',(13.6199323293648,18.5753787975412,-7.42462120245874));
#86453=CARTESIAN_POINT('Ctrl Pts',(9.77596557038624,33.4246212024587,7.42462120245875));
#86454=CARTESIAN_POINT('Ctrl Pts',(9.92556522055718,32.3139004679191,8.53534193699834));
#86455=CARTESIAN_POINT('Ctrl Pts',(10.2247645208991,29.5865129742571,10.2487463857135));
#86456=CARTESIAN_POINT('Ctrl Pts',(10.6735634714119,24.7837755769558,10.7922330265457));
#86457=CARTESIAN_POINT('Ctrl Pts',(11.1223624219247,20.2233815417436,9.19360256427124));
#86458=CARTESIAN_POINT('Ctrl Pts',(11.5711613724375,16.804322041178,5.77829021316907));
#86459=CARTESIAN_POINT('Ctrl Pts',(12.0199603229504,15.2105385150642,1.21574430151797));
#86460=CARTESIAN_POINT('Ctrl Pts',(12.4687592734632,15.7495241089239,-3.58626610827895));
#86461=CARTESIAN_POINT('Ctrl Pts',(12.7679585738051,17.4646580630017,-6.31390046791915));
#86462=CARTESIAN_POINT('Ctrl Pts',(12.917558223976,18.5753787975412,-7.42462120245874));
#86463=CARTESIAN_POINT('Ctrl Pts',(9.07359146499749,33.4246212024587,7.42462120245875));
#86464=CARTESIAN_POINT('Ctrl Pts',(9.22319111516843,32.3139004679191,8.53534193699834));
#86465=CARTESIAN_POINT('Ctrl Pts',(9.52239041551032,29.5865129742571,10.2487463857135));
#86466=CARTESIAN_POINT('Ctrl Pts',(9.97118936602315,24.7837755769558,10.7922330265457));
#86467=CARTESIAN_POINT('Ctrl Pts',(10.419988316536,20.2233815417436,9.19360256427124));
#86468=CARTESIAN_POINT('Ctrl Pts',(10.8687872670488,16.804322041178,5.77829021316907));
#86469=CARTESIAN_POINT('Ctrl Pts',(11.3175862175616,15.2105385150642,1.21574430151797));
#86470=CARTESIAN_POINT('Ctrl Pts',(11.7663851680745,15.7495241089239,-3.58626610827894));
#86471=CARTESIAN_POINT('Ctrl Pts',(12.0655844684163,17.4646580630017,-6.31390046791915));
#86472=CARTESIAN_POINT('Ctrl Pts',(12.2151841185873,18.5753787975412,-7.42462120245874));
#86473=CARTESIAN_POINT('Ctrl Pts',(8.37121735960875,33.4246212024587,7.42462120245875));
#86474=CARTESIAN_POINT('Ctrl Pts',(8.52081700977969,32.3139004679191,8.53534193699834));
#86475=CARTESIAN_POINT('Ctrl Pts',(8.82001631012158,29.5865129742571,10.2487463857135));
#86476=CARTESIAN_POINT('Ctrl Pts',(9.2688152606344,24.7837755769558,10.7922330265457));
#86477=CARTESIAN_POINT('Ctrl Pts',(9.71761421114723,20.2233815417436,9.19360256427124));
#86478=CARTESIAN_POINT('Ctrl Pts',(10.1664131616601,16.804322041178,5.77829021316907));
#86479=CARTESIAN_POINT('Ctrl Pts',(10.6152121121729,15.2105385150642,1.21574430151797));
#86480=CARTESIAN_POINT('Ctrl Pts',(11.0640110626857,15.7495241089239,-3.58626610827894));
#86481=CARTESIAN_POINT('Ctrl Pts',(11.3632103630276,17.4646580630017,-6.31390046791915));
#86482=CARTESIAN_POINT('Ctrl Pts',(11.5128100131985,18.5753787975412,-7.42462120245874));
#86483=CARTESIAN_POINT('Ctrl Pts',(5.35868174475438,30.2439392339151,4.24050270859203));
#86484=CARTESIAN_POINT('Ctrl Pts',(5.5084164076812,29.6089928430004,4.87597245720932));
#86485=CARTESIAN_POINT('Ctrl Pts',(5.80775072077896,28.0500642248033,5.85575779538567));
#86486=CARTESIAN_POINT('Ctrl Pts',(6.25668468404766,25.3050829459043,6.16637363300279));
#86487=CARTESIAN_POINT('Ctrl Pts',(6.70548363456049,22.6993954022398,5.25296843898345));
#86488=CARTESIAN_POINT('Ctrl Pts',(7.15428258507332,20.7458430022638,3.30154467940644));
#86489=CARTESIAN_POINT('Ctrl Pts',(7.60308153558614,19.8351883604915,0.694633848166402));
#86490=CARTESIAN_POINT('Ctrl Pts',(8.05201549885485,20.143252256087,-2.04992724536302));
#86491=CARTESIAN_POINT('Ctrl Pts',(8.35134981195262,21.1240284360682,-3.60899296659441));
#86492=CARTESIAN_POINT('Ctrl Pts',(8.50108447487943,21.7594972901986,-4.24393923374772));
#86493=CARTESIAN_POINT('Ctrl Pts',(4.9707042423387,31.3051687692584,5.30087291443731));
#86494=CARTESIAN_POINT('Ctrl Pts',(5.12043890526552,30.5114491664153,6.09524674458825));
#86495=CARTESIAN_POINT('Ctrl Pts',(5.41977321836328,28.5626984980101,7.3200349166553));
#86496=CARTESIAN_POINT('Ctrl Pts',(5.86870718163198,25.1313136099707,7.70832262534694));
#86497=CARTESIAN_POINT('Ctrl Pts',(6.31750613214481,21.8740539233512,6.56651346128887));
#86498=CARTESIAN_POINT('Ctrl Pts',(6.76630508265764,19.4320007717319,4.12712123291654));
#86499=CARTESIAN_POINT('Ctrl Pts',(7.21510403317047,18.2936299565934,0.868332366286644));
#86500=CARTESIAN_POINT('Ctrl Pts',(7.66403799643918,18.6787275906001,-2.56252726581087));
#86501=CARTESIAN_POINT('Ctrl Pts',(7.96337230953693,19.9047543720601,-4.51144932091485));
#86502=CARTESIAN_POINT('Ctrl Pts',(8.11310697246375,20.6991270840509,-5.30516876904924));
#86503=CARTESIAN_POINT('Ctrl Pts',(4.58272673992303,32.3663983046018,6.36124312028259));
#86504=CARTESIAN_POINT('Ctrl Pts',(4.73246140284985,31.4139054898301,7.31452103196719));
#86505=CARTESIAN_POINT('Ctrl Pts',(5.0317957159476,29.075332771217,8.78431203792494));
#86506=CARTESIAN_POINT('Ctrl Pts',(5.48072967921631,24.9575442740369,9.25027161769109));
#86507=CARTESIAN_POINT('Ctrl Pts',(5.92952862972914,21.0487124444625,7.88005848359428));
#86508=CARTESIAN_POINT('Ctrl Pts',(6.37832758024196,18.1181585412,4.95269778642663));
#86509=CARTESIAN_POINT('Ctrl Pts',(6.82712653075479,16.7520715526952,1.04203088440688));
#86510=CARTESIAN_POINT('Ctrl Pts',(7.2760604940235,17.2142029251132,-3.07512728625873));
#86511=CARTESIAN_POINT('Ctrl Pts',(7.57539480712126,18.6854803080521,-5.41390567523528));
#86512=CARTESIAN_POINT('Ctrl Pts',(7.72512947004808,19.6387568779032,-6.36639830435076));
#86513=CARTESIAN_POINT('Ctrl Pts',(4.19474923750735,33.4276278399451,7.42161332612787));
#86514=CARTESIAN_POINT('Ctrl Pts',(4.34448390043417,32.3163618132449,8.53379531934612));
#86515=CARTESIAN_POINT('Ctrl Pts',(4.64381821353193,29.5879670444238,10.2485891591946));
#86516=CARTESIAN_POINT('Ctrl Pts',(5.09275217680063,24.7837749381033,10.7922206100352));
#86517=CARTESIAN_POINT('Ctrl Pts',(5.54155112731346,20.2233709655738,9.19360350589969));
#86518=CARTESIAN_POINT('Ctrl Pts',(5.99035007782629,16.8043163106681,5.77827433993672));
#86519=CARTESIAN_POINT('Ctrl Pts',(6.43914902833912,15.210513148797,1.21572940252713));
#86520=CARTESIAN_POINT('Ctrl Pts',(6.88808299160782,15.7496782596263,-3.58772730670658));
#86521=CARTESIAN_POINT('Ctrl Pts',(7.18741730470558,17.4662062440441,-6.31636202955571));
#86522=CARTESIAN_POINT('Ctrl Pts',(7.3371519676324,18.5783866717555,-7.42762783965229));
#86523=CARTESIAN_POINT('Ctrl Pts',(4.19515427577498,33.4246212024587,7.42462120245875));
#86524=CARTESIAN_POINT('Ctrl Pts',(4.34475392594592,32.3139004679191,8.53534193699834));
#86525=CARTESIAN_POINT('Ctrl Pts',(4.64395322628781,29.5865222278826,10.2487526513479));
#86526=CARTESIAN_POINT('Ctrl Pts',(5.09275217680063,24.7837749381033,10.7922206100352));
#86527=CARTESIAN_POINT('Ctrl Pts',(5.54155112731346,20.2233709655738,9.1936035058997));
#86528=CARTESIAN_POINT('Ctrl Pts',(5.99035007782629,16.8043163106681,5.77827433993673));
#86529=CARTESIAN_POINT('Ctrl Pts',(6.43914902833912,15.2105131487971,1.21572940252714));
#86530=CARTESIAN_POINT('Ctrl Pts',(6.88794797885194,15.7495161106836,-3.58628271132928));
#86531=CARTESIAN_POINT('Ctrl Pts',(7.18714727919383,17.4646580630017,-6.31390046791915));
#86532=CARTESIAN_POINT('Ctrl Pts',(7.33674692936478,18.5753787975412,-7.42462120245874));
#86533=CARTESIAN_POINT('Ctrl Pts',(2.08762722947389,33.4276297757683,7.4216136630885));
#86534=CARTESIAN_POINT('Ctrl Pts',(2.23736192827097,32.3163634308879,8.53379621253978));
#86535=CARTESIAN_POINT('Ctrl Pts',(2.53669627723901,29.5879716382176,10.2485932995738));
#86536=CARTESIAN_POINT('Ctrl Pts',(2.98563027637797,24.7837746802806,10.7922175564503));
#86537=CARTESIAN_POINT('Ctrl Pts',(3.4344292268908,20.2233662640449,9.19360566949466));
#86538=CARTESIAN_POINT('Ctrl Pts',(3.88322817740363,16.8043131390746,5.77826939950743));
#86539=CARTESIAN_POINT('Ctrl Pts',(4.33202712791647,15.210502056439,1.21572426912528));
#86540=CARTESIAN_POINT('Ctrl Pts',(4.78096112705543,15.7496740126713,-3.58773440230587));
#86541=CARTESIAN_POINT('Ctrl Pts',(5.08029547602347,17.4662053513639,-6.31636364499683));
#86542=CARTESIAN_POINT('Ctrl Pts',(5.23003017482055,18.5783863347936,-7.42762977547842));
#86543=CARTESIAN_POINT('Ctrl Pts',(1.69964957489386,32.3663997101047,6.36124315556745));
#86544=CARTESIAN_POINT('Ctrl Pts',(1.84938427369095,31.4139066605754,7.31452150601911));
#86545=CARTESIAN_POINT('Ctrl Pts',(2.14871862265898,29.0753365860982,8.78431523663789));
#86546=CARTESIAN_POINT('Ctrl Pts',(2.59765262179796,24.9575440945989,9.25026863171355));
#86547=CARTESIAN_POINT('Ctrl Pts',(3.04645157231079,21.0487086120065,7.88006002399772));
#86548=CARTESIAN_POINT('Ctrl Pts',(3.49525052282361,18.1181561368879,4.9526933544726));
#86549=CARTESIAN_POINT('Ctrl Pts',(3.94404947333644,16.7520624137522,1.04202644291405));
#86550=CARTESIAN_POINT('Ctrl Pts',(4.39298347247541,17.2141996351108,-3.07513324550561));
#86551=CARTESIAN_POINT('Ctrl Pts',(4.69231782144344,18.6854798344402,-5.41390684409329));
#86552=CARTESIAN_POINT('Ctrl Pts',(4.84205252024054,19.6387568426173,-6.36639970985615));
#86553=CARTESIAN_POINT('Ctrl Pts',(1.31167192031384,31.305169644441,5.3008726480464));
#86554=CARTESIAN_POINT('Ctrl Pts',(1.46140661911093,30.5114498902629,6.09524679949844));
#86555=CARTESIAN_POINT('Ctrl Pts',(1.76074096807896,28.5627015339787,7.32003717370199));
#86556=CARTESIAN_POINT('Ctrl Pts',(2.20967496721793,25.131313508917,7.70831970697682));
#86557=CARTESIAN_POINT('Ctrl Pts',(2.65847391773076,21.8740509599683,6.56651437850079));
#86558=CARTESIAN_POINT('Ctrl Pts',(3.10727286824359,19.4319991347012,4.12711730943777));
#86559=CARTESIAN_POINT('Ctrl Pts',(3.55607181875642,18.2936227710653,0.868328616702831));
#86560=CARTESIAN_POINT('Ctrl Pts',(4.00500581789539,18.6787252575502,-2.56253208870534));
#86561=CARTESIAN_POINT('Ctrl Pts',(4.30434016686343,19.9047543175165,-4.51145004318976));
#86562=CARTESIAN_POINT('Ctrl Pts',(4.45407486566051,20.6991273504409,-5.30516964423389));
#86563=CARTESIAN_POINT('Ctrl Pts',(0.923694265733817,30.2439395787773,4.24050214052534));
#86564=CARTESIAN_POINT('Ctrl Pts',(1.0734289645309,29.6089931199504,4.87597209297777));
#86565=CARTESIAN_POINT('Ctrl Pts',(1.37276331349894,28.0500664818591,5.85575911076608));
#86566=CARTESIAN_POINT('Ctrl Pts',(1.82169731263791,25.3050829232352,6.16637078224008));
#86567=CARTESIAN_POINT('Ctrl Pts',(2.27049626315073,22.6993933079299,5.25296873300386));
#86568=CARTESIAN_POINT('Ctrl Pts',(2.71929521366356,20.7458421325144,3.30154126440294));
#86569=CARTESIAN_POINT('Ctrl Pts',(3.16809416417639,19.8351831283785,0.6946307904916));
#86570=CARTESIAN_POINT('Ctrl Pts',(3.61702816331537,20.1432508799898,-2.04993093190507));
#86571=CARTESIAN_POINT('Ctrl Pts',(3.9163625122834,21.124028800593,-3.60899324228622));
#86572=CARTESIAN_POINT('Ctrl Pts',(4.06609721108049,21.7594978582645,-4.24393957861161));
#86573=CARTESIAN_POINT('Ctrl Pts',(2.08803195960875,33.4246212024587,7.42462120245875));
#86574=CARTESIAN_POINT('Ctrl Pts',(2.21811206017887,32.4588257297478,8.39041667516967));
#86575=CARTESIAN_POINT('Ctrl Pts',(2.34820226714463,31.3016837902186,9.16424028291839));
#86576=CARTESIAN_POINT('Ctrl Pts',(2.62717564621961,28.599440768817,10.2935716436691));
#86577=CARTESIAN_POINT('Ctrl Pts',(2.7581160852288,27.2104401715646,10.4952143025461));
#86578=CARTESIAN_POINT('Ctrl Pts',(3.03683618944768,24.2839074379147,10.508047074406));
#86579=CARTESIAN_POINT('Ctrl Pts',(3.17097575048872,22.9060540952459,10.0808266335396));
#86580=CARTESIAN_POINT('Ctrl Pts',(3.39661765884711,20.7150047323306,9.17859210179939));
#86581=CARTESIAN_POINT('Ctrl Pts',(3.52698910038257,19.5549163112383,8.40289350048828));
#86582=CARTESIAN_POINT('Ctrl Pts',(3.7906967856087,17.5961616011175,6.44526974701291));
#86583=CARTESIAN_POINT('Ctrl Pts',(3.92095407984858,16.821005659722,5.28667072334715));
#86584=CARTESIAN_POINT('Ctrl Pts',(4.15157399185054,15.9001504081183,3.04686683603555));
#86585=CARTESIAN_POINT('Ctrl Pts',(4.28507227448216,15.4945892500986,1.67135405527008));
#86586=CARTESIAN_POINT('Ctrl Pts',(4.55616748351115,15.5046184878954,-1.17517952963084));
#86587=CARTESIAN_POINT('Ctrl Pts',(4.68788920228244,15.6947442723585,-2.57456045049193));
#86588=CARTESIAN_POINT('Ctrl Pts',(4.96973339204285,16.8367707735847,-5.30408588680115));
#86589=CARTESIAN_POINT('Ctrl Pts',(5.09968523508116,17.6106281357367,-6.45987054065413));
#86590=CARTESIAN_POINT('Ctrl Pts',(5.22962461319854,18.5753787975412,-7.42462120245874));
#86591=CARTESIAN_POINT('Ctrl Pts',(4.19515427577498,33.4246212024587,7.42462120245875));
#86592=CARTESIAN_POINT('Ctrl Pts',(4.34475392594592,32.3139004679191,8.53534193699834));
#86593=CARTESIAN_POINT('Ctrl Pts',(4.64395322628781,29.5865222278826,10.2487526513479));
#86594=CARTESIAN_POINT('Ctrl Pts',(5.09275217680063,24.7837749381033,10.7922206100352));
#86595=CARTESIAN_POINT('Ctrl Pts',(5.54155112731346,20.2233709655738,9.1936035058997));
#86596=CARTESIAN_POINT('Ctrl Pts',(5.99035007782629,16.8043163106681,5.77827433993673));
#86597=CARTESIAN_POINT('Ctrl Pts',(6.43914902833912,15.2105131487971,1.21572940252714));
#86598=CARTESIAN_POINT('Ctrl Pts',(6.88794797885194,15.7495161106836,-3.58628271132928));
#86599=CARTESIAN_POINT('Ctrl Pts',(7.18714727919383,17.4646580630017,-6.31390046791915));
#86600=CARTESIAN_POINT('Ctrl Pts',(7.33674692936478,18.5753787975412,-7.42462120245874));
#86601=CARTESIAN_POINT('Ctrl Pts',(3.49277937258034,33.4246212024587,7.42462120245875));
#86602=CARTESIAN_POINT('Ctrl Pts',(3.64237902275128,32.3139004679191,8.53534193699834));
#86603=CARTESIAN_POINT('Ctrl Pts',(3.94157832309317,29.5865222278826,10.2487526513479));
#86604=CARTESIAN_POINT('Ctrl Pts',(4.39037727360599,24.7837749381034,10.7922206100352));
#86605=CARTESIAN_POINT('Ctrl Pts',(4.83917622411882,20.2233709655738,9.1936035058997));
#86606=CARTESIAN_POINT('Ctrl Pts',(5.28797517463164,16.8043163106681,5.77827433993673));
#86607=CARTESIAN_POINT('Ctrl Pts',(5.73677412514448,15.2105131487971,1.21572940252714));
#86608=CARTESIAN_POINT('Ctrl Pts',(6.1855730756573,15.7495161106836,-3.58628271132928));
#86609=CARTESIAN_POINT('Ctrl Pts',(6.48477237599919,17.4646580630017,-6.31390046791915));
#86610=CARTESIAN_POINT('Ctrl Pts',(6.63437202617013,18.5753787975412,-7.42462120245874));
#86611=CARTESIAN_POINT('Ctrl Pts',(2.79040446938569,33.4246212024587,7.42462120245875));
#86612=CARTESIAN_POINT('Ctrl Pts',(2.94000411955663,32.3139004679191,8.53534193699834));
#86613=CARTESIAN_POINT('Ctrl Pts',(3.23920341989852,29.5865222278826,10.2487526513479));
#86614=CARTESIAN_POINT('Ctrl Pts',(3.68800237041135,24.7837749381034,10.7922206100352));
#86615=CARTESIAN_POINT('Ctrl Pts',(4.13680132092417,20.2233709655738,9.1936035058997));
#86616=CARTESIAN_POINT('Ctrl Pts',(4.585600271437,16.8043163106681,5.77827433993673));
#86617=CARTESIAN_POINT('Ctrl Pts',(5.03439922194982,15.2105131487971,1.21572940252714));
#86618=CARTESIAN_POINT('Ctrl Pts',(5.48319817246266,15.7495161106836,-3.58628271132928));
#86619=CARTESIAN_POINT('Ctrl Pts',(5.78239747280454,17.4646580630017,-6.31390046791915));
#86620=CARTESIAN_POINT('Ctrl Pts',(5.93199712297549,18.5753787975412,-7.42462120245874));
#86621=CARTESIAN_POINT('Ctrl Pts',(2.08802956619104,33.4246212024587,7.42462120245875));
#86622=CARTESIAN_POINT('Ctrl Pts',(2.23762921636198,32.3139004679191,8.53534193699834));
#86623=CARTESIAN_POINT('Ctrl Pts',(2.53682851670387,29.5865222278826,10.2487526513479));
#86624=CARTESIAN_POINT('Ctrl Pts',(2.98562746721669,24.7837749381033,10.7922206100352));
#86625=CARTESIAN_POINT('Ctrl Pts',(3.43442641772952,20.2233709655738,9.1936035058997));
#86626=CARTESIAN_POINT('Ctrl Pts',(3.88322536824235,16.8043163106681,5.77827433993673));
#86627=CARTESIAN_POINT('Ctrl Pts',(4.33202431875518,15.2105131487971,1.21572940252714));
#86628=CARTESIAN_POINT('Ctrl Pts',(4.780823269268,15.7495161106836,-3.58628271132928));
#86629=CARTESIAN_POINT('Ctrl Pts',(5.08002256960989,17.4646580630017,-6.31390046791915));
#86630=CARTESIAN_POINT('Ctrl Pts',(5.22962221978083,18.5753787975412,-7.42462120245874));
#86631=CARTESIAN_POINT('Ctrl Pts',(-0.924503774144115,30.2439398471762,
4.24050169840643));
#86632=CARTESIAN_POINT('Ctrl Pts',(-0.774769047429751,29.6089933369654,
4.87597181055117));
#86633=CARTESIAN_POINT('Ctrl Pts',(-0.475434670544444,28.0500666106541,
5.85575897175579));
#86634=CARTESIAN_POINT('Ctrl Pts',(-0.0265006434881952,25.3050829374398,
6.16637065619458));
#86635=CARTESIAN_POINT('Ctrl Pts',(0.422298307024632,22.6993933753954,5.25296862563014));
#86636=CARTESIAN_POINT('Ctrl Pts',(0.871097257537459,20.7458422399122,3.30154119691606));
#86637=CARTESIAN_POINT('Ctrl Pts',(1.31989620805029,19.8351832543889,0.694630776291687));
#86638=CARTESIAN_POINT('Ctrl Pts',(1.76883023510653,20.143251018862,-2.04993106067715));
#86639=CARTESIAN_POINT('Ctrl Pts',(2.06816461199185,21.1240290832044,-3.60899345932658));
#86640=CARTESIAN_POINT('Ctrl Pts',(2.21789933870621,21.759498300383,-4.24393984701044));
#86641=CARTESIAN_POINT('Ctrl Pts',(-1.31248159385698,31.3051704533329,5.30087256836657));
#86642=CARTESIAN_POINT('Ctrl Pts',(-1.16274686714261,30.5114505640989,6.09524699032489));
#86643=CARTESIAN_POINT('Ctrl Pts',(-0.863412490257304,28.5627019236485,
7.32003765309461));
#86644=CARTESIAN_POINT('Ctrl Pts',(-0.414478463201055,25.131313449161,7.70832023722244));
#86645=CARTESIAN_POINT('Ctrl Pts',(0.0343204873117733,21.8740506761476,
6.56651483020448));
#86646=CARTESIAN_POINT('Ctrl Pts',(0.4831194378246,19.431998682895,4.12711759333603));
#86647=CARTESIAN_POINT('Ctrl Pts',(0.931918388337429,18.2936222409493,0.868328676432679));
#86648=CARTESIAN_POINT('Ctrl Pts',(1.38085241539368,18.6787247778748,-2.56253247833145));
#86649=CARTESIAN_POINT('Ctrl Pts',(1.68018679227898,19.9047541269212,-4.51145071705737));
#86650=CARTESIAN_POINT('Ctrl Pts',(1.82992151899334,20.6991274301201,-5.30517045312578));
#86651=CARTESIAN_POINT('Ctrl Pts',(-1.70045941356983,32.3664010594897,6.36124343832671));
#86652=CARTESIAN_POINT('Ctrl Pts',(-1.55072468685547,31.4139077912323,7.31452217009862));
#86653=CARTESIAN_POINT('Ctrl Pts',(-1.25139030997017,29.0753372366429,8.78431633443344));
#86654=CARTESIAN_POINT('Ctrl Pts',(-0.802456282913913,24.9575439608823,
9.25026981825031));
#86655=CARTESIAN_POINT('Ctrl Pts',(-0.353657332401086,21.0487079768996,
7.88006103477882));
#86656=CARTESIAN_POINT('Ctrl Pts',(0.0951416181117414,18.1181551258777,
4.952693989756));
#86657=CARTESIAN_POINT('Ctrl Pts',(0.54394056862457,16.7520612275095,1.04202657657367));
#86658=CARTESIAN_POINT('Ctrl Pts',(0.992874595680818,17.2141985368875,-3.07513389598574));
#86659=CARTESIAN_POINT('Ctrl Pts',(1.29220897256613,18.6854791706381,-5.41390797478815));
#86660=CARTESIAN_POINT('Ctrl Pts',(1.44194369928049,19.6387565598573,-6.36640105924111));
#86661=CARTESIAN_POINT('Ctrl Pts',(-2.08843723328269,33.4276316656465,7.42161430828685));
#86662=CARTESIAN_POINT('Ctrl Pts',(-1.93870250656833,32.3163650183657,8.53379734987234));
#86663=CARTESIAN_POINT('Ctrl Pts',(-1.63936812968302,29.5879725496372,10.2485950157723));
#86664=CARTESIAN_POINT('Ctrl Pts',(-1.19043410262678,24.7837744726036,10.7922193992782));
#86665=CARTESIAN_POINT('Ctrl Pts',(-0.741635152113946,20.2233652776518,
9.19360723935315));
#86666=CARTESIAN_POINT('Ctrl Pts',(-0.292836201601118,16.8043115688604,
5.77827038617597));
#86667=CARTESIAN_POINT('Ctrl Pts',(0.15596274891171,15.2105002140697,1.21572447671466));
#86668=CARTESIAN_POINT('Ctrl Pts',(0.604896775967959,15.7496722959002,-3.58773531364002));
#86669=CARTESIAN_POINT('Ctrl Pts',(0.904231152853266,17.4662042143551,-6.31636523251894));
#86670=CARTESIAN_POINT('Ctrl Pts',(1.05396587956763,18.5783856895944,-7.42763166535646));
#86671=CARTESIAN_POINT('Ctrl Pts',(-2.08803112422502,33.4246212024587,7.42462120245876));
#86672=CARTESIAN_POINT('Ctrl Pts',(-1.95795102164571,32.4588257148303,8.39041669008711));
#86673=CARTESIAN_POINT('Ctrl Pts',(-1.82785996694436,31.3016837529055,9.1642403083045));
#86674=CARTESIAN_POINT('Ctrl Pts',(-1.54888671495528,28.599441070071,10.2935715065643));
#86675=CARTESIAN_POINT('Ctrl Pts',(-1.4179475651678,27.210440567088,10.4952142905163));
#86676=CARTESIAN_POINT('Ctrl Pts',(-1.13922861879923,24.2839070763066,10.5080470913502));
#86677=CARTESIAN_POINT('Ctrl Pts',(-1.00508812325812,22.9060536884507,10.0808264748192));
#86678=CARTESIAN_POINT('Ctrl Pts',(-0.779445153014362,20.7150047089726,
9.17859207969596));
#86679=CARTESIAN_POINT('Ctrl Pts',(-0.649074110348536,19.5549162993542,
8.40289349433808));
#86680=CARTESIAN_POINT('Ctrl Pts',(-0.385366820301348,17.5961615542775,
6.44526969447176));
#86681=CARTESIAN_POINT('Ctrl Pts',(-0.255108777477327,16.8210056428898,
5.28667067345667));
#86682=CARTESIAN_POINT('Ctrl Pts',(-0.0244870309043847,15.9001505892118,
3.04686728314339));
#86683=CARTESIAN_POINT('Ctrl Pts',(0.109012683773514,15.4945892040144,1.67135439212475));
#86684=CARTESIAN_POINT('Ctrl Pts',(0.380107909868443,15.5046185193411,-1.17517988914753));
#86685=CARTESIAN_POINT('Ctrl Pts',(0.511829062496731,15.6947443684176,-2.57456079137983));
#86686=CARTESIAN_POINT('Ctrl Pts',(0.793671459716859,16.8367708937086,-5.30408607867575));
#86687=CARTESIAN_POINT('Ctrl Pts',(0.923622163707121,17.6106282282455,-6.45987063316294));
#86688=CARTESIAN_POINT('Ctrl Pts',(1.05356152936475,18.5753787975412,-7.42462120245874));
#86689=CARTESIAN_POINT('Ctrl Pts',(-4.1955583921502,33.427627197915,7.42161396868715));
#86690=CARTESIAN_POINT('Ctrl Pts',(-4.04582375805961,32.3163612875677,8.53379564973379));
#86691=CARTESIAN_POINT('Ctrl Pts',(-3.74648947379807,29.5879667358391,10.2485891941145));
#86692=CARTESIAN_POINT('Ctrl Pts',(-3.2975555393656,24.7837749381033,10.7922206100334));
#86693=CARTESIAN_POINT('Ctrl Pts',(-2.84875658885277,20.2233709655724,9.19360350589995));
#86694=CARTESIAN_POINT('Ctrl Pts',(-2.39995763833994,16.8043163106674,5.77827433993448));
#86695=CARTESIAN_POINT('Ctrl Pts',(-1.95115868782712,15.2105131487934,1.21572940252506));
#86696=CARTESIAN_POINT('Ctrl Pts',(-1.50222475339464,15.7496782249932,-3.58772699817009));
#86697=CARTESIAN_POINT('Ctrl Pts',(-1.2028904691331,17.4662059133223,-6.31636150383227));
#86698=CARTESIAN_POINT('Ctrl Pts',(-1.05315583504251,18.5783860291971,-7.42762719762228));
#86699=CARTESIAN_POINT('Ctrl Pts',(-4.58353588364633,32.3663977841704,6.36124370087948));
#86700=CARTESIAN_POINT('Ctrl Pts',(-4.43380124955573,31.4139050646589,7.31452134946661));
#86701=CARTESIAN_POINT('Ctrl Pts',(-4.1344669652942,29.0753325211495,8.78431210906737));
#86702=CARTESIAN_POINT('Ctrl Pts',(-3.68553303086173,24.9575442691462,9.25027166108737));
#86703=CARTESIAN_POINT('Ctrl Pts',(-3.23673408034891,21.0487124212322,7.88005852056394));
#86704=CARTESIAN_POINT('Ctrl Pts',(-2.78793512983608,18.1181585042216,4.95269780966037));
#86705=CARTESIAN_POINT('Ctrl Pts',(-2.33913617932325,16.7520715093053,1.04203088929382));
#86706=CARTESIAN_POINT('Ctrl Pts',(-1.89020224489077,17.2142028542096,-3.0751270362317));
#86707=CARTESIAN_POINT('Ctrl Pts',(-1.59086796062924,18.6854799902663,-5.41390525002451));
#86708=CARTESIAN_POINT('Ctrl Pts',(-1.44113332653865,19.6387562973071,-6.36639778391949));
#86709=CARTESIAN_POINT('Ctrl Pts',(-4.97151337514246,31.3051683704258,5.30087343307181));
#86710=CARTESIAN_POINT('Ctrl Pts',(-4.82177874105187,30.5114488417502,6.09524704919943));
#86711=CARTESIAN_POINT('Ctrl Pts',(-4.52244445679034,28.56269830646,7.32003502402029));
#86712=CARTESIAN_POINT('Ctrl Pts',(-4.07351052235786,25.1313136001892,7.70832271214129));
#86713=CARTESIAN_POINT('Ctrl Pts',(-3.62471157184503,21.8740538768921,6.56651353522793));
#86714=CARTESIAN_POINT('Ctrl Pts',(-3.1759126213322,19.4320006977758,4.12712127938628));
#86715=CARTESIAN_POINT('Ctrl Pts',(-2.72711367081938,18.2936298698171,0.868332376062584));
#86716=CARTESIAN_POINT('Ctrl Pts',(-2.27817973638691,18.678727483426,-2.56252707429332));
#86717=CARTESIAN_POINT('Ctrl Pts',(-1.97884545212538,19.9047540672103,-4.51144899621676));
#86718=CARTESIAN_POINT('Ctrl Pts',(-1.82911081803478,20.699126565417,-5.30516837021671));
#86719=CARTESIAN_POINT('Ctrl Pts',(-5.3594908666386,30.2439389566812,4.24050316526413));
#86720=CARTESIAN_POINT('Ctrl Pts',(-5.209756232548,29.6089926188414,4.87597274893225));
#86721=CARTESIAN_POINT('Ctrl Pts',(-4.91042194828647,28.0500640917706,5.8557579389732));
#86722=CARTESIAN_POINT('Ctrl Pts',(-4.46148801385399,25.3050829312321,6.16637376319522));
#86723=CARTESIAN_POINT('Ctrl Pts',(-4.01268906334117,22.6993953325519,5.25296854989192));
#86724=CARTESIAN_POINT('Ctrl Pts',(-3.56389011282834,20.74584289133,3.30154474911218));
#86725=CARTESIAN_POINT('Ctrl Pts',(-3.11509116231551,19.835188230329,0.694633862831345));
#86726=CARTESIAN_POINT('Ctrl Pts',(-2.66615722788303,20.1432521126424,-2.04992711235493));
#86727=CARTESIAN_POINT('Ctrl Pts',(-2.3668229436215,21.1240281441544,-3.608992742409));
#86728=CARTESIAN_POINT('Ctrl Pts',(-2.21708830953092,21.759496833527,-4.24393895651391));
#86729=CARTESIAN_POINT('Ctrl Pts',(-4.19515344039125,33.4246212024587,7.42462120245875));
#86730=CARTESIAN_POINT('Ctrl Pts',(-4.04555379022031,32.3139004679191,8.53534193699834));
#86731=CARTESIAN_POINT('Ctrl Pts',(-3.74635448987842,29.586522227884,10.2487526513489));
#86732=CARTESIAN_POINT('Ctrl Pts',(-3.2975555393656,24.7837749381033,10.7922206100334));
#86733=CARTESIAN_POINT('Ctrl Pts',(-2.84875658885277,20.2233709655724,9.19360350589995));
#86734=CARTESIAN_POINT('Ctrl Pts',(-2.39995763833994,16.8043163106674,5.77827433993448));
#86735=CARTESIAN_POINT('Ctrl Pts',(-1.95115868782712,15.2105131487934,1.21572940252506));
#86736=CARTESIAN_POINT('Ctrl Pts',(-1.50235973731429,15.7495161106825,-3.58628271133166));
#86737=CARTESIAN_POINT('Ctrl Pts',(-1.2031604369724,17.4646580630017,-6.31390046791915));
#86738=CARTESIAN_POINT('Ctrl Pts',(-1.05356078680146,18.5753787975412,-7.42462120245874));
#86739=CARTESIAN_POINT('Ctrl Pts',(-2.08802985083253,33.4246212024587,7.42462120245875));
#86740=CARTESIAN_POINT('Ctrl Pts',(-1.93843020066159,32.3139004679191,8.53534193699834));
#86741=CARTESIAN_POINT('Ctrl Pts',(-1.6392309003197,29.586522227884,10.2487526513489));
#86742=CARTESIAN_POINT('Ctrl Pts',(-1.19043194980688,24.7837749381033,10.7922206100334));
#86743=CARTESIAN_POINT('Ctrl Pts',(-0.741632999294046,20.2233709655724,
9.19360350589995));
#86744=CARTESIAN_POINT('Ctrl Pts',(-0.292834048781219,16.8043163106674,
5.77827433993448));
#86745=CARTESIAN_POINT('Ctrl Pts',(0.155964901731608,15.2105131487934,1.21572940252506));
#86746=CARTESIAN_POINT('Ctrl Pts',(0.604763852244435,15.7495161106825,-3.58628271133166));
#86747=CARTESIAN_POINT('Ctrl Pts',(0.90396315258632,17.4646580630017,-6.31390046791915));
#86748=CARTESIAN_POINT('Ctrl Pts',(1.05356280275726,18.5753787975412,-7.42462120245874));
#86749=CARTESIAN_POINT('Ctrl Pts',(-2.79040438068543,33.4246212024587,7.42462120245875));
#86750=CARTESIAN_POINT('Ctrl Pts',(-2.64080473051449,32.3139004679191,8.53534193699834));
#86751=CARTESIAN_POINT('Ctrl Pts',(-2.34160543017261,29.586522227884,10.2487526513489));
#86752=CARTESIAN_POINT('Ctrl Pts',(-1.89280647965978,24.7837749381033,10.7922206100334));
#86753=CARTESIAN_POINT('Ctrl Pts',(-1.44400752914695,20.2233709655724,9.19360350589994));
#86754=CARTESIAN_POINT('Ctrl Pts',(-0.995208578634126,16.8043163106674,
5.77827433993448));
#86755=CARTESIAN_POINT('Ctrl Pts',(-0.5464096281213,15.2105131487934,1.21572940252506));
#86756=CARTESIAN_POINT('Ctrl Pts',(-0.0976106776084724,15.7495161106825,
-3.58628271133166));
#86757=CARTESIAN_POINT('Ctrl Pts',(0.201588622733412,17.4646580630017,-6.31390046791915));
#86758=CARTESIAN_POINT('Ctrl Pts',(0.351188272904354,18.5753787975412,-7.42462120245874));
#86759=CARTESIAN_POINT('Ctrl Pts',(-3.49277891053835,33.4246212024587,7.42462120245875));
#86760=CARTESIAN_POINT('Ctrl Pts',(-3.3431792603674,32.3139004679191,8.53534193699834));
#86761=CARTESIAN_POINT('Ctrl Pts',(-3.04397996002552,29.586522227884,10.2487526513489));
#86762=CARTESIAN_POINT('Ctrl Pts',(-2.59518100951269,24.7837749381033,10.7922206100334));
#86763=CARTESIAN_POINT('Ctrl Pts',(-2.14638205899987,20.2233709655724,9.19360350589995));
#86764=CARTESIAN_POINT('Ctrl Pts',(-1.69758310848704,16.8043163106674,5.77827433993448));
#86765=CARTESIAN_POINT('Ctrl Pts',(-1.24878415797421,15.2105131487934,1.21572940252507));
#86766=CARTESIAN_POINT('Ctrl Pts',(-0.79998520746138,15.7495161106825,-3.58628271133166));
#86767=CARTESIAN_POINT('Ctrl Pts',(-0.500785907119496,17.4646580630017,
-6.31390046791915));
#86768=CARTESIAN_POINT('Ctrl Pts',(-0.351186256948554,18.5753787975412,
-7.42462120245874));
#86769=CARTESIAN_POINT('Ctrl Pts',(-4.19515344039125,33.4246212024587,7.42462120245875));
#86770=CARTESIAN_POINT('Ctrl Pts',(-4.04555379022031,32.3139004679191,8.53534193699834));
#86771=CARTESIAN_POINT('Ctrl Pts',(-3.74635448987842,29.586522227884,10.2487526513489));
#86772=CARTESIAN_POINT('Ctrl Pts',(-3.2975555393656,24.7837749381033,10.7922206100334));
#86773=CARTESIAN_POINT('Ctrl Pts',(-2.84875658885277,20.2233709655724,9.19360350589995));
#86774=CARTESIAN_POINT('Ctrl Pts',(-2.39995763833994,16.8043163106674,5.77827433993448));
#86775=CARTESIAN_POINT('Ctrl Pts',(-1.95115868782712,15.2105131487934,1.21572940252506));
#86776=CARTESIAN_POINT('Ctrl Pts',(-1.50235973731429,15.7495161106825,-3.58628271133166));
#86777=CARTESIAN_POINT('Ctrl Pts',(-1.2031604369724,17.4646580630017,-6.31390046791915));
#86778=CARTESIAN_POINT('Ctrl Pts',(-1.05356078680146,18.5753787975412,-7.42462120245874));
#86779=CARTESIAN_POINT('Ctrl Pts',(-7.20768885204555,30.2439381858381,4.24050443502072));
#86780=CARTESIAN_POINT('Ctrl Pts',(-7.05795429813301,29.6089919988744,4.8759735623196));
#86781=CARTESIAN_POINT('Ctrl Pts',(-6.75862009404954,28.0500600640715,5.85575582850576));
#86782=CARTESIAN_POINT('Ctrl Pts',(-6.30968623979511,25.3050830975113,6.16637897680622));
#86783=CARTESIAN_POINT('Ctrl Pts',(-5.86088728928228,22.699399225175,5.2529683928905));
#86784=CARTESIAN_POINT('Ctrl Pts',(-5.41208833876945,20.7458447252201,3.30155110112974));
#86785=CARTESIAN_POINT('Ctrl Pts',(-4.96328938825663,19.8351977432586,0.694639650183325));
#86786=CARTESIAN_POINT('Ctrl Pts',(-4.51435553400221,20.14325476527,-2.04992028301914));
#86787=CARTESIAN_POINT('Ctrl Pts',(-4.21502132991872,21.1240273297457,-3.60899212489599));
#86788=CARTESIAN_POINT('Ctrl Pts',(-4.06528677600618,21.7594955637725,-4.24393818566755));
#86789=CARTESIAN_POINT('Ctrl Pts',(-7.5956663131803,31.3051672614807,5.30087487511165));
#86790=CARTESIAN_POINT('Ctrl Pts',(-7.44593175926777,30.5114479431546,6.09524789898784));
#86791=CARTESIAN_POINT('Ctrl Pts',(-7.14659755518428,28.5626932013935,7.32003218526599));
#86792=CARTESIAN_POINT('Ctrl Pts',(-6.69766370092986,25.1313138318473,7.70832901826905));
#86793=CARTESIAN_POINT('Ctrl Pts',(-6.24886475041704,21.8740588559346,6.56651315906309));
#86794=CARTESIAN_POINT('Ctrl Pts',(-5.80006579990421,19.4320031701889,4.1271291067027));
#86795=CARTESIAN_POINT('Ctrl Pts',(-5.35126684939138,18.2936419726602,0.868339586796149));
#86796=CARTESIAN_POINT('Ctrl Pts',(-4.90233299513695,18.6787309999456,-2.56251846702403));
#86797=CARTESIAN_POINT('Ctrl Pts',(-4.60299879105348,19.9047532161451,-4.51144810068888));
#86798=CARTESIAN_POINT('Ctrl Pts',(-4.45326423714094,20.6991251233798,-5.30516726126762));
#86799=CARTESIAN_POINT('Ctrl Pts',(-7.98364377431505,32.3663963371234,6.36124531520258));
#86800=CARTESIAN_POINT('Ctrl Pts',(-7.83390922040251,31.4139038874348,7.31452223565608));
#86801=CARTESIAN_POINT('Ctrl Pts',(-7.53457501631904,29.0753263387154,8.78430854202622));
#86802=CARTESIAN_POINT('Ctrl Pts',(-7.08564116206461,24.9575445661833,9.2502790597319));
#86803=CARTESIAN_POINT('Ctrl Pts',(-6.63684221155178,21.0487184866942,7.88005792523567));
#86804=CARTESIAN_POINT('Ctrl Pts',(-6.18804326103897,18.1181616151576,4.95270711227565));
#86805=CARTESIAN_POINT('Ctrl Pts',(-5.73924431052613,16.7520862020617,1.04203952340898));
#86806=CARTESIAN_POINT('Ctrl Pts',(-5.29031045627171,17.2142072346213,-3.07511665102894));
#86807=CARTESIAN_POINT('Ctrl Pts',(-4.99097625218822,18.6854791025447,-5.41390407648176));
#86808=CARTESIAN_POINT('Ctrl Pts',(-4.84124169827569,19.6387546829872,-6.36639633686769));
#86809=CARTESIAN_POINT('Ctrl Pts',(-8.37162123544981,33.4276254127661,7.42161575529352));
#86810=CARTESIAN_POINT('Ctrl Pts',(-8.22188668153727,32.3163598317151,8.53379657232431));
#86811=CARTESIAN_POINT('Ctrl Pts',(-7.92255247745379,29.5879594760374,10.2485848987865));
#86812=CARTESIAN_POINT('Ctrl Pts',(-7.47361862319936,24.7837753005193,10.7922291011947));
#86813=CARTESIAN_POINT('Ctrl Pts',(-7.02481967268654,20.2233781174538,9.19360269140826));
#86814=CARTESIAN_POINT('Ctrl Pts',(-6.57602072217371,16.8043200601264,5.7782851178486));
#86815=CARTESIAN_POINT('Ctrl Pts',(-6.12722177166088,15.2105304314633,1.2157394600218));
#86816=CARTESIAN_POINT('Ctrl Pts',(-5.67828791740646,15.749683469297,-3.58771483503384));
#86817=CARTESIAN_POINT('Ctrl Pts',(-5.37895371332298,17.4662049889442,-6.31636005227465));
#86818=CARTESIAN_POINT('Ctrl Pts',(-5.22921915941045,18.5783842425945,-7.42762541246777));
#86819=CARTESIAN_POINT('Ctrl Pts',(-8.37121652422502,33.4246212024587,7.42462120245875));
#86820=CARTESIAN_POINT('Ctrl Pts',(-8.22161687405408,32.3139004679191,8.53534193699834));
#86821=CARTESIAN_POINT('Ctrl Pts',(-8.07201676796994,30.9502068124086,9.39204424902068));
#86822=CARTESIAN_POINT('Ctrl Pts',(-7.92241722279933,29.4679036763263,9.91097645495401));
#86823=CARTESIAN_POINT('Ctrl Pts',(-7.77281767762872,27.985600540244,10.4299086608873));
#86824=CARTESIAN_POINT('Ctrl Pts',(-7.62321818610899,26.384687907658,10.6110686467821));
#86825=CARTESIAN_POINT('Ctrl Pts',(-7.47361866868718,24.8241663324414,10.43521127997));
#86826=CARTESIAN_POINT('Ctrl Pts',(-7.32401915126538,23.2636447572247,10.259353913158));
#86827=CARTESIAN_POINT('Ctrl Pts',(-7.17441957677565,21.7435129664056,9.72647916848619));
#86828=CARTESIAN_POINT('Ctrl Pts',(-7.02481986772503,20.4136040170806,8.8908221268261));
#86829=CARTESIAN_POINT('Ctrl Pts',(-6.87522015867441,19.0836950677556,8.05516508516602));
#86830=CARTESIAN_POINT('Ctrl Pts',(-6.72562077057793,17.9440089158971,6.91672732344894));
#86831=CARTESIAN_POINT('Ctrl Pts',(-6.57602101558995,17.108534919825,5.58708444540028));
#86832=CARTESIAN_POINT('Ctrl Pts',(-6.42642126060197,16.2730609237529,4.25744156735162));
#86833=CARTESIAN_POINT('Ctrl Pts',(-6.27682088159159,15.7417995729601,2.73659303696763));
#86834=CARTESIAN_POINT('Ctrl Pts',(-6.1272209307994,15.5659998279322,1.1758336557523));
#86835=CARTESIAN_POINT('Ctrl Pts',(-5.97762098000721,15.3902000829043,-0.384925725463033));
#86836=CARTESIAN_POINT('Ctrl Pts',(-5.82802150279226,15.5698619777324,-1.98559593691079));
#86837=CARTESIAN_POINT('Ctrl Pts',(-5.67842209597348,16.0884764653087,-3.46783962661608));
#86838=CARTESIAN_POINT('Ctrl Pts',(-5.52882268915469,16.6070909528849,-4.95008331632137));
#86839=CARTESIAN_POINT('Ctrl Pts',(-5.37922352080617,17.4646580630017,-6.31390046791915));
#86840=CARTESIAN_POINT('Ctrl Pts',(-5.22962387063524,18.5753787975412,-7.4246212024587));
#86841=CARTESIAN_POINT('Ctrl Pts',(-10.4787433156322,33.4276236613913,7.42161750810454));
#86842=CARTESIAN_POINT('Ctrl Pts',(-10.3290088403809,32.3163584003089,8.53379747526706));
#86843=CARTESIAN_POINT('Ctrl Pts',(-10.0296747149587,29.5879557794486,10.2485831152121));
#86844=CARTESIAN_POINT('Ctrl Pts',(-9.5807409393656,24.7837755769557,10.7922330265442));
#86845=CARTESIAN_POINT('Ctrl Pts',(-9.13194198885277,20.2233815417423,9.19360256427126));
#86846=CARTESIAN_POINT('Ctrl Pts',(-8.68314303833994,16.8043220411772,5.77829021316709));
#86847=CARTESIAN_POINT('Ctrl Pts',(-8.23434408782711,15.2105385150611,1.21574430151608));
#86848=CARTESIAN_POINT('Ctrl Pts',(-7.78541031223398,15.7496860272516,-3.58770869507484));
#86849=CARTESIAN_POINT('Ctrl Pts',(-7.4860761868118,17.4662040843916,-6.31635862294282));
#86850=CARTESIAN_POINT('Ctrl Pts',(-7.33634171156056,18.5783824897868,-7.42762366109035));
#86851=CARTESIAN_POINT('Ctrl Pts',(-10.8667207469799,32.3663949174539,6.36124689898917));
#86852=CARTESIAN_POINT('Ctrl Pts',(-10.7169862717286,31.4139027298284,7.31452310319999));
#86853=CARTESIAN_POINT('Ctrl Pts',(-10.4176521463065,29.0753232096377,8.78430712570177));
#86854=CARTESIAN_POINT('Ctrl Pts',(-9.96871837071332,24.9575447897825,9.25028254262678));
#86855=CARTESIAN_POINT('Ctrl Pts',(-9.5199194202005,21.0487213583686,7.88005791711107));
#86856=CARTESIAN_POINT('Ctrl Pts',(-9.07112046968767,18.1181632122936,4.95271154297956));
#86857=CARTESIAN_POINT('Ctrl Pts',(-8.62232151917484,16.7520930123547,1.04204368650602));
#86858=CARTESIAN_POINT('Ctrl Pts',(-8.17338774358171,17.2142093146667,-3.07511142767717));
#86859=CARTESIAN_POINT('Ctrl Pts',(-7.87405361815953,18.685478233621,-5.41390292065324));
#86860=CARTESIAN_POINT('Ctrl Pts',(-7.72431914290828,19.6387530992035,-6.36639491719599));
#86861=CARTESIAN_POINT('Ctrl Pts',(-11.2546981783276,31.3051661735166,5.30087628987379));
#86862=CARTESIAN_POINT('Ctrl Pts',(-11.1049637030764,30.5114470593478,6.0952487311329));
#86863=CARTESIAN_POINT('Ctrl Pts',(-10.8056295776542,28.5626906398269,7.32003113619143));
#86864=CARTESIAN_POINT('Ctrl Pts',(-10.3566958020611,25.1313140026092,7.70833205870936));
#86865=CARTESIAN_POINT('Ctrl Pts',(-9.90789685154823,21.874061174995,6.5665132699509));
#86866=CARTESIAN_POINT('Ctrl Pts',(-9.4590979010354,19.43200438341,4.12713287279204));
#86867=CARTESIAN_POINT('Ctrl Pts',(-9.01029895052258,18.2936475096483,0.868343071495974));
#86868=CARTESIAN_POINT('Ctrl Pts',(-8.56136517492943,18.6787326020819,-2.56251416027952));
#86869=CARTESIAN_POINT('Ctrl Pts',(-8.26203104950726,19.9047523828503,-4.51144721836367));
#86870=CARTESIAN_POINT('Ctrl Pts',(-8.11229657425601,20.6991237086201,-5.30516617330163));
#86871=CARTESIAN_POINT('Ctrl Pts',(-11.6426756096754,30.2439374295793,4.2405056807584));
#86872=CARTESIAN_POINT('Ctrl Pts',(-11.4929411344241,29.6089913888673,4.87597435906582));
#86873=CARTESIAN_POINT('Ctrl Pts',(-11.1936070090019,28.050058070016,5.85575514668108));
#86874=CARTESIAN_POINT('Ctrl Pts',(-10.7446732334088,25.3050832154359,6.16638157479195));
#86875=CARTESIAN_POINT('Ctrl Pts',(-10.295874282896,22.6994009916213,5.25296862279071));
#86876=CARTESIAN_POINT('Ctrl Pts',(-9.84707533238312,20.7458455545263,3.30155420260451));
#86877=CARTESIAN_POINT('Ctrl Pts',(-9.3982763818703,19.835202006942,0.694642456485917));
#86878=CARTESIAN_POINT('Ctrl Pts',(-8.94934260627717,20.143255889497,-2.04991689288185));
#86879=CARTESIAN_POINT('Ctrl Pts',(-8.65000848085499,21.1240265320798,-3.6089915160741));
#86880=CARTESIAN_POINT('Ctrl Pts',(-8.50027400560374,21.7594943180368,-4.24393742940726));
#86881=CARTESIAN_POINT('Ctrl Pts',(-10.4783388403913,33.4246212024587,7.42462120245875));
#86882=CARTESIAN_POINT('Ctrl Pts',(-10.3287391902203,32.3139004679191,8.53534193699834));
#86883=CARTESIAN_POINT('Ctrl Pts',(-10.0295398898784,29.5865129742582,10.2487463857142));
#86884=CARTESIAN_POINT('Ctrl Pts',(-9.58074093936559,24.7837755769557,10.7922330265442));
#86885=CARTESIAN_POINT('Ctrl Pts',(-9.13194198885277,20.2233815417423,9.19360256427126));
#86886=CARTESIAN_POINT('Ctrl Pts',(-8.68314303833994,16.8043220411772,5.77829021316709));
#86887=CARTESIAN_POINT('Ctrl Pts',(-8.23434408782711,15.2105385150611,1.21574430151608));
#86888=CARTESIAN_POINT('Ctrl Pts',(-7.78554513731429,15.7495241089229,-3.58626610828099));
#86889=CARTESIAN_POINT('Ctrl Pts',(-7.4863458369724,17.4646580630017,-6.31390046791915));
#86890=CARTESIAN_POINT('Ctrl Pts',(-7.33674618680146,18.5753787975412,-7.42462120245874));
#86891=CARTESIAN_POINT('Ctrl Pts',(-8.37121652422502,33.4246212024587,7.42462120245875));
#86892=CARTESIAN_POINT('Ctrl Pts',(-8.22161687405408,32.3139004679191,8.53534193699834));
#86893=CARTESIAN_POINT('Ctrl Pts',(-7.92241757371219,29.5865129742582,10.2487463857142));
#86894=CARTESIAN_POINT('Ctrl Pts',(-7.47361862319936,24.7837755769557,10.7922330265442));
#86895=CARTESIAN_POINT('Ctrl Pts',(-7.02481967268654,20.2233815417423,9.19360256427126));
#86896=CARTESIAN_POINT('Ctrl Pts',(-6.57602072217371,16.8043220411772,5.77829021316709));
#86897=CARTESIAN_POINT('Ctrl Pts',(-6.12722177166088,15.2105385150611,1.21574430151608));
#86898=CARTESIAN_POINT('Ctrl Pts',(-5.67842282114805,15.7495241089229,-3.58626610828099));
#86899=CARTESIAN_POINT('Ctrl Pts',(-5.37922352080617,17.4646580630017,-6.31390046791915));
#86900=CARTESIAN_POINT('Ctrl Pts',(-5.22962387063522,18.5753787975412,-7.42462120245874));
#86901=CARTESIAN_POINT('Ctrl Pts',(-9.07359062961376,33.4246212024587,7.42462120245875));
#86902=CARTESIAN_POINT('Ctrl Pts',(-8.92399097944282,32.3139004679191,8.53534193699834));
#86903=CARTESIAN_POINT('Ctrl Pts',(-8.62479167910094,29.5865129742582,10.2487463857142));
#86904=CARTESIAN_POINT('Ctrl Pts',(-8.17599272858811,24.7837755769557,10.7922330265442));
#86905=CARTESIAN_POINT('Ctrl Pts',(-7.72719377807528,20.2233815417423,9.19360256427126));
#86906=CARTESIAN_POINT('Ctrl Pts',(-7.27839482756245,16.8043220411772,5.77829021316709));
#86907=CARTESIAN_POINT('Ctrl Pts',(-6.82959587704963,15.2105385150611,1.21574430151608));
#86908=CARTESIAN_POINT('Ctrl Pts',(-6.3807969265368,15.7495241089229,-3.586266108281));
#86909=CARTESIAN_POINT('Ctrl Pts',(-6.08159762619491,17.4646580630017,-6.31390046791915));
#86910=CARTESIAN_POINT('Ctrl Pts',(-5.93199797602397,18.5753787975412,-7.42462120245874));
#86911=CARTESIAN_POINT('Ctrl Pts',(-9.77596473500251,33.4246212024587,7.42462120245875));
#86912=CARTESIAN_POINT('Ctrl Pts',(-9.62636508483157,32.3139004679191,8.53534193699834));
#86913=CARTESIAN_POINT('Ctrl Pts',(-9.32716578448968,29.5865129742582,10.2487463857142));
#86914=CARTESIAN_POINT('Ctrl Pts',(-8.87836683397685,24.7837755769557,10.7922330265442));
#86915=CARTESIAN_POINT('Ctrl Pts',(-8.42956788346403,20.2233815417423,9.19360256427127));
#86916=CARTESIAN_POINT('Ctrl Pts',(-7.98076893295119,16.8043220411772,5.77829021316709));
#86917=CARTESIAN_POINT('Ctrl Pts',(-7.53196998243837,15.2105385150611,1.21574430151608));
#86918=CARTESIAN_POINT('Ctrl Pts',(-7.08317103192554,15.7495241089229,-3.586266108281));
#86919=CARTESIAN_POINT('Ctrl Pts',(-6.78397173158366,17.4646580630017,-6.31390046791915));
#86920=CARTESIAN_POINT('Ctrl Pts',(-6.63437208141271,18.5753787975412,-7.42462120245874));
#86921=CARTESIAN_POINT('Ctrl Pts',(-10.4783388403913,33.4246212024587,7.42462120245875));
#86922=CARTESIAN_POINT('Ctrl Pts',(-10.3287391902203,32.3139004679191,8.53534193699834));
#86923=CARTESIAN_POINT('Ctrl Pts',(-10.0295398898784,29.5865129742582,10.2487463857142));
#86924=CARTESIAN_POINT('Ctrl Pts',(-9.58074093936559,24.7837755769557,10.7922330265442));
#86925=CARTESIAN_POINT('Ctrl Pts',(-9.13194198885277,20.2233815417423,9.19360256427126));
#86926=CARTESIAN_POINT('Ctrl Pts',(-8.68314303833994,16.8043220411772,5.77829021316709));
#86927=CARTESIAN_POINT('Ctrl Pts',(-8.23434408782711,15.2105385150611,1.21574430151608));
#86928=CARTESIAN_POINT('Ctrl Pts',(-7.78554513731429,15.7495241089229,-3.58626610828099));
#86929=CARTESIAN_POINT('Ctrl Pts',(-7.4863458369724,17.4646580630017,-6.31390046791915));
#86930=CARTESIAN_POINT('Ctrl Pts',(-7.33674618680146,18.5753787975412,-7.42462120245874));
#86931=CARTESIAN_POINT('Ctrl Pts',(-13.4908740109291,30.2439369421926,4.24050648359456));
#86932=CARTESIAN_POINT('Ctrl Pts',(-13.3411395863725,29.608990997377,4.87597487355288));
#86933=CARTESIAN_POINT('Ctrl Pts',(-13.041805511645,28.0500549640659,5.8557535852361));
#86934=CARTESIAN_POINT('Ctrl Pts',(-12.5928717867465,25.3050835881141,6.16638591073518));
#86935=CARTESIAN_POINT('Ctrl Pts',(-12.1440728362336,22.6994045647989,5.25296892729081));
#86936=CARTESIAN_POINT('Ctrl Pts',(-11.6952738857208,20.7458476630348,3.30155975703115));
#86937=CARTESIAN_POINT('Ctrl Pts',(-11.246474935208,19.8352103074259,0.694647717400992));
#86938=CARTESIAN_POINT('Ctrl Pts',(-10.7975412103096,20.1432585780077,-2.04991105844832));
#86939=CARTESIAN_POINT('Ctrl Pts',(-10.498207135582,21.1240260162405,-3.60899112699502));
#86940=CARTESIAN_POINT('Ctrl Pts',(-10.3484727110254,21.7594935152029,-4.24393694201739));
#86941=CARTESIAN_POINT('Ctrl Pts',(-13.8788514230801,31.305165472356,5.30087720164032));
#86942=CARTESIAN_POINT('Ctrl Pts',(-13.7291169985234,30.5114464918125,6.09524926868588));
#86943=CARTESIAN_POINT('Ctrl Pts',(-13.4297829237959,28.5626867128182,7.32002905749346));
#86944=CARTESIAN_POINT('Ctrl Pts',(-12.9808491988975,25.1313144835263,7.70833734535978));
#86945=CARTESIAN_POINT('Ctrl Pts',(-12.5320502483847,21.8740657131446,6.56651353684457));
#86946=CARTESIAN_POINT('Ctrl Pts',(-12.0832512978718,19.4320071329416,4.12713974465246));
#86947=CARTESIAN_POINT('Ctrl Pts',(-11.634452347359,18.2936580192251,0.868349632900707));
#86948=CARTESIAN_POINT('Ctrl Pts',(-11.1855186224605,18.6787360896981,-2.56250682251239));
#86949=CARTESIAN_POINT('Ctrl Pts',(-10.886184547733,19.904751843607,-4.5114466538425));
#86950=CARTESIAN_POINT('Ctrl Pts',(-10.7364501231764,20.6991227968565,-5.30516547213704));
#86951=CARTESIAN_POINT('Ctrl Pts',(-14.266828835231,32.3663940025195,6.36124791968608));
#86952=CARTESIAN_POINT('Ctrl Pts',(-14.1170944106744,31.413901986248,7.3145236638189));
#86953=CARTESIAN_POINT('Ctrl Pts',(-13.8177603359469,29.0753184615703,8.78430452975083));
#86954=CARTESIAN_POINT('Ctrl Pts',(-13.3688266110484,24.9575453789385,9.25028877998437));
#86955=CARTESIAN_POINT('Ctrl Pts',(-12.9200276605356,21.0487268614902,7.88005814639835));
#86956=CARTESIAN_POINT('Ctrl Pts',(-12.4712287100228,18.1181666028484,4.95271973227379));
#86957=CARTESIAN_POINT('Ctrl Pts',(-12.0224297595099,16.7521057310242,1.04205154840042));
#86958=CARTESIAN_POINT('Ctrl Pts',(-11.5734960346114,17.2142136013887,-3.07510258657646));
#86959=CARTESIAN_POINT('Ctrl Pts',(-11.2741619598839,18.6854776709736,-5.41390218068998));
#86960=CARTESIAN_POINT('Ctrl Pts',(-11.1244275353273,19.63875207851,-6.36639400225669));
#86961=CARTESIAN_POINT('Ctrl Pts',(-14.6548062473819,33.4276225326829,7.42161863773185));
#86962=CARTESIAN_POINT('Ctrl Pts',(-14.5050718228254,32.3163574806835,8.5337980589519));
#86963=CARTESIAN_POINT('Ctrl Pts',(-14.2057377480978,29.5879502103225,10.2485800020082));
#86964=CARTESIAN_POINT('Ctrl Pts',(-13.7568040231994,24.7837762743506,10.792240214609));
#86965=CARTESIAN_POINT('Ctrl Pts',(-13.3080050726865,20.2233880098358,9.19360275595211));
#86966=CARTESIAN_POINT('Ctrl Pts',(-12.8592061221737,16.8043260727552,5.7782997198951));
#86967=CARTESIAN_POINT('Ctrl Pts',(-12.4104071716609,15.2105534428233,1.21575346390014));
#86968=CARTESIAN_POINT('Ctrl Pts',(-11.9614734467625,15.7496911130792,-3.58769835064053));
#86969=CARTESIAN_POINT('Ctrl Pts',(-11.6621393720349,17.4662034983402,-6.31635770753746));
#86970=CARTESIAN_POINT('Ctrl Pts',(-11.5124049474783,18.5783813601636,-7.42762253237636));
#86971=CARTESIAN_POINT('Ctrl Pts',(-14.654401924225,33.4246212024587,7.42462120245875));
#86972=CARTESIAN_POINT('Ctrl Pts',(-14.5048022740541,32.3139004679191,8.53534193699834));
#86973=CARTESIAN_POINT('Ctrl Pts',(-14.3552022737683,30.950203150656,9.39204196234938));
#86974=CARTESIAN_POINT('Ctrl Pts',(-14.2056027244668,29.467899597397,9.91097554778974));
#86975=CARTESIAN_POINT('Ctrl Pts',(-14.0560031751652,27.9855960441379,10.4299091332301));
#86976=CARTESIAN_POINT('Ctrl Pts',(-13.9064036151766,26.3846862358993,10.6110743887871));
#86977=CARTESIAN_POINT('Ctrl Pts',(-13.7568040801578,24.8241674369159,10.4352178717254));
#86978=CARTESIAN_POINT('Ctrl Pts',(-13.6072045451391,23.2636486379325,10.2593613546637));
#86979=CARTESIAN_POINT('Ctrl Pts',(-13.4576049659318,21.7435197923166,9.72648287486196));
#86980=CARTESIAN_POINT('Ctrl Pts',(-13.308005280278,20.4136116476536,8.89082647512689));
#86981=CARTESIAN_POINT('Ctrl Pts',(-13.1584055946242,19.0837035029906,8.05517007539182));
#86982=CARTESIAN_POINT('Ctrl Pts',(-13.0088061501224,17.944016056696,6.91673693379781));
#86983=CARTESIAN_POINT('Ctrl Pts',(-12.8592063826122,17.1085441761431,5.58709619172128));
#86984=CARTESIAN_POINT('Ctrl Pts',(-12.7096066151021,16.2730722955903,4.25745544964474));
#86985=CARTESIAN_POINT('Ctrl Pts',(-12.5600063513476,15.7418162640707,2.73660675503515));
#86986=CARTESIAN_POINT('Ctrl Pts',(-12.4104064355152,15.5660167942965,1.17584743948898));
#86987=CARTESIAN_POINT('Ctrl Pts',(-12.2608065196829,15.3902173245223,-0.384911876057196));
#86988=CARTESIAN_POINT('Ctrl Pts',(-12.1112069917185,15.5698744476954,-1.98558179310599));
#86989=CARTESIAN_POINT('Ctrl Pts',(-11.961607556327,16.0884846261068,-3.46782894584021));
#86990=CARTESIAN_POINT('Ctrl Pts',(-11.8120081209356,16.6070948045182,-4.95007609857443));
#86991=CARTESIAN_POINT('Ctrl Pts',(-11.6624089208062,17.4646580630017,-6.31390046791915));
#86992=CARTESIAN_POINT('Ctrl Pts',(-11.5128092706352,18.5753787975412,-7.4246212024587));
#86993=CARTESIAN_POINT('Ctrl Pts',(-16.7615242403913,33.4246212024587,7.42462120245875));
#86994=CARTESIAN_POINT('Ctrl Pts',(-16.6119245902203,32.3139004679191,8.53534193699834));
#86995=CARTESIAN_POINT('Ctrl Pts',(-16.3127252898784,29.5865056944476,10.2487418519882));
#86996=CARTESIAN_POINT('Ctrl Pts',(-15.8639263393656,24.7837766896879,10.7922435813033));
#86997=CARTESIAN_POINT('Ctrl Pts',(-15.4151273888528,20.2233911279431,9.19360303844964));
#86998=CARTESIAN_POINT('Ctrl Pts',(-14.9663284383399,16.8043281386818,5.77830424745898));
#86999=CARTESIAN_POINT('Ctrl Pts',(-14.5175294878271,15.2105604801153,1.2157578802817));
#87000=CARTESIAN_POINT('Ctrl Pts',(-14.0686160154007,15.7496693261982,-3.58747702651184));
#87001=CARTESIAN_POINT('Ctrl Pts',(-13.7693021931453,17.4659712295614,-6.31598847532156));
#87002=CARTESIAN_POINT('Ctrl Pts',(-13.6195880210608,18.5779300880552,-7.42717160290573));
#87003=CARTESIAN_POINT('Ctrl Pts',(-17.1494939834484,32.3638424588395,6.3638424588395));
#87004=CARTESIAN_POINT('Ctrl Pts',(-16.9998943332774,31.4118138532541,7.31587106442488));
#87005=CARTESIAN_POINT('Ctrl Pts',(-16.7006950329356,29.0740904612934,8.78447219984358));
#87006=CARTESIAN_POINT('Ctrl Pts',(-16.2518960824227,24.9575423000662,9.25032214520139));
#87007=CARTESIAN_POINT('Ctrl Pts',(-15.8030971319099,21.0487132197491,7.88008435318242));
#87008=CARTESIAN_POINT('Ctrl Pts',(-15.3542981813971,18.1181424031123,4.9527399320917));
#87009=CARTESIAN_POINT('Ctrl Pts',(-14.9054992308842,16.7520812912335,1.04205876734065));
#87010=CARTESIAN_POINT('Ctrl Pts',(-14.4565857584578,17.2141659782612,-3.07492301612194));
#87011=CARTESIAN_POINT('Ctrl Pts',(-14.1572719362024,18.6852544859406,-5.41360354053909));
#87012=CARTESIAN_POINT('Ctrl Pts',(-14.0075577641179,19.6383443208567,-6.36602847563537));
#87013=CARTESIAN_POINT('Ctrl Pts',(-17.5374637265055,31.3030637152202,5.30306371522026));
#87014=CARTESIAN_POINT('Ctrl Pts',(-17.3878640763346,30.5097272385891,6.09640019185142));
#87015=CARTESIAN_POINT('Ctrl Pts',(-17.0886647759927,28.5616752281392,7.32020254769893));
#87016=CARTESIAN_POINT('Ctrl Pts',(-16.6398658254799,25.1313079104446,7.70840070909949));
#87017=CARTESIAN_POINT('Ctrl Pts',(-16.191066874967,21.8740353115551,6.5665656679152));
#87018=CARTESIAN_POINT('Ctrl Pts',(-15.7422679244542,19.431956667543,4.1271756167244));
#87019=CARTESIAN_POINT('Ctrl Pts',(-15.2934689739414,18.2936021023516,0.868359654399596));
#87020=CARTESIAN_POINT('Ctrl Pts',(-14.844555501515,18.6786626303243,-2.56236900573204));
#87021=CARTESIAN_POINT('Ctrl Pts',(-14.5452416792596,19.9045377423199,-4.51121860575662));
#87022=CARTESIAN_POINT('Ctrl Pts',(-14.395527507175,20.6987585536582,-5.30488534836501));
#87023=CARTESIAN_POINT('Ctrl Pts',(-17.9254334695626,30.242284971601,4.242284971601));
#87024=CARTESIAN_POINT('Ctrl Pts',(-17.7758338193916,29.607640623924,4.87692931927796));
#87025=CARTESIAN_POINT('Ctrl Pts',(-17.4766345190497,28.049259994985,5.85593289555428));
#87026=CARTESIAN_POINT('Ctrl Pts',(-17.0278355685369,25.3050735208229,6.1664792729976));
#87027=CARTESIAN_POINT('Ctrl Pts',(-16.5790366180241,22.699357403361,5.25304698264799));
#87028=CARTESIAN_POINT('Ctrl Pts',(-16.1302376675113,20.7457709319735,3.30161130135711));
#87029=CARTESIAN_POINT('Ctrl Pts',(-15.6814387169984,19.8351229134697,0.694660541458542));
#87030=CARTESIAN_POINT('Ctrl Pts',(-15.2325252445721,20.1431592823874,-2.04981499534212));
#87031=CARTESIAN_POINT('Ctrl Pts',(-14.9332114223166,21.1238209986992,-3.60883367097415));
#87032=CARTESIAN_POINT('Ctrl Pts',(-14.7834972502322,21.7591727864597,-4.24374222109464));
#87033=CARTESIAN_POINT('Ctrl Pts',(-16.7615242403913,33.4246212024587,7.42462120245875));
#87034=CARTESIAN_POINT('Ctrl Pts',(-16.6119245902203,32.3139004679191,8.53534193699834));
#87035=CARTESIAN_POINT('Ctrl Pts',(-16.3127252898784,29.5865056944476,10.2487418519882));
#87036=CARTESIAN_POINT('Ctrl Pts',(-15.8639263393656,24.7837766896879,10.7922435813033));
#87037=CARTESIAN_POINT('Ctrl Pts',(-15.4151273888528,20.2233911279431,9.19360303844964));
#87038=CARTESIAN_POINT('Ctrl Pts',(-14.9663284383399,16.8043281386818,5.77830424745898));
#87039=CARTESIAN_POINT('Ctrl Pts',(-14.5175294878271,15.2105604801153,1.2157578802817));
#87040=CARTESIAN_POINT('Ctrl Pts',(-14.0687305373143,15.7495317946237,-3.58625167756031));
#87041=CARTESIAN_POINT('Ctrl Pts',(-13.7695312369724,17.4646580630017,-6.31390046791915));
#87042=CARTESIAN_POINT('Ctrl Pts',(-13.6199315868015,18.5753787975412,-7.42462120245874));
#87043=CARTESIAN_POINT('Ctrl Pts',(-14.654401924225,33.4246212024587,7.42462120245875));
#87044=CARTESIAN_POINT('Ctrl Pts',(-14.5048022740541,32.3139004679191,8.53534193699834));
#87045=CARTESIAN_POINT('Ctrl Pts',(-14.2056029737122,29.5865056944476,10.2487418519882));
#87046=CARTESIAN_POINT('Ctrl Pts',(-13.7568040231994,24.7837766896879,10.7922435813033));
#87047=CARTESIAN_POINT('Ctrl Pts',(-13.3080050726865,20.2233911279431,9.19360303844964));
#87048=CARTESIAN_POINT('Ctrl Pts',(-12.8592061221737,16.8043281386818,5.77830424745898));
#87049=CARTESIAN_POINT('Ctrl Pts',(-12.4104071716609,15.2105604801153,1.2157578802817));
#87050=CARTESIAN_POINT('Ctrl Pts',(-11.9616082211481,15.7495317946237,-3.58625167756031));
#87051=CARTESIAN_POINT('Ctrl Pts',(-11.6624089208062,17.4646580630017,-6.31390046791915));
#87052=CARTESIAN_POINT('Ctrl Pts',(-11.5128092706352,18.5753787975412,-7.42462120245874));
#87053=CARTESIAN_POINT('Ctrl Pts',(-15.3567760296138,33.4246212024587,7.42462120245875));
#87054=CARTESIAN_POINT('Ctrl Pts',(-15.2071763794428,32.3139004679191,8.53534193699834));
#87055=CARTESIAN_POINT('Ctrl Pts',(-14.9079770791009,29.5865056944476,10.2487418519882));
#87056=CARTESIAN_POINT('Ctrl Pts',(-14.4591781285881,24.7837766896879,10.7922435813033));
#87057=CARTESIAN_POINT('Ctrl Pts',(-14.0103791780753,20.2233911279431,9.19360303844963));
#87058=CARTESIAN_POINT('Ctrl Pts',(-13.5615802275625,16.8043281386818,5.77830424745898));
#87059=CARTESIAN_POINT('Ctrl Pts',(-13.1127812770496,15.2105604801153,1.2157578802817));
#87060=CARTESIAN_POINT('Ctrl Pts',(-12.6639823265368,15.7495317946237,-3.58625167756031));
#87061=CARTESIAN_POINT('Ctrl Pts',(-12.3647830261949,17.4646580630017,-6.31390046791915));
#87062=CARTESIAN_POINT('Ctrl Pts',(-12.215183376024,18.5753787975412,-7.42462120245874));
#87063=CARTESIAN_POINT('Ctrl Pts',(-16.0591501350025,33.4246212024587,7.42462120245875));
#87064=CARTESIAN_POINT('Ctrl Pts',(-15.9095504848316,32.3139004679191,8.53534193699834));
#87065=CARTESIAN_POINT('Ctrl Pts',(-15.6103511844897,29.5865056944476,10.2487418519882));
#87066=CARTESIAN_POINT('Ctrl Pts',(-15.1615522339768,24.7837766896879,10.7922435813033));
#87067=CARTESIAN_POINT('Ctrl Pts',(-14.712753283464,20.2233911279431,9.19360303844964));
#87068=CARTESIAN_POINT('Ctrl Pts',(-14.2639543329512,16.8043281386818,5.77830424745898));
#87069=CARTESIAN_POINT('Ctrl Pts',(-13.8151553824384,15.2105604801153,1.2157578802817));
#87070=CARTESIAN_POINT('Ctrl Pts',(-13.3663564319255,15.7495317946237,-3.58625167756031));
#87071=CARTESIAN_POINT('Ctrl Pts',(-13.0671571315837,17.4646580630017,-6.31390046791915));
#87072=CARTESIAN_POINT('Ctrl Pts',(-12.9175574814127,18.5753787975412,-7.42462120245874));
#87073=CARTESIAN_POINT('Ctrl Pts',(-16.7615242403913,33.4246212024587,7.42462120245875));
#87074=CARTESIAN_POINT('Ctrl Pts',(-16.6119245902203,32.3139004679191,8.53534193699834));
#87075=CARTESIAN_POINT('Ctrl Pts',(-16.3127252898784,29.5865056944476,10.2487418519882));
#87076=CARTESIAN_POINT('Ctrl Pts',(-15.8639263393656,24.7837766896879,10.7922435813033));
#87077=CARTESIAN_POINT('Ctrl Pts',(-15.4151273888528,20.2233911279431,9.19360303844964));
#87078=CARTESIAN_POINT('Ctrl Pts',(-14.9663284383399,16.8043281386818,5.77830424745898));
#87079=CARTESIAN_POINT('Ctrl Pts',(-14.5175294878271,15.2105604801153,1.2157578802817));
#87080=CARTESIAN_POINT('Ctrl Pts',(-14.0687305373143,15.7495317946237,-3.58625167756031));
#87081=CARTESIAN_POINT('Ctrl Pts',(-13.7695312369724,17.4646580630017,-6.31390046791915));
#87082=CARTESIAN_POINT('Ctrl Pts',(-13.6199315868015,18.5753787975412,-7.42462120245874));
#87083=CARTESIAN_POINT('Origin',(-36.6591285358979,26.,7.7715611723761E-15));
#87084=CARTESIAN_POINT('',(0.,0.,0.));
#87085=CARTESIAN_POINT('Origin',(0.,0.,29.5000004769));
#87086=CARTESIAN_POINT('',(-22.5,-2.75545529808155E-15,30.0000004769));
#87087=CARTESIAN_POINT('Origin',(0.,0.,30.0000004769));
#87088=CARTESIAN_POINT('',(-23.,-2.81668763803891E-15,29.5000004769));
#87089=CARTESIAN_POINT('Origin',(-22.5,-2.75545529808154E-15,29.5000004769));
#87090=CARTESIAN_POINT('',(23.,2.81668763803891E-15,29.5000004769));
#87091=CARTESIAN_POINT('Origin',(0.,0.,29.5000004769));
#87092=CARTESIAN_POINT('Origin',(0.,0.,29.5000004769));
#87093=CARTESIAN_POINT('Origin',(0.,0.,27.0000004769));
#87094=CARTESIAN_POINT('',(23.,2.81668763803891E-15,27.0000004769));
#87095=CARTESIAN_POINT('',(23.,2.81668763803891E-15,27.0000004769));
#87096=CARTESIAN_POINT('Origin',(0.,0.,27.0000004769));
#87097=CARTESIAN_POINT('Origin',(0.,0.,30.0000004769));
#87098=CARTESIAN_POINT('',(-20.3644359551636,4.86632242102517E-15,30.0000004769));
#87099=CARTESIAN_POINT('Origin',(-21.3644359551636,4.74385774111043E-15,
30.0000004769));
#87100=CARTESIAN_POINT('',(1.,21.3644359551636,30.0000004769));
#87101=CARTESIAN_POINT('Origin',(2.61638881080797E-15,21.3644359551636,
30.0000004769));
#87102=CARTESIAN_POINT('',(1.,-21.3644359551636,30.0000004769));
#87103=CARTESIAN_POINT('Origin',(0.,-21.3644359551636,30.0000004769));
#87104=CARTESIAN_POINT('',(22.3644359551636,4.86632242102517E-15,30.0000004769));
#87105=CARTESIAN_POINT('Origin',(21.3644359551636,4.74385774111043E-15,
30.0000004769));
#87106=CARTESIAN_POINT('',(10.,1.22464679914735E-15,30.0000004769));
#87107=CARTESIAN_POINT('Origin',(0.,0.,30.0000004769));
#87108=CARTESIAN_POINT('Origin',(-21.3644359551636,4.74385774111043E-15,
30.0000004769));
#87109=CARTESIAN_POINT('',(-20.3644359551636,4.86632242102517E-15,27.0000004769));
#87110=CARTESIAN_POINT('',(-20.3644359551636,4.62139306119569E-15,30.0000004769));
#87111=CARTESIAN_POINT('Origin',(-21.3644359551636,4.74385774111043E-15,
27.0000004769));
#87112=CARTESIAN_POINT('Origin',(2.61638881080797E-15,21.3644359551636,
30.0000004769));
#87113=CARTESIAN_POINT('',(1.,21.3644359551636,27.0000004769));
#87114=CARTESIAN_POINT('',(1.,21.3644359551636,30.0000004769));
#87115=CARTESIAN_POINT('Origin',(2.61638881080797E-15,21.3644359551636,
27.0000004769));
#87116=CARTESIAN_POINT('Origin',(0.,-21.3644359551636,30.0000004769));
#87117=CARTESIAN_POINT('',(1.,-21.3644359551636,27.0000004769));
#87118=CARTESIAN_POINT('',(1.,-21.3644359551636,30.0000004769));
#87119=CARTESIAN_POINT('Origin',(0.,-21.3644359551636,27.0000004769));
#87120=CARTESIAN_POINT('Origin',(21.3644359551636,4.74385774111043E-15,
30.0000004769));
#87121=CARTESIAN_POINT('',(22.3644359551636,4.86632242102517E-15,27.0000004769));
#87122=CARTESIAN_POINT('',(22.3644359551636,4.62139306119569E-15,30.0000004769));
#87123=CARTESIAN_POINT('Origin',(21.3644359551636,4.74385774111043E-15,
27.0000004769));
#87124=CARTESIAN_POINT('Origin',(0.,0.,27.0000004769));
#87125=CARTESIAN_POINT('',(10.,1.22464679914735E-15,27.0000004769));
#87126=CARTESIAN_POINT('Origin',(0.,0.,27.0000004769));
#87127=CARTESIAN_POINT('',(10.,1.22464679914735E-15,27.0000004769));
#87128=CARTESIAN_POINT('Origin',(0.,0.,27.0000004769));
#87129=CARTESIAN_POINT('',(0.,0.,0.));
#87130=CARTESIAN_POINT('Origin',(-21.3644359551636,4.74385774111043E-15,
30.0000004769));
#87131=CARTESIAN_POINT('',(-20.3644359551636,4.62139306119569E-15,27.0000004769));
#87132=CARTESIAN_POINT('Origin',(-21.3644359551636,4.74385774111043E-15,
27.0000004769));
#87133=CARTESIAN_POINT('',(-20.3644359551636,4.86632242102517E-15,22.0000004769));
#87134=CARTESIAN_POINT('',(-20.3644359551636,4.62139306119569E-15,30.0000004769));
#87135=CARTESIAN_POINT('Origin',(-21.3644359551636,4.74385774111043E-15,
22.0000004769));
#87136=CARTESIAN_POINT('Origin',(-21.3644359551636,4.71844785465692E-15,
22.0000004769));
#87137=CARTESIAN_POINT('Origin',(2.61638881080797E-15,21.3644359551636,
30.0000004769));
#87138=CARTESIAN_POINT('',(1.,21.3644359551636,27.0000004769));
#87139=CARTESIAN_POINT('Origin',(2.61638881080797E-15,21.3644359551636,
27.0000004769));
#87140=CARTESIAN_POINT('',(1.,21.3644359551636,22.0000004769));
#87141=CARTESIAN_POINT('',(1.,21.3644359551636,30.0000004769));
#87142=CARTESIAN_POINT('Origin',(2.61638881080797E-15,21.3644359551636,
22.0000004769));
#87143=CARTESIAN_POINT('Origin',(2.63677968348475E-15,21.3644359551636,
22.0000004769));
#87144=CARTESIAN_POINT('Origin',(0.,-21.3644359551636,30.0000004769));
#87145=CARTESIAN_POINT('',(1.,-21.3644359551636,27.0000004769));
#87146=CARTESIAN_POINT('Origin',(0.,-21.3644359551636,27.0000004769));
#87147=CARTESIAN_POINT('',(1.,-21.3644359551636,22.0000004769));
#87148=CARTESIAN_POINT('',(1.,-21.3644359551636,30.0000004769));
#87149=CARTESIAN_POINT('Origin',(0.,-21.3644359551636,22.0000004769));
#87150=CARTESIAN_POINT('Origin',(0.,-21.3644359551636,22.0000004769));
#87151=CARTESIAN_POINT('Origin',(21.3644359551636,4.74385774111043E-15,
30.0000004769));
#87152=CARTESIAN_POINT('',(22.3644359551636,4.62139306119569E-15,27.0000004769));
#87153=CARTESIAN_POINT('Origin',(21.3644359551636,4.74385774111043E-15,
27.0000004769));
#87154=CARTESIAN_POINT('',(22.3644359551636,4.86632242102517E-15,22.0000004769));
#87155=CARTESIAN_POINT('',(22.3644359551636,4.62139306119569E-15,30.0000004769));
#87156=CARTESIAN_POINT('Origin',(21.3644359551636,4.74385774111043E-15,
22.0000004769));
#87157=CARTESIAN_POINT('Origin',(21.3644359551636,4.71844785465692E-15,
22.0000004769));
#87158=CARTESIAN_POINT('Origin',(0.,0.,-27.));
#87159=CARTESIAN_POINT('',(8.5,1.04094977927525E-15,-27.));
#87160=CARTESIAN_POINT('Origin',(0.,0.,-27.));
#87161=CARTESIAN_POINT('',(8.5,1.04094977927525E-15,-28.));
#87162=CARTESIAN_POINT('',(8.5,-1.04094977927525E-15,-27.));
#87163=CARTESIAN_POINT('Origin',(0.,0.,-28.));
#87164=CARTESIAN_POINT('Origin',(26.3408711739,15.6090782051017,5.99920149541289));
#87165=CARTESIAN_POINT('',(23.3408711739,14.6090782051017,5.99920149541289));
#87166=CARTESIAN_POINT('Origin',(23.3408711739,15.6090782051017,5.99920149541289));
#87167=CARTESIAN_POINT('',(18.3408711739,14.6090782051017,5.99920149541289));
#87168=CARTESIAN_POINT('',(26.3408711739,14.6090782051017,5.99920149541289));
#87169=CARTESIAN_POINT('Origin',(18.3408711739,15.6090782051017,5.99920149541289));
#87170=CARTESIAN_POINT('Origin',(18.3408711739,15.6090782051017,5.99920149541289));
#87171=CARTESIAN_POINT('Origin',(26.3408711739,36.3909217948983,5.99920149541289));
#87172=CARTESIAN_POINT('',(23.3408711739,35.3909217948983,5.99920149541289));
#87173=CARTESIAN_POINT('Origin',(23.3408711739,36.3909217948983,5.99920149541289));
#87174=CARTESIAN_POINT('',(18.3408711739,35.3909217948983,5.99920149541289));
#87175=CARTESIAN_POINT('',(26.3408711739,35.3909217948983,5.99920149541289));
#87176=CARTESIAN_POINT('Origin',(18.3408711739,36.3909217948983,5.99920149541289));
#87177=CARTESIAN_POINT('Origin',(18.3408711739,36.3909217948983,5.99920149541289));
#87178=CARTESIAN_POINT('Origin',(26.3408711739,26.,-11.9984029908258));
#87179=CARTESIAN_POINT('',(23.3408711739,25.,-11.9984029908258));
#87180=CARTESIAN_POINT('Origin',(23.3408711739,26.,-11.9984029908258));
#87181=CARTESIAN_POINT('',(18.3408711739,25.,-11.9984029908258));
#87182=CARTESIAN_POINT('',(26.3408711739,25.,-11.9984029908258));
#87183=CARTESIAN_POINT('Origin',(18.3408711739,26.,-11.9984029908258));
#87184=CARTESIAN_POINT('Origin',(18.3408711739,26.,-11.9984029908258));
#87185=CARTESIAN_POINT('Origin',(25.,-24.,-23.));
#87186=CARTESIAN_POINT('',(27.5,-24.,-23.));
#87187=CARTESIAN_POINT('Origin',(25.,-24.,-23.));
#87188=CARTESIAN_POINT('',(27.5,-24.,-28.));
#87189=CARTESIAN_POINT('',(27.5,-24.,-23.));
#87190=CARTESIAN_POINT('Origin',(25.,-24.,-28.));
#87191=CARTESIAN_POINT('Origin',(25.,46.,-23.));
#87192=CARTESIAN_POINT('',(27.5,46.,-23.));
#87193=CARTESIAN_POINT('Origin',(25.,46.,-23.));
#87194=CARTESIAN_POINT('',(27.5,46.,-28.));
#87195=CARTESIAN_POINT('',(27.5,46.,-23.));
#87196=CARTESIAN_POINT('Origin',(25.,46.,-28.));
#87197=CARTESIAN_POINT('Origin',(-25.,-24.,-23.));
#87198=CARTESIAN_POINT('',(-22.5,-24.,-23.));
#87199=CARTESIAN_POINT('Origin',(-25.,-24.,-23.));
#87200=CARTESIAN_POINT('',(-22.5,-24.,-28.));
#87201=CARTESIAN_POINT('',(-22.5,-24.,-23.));
#87202=CARTESIAN_POINT('Origin',(-25.,-24.,-28.));
#87203=CARTESIAN_POINT('Origin',(-25.,46.,-23.));
#87204=CARTESIAN_POINT('',(-22.5,46.,-23.));
#87205=CARTESIAN_POINT('Origin',(-25.,46.,-23.));
#87206=CARTESIAN_POINT('',(-22.5,46.,-28.));
#87207=CARTESIAN_POINT('',(-22.5,46.,-23.));
#87208=CARTESIAN_POINT('Origin',(-25.,46.,-28.));
#87209=CARTESIAN_POINT('Origin',(-25.,-24.,-23.));
#87210=CARTESIAN_POINT('',(-30.,-24.,-28.));
#87211=CARTESIAN_POINT('',(-25.,-29.,-28.));
#87212=CARTESIAN_POINT('Origin',(-25.,-24.,-28.));
#87213=CARTESIAN_POINT('',(-25.,-29.,-23.));
#87214=CARTESIAN_POINT('',(-25.,-29.,-23.));
#87215=CARTESIAN_POINT('',(-30.,-24.,-23.));
#87216=CARTESIAN_POINT('Origin',(-25.,-24.,-23.));
#87217=CARTESIAN_POINT('',(-30.,-24.,-23.));
#87218=CARTESIAN_POINT('Origin',(0.,11.,-23.));
#87219=CARTESIAN_POINT('',(25.,-29.,-23.));
#87220=CARTESIAN_POINT('',(-30.,-29.,-23.));
#87221=CARTESIAN_POINT('',(30.,-24.,-23.));
#87222=CARTESIAN_POINT('Origin',(25.,-24.,-23.));
#87223=CARTESIAN_POINT('',(30.,46.,-23.));
#87224=CARTESIAN_POINT('',(30.,-29.,-23.));
#87225=CARTESIAN_POINT('',(25.,51.,-23.));
#87226=CARTESIAN_POINT('Origin',(25.,46.,-23.));
#87227=CARTESIAN_POINT('',(3.,51.,-23.));
#87228=CARTESIAN_POINT('',(30.,51.,-23.));
#87229=CARTESIAN_POINT('',(3.,34.3713153881227,-23.));
#87230=CARTESIAN_POINT('',(3.,25.9043179837241,-23.));
#87231=CARTESIAN_POINT('',(23.341,34.3713153881227,-23.));
#87232=CARTESIAN_POINT('',(0.,34.3713153881227,-23.));
#87233=CARTESIAN_POINT('',(23.341,17.6286846118773,-23.));
#87234=CARTESIAN_POINT('',(23.341,18.5,-23.));
#87235=CARTESIAN_POINT('',(14.7725921509309,17.6286846118481,-23.));
#87236=CARTESIAN_POINT('',(0.,17.6286846118773,-23.));
#87237=CARTESIAN_POINT('',(-23.,-2.81668763803891E-15,-23.0000000000237));
#87238=CARTESIAN_POINT('Origin',(0.,0.,-23.));
#87239=CARTESIAN_POINT('',(-14.7725921509309,17.6286846118481,-23.));
#87240=CARTESIAN_POINT('Origin',(0.,0.,-23.));
#87241=CARTESIAN_POINT('',(-23.341,17.6286846118773,-23.));
#87242=CARTESIAN_POINT('',(0.,17.6286846118773,-23.));
#87243=CARTESIAN_POINT('',(-23.341,34.3713153881227,-23.));
#87244=CARTESIAN_POINT('',(-23.341,18.5,-23.));
#87245=CARTESIAN_POINT('',(-3.,34.3713153881227,-23.));
#87246=CARTESIAN_POINT('',(0.,34.3713153881227,-23.));
#87247=CARTESIAN_POINT('',(-3.,51.,-23.));
#87248=CARTESIAN_POINT('',(-3.,25.9043179837241,-23.));
#87249=CARTESIAN_POINT('',(-25.,51.,-23.));
#87250=CARTESIAN_POINT('',(30.,51.,-23.));
#87251=CARTESIAN_POINT('',(-30.,46.,-23.));
#87252=CARTESIAN_POINT('Origin',(-25.,46.,-23.));
#87253=CARTESIAN_POINT('',(-30.,-29.,-23.));
#87254=CARTESIAN_POINT('Origin',(30.,-29.,-23.));
#87255=CARTESIAN_POINT('',(25.,-29.,-28.));
#87256=CARTESIAN_POINT('',(-30.,-29.,-28.));
#87257=CARTESIAN_POINT('',(25.,-29.,-23.));
#87258=CARTESIAN_POINT('Origin',(25.,-24.,-23.));
#87259=CARTESIAN_POINT('',(30.,-24.,-28.));
#87260=CARTESIAN_POINT('Origin',(25.,-24.,-28.));
#87261=CARTESIAN_POINT('',(30.,-24.,-23.));
#87262=CARTESIAN_POINT('Origin',(-25.,46.,-23.));
#87263=CARTESIAN_POINT('',(-25.,51.,-28.));
#87264=CARTESIAN_POINT('',(-30.,46.,-28.));
#87265=CARTESIAN_POINT('Origin',(-25.,46.,-28.));
#87266=CARTESIAN_POINT('',(-30.,46.,-23.));
#87267=CARTESIAN_POINT('',(-25.,51.,-23.));
#87268=CARTESIAN_POINT('Origin',(-30.,51.,-23.));
#87269=CARTESIAN_POINT('',(30.,51.,-23.));
#87270=CARTESIAN_POINT('',(25.,51.,-28.));
#87271=CARTESIAN_POINT('',(25.,51.,-23.));
#87272=CARTESIAN_POINT('',(30.,51.,-28.));
#87273=CARTESIAN_POINT('Origin',(25.,46.,-23.));
#87274=CARTESIAN_POINT('',(30.,46.,-28.));
#87275=CARTESIAN_POINT('Origin',(25.,46.,-28.));
#87276=CARTESIAN_POINT('',(30.,46.,-23.));
#87277=CARTESIAN_POINT('Origin',(30.,51.,-23.));
#87278=CARTESIAN_POINT('',(30.,-29.,-28.));
#87279=CARTESIAN_POINT('Origin',(-3.,40.8086359674483,-11.5));
#87280=CARTESIAN_POINT('',(-3.,30.6172719348965,-12.6858503806098));
#87281=CARTESIAN_POINT('',(-3.,32.8998127405133,-18.9570797030256));
#87282=CARTESIAN_POINT('',(-3.,39.5,0.));
#87283=CARTESIAN_POINT('Origin',(-3.,26.,7.77156117237612E-15));
#87284=CARTESIAN_POINT('',(-3.,39.5,9.86076131526265E-31));
#87285=CARTESIAN_POINT('Origin',(0.,51.,-23.));
#87286=CARTESIAN_POINT('',(3.,39.5,0.));
#87287=CARTESIAN_POINT('',(0.,39.5,1.11022302462516E-15));
#87288=CARTESIAN_POINT('',(3.,39.5,9.86076131526265E-31));
#87289=CARTESIAN_POINT('Origin',(3.,40.8086359674483,-11.5));
#87290=CARTESIAN_POINT('',(3.,30.6172719348965,-12.6858503806098));
#87291=CARTESIAN_POINT('Origin',(3.,26.,7.77156117237612E-15));
#87292=CARTESIAN_POINT('',(3.,32.8998127405133,-18.9570797030256));
#87293=CARTESIAN_POINT('Origin',(0.,26.,7.77156117237612E-15));
#87294=CARTESIAN_POINT('',(-23.341,30.6172719348965,-12.6858503806098));
#87295=CARTESIAN_POINT('',(0.,30.6172719348965,-12.6858503806098));
#87296=CARTESIAN_POINT('',(-23.3408711738295,21.3827280651035,-12.6858503806098));
#87297=CARTESIAN_POINT('Origin',(-23.3408711739,26.,7.77156117237612E-15));
#87298=CARTESIAN_POINT('',(-8.47224530415857,21.3827280651035,-12.6858503806098));
#87299=CARTESIAN_POINT('',(0.,21.3827280651035,-12.6858503806098));
#87300=CARTESIAN_POINT('',(8.47224530415857,21.3827280651035,-12.6858503806098));
#87301=CARTESIAN_POINT('Ctrl Pts',(-8.47224530415855,21.3827280651035,-12.6858503806098));
#87302=CARTESIAN_POINT('Ctrl Pts',(-9.35628286281192,21.0324554978147,-12.5583615922366));
#87303=CARTESIAN_POINT('Ctrl Pts',(-10.209624743653,20.6302930419102,-12.3957375602561));
#87304=CARTESIAN_POINT('Ctrl Pts',(-12.1079676069651,19.5944481184793,-11.9018501855925));
#87305=CARTESIAN_POINT('Ctrl Pts',(-13.1142232633922,18.928496485912,-11.5302951941811));
#87306=CARTESIAN_POINT('Ctrl Pts',(-14.6740782199554,17.7306523050959,-10.6891601041063));
#87307=CARTESIAN_POINT('Ctrl Pts',(-15.3466928743124,17.1509714206232,-10.226343468984));
#87308=CARTESIAN_POINT('Ctrl Pts',(-16.5328372723469,16.0106865238809,-9.11575746654458));
#87309=CARTESIAN_POINT('Ctrl Pts',(-17.0470433193552,15.4527028814967,-8.46602249011973));
#87310=CARTESIAN_POINT('Ctrl Pts',(-18.0617605062209,14.2705140920159,-6.79548401503536));
#87311=CARTESIAN_POINT('Ctrl Pts',(-18.5481190870437,13.6110072927135,-5.54965650514264));
#87312=CARTESIAN_POINT('Ctrl Pts',(-19.1670802823021,12.7245909828806,-2.83714766145209));
#87313=CARTESIAN_POINT('Ctrl Pts',(-19.3067345763078,12.5,-1.37132291257204));
#87314=CARTESIAN_POINT('Ctrl Pts',(-19.3067345763078,12.5,1.37132291257206));
#87315=CARTESIAN_POINT('Ctrl Pts',(-19.1670802823021,12.7245909828806,2.83714766145211));
#87316=CARTESIAN_POINT('Ctrl Pts',(-18.5481190870437,13.6110072927135,5.54965650514266));
#87317=CARTESIAN_POINT('Ctrl Pts',(-18.0617605062209,14.2705140920159,6.79548401503537));
#87318=CARTESIAN_POINT('Ctrl Pts',(-17.0470433193552,15.4527028814967,8.46602249011974));
#87319=CARTESIAN_POINT('Ctrl Pts',(-16.5328372723469,16.0106865238809,9.11575746654459));
#87320=CARTESIAN_POINT('Ctrl Pts',(-15.3466928743124,17.1509714206232,10.226343468984));
#87321=CARTESIAN_POINT('Ctrl Pts',(-14.6740782199554,17.7306523050959,10.6891601041063));
#87322=CARTESIAN_POINT('Ctrl Pts',(-13.1142232633922,18.928496485912,11.5302951941811));
#87323=CARTESIAN_POINT('Ctrl Pts',(-12.1079676069651,19.5944481184793,11.9018501855925));
#87324=CARTESIAN_POINT('Ctrl Pts',(-9.92554422303049,20.7853036940003,12.4696461176801));
#87325=CARTESIAN_POINT('Ctrl Pts',(-8.74955002586604,21.3099969687168,12.666995319975));
#87326=CARTESIAN_POINT('Ctrl Pts',(-6.30687367788335,22.1561289830517,12.9488785425586));
#87327=CARTESIAN_POINT('Ctrl Pts',(-5.03861971528053,22.4782166140122,13.0343544769648));
#87328=CARTESIAN_POINT('Ctrl Pts',(-2.49822268817386,22.9001483475584,13.141091066862));
#87329=CARTESIAN_POINT('Ctrl Pts',(-1.22608486406836,23.,13.1624465810882));
#87330=CARTESIAN_POINT('Ctrl Pts',(0.,23.,13.1624465810882));
#87331=CARTESIAN_POINT('Ctrl Pts',(1.22608486406836,23.,13.1624465810882));
#87332=CARTESIAN_POINT('Ctrl Pts',(2.49822268817386,22.9001483475584,13.141091066862));
#87333=CARTESIAN_POINT('Ctrl Pts',(5.03861971528053,22.4782166140122,13.0343544769648));
#87334=CARTESIAN_POINT('Ctrl Pts',(6.30687367788335,22.1561289830517,12.9488785425586));
#87335=CARTESIAN_POINT('Ctrl Pts',(8.74955002586604,21.3099969687168,12.666995319975));
#87336=CARTESIAN_POINT('Ctrl Pts',(9.92554422303049,20.7853036940003,12.4696461176801));
#87337=CARTESIAN_POINT('Ctrl Pts',(12.1079676069651,19.5944481184793,11.9018501855925));
#87338=CARTESIAN_POINT('Ctrl Pts',(13.1142232633922,18.928496485912,11.5302951941811));
#87339=CARTESIAN_POINT('Ctrl Pts',(14.6740782199554,17.7306523050959,10.6891601041063));
#87340=CARTESIAN_POINT('Ctrl Pts',(15.3466928743123,17.1509714206232,10.226343468984));
#87341=CARTESIAN_POINT('Ctrl Pts',(16.5328372723469,16.0106865238809,9.1157574665446));
#87342=CARTESIAN_POINT('Ctrl Pts',(17.0470433193552,15.4527028814967,8.46602249011975));
#87343=CARTESIAN_POINT('Ctrl Pts',(18.0617605062209,14.2705140920159,6.79548401503537));
#87344=CARTESIAN_POINT('Ctrl Pts',(18.5481190870437,13.6110072927135,5.54965650514266));
#87345=CARTESIAN_POINT('Ctrl Pts',(19.1670802823021,12.7245909828806,2.83714766145211));
#87346=CARTESIAN_POINT('Ctrl Pts',(19.3067345763078,12.5,1.37132291257206));
#87347=CARTESIAN_POINT('Ctrl Pts',(19.3067345763078,12.5,-1.37132291257204));
#87348=CARTESIAN_POINT('Ctrl Pts',(19.1670802823021,12.7245909828806,-2.83714766145209));
#87349=CARTESIAN_POINT('Ctrl Pts',(18.5481190870437,13.6110072927135,-5.54965650514264));
#87350=CARTESIAN_POINT('Ctrl Pts',(18.0617605062209,14.2705140920159,-6.79548401503536));
#87351=CARTESIAN_POINT('Ctrl Pts',(17.0470433193552,15.4527028814967,-8.46602249011973));
#87352=CARTESIAN_POINT('Ctrl Pts',(16.5328372723469,16.0106865238809,-9.11575746654458));
#87353=CARTESIAN_POINT('Ctrl Pts',(15.3466928743124,17.1509714206232,-10.226343468984));
#87354=CARTESIAN_POINT('Ctrl Pts',(14.6740782199554,17.7306523050959,-10.6891601041063));
#87355=CARTESIAN_POINT('Ctrl Pts',(13.1142232633922,18.928496485912,-11.5302951941811));
#87356=CARTESIAN_POINT('Ctrl Pts',(12.1079676069651,19.5944481184793,-11.9018501855925));
#87357=CARTESIAN_POINT('Ctrl Pts',(10.209624743653,20.6302930419102,-12.3957375602561));
#87358=CARTESIAN_POINT('Ctrl Pts',(9.35628286281192,21.0324554978147,-12.5583615922366));
#87359=CARTESIAN_POINT('Ctrl Pts',(8.47224530415855,21.3827280651035,-12.6858503806098));
#87360=CARTESIAN_POINT('',(23.3408711738295,21.3827280651035,-12.6858503806098));
#87361=CARTESIAN_POINT('',(0.,21.3827280651035,-12.6858503806098));
#87362=CARTESIAN_POINT('',(23.3408711739,30.6172719348965,-12.6858503806098));
#87363=CARTESIAN_POINT('Origin',(23.3408711739,26.,7.77156117237612E-15));
#87364=CARTESIAN_POINT('',(0.,30.6172719348965,-12.6858503806098));
#87365=CARTESIAN_POINT('Origin',(0.,34.3713153881227,-23.));
#87366=CARTESIAN_POINT('',(-23.341,26.,7.77156117237612E-15));
#87367=CARTESIAN_POINT('Origin',(0.,21.3827280651035,-12.6858503806098));
#87368=CARTESIAN_POINT('Origin',(0.,0.,-71.4344129058201));
#87369=CARTESIAN_POINT('',(23.341,26.,7.77156117237612E-15));
#87370=CARTESIAN_POINT('Origin',(0.,21.3827280651035,-12.6858503806098));
#87371=CARTESIAN_POINT('',(-23.341,26.,7.77156117237612E-15));
#87372=CARTESIAN_POINT('Origin',(0.,0.,-71.4344129058201));
#87373=CARTESIAN_POINT('Origin',(-23.341,26.,-17.8407788049984));
#87374=CARTESIAN_POINT('',(-23.341,22.,-12.8937969582276));
#87375=CARTESIAN_POINT('Origin',(-23.341,26.,7.77156117237612E-15));
#87376=CARTESIAN_POINT('Origin',(-23.3408711739,26.,7.77156117237612E-15));
#87377=CARTESIAN_POINT('Origin',(0.,34.3713153881227,-23.));
#87378=CARTESIAN_POINT('',(23.341,26.,7.77156117237612E-15));
#87379=CARTESIAN_POINT('Origin',(23.341,26.,-17.8407788049984));
#87380=CARTESIAN_POINT('Origin',(23.3408711739,26.,6.66133814775094E-15));
#87381=CARTESIAN_POINT('Origin',(-23.3408711739,26.,8.88178419700125E-15));
#87382=CARTESIAN_POINT('',(-23.3408711739,15.5,6.4856820332714E-15));
#87383=CARTESIAN_POINT('Origin',(-23.3408711739,26.,7.77156117237612E-15));
#87384=CARTESIAN_POINT('Origin',(-30.,51.,-23.));
#87385=CARTESIAN_POINT('',(-30.,-29.,-28.));
#87386=CARTESIAN_POINT('Origin',(0.,26.,7.77156117237612E-15));
#87387=CARTESIAN_POINT('',(-12.6392246597645,15.5,9.07151189591777E-15));
#87388=CARTESIAN_POINT('',(0.,15.5,6.4856820332714E-15));
#87389=CARTESIAN_POINT('',(0.,20.,-8.61684396980704));
#87390=CARTESIAN_POINT('Ctrl Pts',(-12.6392246597645,15.5,8.04911692853238E-15));
#87391=CARTESIAN_POINT('Ctrl Pts',(-12.6392246597645,15.5,-0.770455991080875));
#87392=CARTESIAN_POINT('Ctrl Pts',(-12.5292156787668,15.5917627320068,-1.59562994116201));
#87393=CARTESIAN_POINT('Ctrl Pts',(-12.0712736606586,15.9489399276083,-3.13904558498715));
#87394=CARTESIAN_POINT('Ctrl Pts',(-11.721971300226,16.2122340102582,-3.85737065648558));
#87395=CARTESIAN_POINT('Ctrl Pts',(-10.7496243003215,16.8795515666301,-5.2831275200831));
#87396=CARTESIAN_POINT('Ctrl Pts',(-10.0374064060355,17.3236709304054,-5.95380333582132));
#87397=CARTESIAN_POINT('Ctrl Pts',(-8.39213189202835,18.1777673238428,-7.03840434115244));
#87398=CARTESIAN_POINT('Ctrl Pts',(-7.45822274458716,18.5875681292269,-7.45117458755254));
#87399=CARTESIAN_POINT('Ctrl Pts',(-5.4523017781929,19.2716230475986,-8.07420868943815));
#87400=CARTESIAN_POINT('Ctrl Pts',(-4.37926194389239,19.546103021309,-8.28545463335066));
#87401=CARTESIAN_POINT('Ctrl Pts',(-2.19300975565939,19.91026838696,-8.55667651899198));
#87402=CARTESIAN_POINT('Ctrl Pts',(-1.07982886357284,20.,-8.61684396980704));
#87403=CARTESIAN_POINT('Ctrl Pts',(-2.77555756156289E-16,20.,-8.61684396980704));
#87404=CARTESIAN_POINT('',(12.6392246597645,15.5,7.33678841994096E-15));
#87405=CARTESIAN_POINT('Ctrl Pts',(0.,20.,-8.61684396980704));
#87406=CARTESIAN_POINT('Ctrl Pts',(1.07982886357284,20.,-8.61684396980704));
#87407=CARTESIAN_POINT('Ctrl Pts',(2.19300975565939,19.91026838696,-8.55667651899198));
#87408=CARTESIAN_POINT('Ctrl Pts',(4.37926194389239,19.546103021309,-8.28545463335066));
#87409=CARTESIAN_POINT('Ctrl Pts',(5.4523017781929,19.2716230475986,-8.07420868943815));
#87410=CARTESIAN_POINT('Ctrl Pts',(7.45822274458716,18.5875681292269,-7.45117458755254));
#87411=CARTESIAN_POINT('Ctrl Pts',(8.39213189202836,18.1777673238428,-7.03840434115244));
#87412=CARTESIAN_POINT('Ctrl Pts',(10.0374064060355,17.3236709304054,-5.95380333582132));
#87413=CARTESIAN_POINT('Ctrl Pts',(10.7496243003215,16.8795515666301,-5.2831275200831));
#87414=CARTESIAN_POINT('Ctrl Pts',(11.721971300226,16.2122340102582,-3.85737065648558));
#87415=CARTESIAN_POINT('Ctrl Pts',(12.0712736606586,15.9489399276083,-3.13904558498714));
#87416=CARTESIAN_POINT('Ctrl Pts',(12.5292156787668,15.5917627320068,-1.59562994116201));
#87417=CARTESIAN_POINT('Ctrl Pts',(12.6392246597645,15.5,-0.770455991080874));
#87418=CARTESIAN_POINT('Ctrl Pts',(12.6392246597645,15.5,8.32667268468867E-15));
#87419=CARTESIAN_POINT('',(23.3408711739,15.5,6.4856820332714E-15));
#87420=CARTESIAN_POINT('',(0.,15.5,6.4856820332714E-15));
#87421=CARTESIAN_POINT('Origin',(23.3408711739,26.,7.77156117237612E-15));
#87422=CARTESIAN_POINT('Ctrl Pts',(12.6392246597645,15.5,8.32667268468867E-15));
#87423=CARTESIAN_POINT('Ctrl Pts',(12.6392246597645,15.5,0.77045599108089));
#87424=CARTESIAN_POINT('Ctrl Pts',(12.5292156787668,15.5917627320068,1.59562994116203));
#87425=CARTESIAN_POINT('Ctrl Pts',(12.0712736606586,15.9489399276083,3.13904558498716));
#87426=CARTESIAN_POINT('Ctrl Pts',(11.721971300226,16.2122340102582,3.8573706564856));
#87427=CARTESIAN_POINT('Ctrl Pts',(10.7496243003215,16.8795515666301,5.28312752008312));
#87428=CARTESIAN_POINT('Ctrl Pts',(10.0374064060355,17.3236709304054,5.95380333582134));
#87429=CARTESIAN_POINT('Ctrl Pts',(8.39213189202835,18.1777673238429,7.03840434115246));
#87430=CARTESIAN_POINT('Ctrl Pts',(7.45822274458715,18.5875681292269,7.45117458755255));
#87431=CARTESIAN_POINT('Ctrl Pts',(5.4523017781929,19.2716230475986,8.07420868943816));
#87432=CARTESIAN_POINT('Ctrl Pts',(4.37926194389238,19.546103021309,8.28545463335068));
#87433=CARTESIAN_POINT('Ctrl Pts',(2.19300975565938,19.91026838696,8.556676518992));
#87434=CARTESIAN_POINT('Ctrl Pts',(1.07982886357284,20.,8.61684396980705));
#87435=CARTESIAN_POINT('Ctrl Pts',(0.,20.,8.61684396980705));
#87436=CARTESIAN_POINT('Ctrl Pts',(-1.07982886357284,20.,8.61684396980705));
#87437=CARTESIAN_POINT('Ctrl Pts',(-2.19300975565939,19.91026838696,8.556676518992));
#87438=CARTESIAN_POINT('Ctrl Pts',(-4.37926194389239,19.546103021309,8.28545463335068));
#87439=CARTESIAN_POINT('Ctrl Pts',(-5.4523017781929,19.2716230475986,8.07420868943816));
#87440=CARTESIAN_POINT('Ctrl Pts',(-7.45822274458715,18.5875681292269,7.45117458755255));
#87441=CARTESIAN_POINT('Ctrl Pts',(-8.39213189202835,18.1777673238429,7.03840434115246));
#87442=CARTESIAN_POINT('Ctrl Pts',(-10.0374064060354,17.3236709304054,5.95380333582134));
#87443=CARTESIAN_POINT('Ctrl Pts',(-10.7496243003215,16.8795515666301,5.28312752008312));
#87444=CARTESIAN_POINT('Ctrl Pts',(-11.721971300226,16.2122340102582,3.8573706564856));
#87445=CARTESIAN_POINT('Ctrl Pts',(-12.0712736606586,15.9489399276083,3.13904558498717));
#87446=CARTESIAN_POINT('Ctrl Pts',(-12.5292156787668,15.5917627320068,1.59562994116203));
#87447=CARTESIAN_POINT('Ctrl Pts',(-12.6392246597645,15.5,0.770455991080891));
#87448=CARTESIAN_POINT('Ctrl Pts',(-12.6392246597645,15.5,7.7715611723761E-15));
#87449=CARTESIAN_POINT('Origin',(0.,11.,-27.));
#87450=CARTESIAN_POINT('',(-20.,-2.44929359829471E-15,-27.));
#87451=CARTESIAN_POINT('Origin',(0.,0.,-27.));
#87452=CARTESIAN_POINT('Origin',(0.,0.,0.));
#87453=CARTESIAN_POINT('',(-20.,-2.44929359829471E-15,27.0000004769));
#87454=CARTESIAN_POINT('',(-20.,-2.44929359829471E-15,0.));
#87455=CARTESIAN_POINT('Origin',(0.,0.,27.0000004769));
#87456=CARTESIAN_POINT('Origin',(0.,0.,27.0000004769));
#87457=CARTESIAN_POINT('',(-23.,2.81668763803891E-15,27.0000004769));
#87458=CARTESIAN_POINT('Origin',(0.,0.,27.0000004769));
#87459=CARTESIAN_POINT('Origin',(0.,0.,0.));
#87460=CARTESIAN_POINT('',(-23.,-2.81668763803891E-15,0.));
#87461=CARTESIAN_POINT('Origin',(23.3408711739,26.,8.88178419700125E-15));
#87462=CARTESIAN_POINT('Origin',(0.,11.,-28.));
#87463=CARTESIAN_POINT('',(0.,0.,0.));
#87464=CARTESIAN_POINT('Origin',(-26.3408711739,15.6090782051017,5.99920149541289));
#87465=CARTESIAN_POINT('',(-23.3408711739,14.6090782051017,5.99920149541289));
#87466=CARTESIAN_POINT('Origin',(-23.3408711739,15.6090782051017,5.99920149541289));
#87467=CARTESIAN_POINT('',(-26.3408711739,14.6090782051017,5.99920149541289));
#87468=CARTESIAN_POINT('',(-26.3408711739,14.6090782051017,5.99920149541289));
#87469=CARTESIAN_POINT('Origin',(-26.3408711739,15.6090782051017,5.99920149541289));
#87470=CARTESIAN_POINT('Origin',(-26.3408711739,36.3909217948983,5.99920149541289));
#87471=CARTESIAN_POINT('',(-23.3408711739,35.3909217948983,5.99920149541289));
#87472=CARTESIAN_POINT('Origin',(-23.3408711739,36.3909217948983,5.99920149541289));
#87473=CARTESIAN_POINT('',(-26.3408711739,35.3909217948983,5.99920149541289));
#87474=CARTESIAN_POINT('',(-26.3408711739,35.3909217948983,5.99920149541289));
#87475=CARTESIAN_POINT('Origin',(-26.3408711739,36.3909217948983,5.99920149541289));
#87476=CARTESIAN_POINT('Origin',(-26.3408711739,26.,-11.9984029908258));
#87477=CARTESIAN_POINT('',(-23.3408711739,25.,-11.9984029908258));
#87478=CARTESIAN_POINT('Origin',(-23.3408711739,26.,-11.9984029908258));
#87479=CARTESIAN_POINT('',(-26.3408711739,25.,-11.9984029908258));
#87480=CARTESIAN_POINT('',(-26.3408711739,25.,-11.9984029908258));
#87481=CARTESIAN_POINT('Origin',(-26.3408711739,26.,-11.9984029908258));
#87482=CARTESIAN_POINT('Origin',(-26.0408711739,26.,7.77156117237612E-15));
#87483=CARTESIAN_POINT('',(-26.3408711739,26.,13.2));
#87484=CARTESIAN_POINT('Origin',(-26.3408711739,26.,7.77156117237612E-15));
#87485=CARTESIAN_POINT('',(-26.0408711739,26.,13.5));
#87486=CARTESIAN_POINT('Origin',(-26.0408711739,26.,13.2));
#87487=CARTESIAN_POINT('',(-26.0408711739,30.,12.8937969582276));
#87488=CARTESIAN_POINT('Origin',(-26.0408711739,26.,7.77156117237612E-15));
#87489=CARTESIAN_POINT('Origin',(-26.0408711739,26.,7.77156117237612E-15));
#87490=CARTESIAN_POINT('Origin',(-23.3408711739,26.,7.77156117237612E-15));
#87491=CARTESIAN_POINT('',(-23.3408711739,30.,12.8937969582276));
#87492=CARTESIAN_POINT('Origin',(-23.3408711739,26.,7.77156117237612E-15));
#87493=CARTESIAN_POINT('',(-23.3408711739,30.,12.8937969582276));
#87494=CARTESIAN_POINT('Origin',(-26.3408711739,26.,1.11022302462516E-14));
#87495=CARTESIAN_POINT('',(-26.3408711739,20.5,7.09800543284508E-15));
#87496=CARTESIAN_POINT('Origin',(-26.3408711739,26.,7.77156117237612E-15));
#87497=CARTESIAN_POINT('Origin',(-23.3408711739,26.,7.77156117237612E-15));
#87498=CARTESIAN_POINT('',(-23.3408711739,20.5,7.09800543284508E-15));
#87499=CARTESIAN_POINT('',(-23.3408711739,20.5,7.09800543284507E-15));
#87500=CARTESIAN_POINT('Origin',(-23.3408711739,26.,7.77156117237612E-15));
#87501=CARTESIAN_POINT('Origin',(-23.3408711739,26.,1.11022302462516E-14));
#87502=CARTESIAN_POINT('',(0.,0.,0.));
#87503=CARTESIAN_POINT('Origin',(0.,8.67361737988404E-16,-1.84345908510495E-15));
#87504=CARTESIAN_POINT('',(7.64383710467806E-16,6.24166666666667,1.57709296562448));
#87505=CARTESIAN_POINT('Origin',(0.,2.61383781769835E-16,1.57709296562448));
#87506=CARTESIAN_POINT('',(-7.64383710467806E-16,6.24166666666667,-1.57709296562448));
#87507=CARTESIAN_POINT('Origin',(-9.27159680854475E-16,7.57083333333333,
-4.52719563823237E-16));
#87508=CARTESIAN_POINT('Origin',(0.,8.40798337462783E-16,-1.57709296562448));
#87509=CARTESIAN_POINT('Origin',(0.,8.93829624710071E-16,-1.86578184737232));
#87510=CARTESIAN_POINT('',(5.51091059616309E-16,4.5,-1.86578184737232));
#87511=CARTESIAN_POINT('',(-5.51091059616309E-16,-4.5,-1.86578184737232));
#87512=CARTESIAN_POINT('Origin',(0.,8.93829624710071E-16,-1.86578184737232));
#87513=CARTESIAN_POINT('',(-5.81962364344815E-16,-4.75208333333333,-2.80656965511364));
#87514=CARTESIAN_POINT('',(-5.51091059616309E-16,-4.5,-1.86578184737232));
#87515=CARTESIAN_POINT('',(5.97398016709068E-16,4.75208333333333,-2.80656965511364));
#87516=CARTESIAN_POINT('Origin',(0.,1.06664954132416E-15,-2.80656965511364));
#87517=CARTESIAN_POINT('Origin',(0.,1.06664954132416E-15,-2.80656965511364));
#87518=CARTESIAN_POINT('Origin',(0.,8.93829624710071E-16,-1.86578184737232));
#87519=CARTESIAN_POINT('Origin',(0.,0.,3.));
#87520=CARTESIAN_POINT('',(-5.51091059616309E-16,4.5,1.86578184737232));
#87521=CARTESIAN_POINT('',(-5.51091059616309E-16,4.5,3.));
#87522=CARTESIAN_POINT('Origin',(0.,2.08352494522548E-16,1.86578184737232));
#87523=CARTESIAN_POINT('Origin',(0.,3.55325779084578E-17,2.80656965511364));
#87524=CARTESIAN_POINT('',(-5.81962364344815E-16,4.75208333333333,2.80656965511364));
#87525=CARTESIAN_POINT('',(-5.81962364344815E-16,4.75208333333333,2.80656965511364));
#87526=CARTESIAN_POINT('Origin',(0.,3.55325779084578E-17,2.80656965511364));
#87527=CARTESIAN_POINT('Origin',(0.,0.,2.73902412952163));
#87528=CARTESIAN_POINT('',(-6.12833669073321E-16,5.00416666666667,3.));
#87529=CARTESIAN_POINT('Origin',(-6.12833669073322E-16,5.00416666666667,
2.73902412952163));
#87530=CARTESIAN_POINT('Origin',(0.,-1.49799954810032E-31,3.));
#87531=CARTESIAN_POINT('Origin',(0.,0.,2.73902412952163));
#87532=CARTESIAN_POINT('',(-7.32423384024203E-16,5.98069079618829,3.));
#87533=CARTESIAN_POINT('Origin',(0.,-1.96513426654064E-31,3.));
#87534=CARTESIAN_POINT('',(-7.64383710467806E-16,6.24166666666667,2.73902412952163));
#87535=CARTESIAN_POINT('Origin',(-7.32423384024202E-16,5.98069079618829,
2.73902412952163));
#87536=CARTESIAN_POINT('Origin',(0.,4.79404896654054E-17,2.73902412952163));
#87537=CARTESIAN_POINT('Origin',(0.,0.,3.));
#87538=CARTESIAN_POINT('',(-7.64383710467807E-16,6.24166666666667,3.));
#87539=CARTESIAN_POINT('Origin',(0.,0.,3.));
#87540=CARTESIAN_POINT('',(-7.64383710467806E-16,6.24166666666667,-2.73902412952163));
#87541=CARTESIAN_POINT('',(-7.64383710467807E-16,6.24166666666667,3.));
#87542=CARTESIAN_POINT('Origin',(0.,1.05424162956721E-15,-2.73902412952163));
#87543=CARTESIAN_POINT('Origin',(0.,8.67361737988404E-16,-2.73902412952163));
#87544=CARTESIAN_POINT('',(-7.32423384024202E-16,5.98069079618829,-3.));
#87545=CARTESIAN_POINT('Origin',(-7.32423384024202E-16,5.98069079618829,
-2.73902412952163));
#87546=CARTESIAN_POINT('Origin',(0.,1.10218211923262E-15,-3.));
#87547=CARTESIAN_POINT('Origin',(0.,8.67361737988404E-16,-2.73902412952163));
#87548=CARTESIAN_POINT('',(-6.12833669073321E-16,5.00416666666667,-3.));
#87549=CARTESIAN_POINT('Origin',(0.,1.10218211923262E-15,-3.));
#87550=CARTESIAN_POINT('Origin',(-6.12833669073322E-16,5.00416666666667,
-2.73902412952163));
#87551=CARTESIAN_POINT('Origin',(0.,5.00416666666667,-3.));
#87552=CARTESIAN_POINT('Origin',(0.,5.00416666666667,3.));
#87553=CARTESIAN_POINT('Origin',(0.,7.57083333333333,-5.42416478122349E-16));
#87554=CARTESIAN_POINT('',(-2.0625,7.57083333333333,-5.42416478122349E-16));
#87555=CARTESIAN_POINT('',(2.0625,7.57083333333333,-5.42416478122349E-16));
#87556=CARTESIAN_POINT('Origin',(0.,7.57083333333333,-5.42416478122349E-16));
#87557=CARTESIAN_POINT('Origin',(0.,0.,3.));
#87558=CARTESIAN_POINT('',(-7.91325940049048E-16,6.46166666666667,2.0625));
#87559=CARTESIAN_POINT('Origin',(0.,1.72215956130097E-16,2.0625));
#87560=CARTESIAN_POINT('',(-7.91325940049048E-16,6.46166666666667,2.956));
#87561=CARTESIAN_POINT('',(-7.91325940049049E-16,6.46166666666667,3.));
#87562=CARTESIAN_POINT('Origin',(0.,8.08266887437239E-18,2.956));
#87563=CARTESIAN_POINT('Origin',(0.,0.,2.956));
#87564=CARTESIAN_POINT('',(-7.96714385965296E-16,6.50566666666666,3.));
#87565=CARTESIAN_POINT('Origin',(-7.96714385965296E-16,6.50566666666666,
2.956));
#87566=CARTESIAN_POINT('Origin',(0.,-9.91324452525291E-32,3.));
#87567=CARTESIAN_POINT('Origin',(0.,3.4998982877922E-17,2.80947441116742));
#87568=CARTESIAN_POINT('',(1.08993565124114E-15,8.9,2.80947441116742));
#87569=CARTESIAN_POINT('',(-1.08993565124114E-15,-8.9,2.80947441116742));
#87570=CARTESIAN_POINT('Origin',(0.,3.4998982877922E-17,2.80947441116742));
#87571=CARTESIAN_POINT('',(-1.07646453645052E-15,-8.79,3.));
#87572=CARTESIAN_POINT('',(-1.08993565124114E-15,-8.9,2.80947441116742));
#87573=CARTESIAN_POINT('Origin',(0.,-1.01714425032945E-31,3.));
#87574=CARTESIAN_POINT('Origin',(0.,3.4998982877922E-17,2.80947441116742));
#87575=CARTESIAN_POINT('Origin',(0.,0.,3.));
#87576=CARTESIAN_POINT('',(-1.08993565124114E-15,8.9,2.0625));
#87577=CARTESIAN_POINT('',(-1.08993565124114E-15,8.9,3.));
#87578=CARTESIAN_POINT('Origin',(0.,1.72215956130097E-16,2.0625));
#87579=CARTESIAN_POINT('Origin',(0.,8.9,2.0625));
#87580=CARTESIAN_POINT('Origin',(0.,8.79,3.));
#87581=CARTESIAN_POINT('Origin',(0.,0.,3.));
#87582=CARTESIAN_POINT('',(-1.08993565124114E-15,8.9,-2.0625));
#87583=CARTESIAN_POINT('Origin',(0.,9.29966163102522E-16,-2.0625));
#87584=CARTESIAN_POINT('',(-1.08993565124114E-15,8.9,-2.80947441116743));
#87585=CARTESIAN_POINT('',(-1.08993565124114E-15,8.9,3.));
#87586=CARTESIAN_POINT('Origin',(0.,1.0671831363547E-15,-2.80947441116743));
#87587=CARTESIAN_POINT('Origin',(0.,0.,3.));
#87588=CARTESIAN_POINT('',(-7.91325940049048E-16,6.46166666666667,-2.956));
#87589=CARTESIAN_POINT('Origin',(0.,1.09409945035825E-15,-2.956));
#87590=CARTESIAN_POINT('',(-7.91325940049048E-16,6.46166666666667,-2.0625));
#87591=CARTESIAN_POINT('',(-7.91325940049049E-16,6.46166666666667,3.));
#87592=CARTESIAN_POINT('Origin',(0.,9.29966163102522E-16,-2.0625));
#87593=CARTESIAN_POINT('Origin',(0.,8.67361737988404E-16,-2.956));
#87594=CARTESIAN_POINT('',(-7.96714385965296E-16,6.50566666666667,-3.));
#87595=CARTESIAN_POINT('Origin',(0.,1.10218211923262E-15,-3.00000000000001));
#87596=CARTESIAN_POINT('Origin',(-7.96714385965296E-16,6.50566666666666,
-2.956));
#87597=CARTESIAN_POINT('Origin',(0.,1.10218211923262E-15,-3.00000000000001));
#87598=CARTESIAN_POINT('',(-1.07646453645052E-15,8.79,-3.));
#87599=CARTESIAN_POINT('',(-1.07646453645052E-15,8.79,-3.00000000000001));
#87600=CARTESIAN_POINT('Origin',(0.,1.10218211923262E-15,-3.00000000000001));
#87601=CARTESIAN_POINT('Origin',(0.,8.79,-3.));
#87602=CARTESIAN_POINT('Origin',(0.,8.9,-2.0625));
#87603=CARTESIAN_POINT('Origin',(0.,2.75545529808154E-17,2.85));
#87604=CARTESIAN_POINT('',(-1.08993565124114E-15,8.9,2.52448092746025));
#87605=CARTESIAN_POINT('Origin',(0.,8.73514365178982E-17,2.52448092746025));
#87606=CARTESIAN_POINT('',(-1.1044451750474E-15,9.01847925309041,2.85));
#87607=CARTESIAN_POINT('',(-1.1044451750474E-15,9.01847925309041,2.85));
#87608=CARTESIAN_POINT('Origin',(0.,2.75545529808154E-17,2.85));
#87609=CARTESIAN_POINT('Origin',(0.,-9.27691267013628E-33,3.));
#87610=CARTESIAN_POINT('',(-1.12281487703461E-15,9.16847925309041,3.));
#87611=CARTESIAN_POINT('',(-1.12281487703461E-15,9.16847925309041,3.));
#87612=CARTESIAN_POINT('Origin',(0.,-9.27691267013628E-33,3.));
#87613=CARTESIAN_POINT('Origin',(0.,5.5109105961631E-17,2.7));
#87614=CARTESIAN_POINT('',(1.22464679914735E-15,10.,2.7));
#87615=CARTESIAN_POINT('',(-1.22464679914735E-15,-10.,2.7));
#87616=CARTESIAN_POINT('Origin',(0.,5.5109105961631E-17,2.7));
#87617=CARTESIAN_POINT('',(-1.20343529437285E-15,-9.82679491924311,3.));
#87618=CARTESIAN_POINT('',(-1.22464679914735E-15,-10.,2.7));
#87619=CARTESIAN_POINT('Origin',(0.,1.29376829386856E-32,3.));
#87620=CARTESIAN_POINT('Origin',(0.,5.5109105961631E-17,2.7));
#87621=CARTESIAN_POINT('Origin',(0.,0.,3.));
#87622=CARTESIAN_POINT('',(-1.22464679914735E-15,10.,-2.7));
#87623=CARTESIAN_POINT('',(-1.22464679914735E-15,10.,3.));
#87624=CARTESIAN_POINT('Origin',(0.,1.04707301327099E-15,-2.7));
#87625=CARTESIAN_POINT('Origin',(0.,1.10218211923262E-15,-3.));
#87626=CARTESIAN_POINT('',(-1.20343529437285E-15,9.82679491924311,-3.));
#87627=CARTESIAN_POINT('',(-1.20343529437285E-15,9.82679491924311,-3.));
#87628=CARTESIAN_POINT('Origin',(0.,1.10218211923262E-15,-3.));
#87629=CARTESIAN_POINT('Origin',(0.,1.0746275662518E-15,-2.85));
#87630=CARTESIAN_POINT('',(-1.1044451750474E-15,-9.0184792530904,-2.85000000000001));
#87631=CARTESIAN_POINT('Origin',(0.,1.0746275662518E-15,-2.85));
#87632=CARTESIAN_POINT('',(-1.12281487703461E-15,-9.1684792530904,-3.00000000000001));
#87633=CARTESIAN_POINT('',(-1.1044451750474E-15,-9.0184792530904,-2.85));
#87634=CARTESIAN_POINT('Origin',(0.,1.10218211923262E-15,-3.));
#87635=CARTESIAN_POINT('Origin',(0.,1.01483068271472E-15,-2.52448092746026));
#87636=CARTESIAN_POINT('',(1.08993565124114E-15,8.9,-2.52448092746025));
#87637=CARTESIAN_POINT('',(-1.08993565124114E-15,-8.9,-2.52448092746026));
#87638=CARTESIAN_POINT('Origin',(0.,1.01483068271472E-15,-2.52448092746026));
#87639=CARTESIAN_POINT('',(-1.08993565124114E-15,-8.9,-2.52448092746026));
#87640=CARTESIAN_POINT('Origin',(0.,1.01483068271472E-15,-2.52448092746026));
#87641=CARTESIAN_POINT('Origin',(0.,0.,3.));
#87642=CARTESIAN_POINT('',(-1.08993565124114E-15,8.9,-1.57709296562448));
#87643=CARTESIAN_POINT('',(-1.08993565124114E-15,8.9,3.));
#87644=CARTESIAN_POINT('Origin',(0.,8.40798337462783E-16,-1.57709296562448));
#87645=CARTESIAN_POINT('Origin',(0.,8.67361737988404E-16,-1.84345908510495E-15));
#87646=CARTESIAN_POINT('',(-1.08993565124114E-15,8.9,1.57709296562448));
#87647=CARTESIAN_POINT('Origin',(-9.27159680854475E-16,7.57083333333333,
-4.52719563823237E-16));
#87648=CARTESIAN_POINT('Origin',(0.,2.61383781769836E-16,1.57709296562448));
#87649=CARTESIAN_POINT('Origin',(0.,0.,3.));
#87650=CARTESIAN_POINT('',(-1.08993565124114E-15,8.9,3.));
#87651=CARTESIAN_POINT('Origin',(0.,9.82679491924311,-3.));
#87652=CARTESIAN_POINT('Origin',(0.,9.82679491924311,3.));
#87653=CARTESIAN_POINT('Origin',(4.86643786166852,5.79959480477993,-8.67787717300259E-16));
#87654=CARTESIAN_POINT('',(3.28647119773563,7.12534424975842,-6.24251495160616E-16));
#87655=CARTESIAN_POINT('',(6.44640452560141,4.47384535980144,-1.1113239394399E-15));
#87656=CARTESIAN_POINT('Origin',(4.86643786166852,5.79959480477993,-8.67787717300259E-16));
#87657=CARTESIAN_POINT('Origin',(7.45581536342993,1.31466141175336,-1.69165661592412E-15));
#87658=CARTESIAN_POINT('',(7.09766599699189,3.34582740234104,-1.31853747658759E-15));
#87659=CARTESIAN_POINT('',(7.81396472986797,-0.716504578834321,-2.06477575526065E-15));
#87660=CARTESIAN_POINT('Origin',(7.45581536342993,1.31466141175336,-1.69165661592412E-15));
#87661=CARTESIAN_POINT('Origin',(6.55653399448467,-3.7854166666667,-2.62852576004492E-15));
#87662=CARTESIAN_POINT('',(7.58778399448468,-1.9992392713613,-2.3004102955644E-15));
#87663=CARTESIAN_POINT('',(5.52528399448466,-5.5715940619721,-2.95664122452544E-15));
#87664=CARTESIAN_POINT('Origin',(6.55653399448467,-3.7854166666667,-2.62852576004492E-15));
#87665=CARTESIAN_POINT('Origin',(2.58937750176137,-7.11425621653333,-3.24002366498782E-15));
#87666=CARTESIAN_POINT('',(4.52749353213231,-6.40883967092415,-3.11044074779094E-15));
#87667=CARTESIAN_POINT('',(0.651261471390429,-7.81967276214251,-3.3696065821847E-15));
#87668=CARTESIAN_POINT('Origin',(2.58937750176137,-7.11425621653333,-3.24002366498782E-15));
#87669=CARTESIAN_POINT('Origin',(-2.58937750176147,-7.1142562165333,-3.24002366498781E-15));
#87670=CARTESIAN_POINT('',(-0.651261471390539,-7.81967276214251,-3.36960658218469E-15));
#87671=CARTESIAN_POINT('',(-4.5274935321324,-6.40883967092409,-3.11044074779093E-15));
#87672=CARTESIAN_POINT('Origin',(-2.58937750176147,-7.1142562165333,-3.24002366498781E-15));
#87673=CARTESIAN_POINT('Origin',(-6.55653399448472,-3.78541666666661,-2.62852576004491E-15));
#87674=CARTESIAN_POINT('',(-5.52528399448474,-5.57159406197203,-2.95664122452543E-15));
#87675=CARTESIAN_POINT('',(-7.5877839944847,-1.9992392713612,-2.30041029556439E-15));
#87676=CARTESIAN_POINT('Origin',(-6.55653399448472,-3.78541666666661,-2.62852576004491E-15));
#87677=CARTESIAN_POINT('Origin',(-7.45581536342991,1.31466141175346,-1.6916566159241E-15));
#87678=CARTESIAN_POINT('',(-7.81396472986797,-0.716504578834215,-2.06477575526062E-15));
#87679=CARTESIAN_POINT('',(-7.09766599699184,3.34582740234114,-1.31853747658758E-15));
#87680=CARTESIAN_POINT('Origin',(-7.45581536342991,1.31466141175346,-1.6916566159241E-15));
#87681=CARTESIAN_POINT('Origin',(-4.86643786166844,5.79959480477999,-8.67787717300247E-16));
#87682=CARTESIAN_POINT('',(-6.44640452560135,4.47384535980152,-1.11132393943989E-15));
#87683=CARTESIAN_POINT('',(-3.28647119773553,7.12534424975846,-6.24251495160608E-16));
#87684=CARTESIAN_POINT('Origin',(-4.86643786166844,5.79959480477999,-8.67787717300247E-16));
#87685=CARTESIAN_POINT('Origin',(0.,0.,3.));
#87686=CARTESIAN_POINT('',(-7.64383710467806E-16,6.24166666666667,2.0625));
#87687=CARTESIAN_POINT('Origin',(0.,1.72215956130097E-16,2.0625));
#87688=CARTESIAN_POINT('',(-7.64383710467806E-16,6.24166666666667,2.9175));
#87689=CARTESIAN_POINT('',(-7.64383710467807E-16,6.24166666666667,3.));
#87690=CARTESIAN_POINT('Origin',(0.,1.51550041394482E-17,2.9175));
#87691=CARTESIAN_POINT('Origin',(0.,0.,2.9175));
#87692=CARTESIAN_POINT('',(-7.84590382653737E-16,6.40666666666666,2.9175));
#87693=CARTESIAN_POINT('Origin',(-7.74487046560772E-16,6.32416666666667,
2.9175));
#87694=CARTESIAN_POINT('Origin',(0.,1.51550041394483E-17,2.9175));
#87695=CARTESIAN_POINT('Origin',(0.,0.,3.));
#87696=CARTESIAN_POINT('',(-7.84590382653738E-16,6.40666666666667,2.8925));
#87697=CARTESIAN_POINT('',(-7.84590382653738E-16,6.40666666666667,3.));
#87698=CARTESIAN_POINT('Origin',(0.,1.97474296362508E-17,2.8925));
#87699=CARTESIAN_POINT('Origin',(0.,0.,2.8925));
#87700=CARTESIAN_POINT('',(-7.90156322781782E-16,6.45211601689499,2.8964763029096));
#87701=CARTESIAN_POINT('Origin',(-7.87394654311583E-16,6.42956528249449,
2.8925));
#87702=CARTESIAN_POINT('',(7.90741131415415E-16,-6.45211601689499,2.8964763029096));
#87703=CARTESIAN_POINT('Origin',(0.,1.9016994641649E-17,2.8964763029096));
#87704=CARTESIAN_POINT('Origin',(0.,1.9016994641649E-17,2.8964763029096));
#87705=CARTESIAN_POINT('Origin',(0.,2.89668383572898E-17,2.84231187649393));
#87706=CARTESIAN_POINT('',(7.91325940049048E-16,6.46166666666667,2.84231187649393));
#87707=CARTESIAN_POINT('',(-7.91325940049049E-16,-6.46166666666667,2.84231187649393));
#87708=CARTESIAN_POINT('Origin',(0.,2.89668383572898E-17,2.84231187649393));
#87709=CARTESIAN_POINT('',(-7.91325940049049E-16,-6.46166666666667,2.84231187649393));
#87710=CARTESIAN_POINT('Origin',(0.,2.89668383572898E-17,2.84231187649393));
#87711=CARTESIAN_POINT('Origin',(0.,0.,3.));
#87712=CARTESIAN_POINT('',(-7.91325940049048E-16,6.46166666666667,2.0625));
#87713=CARTESIAN_POINT('',(-7.91325940049049E-16,6.46166666666667,3.));
#87714=CARTESIAN_POINT('Origin',(0.,1.72215956130097E-16,2.0625));
#87715=CARTESIAN_POINT('Origin',(0.,6.24166666666667,2.0625));
#87716=CARTESIAN_POINT('',(0.,0.,0.));
#87717=CARTESIAN_POINT('Origin',(0.,0.,5.225));
#87718=CARTESIAN_POINT('',(-20.,2.44929359829471E-15,5.225));
#87719=CARTESIAN_POINT('',(20.,-2.44929359829471E-15,5.225));
#87720=CARTESIAN_POINT('Origin',(0.,0.,5.225));
#87721=CARTESIAN_POINT('Origin',(0.,0.,5.225));
#87722=CARTESIAN_POINT('',(19.725,-2.41561581131815E-15,5.5));
#87723=CARTESIAN_POINT('Origin',(19.725,-2.41561581131815E-15,5.225));
#87724=CARTESIAN_POINT('Origin',(0.,0.,5.5));
#87725=CARTESIAN_POINT('Origin',(0.,0.,-5.225));
#87726=CARTESIAN_POINT('',(-20.,-2.44929359829471E-15,-5.225));
#87727=CARTESIAN_POINT('Origin',(0.,0.,-5.225));
#87728=CARTESIAN_POINT('',(-19.725,-2.41561581131815E-15,-5.5));
#87729=CARTESIAN_POINT('Origin',(-19.725,-2.41561581131815E-15,-5.225));
#87730=CARTESIAN_POINT('Origin',(0.,0.,-5.5));
#87731=CARTESIAN_POINT('Origin',(0.,0.,5.5));
#87732=CARTESIAN_POINT('',(15.4,-1.88595607068692E-15,5.5));
#87733=CARTESIAN_POINT('Origin',(0.,0.,5.5));
#87734=CARTESIAN_POINT('',(18.1997760045464,-2.22882974291666E-15,-5.5));
#87735=CARTESIAN_POINT('',(15.4,-1.88595607068692E-15,5.5));
#87736=CARTESIAN_POINT('Origin',(0.,0.,-5.5));
#87737=CARTESIAN_POINT('Origin',(0.,0.,4.25));
#87738=CARTESIAN_POINT('',(-20.,-2.44929359829471E-15,4.25));
#87739=CARTESIAN_POINT('Origin',(0.,15.4,5.5));
#87740=CARTESIAN_POINT('Origin',(0.,20.,-5.5));
#87741=CARTESIAN_POINT('Origin',(0.,0.,4.94191290631434));
#87742=CARTESIAN_POINT('',(13.0685506725942,1.81711532400453E-15,5.03423736132904));
#87743=CARTESIAN_POINT('',(-13.0685506725942,-1.60043587506875E-15,5.03423736132903));
#87744=CARTESIAN_POINT('Origin',(0.,0.,5.03423736132904));
#87745=CARTESIAN_POINT('Origin',(0.,0.,5.03423736132904));
#87746=CARTESIAN_POINT('',(-12.7058184384753,-1.55601398812262E-15,4.94191290631434));
#87747=CARTESIAN_POINT('',(-12.7058184384753,-1.55601398812262E-15,4.94191290631434));
#87748=CARTESIAN_POINT('',(12.7058184384753,1.55601398812262E-15,4.94191290631434));
#87749=CARTESIAN_POINT('Origin',(0.,0.,4.94191290631434));
#87750=CARTESIAN_POINT('Origin',(0.,0.,4.94191290631434));
#87751=CARTESIAN_POINT('Origin',(0.,0.,-8.86869034258935));
#87752=CARTESIAN_POINT('',(17.5762965073726,2.15247552586186E-15,-8.62202959520812));
#87753=CARTESIAN_POINT('',(-17.5762965073726,-2.15247552586187E-15,-8.6220295952081));
#87754=CARTESIAN_POINT('Origin',(0.,0.,-8.62202959520812));
#87755=CARTESIAN_POINT('Origin',(0.,0.,-8.62202959520812));
#87756=CARTESIAN_POINT('',(-16.6071946160828,-2.0337947729403E-15,-8.86869034258935));
#87757=CARTESIAN_POINT('',(-16.6071946160828,-2.0337947729403E-15,-8.86869034258935));
#87758=CARTESIAN_POINT('',(16.6071946160828,2.0337947729403E-15,-8.86869034258935));
#87759=CARTESIAN_POINT('Origin',(0.,0.,-8.86869034258935));
#87760=CARTESIAN_POINT('Origin',(0.,0.,-8.86869034258935));
#87761=CARTESIAN_POINT('Origin',(0.,0.,5.64211868066453));
#87762=CARTESIAN_POINT('',(-13.3064408708579,-1.62956902205396E-15,6.12666962630939));
#87763=CARTESIAN_POINT('Origin',(0.,0.,6.12666962630939));
#87764=CARTESIAN_POINT('',(-13.9143221901933,-1.70401301325252E-15,5.76544905435514));
#87765=CARTESIAN_POINT('Origin',(-13.4297712445485,-1.64467263679175E-15,
5.64211868066453));
#87766=CARTESIAN_POINT('',(13.9143221901933,1.92824426955719E-15,5.76544905435514));
#87767=CARTESIAN_POINT('Origin',(0.,0.,5.76544905435514));
#87768=CARTESIAN_POINT('Origin',(0.,0.,5.76544905435514));
#87769=CARTESIAN_POINT('Origin',(0.,0.,6.12666962630939));
#87770=CARTESIAN_POINT('',(12.4591576910941,1.54091037338483E-15,5.91101479760407));
#87771=CARTESIAN_POINT('',(-12.4591576910941,-1.52580675864705E-15,5.91101479760407));
#87772=CARTESIAN_POINT('Origin',(0.,0.,5.91101479760407));
#87773=CARTESIAN_POINT('Origin',(0.,0.,5.91101479760407));
#87774=CARTESIAN_POINT('',(-13.3064408708579,-1.62956902205396E-15,6.12666962630939));
#87775=CARTESIAN_POINT('Origin',(0.,0.,5.91101479760407));
#87776=CARTESIAN_POINT('',(12.4591576910941,-1.52580675864705E-15,5.91101479760407));
#87777=CARTESIAN_POINT('Origin',(0.,0.,5.03423736132904));
#87778=CARTESIAN_POINT('',(13.6758990082496,-1.71737624121704E-15,2.64803515038039));
#87779=CARTESIAN_POINT('',(13.0685506725942,-1.60043587506875E-15,5.03423736132904));
#87780=CARTESIAN_POINT('',(12.8785649144981,-4.62651215577902,2.6147440184906));
#87781=CARTESIAN_POINT('Origin',(-0.937114226824163,0.134736684811201,-1.03836599339337));
#87782=CARTESIAN_POINT('',(14.9513426147766,-4.92290433508688,-5.46532997546471));
#87783=CARTESIAN_POINT('Ctrl Pts',(12.8785649144981,-4.62651215577902,2.61474401849061));
#87784=CARTESIAN_POINT('Ctrl Pts',(13.278829444552,-4.68375292971506,1.05871968629378));
#87785=CARTESIAN_POINT('Ctrl Pts',(13.678412855787,-4.74088814688723,-0.497483831381018));
#87786=CARTESIAN_POINT('Ctrl Pts',(14.0774687012176,-4.79794842577841,-2.05382524940579));
#87787=CARTESIAN_POINT('Ctrl Pts',(14.3690279116768,-4.83963795382966,-3.19092342811977));
#87788=CARTESIAN_POINT('Ctrl Pts',(14.6603042032756,-4.8812871409245,-4.32809569652915));
#87789=CARTESIAN_POINT('Ctrl Pts',(14.9513426147766,-4.92290433508687,-5.46532997546471));
#87790=CARTESIAN_POINT('',(15.73602449803,-1.07552855510562E-15,-5.44596249471135));
#87791=CARTESIAN_POINT('Origin',(-1.07828029600555,0.155033301408076,-9.68767988915812));
#87792=CARTESIAN_POINT('',(13.0685506725942,-1.60043587506875E-15,5.03423736132904));
#87793=CARTESIAN_POINT('',(15.7326506103909,0.51121213621885,-5.46532997546471));
#87794=CARTESIAN_POINT('Origin',(-1.07828029600555,0.155033301408076,-9.68767988915812));
#87795=CARTESIAN_POINT('',(13.6603316446047,0.810794884002057,2.6147440184906));
#87796=CARTESIAN_POINT('Ctrl Pts',(15.7326506103909,0.511212136218851,-5.46532997546471));
#87797=CARTESIAN_POINT('Ctrl Pts',(15.3395296796034,0.568042178714901,-3.92886882847666));
#87798=CARTESIAN_POINT('Ctrl Pts',(14.9459770913082,0.624938443835918,-2.39252047018801));
#87799=CARTESIAN_POINT('Ctrl Pts',(14.5518755460098,0.681912741033039,-0.856315892565244));
#87800=CARTESIAN_POINT('Ctrl Pts',(14.2550284656633,0.724827197927523,0.30079158169481));
#87801=CARTESIAN_POINT('Ctrl Pts',(13.9578694621683,0.767785972485785,1.45781746616772));
#87802=CARTESIAN_POINT('Ctrl Pts',(13.6603316446047,0.810794884002048,2.61474401849061));
#87803=CARTESIAN_POINT('Origin',(-0.937114226824163,0.134736684811201,-1.03836599339337));
#87804=CARTESIAN_POINT('',(-12.8785649144981,-4.62651215577884,2.6147440184906));
#87805=CARTESIAN_POINT('',(-13.6603316446047,0.810794884002255,2.6147440184906));
#87806=CARTESIAN_POINT('Origin',(0.937114226824163,0.134736684811185,-1.03836599339337));
#87807=CARTESIAN_POINT('',(-15.7326506103909,0.511212136219076,-5.46532997546471));
#87808=CARTESIAN_POINT('Ctrl Pts',(-13.6603316446047,0.810794884002257,
2.61474401849061));
#87809=CARTESIAN_POINT('Ctrl Pts',(-14.0605092383751,0.752949454933123,
1.05871968629378));
#87810=CARTESIAN_POINT('Ctrl Pts',(-14.4600035646476,0.695194638237067,
-0.497483831381016));
#87811=CARTESIAN_POINT('Ctrl Pts',(-14.8589705815908,0.63751655140806,-2.05382524514076));
#87812=CARTESIAN_POINT('Ctrl Pts',(-15.1504648938438,0.595375638655163,
-3.19092342811977));
#87813=CARTESIAN_POINT('Ctrl Pts',(-15.4416763809839,0.553275726649975,
-4.32809569652915));
#87814=CARTESIAN_POINT('Ctrl Pts',(-15.7326506103909,0.51121213621909,-5.46532997546471));
#87815=CARTESIAN_POINT('',(-14.9513426147767,-4.92290433508666,-5.46532997546471));
#87816=CARTESIAN_POINT('Origin',(1.07828029600555,0.155033301408058,-9.68767988915812));
#87817=CARTESIAN_POINT('Ctrl Pts',(-14.9513426147767,-4.92290433508665,
-5.46532997546471));
#87818=CARTESIAN_POINT('Ctrl Pts',(-14.5221701265151,-4.86153458433446,
-3.78833599137146));
#87819=CARTESIAN_POINT('Ctrl Pts',(-14.0924827365919,-4.80009582568339,
-2.11147616269138));
#87820=CARTESIAN_POINT('Ctrl Pts',(-13.6621274936101,-4.73855928020904,
-0.434791406020226));
#87821=CARTESIAN_POINT('Ctrl Pts',(-13.4012014616513,-4.70124943702037,
0.58178898317796));
#87822=CARTESIAN_POINT('Ctrl Pts',(-13.1400290384343,-4.66390345000266,
1.59830486814573));
#87823=CARTESIAN_POINT('Ctrl Pts',(-12.8785649144981,-4.62651215577882,
2.6147440184906));
#87824=CARTESIAN_POINT('',(12.9587657595714,8.93577210236536,-5.46532997546471));
#87825=CARTESIAN_POINT('',(15.2393928192273,3.94189542962978,-5.46532997546471));
#87826=CARTESIAN_POINT('Origin',(-0.990924439240726,-0.452540028181473,
-9.68767988916879));
#87827=CARTESIAN_POINT('',(11.0534534467936,8.06741692762184,2.6147440184906));
#87828=CARTESIAN_POINT('Ctrl Pts',(12.9587657595714,8.93577210236537,-5.46532997546471));
#87829=CARTESIAN_POINT('Ctrl Pts',(12.5973267470854,8.77104335500624,-3.92886882847666));
#87830=CARTESIAN_POINT('Ctrl Pts',(12.235488798542,8.60613694599651,-2.39252047018801));
#87831=CARTESIAN_POINT('Ctrl Pts',(11.8731468506549,8.44099939318352,-0.856315892565245));
#87832=CARTESIAN_POINT('Ctrl Pts',(11.6002218885467,8.3166136834777,0.300791581694808));
#87833=CARTESIAN_POINT('Ctrl Pts',(11.3270105600498,8.19209661777709,1.45781746616771));
#87834=CARTESIAN_POINT('Ctrl Pts',(11.0534534467936,8.06741692762186,2.6147440184906));
#87835=CARTESIAN_POINT('',(13.3354195459858,3.07060816729373,2.6147440184906));
#87836=CARTESIAN_POINT('Origin',(-0.861194805452217,-0.393294489564575,
-1.03836599340818));
#87837=CARTESIAN_POINT('Ctrl Pts',(13.3354195459858,3.07060816729374,2.61474401849061));
#87838=CARTESIAN_POINT('Ctrl Pts',(13.7030901947733,3.23885350672491,1.05871968629378));
#87839=CARTESIAN_POINT('Ctrl Pts',(14.0701307816529,3.40681940552155,-0.49748383138102));
#87840=CARTESIAN_POINT('Ctrl Pts',(14.4366870362378,3.57456312234433,-2.05382524514076));
#87841=CARTESIAN_POINT('Ctrl Pts',(14.7045013135956,3.6971204699282,-3.19092342811977));
#87842=CARTESIAN_POINT('Ctrl Pts',(14.9720557734904,3.81955879654057,-4.32809569652915));
#87843=CARTESIAN_POINT('Ctrl Pts',(15.2393928192273,3.94189542962981,-5.46532997546471));
#87844=CARTESIAN_POINT('',(-15.2393928192272,3.94189542963,-5.46532997546471));
#87845=CARTESIAN_POINT('',(-12.9587657595713,8.93577210236555,-5.46532997546471));
#87846=CARTESIAN_POINT('Origin',(0.990924439244865,-0.452540028182586,-9.68767988916981));
#87847=CARTESIAN_POINT('',(-13.3354195459858,3.07060816729392,2.6147440184906));
#87848=CARTESIAN_POINT('Ctrl Pts',(-15.2393928192272,3.94189542963002,-5.46532997546471));
#87849=CARTESIAN_POINT('Ctrl Pts',(-14.8782069215336,3.77661243818618,-3.92886882847666));
#87850=CARTESIAN_POINT('Ctrl Pts',(-14.5166255085638,3.61114429462567,-2.39252047018801));
#87851=CARTESIAN_POINT('Ctrl Pts',(-14.154539359383,3.44544662077634,-0.856315892565249));
#87852=CARTESIAN_POINT('Ctrl Pts',(-13.8818070712189,3.32063901398268,0.300791581694806));
#87853=CARTESIAN_POINT('Ctrl Pts',(-13.6087879807142,3.19570100579582,1.45781746616771));
#87854=CARTESIAN_POINT('Ctrl Pts',(-13.3354195459858,3.07060816729395,2.6147440184906));
#87855=CARTESIAN_POINT('',(-11.0534534467934,8.06741692762199,2.6147440184906));
#87856=CARTESIAN_POINT('Origin',(0.861194805416237,-0.393294489547195,-1.03836599339796));
#87857=CARTESIAN_POINT('Ctrl Pts',(-11.0534534467934,8.06741692762199,2.6147440184906));
#87858=CARTESIAN_POINT('Ctrl Pts',(-11.4213778613707,8.23510659748291,1.05871968629378));
#87859=CARTESIAN_POINT('Ctrl Pts',(-11.788678486004,8.40250309302417,-0.497483831381018));
#87860=CARTESIAN_POINT('Ctrl Pts',(-12.1554940265031,8.56967905289034,-2.05382524514076));
#87861=CARTESIAN_POINT('Ctrl Pts',(-12.4234977440052,8.69182158442034,-3.19092342811977));
#87862=CARTESIAN_POINT('Ctrl Pts',(-12.6912413672041,8.81384570117397,-4.32809569652915));
#87863=CARTESIAN_POINT('Ctrl Pts',(-12.9587657595713,8.93577210236556,-5.46532997546471));
#87864=CARTESIAN_POINT('',(-2.74499836100712,15.4997618392967,-5.46532997546471));
#87865=CARTESIAN_POINT('',(2.74499836100712,15.4997618392967,-5.46532997546471));
#87866=CARTESIAN_POINT('Origin',(-9.82547376793264E-14,-1.08936849638624,
-9.68767988911357));
#87867=CARTESIAN_POINT('',(-2.74661004991401,13.4059010222448,2.6147440184906));
#87868=CARTESIAN_POINT('Ctrl Pts',(-2.74499836100712,15.4997618392967,-5.46532997546471));
#87869=CARTESIAN_POINT('Ctrl Pts',(-2.74530301392585,15.1025545544441,-3.92886882847666));
#87870=CARTESIAN_POINT('Ctrl Pts',(-2.7456117841503,14.7049105812728,-2.39252047018801));
#87871=CARTESIAN_POINT('Ctrl Pts',(-2.74591966746971,14.3067121335667,-0.856315892565247));
#87872=CARTESIAN_POINT('Ctrl Pts',(-2.74615157283914,14.0067791644875,0.300791581694806));
#87873=CARTESIAN_POINT('Ctrl Pts',(-2.74638295349,13.7065311401264,1.45781746616772));
#87874=CARTESIAN_POINT('Ctrl Pts',(-2.746610049914,13.4059010222448,2.61474401849061));
#87875=CARTESIAN_POINT('',(2.74661004991401,13.4059010222448,2.6147440184906));
#87876=CARTESIAN_POINT('Origin',(-3.71924713249427E-14,-0.94675078472652,
-1.03836599339739));
#87877=CARTESIAN_POINT('Ctrl Pts',(2.746610049914,13.4059010222448,2.61474401849061));
#87878=CARTESIAN_POINT('Ctrl Pts',(2.74630461344459,13.8102376480019,1.05871968629378));
#87879=CARTESIAN_POINT('Ctrl Pts',(2.7459916279415,14.2138850654537,-0.497483831381017));
#87880=CARTESIAN_POINT('Ctrl Pts',(2.74567954736412,14.6169996210264,-2.05382524514076));
#87881=CARTESIAN_POINT('Ctrl Pts',(2.74545153424673,14.9115242186639,-3.19092342811977));
#87882=CARTESIAN_POINT('Ctrl Pts',(2.74522385433836,15.2057630349255,-4.32809569652915));
#87883=CARTESIAN_POINT('Ctrl Pts',(2.74499836100712,15.4997618392967,-5.46532997546471));
#87884=CARTESIAN_POINT('',(6.07056434235145,14.5232875631595,-5.46532997546471));
#87885=CARTESIAN_POINT('',(10.6890434799775,11.5551712475411,-5.46532997546471));
#87886=CARTESIAN_POINT('Origin',(-0.588957074466897,-0.916435096252204,
-9.68767988914712));
#87887=CARTESIAN_POINT('',(4.93718187959547,12.7626910983658,2.6147440184906));
#87888=CARTESIAN_POINT('Ctrl Pts',(6.07056434235145,14.5232875631595,-5.46532997546471));
#87889=CARTESIAN_POINT('Ctrl Pts',(5.85556158082525,14.189300239314,-3.92886882847666));
#87890=CARTESIAN_POINT('Ctrl Pts',(5.64031926407142,13.8549477758611,-2.39252047018801));
#87891=CARTESIAN_POINT('Ctrl Pts',(5.4247779218639,13.5201283792499,-0.856315892565248));
#87892=CARTESIAN_POINT('Ctrl Pts',(5.26242682506772,13.267934086908,0.300791581694809));
#87893=CARTESIAN_POINT('Ctrl Pts',(5.09990583794776,13.0154744695129,1.45781746616771));
#87894=CARTESIAN_POINT('Ctrl Pts',(4.93718187959545,12.7626910983658,2.6147440184906));
#87895=CARTESIAN_POINT('',(9.55837269519504,9.79283209313127,2.6147440184906));
#87896=CARTESIAN_POINT('Origin',(-0.511852118179011,-0.796457442358354,
-1.03836599339643));
#87897=CARTESIAN_POINT('Ctrl Pts',(9.55837269519502,9.79283209313128,2.6147440184906));
#87898=CARTESIAN_POINT('Ctrl Pts',(9.77671662956264,10.133146839425,1.05871968629378));
#87899=CARTESIAN_POINT('Ctrl Pts',(9.99468159913746,10.4728858681128,-0.497483831381017));
#87900=CARTESIAN_POINT('Ctrl Pts',(10.2123592431023,10.8121761356224,-2.05382524514076));
#87901=CARTESIAN_POINT('Ctrl Pts',(10.3713994454892,11.0600692670888,-3.19092342811977));
#87902=CARTESIAN_POINT('Ctrl Pts',(10.5302854231128,11.3077218038168,-4.32809569652915));
#87903=CARTESIAN_POINT('Ctrl Pts',(10.6890434799775,11.5551712475411,-5.46532997546471));
#87904=CARTESIAN_POINT('',(-10.6890434799774,11.5551712475413,-5.46532997546471));
#87905=CARTESIAN_POINT('',(-6.07056434235124,14.5232875631596,-5.46532997546471));
#87906=CARTESIAN_POINT('Origin',(0.588957074505134,-0.916435096306598,-9.6876798891643));
#87907=CARTESIAN_POINT('',(-9.55837269519489,9.79283209313141,2.6147440184906));
#87908=CARTESIAN_POINT('Ctrl Pts',(-10.6890434799774,11.5551712475413,-5.46532997546471));
#87909=CARTESIAN_POINT('Ctrl Pts',(-10.4745532991395,11.2208545080897,-3.92886882847666));
#87910=CARTESIAN_POINT('Ctrl Pts',(-10.25983049047,10.8861681770637,-2.39252047018801));
#87911=CARTESIAN_POINT('Ctrl Pts',(-10.0448071641228,10.5510158718736,-0.856315892565248));
#87912=CARTESIAN_POINT('Ctrl Pts',(-9.88284624974924,10.2985708245147,0.300791581694807));
#87913=CARTESIAN_POINT('Ctrl Pts',(-9.72071456220919,10.0458610194711,1.45781746616771));
#87914=CARTESIAN_POINT('Ctrl Pts',(-9.55837269519489,9.79283209313141,2.6147440184906));
#87915=CARTESIAN_POINT('',(-4.93718187959529,12.7626910983659,2.6147440184906));
#87916=CARTESIAN_POINT('Origin',(0.511852118212275,-0.796457442409964,-1.03836599341197));
#87917=CARTESIAN_POINT('Ctrl Pts',(-4.93718187959529,12.7626910983659,2.61474401849061));
#87918=CARTESIAN_POINT('Ctrl Pts',(-5.15603971298079,13.1026755818146,1.05871968629378));
#87919=CARTESIAN_POINT('Ctrl Pts',(-5.374531282876,13.4420761850259,-0.497483831381019));
#87920=CARTESIAN_POINT('Ctrl Pts',(-5.59273400461729,13.7810290055386,-2.05382524514076));
#87921=CARTESIAN_POINT('Ctrl Pts',(-5.75215784068531,14.0286755906086,-3.19092342811977));
#87922=CARTESIAN_POINT('Ctrl Pts',(-5.91142689136349,14.2760819412331,-4.32809569652915));
#87923=CARTESIAN_POINT('Ctrl Pts',(-6.07056434235125,14.5232875631596,-5.46532997546471));
#87924=CARTESIAN_POINT('',(13.5115300540086,-8.07565407112479,-5.46532997546471));
#87925=CARTESIAN_POINT('',(9.9163467712731,-12.2247167569933,-5.46532997546471));
#87926=CARTESIAN_POINT('Origin',(-0.823289777622591,0.713384653218671,-9.68767988916813));
#87927=CARTESIAN_POINT('',(11.9301510645449,-6.70324880648548,2.6147440184906));
#87928=CARTESIAN_POINT('Ctrl Pts',(13.5115300540086,-8.07565407112482,-5.46532997546471));
#87929=CARTESIAN_POINT('Ctrl Pts',(13.2115403227848,-7.81530837572417,-3.92886882847666));
#87930=CARTESIAN_POINT('Ctrl Pts',(12.9112232608118,-7.55467359863853,-2.39252047018801));
#87931=CARTESIAN_POINT('Ctrl Pts',(12.6104865741459,-7.29367638823024,-0.856315892565246));
#87932=CARTESIAN_POINT('Ctrl Pts',(12.3839642261499,-7.09708680158041,0.300791581694807));
#87933=CARTESIAN_POINT('Ctrl Pts',(12.1572034316412,-6.90029129415331,1.45781746616771));
#87934=CARTESIAN_POINT('Ctrl Pts',(11.9301510645449,-6.70324880648547,2.6147440184906));
#87935=CARTESIAN_POINT('',(8.33285691824855,-10.8547475587647,2.6147440184906));
#87936=CARTESIAN_POINT('Origin',(-0.715506502546432,0.619989913722224,-1.0383659933872));
#87937=CARTESIAN_POINT('Ctrl Pts',(8.33285691824854,-10.8547475587647,2.6147440184906));
#87938=CARTESIAN_POINT('Ctrl Pts',(8.63863416941083,-11.1193009047872,1.05871968629378));
#87939=CARTESIAN_POINT('Ctrl Pts',(8.94389549525559,-11.3833972101742,-0.497483831381018));
#87940=CARTESIAN_POINT('Ctrl Pts',(9.24875351836159,-11.647145249137,-2.05382524514076));
#87941=CARTESIAN_POINT('Ctrl Pts',(9.47148967450035,-11.8398455224944,-3.19092342811977));
#87942=CARTESIAN_POINT('Ctrl Pts',(9.69400963328047,-12.0323589006728,-4.32809569652915));
#87943=CARTESIAN_POINT('Ctrl Pts',(9.91634677127309,-12.2247167569933,-5.46532997546471));
#87944=CARTESIAN_POINT('',(-1.73298089344877,-15.6452679842754,-5.46532997546471));
#87945=CARTESIAN_POINT('',(-7.00059417338805,-14.0985571707312,-5.46532997546471));
#87946=CARTESIAN_POINT('Origin',(0.306910571885848,1.04524141815081,-9.68767988916436));
#87947=CARTESIAN_POINT('',(-1.14152572760881,-13.6366773078239,2.6147440184906));
#87948=CARTESIAN_POINT('Ctrl Pts',(-1.73298089344877,-15.6452679842754,
-5.46532997546471));
#87949=CARTESIAN_POINT('Ctrl Pts',(-1.62078235715629,-15.2642362160366,
-3.92886882847666));
#87950=CARTESIAN_POINT('Ctrl Pts',(-1.5084568410213,-14.8827866084033,-2.39252047018801));
#87951=CARTESIAN_POINT('Ctrl Pts',(-1.3959759623371,-14.5008047364799,-0.856315892565247));
#87952=CARTESIAN_POINT('Ctrl Pts',(-1.31125256850485,-14.2130864953857,
0.300791581694806));
#87953=CARTESIAN_POINT('Ctrl Pts',(-1.2264409168063,-13.925065813132,1.45781746616772));
#87954=CARTESIAN_POINT('Ctrl Pts',(-1.14152572760881,-13.6366773078239,
2.61474401849061));
#87955=CARTESIAN_POINT('',(-6.4122318159117,-12.0890583638066,2.6147440184906));
#87956=CARTESIAN_POINT('Origin',(0.266730519261321,0.908400725671796,-1.03836599338752));
#87957=CARTESIAN_POINT('Ctrl Pts',(-6.4122318159117,-12.0890583638066,2.61474401849061));
#87958=CARTESIAN_POINT('Ctrl Pts',(-6.5258535431646,-12.477102566593,1.05871968629378));
#87959=CARTESIAN_POINT('Ctrl Pts',(-6.63927385475469,-12.8644876056617,
-0.497483831381018));
#87960=CARTESIAN_POINT('Ctrl Pts',(-6.75254491007499,-13.2513611125545,
-2.05382524514076));
#87961=CARTESIAN_POINT('Ctrl Pts',(-6.83530330103606,-13.5340196332628,
-3.19092342811977));
#87962=CARTESIAN_POINT('Ctrl Pts',(-6.91798149779113,-13.8164038548732,
-4.32809569652915));
#87963=CARTESIAN_POINT('Ctrl Pts',(-7.00059417338803,-14.0985571707312,
-5.46532997546471));
#87964=CARTESIAN_POINT('',(-9.91634677127328,-12.2247167569932,-5.46532997546471));
#87965=CARTESIAN_POINT('',(-13.5115300540087,-8.07565407112461,-5.46532997546471));
#87966=CARTESIAN_POINT('Origin',(0.823289777498141,0.713384653116,-9.68767988912725));
#87967=CARTESIAN_POINT('',(-8.33285691824872,-10.8547475587646,2.61474401849061));
#87968=CARTESIAN_POINT('Ctrl Pts',(-9.91634677127329,-12.2247167569932,
-5.46532997546471));
#87969=CARTESIAN_POINT('Ctrl Pts',(-9.61595802958152,-11.9648315442198,
-3.92886882847666));
#87970=CARTESIAN_POINT('Ctrl Pts',(-9.31523656461692,-11.7046634730656,
-2.39252047018801));
#87971=CARTESIAN_POINT('Ctrl Pts',(-9.01409663655801,-11.4441316280326,
-0.856315892565249));
#87972=CARTESIAN_POINT('Ctrl Pts',(-8.78727055712117,-11.2478925661512,
0.300791581694807));
#87973=CARTESIAN_POINT('Ctrl Pts',(-8.56020671840674,-11.0514467903809,
1.45781746616772));
#87974=CARTESIAN_POINT('Ctrl Pts',(-8.3328569182487,-10.8547475587646,2.61474401849061));
#87975=CARTESIAN_POINT('',(-11.930151064545,-6.70324880648531,2.61474401849061));
#87976=CARTESIAN_POINT('Origin',(0.715506502489277,0.619989913672336,-1.03836599336785));
#87977=CARTESIAN_POINT('Ctrl Pts',(-11.930151064545,-6.70324880648531,2.61474401849061));
#87978=CARTESIAN_POINT('Ctrl Pts',(-12.2355282790063,-6.96826381947133,
1.05871968629378));
#87979=CARTESIAN_POINT('Ctrl Pts',(-12.5403796810185,-7.23283320217974,
-0.49748383138102));
#87980=CARTESIAN_POINT('Ctrl Pts',(-12.8448289654926,-7.49705295066959,
-2.05382524514076));
#87981=CARTESIAN_POINT('Ctrl Pts',(-13.0672664879565,-7.69009786565978,
-3.19092342811977));
#87982=CARTESIAN_POINT('Ctrl Pts',(-13.2894882494729,-7.88295538182595,
-4.32809569652915));
#87983=CARTESIAN_POINT('Ctrl Pts',(-13.5115300540087,-8.07565407112462,
-5.46532997546471));
#87984=CARTESIAN_POINT('',(7.00059417338784,-14.0985571707313,-5.46532997546471));
#87985=CARTESIAN_POINT('',(1.73298089344855,-15.6452679842754,-5.46532997546471));
#87986=CARTESIAN_POINT('Origin',(-0.306910571834217,1.04524141797904,-9.68767988911857));
#87987=CARTESIAN_POINT('',(6.41223181591152,-12.0890583638067,2.6147440184906));
#87988=CARTESIAN_POINT('Ctrl Pts',(7.00059417338784,-14.0985571707313,-5.46532997546471));
#87989=CARTESIAN_POINT('Ctrl Pts',(6.88898026176519,-13.717353741201,-3.92886882847666));
#87990=CARTESIAN_POINT('Ctrl Pts',(6.77724727135186,-13.3357301523181,-2.39252047018801));
#87991=CARTESIAN_POINT('Ctrl Pts',(6.665357216431,-12.9535747988851,-0.856315892565249));
#87992=CARTESIAN_POINT('Ctrl Pts',(6.58107884574378,-12.6657258872056,0.300791581694807));
#87993=CARTESIAN_POINT('Ctrl Pts',(6.4967112102627,-12.3775748300272,1.45781746616771));
#87994=CARTESIAN_POINT('Ctrl Pts',(6.41223181591153,-12.0890583638067,2.6147440184906));
#87995=CARTESIAN_POINT('',(1.14152572760861,-13.6366773078239,2.6147440184906));
#87996=CARTESIAN_POINT('Origin',(-0.266730519284407,0.908400725745018,-1.03836599340707));
#87997=CARTESIAN_POINT('Ctrl Pts',(1.14152572760862,-13.6366773078239,2.6147440184906));
#87998=CARTESIAN_POINT('Ctrl Pts',(1.2557335831541,-14.0245494078154,1.05871968629378));
#87999=CARTESIAN_POINT('Ctrl Pts',(1.36975450952629,-14.411758090472,-0.497483831381019));
#88000=CARTESIAN_POINT('Ctrl Pts',(1.48362444308898,-14.7984557508468,-2.05382524514076));
#88001=CARTESIAN_POINT('Ctrl Pts',(1.56682038801811,-15.080985794118,-3.19092342811977));
#88002=CARTESIAN_POINT('Ctrl Pts',(1.6499354993178,-15.3632417260429,-4.32809569652915));
#88003=CARTESIAN_POINT('Ctrl Pts',(1.73298089344855,-15.6452679842754,-5.46532997546471));
#88004=CARTESIAN_POINT('Origin',(0.,0.,-8.62202959520812));
#88005=CARTESIAN_POINT('',(16.7057269056484,-5.55111512312578E-16,-5.20166110736635));
#88006=CARTESIAN_POINT('',(17.5762965073726,-2.15247552586187E-15,-8.62202959520812));
#88007=CARTESIAN_POINT('',(16.0018747190063,-4.80108026882922,-5.20507760384135));
#88008=CARTESIAN_POINT('Origin',(-1.14472725656124,0.164586932037927,-9.70476622209448));
#88009=CARTESIAN_POINT('',(13.9356166188379,-4.51728618677704,2.87709523867187));
#88010=CARTESIAN_POINT('Ctrl Pts',(16.0018747190063,-4.80108026882921,-5.20507760384135));
#88011=CARTESIAN_POINT('Ctrl Pts',(15.6318627383349,-4.74997519723103,-3.75496347264913));
#88012=CARTESIAN_POINT('Ctrl Pts',(15.2615370048954,-4.69896135726135,-2.30492612391988));
#88013=CARTESIAN_POINT('Ctrl Pts',(14.8908189592186,-4.64805794703302,-0.854985236809349));
#88014=CARTESIAN_POINT('Ctrl Pts',(14.5727290602808,-4.60438092401258,0.389118080051586));
#88015=CARTESIAN_POINT('Ctrl Pts',(14.2543502786107,-4.56078522296996,1.63315045290804));
#88016=CARTESIAN_POINT('Ctrl Pts',(13.9356166188379,-4.51728618677703,2.87709523867187));
#88017=CARTESIAN_POINT('',(14.6456014158681,-9.0205620750794E-16,2.89233653772541));
#88018=CARTESIAN_POINT('Origin',(-1.00356118737986,0.144290315441051,-1.05545232632974));
#88019=CARTESIAN_POINT('',(17.5762965073726,-2.15247552586187E-15,-8.62202959520812));
#88020=CARTESIAN_POINT('',(14.6437928161456,0.408187454831152,2.87709523867187));
#88021=CARTESIAN_POINT('Origin',(-1.00356118737986,0.144290315441051,-1.05545232632974));
#88022=CARTESIAN_POINT('',(16.7063069772842,0.0983537048588373,-5.20507760384135));
#88023=CARTESIAN_POINT('Ctrl Pts',(14.6437928161456,0.408187454831128,2.87709523867187));
#88024=CARTESIAN_POINT('Ctrl Pts',(15.0641690510667,0.344669830214016,1.23307977231272));
#88025=CARTESIAN_POINT('Ctrl Pts',(15.4839997756004,0.281487984625945,-0.411088229465956));
#88026=CARTESIAN_POINT('Ctrl Pts',(15.9034155138528,0.218567936571954,-2.05537199759547));
#88027=CARTESIAN_POINT('Ctrl Pts',(16.1712077467516,0.178394193372236,-3.1052286949651));
#88028=CARTESIAN_POINT('Ctrl Pts',(16.4388297533631,0.138327718067133,-4.15513295741812));
#88029=CARTESIAN_POINT('Ctrl Pts',(16.7063069772842,0.0983537048588252,
-5.20507760384135));
#88030=CARTESIAN_POINT('Origin',(-1.14472725656124,0.164586932037927,-9.70476622209448));
#88031=CARTESIAN_POINT('',(-14.6437928161456,0.408187454831364,2.87709523867187));
#88032=CARTESIAN_POINT('',(-13.935616618838,-4.51728618677683,2.87709523867187));
#88033=CARTESIAN_POINT('Origin',(1.00356118737986,0.144290315441036,-1.05545232632974));
#88034=CARTESIAN_POINT('',(-16.0018747190064,-4.80108026882899,-5.20507760384135));
#88035=CARTESIAN_POINT('Ctrl Pts',(-13.935616618838,-4.51728618677684,2.87709523867187));
#88036=CARTESIAN_POINT('Ctrl Pts',(-14.3568596453072,-4.57477514375573,
1.23307977231272));
#88037=CARTESIAN_POINT('Ctrl Pts',(-14.7774846585082,-4.63243259031745,
-0.411088229465949));
#88038=CARTESIAN_POINT('Ctrl Pts',(-15.1976377383996,-4.69022431462755,
-2.05537199759547));
#88039=CARTESIAN_POINT('Ctrl Pts',(-15.4659007556441,-4.72712368078047,
-3.1052286949651));
#88040=CARTESIAN_POINT('Ctrl Pts',(-15.7339702211038,-4.76407801143741,
-4.15513295741812));
#88041=CARTESIAN_POINT('Ctrl Pts',(-16.0018747190064,-4.80108026882899,
-5.20507760384135));
#88042=CARTESIAN_POINT('',(-16.7063069772842,0.0983537048590811,-5.20507760384135));
#88043=CARTESIAN_POINT('Origin',(1.14472725656124,0.164586932037911,-9.70476622209449));
#88044=CARTESIAN_POINT('Ctrl Pts',(-16.7063069772842,0.0983537048590963,
-5.20507760384135));
#88045=CARTESIAN_POINT('Ctrl Pts',(-16.3368851191879,0.153563169121086,
-3.75496347264913));
#88046=CARTESIAN_POINT('Ctrl Pts',(-15.9671879204351,0.208948563859175,
-2.30492612391988));
#88047=CARTESIAN_POINT('Ctrl Pts',(-15.5971454125005,0.264550442287883,
-0.854985236809342));
#88048=CARTESIAN_POINT('Ctrl Pts',(-15.2796351501211,0.312258926124563,
0.389118080051595));
#88049=CARTESIAN_POINT('Ctrl Pts',(-14.9618706178388,0.360126825498279,
1.63315045290804));
#88050=CARTESIAN_POINT('Ctrl Pts',(-14.6437928161456,0.40818745483137,2.87709523867187));
#88051=CARTESIAN_POINT('',(10.8659736780762,-12.6901923664643,-5.20507760384135));
#88052=CARTESIAN_POINT('',(14.1074137925972,-8.94937105918356,-5.20507760384135));
#88053=CARTESIAN_POINT('Origin',(-0.874023435400204,0.757345617923459,-9.70476622215003));
#88054=CARTESIAN_POINT('',(9.28115741607829,-11.334346123992,2.87709523867187));
#88055=CARTESIAN_POINT('Ctrl Pts',(10.8659736780762,-12.6901923664643,-5.20507760384135));
#88056=CARTESIAN_POINT('Ctrl Pts',(10.5513660696195,-12.4206261621453,-3.59666600951091));
#88057=CARTESIAN_POINT('Ctrl Pts',(10.2363736133453,-12.1509459082059,-1.9883487212344));
#88058=CARTESIAN_POINT('Ctrl Pts',(9.92089023043911,-11.8811150096239,-0.380153053637523));
#88059=CARTESIAN_POINT('Ctrl Pts',(9.70788468030107,-11.6989327391434,0.705655649662519));
#88060=CARTESIAN_POINT('Ctrl Pts',(9.49465478510907,-11.5166815848276,1.79140883582473));
#88061=CARTESIAN_POINT('Ctrl Pts',(9.28115741607828,-11.334346123992,2.87709523867188));
#88062=CARTESIAN_POINT('',(12.5398252398854,-7.5736429803373,2.87709523867187));
#88063=CARTESIAN_POINT('Origin',(-0.766240160099769,0.663950878237602,-1.05545232629423));
#88064=CARTESIAN_POINT('Ctrl Pts',(12.5398252398854,-7.57364298033732,2.87709523867187));
#88065=CARTESIAN_POINT('Ctrl Pts',(12.8591280121352,-7.85434995773017,1.23307977231272));
#88066=CARTESIAN_POINT('Ctrl Pts',(13.1781534076931,-8.13447953464675,-0.411088229465952));
#88067=CARTESIAN_POINT('Ctrl Pts',(13.4969712330088,-8.41416451494068,-2.05537199759547));
#88068=CARTESIAN_POINT('Ctrl Pts',(13.7005328296359,-8.59274023003717,-3.10522869496511));
#88069=CARTESIAN_POINT('Ctrl Pts',(13.9040092161996,-8.77113367435921,-4.15513295741812));
#88070=CARTESIAN_POINT('Ctrl Pts',(14.1074137925972,-8.94937105918357,-5.20507760384135));
#88071=CARTESIAN_POINT('',(-7.02951640698345,-15.1557337451693,-5.20507760384135));
#88072=CARTESIAN_POINT('',(-2.28020276965841,-16.5502580523615,-5.20507760384135));
#88073=CARTESIAN_POINT('Origin',(0.325823348666811,1.10965242068313,-9.70476622200136));
#88074=CARTESIAN_POINT('',(-6.45455175213294,-13.1508952820527,2.87709523867187));
#88075=CARTESIAN_POINT('Ctrl Pts',(-7.02951640698346,-15.1557337451693,
-5.20507760384135));
#88076=CARTESIAN_POINT('Ctrl Pts',(-6.91686081367391,-14.7640340059215,
-3.62275895686273));
#88077=CARTESIAN_POINT('Ctrl Pts',(-6.80425954802681,-14.3719495108703,
-2.04053160694041));
#88078=CARTESIAN_POINT('Ctrl Pts',(-6.69172285615924,-13.9793742084975,
-0.458421487187023));
#88079=CARTESIAN_POINT('Ctrl Pts',(-6.61263250329852,-13.7034738006056,
0.653479400952417));
#88080=CARTESIAN_POINT('Ctrl Pts',(-6.53357407923927,-13.4273304491785,
1.76532233007841));
#88081=CARTESIAN_POINT('Ctrl Pts',(-6.45455175213295,-13.1508952820527,
2.87709523867187));
#88082=CARTESIAN_POINT('',(-1.67999631123863,-14.5528312515023,2.87709523867187));
#88083=CARTESIAN_POINT('Origin',(0.285643296086849,0.972811728362482,-1.05545232626613));
#88084=CARTESIAN_POINT('Ctrl Pts',(-1.6799963112386,-14.5528312515023,2.87709523867187));
#88085=CARTESIAN_POINT('Ctrl Pts',(-1.8026931939087,-14.9598891620095,1.23307977231273));
#88086=CARTESIAN_POINT('Ctrl Pts',(-1.92498008107355,-15.3664549009767,
-0.41108822946595));
#88087=CARTESIAN_POINT('Ctrl Pts',(-2.04694877672028,-15.7726471352984,
-2.05537199759547));
#88088=CARTESIAN_POINT('Ctrl Pts',(-2.12482441745583,-16.0319963096245,
-3.1052286949651));
#88089=CARTESIAN_POINT('Ctrl Pts',(-2.20256965640269,-16.2911922561345,
-4.15513295741812));
#88090=CARTESIAN_POINT('Ctrl Pts',(-2.28020276965841,-16.5502580523615,
-5.20507760384135));
#88091=CARTESIAN_POINT('',(-14.1074137925973,-8.94937105918337,-5.20507760384135));
#88092=CARTESIAN_POINT('',(-10.8659736780764,-12.6901923664641,-5.20507760384135));
#88093=CARTESIAN_POINT('Origin',(0.874023435123159,0.757345617689386,-9.70476622205794));
#88094=CARTESIAN_POINT('',(-12.5398252398855,-7.57364298033712,2.87709523867187));
#88095=CARTESIAN_POINT('Ctrl Pts',(-14.1074137925973,-8.94937105918338,
-5.20507760384135));
#88096=CARTESIAN_POINT('Ctrl Pts',(-13.8264848392586,-8.70320136698007,
-3.75496347264913));
#88097=CARTESIAN_POINT('Ctrl Pts',(-13.5454193698163,-8.4567348122447,-2.30492612391989));
#88098=CARTESIAN_POINT('Ctrl Pts',(-13.2641804477244,-8.20989945160143,
-0.854985236809355));
#88099=CARTESIAN_POINT('Ctrl Pts',(-13.0228669714886,-7.99810551322451,
0.389118080051585));
#88100=CARTESIAN_POINT('Ctrl Pts',(-12.781425776345,-7.7860399972756,1.63315045290803));
#88101=CARTESIAN_POINT('Ctrl Pts',(-12.5398252398854,-7.57364298033715,
2.87709523867186));
#88102=CARTESIAN_POINT('',(-9.28115741607846,-11.3343461239919,2.87709523867187));
#88103=CARTESIAN_POINT('Origin',(0.766240160049487,0.66395087819444,-1.05545232627727));
#88104=CARTESIAN_POINT('Ctrl Pts',(-9.28115741607846,-11.3343461239919,
2.87709523867187));
#88105=CARTESIAN_POINT('Ctrl Pts',(-9.60444872358046,-11.610450086327,1.23307977231272));
#88106=CARTESIAN_POINT('Ctrl Pts',(-9.92712903289141,-11.8863616679203,
-0.411088229465947));
#88107=CARTESIAN_POINT('Ctrl Pts',(-10.2493397311838,-12.1621310652273,
-2.05537200053958));
#88108=CARTESIAN_POINT('Ctrl Pts',(-10.4550676381112,-12.3382067238051,
-3.1052286949651));
#88109=CARTESIAN_POINT('Ctrl Pts',(-10.6606030034384,-12.5142239799647,
-4.15513295741812));
#88110=CARTESIAN_POINT('Ctrl Pts',(-10.8659736780764,-12.6901923664641,
-5.20507760384135));
#88111=CARTESIAN_POINT('',(2.28020276965817,-16.5502580523615,-5.20507760384135));
#88112=CARTESIAN_POINT('',(7.02951640698323,-15.1557337451694,-5.20507760384135));
#88113=CARTESIAN_POINT('Origin',(-0.325823348773507,1.10965242105334,-9.70476622209937));
#88114=CARTESIAN_POINT('',(1.67999631123842,-14.5528312515024,2.87709523867187));
#88115=CARTESIAN_POINT('Ctrl Pts',(2.28020276965818,-16.5502580523615,-5.20507760384135));
#88116=CARTESIAN_POINT('Ctrl Pts',(2.17298104614731,-16.1924535020959,-3.75496347264914));
#88117=CARTESIAN_POINT('Ctrl Pts',(2.06554599781792,-15.8344014512619,-2.30492612391988));
#88118=CARTESIAN_POINT('Ctrl Pts',(1.95784752666939,-15.4760384148371,-0.854985236809349));
#88119=CARTESIAN_POINT('Ctrl Pts',(1.86543822476761,-15.1685495742783,0.389118080051586));
#88120=CARTESIAN_POINT('Ctrl Pts',(1.77283494356892,-14.8608317391138,1.63315045290804));
#88121=CARTESIAN_POINT('Ctrl Pts',(1.67999631123846,-14.5528312515024,2.87709523867186));
#88122=CARTESIAN_POINT('',(6.45455175213275,-13.1508952820528,2.87709523867187));
#88123=CARTESIAN_POINT('Origin',(-0.285643296179897,0.972811728678056,-1.05545232634991));
#88124=CARTESIAN_POINT('Ctrl Pts',(6.45455175213274,-13.1508952820528,2.87709523867187));
#88125=CARTESIAN_POINT('Ctrl Pts',(6.57140468760753,-13.5596691302799,1.23307977231272));
#88126=CARTESIAN_POINT('Ctrl Pts',(6.68833644522585,-13.967807277155,-0.41108822946595));
#88127=CARTESIAN_POINT('Ctrl Pts',(6.80533395090074,-14.375459185214,-2.05537200005118));
#88128=CARTESIAN_POINT('Ctrl Pts',(6.88003554244981,-14.635740343811,-3.1052286949651));
#88129=CARTESIAN_POINT('Ctrl Pts',(6.95476399392733,-14.8958220990456,-4.15513295741812));
#88130=CARTESIAN_POINT('Ctrl Pts',(7.02951640698322,-15.1557337451694,-5.20507760384135));
#88131=CARTESIAN_POINT('',(16.0572936004958,4.61234089134698,-5.20507760384135));
#88132=CARTESIAN_POINT('',(14.0010657378079,9.11485186254263,-5.20507760384135));
#88133=CARTESIAN_POINT('Origin',(-1.05198826215219,-0.480426941701518,-9.70476622208446));
#88134=CARTESIAN_POINT('',(14.1656160094783,3.73398019712069,2.87709523867187));
#88135=CARTESIAN_POINT('Ctrl Pts',(16.0572936004958,4.61234089134702,-5.20507760384136));
#88136=CARTESIAN_POINT('Ctrl Pts',(15.7183902268811,4.45528963367599,-3.75496347264913));
#88137=CARTESIAN_POINT('Ctrl Pts',(15.3792722311841,4.29799199952221,-2.30492612391988));
#88138=CARTESIAN_POINT('Ctrl Pts',(15.039883904257,4.14038936594967,-0.854985236809349));
#88139=CARTESIAN_POINT('Ctrl Pts',(14.7486760715879,4.00516043288306,0.38911808005159));
#88140=CARTESIAN_POINT('Ctrl Pts',(14.4572691812803,3.86970690561884,1.63315045290804));
#88141=CARTESIAN_POINT('Ctrl Pts',(14.1656160094783,3.73398019712069,2.87709523867187));
#88142=CARTESIAN_POINT('',(12.0984596413753,8.26042125720544,2.87709523867187));
#88143=CARTESIAN_POINT('Origin',(-0.92225862834957,-0.42118140307714,-1.05545232631937));
#88144=CARTESIAN_POINT('Ctrl Pts',(12.0984596413753,8.26042125720544,2.87709523867187));
#88145=CARTESIAN_POINT('Ctrl Pts',(12.4864428546168,8.43425938238591,1.23307977231272));
#88146=CARTESIAN_POINT('Ctrl Pts',(12.8737856194689,8.60808505767906,-0.411088229465946));
#88147=CARTESIAN_POINT('Ctrl Pts',(13.2606377386196,8.7819066131822,-2.05537200357358));
#88148=CARTESIAN_POINT('Ctrl Pts',(13.5076384645677,8.89288972085904,-3.1052286949651));
#88149=CARTESIAN_POINT('Ctrl Pts',(13.7544379950536,9.00387103738414,-4.15513295741834));
#88150=CARTESIAN_POINT('Ctrl Pts',(14.0010657378079,9.11485186254263,-5.20507760384135));
#88151=CARTESIAN_POINT('',(-14.0010657378077,9.11485186254283,-5.20507760384135));
#88152=CARTESIAN_POINT('',(-16.0572936004957,4.61234089134721,-5.20507760384135));
#88153=CARTESIAN_POINT('Origin',(1.05198826173568,-0.480426941512203,-9.7047662219679));
#88154=CARTESIAN_POINT('',(-12.0984596413752,8.26042125720561,2.87709523867187));
#88155=CARTESIAN_POINT('Ctrl Pts',(-14.0010657378077,9.11485186254283,-5.20507760384135));
#88156=CARTESIAN_POINT('Ctrl Pts',(-13.5855255950981,8.92786159368845,-3.43603838975674));
#88157=CARTESIAN_POINT('Ctrl Pts',(-13.1695007029774,8.74087017903734,-1.66711304381579));
#88158=CARTESIAN_POINT('Ctrl Pts',(-12.7528393518526,8.55387043894279,0.101661445498907));
#88159=CARTESIAN_POINT('Ctrl Pts',(-12.534897354391,8.45605695859243,1.02684983702997));
#88160=CARTESIAN_POINT('Ctrl Pts',(-12.316780375612,8.35824112629394,1.95199680280524));
#88161=CARTESIAN_POINT('Ctrl Pts',(-12.0984596413752,8.26042125720561,2.87709523867187));
#88162=CARTESIAN_POINT('',(-14.1656160094783,3.73398019712089,2.87709523867187));
#88163=CARTESIAN_POINT('Origin',(0.922258628312644,-0.421181403062295,-1.05545232630926));
#88164=CARTESIAN_POINT('Ctrl Pts',(-14.1656160094783,3.73398019712093,2.87709523867186));
#88165=CARTESIAN_POINT('Ctrl Pts',(-14.5510690703717,3.91335858314142,1.23307977231272));
#88166=CARTESIAN_POINT('Ctrl Pts',(-14.9360933177658,4.09226110350664,-0.411088229465959));
#88167=CARTESIAN_POINT('Ctrl Pts',(-15.3207931456275,4.27079551583136,-2.05537199759547));
#88168=CARTESIAN_POINT('Ctrl Pts',(-15.5664196600929,4.38478773063213,-3.1052286949651));
#88169=CARTESIAN_POINT('Ctrl Pts',(-15.8119130644899,4.49862906435458,-4.15513295741812));
#88170=CARTESIAN_POINT('Ctrl Pts',(-16.0572936004957,4.61234089134724,-5.20507760384135));
#88171=CARTESIAN_POINT('',(2.47490798157382,16.5222636691604,-5.20507760384135));
#88172=CARTESIAN_POINT('',(-2.47490798157382,16.5222636691604,-5.20507760384135));
#88173=CARTESIAN_POINT('Origin',(-1.52378110129803E-13,-1.15649874592685,
-9.70476622200868));
#88174=CARTESIAN_POINT('',(2.48806170143598,14.4366489882634,2.87709523867187));
#88175=CARTESIAN_POINT('Ctrl Pts',(2.47490798157379,16.5222636691604,-5.20507760384135));
#88176=CARTESIAN_POINT('Ctrl Pts',(2.47698128110552,16.1487448669395,-3.75496347264913));
#88177=CARTESIAN_POINT('Ctrl Pts',(2.47918953533373,15.7749284891158,-2.30492612391988));
#88178=CARTESIAN_POINT('Ctrl Pts',(2.48156292714035,15.4007395080185,-0.854985236809348));
#88179=CARTESIAN_POINT('Ctrl Pts',(2.4835993857609,15.0796714171367,0.389118080051589));
#88180=CARTESIAN_POINT('Ctrl Pts',(2.48575745091808,14.7583289572565,1.63315045290804));
#88181=CARTESIAN_POINT('Ctrl Pts',(2.48806170143596,14.4366489882634,2.87709523867187));
#88182=CARTESIAN_POINT('',(-2.48806170143598,14.4366489882634,2.87709523867187));
#88183=CARTESIAN_POINT('Origin',(-1.14630527292547E-13,-1.01388103426158,
-1.05545232629072));
#88184=CARTESIAN_POINT('Ctrl Pts',(-2.48806170143596,14.4366489882634,2.87709523867187));
#88185=CARTESIAN_POINT('Ctrl Pts',(-2.48501637053932,14.8617858997204,1.23307977231273));
#88186=CARTESIAN_POINT('Ctrl Pts',(-2.48222576670286,15.2863350669608,-0.411088229465946));
#88187=CARTESIAN_POINT('Ctrl Pts',(-2.47963523697349,15.7104362142084,-2.05537199759546));
#88188=CARTESIAN_POINT('Ctrl Pts',(-2.47798121286961,15.9812200280671,-3.10522869496509));
#88189=CARTESIAN_POINT('Ctrl Pts',(-2.47640913910131,16.2518200824836,-4.15513295741812));
#88190=CARTESIAN_POINT('Ctrl Pts',(-2.47490798157379,16.5222636691604,-5.20507760384135));
#88191=CARTESIAN_POINT('',(11.0146352192429,12.5613764077639,-5.20507760384135));
#88192=CARTESIAN_POINT('',(6.85058505338072,15.2374489563349,-5.20507760384135));
#88193=CARTESIAN_POINT('Origin',(-0.625250427241271,-0.972908655507905,
-9.7047662219421));
#88194=CARTESIAN_POINT('',(9.89813240656923,10.7997342514759,2.87709523867187));
#88195=CARTESIAN_POINT('Ctrl Pts',(11.0146352192428,12.5613764077639,-5.20507760384136));
#88196=CARTESIAN_POINT('Ctrl Pts',(10.7749172616532,12.1837760065475,-3.46868155296237));
#88197=CARTESIAN_POINT('Ctrl Pts',(10.5351317085667,11.8057133276335,-1.73239525071041));
#88198=CARTESIAN_POINT('Ctrl Pts',(10.2952515367979,11.427047819608,0.00374645021393172));
#88199=CARTESIAN_POINT('Ctrl Pts',(10.1629096012127,11.2181379880787,0.961576151002431));
#88200=CARTESIAN_POINT('Ctrl Pts',(10.0305386804728,11.0090438751527,1.91936169771154));
#88201=CARTESIAN_POINT('Ctrl Pts',(9.89813240656922,10.7997342514759,2.87709523867187));
#88202=CARTESIAN_POINT('',(5.71195101409927,13.4900296757646,2.87709523867187));
#88203=CARTESIAN_POINT('Origin',(-0.548145471286394,-0.852931002129471,
-1.05545232634732));
#88204=CARTESIAN_POINT('Ctrl Pts',(5.71195101409927,13.4900296757646,2.87709523867187));
#88205=CARTESIAN_POINT('Ctrl Pts',(5.94435927681535,13.8460311742793,1.23307977231273));
#88206=CARTESIAN_POINT('Ctrl Pts',(6.17623549097855,14.2016759467416,-0.411088229465952));
#88207=CARTESIAN_POINT('Ctrl Pts',(6.40770117419705,14.5570519890308,-2.05537199759546));
#88208=CARTESIAN_POINT('Ctrl Pts',(6.55548941029612,14.7839555961293,-3.10522869496509));
#88209=CARTESIAN_POINT('Ctrl Pts',(6.70310935753085,15.0107489206444,-4.15513295741812));
#88210=CARTESIAN_POINT('Ctrl Pts',(6.85058505338072,15.2374489563349,-5.20507760384135));
#88211=CARTESIAN_POINT('',(-6.8505850533805,15.237448956335,-5.20507760384135));
#88212=CARTESIAN_POINT('',(-11.0146352192427,12.5613764077641,-5.20507760384135));
#88213=CARTESIAN_POINT('Origin',(0.625250427357654,-0.972908655687406,-9.70476622199673));
#88214=CARTESIAN_POINT('',(-5.71195101409907,13.4900296757646,2.87709523867187));
#88215=CARTESIAN_POINT('Ctrl Pts',(-6.85058505338051,15.237448956335,-5.20507760384135));
#88216=CARTESIAN_POINT('Ctrl Pts',(-6.6469013722571,14.9243458547414,-3.75496347264912));
#88217=CARTESIAN_POINT('Ctrl Pts',(-6.44294327850138,14.6110653786382,-2.30492612391988));
#88218=CARTESIAN_POINT('Ctrl Pts',(-6.23864481763592,14.2975607288301,-0.854985236809342));
#88219=CARTESIAN_POINT('Ctrl Pts',(-6.0633491245137,14.0285620557497,0.389118080051595));
#88220=CARTESIAN_POINT('Ctrl Pts',(-5.88780279438331,13.7593983142375,1.63315045290805));
#88221=CARTESIAN_POINT('Ctrl Pts',(-5.71195101409905,13.4900296757646,2.87709523867188));
#88222=CARTESIAN_POINT('',(-9.89813240656907,10.7997342514761,2.87709523867187));
#88223=CARTESIAN_POINT('Origin',(0.548145471174728,-0.85293100195315,-1.0554523262942));
#88224=CARTESIAN_POINT('Ctrl Pts',(-9.89813240656907,10.7997342514761,2.87709523867187));
#88225=CARTESIAN_POINT('Ctrl Pts',(-10.1254168785343,11.1590286103616,1.23307977231272));
#88226=CARTESIAN_POINT('Ctrl Pts',(-10.3525978820251,11.5176908115025,-0.411088229465944));
#88227=CARTESIAN_POINT('Ctrl Pts',(-10.5797049814101,11.8758679471799,-2.05537200295315));
#88228=CARTESIAN_POINT('Ctrl Pts',(-10.7247103095276,12.1045600189986,-3.1052286949651));
#88229=CARTESIAN_POINT('Ctrl Pts',(-10.8696852315395,12.333053198008,-4.15513295741812));
#88230=CARTESIAN_POINT('Ctrl Pts',(-11.0146352192427,12.5613764077641,-5.20507760384135));
#88231=CARTESIAN_POINT('Origin',(0.,15.3635472745355,-5.5));
#88232=CARTESIAN_POINT('Origin',(0.,13.3046975771901,2.58898520239593));
#88233=CARTESIAN_POINT('Origin',(0.,15.3635472745355,-5.5));
#88234=CARTESIAN_POINT('Origin',(0.,15.3635472745355,-5.5));
#88235=CARTESIAN_POINT('Origin',(0.,15.3635472745355,-5.5));
#88236=CARTESIAN_POINT('Origin',(0.,13.3046975771901,2.58898520239593));
#88237=CARTESIAN_POINT('Origin',(0.,15.3635472745355,-5.5));
#88238=CARTESIAN_POINT('Origin',(0.,13.3046975771901,2.58898520239593));
#88239=CARTESIAN_POINT('Origin',(8.30616075752262,12.9246384215219,-5.5));
#88240=CARTESIAN_POINT('Origin',(7.1930625741316,11.1926238400616,2.58898520239593));
#88241=CARTESIAN_POINT('Origin',(8.30616075752262,12.9246384215219,-5.5));
#88242=CARTESIAN_POINT('Origin',(8.30616075752262,12.9246384215219,-5.5));
#88243=CARTESIAN_POINT('Origin',(8.30616075752262,12.9246384215219,-5.5));
#88244=CARTESIAN_POINT('Origin',(7.1930625741316,11.1926238400616,2.58898520239593));
#88245=CARTESIAN_POINT('Origin',(8.30616075752262,12.9246384215219,-5.5));
#88246=CARTESIAN_POINT('Origin',(7.1930625741316,11.1926238400616,2.58898520239593));
#88247=CARTESIAN_POINT('Origin',(-13.9751741630591,6.38224819080644,-5.5));
#88248=CARTESIAN_POINT('Origin',(-12.1023786047278,5.52697111701475,2.58898520239593));
#88249=CARTESIAN_POINT('Origin',(-13.9751741630591,6.38224819080644,-5.5));
#88250=CARTESIAN_POINT('Origin',(-13.9751741630591,6.38224819080644,-5.5));
#88251=CARTESIAN_POINT('Origin',(-13.9751741630591,6.38224819080644,-5.5));
#88252=CARTESIAN_POINT('Origin',(-12.1023786047278,5.52697111701475,2.58898520239593));
#88253=CARTESIAN_POINT('Origin',(-13.9751741630591,6.38224819080644,-5.5));
#88254=CARTESIAN_POINT('Origin',(-12.1023786047278,5.52697111701475,2.58898520239593));
#88255=CARTESIAN_POINT('Origin',(-8.30616075752243,12.924638421522,-5.5));
#88256=CARTESIAN_POINT('Origin',(-7.19306257413143,11.1926238400618,2.58898520239593));
#88257=CARTESIAN_POINT('Origin',(-8.30616075752243,12.924638421522,-5.5));
#88258=CARTESIAN_POINT('Origin',(-8.30616075752243,12.924638421522,-5.5));
#88259=CARTESIAN_POINT('Origin',(-8.30616075752243,12.924638421522,-5.5));
#88260=CARTESIAN_POINT('Origin',(-7.19306257413143,11.1926238400618,2.58898520239593));
#88261=CARTESIAN_POINT('Origin',(-8.30616075752243,12.924638421522,-5.5));
#88262=CARTESIAN_POINT('Origin',(-7.19306257413143,11.1926238400618,2.58898520239593));
#88263=CARTESIAN_POINT('Origin',(-15.2071685156867,-2.18646074567933,-5.5));
#88264=CARTESIAN_POINT('Origin',(-13.1692749396441,-1.89345588397264,2.58898520239593));
#88265=CARTESIAN_POINT('Origin',(-15.2071685156867,-2.18646074567933,-5.5));
#88266=CARTESIAN_POINT('Origin',(-15.2071685156867,-2.18646074567933,-5.5));
#88267=CARTESIAN_POINT('Origin',(-15.2071685156867,-2.18646074567933,-5.5));
#88268=CARTESIAN_POINT('Origin',(-13.1692749396441,-1.89345588397264,2.58898520239593));
#88269=CARTESIAN_POINT('Origin',(-15.2071685156867,-2.18646074567933,-5.5));
#88270=CARTESIAN_POINT('Origin',(-13.1692749396441,-1.89345588397264,2.58898520239593));
#88271=CARTESIAN_POINT('Origin',(-11.6109943133018,-10.0609838442053,-5.5));
#88272=CARTESIAN_POINT('Origin',(-10.0550195308737,-8.71272402031869,2.58898520239593));
#88273=CARTESIAN_POINT('Origin',(-11.6109943133018,-10.0609838442053,-5.5));
#88274=CARTESIAN_POINT('Origin',(-11.6109943133018,-10.0609838442053,-5.5));
#88275=CARTESIAN_POINT('Origin',(-11.6109943133018,-10.0609838442053,-5.5));
#88276=CARTESIAN_POINT('Origin',(-10.0550195308737,-8.71272402031869,2.58898520239593));
#88277=CARTESIAN_POINT('Origin',(-11.6109943133018,-10.0609838442053,-5.5));
#88278=CARTESIAN_POINT('Origin',(-10.0550195308737,-8.71272402031869,2.58898520239593));
#88279=CARTESIAN_POINT('Origin',(-4.32841145580919,-14.741215659711,-5.5));
#88280=CARTESIAN_POINT('Origin',(-3.74836646642385,-12.7657638413797,2.58898520239593));
#88281=CARTESIAN_POINT('Origin',(-4.32841145580919,-14.741215659711,-5.5));
#88282=CARTESIAN_POINT('Origin',(-4.32841145580919,-14.741215659711,-5.5));
#88283=CARTESIAN_POINT('Origin',(-4.32841145580919,-14.741215659711,-5.5));
#88284=CARTESIAN_POINT('Origin',(-3.74836646642385,-12.7657638413797,2.58898520239593));
#88285=CARTESIAN_POINT('Origin',(-4.32841145580919,-14.741215659711,-5.5));
#88286=CARTESIAN_POINT('Origin',(-3.74836646642385,-12.7657638413797,2.58898520239593));
#88287=CARTESIAN_POINT('Origin',(4.32841145580897,-14.741215659711,-5.5));
#88288=CARTESIAN_POINT('Origin',(3.74836646642367,-12.7657638413798,2.58898520239593));
#88289=CARTESIAN_POINT('Origin',(4.32841145580897,-14.741215659711,-5.5));
#88290=CARTESIAN_POINT('Origin',(4.32841145580897,-14.741215659711,-5.5));
#88291=CARTESIAN_POINT('Origin',(4.32841145580897,-14.741215659711,-5.5));
#88292=CARTESIAN_POINT('Origin',(3.74836646642367,-12.7657638413798,2.58898520239593));
#88293=CARTESIAN_POINT('Origin',(4.32841145580897,-14.741215659711,-5.5));
#88294=CARTESIAN_POINT('Origin',(3.74836646642367,-12.7657638413798,2.58898520239593));
#88295=CARTESIAN_POINT('Origin',(11.6109943133017,-10.0609838442055,-5.5));
#88296=CARTESIAN_POINT('Origin',(10.0550195308735,-8.71272402031884,2.58898520239593));
#88297=CARTESIAN_POINT('Origin',(11.6109943133017,-10.0609838442055,-5.5));
#88298=CARTESIAN_POINT('Origin',(11.6109943133017,-10.0609838442055,-5.5));
#88299=CARTESIAN_POINT('Origin',(11.6109943133017,-10.0609838442055,-5.5));
#88300=CARTESIAN_POINT('Origin',(10.0550195308735,-8.71272402031884,2.58898520239593));
#88301=CARTESIAN_POINT('Origin',(11.6109943133017,-10.0609838442055,-5.5));
#88302=CARTESIAN_POINT('Origin',(10.0550195308735,-8.71272402031884,2.58898520239593));
#88303=CARTESIAN_POINT('Origin',(15.2071685156866,-2.18646074567955,-5.5));
#88304=CARTESIAN_POINT('Origin',(13.1692749396441,-1.89345588397283,2.58898520239593));
#88305=CARTESIAN_POINT('Origin',(15.2071685156866,-2.18646074567955,-5.5));
#88306=CARTESIAN_POINT('Origin',(15.2071685156866,-2.18646074567955,-5.5));
#88307=CARTESIAN_POINT('Origin',(15.2071685156866,-2.18646074567955,-5.5));
#88308=CARTESIAN_POINT('Origin',(13.1692749396441,-1.89345588397283,2.58898520239593));
#88309=CARTESIAN_POINT('Origin',(15.2071685156866,-2.18646074567955,-5.5));
#88310=CARTESIAN_POINT('Origin',(13.1692749396441,-1.89345588397283,2.58898520239593));
#88311=CARTESIAN_POINT('Origin',(13.9751741630592,6.38224819080624,-5.5));
#88312=CARTESIAN_POINT('Origin',(12.1023786047279,5.52697111701458,2.58898520239593));
#88313=CARTESIAN_POINT('Origin',(13.9751741630592,6.38224819080624,-5.5));
#88314=CARTESIAN_POINT('Origin',(13.9751741630592,6.38224819080624,-5.5));
#88315=CARTESIAN_POINT('Origin',(13.9751741630592,6.38224819080624,-5.5));
#88316=CARTESIAN_POINT('Origin',(12.1023786047279,5.52697111701458,2.58898520239593));
#88317=CARTESIAN_POINT('Origin',(13.9751741630592,6.38224819080624,-5.5));
#88318=CARTESIAN_POINT('Origin',(12.1023786047279,5.52697111701458,2.58898520239593));
#88319=CARTESIAN_POINT('Origin',(0.,0.,3.975));
#88320=CARTESIAN_POINT('',(8.775,-1.0746275662518E-15,4.25));
#88321=CARTESIAN_POINT('Origin',(0.,0.,4.25));
#88322=CARTESIAN_POINT('',(8.5,-1.04094977927525E-15,3.975));
#88323=CARTESIAN_POINT('Origin',(8.775,-1.0746275662518E-15,3.975));
#88324=CARTESIAN_POINT('',(-8.5,1.04094977927525E-15,3.975));
#88325=CARTESIAN_POINT('Origin',(0.,0.,3.975));
#88326=CARTESIAN_POINT('Origin',(0.,0.,3.975));
#88327=CARTESIAN_POINT('Origin',(0.,0.,-7.475));
#88328=CARTESIAN_POINT('',(-8.775,-1.0746275662518E-15,-7.75));
#88329=CARTESIAN_POINT('Origin',(0.,0.,-7.75));
#88330=CARTESIAN_POINT('',(-8.5,-1.04094977927525E-15,-7.475));
#88331=CARTESIAN_POINT('Origin',(-8.775,-1.0746275662518E-15,-7.475));
#88332=CARTESIAN_POINT('Origin',(0.,0.,-7.475));
#88333=CARTESIAN_POINT('Origin',(0.,0.,1.91101479760404));
#88334=CARTESIAN_POINT('',(-11.9728634517814,-1.46625289028525E-15,2.24999999999999));
#88335=CARTESIAN_POINT('Origin',(0.,0.,2.24999999999999));
#88336=CARTESIAN_POINT('',(-10.6410293263727,-1.30315025041754E-15,1.91101479760404));
#88337=CARTESIAN_POINT('',(-10.6410293263727,-1.30315025041754E-15,1.91101479760404));
#88338=CARTESIAN_POINT('',(10.6410293263727,1.42921843500653E-15,1.91101479760404));
#88339=CARTESIAN_POINT('Origin',(0.,0.,1.91101479760404));
#88340=CARTESIAN_POINT('Origin',(0.,0.,1.91101479760404));
#88341=CARTESIAN_POINT('Origin',(0.,0.,-6.17797040479189));
#88342=CARTESIAN_POINT('',(-12.6998790237181,1.63683793952935E-15,-6.17797040479189));
#88343=CARTESIAN_POINT('',(12.6998790237181,-1.5552866195955E-15,-6.17797040479189));
#88344=CARTESIAN_POINT('Origin',(0.,0.,-6.17797040479189));
#88345=CARTESIAN_POINT('',(12.6998790237181,-1.5552866195955E-15,-6.17797040479189));
#88346=CARTESIAN_POINT('Origin',(0.,0.,-6.17797040479189));
#88347=CARTESIAN_POINT('Origin',(0.,0.,-5.83898520239594));
#88348=CARTESIAN_POINT('',(-14.0317131491268,-1.7183892594632E-15,-5.83898520239594));
#88349=CARTESIAN_POINT('',(-14.0317131491268,-1.7183892594632E-15,-5.83898520239594));
#88350=CARTESIAN_POINT('Origin',(0.,0.,-5.83898520239594));
#88351=CARTESIAN_POINT('Origin',(0.,0.,4.25));
#88352=CARTESIAN_POINT('',(-14.0317131491268,-1.7183892594632E-15,-7.75));
#88353=CARTESIAN_POINT('',(-14.0317131491268,-1.7183892594632E-15,4.25));
#88354=CARTESIAN_POINT('Origin',(0.,0.,-7.75));
#88355=CARTESIAN_POINT('Origin',(0.,0.,4.25));
#88356=CARTESIAN_POINT('',(-8.5,-1.04094977927525E-15,4.25));
#88357=CARTESIAN_POINT('Origin',(0.,0.,4.25));
#88358=CARTESIAN_POINT('',(-11.9728634517814,-1.46625289028525E-15,4.25));
#88359=CARTESIAN_POINT('Origin',(0.,0.,4.25));
#88360=CARTESIAN_POINT('',(-11.9728634517814,-1.46625289028524E-15,4.25));
#88361=CARTESIAN_POINT('Origin',(0.,11.9728634517814,4.25));
#88362=CARTESIAN_POINT('Origin',(0.,8.5,-7.75));
#88363=CARTESIAN_POINT('Origin',(0.,15.3635472745355,-5.5));
#88364=CARTESIAN_POINT('',(-3.21052746786287E-16,15.8452898878137,3.2356296922704));
#88365=CARTESIAN_POINT('Origin',(0.,13.3046975771901,2.58898520239593));
#88366=CARTESIAN_POINT('',(-3.21052746786287E-16,17.9041395851591,-4.85335551012554));
#88367=CARTESIAN_POINT('',(-3.21052746786287E-16,17.9041395851591,-4.85335551012554));
#88368=CARTESIAN_POINT('Origin',(0.,15.3635472745355,-5.5));
#88369=CARTESIAN_POINT('Origin',(0.,15.3635472745355,-5.5));
#88370=CARTESIAN_POINT('Origin',(0.,13.3046975771901,2.58898520239593));
#88371=CARTESIAN_POINT('Origin',(8.30616075752262,12.9246384215219,-5.5));
#88372=CARTESIAN_POINT('',(8.56661047776854,13.3299060968575,3.2356296922704));
#88373=CARTESIAN_POINT('Origin',(7.1930625741316,11.1926238400616,2.58898520239593));
#88374=CARTESIAN_POINT('',(9.67970866115956,15.0619206783177,-4.85335551012554));
#88375=CARTESIAN_POINT('',(9.67970866115956,15.0619206783177,-4.85335551012554));
#88376=CARTESIAN_POINT('Origin',(8.30616075752262,12.9246384215219,-5.5));
#88377=CARTESIAN_POINT('Origin',(8.30616075752262,12.9246384215219,-5.5));
#88378=CARTESIAN_POINT('Origin',(7.1930625741316,11.1926238400616,2.58898520239593));
#88379=CARTESIAN_POINT('Origin',(13.9751741630592,6.38224819080624,-5.5));
#88380=CARTESIAN_POINT('',(14.4133826576228,6.58237130476475,3.2356296922704));
#88381=CARTESIAN_POINT('Origin',(12.1023786047279,5.52697111701458,2.58898520239593));
#88382=CARTESIAN_POINT('',(16.2861782159541,7.43764837855642,-4.85335551012554));
#88383=CARTESIAN_POINT('',(16.2861782159541,7.43764837855642,-4.85335551012554));
#88384=CARTESIAN_POINT('Origin',(13.9751741630592,6.38224819080624,-5.5));
#88385=CARTESIAN_POINT('Origin',(13.9751741630592,6.38224819080624,-5.5));
#88386=CARTESIAN_POINT('Origin',(12.1023786047279,5.52697111701458,2.58898520239593));
#88387=CARTESIAN_POINT('Origin',(15.2071685156866,-2.18646074567955,-5.5));
#88388=CARTESIAN_POINT('',(15.6840076837771,-2.25501986777759,3.2356296922704));
#88389=CARTESIAN_POINT('Origin',(13.1692749396441,-1.89345588397283,2.58898520239593));
#88390=CARTESIAN_POINT('',(17.7219012598197,-2.54802472948431,-4.85335551012554));
#88391=CARTESIAN_POINT('',(17.7219012598196,-2.5480247294843,-4.85335551012554));
#88392=CARTESIAN_POINT('Origin',(15.2071685156866,-2.18646074567955,-5.5));
#88393=CARTESIAN_POINT('Origin',(15.2071685156866,-2.18646074567955,-5.5));
#88394=CARTESIAN_POINT('Origin',(13.1692749396441,-1.89345588397283,2.58898520239593));
#88395=CARTESIAN_POINT('Origin',(11.6109943133017,-10.0609838442055,-5.5));
#88396=CARTESIAN_POINT('',(11.975071088235,-10.3764581655096,3.2356296922704));
#88397=CARTESIAN_POINT('Origin',(10.0550195308735,-8.71272402031884,2.58898520239593));
#88398=CARTESIAN_POINT('',(13.5310458706632,-11.7247179893962,-4.85335551012554));
#88399=CARTESIAN_POINT('',(13.5310458706632,-11.7247179893962,-4.85335551012554));
#88400=CARTESIAN_POINT('Origin',(11.6109943133017,-10.0609838442055,-5.5));
#88401=CARTESIAN_POINT('Origin',(11.6109943133017,-10.0609838442055,-5.5));
#88402=CARTESIAN_POINT('Origin',(10.0550195308735,-8.71272402031884,2.58898520239593));
#88403=CARTESIAN_POINT('Origin',(4.32841145580897,-14.741215659711,-5.5));
#88404=CARTESIAN_POINT('',(4.46413403398731,-15.2034443122421,3.2356296922704));
#88405=CARTESIAN_POINT('Origin',(3.74836646642367,-12.7657638413798,2.58898520239593));
#88406=CARTESIAN_POINT('',(5.04417902337261,-17.1788961305734,-4.85335551012554));
#88407=CARTESIAN_POINT('',(5.04417902337261,-17.1788961305733,-4.85335551012554));
#88408=CARTESIAN_POINT('Origin',(4.32841145580897,-14.741215659711,-5.5));
#88409=CARTESIAN_POINT('Origin',(4.32841145580897,-14.741215659711,-5.5));
#88410=CARTESIAN_POINT('Origin',(3.74836646642367,-12.7657638413798,2.58898520239593));
#88411=CARTESIAN_POINT('Origin',(-4.32841145580919,-14.741215659711,-5.5));
#88412=CARTESIAN_POINT('',(-4.46413403398752,-15.2034443122421,3.2356296922704));
#88413=CARTESIAN_POINT('Origin',(-3.74836646642385,-12.7657638413797,2.58898520239593));
#88414=CARTESIAN_POINT('',(-5.04417902337286,-17.1788961305733,-4.85335551012554));
#88415=CARTESIAN_POINT('',(-5.04417902337286,-17.1788961305733,-4.85335551012554));
#88416=CARTESIAN_POINT('Origin',(-4.32841145580919,-14.741215659711,-5.5));
#88417=CARTESIAN_POINT('Origin',(-4.32841145580919,-14.741215659711,-5.5));
#88418=CARTESIAN_POINT('Origin',(-3.74836646642385,-12.7657638413797,2.58898520239593));
#88419=CARTESIAN_POINT('Origin',(-11.6109943133018,-10.0609838442053,-5.5));
#88420=CARTESIAN_POINT('',(-11.9750710882351,-10.3764581655094,3.2356296922704));
#88421=CARTESIAN_POINT('Origin',(-10.0550195308737,-8.71272402031869,2.58898520239593));
#88422=CARTESIAN_POINT('',(-13.5310458706633,-11.724717989396,-4.85335551012554));
#88423=CARTESIAN_POINT('',(-13.5310458706633,-11.724717989396,-4.85335551012554));
#88424=CARTESIAN_POINT('Origin',(-11.6109943133018,-10.0609838442053,-5.5));
#88425=CARTESIAN_POINT('Origin',(-11.6109943133018,-10.0609838442053,-5.5));
#88426=CARTESIAN_POINT('Origin',(-10.0550195308737,-8.71272402031869,2.58898520239593));
#88427=CARTESIAN_POINT('Origin',(-15.2071685156867,-2.18646074567933,-5.5));
#88428=CARTESIAN_POINT('',(-15.6840076837772,-2.25501986777736,3.2356296922704));
#88429=CARTESIAN_POINT('Origin',(-13.1692749396441,-1.89345588397264,2.58898520239593));
#88430=CARTESIAN_POINT('',(-17.7219012598197,-2.54802472948405,-4.85335551012554));
#88431=CARTESIAN_POINT('',(-17.7219012598197,-2.54802472948405,-4.85335551012554));
#88432=CARTESIAN_POINT('Origin',(-15.2071685156867,-2.18646074567933,-5.5));
#88433=CARTESIAN_POINT('Origin',(-15.2071685156867,-2.18646074567933,-5.5));
#88434=CARTESIAN_POINT('Origin',(-13.1692749396441,-1.89345588397264,2.58898520239593));
#88435=CARTESIAN_POINT('Origin',(-13.9751741630591,6.38224819080644,-5.5));
#88436=CARTESIAN_POINT('',(-14.4133826576227,6.58237130476496,3.2356296922704));
#88437=CARTESIAN_POINT('Origin',(-12.1023786047278,5.52697111701475,2.58898520239593));
#88438=CARTESIAN_POINT('',(-16.286178215954,7.43764837855665,-4.85335551012554));
#88439=CARTESIAN_POINT('',(-16.286178215954,7.43764837855665,-4.85335551012554));
#88440=CARTESIAN_POINT('Origin',(-13.9751741630591,6.38224819080644,-5.5));
#88441=CARTESIAN_POINT('Origin',(-13.9751741630591,6.38224819080644,-5.5));
#88442=CARTESIAN_POINT('Origin',(-12.1023786047278,5.52697111701475,2.58898520239593));
#88443=CARTESIAN_POINT('Origin',(-8.30616075752243,12.924638421522,-5.5));
#88444=CARTESIAN_POINT('',(-8.56661047776834,13.3299060968576,3.2356296922704));
#88445=CARTESIAN_POINT('Origin',(-7.19306257413143,11.1926238400618,2.58898520239593));
#88446=CARTESIAN_POINT('',(-9.67970866115934,15.0619206783178,-4.85335551012554));
#88447=CARTESIAN_POINT('',(-9.67970866115934,15.0619206783178,-4.85335551012554));
#88448=CARTESIAN_POINT('Origin',(-8.30616075752243,12.924638421522,-5.5));
#88449=CARTESIAN_POINT('Origin',(-8.30616075752243,12.924638421522,-5.5));
#88450=CARTESIAN_POINT('Origin',(-7.19306257413143,11.1926238400618,2.58898520239593));
#88451=CARTESIAN_POINT('',(20.3408714641021,26.,-6.92779167366097E-14));
#88452=CARTESIAN_POINT('',(0.,0.,20.8686903425894));
#88453=CARTESIAN_POINT('',(0.,0.,0.));
#88454=CARTESIAN_POINT('',(0.,0.,0.));
#88455=CARTESIAN_POINT('',(0.,0.,0.));
#88456=CARTESIAN_POINT('',(0.,0.,0.));
#88457=CARTESIAN_POINT('',(0.,0.,0.));
#88458=CARTESIAN_POINT('',(0.,0.,0.));
#88459=CARTESIAN_POINT('',(0.,0.,0.));
#88460=CARTESIAN_POINT('',(-20.3408711739,26.,-6.67521593555874E-15));
#88461=CARTESIAN_POINT('',(0.,0.,-20.8686903425894));
#88462=UNCERTAINTY_MEASURE_WITH_UNIT(LENGTH_MEASURE(0.01),#88484,
'DISTANCE_ACCURACY_VALUE',
'Maximum model space distance between geometric entities at asserted c
onnectivities');
#88463=UNCERTAINTY_MEASURE_WITH_UNIT(LENGTH_MEASURE(0.01),#88484,
'DISTANCE_ACCURACY_VALUE',
'Maximum model space distance between geometric entities at asserted c
onnectivities');
#88464=UNCERTAINTY_MEASURE_WITH_UNIT(LENGTH_MEASURE(0.01),#88484,
'DISTANCE_ACCURACY_VALUE',
'Maximum model space distance between geometric entities at asserted c
onnectivities');
#88465=UNCERTAINTY_MEASURE_WITH_UNIT(LENGTH_MEASURE(0.01),#88484,
'DISTANCE_ACCURACY_VALUE',
'Maximum model space distance between geometric entities at asserted c
onnectivities');
#88466=UNCERTAINTY_MEASURE_WITH_UNIT(LENGTH_MEASURE(0.01),#88484,
'DISTANCE_ACCURACY_VALUE',
'Maximum model space distance between geometric entities at asserted c
onnectivities');
#88467=UNCERTAINTY_MEASURE_WITH_UNIT(LENGTH_MEASURE(0.01),#88484,
'DISTANCE_ACCURACY_VALUE',
'Maximum model space distance between geometric entities at asserted c
onnectivities');
#88468=UNCERTAINTY_MEASURE_WITH_UNIT(LENGTH_MEASURE(0.01),#88484,
'DISTANCE_ACCURACY_VALUE',
'Maximum model space distance between geometric entities at asserted c
onnectivities');
#88469=UNCERTAINTY_MEASURE_WITH_UNIT(LENGTH_MEASURE(0.01),#88484,
'DISTANCE_ACCURACY_VALUE',
'Maximum model space distance between geometric entities at asserted c
onnectivities');
#88470=UNCERTAINTY_MEASURE_WITH_UNIT(LENGTH_MEASURE(0.01),#88484,
'DISTANCE_ACCURACY_VALUE',
'Maximum model space distance between geometric entities at asserted c
onnectivities');
#88471=UNCERTAINTY_MEASURE_WITH_UNIT(LENGTH_MEASURE(0.01),#88484,
'DISTANCE_ACCURACY_VALUE',
'Maximum model space distance between geometric entities at asserted c
onnectivities');
#88472=UNCERTAINTY_MEASURE_WITH_UNIT(LENGTH_MEASURE(0.01),#88484,
'DISTANCE_ACCURACY_VALUE',
'Maximum model space distance between geometric entities at asserted c
onnectivities');
#88473=(
GEOMETRIC_REPRESENTATION_CONTEXT(3)
GLOBAL_UNCERTAINTY_ASSIGNED_CONTEXT((#88462))
GLOBAL_UNIT_ASSIGNED_CONTEXT((#88484,#88486,#88487))
REPRESENTATION_CONTEXT('','3D')
);
#88474=(
GEOMETRIC_REPRESENTATION_CONTEXT(3)
GLOBAL_UNCERTAINTY_ASSIGNED_CONTEXT((#88463))
GLOBAL_UNIT_ASSIGNED_CONTEXT((#88484,#88486,#88487))
REPRESENTATION_CONTEXT('','3D')
);
#88475=(
GEOMETRIC_REPRESENTATION_CONTEXT(3)
GLOBAL_UNCERTAINTY_ASSIGNED_CONTEXT((#88464))
GLOBAL_UNIT_ASSIGNED_CONTEXT((#88484,#88486,#88487))
REPRESENTATION_CONTEXT('','3D')
);
#88476=(
GEOMETRIC_REPRESENTATION_CONTEXT(3)
GLOBAL_UNCERTAINTY_ASSIGNED_CONTEXT((#88465))
GLOBAL_UNIT_ASSIGNED_CONTEXT((#88484,#88486,#88487))
REPRESENTATION_CONTEXT('','3D')
);
#88477=(
GEOMETRIC_REPRESENTATION_CONTEXT(3)
GLOBAL_UNCERTAINTY_ASSIGNED_CONTEXT((#88466))
GLOBAL_UNIT_ASSIGNED_CONTEXT((#88484,#88486,#88487))
REPRESENTATION_CONTEXT('','3D')
);
#88478=(
GEOMETRIC_REPRESENTATION_CONTEXT(3)
GLOBAL_UNCERTAINTY_ASSIGNED_CONTEXT((#88467))
GLOBAL_UNIT_ASSIGNED_CONTEXT((#88484,#88486,#88487))
REPRESENTATION_CONTEXT('','3D')
);
#88479=(
GEOMETRIC_REPRESENTATION_CONTEXT(3)
GLOBAL_UNCERTAINTY_ASSIGNED_CONTEXT((#88468))
GLOBAL_UNIT_ASSIGNED_CONTEXT((#88484,#88486,#88487))
REPRESENTATION_CONTEXT('','3D')
);
#88480=(
GEOMETRIC_REPRESENTATION_CONTEXT(3)
GLOBAL_UNCERTAINTY_ASSIGNED_CONTEXT((#88469))
GLOBAL_UNIT_ASSIGNED_CONTEXT((#88484,#88486,#88487))
REPRESENTATION_CONTEXT('','3D')
);
#88481=(
GEOMETRIC_REPRESENTATION_CONTEXT(3)
GLOBAL_UNCERTAINTY_ASSIGNED_CONTEXT((#88470))
GLOBAL_UNIT_ASSIGNED_CONTEXT((#88484,#88486,#88487))
REPRESENTATION_CONTEXT('','3D')
);
#88482=(
GEOMETRIC_REPRESENTATION_CONTEXT(3)
GLOBAL_UNCERTAINTY_ASSIGNED_CONTEXT((#88471))
GLOBAL_UNIT_ASSIGNED_CONTEXT((#88484,#88486,#88487))
REPRESENTATION_CONTEXT('','3D')
);
#88483=(
GEOMETRIC_REPRESENTATION_CONTEXT(3)
GLOBAL_UNCERTAINTY_ASSIGNED_CONTEXT((#88472))
GLOBAL_UNIT_ASSIGNED_CONTEXT((#88484,#88486,#88487))
REPRESENTATION_CONTEXT('','3D')
);
#88484=(
LENGTH_UNIT()
NAMED_UNIT(*)
SI_UNIT(.MILLI.,.METRE.)
);
#88485=(
LENGTH_UNIT()
NAMED_UNIT(*)
SI_UNIT($,.METRE.)
);
#88486=(
NAMED_UNIT(*)
PLANE_ANGLE_UNIT()
SI_UNIT($,.RADIAN.)
);
#88487=(
NAMED_UNIT(*)
SI_UNIT($,.STERADIAN.)
SOLID_ANGLE_UNIT()
);
#88488=SHAPE_DEFINITION_REPRESENTATION(#88498,#88519);
#88489=SHAPE_DEFINITION_REPRESENTATION(#88499,#88520);
#88490=SHAPE_DEFINITION_REPRESENTATION(#88500,#88521);
#88491=SHAPE_DEFINITION_REPRESENTATION(#88501,#88522);
#88492=SHAPE_DEFINITION_REPRESENTATION(#88502,#88523);
#88493=SHAPE_DEFINITION_REPRESENTATION(#88503,#88524);
#88494=SHAPE_DEFINITION_REPRESENTATION(#88504,#88525);
#88495=SHAPE_DEFINITION_REPRESENTATION(#88505,#88526);
#88496=SHAPE_DEFINITION_REPRESENTATION(#88506,#88527);
#88497=SHAPE_DEFINITION_REPRESENTATION(#88507,#88528);
#88498=PRODUCT_DEFINITION_SHAPE('',$,#88530);
#88499=PRODUCT_DEFINITION_SHAPE('',$,#88531);
#88500=PRODUCT_DEFINITION_SHAPE('',$,#88532);
#88501=PRODUCT_DEFINITION_SHAPE('',$,#88533);
#88502=PRODUCT_DEFINITION_SHAPE('',$,#88534);
#88503=PRODUCT_DEFINITION_SHAPE('',$,#88535);
#88504=PRODUCT_DEFINITION_SHAPE('',$,#88536);
#88505=PRODUCT_DEFINITION_SHAPE('',$,#88537);
#88506=PRODUCT_DEFINITION_SHAPE('',$,#88538);
#88507=PRODUCT_DEFINITION_SHAPE('',$,#88539);
#88508=PRODUCT_DEFINITION_SHAPE($,$,#44);
#88509=PRODUCT_DEFINITION_SHAPE($,$,#45);
#88510=PRODUCT_DEFINITION_SHAPE($,$,#46);
#88511=PRODUCT_DEFINITION_SHAPE($,$,#47);
#88512=PRODUCT_DEFINITION_SHAPE($,$,#48);
#88513=PRODUCT_DEFINITION_SHAPE($,$,#49);
#88514=PRODUCT_DEFINITION_SHAPE($,$,#50);
#88515=PRODUCT_DEFINITION_SHAPE($,$,#51);
#88516=PRODUCT_DEFINITION_SHAPE($,$,#52);
#88517=PRODUCT_DEFINITION_SHAPE($,$,#53);
#88518=PRODUCT_DEFINITION_SHAPE($,$,#54);
#88519=SHAPE_REPRESENTATION('',(#13127,#14368,#14369,#14370,#14371,#14372,
#14373,#14374,#14375,#14376,#14377,#14378),#88473);
#88520=SHAPE_REPRESENTATION('',(#13128),#88474);
#88521=SHAPE_REPRESENTATION('',(#13713),#88475);
#88522=SHAPE_REPRESENTATION('',(#13735),#88476);
#88523=SHAPE_REPRESENTATION('',(#13828),#88477);
#88524=SHAPE_REPRESENTATION('',(#13851),#88478);
#88525=SHAPE_REPRESENTATION('',(#13876),#88479);
#88526=SHAPE_REPRESENTATION('',(#13971),#88480);
#88527=SHAPE_REPRESENTATION('',(#13993),#88481);
#88528=SHAPE_REPRESENTATION('',(#14115),#88482);
#88529=PRODUCT_DEFINITION_CONTEXT('part definition',#88561,'design');
#88530=PRODUCT_DEFINITION('MAS-263','MAS-263',#88540,#88529);
#88531=PRODUCT_DEFINITION('Wormgear','Wormgear',#88541,#88529);
#88532=PRODUCT_DEFINITION('Bearing_Cap','Bearing_Cap',#88542,#88529);
#88533=PRODUCT_DEFINITION('Lifting_Screw','Lifting_Screw',#88543,#88529);
#88534=PRODUCT_DEFINITION('Wormgear_Shaft','Wormgear_Shaft',#88544,#88529);
#88535=PRODUCT_DEFINITION('Sleeve_Cap','Sleeve_Cap',#88545,#88529);
#88536=PRODUCT_DEFINITION('Housing','Housing',#88546,#88529);
#88537=PRODUCT_DEFINITION('Bearing_Cap_02','Bearing_Cap_02',#88547,#88529);
#88538=PRODUCT_DEFINITION(
'Permanently Lubricated 440C Stainless Steel Ball Bearing',
'Permanently Lubricated 440C Stainless Steel Ball Bearing',#88548,#88529);
#88539=PRODUCT_DEFINITION('Tapered-Roller Bearing with Steel Ring',
'Tapered-Roller Bearing with Steel Ring',#88549,#88529);
#88540=PRODUCT_DEFINITION_FORMATION('',$,#88563);
#88541=PRODUCT_DEFINITION_FORMATION('',$,#88564);
#88542=PRODUCT_DEFINITION_FORMATION('',$,#88565);
#88543=PRODUCT_DEFINITION_FORMATION('',$,#88566);
#88544=PRODUCT_DEFINITION_FORMATION('',$,#88567);
#88545=PRODUCT_DEFINITION_FORMATION('',$,#88568);
#88546=PRODUCT_DEFINITION_FORMATION('',$,#88569);
#88547=PRODUCT_DEFINITION_FORMATION('',$,#88570);
#88548=PRODUCT_DEFINITION_FORMATION('',$,#88571);
#88549=PRODUCT_DEFINITION_FORMATION('',$,#88572);
#88550=PRODUCT_RELATED_PRODUCT_CATEGORY('MAS-263','MAS-263',(#88563));
#88551=PRODUCT_RELATED_PRODUCT_CATEGORY('Wormgear','Wormgear',(#88564));
#88552=PRODUCT_RELATED_PRODUCT_CATEGORY('Bearing_Cap','Bearing_Cap',(#88565));
#88553=PRODUCT_RELATED_PRODUCT_CATEGORY('Lifting_Screw','Lifting_Screw',
(#88566));
#88554=PRODUCT_RELATED_PRODUCT_CATEGORY('Wormgear_Shaft',
'Wormgear_Shaft',(#88567));
#88555=PRODUCT_RELATED_PRODUCT_CATEGORY('Sleeve_Cap','Sleeve_Cap',(#88568));
#88556=PRODUCT_RELATED_PRODUCT_CATEGORY('Housing','Housing',(#88569));
#88557=PRODUCT_RELATED_PRODUCT_CATEGORY('Bearing_Cap_02',
'Bearing_Cap_02',(#88570));
#88558=PRODUCT_RELATED_PRODUCT_CATEGORY(
'Permanently Lubricated 440C Stainless Steel Ball Bearing',
'Permanently Lubricated 440C Stainless Steel Ball Bearing',(#88571));
#88559=PRODUCT_RELATED_PRODUCT_CATEGORY(
'Tapered-Roller Bearing with Steel Ring',
'Tapered-Roller Bearing with Steel Ring',(#88572));
#88560=APPLICATION_PROTOCOL_DEFINITION('international standard',
'automotive_design',2009,#88561);
#88561=APPLICATION_CONTEXT(
'Core Data for Automotive Mechanical Design Process');
#88562=PRODUCT_CONTEXT('part definition',#88561,'mechanical');
#88563=PRODUCT('MAS-263','MAS-263',$,(#88562));
#88564=PRODUCT('Wormgear','Wormgear',$,(#88562));
#88565=PRODUCT('Bearing_Cap','Bearing_Cap',$,(#88562));
#88566=PRODUCT('Lifting_Screw','Lifting_Screw',$,(#88562));
#88567=PRODUCT('Wormgear_Shaft','Wormgear_Shaft',$,(#88562));
#88568=PRODUCT('Sleeve_Cap','Sleeve_Cap',$,(#88562));
#88569=PRODUCT('Housing','Housing',$,(#88562));
#88570=PRODUCT('Bearing_Cap_02','Bearing_Cap_02',$,(#88562));
#88571=PRODUCT(
'Permanently Lubricated 440C Stainless Steel Ball Bearing',
'Permanently Lubricated 440C Stainless Steel Ball Bearing',$,(#88562));
#88572=PRODUCT('Tapered-Roller Bearing with Steel Ring',
'Tapered-Roller Bearing with Steel Ring',$,(#88562));
#88573=PRESENTATION_STYLE_ASSIGNMENT((#88575));
#88574=PRESENTATION_STYLE_ASSIGNMENT((#88576));
#88575=SURFACE_STYLE_USAGE(.BOTH.,#88577);
#88576=SURFACE_STYLE_USAGE(.BOTH.,#88578);
#88577=SURFACE_SIDE_STYLE('',(#88579));
#88578=SURFACE_SIDE_STYLE('',(#88580));
#88579=SURFACE_STYLE_FILL_AREA(#88581);
#88580=SURFACE_STYLE_FILL_AREA(#88582);
#88581=FILL_AREA_STYLE('Steel - Satin',(#88583));
#88582=FILL_AREA_STYLE('Opaque(160,160,160)',(#88584));
#88583=FILL_AREA_STYLE_COLOUR('Steel - Satin',#88585);
#88584=FILL_AREA_STYLE_COLOUR('Opaque(160,160,160)',#88586);
#88585=COLOUR_RGB('Steel - Satin', 0.66274510, 0.83137255, 0.94901961);
#88586=COLOUR_RGB('Opaque(160,160,160)', 0.66274510, 0.83137255, 0.94901961);
ENDSEC;
END-ISO-10303-21;
